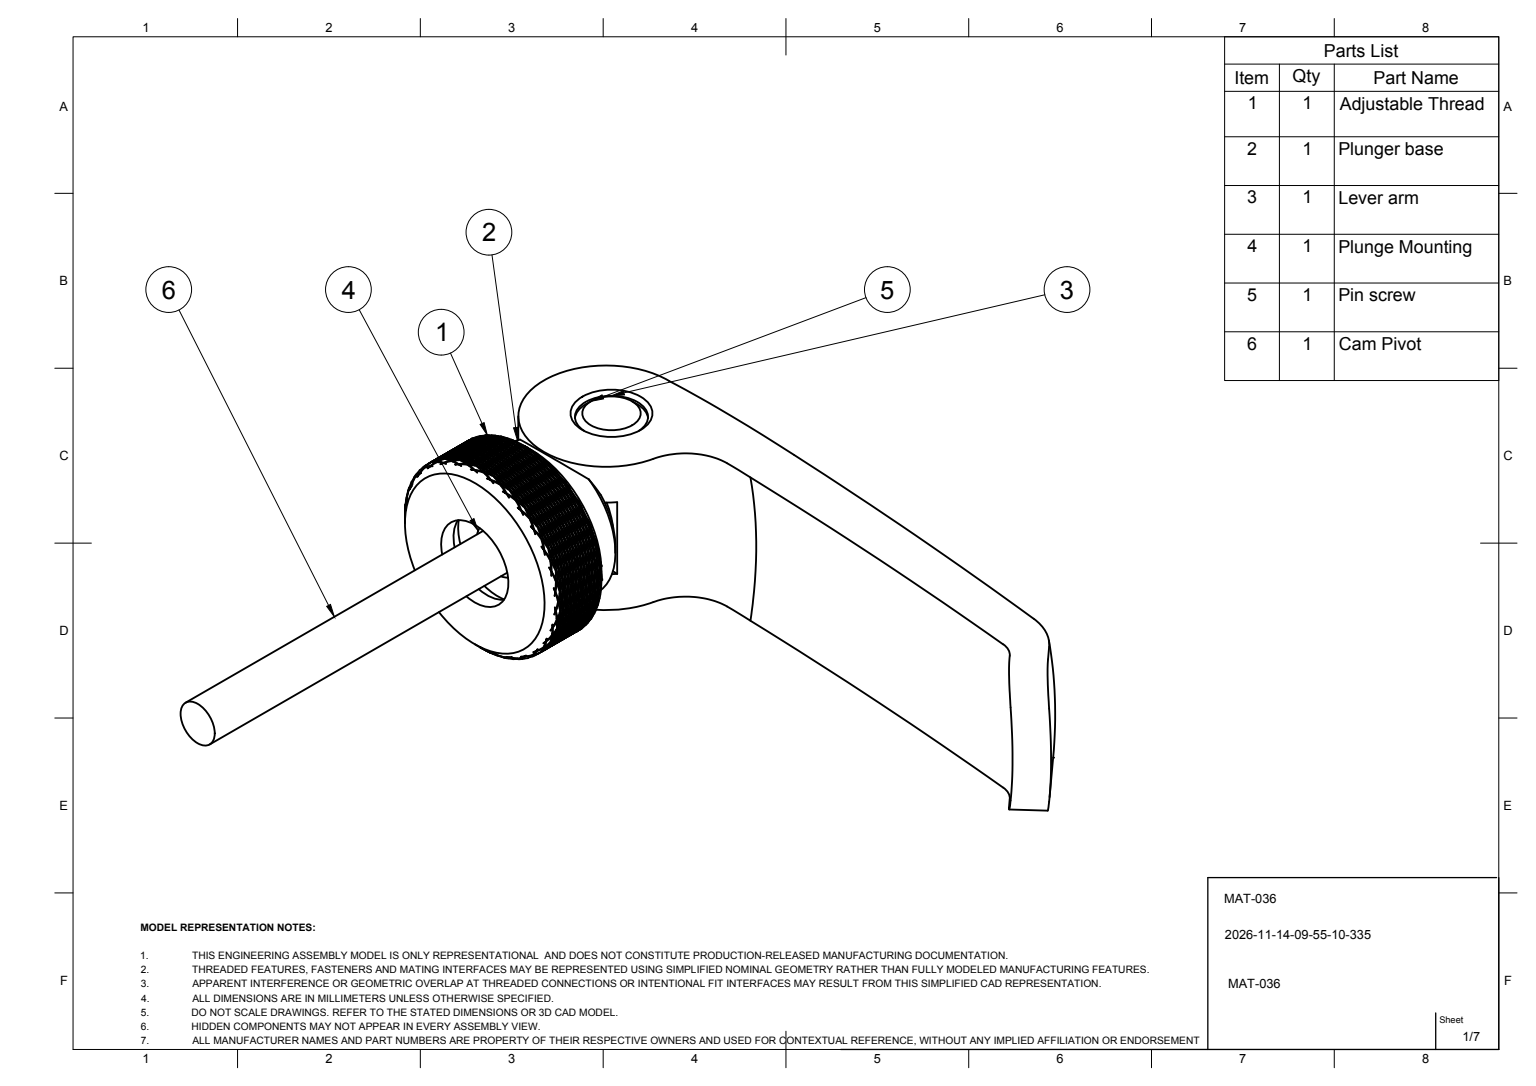
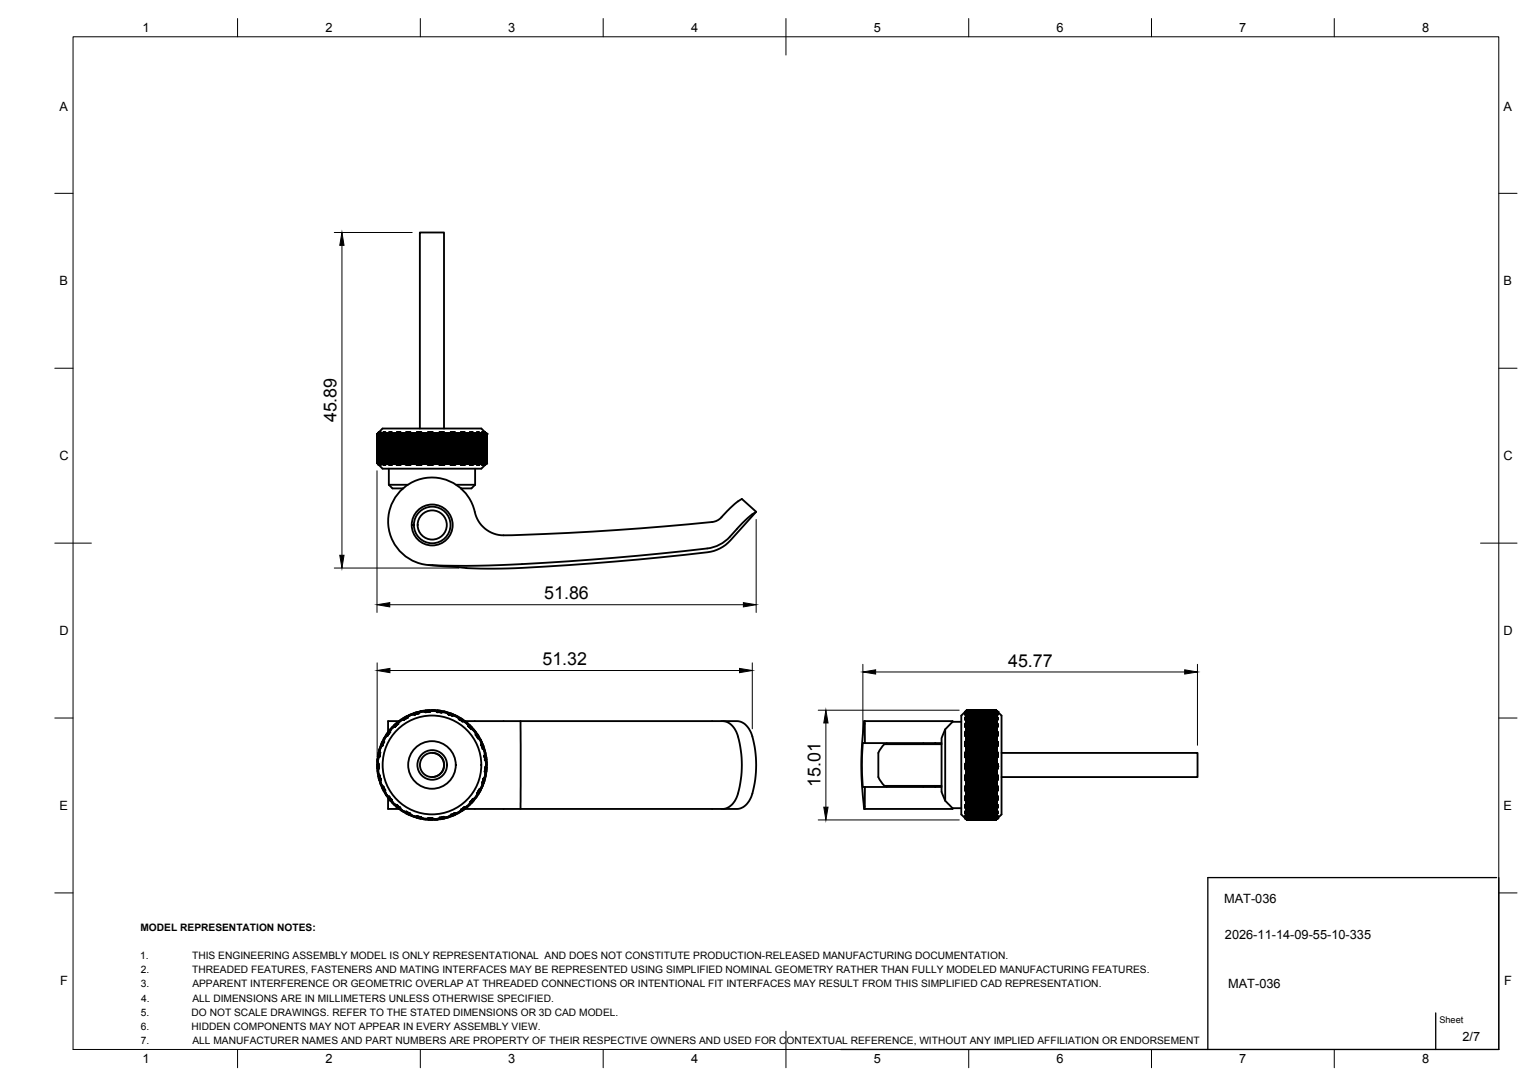
ISO-10303-21;
HEADER;
/* Generated by software containing ST-Developer
 * from STEP Tools, Inc. (www.steptools.com) 
 */

FILE_DESCRIPTION(
/* description */ (''),
/* implementation_level */ '2;1');

FILE_NAME(
/* name */ 'MAT-036.step',
/* time_stamp */ '2026-11-14T09:55:16-08:00',
/* author */ (''),
/* organization */ (''),
/* preprocessor_version */ 'ST-DEVELOPER v20.2',
/* originating_system */ 'Autodesk Translation Framework v15.17.0.0',
/* authorisation */ '');

FILE_SCHEMA (('AUTOMOTIVE_DESIGN { 1 0 10303 214 3 1 1 }'));
ENDSEC;

DATA;
#10=MECHANICAL_DESIGN_GEOMETRIC_PRESENTATION_REPRESENTATION('',(#56,#57,
#58,#59,#60,#61,#62,#63),#170250);
#11=ITEM_DEFINED_TRANSFORMATION($,$,#71472,#77757);
#12=ITEM_DEFINED_TRANSFORMATION($,$,#77641,#77758);
#13=ITEM_DEFINED_TRANSFORMATION($,$,#77681,#77759);
#14=ITEM_DEFINED_TRANSFORMATION($,$,#77711,#77760);
#15=ITEM_DEFINED_TRANSFORMATION($,$,#77739,#77761);
#16=ITEM_DEFINED_TRANSFORMATION($,$,#77751,#77762);
#17=(
REPRESENTATION_RELATIONSHIP($,$,#170276,#170275)
REPRESENTATION_RELATIONSHIP_WITH_TRANSFORMATION(#11)
SHAPE_REPRESENTATION_RELATIONSHIP()
);
#18=(
REPRESENTATION_RELATIONSHIP($,$,#170277,#170275)
REPRESENTATION_RELATIONSHIP_WITH_TRANSFORMATION(#12)
SHAPE_REPRESENTATION_RELATIONSHIP()
);
#19=(
REPRESENTATION_RELATIONSHIP($,$,#170278,#170275)
REPRESENTATION_RELATIONSHIP_WITH_TRANSFORMATION(#13)
SHAPE_REPRESENTATION_RELATIONSHIP()
);
#20=(
REPRESENTATION_RELATIONSHIP($,$,#170279,#170275)
REPRESENTATION_RELATIONSHIP_WITH_TRANSFORMATION(#14)
SHAPE_REPRESENTATION_RELATIONSHIP()
);
#21=(
REPRESENTATION_RELATIONSHIP($,$,#170280,#170275)
REPRESENTATION_RELATIONSHIP_WITH_TRANSFORMATION(#15)
SHAPE_REPRESENTATION_RELATIONSHIP()
);
#22=(
REPRESENTATION_RELATIONSHIP($,$,#170281,#170275)
REPRESENTATION_RELATIONSHIP_WITH_TRANSFORMATION(#16)
SHAPE_REPRESENTATION_RELATIONSHIP()
);
#23=CONTEXT_DEPENDENT_SHAPE_REPRESENTATION(#17,#170269);
#24=CONTEXT_DEPENDENT_SHAPE_REPRESENTATION(#18,#170270);
#25=CONTEXT_DEPENDENT_SHAPE_REPRESENTATION(#19,#170271);
#26=CONTEXT_DEPENDENT_SHAPE_REPRESENTATION(#20,#170272);
#27=CONTEXT_DEPENDENT_SHAPE_REPRESENTATION(#21,#170273);
#28=CONTEXT_DEPENDENT_SHAPE_REPRESENTATION(#22,#170274);
#29=NEXT_ASSEMBLY_USAGE_OCCURRENCE('Adjustable Thread:1',
'Adjustable Thread:1','Adjustable Thread:1',#170283,#170284,
'Adjustable Thread:1');
#30=NEXT_ASSEMBLY_USAGE_OCCURRENCE('Plunger base:1','Plunger base:1',
'Plunger base:1',#170283,#170285,'Plunger base:1');
#31=NEXT_ASSEMBLY_USAGE_OCCURRENCE('Lever arm:1','Lever arm:1',
'Lever arm:1',#170283,#170286,'Lever arm:1');
#32=NEXT_ASSEMBLY_USAGE_OCCURRENCE('Plunge Mounting:1',
'Plunge Mounting:1','Plunge Mounting:1',#170283,#170287,
'Plunge Mounting:1');
#33=NEXT_ASSEMBLY_USAGE_OCCURRENCE('Pin screw:1','Pin screw:1',
'Pin screw:1',#170283,#170288,'Pin screw:1');
#34=NEXT_ASSEMBLY_USAGE_OCCURRENCE('Cam Pivot:1','Cam Pivot:1',
'Cam Pivot:1',#170283,#170289,'Cam Pivot:1');
#35=SPHERICAL_SURFACE('',#77715,4.00000000000002);
#36=B_SPLINE_SURFACE_WITH_KNOTS('',3,3,((#168992,#168993,#168994,#168995),
(#168996,#168997,#168998,#168999),(#169000,#169001,#169002,#169003),(#169004,
#169005,#169006,#169007),(#169008,#169009,#169010,#169011),(#169012,#169013,
#169014,#169015),(#169016,#169017,#169018,#169019),(#169020,#169021,#169022,
#169023),(#169024,#169025,#169026,#169027),(#169028,#169029,#169030,#169031)),
 .UNSPECIFIED.,.F.,.F.,.F.,(4,1,1,1,3,4),(4,4),(0.135790601649557,0.226849968153009,
0.317909334656459,0.40896870115991,0.500028067663362,0.5036704423235),(0.807901539596212,
1.),.UNSPECIFIED.);
#37=B_SPLINE_SURFACE_WITH_KNOTS('',3,3,((#169171,#169172,#169173,#169174,
#169175,#169176,#169177),(#169178,#169179,#169180,#169181,#169182,#169183,
#169184),(#169185,#169186,#169187,#169188,#169189,#169190,#169191),(#169192,
#169193,#169194,#169195,#169196,#169197,#169198),(#169199,#169200,#169201,
#169202,#169203,#169204,#169205),(#169206,#169207,#169208,#169209,#169210,
#169211,#169212),(#169213,#169214,#169215,#169216,#169217,#169218,#169219),
(#169220,#169221,#169222,#169223,#169224,#169225,#169226),(#169227,#169228,
#169229,#169230,#169231,#169232,#169233),(#169234,#169235,#169236,#169237,
#169238,#169239,#169240),(#169241,#169242,#169243,#169244,#169245,#169246,
#169247),(#169248,#169249,#169250,#169251,#169252,#169253,#169254),(#169255,
#169256,#169257,#169258,#169259,#169260,#169261)),.UNSPECIFIED.,.F.,.F.,
 .F.,(4,3,1,1,1,3,4),(4,3,4),(0.114681185572966,0.118496689180301,0.213879533801066,
0.309262378421832,0.404645223042596,0.500028067663362,0.500047049913778),
(-2.58598232202791E-10,0.97179933976621,0.977592668595424),
 .UNSPECIFIED.);
#38=B_SPLINE_SURFACE_WITH_KNOTS('',3,3,((#169612,#169613,#169614,#169615,
#169616,#169617),(#169618,#169619,#169620,#169621,#169622,#169623),(#169624,
#169625,#169626,#169627,#169628,#169629),(#169630,#169631,#169632,#169633,
#169634,#169635),(#169636,#169637,#169638,#169639,#169640,#169641),(#169642,
#169643,#169644,#169645,#169646,#169647),(#169648,#169649,#169650,#169651,
#169652,#169653),(#169654,#169655,#169656,#169657,#169658,#169659),(#169660,
#169661,#169662,#169663,#169664,#169665),(#169666,#169667,#169668,#169669,
#169670,#169671),(#169672,#169673,#169674,#169675,#169676,#169677),(#169678,
#169679,#169680,#169681,#169682,#169683)),.UNSPECIFIED.,.F.,.F.,.F.,(4,
1,1,1,2,1,1,1,4),(4,2,4),(0.618524756843663,0.666209162238205,0.713893567632747,
0.761577973027289,0.809262378421831,0.856946783816374,0.904631189210916,
0.952315594605458,1.),(0.,0.931730586032522,0.937129966266598),
 .UNSPECIFIED.);
#39=B_SPLINE_SURFACE_WITH_KNOTS('',3,3,((#169891,#169892,#169893,#169894),
(#169895,#169896,#169897,#169898),(#169899,#169900,#169901,#169902),(#169903,
#169904,#169905,#169906),(#169907,#169908,#169909,#169910),(#169911,#169912,
#169913,#169914),(#169915,#169916,#169917,#169918),(#169919,#169920,#169921,
#169922),(#169923,#169924,#169925,#169926),(#169927,#169928,#169929,#169930),
(#169931,#169932,#169933,#169934),(#169935,#169936,#169937,#169938),(#169939,
#169940,#169941,#169942),(#169943,#169944,#169945,#169946),(#169947,#169948,
#169949,#169950)),.UNSPECIFIED.,.F.,.F.,.F.,(4,3,1,1,1,2,1,1,1,4),(4,4),
(0.632176856006048,0.635818669312919,0.681341335648804,0.726864001984689,
0.772386668320574,0.81790933465646,0.863432000992345,0.90895466732823,0.954477333664115,
1.),(0.0153819466590792,1.),.UNSPECIFIED.);
#40=OPEN_SHELL('',(#71352));
#41=OPEN_SHELL('',(#71353));
#42=SHELL_BASED_SURFACE_MODEL('Body2',(#40));
#43=SHELL_BASED_SURFACE_MODEL('Body3',(#41));
#44=SHAPE_REPRESENTATION_RELATIONSHIP('SRR','None',#170276,#50);
#45=SHAPE_REPRESENTATION_RELATIONSHIP('SRR','None',#170277,#51);
#46=SHAPE_REPRESENTATION_RELATIONSHIP('SRR','None',#170278,#52);
#47=SHAPE_REPRESENTATION_RELATIONSHIP('SRR','None',#170279,#53);
#48=SHAPE_REPRESENTATION_RELATIONSHIP('SRR','None',#170280,#54);
#49=SHAPE_REPRESENTATION_RELATIONSHIP('SRR','None',#170281,#55);
#50=ADVANCED_BREP_SHAPE_REPRESENTATION('',(#64),#170244);
#51=ADVANCED_BREP_SHAPE_REPRESENTATION('',(#65),#170245);
#52=ADVANCED_BREP_SHAPE_REPRESENTATION('',(#66),#170246);
#53=ADVANCED_BREP_SHAPE_REPRESENTATION('',(#67),#170247);
#54=ADVANCED_BREP_SHAPE_REPRESENTATION('',(#68),#170248);
#55=ADVANCED_BREP_SHAPE_REPRESENTATION('',(#69),#170249);
#56=STYLED_ITEM('',(#170315),#64);
#57=STYLED_ITEM('',(#170314),#65);
#58=STYLED_ITEM('',(#170314),#42);
#59=STYLED_ITEM('',(#170314),#43);
#60=STYLED_ITEM('',(#170316),#66);
#61=STYLED_ITEM('',(#170315),#67);
#62=STYLED_ITEM('',(#170317),#68);
#63=STYLED_ITEM('',(#170315),#69);
#64=MANIFOLD_SOLID_BREP('Body1',#71398);
#65=MANIFOLD_SOLID_BREP('Body1',#71399);
#66=MANIFOLD_SOLID_BREP('Body1',#71400);
#67=MANIFOLD_SOLID_BREP('Body1',#71401);
#68=MANIFOLD_SOLID_BREP('Body1',#71402);
#69=MANIFOLD_SOLID_BREP('Body1',#71403);
#70=FACE_BOUND('',#15472,.T.);
#71=FACE_BOUND('',#15675,.T.);
#72=FACE_BOUND('',#15851,.T.);
#73=FACE_BOUND('',#15853,.T.);
#74=FACE_BOUND('',#15862,.T.);
#75=FACE_BOUND('',#15864,.T.);
#76=FACE_BOUND('',#15893,.T.);
#77=FACE_BOUND('',#15895,.T.);
#78=FACE_BOUND('',#15897,.T.);
#79=FACE_BOUND('',#15901,.T.);
#80=FACE_BOUND('',#15903,.T.);
#81=FACE_BOUND('',#15905,.T.);
#82=FACE_BOUND('',#15911,.T.);
#83=FACE_BOUND('',#15916,.T.);
#84=FACE_BOUND('',#15918,.T.);
#85=FACE_BOUND('',#15920,.T.);
#86=PLANE('',#77414);
#87=PLANE('',#77609);
#88=PLANE('',#77639);
#89=PLANE('',#77640);
#90=PLANE('',#77665);
#91=PLANE('',#77666);
#92=PLANE('',#77667);
#93=PLANE('',#77670);
#94=PLANE('',#77672);
#95=PLANE('',#77673);
#96=PLANE('',#77674);
#97=PLANE('',#77675);
#98=PLANE('',#77702);
#99=PLANE('',#77704);
#100=PLANE('',#77706);
#101=PLANE('',#77707);
#102=PLANE('',#77710);
#103=PLANE('',#77733);
#104=PLANE('',#77734);
#105=PLANE('',#77735);
#106=PLANE('',#77737);
#107=PLANE('',#77738);
#108=PLANE('',#77748);
#109=PLANE('',#77749);
#110=PLANE('',#77755);
#111=PLANE('',#77756);
#112=ELLIPSE('',#76563,9.43047305119864,1.30240788908406);
#113=ELLIPSE('',#76566,9.43046793206525,1.30241506001113);
#114=ELLIPSE('',#76569,9.43050328768157,1.3024182004793);
#115=ELLIPSE('',#76572,9.43068708057878,1.30243363570333);
#116=ELLIPSE('',#76575,9.43006152330499,1.30236357371331);
#117=ELLIPSE('',#76578,9.4302777984402,1.30238875446472);
#118=ELLIPSE('',#76581,9.43072787174344,1.30243587534547);
#119=ELLIPSE('',#76584,9.43045773730215,1.30241075091437);
#120=ELLIPSE('',#76587,9.43030510916545,1.30239601642258);
#121=ELLIPSE('',#76590,9.43064494614307,1.30242369243536);
#122=ELLIPSE('',#76593,9.43056062900003,1.30242031583658);
#123=ELLIPSE('',#76596,9.43045585415815,1.30241175558088);
#124=ELLIPSE('',#76599,9.43046939213538,1.30240966255557);
#125=ELLIPSE('',#76602,9.43067088687587,1.30243579801834);
#126=ELLIPSE('',#76605,9.43040719667397,1.30240457641196);
#127=ELLIPSE('',#76608,9.42988108574405,1.30234497490862);
#128=ELLIPSE('',#76611,9.43068064311873,1.30243410507078);
#129=ELLIPSE('',#76614,9.43052303530734,1.30242084912571);
#130=ELLIPSE('',#76617,9.43038125328305,1.30240668645391);
#131=ELLIPSE('',#76620,9.43072128552616,1.30244009783621);
#132=ELLIPSE('',#76623,9.4305707477918,1.30242345770117);
#133=ELLIPSE('',#76626,9.43046465435441,1.30241113143356);
#134=ELLIPSE('',#76629,9.4308407271015,1.30245127577812);
#135=ELLIPSE('',#76632,9.43070104226015,1.30243878786344);
#136=ELLIPSE('',#76635,9.43055049151391,1.30242224667773);
#137=ELLIPSE('',#76638,9.43061695677763,1.30242474192035);
#138=ELLIPSE('',#76641,9.43035235935973,1.30239838521342);
#139=ELLIPSE('',#76644,9.4305559320503,1.30242196321693);
#140=ELLIPSE('',#76647,9.43068952357752,1.30243327777871);
#141=ELLIPSE('',#77415,9.431895379298,1.30254932670111);
#142=ELLIPSE('',#77418,15.3174410154795,1.90661239924035);
#143=ELLIPSE('',#77421,15.3157768747818,1.90647582479234);
#144=ELLIPSE('',#77424,15.3170696122663,1.90658252792732);
#145=ELLIPSE('',#77427,15.3167139940069,1.90655328959697);
#146=ELLIPSE('',#77430,15.3168209377553,1.90657168275161);
#147=ELLIPSE('',#77433,15.3160754936824,1.90650905813206);
#148=ELLIPSE('',#77436,15.3161208425833,1.90650426169268);
#149=ELLIPSE('',#77439,15.3159589603063,1.90649559716548);
#150=ELLIPSE('',#77442,15.3157944590339,1.9064768703695);
#151=ELLIPSE('',#77445,15.3172323469206,1.9066030234614);
#152=ELLIPSE('',#77448,15.3155039380165,1.9064570427492);
#153=ELLIPSE('',#77451,15.3159291529044,1.90649334528717);
#154=ELLIPSE('',#77454,15.3157700330761,1.90647081272421);
#155=ELLIPSE('',#77457,15.3160955154982,1.90650647722667);
#156=ELLIPSE('',#77460,15.3166693144536,1.90656216883429);
#157=ELLIPSE('',#77463,15.3166817133067,1.90655124693864);
#158=ELLIPSE('',#77466,15.31703730362,1.90657833462818);
#159=ELLIPSE('',#77469,15.3160164937855,1.90649874196003);
#160=ELLIPSE('',#77472,15.3158753484009,1.90648217113556);
#161=ELLIPSE('',#77475,15.3162380117898,1.90650822609983);
#162=ELLIPSE('',#77478,15.3156441463648,1.90646585124018);
#163=ELLIPSE('',#77481,15.317005919152,1.90658194664794);
#164=ELLIPSE('',#77484,15.3161739347467,1.90650429978856);
#165=ELLIPSE('',#77487,15.3153630258202,1.90644004375235);
#166=ELLIPSE('',#77490,15.3163094563979,1.90652013375223);
#167=ELLIPSE('',#77493,15.3167561122212,1.90656182181374);
#168=ELLIPSE('',#77496,15.3163730027201,1.90652953147296);
#169=ELLIPSE('',#77499,15.315903684448,1.90649008174056);
#170=ELLIPSE('',#77530,3.69853833711443,0.520053862149324);
#171=ELLIPSE('',#77535,3.6990050944682,0.520121997590068);
#172=ELLIPSE('',#77538,3.69740745136945,0.519884819312743);
#173=ELLIPSE('',#77541,3.6973850577443,0.519871926709589);
#174=ELLIPSE('',#77544,3.69880689749974,0.520100628836089);
#175=ELLIPSE('',#77547,3.69848799508326,0.520043846508826);
#176=ELLIPSE('',#77552,3.6988594244713,0.520105289468088);
#177=ELLIPSE('',#77555,3.6986202776342,0.520065731438254);
#178=ELLIPSE('',#77558,3.69735633553684,0.519872421748739);
#179=ELLIPSE('',#77561,3.69840385438922,0.520042143078421);
#180=ELLIPSE('',#77566,3.69753466975073,0.519893625210943);
#181=ELLIPSE('',#77569,3.69957450398795,0.520227606150056);
#182=ELLIPSE('',#77574,3.69928463265645,0.520166995452598);
#183=ELLIPSE('',#77579,3.69917885823403,0.520148170670083);
#184=ELLIPSE('',#77582,3.69767815300263,0.519919195910691);
#185=ELLIPSE('',#77589,3.69757944713663,0.519903285571644);
#186=ELLIPSE('',#77592,3.69653763812213,0.519733793607226);
#187=ELLIPSE('',#77595,3.69967418134432,0.520228182339355);
#188=ELLIPSE('',#77598,3.69741584633747,0.519874782638118);
#189=ELLIPSE('',#77601,3.69673411928317,0.519776228529677);
#190=ELLIPSE('',#77604,3.69979295210335,0.520255955848595);
#191=ELLIPSE('',#77607,3.69808486598988,0.51998245490985);
#192=ELLIPSE('',#77705,65.55169862647,42.389902647677);
#193=ELLIPSE('',#77708,65.5506952259048,42.388915448489);
#194=(
BOUNDED_SURFACE()
B_SPLINE_SURFACE(1,2,((#95581,#95582,#95583),(#95584,#95585,#95586)),
 .UNSPECIFIED.,.F.,.F.,.F.)
B_SPLINE_SURFACE_WITH_KNOTS((2,2),(3,3),(0.,0.289681084359929),(0.331965345783649,
0.349369696259361),.UNSPECIFIED.)
GEOMETRIC_REPRESENTATION_ITEM()
RATIONAL_B_SPLINE_SURFACE(((0.988555124858681,0.99035748704491,0.99513694090229),
(0.988555124858681,0.99035748704491,0.99513694090229)))
REPRESENTATION_ITEM('')
SURFACE()
);
#195=(
BOUNDED_SURFACE()
B_SPLINE_SURFACE(1,2,((#95600,#95601,#95602,#95603,#95604),(#95605,#95606,
#95607,#95608,#95609),(#95610,#95611,#95612,#95613,#95614)),
 .UNSPECIFIED.,.F.,.F.,.F.)
B_SPLINE_SURFACE_WITH_KNOTS((2,1,2),(3,2,3),(-0.00289807040992861,0.,0.29039955403664),
(0.383340713896693,0.383933227114987,0.401145492974693),.UNSPECIFIED.)
GEOMETRIC_REPRESENTATION_ITEM()
RATIONAL_B_SPLINE_SURFACE(((0.988246641953811,0.988246641953811,0.988246641953811,
0.986737013496293,0.988139125479962),(0.988246641953811,0.988246641953811,
0.988246641953811,0.986737013496293,0.988139125479962),(0.988246641953811,
0.988246641953811,0.988246641953811,0.986737013496293,0.988139125479961)))
REPRESENTATION_ITEM('')
SURFACE()
);
#196=(
BOUNDED_SURFACE()
B_SPLINE_SURFACE(1,2,((#95639,#95640,#95641),(#95642,#95643,#95644)),
 .UNSPECIFIED.,.F.,.F.,.F.)
B_SPLINE_SURFACE_WITH_KNOTS((2,2),(3,3),(0.,0.289681084359919),(0.331965345783649,
0.349369696259361),.UNSPECIFIED.)
GEOMETRIC_REPRESENTATION_ITEM()
RATIONAL_B_SPLINE_SURFACE(((0.988555124858681,0.99035748704491,0.99513694090229),
(0.988555124858682,0.99035748704491,0.99513694090229)))
REPRESENTATION_ITEM('')
SURFACE()
);
#197=(
BOUNDED_SURFACE()
B_SPLINE_SURFACE(1,2,((#95648,#95649,#95650,#95651,#95652),(#95653,#95654,
#95655,#95656,#95657),(#95658,#95659,#95660,#95661,#95662)),
 .UNSPECIFIED.,.F.,.F.,.F.)
B_SPLINE_SURFACE_WITH_KNOTS((2,1,2),(3,2,3),(-0.00289807040992683,0.,0.290399554012505),
(0.38334071392065,0.383933227114987,0.401145492974695),.UNSPECIFIED.)
GEOMETRIC_REPRESENTATION_ITEM()
RATIONAL_B_SPLINE_SURFACE(((0.988246641953811,0.988246641953811,0.988246641953811,
0.986737013496293,0.988139125479962),(0.988246641953811,0.988246641953811,
0.988246641953811,0.986737013496293,0.988139125479962),(0.988246641953811,
0.988246641953811,0.988246641953811,0.986737013496293,0.988139125479962)))
REPRESENTATION_ITEM('')
SURFACE()
);
#198=(
BOUNDED_SURFACE()
B_SPLINE_SURFACE(1,2,((#95687,#95688,#95689),(#95690,#95691,#95692)),
 .UNSPECIFIED.,.F.,.F.,.F.)
B_SPLINE_SURFACE_WITH_KNOTS((2,2),(3,3),(0.,0.289681084359922),(0.331965345783648,
0.349369696259454),.UNSPECIFIED.)
GEOMETRIC_REPRESENTATION_ITEM()
RATIONAL_B_SPLINE_SURFACE(((0.988555124858681,0.99035748704492,0.995136940902341),
(0.988555124858682,0.99035748704492,0.995136940902341)))
REPRESENTATION_ITEM('')
SURFACE()
);
#199=(
BOUNDED_SURFACE()
B_SPLINE_SURFACE(1,2,((#95696,#95697,#95698,#95699,#95700),(#95701,#95702,
#95703,#95704,#95705),(#95706,#95707,#95708,#95709,#95710)),
 .UNSPECIFIED.,.F.,.F.,.F.)
B_SPLINE_SURFACE_WITH_KNOTS((2,1,2),(3,2,3),(-0.00289807040992654,0.,0.290399554026877),
(0.383340713906249,0.383933227114987,0.401145492974697),.UNSPECIFIED.)
GEOMETRIC_REPRESENTATION_ITEM()
RATIONAL_B_SPLINE_SURFACE(((0.988246641953811,0.988246641953811,0.988246641953811,
0.986737013496293,0.988139125479962),(0.988246641953811,0.988246641953811,
0.988246641953811,0.986737013496293,0.988139125479962),(0.988246641953811,
0.988246641953811,0.988246641953811,0.986737013496293,0.988139125479962)))
REPRESENTATION_ITEM('')
SURFACE()
);
#200=(
BOUNDED_SURFACE()
B_SPLINE_SURFACE(1,2,((#95735,#95736,#95737),(#95738,#95739,#95740)),
 .UNSPECIFIED.,.F.,.F.,.F.)
B_SPLINE_SURFACE_WITH_KNOTS((2,2),(3,3),(0.,0.289681084359918),(0.331965345783649,
0.349369696259361),.UNSPECIFIED.)
GEOMETRIC_REPRESENTATION_ITEM()
RATIONAL_B_SPLINE_SURFACE(((0.988555124858682,0.99035748704491,0.99513694090229),
(0.988555124858682,0.99035748704491,0.99513694090229)))
REPRESENTATION_ITEM('')
SURFACE()
);
#201=(
BOUNDED_SURFACE()
B_SPLINE_SURFACE(1,2,((#95744,#95745,#95746,#95747,#95748),(#95749,#95750,
#95751,#95752,#95753),(#95754,#95755,#95756,#95757,#95758)),
 .UNSPECIFIED.,.F.,.F.,.F.)
B_SPLINE_SURFACE_WITH_KNOTS((2,1,2),(3,2,3),(-0.00289807040992802,0.,0.29039955403663),
(0.383340713896644,0.383933227114987,0.401145492974693),.UNSPECIFIED.)
GEOMETRIC_REPRESENTATION_ITEM()
RATIONAL_B_SPLINE_SURFACE(((0.988246641953811,0.988246641953811,0.988246641953811,
0.986737013496293,0.988139125479962),(0.988246641953811,0.988246641953811,
0.988246641953811,0.986737013496293,0.988139125479962),(0.988246641953811,
0.988246641953811,0.988246641953811,0.986737013496293,0.988139125479962)))
REPRESENTATION_ITEM('')
SURFACE()
);
#202=(
BOUNDED_SURFACE()
B_SPLINE_SURFACE(1,2,((#95783,#95784,#95785),(#95786,#95787,#95788)),
 .UNSPECIFIED.,.F.,.F.,.F.)
B_SPLINE_SURFACE_WITH_KNOTS((2,2),(3,3),(0.,0.289681084359923),(0.331965345783649,
0.349369696259361),.UNSPECIFIED.)
GEOMETRIC_REPRESENTATION_ITEM()
RATIONAL_B_SPLINE_SURFACE(((0.988555124858681,0.99035748704491,0.99513694090229),
(0.988555124858682,0.99035748704491,0.99513694090229)))
REPRESENTATION_ITEM('')
SURFACE()
);
#203=(
BOUNDED_SURFACE()
B_SPLINE_SURFACE(1,2,((#95792,#95793,#95794,#95795,#95796),(#95797,#95798,
#95799,#95800,#95801),(#95802,#95803,#95804,#95805,#95806)),
 .UNSPECIFIED.,.F.,.F.,.F.)
B_SPLINE_SURFACE_WITH_KNOTS((2,1,2),(3,2,3),(-0.00289807040992325,0.,0.290399554035561),
(0.383340713897236,0.383933227114987,0.401145492974693),.UNSPECIFIED.)
GEOMETRIC_REPRESENTATION_ITEM()
RATIONAL_B_SPLINE_SURFACE(((0.988246641953811,0.988246641953811,0.988246641953811,
0.986737013496293,0.988139125479962),(0.988246641953811,0.988246641953811,
0.988246641953811,0.986737013496293,0.988139125479962),(0.988246641953811,
0.988246641953811,0.988246641953811,0.986737013496293,0.988139125479961)))
REPRESENTATION_ITEM('')
SURFACE()
);
#204=(
BOUNDED_SURFACE()
B_SPLINE_SURFACE(1,2,((#95831,#95832,#95833),(#95834,#95835,#95836)),
 .UNSPECIFIED.,.F.,.F.,.F.)
B_SPLINE_SURFACE_WITH_KNOTS((2,2),(3,3),(0.,0.289681084359924),(0.331965345783649,
0.349369696259361),.UNSPECIFIED.)
GEOMETRIC_REPRESENTATION_ITEM()
RATIONAL_B_SPLINE_SURFACE(((0.988555124858681,0.99035748704491,0.99513694090229),
(0.988555124858682,0.99035748704491,0.99513694090229)))
REPRESENTATION_ITEM('')
SURFACE()
);
#205=(
BOUNDED_SURFACE()
B_SPLINE_SURFACE(1,2,((#95840,#95841,#95842,#95843,#95844),(#95845,#95846,
#95847,#95848,#95849),(#95850,#95851,#95852,#95853,#95854)),
 .UNSPECIFIED.,.F.,.F.,.F.)
B_SPLINE_SURFACE_WITH_KNOTS((2,1,2),(3,2,3),(-0.00289807040992448,0.,0.290399554023854),
(0.383340713909065,0.383933227114976,0.401145492974693),.UNSPECIFIED.)
GEOMETRIC_REPRESENTATION_ITEM()
RATIONAL_B_SPLINE_SURFACE(((0.988246641953813,0.988246641953813,0.988246641953813,
0.986737013496292,0.988139125479961),(0.988246641953813,0.988246641953813,
0.988246641953813,0.986737013496292,0.988139125479961),(0.988246641953813,
0.988246641953813,0.988246641953813,0.986737013496292,0.988139125479961)))
REPRESENTATION_ITEM('')
SURFACE()
);
#206=(
BOUNDED_SURFACE()
B_SPLINE_SURFACE(1,2,((#95879,#95880,#95881),(#95882,#95883,#95884)),
 .UNSPECIFIED.,.F.,.F.,.F.)
B_SPLINE_SURFACE_WITH_KNOTS((2,2),(3,3),(0.,0.289681084359932),(0.331965345783649,
0.349369696259361),.UNSPECIFIED.)
GEOMETRIC_REPRESENTATION_ITEM()
RATIONAL_B_SPLINE_SURFACE(((0.988555124858682,0.99035748704491,0.99513694090229),
(0.988555124858682,0.99035748704491,0.99513694090229)))
REPRESENTATION_ITEM('')
SURFACE()
);
#207=(
BOUNDED_SURFACE()
B_SPLINE_SURFACE(1,2,((#95888,#95889,#95890,#95891,#95892),(#95893,#95894,
#95895,#95896,#95897),(#95898,#95899,#95900,#95901,#95902)),
 .UNSPECIFIED.,.F.,.F.,.F.)
B_SPLINE_SURFACE_WITH_KNOTS((2,1,2),(3,2,3),(-0.00289807040992691,0.,0.290399554024332),
(0.383340713908832,0.383933227114987,0.401145492974693),.UNSPECIFIED.)
GEOMETRIC_REPRESENTATION_ITEM()
RATIONAL_B_SPLINE_SURFACE(((0.988246641953811,0.988246641953811,0.988246641953811,
0.986737013496293,0.988139125479962),(0.988246641953811,0.988246641953811,
0.988246641953811,0.986737013496293,0.988139125479962),(0.988246641953811,
0.988246641953811,0.988246641953811,0.986737013496293,0.988139125479962)))
REPRESENTATION_ITEM('')
SURFACE()
);
#208=(
BOUNDED_SURFACE()
B_SPLINE_SURFACE(1,2,((#95912,#95913,#95914),(#95915,#95916,#95917)),
 .UNSPECIFIED.,.F.,.F.,.F.)
B_SPLINE_SURFACE_WITH_KNOTS((2,2),(3,3),(0.,0.289681084359925),(0.331965345783649,
0.349369696259361),.UNSPECIFIED.)
GEOMETRIC_REPRESENTATION_ITEM()
RATIONAL_B_SPLINE_SURFACE(((0.988555124858682,0.99035748704491,0.99513694090229),
(0.988555124858682,0.99035748704491,0.99513694090229)))
REPRESENTATION_ITEM('')
SURFACE()
);
#209=(
BOUNDED_SURFACE()
B_SPLINE_SURFACE(1,2,((#95921,#95922,#95923,#95924,#95925),(#95926,#95927,
#95928,#95929,#95930),(#95931,#95932,#95933,#95934,#95935)),
 .UNSPECIFIED.,.F.,.F.,.F.)
B_SPLINE_SURFACE_WITH_KNOTS((2,1,2),(3,2,3),(-0.00289807040992912,0.,0.290399554034495),
(0.383340713898888,0.383933227114987,0.401145492974693),.UNSPECIFIED.)
GEOMETRIC_REPRESENTATION_ITEM()
RATIONAL_B_SPLINE_SURFACE(((0.988246641953811,0.988246641953811,0.988246641953811,
0.986737013496293,0.988139125479962),(0.988246641953811,0.988246641953811,
0.988246641953811,0.986737013496293,0.988139125479962),(0.988246641953811,
0.988246641953811,0.988246641953811,0.986737013496293,0.988139125479962)))
REPRESENTATION_ITEM('')
SURFACE()
);
#210=(
BOUNDED_SURFACE()
B_SPLINE_SURFACE(1,2,((#95960,#95961,#95962),(#95963,#95964,#95965)),
 .UNSPECIFIED.,.F.,.F.,.F.)
B_SPLINE_SURFACE_WITH_KNOTS((2,2),(3,3),(0.,0.28968108435992),(0.331965345783649,
0.349369696259364),.UNSPECIFIED.)
GEOMETRIC_REPRESENTATION_ITEM()
RATIONAL_B_SPLINE_SURFACE(((0.988555124858682,0.990357487044911,0.995136940902291),
(0.988555124858682,0.990357487044911,0.995136940902291)))
REPRESENTATION_ITEM('')
SURFACE()
);
#211=(
BOUNDED_SURFACE()
B_SPLINE_SURFACE(1,2,((#95969,#95970,#95971,#95972,#95973),(#95974,#95975,
#95976,#95977,#95978),(#95979,#95980,#95981,#95982,#95983)),
 .UNSPECIFIED.,.F.,.F.,.F.)
B_SPLINE_SURFACE_WITH_KNOTS((2,1,2),(3,2,3),(-0.0028980704099176,0.,0.290399554034344),
(0.383340713897888,0.383933227114987,0.401145492974693),.UNSPECIFIED.)
GEOMETRIC_REPRESENTATION_ITEM()
RATIONAL_B_SPLINE_SURFACE(((0.988246641953811,0.988246641953811,0.988246641953811,
0.986737013496293,0.988139125479962),(0.988246641953811,0.988246641953811,
0.988246641953811,0.986737013496293,0.988139125479962),(0.988246641953811,
0.988246641953811,0.988246641953811,0.986737013496293,0.988139125479961)))
REPRESENTATION_ITEM('')
SURFACE()
);
#212=(
BOUNDED_SURFACE()
B_SPLINE_SURFACE(1,2,((#96008,#96009,#96010),(#96011,#96012,#96013)),
 .UNSPECIFIED.,.F.,.F.,.F.)
B_SPLINE_SURFACE_WITH_KNOTS((2,2),(3,3),(0.,0.289681084359917),(0.331965345783649,
0.349369696259361),.UNSPECIFIED.)
GEOMETRIC_REPRESENTATION_ITEM()
RATIONAL_B_SPLINE_SURFACE(((0.988555124858681,0.99035748704491,0.99513694090229),
(0.988555124858681,0.99035748704491,0.99513694090229)))
REPRESENTATION_ITEM('')
SURFACE()
);
#213=(
BOUNDED_SURFACE()
B_SPLINE_SURFACE(1,2,((#96017,#96018,#96019,#96020,#96021),(#96022,#96023,
#96024,#96025,#96026),(#96027,#96028,#96029,#96030,#96031)),
 .UNSPECIFIED.,.F.,.F.,.F.)
B_SPLINE_SURFACE_WITH_KNOTS((2,1,2),(3,2,3),(-0.00289807040991716,0.,0.29039955402085),
(0.383340713911338,0.383933227114987,0.401145492974693),.UNSPECIFIED.)
GEOMETRIC_REPRESENTATION_ITEM()
RATIONAL_B_SPLINE_SURFACE(((0.988246641953811,0.988246641953811,0.988246641953811,
0.986737013496293,0.988139125479962),(0.988246641953811,0.988246641953811,
0.988246641953811,0.986737013496293,0.988139125479962),(0.988246641953811,
0.988246641953811,0.988246641953811,0.986737013496293,0.988139125479962)))
REPRESENTATION_ITEM('')
SURFACE()
);
#214=(
BOUNDED_SURFACE()
B_SPLINE_SURFACE(1,2,((#96056,#96057,#96058),(#96059,#96060,#96061)),
 .UNSPECIFIED.,.F.,.F.,.F.)
B_SPLINE_SURFACE_WITH_KNOTS((2,2),(3,3),(0.,0.289681084359927),(0.331965345783649,
0.349369696259361),.UNSPECIFIED.)
GEOMETRIC_REPRESENTATION_ITEM()
RATIONAL_B_SPLINE_SURFACE(((0.988555124858681,0.99035748704491,0.99513694090229),
(0.988555124858682,0.99035748704491,0.99513694090229)))
REPRESENTATION_ITEM('')
SURFACE()
);
#215=(
BOUNDED_SURFACE()
B_SPLINE_SURFACE(1,2,((#96065,#96066,#96067,#96068,#96069),(#96070,#96071,
#96072,#96073,#96074),(#96075,#96076,#96077,#96078,#96079)),
 .UNSPECIFIED.,.F.,.F.,.F.)
B_SPLINE_SURFACE_WITH_KNOTS((2,1,2),(3,2,3),(-0.00289807040991567,0.,0.290399554021739),
(0.3833407139103,0.383933227114987,0.401145492974693),.UNSPECIFIED.)
GEOMETRIC_REPRESENTATION_ITEM()
RATIONAL_B_SPLINE_SURFACE(((0.988246641953811,0.988246641953811,0.988246641953811,
0.986737013496293,0.988139125479962),(0.988246641953811,0.988246641953811,
0.988246641953811,0.986737013496293,0.988139125479962),(0.988246641953811,
0.988246641953811,0.988246641953811,0.986737013496293,0.988139125479962)))
REPRESENTATION_ITEM('')
SURFACE()
);
#216=(
BOUNDED_SURFACE()
B_SPLINE_SURFACE(1,2,((#96104,#96105,#96106),(#96107,#96108,#96109)),
 .UNSPECIFIED.,.F.,.F.,.F.)
B_SPLINE_SURFACE_WITH_KNOTS((2,2),(3,3),(0.,0.289681084359927),(0.331965345783649,
0.349369696259361),.UNSPECIFIED.)
GEOMETRIC_REPRESENTATION_ITEM()
RATIONAL_B_SPLINE_SURFACE(((0.988555124858681,0.99035748704491,0.99513694090229),
(0.988555124858682,0.99035748704491,0.99513694090229)))
REPRESENTATION_ITEM('')
SURFACE()
);
#217=(
BOUNDED_SURFACE()
B_SPLINE_SURFACE(1,2,((#96113,#96114,#96115,#96116,#96117),(#96118,#96119,
#96120,#96121,#96122),(#96123,#96124,#96125,#96126,#96127)),
 .UNSPECIFIED.,.F.,.F.,.F.)
B_SPLINE_SURFACE_WITH_KNOTS((2,1,2),(3,2,3),(-0.00289807040991562,0.,0.290399554030109),
(0.383340713901925,0.383933227114987,0.401145492974693),.UNSPECIFIED.)
GEOMETRIC_REPRESENTATION_ITEM()
RATIONAL_B_SPLINE_SURFACE(((0.988246641953811,0.988246641953811,0.988246641953811,
0.986737013496293,0.988139125479962),(0.988246641953811,0.988246641953811,
0.988246641953811,0.986737013496293,0.988139125479962),(0.988246641953811,
0.988246641953811,0.988246641953811,0.986737013496293,0.988139125479962)))
REPRESENTATION_ITEM('')
SURFACE()
);
#218=(
BOUNDED_SURFACE()
B_SPLINE_SURFACE(1,2,((#96152,#96153,#96154),(#96155,#96156,#96157)),
 .UNSPECIFIED.,.F.,.F.,.F.)
B_SPLINE_SURFACE_WITH_KNOTS((2,2),(3,3),(0.,0.289681084359926),(0.331965345783649,
0.349369696259361),.UNSPECIFIED.)
GEOMETRIC_REPRESENTATION_ITEM()
RATIONAL_B_SPLINE_SURFACE(((0.988555124858682,0.99035748704491,0.99513694090229),
(0.988555124858682,0.99035748704491,0.99513694090229)))
REPRESENTATION_ITEM('')
SURFACE()
);
#219=(
BOUNDED_SURFACE()
B_SPLINE_SURFACE(1,2,((#96161,#96162,#96163,#96164,#96165),(#96166,#96167,
#96168,#96169,#96170),(#96171,#96172,#96173,#96174,#96175)),
 .UNSPECIFIED.,.F.,.F.,.F.)
B_SPLINE_SURFACE_WITH_KNOTS((2,1,2),(3,2,3),(-0.00289807040991561,0.,0.290399554022484),
(0.383340713909549,0.383933227114987,0.401145492974693),.UNSPECIFIED.)
GEOMETRIC_REPRESENTATION_ITEM()
RATIONAL_B_SPLINE_SURFACE(((0.988246641953811,0.988246641953811,0.988246641953811,
0.986737013496293,0.988139125479962),(0.988246641953811,0.988246641953811,
0.988246641953811,0.986737013496293,0.988139125479962),(0.988246641953811,
0.988246641953811,0.988246641953811,0.986737013496293,0.988139125479962)))
REPRESENTATION_ITEM('')
SURFACE()
);
#220=(
BOUNDED_SURFACE()
B_SPLINE_SURFACE(1,2,((#96200,#96201,#96202),(#96203,#96204,#96205)),
 .UNSPECIFIED.,.F.,.F.,.F.)
B_SPLINE_SURFACE_WITH_KNOTS((2,2),(3,3),(0.,0.289681084359927),(0.331965345783649,
0.349369696259361),.UNSPECIFIED.)
GEOMETRIC_REPRESENTATION_ITEM()
RATIONAL_B_SPLINE_SURFACE(((0.988555124858682,0.99035748704491,0.99513694090229),
(0.988555124858682,0.99035748704491,0.99513694090229)))
REPRESENTATION_ITEM('')
SURFACE()
);
#221=(
BOUNDED_SURFACE()
B_SPLINE_SURFACE(1,2,((#96209,#96210,#96211,#96212,#96213),(#96214,#96215,
#96216,#96217,#96218),(#96219,#96220,#96221,#96222,#96223)),
 .UNSPECIFIED.,.F.,.F.,.F.)
B_SPLINE_SURFACE_WITH_KNOTS((2,1,2),(3,2,3),(-0.00289807040991793,0.,0.290399554012505),
(0.38334071391976,0.383933227114987,0.401145492974693),.UNSPECIFIED.)
GEOMETRIC_REPRESENTATION_ITEM()
RATIONAL_B_SPLINE_SURFACE(((0.988246641953811,0.988246641953811,0.988246641953811,
0.986737013496293,0.988139125479962),(0.988246641953811,0.988246641953811,
0.988246641953811,0.986737013496293,0.988139125479962),(0.988246641953811,
0.988246641953811,0.988246641953811,0.986737013496293,0.988139125479962)))
REPRESENTATION_ITEM('')
SURFACE()
);
#222=(
BOUNDED_SURFACE()
B_SPLINE_SURFACE(1,2,((#96248,#96249,#96250),(#96251,#96252,#96253)),
 .UNSPECIFIED.,.F.,.F.,.F.)
B_SPLINE_SURFACE_WITH_KNOTS((2,2),(3,3),(0.,0.289681084359918),(0.331965345783649,
0.349369696259361),.UNSPECIFIED.)
GEOMETRIC_REPRESENTATION_ITEM()
RATIONAL_B_SPLINE_SURFACE(((0.988555124858682,0.99035748704491,0.99513694090229),
(0.988555124858682,0.99035748704491,0.99513694090229)))
REPRESENTATION_ITEM('')
SURFACE()
);
#223=(
BOUNDED_SURFACE()
B_SPLINE_SURFACE(1,2,((#96257,#96258,#96259,#96260,#96261),(#96262,#96263,
#96264,#96265,#96266),(#96267,#96268,#96269,#96270,#96271)),
 .UNSPECIFIED.,.F.,.F.,.F.)
B_SPLINE_SURFACE_WITH_KNOTS((2,1,2),(3,2,3),(-0.00289807040991568,0.,0.290399554034899),
(0.38334071389714,0.383933227114987,0.401145492974693),.UNSPECIFIED.)
GEOMETRIC_REPRESENTATION_ITEM()
RATIONAL_B_SPLINE_SURFACE(((0.988246641953811,0.988246641953811,0.988246641953811,
0.986737013496293,0.988139125479962),(0.988246641953811,0.988246641953811,
0.988246641953811,0.986737013496293,0.988139125479962),(0.988246641953811,
0.988246641953811,0.988246641953811,0.986737013496293,0.988139125479962)))
REPRESENTATION_ITEM('')
SURFACE()
);
#224=(
BOUNDED_SURFACE()
B_SPLINE_SURFACE(1,2,((#96296,#96297,#96298),(#96299,#96300,#96301)),
 .UNSPECIFIED.,.F.,.F.,.F.)
B_SPLINE_SURFACE_WITH_KNOTS((2,2),(3,3),(0.,0.289681084359924),(0.331965345783649,
0.349369696259361),.UNSPECIFIED.)
GEOMETRIC_REPRESENTATION_ITEM()
RATIONAL_B_SPLINE_SURFACE(((0.988555124858681,0.99035748704491,0.99513694090229),
(0.988555124858682,0.99035748704491,0.99513694090229)))
REPRESENTATION_ITEM('')
SURFACE()
);
#225=(
BOUNDED_SURFACE()
B_SPLINE_SURFACE(1,2,((#96305,#96306,#96307,#96308,#96309),(#96310,#96311,
#96312,#96313,#96314),(#96315,#96316,#96317,#96318,#96319)),
 .UNSPECIFIED.,.F.,.F.,.F.)
B_SPLINE_SURFACE_WITH_KNOTS((2,1,2),(3,2,3),(-0.0028980704099169,0.,0.290399554016211),
(0.383340713915951,0.383933227114987,0.401145492974693),.UNSPECIFIED.)
GEOMETRIC_REPRESENTATION_ITEM()
RATIONAL_B_SPLINE_SURFACE(((0.988246641953811,0.988246641953811,0.988246641953811,
0.986737013496293,0.988139125479962),(0.988246641953811,0.988246641953811,
0.988246641953811,0.986737013496293,0.988139125479962),(0.988246641953811,
0.988246641953811,0.988246641953811,0.986737013496293,0.988139125479962)))
REPRESENTATION_ITEM('')
SURFACE()
);
#226=(
BOUNDED_SURFACE()
B_SPLINE_SURFACE(1,2,((#96344,#96345,#96346),(#96347,#96348,#96349)),
 .UNSPECIFIED.,.F.,.F.,.F.)
B_SPLINE_SURFACE_WITH_KNOTS((2,2),(3,3),(0.,0.289681084359922),(0.331965345783649,
0.349369696259361),.UNSPECIFIED.)
GEOMETRIC_REPRESENTATION_ITEM()
RATIONAL_B_SPLINE_SURFACE(((0.988555124858682,0.99035748704491,0.99513694090229),
(0.988555124858682,0.99035748704491,0.99513694090229)))
REPRESENTATION_ITEM('')
SURFACE()
);
#227=(
BOUNDED_SURFACE()
B_SPLINE_SURFACE(1,2,((#96353,#96354,#96355,#96356,#96357),(#96358,#96359,
#96360,#96361,#96362),(#96363,#96364,#96365,#96366,#96367)),
 .UNSPECIFIED.,.F.,.F.,.F.)
B_SPLINE_SURFACE_WITH_KNOTS((2,1,2),(3,2,3),(-0.00289807040992971,0.,0.290399554009193),
(0.38334071392425,0.383933227114987,0.401145492974693),.UNSPECIFIED.)
GEOMETRIC_REPRESENTATION_ITEM()
RATIONAL_B_SPLINE_SURFACE(((0.988246641953811,0.988246641953811,0.988246641953811,
0.986737013496293,0.988139125479962),(0.988246641953811,0.988246641953811,
0.988246641953811,0.986737013496293,0.988139125479962),(0.988246641953811,
0.988246641953811,0.988246641953811,0.986737013496293,0.988139125479962)))
REPRESENTATION_ITEM('')
SURFACE()
);
#228=(
BOUNDED_SURFACE()
B_SPLINE_SURFACE(1,2,((#96392,#96393,#96394),(#96395,#96396,#96397)),
 .UNSPECIFIED.,.F.,.F.,.F.)
B_SPLINE_SURFACE_WITH_KNOTS((2,2),(3,3),(0.,0.28968108435992),(0.331965345783649,
0.349369696259361),.UNSPECIFIED.)
GEOMETRIC_REPRESENTATION_ITEM()
RATIONAL_B_SPLINE_SURFACE(((0.988555124858682,0.99035748704491,0.99513694090229),
(0.988555124858682,0.99035748704491,0.99513694090229)))
REPRESENTATION_ITEM('')
SURFACE()
);
#229=(
BOUNDED_SURFACE()
B_SPLINE_SURFACE(1,2,((#96401,#96402,#96403,#96404,#96405),(#96406,#96407,
#96408,#96409,#96410),(#96411,#96412,#96413,#96414,#96415)),
 .UNSPECIFIED.,.F.,.F.,.F.)
B_SPLINE_SURFACE_WITH_KNOTS((2,1,2),(3,2,3),(-0.00289807040991918,0.,0.290399554039631),
(0.383340713892758,0.383933227114987,0.401145492974693),.UNSPECIFIED.)
GEOMETRIC_REPRESENTATION_ITEM()
RATIONAL_B_SPLINE_SURFACE(((0.988246641953811,0.988246641953811,0.988246641953811,
0.986737013496293,0.988139125479962),(0.988246641953811,0.988246641953811,
0.988246641953811,0.986737013496293,0.988139125479962),(0.988246641953811,
0.988246641953811,0.988246641953811,0.986737013496293,0.988139125479962)))
REPRESENTATION_ITEM('')
SURFACE()
);
#230=(
BOUNDED_SURFACE()
B_SPLINE_SURFACE(1,2,((#96440,#96441,#96442),(#96443,#96444,#96445)),
 .UNSPECIFIED.,.F.,.F.,.F.)
B_SPLINE_SURFACE_WITH_KNOTS((2,2),(3,3),(0.,0.289681084359919),(0.331965345783649,
0.349369696259361),.UNSPECIFIED.)
GEOMETRIC_REPRESENTATION_ITEM()
RATIONAL_B_SPLINE_SURFACE(((0.988555124858682,0.99035748704491,0.99513694090229),
(0.988555124858682,0.99035748704491,0.99513694090229)))
REPRESENTATION_ITEM('')
SURFACE()
);
#231=(
BOUNDED_SURFACE()
B_SPLINE_SURFACE(1,2,((#96449,#96450,#96451,#96452,#96453),(#96454,#96455,
#96456,#96457,#96458),(#96459,#96460,#96461,#96462,#96463)),
 .UNSPECIFIED.,.F.,.F.,.F.)
B_SPLINE_SURFACE_WITH_KNOTS((2,1,2),(3,2,3),(-0.0028980704099156,0.,0.290399554016024),
(0.383340713916008,0.383933227114987,0.401145492974693),.UNSPECIFIED.)
GEOMETRIC_REPRESENTATION_ITEM()
RATIONAL_B_SPLINE_SURFACE(((0.988246641953811,0.988246641953811,0.988246641953811,
0.986737013496293,0.988139125479962),(0.988246641953811,0.988246641953811,
0.988246641953811,0.986737013496293,0.988139125479962),(0.988246641953811,
0.988246641953811,0.988246641953811,0.986737013496293,0.988139125479962)))
REPRESENTATION_ITEM('')
SURFACE()
);
#232=(
BOUNDED_SURFACE()
B_SPLINE_SURFACE(1,2,((#96488,#96489,#96490),(#96491,#96492,#96493)),
 .UNSPECIFIED.,.F.,.F.,.F.)
B_SPLINE_SURFACE_WITH_KNOTS((2,2),(3,3),(0.,0.289681084359922),(0.331965345783649,
0.349369696259361),.UNSPECIFIED.)
GEOMETRIC_REPRESENTATION_ITEM()
RATIONAL_B_SPLINE_SURFACE(((0.988555124858681,0.99035748704491,0.99513694090229),
(0.988555124858682,0.99035748704491,0.99513694090229)))
REPRESENTATION_ITEM('')
SURFACE()
);
#233=(
BOUNDED_SURFACE()
B_SPLINE_SURFACE(1,2,((#96497,#96498,#96499,#96500,#96501),(#96502,#96503,
#96504,#96505,#96506),(#96507,#96508,#96509,#96510,#96511)),
 .UNSPECIFIED.,.F.,.F.,.F.)
B_SPLINE_SURFACE_WITH_KNOTS((2,1,2),(3,2,3),(-0.00289807040991647,0.,0.290399554018306),
(0.383340713913812,0.383933227114987,0.401145492974693),.UNSPECIFIED.)
GEOMETRIC_REPRESENTATION_ITEM()
RATIONAL_B_SPLINE_SURFACE(((0.988246641953811,0.988246641953811,0.988246641953811,
0.986737013496293,0.988139125479962),(0.988246641953811,0.988246641953811,
0.988246641953811,0.986737013496293,0.988139125479962),(0.988246641953811,
0.988246641953811,0.988246641953811,0.986737013496293,0.988139125479962)))
REPRESENTATION_ITEM('')
SURFACE()
);
#234=(
BOUNDED_SURFACE()
B_SPLINE_SURFACE(1,2,((#96536,#96537,#96538),(#96539,#96540,#96541)),
 .UNSPECIFIED.,.F.,.F.,.F.)
B_SPLINE_SURFACE_WITH_KNOTS((2,2),(3,3),(0.,0.289681084359919),(0.331965345783649,
0.349369696259361),.UNSPECIFIED.)
GEOMETRIC_REPRESENTATION_ITEM()
RATIONAL_B_SPLINE_SURFACE(((0.988555124858681,0.99035748704491,0.99513694090229),
(0.988555124858681,0.99035748704491,0.99513694090229)))
REPRESENTATION_ITEM('')
SURFACE()
);
#235=(
BOUNDED_SURFACE()
B_SPLINE_SURFACE(1,2,((#96545,#96546,#96547,#96548,#96549),(#96550,#96551,
#96552,#96553,#96554),(#96555,#96556,#96557,#96558,#96559)),
 .UNSPECIFIED.,.F.,.F.,.F.)
B_SPLINE_SURFACE_WITH_KNOTS((2,1,2),(3,2,3),(-0.00289807040991561,0.,0.29039955400762),
(0.383340713924413,0.383933227114987,0.401145492974693),.UNSPECIFIED.)
GEOMETRIC_REPRESENTATION_ITEM()
RATIONAL_B_SPLINE_SURFACE(((0.988246641953811,0.988246641953811,0.988246641953811,
0.986737013496293,0.988139125479961),(0.988246641953811,0.988246641953811,
0.988246641953811,0.986737013496293,0.988139125479961),(0.988246641953811,
0.988246641953811,0.988246641953811,0.986737013496293,0.988139125479961)))
REPRESENTATION_ITEM('')
SURFACE()
);
#236=(
BOUNDED_SURFACE()
B_SPLINE_SURFACE(1,2,((#96584,#96585,#96586),(#96587,#96588,#96589)),
 .UNSPECIFIED.,.F.,.F.,.F.)
B_SPLINE_SURFACE_WITH_KNOTS((2,2),(3,3),(0.,0.289681084359919),(0.331965345783649,
0.349369696259361),.UNSPECIFIED.)
GEOMETRIC_REPRESENTATION_ITEM()
RATIONAL_B_SPLINE_SURFACE(((0.988555124858682,0.99035748704491,0.99513694090229),
(0.988555124858682,0.99035748704491,0.99513694090229)))
REPRESENTATION_ITEM('')
SURFACE()
);
#237=(
BOUNDED_SURFACE()
B_SPLINE_SURFACE(1,2,((#96593,#96594,#96595,#96596,#96597),(#96598,#96599,
#96600,#96601,#96602),(#96603,#96604,#96605,#96606,#96607)),
 .UNSPECIFIED.,.F.,.F.,.F.)
B_SPLINE_SURFACE_WITH_KNOTS((2,1,2),(3,2,3),(-0.00289807040991639,0.,0.290399554026997),
(0.383340713905114,0.383933227114987,0.401145492974693),.UNSPECIFIED.)
GEOMETRIC_REPRESENTATION_ITEM()
RATIONAL_B_SPLINE_SURFACE(((0.988246641953811,0.988246641953811,0.988246641953811,
0.986737013496293,0.988139125479962),(0.988246641953811,0.988246641953811,
0.988246641953811,0.986737013496293,0.988139125479962),(0.988246641953811,
0.988246641953811,0.988246641953811,0.986737013496293,0.988139125479962)))
REPRESENTATION_ITEM('')
SURFACE()
);
#238=(
BOUNDED_SURFACE()
B_SPLINE_SURFACE(1,2,((#96632,#96633,#96634),(#96635,#96636,#96637)),
 .UNSPECIFIED.,.F.,.F.,.F.)
B_SPLINE_SURFACE_WITH_KNOTS((2,2),(3,3),(0.,0.28968108435992),(0.331965345783649,
0.349369696259361),.UNSPECIFIED.)
GEOMETRIC_REPRESENTATION_ITEM()
RATIONAL_B_SPLINE_SURFACE(((0.988555124858682,0.99035748704491,0.99513694090229),
(0.988555124858682,0.99035748704491,0.99513694090229)))
REPRESENTATION_ITEM('')
SURFACE()
);
#239=(
BOUNDED_SURFACE()
B_SPLINE_SURFACE(1,2,((#96641,#96642,#96643,#96644,#96645),(#96646,#96647,
#96648,#96649,#96650),(#96651,#96652,#96653,#96654,#96655)),
 .UNSPECIFIED.,.F.,.F.,.F.)
B_SPLINE_SURFACE_WITH_KNOTS((2,1,2),(3,2,3),(-0.00289807040991643,0.,0.290399554033924),
(0.383340713898191,0.383933227114987,0.401145492974693),.UNSPECIFIED.)
GEOMETRIC_REPRESENTATION_ITEM()
RATIONAL_B_SPLINE_SURFACE(((0.988246641953811,0.988246641953811,0.988246641953811,
0.986737013496293,0.988139125479961),(0.988246641953811,0.988246641953811,
0.988246641953811,0.986737013496293,0.988139125479961),(0.988246641953811,
0.988246641953811,0.988246641953811,0.986737013496293,0.988139125479961)))
REPRESENTATION_ITEM('')
SURFACE()
);
#240=(
BOUNDED_SURFACE()
B_SPLINE_SURFACE(1,2,((#96680,#96681,#96682),(#96683,#96684,#96685)),
 .UNSPECIFIED.,.F.,.F.,.F.)
B_SPLINE_SURFACE_WITH_KNOTS((2,2),(3,3),(0.,0.289681084359918),(0.331965345783649,
0.349369696259361),.UNSPECIFIED.)
GEOMETRIC_REPRESENTATION_ITEM()
RATIONAL_B_SPLINE_SURFACE(((0.988555124858681,0.99035748704491,0.99513694090229),
(0.988555124858681,0.99035748704491,0.99513694090229)))
REPRESENTATION_ITEM('')
SURFACE()
);
#241=(
BOUNDED_SURFACE()
B_SPLINE_SURFACE(1,2,((#96689,#96690,#96691,#96692,#96693),(#96694,#96695,
#96696,#96697,#96698),(#96699,#96700,#96701,#96702,#96703)),
 .UNSPECIFIED.,.F.,.F.,.F.)
B_SPLINE_SURFACE_WITH_KNOTS((2,1,2),(3,2,3),(-0.00289807040991642,0.,0.290399554026227),
(0.383340713905887,0.383933227114987,0.401145492974693),.UNSPECIFIED.)
GEOMETRIC_REPRESENTATION_ITEM()
RATIONAL_B_SPLINE_SURFACE(((0.988246641953811,0.988246641953811,0.988246641953811,
0.986737013496293,0.988139125479962),(0.988246641953811,0.988246641953811,
0.988246641953811,0.986737013496293,0.988139125479962),(0.988246641953811,
0.988246641953811,0.988246641953811,0.986737013496293,0.988139125479961)))
REPRESENTATION_ITEM('')
SURFACE()
);
#242=(
BOUNDED_SURFACE()
B_SPLINE_SURFACE(1,2,((#96728,#96729,#96730),(#96731,#96732,#96733)),
 .UNSPECIFIED.,.F.,.F.,.F.)
B_SPLINE_SURFACE_WITH_KNOTS((2,2),(3,3),(0.,0.289681084359924),(0.331965345783649,
0.349369696259361),.UNSPECIFIED.)
GEOMETRIC_REPRESENTATION_ITEM()
RATIONAL_B_SPLINE_SURFACE(((0.988555124858681,0.99035748704491,0.99513694090229),
(0.988555124858681,0.99035748704491,0.99513694090229)))
REPRESENTATION_ITEM('')
SURFACE()
);
#243=(
BOUNDED_SURFACE()
B_SPLINE_SURFACE(1,2,((#96737,#96738,#96739,#96740,#96741),(#96742,#96743,
#96744,#96745,#96746),(#96747,#96748,#96749,#96750,#96751)),
 .UNSPECIFIED.,.F.,.F.,.F.)
B_SPLINE_SURFACE_WITH_KNOTS((2,1,2),(3,2,3),(-0.00289807040991638,0.,0.290399554027218),
(0.383340713904892,0.383933227114987,0.401145492974692),.UNSPECIFIED.)
GEOMETRIC_REPRESENTATION_ITEM()
RATIONAL_B_SPLINE_SURFACE(((0.988246641953811,0.988246641953811,0.988246641953811,
0.986737013496293,0.988139125479961),(0.988246641953811,0.988246641953811,
0.988246641953811,0.986737013496293,0.988139125479961),(0.988246641953811,
0.988246641953811,0.988246641953811,0.986737013496293,0.988139125479961)))
REPRESENTATION_ITEM('')
SURFACE()
);
#244=(
BOUNDED_SURFACE()
B_SPLINE_SURFACE(1,2,((#96764,#96765,#96766),(#96767,#96768,#96769)),
 .UNSPECIFIED.,.F.,.F.,.F.)
B_SPLINE_SURFACE_WITH_KNOTS((2,2),(3,3),(0.,0.289681084359914),(0.33196534578365,
0.349369696259362),.UNSPECIFIED.)
GEOMETRIC_REPRESENTATION_ITEM()
RATIONAL_B_SPLINE_SURFACE(((0.988555124858682,0.990357487044911,0.99513694090229),
(0.988555124858682,0.990357487044911,0.99513694090229)))
REPRESENTATION_ITEM('')
SURFACE()
);
#245=(
BOUNDED_SURFACE()
B_SPLINE_SURFACE(1,2,((#96785,#96786,#96787,#96788,#96789),(#96790,#96791,
#96792,#96793,#96794),(#96795,#96796,#96797,#96798,#96799)),
 .UNSPECIFIED.,.F.,.F.,.F.)
B_SPLINE_SURFACE_WITH_KNOTS((2,1,2),(3,2,3),(-0.00289807040991564,0.,0.290399554037147),
(0.383340713894887,0.383933227114985,0.401145492974692),.UNSPECIFIED.)
GEOMETRIC_REPRESENTATION_ITEM()
RATIONAL_B_SPLINE_SURFACE(((0.988246641953811,0.988246641953811,0.988246641953811,
0.986737013496293,0.988139125479961),(0.988246641953811,0.988246641953811,
0.988246641953811,0.986737013496293,0.988139125479961),(0.988246641953811,
0.988246641953811,0.988246641953811,0.986737013496293,0.988139125479961)))
REPRESENTATION_ITEM('')
SURFACE()
);
#246=(
BOUNDED_SURFACE()
B_SPLINE_SURFACE(1,2,((#96824,#96825,#96826),(#96827,#96828,#96829)),
 .UNSPECIFIED.,.F.,.F.,.F.)
B_SPLINE_SURFACE_WITH_KNOTS((2,2),(3,3),(0.,0.289681084359935),(0.33196534578365,
0.349369696259361),.UNSPECIFIED.)
GEOMETRIC_REPRESENTATION_ITEM()
RATIONAL_B_SPLINE_SURFACE(((0.988555124858682,0.990357487044911,0.99513694090229),
(0.988555124858682,0.990357487044911,0.99513694090229)))
REPRESENTATION_ITEM('')
SURFACE()
);
#247=(
BOUNDED_SURFACE()
B_SPLINE_SURFACE(1,2,((#96833,#96834,#96835,#96836,#96837),(#96838,#96839,
#96840,#96841,#96842),(#96843,#96844,#96845,#96846,#96847)),
 .UNSPECIFIED.,.F.,.F.,.F.)
B_SPLINE_SURFACE_WITH_KNOTS((2,1,2),(3,2,3),(-0.00289807040991981,0.,0.29039955402774),
(0.383340713904713,0.383933227114987,0.401145492974693),.UNSPECIFIED.)
GEOMETRIC_REPRESENTATION_ITEM()
RATIONAL_B_SPLINE_SURFACE(((0.988246641953811,0.988246641953811,0.988246641953811,
0.986737013496293,0.988139125479962),(0.988246641953811,0.988246641953811,
0.988246641953811,0.986737013496293,0.988139125479962),(0.988246641953811,
0.988246641953811,0.988246641953811,0.986737013496293,0.988139125479962)))
REPRESENTATION_ITEM('')
SURFACE()
);
#248=(
BOUNDED_SURFACE()
B_SPLINE_SURFACE(1,2,((#96872,#96873,#96874),(#96875,#96876,#96877)),
 .UNSPECIFIED.,.F.,.F.,.F.)
B_SPLINE_SURFACE_WITH_KNOTS((2,2),(3,3),(0.,0.289681084359928),(0.331965345783649,
0.349369696259361),.UNSPECIFIED.)
GEOMETRIC_REPRESENTATION_ITEM()
RATIONAL_B_SPLINE_SURFACE(((0.988555124858681,0.99035748704491,0.99513694090229),
(0.988555124858681,0.99035748704491,0.99513694090229)))
REPRESENTATION_ITEM('')
SURFACE()
);
#249=(
BOUNDED_SURFACE()
B_SPLINE_SURFACE(1,2,((#96881,#96882,#96883,#96884,#96885),(#96886,#96887,
#96888,#96889,#96890),(#96891,#96892,#96893,#96894,#96895)),
 .UNSPECIFIED.,.F.,.F.,.F.)
B_SPLINE_SURFACE_WITH_KNOTS((2,1,2),(3,2,3),(-0.00289807040991899,0.,0.290399554020957),
(0.383340713911414,0.383933227114987,0.401145492974693),.UNSPECIFIED.)
GEOMETRIC_REPRESENTATION_ITEM()
RATIONAL_B_SPLINE_SURFACE(((0.988246641953811,0.988246641953811,0.988246641953811,
0.986737013496293,0.988139125479962),(0.988246641953811,0.988246641953811,
0.988246641953811,0.986737013496293,0.988139125479962),(0.988246641953811,
0.988246641953811,0.988246641953811,0.986737013496293,0.988139125479962)))
REPRESENTATION_ITEM('')
SURFACE()
);
#250=(
BOUNDED_SURFACE()
B_SPLINE_SURFACE(1,2,((#96920,#96921,#96922),(#96923,#96924,#96925)),
 .UNSPECIFIED.,.F.,.F.,.F.)
B_SPLINE_SURFACE_WITH_KNOTS((2,2),(3,3),(0.,0.289681084359927),(0.331965345783649,
0.349369696259361),.UNSPECIFIED.)
GEOMETRIC_REPRESENTATION_ITEM()
RATIONAL_B_SPLINE_SURFACE(((0.988555124858681,0.99035748704491,0.99513694090229),
(0.988555124858681,0.99035748704491,0.99513694090229)))
REPRESENTATION_ITEM('')
SURFACE()
);
#251=(
BOUNDED_SURFACE()
B_SPLINE_SURFACE(1,2,((#96941,#96942,#96943,#96944,#96945),(#96946,#96947,
#96948,#96949,#96950),(#96951,#96952,#96953,#96954,#96955)),
 .UNSPECIFIED.,.F.,.F.,.F.)
B_SPLINE_SURFACE_WITH_KNOTS((2,1,2),(3,2,3),(-0.0028980704099201,0.,0.290399554036522),
(0.383340713895899,0.383933227114987,0.401145492974693),.UNSPECIFIED.)
GEOMETRIC_REPRESENTATION_ITEM()
RATIONAL_B_SPLINE_SURFACE(((0.988246641953811,0.988246641953811,0.988246641953811,
0.986737013496293,0.988139125479962),(0.988246641953811,0.988246641953811,
0.988246641953811,0.986737013496293,0.988139125479962),(0.988246641953811,
0.988246641953811,0.988246641953811,0.986737013496293,0.988139125479962)))
REPRESENTATION_ITEM('')
SURFACE()
);
#252=(
BOUNDED_SURFACE()
B_SPLINE_SURFACE(1,2,((#96958,#96959,#96960,#96961,#96962),(#96963,#96964,
#96965,#96966,#96967)),.UNSPECIFIED.,.F.,.F.,.F.)
B_SPLINE_SURFACE_WITH_KNOTS((2,2),(3,2,3),(0.709593954894314,1.),(0.331470144829386,
0.332069149066804,0.349473499542517),.UNSPECIFIED.)
GEOMETRIC_REPRESENTATION_ITEM()
RATIONAL_B_SPLINE_SURFACE(((0.988576730109495,0.988576730109495,0.988576730109495,
0.990396848309667,0.99519405818099),(0.988576730109495,0.988576730109495,
0.988576730109495,0.990396848309667,0.99519405818099)))
REPRESENTATION_ITEM('')
SURFACE()
);
#253=(
BOUNDED_SURFACE()
B_SPLINE_SURFACE(1,2,((#96978,#96979,#96980),(#96981,#96982,#96983),(#96984,
#96985,#96986)),.UNSPECIFIED.,.F.,.F.,.F.)
B_SPLINE_SURFACE_WITH_KNOTS((2,1,2),(3,3),(0.707422104796139,0.710318915639742,
1.),(0.383830569465724,0.401042835325431),.UNSPECIFIED.)
GEOMETRIC_REPRESENTATION_ITEM()
RATIONAL_B_SPLINE_SURFACE(((0.988264753026337,0.986737758323643,0.988122504062136),
(0.988264753026337,0.986737758323643,0.988122504062136),(0.988264753026337,
0.986737758323643,0.988122504062136)))
REPRESENTATION_ITEM('')
SURFACE()
);
#254=(
BOUNDED_SURFACE()
B_SPLINE_SURFACE(1,2,((#96997,#96998,#96999,#97000,#97001),(#97002,#97003,
#97004,#97005,#97006)),.UNSPECIFIED.,.F.,.F.,.F.)
B_SPLINE_SURFACE_WITH_KNOTS((2,2),(3,2,3),(0.709593954927603,1.),(0.331470144862805,
0.332069149066804,0.349473499542517),.UNSPECIFIED.)
GEOMETRIC_REPRESENTATION_ITEM()
RATIONAL_B_SPLINE_SURFACE(((0.988576730109495,0.988576730109495,0.988576730109495,
0.990396848309667,0.99519405818099),(0.988576730109495,0.988576730109495,
0.988576730109495,0.990396848309667,0.99519405818099)))
REPRESENTATION_ITEM('')
SURFACE()
);
#255=(
BOUNDED_SURFACE()
B_SPLINE_SURFACE(1,2,((#97014,#97015,#97016),(#97017,#97018,#97019),(#97020,
#97021,#97022)),.UNSPECIFIED.,.F.,.F.,.F.)
B_SPLINE_SURFACE_WITH_KNOTS((2,1,2),(3,3),(0.707422104796059,0.710318915639662,
1.),(0.383830569465724,0.401042835325431),.UNSPECIFIED.)
GEOMETRIC_REPRESENTATION_ITEM()
RATIONAL_B_SPLINE_SURFACE(((0.988264753026337,0.986737758323643,0.988122504062136),
(0.988264753026337,0.986737758323643,0.988122504062136),(0.988264753026337,
0.986737758323643,0.988122504062136)))
REPRESENTATION_ITEM('')
SURFACE()
);
#256=(
BOUNDED_SURFACE()
B_SPLINE_SURFACE(1,2,((#97033,#97034,#97035,#97036,#97037),(#97038,#97039,
#97040,#97041,#97042)),.UNSPECIFIED.,.F.,.F.,.F.)
B_SPLINE_SURFACE_WITH_KNOTS((2,2),(3,2,3),(0.70959395491761,1.),(0.33147014485254,
0.332069149066805,0.349473499542517),.UNSPECIFIED.)
GEOMETRIC_REPRESENTATION_ITEM()
RATIONAL_B_SPLINE_SURFACE(((0.988576730109495,0.988576730109495,0.988576730109495,
0.990396848309667,0.99519405818099),(0.988576730109495,0.988576730109495,
0.988576730109495,0.990396848309667,0.99519405818099)))
REPRESENTATION_ITEM('')
SURFACE()
);
#257=(
BOUNDED_SURFACE()
B_SPLINE_SURFACE(1,2,((#97050,#97051,#97052),(#97053,#97054,#97055),(#97056,
#97057,#97058)),.UNSPECIFIED.,.F.,.F.,.F.)
B_SPLINE_SURFACE_WITH_KNOTS((2,1,2),(3,3),(0.707422104796478,0.710318915640077,
1.),(0.383830569465723,0.40104283532543),.UNSPECIFIED.)
GEOMETRIC_REPRESENTATION_ITEM()
RATIONAL_B_SPLINE_SURFACE(((0.988264753026337,0.986737758323643,0.988122504062136),
(0.988264753026337,0.986737758323643,0.988122504062136),(0.988264753026337,
0.986737758323643,0.988122504062136)))
REPRESENTATION_ITEM('')
SURFACE()
);
#258=(
BOUNDED_SURFACE()
B_SPLINE_SURFACE(1,2,((#97069,#97070,#97071,#97072,#97073),(#97074,#97075,
#97076,#97077,#97078)),.UNSPECIFIED.,.F.,.F.,.F.)
B_SPLINE_SURFACE_WITH_KNOTS((2,2),(3,2,3),(0.709593954926867,1.),(0.331470144853475,
0.332069149066805,0.349473499542518),.UNSPECIFIED.)
GEOMETRIC_REPRESENTATION_ITEM()
RATIONAL_B_SPLINE_SURFACE(((0.988576730109495,0.988576730109495,0.988576730109495,
0.990396848309667,0.995194058180991),(0.988576730109495,0.988576730109495,
0.988576730109495,0.990396848309667,0.995194058180991)))
REPRESENTATION_ITEM('')
SURFACE()
);
#259=(
BOUNDED_SURFACE()
B_SPLINE_SURFACE(1,2,((#97086,#97087,#97088),(#97089,#97090,#97091),(#97092,
#97093,#97094)),.UNSPECIFIED.,.F.,.F.,.F.)
B_SPLINE_SURFACE_WITH_KNOTS((2,1,2),(3,3),(0.707422104796401,0.710318915640001,
1.),(0.383830569465724,0.40104283532543),.UNSPECIFIED.)
GEOMETRIC_REPRESENTATION_ITEM()
RATIONAL_B_SPLINE_SURFACE(((0.988264753026337,0.986737758323643,0.988122504062135),
(0.988264753026337,0.986737758323643,0.988122504062135),(0.988264753026337,
0.986737758323643,0.988122504062135)))
REPRESENTATION_ITEM('')
SURFACE()
);
#260=(
BOUNDED_SURFACE()
B_SPLINE_SURFACE(1,2,((#97105,#97106,#97107,#97108,#97109),(#97110,#97111,
#97112,#97113,#97114)),.UNSPECIFIED.,.F.,.F.,.F.)
B_SPLINE_SURFACE_WITH_KNOTS((2,2),(3,2,3),(0.709593954920529,1.),(0.331470144847347,
0.332069149066804,0.349473499542517),.UNSPECIFIED.)
GEOMETRIC_REPRESENTATION_ITEM()
RATIONAL_B_SPLINE_SURFACE(((0.988576730109495,0.988576730109495,0.988576730109495,
0.990396848309667,0.99519405818099),(0.988576730109495,0.988576730109495,
0.988576730109495,0.990396848309667,0.99519405818099)))
REPRESENTATION_ITEM('')
SURFACE()
);
#261=(
BOUNDED_SURFACE()
B_SPLINE_SURFACE(1,2,((#97122,#97123,#97124),(#97125,#97126,#97127),(#97128,
#97129,#97130)),.UNSPECIFIED.,.F.,.F.,.F.)
B_SPLINE_SURFACE_WITH_KNOTS((2,1,2),(3,3),(0.707422104796399,0.710318915639999,
1.),(0.383830569465724,0.401042835325431),.UNSPECIFIED.)
GEOMETRIC_REPRESENTATION_ITEM()
RATIONAL_B_SPLINE_SURFACE(((0.988264753026337,0.986737758323643,0.988122504062135),
(0.988264753026337,0.986737758323643,0.988122504062135),(0.988264753026337,
0.986737758323643,0.988122504062135)))
REPRESENTATION_ITEM('')
SURFACE()
);
#262=(
BOUNDED_SURFACE()
B_SPLINE_SURFACE(1,2,((#97141,#97142,#97143,#97144,#97145),(#97146,#97147,
#97148,#97149,#97150)),.UNSPECIFIED.,.F.,.F.,.F.)
B_SPLINE_SURFACE_WITH_KNOTS((2,2),(3,2,3),(0.709593954913145,1.),(0.331470144839669,
0.332069149066804,0.349473499542517),.UNSPECIFIED.)
GEOMETRIC_REPRESENTATION_ITEM()
RATIONAL_B_SPLINE_SURFACE(((0.988576730109495,0.988576730109495,0.988576730109495,
0.990396848309667,0.99519405818099),(0.988576730109495,0.988576730109495,
0.988576730109495,0.990396848309667,0.99519405818099)))
REPRESENTATION_ITEM('')
SURFACE()
);
#263=(
BOUNDED_SURFACE()
B_SPLINE_SURFACE(1,2,((#97158,#97159,#97160),(#97161,#97162,#97163),(#97164,
#97165,#97166)),.UNSPECIFIED.,.F.,.F.,.F.)
B_SPLINE_SURFACE_WITH_KNOTS((2,1,2),(3,3),(0.707422104796394,0.710318915639994,
1.),(0.383830569465724,0.401042835325431),.UNSPECIFIED.)
GEOMETRIC_REPRESENTATION_ITEM()
RATIONAL_B_SPLINE_SURFACE(((0.988264753026337,0.986737758323643,0.988122504062135),
(0.988264753026337,0.986737758323643,0.988122504062135),(0.988264753026337,
0.986737758323643,0.988122504062135)))
REPRESENTATION_ITEM('')
SURFACE()
);
#264=(
BOUNDED_SURFACE()
B_SPLINE_SURFACE(1,2,((#97177,#97178,#97179,#97180,#97181),(#97182,#97183,
#97184,#97185,#97186)),.UNSPECIFIED.,.F.,.F.,.F.)
B_SPLINE_SURFACE_WITH_KNOTS((2,2),(3,2,3),(0.709593954887389,1.),(0.331470144814559,
0.332069149066804,0.349473499542517),.UNSPECIFIED.)
GEOMETRIC_REPRESENTATION_ITEM()
RATIONAL_B_SPLINE_SURFACE(((0.988576730109495,0.988576730109495,0.988576730109495,
0.990396848309667,0.99519405818099),(0.988576730109495,0.988576730109495,
0.988576730109495,0.990396848309667,0.99519405818099)))
REPRESENTATION_ITEM('')
SURFACE()
);
#265=(
BOUNDED_SURFACE()
B_SPLINE_SURFACE(1,2,((#97194,#97195,#97196),(#97197,#97198,#97199),(#97200,
#97201,#97202)),.UNSPECIFIED.,.F.,.F.,.F.)
B_SPLINE_SURFACE_WITH_KNOTS((2,1,2),(3,3),(0.7074221047964,0.71031891564,
1.),(0.383830569465724,0.401042835325431),.UNSPECIFIED.)
GEOMETRIC_REPRESENTATION_ITEM()
RATIONAL_B_SPLINE_SURFACE(((0.988264753026337,0.986737758323643,0.988122504062136),
(0.988264753026337,0.986737758323643,0.988122504062136),(0.988264753026337,
0.986737758323643,0.988122504062136)))
REPRESENTATION_ITEM('')
SURFACE()
);
#266=(
BOUNDED_SURFACE()
B_SPLINE_SURFACE(1,2,((#97213,#97214,#97215,#97216,#97217),(#97218,#97219,
#97220,#97221,#97222)),.UNSPECIFIED.,.F.,.F.,.F.)
B_SPLINE_SURFACE_WITH_KNOTS((2,2),(3,2,3),(0.709593954900147,1.),(0.331470144834562,
0.332069149066804,0.349473499542517),.UNSPECIFIED.)
GEOMETRIC_REPRESENTATION_ITEM()
RATIONAL_B_SPLINE_SURFACE(((0.988576730109495,0.988576730109495,0.988576730109495,
0.990396848309667,0.99519405818099),(0.988576730109495,0.988576730109495,
0.988576730109495,0.990396848309667,0.99519405818099)))
REPRESENTATION_ITEM('')
SURFACE()
);
#267=(
BOUNDED_SURFACE()
B_SPLINE_SURFACE(1,2,((#97230,#97231,#97232),(#97233,#97234,#97235),(#97236,
#97237,#97238)),.UNSPECIFIED.,.F.,.F.,.F.)
B_SPLINE_SURFACE_WITH_KNOTS((2,1,2),(3,3),(0.70742210479648,0.710318915640079,
1.),(0.383830569465724,0.401042835325431),.UNSPECIFIED.)
GEOMETRIC_REPRESENTATION_ITEM()
RATIONAL_B_SPLINE_SURFACE(((0.988264753026337,0.986737758323643,0.988122504062135),
(0.988264753026337,0.986737758323643,0.988122504062135),(0.988264753026337,
0.986737758323643,0.988122504062135)))
REPRESENTATION_ITEM('')
SURFACE()
);
#268=(
BOUNDED_SURFACE()
B_SPLINE_SURFACE(1,2,((#97249,#97250,#97251,#97252,#97253),(#97254,#97255,
#97256,#97257,#97258)),.UNSPECIFIED.,.F.,.F.,.F.)
B_SPLINE_SURFACE_WITH_KNOTS((2,2),(3,2,3),(0.709593954911915,1.),(0.331470144846543,
0.332069149066804,0.349473499542517),.UNSPECIFIED.)
GEOMETRIC_REPRESENTATION_ITEM()
RATIONAL_B_SPLINE_SURFACE(((0.988576730109495,0.988576730109495,0.988576730109495,
0.990396848309667,0.99519405818099),(0.988576730109495,0.988576730109495,
0.988576730109495,0.990396848309667,0.99519405818099)))
REPRESENTATION_ITEM('')
SURFACE()
);
#269=(
BOUNDED_SURFACE()
B_SPLINE_SURFACE(1,2,((#97266,#97267,#97268),(#97269,#97270,#97271),(#97272,
#97273,#97274)),.UNSPECIFIED.,.F.,.F.,.F.)
B_SPLINE_SURFACE_WITH_KNOTS((2,1,2),(3,3),(0.707422104796394,0.710318915639994,
1.),(0.383830569465724,0.401042835325431),.UNSPECIFIED.)
GEOMETRIC_REPRESENTATION_ITEM()
RATIONAL_B_SPLINE_SURFACE(((0.988264753026337,0.986737758323643,0.988122504062135),
(0.988264753026337,0.986737758323643,0.988122504062135),(0.988264753026337,
0.986737758323643,0.988122504062135)))
REPRESENTATION_ITEM('')
SURFACE()
);
#270=(
BOUNDED_SURFACE()
B_SPLINE_SURFACE(1,2,((#97285,#97286,#97287,#97288,#97289),(#97290,#97291,
#97292,#97293,#97294)),.UNSPECIFIED.,.F.,.F.,.F.)
B_SPLINE_SURFACE_WITH_KNOTS((2,2),(3,2,3),(0.709593954893798,1.),(0.331470144828196,
0.332069149066804,0.349473499542517),.UNSPECIFIED.)
GEOMETRIC_REPRESENTATION_ITEM()
RATIONAL_B_SPLINE_SURFACE(((0.988576730109495,0.988576730109495,0.988576730109495,
0.990396848309667,0.99519405818099),(0.988576730109495,0.988576730109495,
0.988576730109495,0.990396848309667,0.99519405818099)))
REPRESENTATION_ITEM('')
SURFACE()
);
#271=(
BOUNDED_SURFACE()
B_SPLINE_SURFACE(1,2,((#97302,#97303,#97304),(#97305,#97306,#97307),(#97308,
#97309,#97310)),.UNSPECIFIED.,.F.,.F.,.F.)
B_SPLINE_SURFACE_WITH_KNOTS((2,1,2),(3,3),(0.707422104796478,0.710318915640077,
1.),(0.383830569465724,0.401042835325431),.UNSPECIFIED.)
GEOMETRIC_REPRESENTATION_ITEM()
RATIONAL_B_SPLINE_SURFACE(((0.988264753026337,0.986737758323643,0.988122504062136),
(0.988264753026337,0.986737758323643,0.988122504062136),(0.988264753026337,
0.986737758323643,0.988122504062136)))
REPRESENTATION_ITEM('')
SURFACE()
);
#272=(
BOUNDED_SURFACE()
B_SPLINE_SURFACE(1,2,((#97321,#97322,#97323,#97324,#97325),(#97326,#97327,
#97328,#97329,#97330)),.UNSPECIFIED.,.F.,.F.,.F.)
B_SPLINE_SURFACE_WITH_KNOTS((2,2),(3,2,3),(0.709593954913158,1.),(0.331470144847742,
0.332069149066804,0.349473499542517),.UNSPECIFIED.)
GEOMETRIC_REPRESENTATION_ITEM()
RATIONAL_B_SPLINE_SURFACE(((0.988576730109495,0.988576730109495,0.988576730109495,
0.990396848309667,0.99519405818099),(0.988576730109495,0.988576730109495,
0.988576730109495,0.990396848309667,0.99519405818099)))
REPRESENTATION_ITEM('')
SURFACE()
);
#273=(
BOUNDED_SURFACE()
B_SPLINE_SURFACE(1,2,((#97338,#97339,#97340),(#97341,#97342,#97343),(#97344,
#97345,#97346)),.UNSPECIFIED.,.F.,.F.,.F.)
B_SPLINE_SURFACE_WITH_KNOTS((2,1,2),(3,3),(0.707422104796117,0.71031891563972,
1.),(0.383830569465724,0.401042835325431),.UNSPECIFIED.)
GEOMETRIC_REPRESENTATION_ITEM()
RATIONAL_B_SPLINE_SURFACE(((0.988264753026337,0.986737758323643,0.988122504062136),
(0.988264753026337,0.986737758323643,0.988122504062136),(0.988264753026337,
0.986737758323643,0.988122504062136)))
REPRESENTATION_ITEM('')
SURFACE()
);
#274=(
BOUNDED_SURFACE()
B_SPLINE_SURFACE(1,2,((#97357,#97358,#97359,#97360,#97361),(#97362,#97363,
#97364,#97365,#97366)),.UNSPECIFIED.,.F.,.F.,.F.)
B_SPLINE_SURFACE_WITH_KNOTS((2,2),(3,2,3),(0.709593954916007,1.),(0.331470144842851,
0.332069149066804,0.349473499542517),.UNSPECIFIED.)
GEOMETRIC_REPRESENTATION_ITEM()
RATIONAL_B_SPLINE_SURFACE(((0.988576730109495,0.988576730109495,0.988576730109495,
0.990396848309667,0.99519405818099),(0.988576730109495,0.988576730109495,
0.988576730109495,0.990396848309667,0.99519405818099)))
REPRESENTATION_ITEM('')
SURFACE()
);
#275=(
BOUNDED_SURFACE()
B_SPLINE_SURFACE(1,2,((#97374,#97375,#97376),(#97377,#97378,#97379),(#97380,
#97381,#97382)),.UNSPECIFIED.,.F.,.F.,.F.)
B_SPLINE_SURFACE_WITH_KNOTS((2,1,2),(3,3),(0.707422104795055,0.710318915638668,
1.),(0.383830569465724,0.401042835325431),.UNSPECIFIED.)
GEOMETRIC_REPRESENTATION_ITEM()
RATIONAL_B_SPLINE_SURFACE(((0.988264753026337,0.986737758323643,0.988122504062136),
(0.988264753026337,0.986737758323643,0.988122504062136),(0.988264753026337,
0.986737758323643,0.988122504062136)))
REPRESENTATION_ITEM('')
SURFACE()
);
#276=(
BOUNDED_SURFACE()
B_SPLINE_SURFACE(1,2,((#97393,#97394,#97395,#97396,#97397),(#97398,#97399,
#97400,#97401,#97402)),.UNSPECIFIED.,.F.,.F.,.F.)
B_SPLINE_SURFACE_WITH_KNOTS((2,2),(3,2,3),(0.709593954907459,1.),(0.331470144835858,
0.332069149066804,0.349473499542517),.UNSPECIFIED.)
GEOMETRIC_REPRESENTATION_ITEM()
RATIONAL_B_SPLINE_SURFACE(((0.988576730109495,0.988576730109495,0.988576730109495,
0.990396848309667,0.99519405818099),(0.988576730109495,0.988576730109495,
0.988576730109495,0.990396848309667,0.99519405818099)))
REPRESENTATION_ITEM('')
SURFACE()
);
#277=(
BOUNDED_SURFACE()
B_SPLINE_SURFACE(1,2,((#97410,#97411,#97412),(#97413,#97414,#97415),(#97416,
#97417,#97418)),.UNSPECIFIED.,.F.,.F.,.F.)
B_SPLINE_SURFACE_WITH_KNOTS((2,1,2),(3,3),(0.707422104796353,0.710318915639953,
1.),(0.383830569465724,0.401042835325431),.UNSPECIFIED.)
GEOMETRIC_REPRESENTATION_ITEM()
RATIONAL_B_SPLINE_SURFACE(((0.988264753026337,0.986737758323643,0.988122504062136),
(0.988264753026337,0.986737758323643,0.988122504062136),(0.988264753026337,
0.986737758323643,0.988122504062136)))
REPRESENTATION_ITEM('')
SURFACE()
);
#278=(
BOUNDED_SURFACE()
B_SPLINE_SURFACE(1,2,((#97429,#97430,#97431,#97432,#97433),(#97434,#97435,
#97436,#97437,#97438)),.UNSPECIFIED.,.F.,.F.,.F.)
B_SPLINE_SURFACE_WITH_KNOTS((2,2),(3,2,3),(0.709593954923838,1.),(0.331470144850567,
0.332069149066804,0.349473499542517),.UNSPECIFIED.)
GEOMETRIC_REPRESENTATION_ITEM()
RATIONAL_B_SPLINE_SURFACE(((0.988576730109495,0.988576730109495,0.988576730109495,
0.990396848309667,0.99519405818099),(0.988576730109495,0.988576730109495,
0.988576730109495,0.990396848309667,0.99519405818099)))
REPRESENTATION_ITEM('')
SURFACE()
);
#279=(
BOUNDED_SURFACE()
B_SPLINE_SURFACE(1,2,((#97446,#97447,#97448),(#97449,#97450,#97451),(#97452,
#97453,#97454)),.UNSPECIFIED.,.F.,.F.,.F.)
B_SPLINE_SURFACE_WITH_KNOTS((2,1,2),(3,3),(0.707422104796472,0.710318915640071,
1.),(0.383830569465724,0.401042835325431),.UNSPECIFIED.)
GEOMETRIC_REPRESENTATION_ITEM()
RATIONAL_B_SPLINE_SURFACE(((0.988264753026337,0.986737758323643,0.988122504062136),
(0.988264753026337,0.986737758323643,0.988122504062136),(0.988264753026337,
0.986737758323643,0.988122504062136)))
REPRESENTATION_ITEM('')
SURFACE()
);
#280=(
BOUNDED_SURFACE()
B_SPLINE_SURFACE(1,2,((#97462,#97463,#97464,#97465,#97466),(#97467,#97468,
#97469,#97470,#97471)),.UNSPECIFIED.,.F.,.F.,.F.)
B_SPLINE_SURFACE_WITH_KNOTS((2,2),(3,2,3),(0.709961110188848,1.),(0.331837300123762,
0.332069149066804,0.349473499542517),.UNSPECIFIED.)
GEOMETRIC_REPRESENTATION_ITEM()
RATIONAL_B_SPLINE_SURFACE(((0.988576730109495,0.988576730109495,0.988576730109495,
0.990396848309667,0.99519405818099),(0.988576730109495,0.988576730109495,
0.988576730109495,0.990396848309667,0.99519405818099)))
REPRESENTATION_ITEM('')
SURFACE()
);
#281=(
BOUNDED_SURFACE()
B_SPLINE_SURFACE(1,2,((#97473,#97474,#97475),(#97476,#97477,#97478),(#97479,
#97480,#97481)),.UNSPECIFIED.,.F.,.F.,.F.)
B_SPLINE_SURFACE_WITH_KNOTS((2,1,2),(3,3),(0.707422104796241,0.710318915639843,
1.),(0.383830569465724,0.401042835325431),.UNSPECIFIED.)
GEOMETRIC_REPRESENTATION_ITEM()
RATIONAL_B_SPLINE_SURFACE(((0.988264753026337,0.986737758323643,0.988122504062135),
(0.988264753026337,0.986737758323643,0.988122504062135),(0.988264753026337,
0.986737758323643,0.988122504062135)))
REPRESENTATION_ITEM('')
SURFACE()
);
#282=(
BOUNDED_SURFACE()
B_SPLINE_SURFACE(1,2,((#97492,#97493,#97494,#97495,#97496),(#97497,#97498,
#97499,#97500,#97501)),.UNSPECIFIED.,.F.,.F.,.F.)
B_SPLINE_SURFACE_WITH_KNOTS((2,2),(3,2,3),(0.70959395489228,1.),(0.331470144827466,
0.332069149066804,0.349473499542517),.UNSPECIFIED.)
GEOMETRIC_REPRESENTATION_ITEM()
RATIONAL_B_SPLINE_SURFACE(((0.988576730109495,0.988576730109495,0.988576730109495,
0.990396848309667,0.99519405818099),(0.988576730109495,0.988576730109495,
0.988576730109495,0.990396848309667,0.99519405818099)))
REPRESENTATION_ITEM('')
SURFACE()
);
#283=(
BOUNDED_SURFACE()
B_SPLINE_SURFACE(1,2,((#97509,#97510,#97511),(#97512,#97513,#97514),(#97515,
#97516,#97517)),.UNSPECIFIED.,.F.,.F.,.F.)
B_SPLINE_SURFACE_WITH_KNOTS((2,1,2),(3,3),(0.707422104796478,0.710318915640077,
1.),(0.383830569465724,0.401042835325431),.UNSPECIFIED.)
GEOMETRIC_REPRESENTATION_ITEM()
RATIONAL_B_SPLINE_SURFACE(((0.988264753026337,0.986737758323643,0.988122504062136),
(0.988264753026337,0.986737758323643,0.988122504062136),(0.988264753026337,
0.986737758323643,0.988122504062136)))
REPRESENTATION_ITEM('')
SURFACE()
);
#284=(
BOUNDED_SURFACE()
B_SPLINE_SURFACE(1,2,((#97528,#97529,#97530,#97531,#97532),(#97533,#97534,
#97535,#97536,#97537)),.UNSPECIFIED.,.F.,.F.,.F.)
B_SPLINE_SURFACE_WITH_KNOTS((2,2),(3,2,3),(0.709593954915317,1.),(0.33147014485014,
0.332069149066804,0.349473499542517),.UNSPECIFIED.)
GEOMETRIC_REPRESENTATION_ITEM()
RATIONAL_B_SPLINE_SURFACE(((0.988576730109495,0.988576730109495,0.988576730109495,
0.990396848309667,0.99519405818099),(0.988576730109495,0.988576730109495,
0.988576730109495,0.990396848309667,0.99519405818099)))
REPRESENTATION_ITEM('')
SURFACE()
);
#285=(
BOUNDED_SURFACE()
B_SPLINE_SURFACE(1,2,((#97545,#97546,#97547),(#97548,#97549,#97550),(#97551,
#97552,#97553)),.UNSPECIFIED.,.F.,.F.,.F.)
B_SPLINE_SURFACE_WITH_KNOTS((2,1,2),(3,3),(0.707422104796476,0.710318915640075,
1.),(0.383830569465724,0.401042835325431),.UNSPECIFIED.)
GEOMETRIC_REPRESENTATION_ITEM()
RATIONAL_B_SPLINE_SURFACE(((0.988264753026337,0.986737758323643,0.988122504062135),
(0.988264753026337,0.986737758323643,0.988122504062135),(0.988264753026337,
0.986737758323643,0.988122504062135)))
REPRESENTATION_ITEM('')
SURFACE()
);
#286=(
BOUNDED_SURFACE()
B_SPLINE_SURFACE(1,2,((#97564,#97565,#97566,#97567,#97568),(#97569,#97570,
#97571,#97572,#97573)),.UNSPECIFIED.,.F.,.F.,.F.)
B_SPLINE_SURFACE_WITH_KNOTS((2,2),(3,2,3),(0.70959395491621,1.),(0.331470144850383,
0.332069149066804,0.349473499542517),.UNSPECIFIED.)
GEOMETRIC_REPRESENTATION_ITEM()
RATIONAL_B_SPLINE_SURFACE(((0.988576730109495,0.988576730109495,0.988576730109495,
0.990396848309667,0.99519405818099),(0.988576730109495,0.988576730109495,
0.988576730109495,0.990396848309667,0.99519405818099)))
REPRESENTATION_ITEM('')
SURFACE()
);
#287=(
BOUNDED_SURFACE()
B_SPLINE_SURFACE(1,2,((#97581,#97582,#97583),(#97584,#97585,#97586),(#97587,
#97588,#97589)),.UNSPECIFIED.,.F.,.F.,.F.)
B_SPLINE_SURFACE_WITH_KNOTS((2,1,2),(3,3),(0.707422104796473,0.710318915640072,
1.),(0.383830569465724,0.401042835325431),.UNSPECIFIED.)
GEOMETRIC_REPRESENTATION_ITEM()
RATIONAL_B_SPLINE_SURFACE(((0.988264753026337,0.986737758323643,0.988122504062135),
(0.988264753026337,0.986737758323643,0.988122504062135),(0.988264753026337,
0.986737758323643,0.988122504062135)))
REPRESENTATION_ITEM('')
SURFACE()
);
#288=(
BOUNDED_SURFACE()
B_SPLINE_SURFACE(1,2,((#97600,#97601,#97602,#97603,#97604),(#97605,#97606,
#97607,#97608,#97609)),.UNSPECIFIED.,.F.,.F.,.F.)
B_SPLINE_SURFACE_WITH_KNOTS((2,2),(3,2,3),(0.709593954915993,1.),(0.331470144842909,
0.332069149066804,0.349473499542517),.UNSPECIFIED.)
GEOMETRIC_REPRESENTATION_ITEM()
RATIONAL_B_SPLINE_SURFACE(((0.988576730109495,0.988576730109495,0.988576730109495,
0.990396848309667,0.99519405818099),(0.988576730109495,0.988576730109495,
0.988576730109495,0.990396848309667,0.99519405818099)))
REPRESENTATION_ITEM('')
SURFACE()
);
#289=(
BOUNDED_SURFACE()
B_SPLINE_SURFACE(1,2,((#97617,#97618,#97619),(#97620,#97621,#97622),(#97623,
#97624,#97625)),.UNSPECIFIED.,.F.,.F.,.F.)
B_SPLINE_SURFACE_WITH_KNOTS((2,1,2),(3,3),(0.707422104796323,0.710318915639924,
1.),(0.383830569465724,0.401042835325431),.UNSPECIFIED.)
GEOMETRIC_REPRESENTATION_ITEM()
RATIONAL_B_SPLINE_SURFACE(((0.988264753026337,0.986737758323643,0.988122504062136),
(0.988264753026337,0.986737758323643,0.988122504062136),(0.988264753026337,
0.986737758323643,0.988122504062136)))
REPRESENTATION_ITEM('')
SURFACE()
);
#290=(
BOUNDED_SURFACE()
B_SPLINE_SURFACE(1,2,((#97636,#97637,#97638,#97639,#97640),(#97641,#97642,
#97643,#97644,#97645)),.UNSPECIFIED.,.F.,.F.,.F.)
B_SPLINE_SURFACE_WITH_KNOTS((2,2),(3,2,3),(0.7095939549075,1.),(0.331470144834758,
0.332069149066804,0.349473499542517),.UNSPECIFIED.)
GEOMETRIC_REPRESENTATION_ITEM()
RATIONAL_B_SPLINE_SURFACE(((0.988576730109495,0.988576730109495,0.988576730109495,
0.990396848309667,0.99519405818099),(0.988576730109495,0.988576730109495,
0.988576730109495,0.990396848309667,0.99519405818099)))
REPRESENTATION_ITEM('')
SURFACE()
);
#291=(
BOUNDED_SURFACE()
B_SPLINE_SURFACE(1,2,((#97653,#97654,#97655),(#97656,#97657,#97658),(#97659,
#97660,#97661)),.UNSPECIFIED.,.F.,.F.,.F.)
B_SPLINE_SURFACE_WITH_KNOTS((2,1,2),(3,3),(0.707422104796278,0.710318915639879,
1.),(0.383830569465724,0.401042835325431),.UNSPECIFIED.)
GEOMETRIC_REPRESENTATION_ITEM()
RATIONAL_B_SPLINE_SURFACE(((0.988264753026337,0.986737758323643,0.988122504062136),
(0.988264753026337,0.986737758323643,0.988122504062136),(0.988264753026337,
0.986737758323643,0.988122504062136)))
REPRESENTATION_ITEM('')
SURFACE()
);
#292=(
BOUNDED_SURFACE()
B_SPLINE_SURFACE(1,2,((#97672,#97673,#97674,#97675,#97676),(#97677,#97678,
#97679,#97680,#97681)),.UNSPECIFIED.,.F.,.F.,.F.)
B_SPLINE_SURFACE_WITH_KNOTS((2,2),(3,2,3),(0.709593954908083,1.),(0.331470144835444,
0.332069149066804,0.349473499542517),.UNSPECIFIED.)
GEOMETRIC_REPRESENTATION_ITEM()
RATIONAL_B_SPLINE_SURFACE(((0.988576730109495,0.988576730109495,0.988576730109495,
0.990396848309667,0.99519405818099),(0.988576730109495,0.988576730109495,
0.988576730109495,0.990396848309667,0.99519405818099)))
REPRESENTATION_ITEM('')
SURFACE()
);
#293=(
BOUNDED_SURFACE()
B_SPLINE_SURFACE(1,2,((#97689,#97690,#97691),(#97692,#97693,#97694),(#97695,
#97696,#97697)),.UNSPECIFIED.,.F.,.F.,.F.)
B_SPLINE_SURFACE_WITH_KNOTS((2,1,2),(3,3),(0.707422104795113,0.710318915638726,
1.),(0.383830569465724,0.401042835325439),.UNSPECIFIED.)
GEOMETRIC_REPRESENTATION_ITEM()
RATIONAL_B_SPLINE_SURFACE(((0.988264753026337,0.986737758323642,0.988122504062137),
(0.988264753026337,0.986737758323642,0.988122504062137),(0.988264753026337,
0.986737758323642,0.988122504062137)))
REPRESENTATION_ITEM('')
SURFACE()
);
#294=(
BOUNDED_SURFACE()
B_SPLINE_SURFACE(1,2,((#97708,#97709,#97710,#97711,#97712),(#97713,#97714,
#97715,#97716,#97717)),.UNSPECIFIED.,.F.,.F.,.F.)
B_SPLINE_SURFACE_WITH_KNOTS((2,2),(3,2,3),(0.709593954917731,1.),(0.331470144846068,
0.332069149066804,0.349473499542517),.UNSPECIFIED.)
GEOMETRIC_REPRESENTATION_ITEM()
RATIONAL_B_SPLINE_SURFACE(((0.988576730109495,0.988576730109495,0.988576730109495,
0.990396848309667,0.99519405818099),(0.988576730109495,0.988576730109495,
0.988576730109495,0.990396848309667,0.99519405818099)))
REPRESENTATION_ITEM('')
SURFACE()
);
#295=(
BOUNDED_SURFACE()
B_SPLINE_SURFACE(1,2,((#97725,#97726,#97727),(#97728,#97729,#97730),(#97731,
#97732,#97733)),.UNSPECIFIED.,.F.,.F.,.F.)
B_SPLINE_SURFACE_WITH_KNOTS((2,1,2),(3,3),(0.707422104795338,0.710318915638948,
1.),(0.383830569465724,0.401042835325431),.UNSPECIFIED.)
GEOMETRIC_REPRESENTATION_ITEM()
RATIONAL_B_SPLINE_SURFACE(((0.988264753026337,0.986737758323643,0.988122504062136),
(0.988264753026337,0.986737758323643,0.988122504062136),(0.988264753026337,
0.986737758323643,0.988122504062136)))
REPRESENTATION_ITEM('')
SURFACE()
);
#296=(
BOUNDED_SURFACE()
B_SPLINE_SURFACE(1,2,((#97744,#97745,#97746,#97747,#97748),(#97749,#97750,
#97751,#97752,#97753)),.UNSPECIFIED.,.F.,.F.,.F.)
B_SPLINE_SURFACE_WITH_KNOTS((2,2),(3,2,3),(0.709593954917719,1.),(0.331470144853412,
0.332069149066804,0.349473499542517),.UNSPECIFIED.)
GEOMETRIC_REPRESENTATION_ITEM()
RATIONAL_B_SPLINE_SURFACE(((0.988576730109495,0.988576730109495,0.988576730109495,
0.990396848309667,0.99519405818099),(0.988576730109495,0.988576730109495,
0.988576730109495,0.990396848309667,0.99519405818099)))
REPRESENTATION_ITEM('')
SURFACE()
);
#297=(
BOUNDED_SURFACE()
B_SPLINE_SURFACE(1,2,((#97761,#97762,#97763),(#97764,#97765,#97766),(#97767,
#97768,#97769)),.UNSPECIFIED.,.F.,.F.,.F.)
B_SPLINE_SURFACE_WITH_KNOTS((2,1,2),(3,3),(0.707422104795584,0.710318915639192,
1.),(0.383830569465714,0.401042835325431),.UNSPECIFIED.)
GEOMETRIC_REPRESENTATION_ITEM()
RATIONAL_B_SPLINE_SURFACE(((0.988264753026339,0.986737758323642,0.988122504062136),
(0.988264753026339,0.986737758323642,0.988122504062136),(0.988264753026339,
0.986737758323642,0.988122504062136)))
REPRESENTATION_ITEM('')
SURFACE()
);
#298=(
BOUNDED_SURFACE()
B_SPLINE_SURFACE(1,2,((#97780,#97781,#97782,#97783,#97784),(#97785,#97786,
#97787,#97788,#97789)),.UNSPECIFIED.,.F.,.F.,.F.)
B_SPLINE_SURFACE_WITH_KNOTS((2,2),(3,2,3),(0.709593954893256,1.),(0.331470144829105,
0.332069149066804,0.349473499542517),.UNSPECIFIED.)
GEOMETRIC_REPRESENTATION_ITEM()
RATIONAL_B_SPLINE_SURFACE(((0.988576730109495,0.988576730109495,0.988576730109495,
0.990396848309667,0.99519405818099),(0.988576730109495,0.988576730109495,
0.988576730109495,0.990396848309667,0.99519405818099)))
REPRESENTATION_ITEM('')
SURFACE()
);
#299=(
BOUNDED_SURFACE()
B_SPLINE_SURFACE(1,2,((#97797,#97798,#97799),(#97800,#97801,#97802),(#97803,
#97804,#97805)),.UNSPECIFIED.,.F.,.F.,.F.)
B_SPLINE_SURFACE_WITH_KNOTS((2,1,2),(3,3),(0.707422104795713,0.71031891563932,
1.),(0.383830569465724,0.401042835325432),.UNSPECIFIED.)
GEOMETRIC_REPRESENTATION_ITEM()
RATIONAL_B_SPLINE_SURFACE(((0.988264753026337,0.986737758323643,0.988122504062136),
(0.988264753026337,0.986737758323643,0.988122504062136),(0.988264753026337,
0.986737758323643,0.988122504062136)))
REPRESENTATION_ITEM('')
SURFACE()
);
#300=(
BOUNDED_SURFACE()
B_SPLINE_SURFACE(1,2,((#97816,#97817,#97818,#97819,#97820),(#97821,#97822,
#97823,#97824,#97825)),.UNSPECIFIED.,.F.,.F.,.F.)
B_SPLINE_SURFACE_WITH_KNOTS((2,2),(3,2,3),(0.709593954897723,1.),(0.331470144833009,
0.332069149066804,0.349473499542517),.UNSPECIFIED.)
GEOMETRIC_REPRESENTATION_ITEM()
RATIONAL_B_SPLINE_SURFACE(((0.988576730109495,0.988576730109495,0.988576730109495,
0.990396848309667,0.99519405818099),(0.988576730109495,0.988576730109495,
0.988576730109495,0.990396848309667,0.99519405818099)))
REPRESENTATION_ITEM('')
SURFACE()
);
#301=(
BOUNDED_SURFACE()
B_SPLINE_SURFACE(1,2,((#97833,#97834,#97835),(#97836,#97837,#97838),(#97839,
#97840,#97841)),.UNSPECIFIED.,.F.,.F.,.F.)
B_SPLINE_SURFACE_WITH_KNOTS((2,1,2),(3,3),(0.707422104795225,0.710318915638837,
1.),(0.383830569465724,0.401042835325431),.UNSPECIFIED.)
GEOMETRIC_REPRESENTATION_ITEM()
RATIONAL_B_SPLINE_SURFACE(((0.988264753026337,0.986737758323643,0.988122504062136),
(0.988264753026337,0.986737758323643,0.988122504062136),(0.988264753026337,
0.986737758323643,0.988122504062136)))
REPRESENTATION_ITEM('')
SURFACE()
);
#302=(
BOUNDED_SURFACE()
B_SPLINE_SURFACE(1,2,((#97852,#97853,#97854,#97855,#97856),(#97857,#97858,
#97859,#97860,#97861)),.UNSPECIFIED.,.F.,.F.,.F.)
B_SPLINE_SURFACE_WITH_KNOTS((2,2),(3,2,3),(0.709593954907626,1.),(0.331470144835888,
0.332069149066804,0.349473499542517),.UNSPECIFIED.)
GEOMETRIC_REPRESENTATION_ITEM()
RATIONAL_B_SPLINE_SURFACE(((0.988576730109495,0.988576730109495,0.988576730109495,
0.990396848309667,0.99519405818099),(0.988576730109495,0.988576730109495,
0.988576730109495,0.990396848309667,0.99519405818099)))
REPRESENTATION_ITEM('')
SURFACE()
);
#303=(
BOUNDED_SURFACE()
B_SPLINE_SURFACE(1,2,((#97869,#97870,#97871),(#97872,#97873,#97874),(#97875,
#97876,#97877)),.UNSPECIFIED.,.F.,.F.,.F.)
B_SPLINE_SURFACE_WITH_KNOTS((2,1,2),(3,3),(0.707422104795377,0.710318915638987,
1.),(0.383830569465724,0.401042835325434),.UNSPECIFIED.)
GEOMETRIC_REPRESENTATION_ITEM()
RATIONAL_B_SPLINE_SURFACE(((0.988264753026337,0.986737758323643,0.988122504062136),
(0.988264753026337,0.986737758323643,0.988122504062136),(0.988264753026337,
0.986737758323643,0.988122504062136)))
REPRESENTATION_ITEM('')
SURFACE()
);
#304=(
BOUNDED_SURFACE()
B_SPLINE_SURFACE(1,2,((#97888,#97889,#97890,#97891,#97892),(#97893,#97894,
#97895,#97896,#97897)),.UNSPECIFIED.,.F.,.F.,.F.)
B_SPLINE_SURFACE_WITH_KNOTS((2,2),(3,2,3),(0.709593954929305,1.),(0.331470144857018,
0.332069149066804,0.349473499542517),.UNSPECIFIED.)
GEOMETRIC_REPRESENTATION_ITEM()
RATIONAL_B_SPLINE_SURFACE(((0.988576730109495,0.988576730109495,0.988576730109495,
0.990396848309667,0.99519405818099),(0.988576730109495,0.988576730109495,
0.988576730109495,0.990396848309667,0.99519405818099)))
REPRESENTATION_ITEM('')
SURFACE()
);
#305=(
BOUNDED_SURFACE()
B_SPLINE_SURFACE(1,2,((#97905,#97906,#97907),(#97908,#97909,#97910),(#97911,
#97912,#97913)),.UNSPECIFIED.,.F.,.F.,.F.)
B_SPLINE_SURFACE_WITH_KNOTS((2,1,2),(3,3),(0.707422104795348,0.710318915638958,
1.),(0.383830569465724,0.401042835325432),.UNSPECIFIED.)
GEOMETRIC_REPRESENTATION_ITEM()
RATIONAL_B_SPLINE_SURFACE(((0.988264753026337,0.986737758323643,0.988122504062136),
(0.988264753026337,0.986737758323643,0.988122504062136),(0.988264753026337,
0.986737758323643,0.988122504062136)))
REPRESENTATION_ITEM('')
SURFACE()
);
#306=(
BOUNDED_SURFACE()
B_SPLINE_SURFACE(1,2,((#97924,#97925,#97926,#97927,#97928),(#97929,#97930,
#97931,#97932,#97933)),.UNSPECIFIED.,.F.,.F.,.F.)
B_SPLINE_SURFACE_WITH_KNOTS((2,2),(3,2,3),(0.709593954903671,1.),(0.331470144831592,
0.332069149066804,0.349473499542517),.UNSPECIFIED.)
GEOMETRIC_REPRESENTATION_ITEM()
RATIONAL_B_SPLINE_SURFACE(((0.988576730109495,0.988576730109495,0.988576730109495,
0.990396848309667,0.99519405818099),(0.988576730109495,0.988576730109495,
0.988576730109495,0.990396848309667,0.99519405818099)))
REPRESENTATION_ITEM('')
SURFACE()
);
#307=(
BOUNDED_SURFACE()
B_SPLINE_SURFACE(1,2,((#97941,#97942,#97943),(#97944,#97945,#97946),(#97947,
#97948,#97949)),.UNSPECIFIED.,.F.,.F.,.F.)
B_SPLINE_SURFACE_WITH_KNOTS((2,1,2),(3,3),(0.707422104795167,0.710318915638779,
1.),(0.383830569465724,0.401042835325431),.UNSPECIFIED.)
GEOMETRIC_REPRESENTATION_ITEM()
RATIONAL_B_SPLINE_SURFACE(((0.988264753026337,0.986737758323643,0.988122504062136),
(0.988264753026337,0.986737758323643,0.988122504062136),(0.988264753026337,
0.986737758323643,0.988122504062136)))
REPRESENTATION_ITEM('')
SURFACE()
);
#308=(
BOUNDED_SURFACE()
B_SPLINE_SURFACE(1,2,((#97960,#97961,#97962,#97963,#97964),(#97965,#97966,
#97967,#97968,#97969)),.UNSPECIFIED.,.F.,.F.,.F.)
B_SPLINE_SURFACE_WITH_KNOTS((2,2),(3,2,3),(0.709593954891873,1.),(0.33147014482002,
0.332069149066804,0.349473499542517),.UNSPECIFIED.)
GEOMETRIC_REPRESENTATION_ITEM()
RATIONAL_B_SPLINE_SURFACE(((0.988576730109495,0.988576730109495,0.988576730109495,
0.990396848309667,0.99519405818099),(0.988576730109495,0.988576730109495,
0.988576730109495,0.990396848309667,0.99519405818099)))
REPRESENTATION_ITEM('')
SURFACE()
);
#309=(
BOUNDED_SURFACE()
B_SPLINE_SURFACE(1,2,((#97983,#97984,#97985),(#97986,#97987,#97988),(#97989,
#97990,#97991)),.UNSPECIFIED.,.F.,.F.,.F.)
B_SPLINE_SURFACE_WITH_KNOTS((2,1,2),(3,3),(0.707422104796028,0.710318915639632,
1.),(0.383830569465724,0.401042835325431),.UNSPECIFIED.)
GEOMETRIC_REPRESENTATION_ITEM()
RATIONAL_B_SPLINE_SURFACE(((0.988264753026337,0.986737758323643,0.988122504062135),
(0.988264753026337,0.986737758323643,0.988122504062135),(0.988264753026337,
0.986737758323643,0.988122504062135)))
REPRESENTATION_ITEM('')
SURFACE()
);
#310=(
BOUNDED_SURFACE()
B_SPLINE_SURFACE(1,2,((#97993,#97994,#97995),(#97996,#97997,#97998)),
 .UNSPECIFIED.,.F.,.F.,.F.)
B_SPLINE_SURFACE_WITH_KNOTS((2,2),(3,3),(0.710318915639632,1.),(0.366717817351065,
0.383933227114987),.UNSPECIFIED.)
GEOMETRIC_REPRESENTATION_ITEM()
RATIONAL_B_SPLINE_SURFACE(((0.994179254576316,0.989756546152321,0.988246641953811),
(0.994179254576316,0.989756546152321,0.988246641953811)))
REPRESENTATION_ITEM('')
SURFACE()
);
#311=(
BOUNDED_SURFACE()
B_SPLINE_SURFACE(1,2,((#98007,#98008,#98009,#98010,#98011,#98012,#98013),
(#98014,#98015,#98016,#98017,#98018,#98019,#98020)),.UNSPECIFIED.,.F.,.F.,
 .F.)
B_SPLINE_SURFACE_WITH_KNOTS((2,2),(3,2,2,3),(0.710192959007138,1.),(0.349194141236593,
0.349369696259361,0.357142857142857,0.366925198536205),.UNSPECIFIED.)
GEOMETRIC_REPRESENTATION_ITEM()
RATIONAL_B_SPLINE_SURFACE(((0.99513694090229,0.99513694090229,0.99513694090229,
0.997271548787858,1.,0.99656630788526,0.994073123128689),(0.99513694090229,
0.99513694090229,0.99513694090229,0.997271548787858,1.,0.99656630788526,
0.994073123128689)))
REPRESENTATION_ITEM('')
SURFACE()
);
#312=(
BOUNDED_SURFACE()
B_SPLINE_SURFACE(1,2,((#98033,#98034,#98035),(#98036,#98037,#98038)),
 .UNSPECIFIED.,.F.,.F.,.F.)
B_SPLINE_SURFACE_WITH_KNOTS((2,2),(3,3),(0.710318915638778,1.),(0.366717817351071,
0.383933227114987),.UNSPECIFIED.)
GEOMETRIC_REPRESENTATION_ITEM()
RATIONAL_B_SPLINE_SURFACE(((0.994179254576313,0.989756546152321,0.988246641953811),
(0.994179254576313,0.989756546152321,0.988246641953811)))
REPRESENTATION_ITEM('')
SURFACE()
);
#313=(
BOUNDED_SURFACE()
B_SPLINE_SURFACE(1,2,((#98040,#98041,#98042,#98043,#98044,#98045,#98046),
(#98047,#98048,#98049,#98050,#98051,#98052,#98053)),.UNSPECIFIED.,.F.,.F.,
 .F.)
B_SPLINE_SURFACE_WITH_KNOTS((2,2),(3,2,2,3),(0.710192959007322,1.),(0.349194141236593,
0.349369696259361,0.357142857142857,0.366925198536205),.UNSPECIFIED.)
GEOMETRIC_REPRESENTATION_ITEM()
RATIONAL_B_SPLINE_SURFACE(((0.99513694090229,0.99513694090229,0.99513694090229,
0.997271548787858,1.,0.99656630788526,0.99407312312869),(0.99513694090229,
0.99513694090229,0.99513694090229,0.997271548787858,1.,0.99656630788526,
0.99407312312869)))
REPRESENTATION_ITEM('')
SURFACE()
);
#314=(
BOUNDED_SURFACE()
B_SPLINE_SURFACE(1,2,((#98066,#98067,#98068),(#98069,#98070,#98071)),
 .UNSPECIFIED.,.F.,.F.,.F.)
B_SPLINE_SURFACE_WITH_KNOTS((2,2),(3,3),(0.710318915638965,1.),(0.366717817351071,
0.383933227115084),.UNSPECIFIED.)
GEOMETRIC_REPRESENTATION_ITEM()
RATIONAL_B_SPLINE_SURFACE(((0.994179254576314,0.989756546152296,0.988246641953794),
(0.994179254576314,0.989756546152296,0.988246641953794)))
REPRESENTATION_ITEM('')
SURFACE()
);
#315=(
BOUNDED_SURFACE()
B_SPLINE_SURFACE(1,2,((#98073,#98074,#98075,#98076,#98077,#98078,#98079),
(#98080,#98081,#98082,#98083,#98084,#98085,#98086)),.UNSPECIFIED.,.F.,.F.,
 .F.)
B_SPLINE_SURFACE_WITH_KNOTS((2,2),(3,2,2,3),(0.710192959007349,1.),(0.349194141236593,
0.349369696259361,0.357142857142857,0.366925198536205),.UNSPECIFIED.)
GEOMETRIC_REPRESENTATION_ITEM()
RATIONAL_B_SPLINE_SURFACE(((0.99513694090229,0.99513694090229,0.99513694090229,
0.997271548787858,1.,0.99656630788526,0.994073123128689),(0.99513694090229,
0.99513694090229,0.99513694090229,0.997271548787858,1.,0.99656630788526,
0.994073123128689)))
REPRESENTATION_ITEM('')
SURFACE()
);
#316=(
BOUNDED_SURFACE()
B_SPLINE_SURFACE(1,2,((#98099,#98100,#98101),(#98102,#98103,#98104)),
 .UNSPECIFIED.,.F.,.F.,.F.)
B_SPLINE_SURFACE_WITH_KNOTS((2,2),(3,3),(0.710318915638993,1.),(0.366717817351071,
0.383933227114987),.UNSPECIFIED.)
GEOMETRIC_REPRESENTATION_ITEM()
RATIONAL_B_SPLINE_SURFACE(((0.994179254576313,0.989756546152321,0.988246641953811),
(0.994179254576313,0.989756546152321,0.988246641953811)))
REPRESENTATION_ITEM('')
SURFACE()
);
#317=(
BOUNDED_SURFACE()
B_SPLINE_SURFACE(1,2,((#98106,#98107,#98108,#98109,#98110,#98111,#98112),
(#98113,#98114,#98115,#98116,#98117,#98118,#98119)),.UNSPECIFIED.,.F.,.F.,
 .F.)
B_SPLINE_SURFACE_WITH_KNOTS((2,2),(3,2,2,3),(0.710192959007199,1.),(0.349194141236593,
0.349369696259361,0.357142857142857,0.366925198536205),.UNSPECIFIED.)
GEOMETRIC_REPRESENTATION_ITEM()
RATIONAL_B_SPLINE_SURFACE(((0.99513694090229,0.99513694090229,0.99513694090229,
0.997271548787858,1.,0.99656630788526,0.994073123128689),(0.99513694090229,
0.99513694090229,0.99513694090229,0.997271548787858,1.,0.99656630788526,
0.994073123128689)))
REPRESENTATION_ITEM('')
SURFACE()
);
#318=(
BOUNDED_SURFACE()
B_SPLINE_SURFACE(1,2,((#98132,#98133,#98134),(#98135,#98136,#98137)),
 .UNSPECIFIED.,.F.,.F.,.F.)
B_SPLINE_SURFACE_WITH_KNOTS((2,2),(3,3),(0.710318915638838,1.),(0.366717817351071,
0.383933227114987),.UNSPECIFIED.)
GEOMETRIC_REPRESENTATION_ITEM()
RATIONAL_B_SPLINE_SURFACE(((0.994179254576313,0.98975654615232,0.988246641953811),
(0.994179254576313,0.989756546152321,0.988246641953811)))
REPRESENTATION_ITEM('')
SURFACE()
);
#319=(
BOUNDED_SURFACE()
B_SPLINE_SURFACE(1,2,((#98139,#98140,#98141,#98142,#98143,#98144,#98145),
(#98146,#98147,#98148,#98149,#98150,#98151,#98152)),.UNSPECIFIED.,.F.,.F.,
 .F.)
B_SPLINE_SURFACE_WITH_KNOTS((2,2),(3,2,2,3),(0.710192959007675,1.),(0.349194141236593,
0.349369696259361,0.357142857142857,0.366925198536205),.UNSPECIFIED.)
GEOMETRIC_REPRESENTATION_ITEM()
RATIONAL_B_SPLINE_SURFACE(((0.99513694090229,0.99513694090229,0.99513694090229,
0.997271548787858,1.,0.99656630788526,0.99407312312869),(0.99513694090229,
0.99513694090229,0.99513694090229,0.997271548787858,1.,0.99656630788526,
0.99407312312869)))
REPRESENTATION_ITEM('')
SURFACE()
);
#320=(
BOUNDED_SURFACE()
B_SPLINE_SURFACE(1,2,((#98165,#98166,#98167),(#98168,#98169,#98170)),
 .UNSPECIFIED.,.F.,.F.,.F.)
B_SPLINE_SURFACE_WITH_KNOTS((2,2),(3,3),(0.710318915639317,1.),(0.366717817351071,
0.383933227114987),.UNSPECIFIED.)
GEOMETRIC_REPRESENTATION_ITEM()
RATIONAL_B_SPLINE_SURFACE(((0.994179254576314,0.989756546152321,0.988246641953811),
(0.994179254576314,0.989756546152321,0.988246641953811)))
REPRESENTATION_ITEM('')
SURFACE()
);
#321=(
BOUNDED_SURFACE()
B_SPLINE_SURFACE(1,2,((#98172,#98173,#98174,#98175,#98176,#98177,#98178),
(#98179,#98180,#98181,#98182,#98183,#98184,#98185)),.UNSPECIFIED.,.F.,.F.,
 .F.)
B_SPLINE_SURFACE_WITH_KNOTS((2,2),(3,2,2,3),(0.71019295900755,1.),(0.349194141236582,
0.349369696259351,0.357142857142857,0.366925198536205),.UNSPECIFIED.)
GEOMETRIC_REPRESENTATION_ITEM()
RATIONAL_B_SPLINE_SURFACE(((0.995136940902284,0.995136940902284,0.995136940902284,
0.997271548787855,1.,0.99656630788526,0.99407312312869),(0.995136940902284,
0.995136940902284,0.995136940902284,0.997271548787855,1.,0.99656630788526,
0.99407312312869)))
REPRESENTATION_ITEM('')
SURFACE()
);
#322=(
BOUNDED_SURFACE()
B_SPLINE_SURFACE(1,2,((#98198,#98199,#98200),(#98201,#98202,#98203)),
 .UNSPECIFIED.,.F.,.F.,.F.)
B_SPLINE_SURFACE_WITH_KNOTS((2,2),(3,3),(0.710318915639189,1.),(0.366717817351071,
0.383933227114987),.UNSPECIFIED.)
GEOMETRIC_REPRESENTATION_ITEM()
RATIONAL_B_SPLINE_SURFACE(((0.994179254576313,0.98975654615232,0.988246641953811),
(0.994179254576313,0.989756546152321,0.988246641953811)))
REPRESENTATION_ITEM('')
SURFACE()
);
#323=(
BOUNDED_SURFACE()
B_SPLINE_SURFACE(1,2,((#98205,#98206,#98207,#98208,#98209,#98210,#98211),
(#98212,#98213,#98214,#98215,#98216,#98217,#98218)),.UNSPECIFIED.,.F.,.F.,
 .F.)
B_SPLINE_SURFACE_WITH_KNOTS((2,2),(3,2,2,3),(0.71019295900731,1.),(0.349194141236593,
0.349369696259361,0.357142857142857,0.366925198536205),.UNSPECIFIED.)
GEOMETRIC_REPRESENTATION_ITEM()
RATIONAL_B_SPLINE_SURFACE(((0.99513694090229,0.99513694090229,0.99513694090229,
0.997271548787858,1.,0.99656630788526,0.99407312312869),(0.99513694090229,
0.99513694090229,0.99513694090229,0.997271548787858,1.,0.99656630788526,
0.99407312312869)))
REPRESENTATION_ITEM('')
SURFACE()
);
#324=(
BOUNDED_SURFACE()
B_SPLINE_SURFACE(1,2,((#98231,#98232,#98233),(#98234,#98235,#98236)),
 .UNSPECIFIED.,.F.,.F.,.F.)
B_SPLINE_SURFACE_WITH_KNOTS((2,2),(3,3),(0.71031891563895,1.),(0.366717817351071,
0.383933227114987),.UNSPECIFIED.)
GEOMETRIC_REPRESENTATION_ITEM()
RATIONAL_B_SPLINE_SURFACE(((0.994179254576313,0.98975654615232,0.988246641953811),
(0.994179254576313,0.989756546152321,0.988246641953811)))
REPRESENTATION_ITEM('')
SURFACE()
);
#325=(
BOUNDED_SURFACE()
B_SPLINE_SURFACE(1,2,((#98238,#98239,#98240,#98241,#98242,#98243,#98244),
(#98245,#98246,#98247,#98248,#98249,#98250,#98251)),.UNSPECIFIED.,.F.,.F.,
 .F.)
B_SPLINE_SURFACE_WITH_KNOTS((2,2),(3,2,2,3),(0.710192959007093,1.),(0.349194141236593,
0.349369696259361,0.357142857142857,0.366925198536205),.UNSPECIFIED.)
GEOMETRIC_REPRESENTATION_ITEM()
RATIONAL_B_SPLINE_SURFACE(((0.99513694090229,0.99513694090229,0.99513694090229,
0.997271548787859,1.,0.99656630788526,0.994073123128689),(0.99513694090229,
0.99513694090229,0.99513694090229,0.997271548787859,1.,0.99656630788526,
0.994073123128689)))
REPRESENTATION_ITEM('')
SURFACE()
);
#326=(
BOUNDED_SURFACE()
B_SPLINE_SURFACE(1,2,((#98266,#98267,#98268),(#98269,#98270,#98271)),
 .UNSPECIFIED.,.F.,.F.,.F.)
B_SPLINE_SURFACE_WITH_KNOTS((2,2),(3,3),(0.710318915638735,1.),(0.366717817351071,
0.38393322711499),.UNSPECIFIED.)
GEOMETRIC_REPRESENTATION_ITEM()
RATIONAL_B_SPLINE_SURFACE(((0.994179254576314,0.98975654615232,0.988246641953811),
(0.994179254576314,0.98975654615232,0.988246641953811)))
REPRESENTATION_ITEM('')
SURFACE()
);
#327=(
BOUNDED_SURFACE()
B_SPLINE_SURFACE(1,2,((#98273,#98274,#98275,#98276,#98277,#98278,#98279),
(#98280,#98281,#98282,#98283,#98284,#98285,#98286)),.UNSPECIFIED.,.F.,.F.,
 .F.)
B_SPLINE_SURFACE_WITH_KNOTS((2,2),(3,2,2,3),(0.710192959008241,1.),(0.349194141236593,
0.349369696259361,0.357142857142857,0.366925198536205),.UNSPECIFIED.)
GEOMETRIC_REPRESENTATION_ITEM()
RATIONAL_B_SPLINE_SURFACE(((0.99513694090229,0.99513694090229,0.99513694090229,
0.997271548787858,1.,0.99656630788526,0.99407312312869),(0.99513694090229,
0.99513694090229,0.99513694090229,0.997271548787858,1.,0.99656630788526,
0.99407312312869)))
REPRESENTATION_ITEM('')
SURFACE()
);
#328=(
BOUNDED_SURFACE()
B_SPLINE_SURFACE(1,2,((#98299,#98300,#98301),(#98302,#98303,#98304)),
 .UNSPECIFIED.,.F.,.F.,.F.)
B_SPLINE_SURFACE_WITH_KNOTS((2,2),(3,3),(0.710318915639881,1.),(0.366717817351071,
0.383933227114987),.UNSPECIFIED.)
GEOMETRIC_REPRESENTATION_ITEM()
RATIONAL_B_SPLINE_SURFACE(((0.994179254576313,0.989756546152321,0.988246641953811),
(0.994179254576313,0.989756546152321,0.988246641953811)))
REPRESENTATION_ITEM('')
SURFACE()
);
#329=(
BOUNDED_SURFACE()
B_SPLINE_SURFACE(1,2,((#98306,#98307,#98308,#98309,#98310,#98311,#98312),
(#98313,#98314,#98315,#98316,#98317,#98318,#98319)),.UNSPECIFIED.,.F.,.F.,
 .F.)
B_SPLINE_SURFACE_WITH_KNOTS((2,2),(3,2,2,3),(0.710192959008286,1.),(0.349194141236593,
0.349369696259361,0.357142857142857,0.366925198536205),.UNSPECIFIED.)
GEOMETRIC_REPRESENTATION_ITEM()
RATIONAL_B_SPLINE_SURFACE(((0.99513694090229,0.99513694090229,0.99513694090229,
0.997271548787858,1.,0.99656630788526,0.994073123128689),(0.99513694090229,
0.99513694090229,0.99513694090229,0.997271548787858,1.,0.99656630788526,
0.994073123128689)))
REPRESENTATION_ITEM('')
SURFACE()
);
#330=(
BOUNDED_SURFACE()
B_SPLINE_SURFACE(1,2,((#98332,#98333,#98334),(#98335,#98336,#98337)),
 .UNSPECIFIED.,.F.,.F.,.F.)
B_SPLINE_SURFACE_WITH_KNOTS((2,2),(3,3),(0.710318915639926,1.),(0.366717817351071,
0.383933227114987),.UNSPECIFIED.)
GEOMETRIC_REPRESENTATION_ITEM()
RATIONAL_B_SPLINE_SURFACE(((0.994179254576313,0.989756546152321,0.988246641953811),
(0.994179254576313,0.989756546152321,0.988246641953811)))
REPRESENTATION_ITEM('')
SURFACE()
);
#331=(
BOUNDED_SURFACE()
B_SPLINE_SURFACE(1,2,((#98339,#98340,#98341,#98342,#98343,#98344,#98345),
(#98346,#98347,#98348,#98349,#98350,#98351,#98352)),.UNSPECIFIED.,.F.,.F.,
 .F.)
B_SPLINE_SURFACE_WITH_KNOTS((2,2),(3,2,2,3),(0.710192959008439,1.),(0.349194141236593,
0.349369696259361,0.357142857142857,0.366925198536205),.UNSPECIFIED.)
GEOMETRIC_REPRESENTATION_ITEM()
RATIONAL_B_SPLINE_SURFACE(((0.99513694090229,0.99513694090229,0.99513694090229,
0.997271548787858,1.,0.99656630788526,0.994073123128689),(0.99513694090229,
0.99513694090229,0.99513694090229,0.997271548787858,1.,0.99656630788526,
0.994073123128689)))
REPRESENTATION_ITEM('')
SURFACE()
);
#332=(
BOUNDED_SURFACE()
B_SPLINE_SURFACE(1,2,((#98365,#98366,#98367),(#98368,#98369,#98370)),
 .UNSPECIFIED.,.F.,.F.,.F.)
B_SPLINE_SURFACE_WITH_KNOTS((2,2),(3,3),(0.710318915640072,1.),(0.366717817351071,
0.383933227114987),.UNSPECIFIED.)
GEOMETRIC_REPRESENTATION_ITEM()
RATIONAL_B_SPLINE_SURFACE(((0.994179254576314,0.989756546152321,0.988246641953811),
(0.994179254576314,0.989756546152321,0.988246641953811)))
REPRESENTATION_ITEM('')
SURFACE()
);
#333=(
BOUNDED_SURFACE()
B_SPLINE_SURFACE(1,2,((#98372,#98373,#98374,#98375,#98376,#98377,#98378),
(#98379,#98380,#98381,#98382,#98383,#98384,#98385)),.UNSPECIFIED.,.F.,.F.,
 .F.)
B_SPLINE_SURFACE_WITH_KNOTS((2,2),(3,2,2,3),(0.710192959008445,1.),(0.349194141236593,
0.349369696259361,0.357142857142857,0.366925198536205),.UNSPECIFIED.)
GEOMETRIC_REPRESENTATION_ITEM()
RATIONAL_B_SPLINE_SURFACE(((0.99513694090229,0.99513694090229,0.99513694090229,
0.997271548787858,1.,0.99656630788526,0.99407312312869),(0.99513694090229,
0.99513694090229,0.99513694090229,0.997271548787858,1.,0.99656630788526,
0.99407312312869)))
REPRESENTATION_ITEM('')
SURFACE()
);
#334=(
BOUNDED_SURFACE()
B_SPLINE_SURFACE(1,2,((#98398,#98399,#98400),(#98401,#98402,#98403)),
 .UNSPECIFIED.,.F.,.F.,.F.)
B_SPLINE_SURFACE_WITH_KNOTS((2,2),(3,3),(0.710318915640078,1.),(0.36671781735104,
0.383933227114987),.UNSPECIFIED.)
GEOMETRIC_REPRESENTATION_ITEM()
RATIONAL_B_SPLINE_SURFACE(((0.994179254576329,0.989756546152323,0.988246641953811),
(0.994179254576329,0.989756546152323,0.988246641953811)))
REPRESENTATION_ITEM('')
SURFACE()
);
#335=(
BOUNDED_SURFACE()
B_SPLINE_SURFACE(1,2,((#98405,#98406,#98407,#98408,#98409,#98410,#98411),
(#98412,#98413,#98414,#98415,#98416,#98417,#98418)),.UNSPECIFIED.,.F.,.F.,
 .F.)
B_SPLINE_SURFACE_WITH_KNOTS((2,2),(3,2,2,3),(0.710192959008438,1.),(0.349194141236593,
0.349369696259361,0.357142857142857,0.366925198536205),.UNSPECIFIED.)
GEOMETRIC_REPRESENTATION_ITEM()
RATIONAL_B_SPLINE_SURFACE(((0.99513694090229,0.99513694090229,0.99513694090229,
0.997271548787858,1.,0.99656630788526,0.99407312312869),(0.99513694090229,
0.99513694090229,0.99513694090229,0.997271548787858,1.,0.99656630788526,
0.99407312312869)))
REPRESENTATION_ITEM('')
SURFACE()
);
#336=(
BOUNDED_SURFACE()
B_SPLINE_SURFACE(1,2,((#98433,#98434,#98435),(#98436,#98437,#98438)),
 .UNSPECIFIED.,.F.,.F.,.F.)
B_SPLINE_SURFACE_WITH_KNOTS((2,2),(3,3),(0.710318915640075,1.),(0.366717817351071,
0.383933227114987),.UNSPECIFIED.)
GEOMETRIC_REPRESENTATION_ITEM()
RATIONAL_B_SPLINE_SURFACE(((0.994179254576313,0.989756546152321,0.988246641953811),
(0.994179254576313,0.989756546152321,0.988246641953811)))
REPRESENTATION_ITEM('')
SURFACE()
);
#337=(
BOUNDED_SURFACE()
B_SPLINE_SURFACE(1,2,((#98440,#98441,#98442,#98443,#98444,#98445,#98446),
(#98447,#98448,#98449,#98450,#98451,#98452,#98453)),.UNSPECIFIED.,.F.,.F.,
 .F.)
B_SPLINE_SURFACE_WITH_KNOTS((2,2),(3,2,2,3),(0.710192959008205,1.),(0.349194141236593,
0.349369696259361,0.357142857142857,0.366925198536205),.UNSPECIFIED.)
GEOMETRIC_REPRESENTATION_ITEM()
RATIONAL_B_SPLINE_SURFACE(((0.99513694090229,0.99513694090229,0.99513694090229,
0.997271548787858,1.,0.99656630788526,0.99407312312869),(0.99513694090229,
0.99513694090229,0.99513694090229,0.997271548787858,1.,0.99656630788526,
0.99407312312869)))
REPRESENTATION_ITEM('')
SURFACE()
);
#338=(
BOUNDED_SURFACE()
B_SPLINE_SURFACE(1,2,((#98468,#98469,#98470),(#98471,#98472,#98473)),
 .UNSPECIFIED.,.F.,.F.,.F.)
B_SPLINE_SURFACE_WITH_KNOTS((2,2),(3,3),(0.710318915639842,1.),(0.366717817351071,
0.383933227114987),.UNSPECIFIED.)
GEOMETRIC_REPRESENTATION_ITEM()
RATIONAL_B_SPLINE_SURFACE(((0.994179254576314,0.989756546152321,0.988246641953811),
(0.994179254576314,0.989756546152321,0.988246641953811)))
REPRESENTATION_ITEM('')
SURFACE()
);
#339=(
BOUNDED_SURFACE()
B_SPLINE_SURFACE(1,2,((#98475,#98476,#98477,#98478,#98479,#98480,#98481),
(#98482,#98483,#98484,#98485,#98486,#98487,#98488)),.UNSPECIFIED.,.F.,.F.,
 .F.)
B_SPLINE_SURFACE_WITH_KNOTS((2,2),(3,2,2,3),(0.710192959008435,1.),(0.349194141236593,
0.349369696259361,0.357142857142857,0.366925198536205),.UNSPECIFIED.)
GEOMETRIC_REPRESENTATION_ITEM()
RATIONAL_B_SPLINE_SURFACE(((0.99513694090229,0.99513694090229,0.99513694090229,
0.997271548787858,1.,0.99656630788526,0.994073123128689),(0.99513694090229,
0.99513694090229,0.99513694090229,0.997271548787858,1.,0.99656630788526,
0.994073123128689)))
REPRESENTATION_ITEM('')
SURFACE()
);
#340=(
BOUNDED_SURFACE()
B_SPLINE_SURFACE(1,2,((#98501,#98502,#98503),(#98504,#98505,#98506)),
 .UNSPECIFIED.,.F.,.F.,.F.)
B_SPLINE_SURFACE_WITH_KNOTS((2,2),(3,3),(0.710318915640073,1.),(0.366717817351071,
0.383933227114987),.UNSPECIFIED.)
GEOMETRIC_REPRESENTATION_ITEM()
RATIONAL_B_SPLINE_SURFACE(((0.994179254576314,0.989756546152321,0.988246641953811),
(0.994179254576314,0.989756546152321,0.988246641953811)))
REPRESENTATION_ITEM('')
SURFACE()
);
#341=(
BOUNDED_SURFACE()
B_SPLINE_SURFACE(1,2,((#98508,#98509,#98510,#98511,#98512,#98513,#98514),
(#98515,#98516,#98517,#98518,#98519,#98520,#98521)),.UNSPECIFIED.,.F.,.F.,
 .F.)
B_SPLINE_SURFACE_WITH_KNOTS((2,2),(3,2,2,3),(0.71019295900831,1.),(0.349194141236593,
0.349369696259361,0.357142857142857,0.366925198536205),.UNSPECIFIED.)
GEOMETRIC_REPRESENTATION_ITEM()
RATIONAL_B_SPLINE_SURFACE(((0.99513694090229,0.99513694090229,0.99513694090229,
0.997271548787858,1.,0.99656630788526,0.99407312312869),(0.99513694090229,
0.99513694090229,0.99513694090229,0.997271548787858,1.,0.99656630788526,
0.99407312312869)))
REPRESENTATION_ITEM('')
SURFACE()
);
#342=(
BOUNDED_SURFACE()
B_SPLINE_SURFACE(1,2,((#98534,#98535,#98536),(#98537,#98538,#98539)),
 .UNSPECIFIED.,.F.,.F.,.F.)
B_SPLINE_SURFACE_WITH_KNOTS((2,2),(3,3),(0.71031891563995,1.),(0.366717817351071,
0.383933227114987),.UNSPECIFIED.)
GEOMETRIC_REPRESENTATION_ITEM()
RATIONAL_B_SPLINE_SURFACE(((0.994179254576314,0.989756546152321,0.988246641953811),
(0.994179254576314,0.989756546152321,0.988246641953811)))
REPRESENTATION_ITEM('')
SURFACE()
);
#343=(
BOUNDED_SURFACE()
B_SPLINE_SURFACE(1,2,((#98541,#98542,#98543,#98544,#98545,#98546,#98547),
(#98548,#98549,#98550,#98551,#98552,#98553,#98554)),.UNSPECIFIED.,.F.,.F.,
 .F.)
B_SPLINE_SURFACE_WITH_KNOTS((2,2),(3,2,2,3),(0.710192959007032,1.),(0.349194141236593,
0.349369696259361,0.357142857142857,0.366925198536205),.UNSPECIFIED.)
GEOMETRIC_REPRESENTATION_ITEM()
RATIONAL_B_SPLINE_SURFACE(((0.99513694090229,0.99513694090229,0.99513694090229,
0.997271548787858,1.,0.99656630788526,0.994073123128689),(0.99513694090229,
0.99513694090229,0.99513694090229,0.997271548787858,1.,0.99656630788526,
0.994073123128689)))
REPRESENTATION_ITEM('')
SURFACE()
);
#344=(
BOUNDED_SURFACE()
B_SPLINE_SURFACE(1,2,((#98569,#98570,#98571),(#98572,#98573,#98574)),
 .UNSPECIFIED.,.F.,.F.,.F.)
B_SPLINE_SURFACE_WITH_KNOTS((2,2),(3,3),(0.710318915638672,1.),(0.366717817351071,
0.383933227114987),.UNSPECIFIED.)
GEOMETRIC_REPRESENTATION_ITEM()
RATIONAL_B_SPLINE_SURFACE(((0.994179254576314,0.989756546152321,0.988246641953811),
(0.994179254576314,0.989756546152321,0.988246641953811)))
REPRESENTATION_ITEM('')
SURFACE()
);
#345=(
BOUNDED_SURFACE()
B_SPLINE_SURFACE(1,2,((#98576,#98577,#98578,#98579,#98580,#98581,#98582),
(#98583,#98584,#98585,#98586,#98587,#98588,#98589)),.UNSPECIFIED.,.F.,.F.,
 .F.)
B_SPLINE_SURFACE_WITH_KNOTS((2,2),(3,2,2,3),(0.710192959008083,1.),(0.349194141236593,
0.349369696259361,0.357142857142857,0.366925198536205),.UNSPECIFIED.)
GEOMETRIC_REPRESENTATION_ITEM()
RATIONAL_B_SPLINE_SURFACE(((0.99513694090229,0.99513694090229,0.99513694090229,
0.997271548787858,1.,0.99656630788526,0.99407312312869),(0.99513694090229,
0.99513694090229,0.99513694090229,0.997271548787858,1.,0.996566307885261,
0.99407312312869)))
REPRESENTATION_ITEM('')
SURFACE()
);
#346=(
BOUNDED_SURFACE()
B_SPLINE_SURFACE(1,2,((#98602,#98603,#98604),(#98605,#98606,#98607)),
 .UNSPECIFIED.,.F.,.F.,.F.)
B_SPLINE_SURFACE_WITH_KNOTS((2,2),(3,3),(0.71031891563972,1.),(0.36671781735083,
0.383933227114987),.UNSPECIFIED.)
GEOMETRIC_REPRESENTATION_ITEM()
RATIONAL_B_SPLINE_SURFACE(((0.994179254576438,0.989756546152342,0.988246641953811),
(0.994179254576438,0.989756546152342,0.988246641953811)))
REPRESENTATION_ITEM('')
SURFACE()
);
#347=(
BOUNDED_SURFACE()
B_SPLINE_SURFACE(1,2,((#98609,#98610,#98611,#98612,#98613,#98614,#98615),
(#98616,#98617,#98618,#98619,#98620,#98621,#98622)),.UNSPECIFIED.,.F.,.F.,
 .F.)
B_SPLINE_SURFACE_WITH_KNOTS((2,2),(3,2,2,3),(0.710192959008441,1.),(0.349194141236593,
0.349369696259361,0.357142857142857,0.366925198536205),.UNSPECIFIED.)
GEOMETRIC_REPRESENTATION_ITEM()
RATIONAL_B_SPLINE_SURFACE(((0.99513694090229,0.99513694090229,0.99513694090229,
0.997271548787858,1.,0.99656630788526,0.99407312312869),(0.99513694090229,
0.99513694090229,0.99513694090229,0.997271548787858,1.,0.99656630788526,
0.99407312312869)))
REPRESENTATION_ITEM('')
SURFACE()
);
#348=(
BOUNDED_SURFACE()
B_SPLINE_SURFACE(1,2,((#98635,#98636,#98637),(#98638,#98639,#98640)),
 .UNSPECIFIED.,.F.,.F.,.F.)
B_SPLINE_SURFACE_WITH_KNOTS((2,2),(3,3),(0.710318915640079,1.),(0.366717817350746,
0.383933227114987),.UNSPECIFIED.)
GEOMETRIC_REPRESENTATION_ITEM()
RATIONAL_B_SPLINE_SURFACE(((0.99417925457648,0.989756546152349,0.988246641953811),
(0.99417925457648,0.989756546152349,0.988246641953811)))
REPRESENTATION_ITEM('')
SURFACE()
);
#349=(
BOUNDED_SURFACE()
B_SPLINE_SURFACE(1,2,((#98642,#98643,#98644,#98645,#98646,#98647,#98648),
(#98649,#98650,#98651,#98652,#98653,#98654,#98655)),.UNSPECIFIED.,.F.,.F.,
 .F.)
B_SPLINE_SURFACE_WITH_KNOTS((2,2),(3,2,2,3),(0.710192959008353,1.),(0.349194141236593,
0.349369696259361,0.357142857142857,0.366925198536205),.UNSPECIFIED.)
GEOMETRIC_REPRESENTATION_ITEM()
RATIONAL_B_SPLINE_SURFACE(((0.99513694090229,0.99513694090229,0.99513694090229,
0.997271548787858,1.,0.99656630788526,0.994073123128689),(0.99513694090229,
0.99513694090229,0.99513694090229,0.997271548787858,1.,0.99656630788526,
0.994073123128689)))
REPRESENTATION_ITEM('')
SURFACE()
);
#350=(
BOUNDED_SURFACE()
B_SPLINE_SURFACE(1,2,((#98668,#98669,#98670),(#98671,#98672,#98673)),
 .UNSPECIFIED.,.F.,.F.,.F.)
B_SPLINE_SURFACE_WITH_KNOTS((2,2),(3,3),(0.710318915639995,1.),(0.366717817351071,
0.383933227114987),.UNSPECIFIED.)
GEOMETRIC_REPRESENTATION_ITEM()
RATIONAL_B_SPLINE_SURFACE(((0.994179254576314,0.989756546152321,0.988246641953811),
(0.994179254576314,0.989756546152321,0.988246641953811)))
REPRESENTATION_ITEM('')
SURFACE()
);
#351=(
BOUNDED_SURFACE()
B_SPLINE_SURFACE(1,2,((#98675,#98676,#98677,#98678,#98679,#98680,#98681),
(#98682,#98683,#98684,#98685,#98686,#98687,#98688)),.UNSPECIFIED.,.F.,.F.,
 .F.)
B_SPLINE_SURFACE_WITH_KNOTS((2,2),(3,2,2,3),(0.710192959008441,1.),(0.349194141236593,
0.349369696259361,0.357142857142857,0.366925198536205),.UNSPECIFIED.)
GEOMETRIC_REPRESENTATION_ITEM()
RATIONAL_B_SPLINE_SURFACE(((0.99513694090229,0.99513694090229,0.99513694090229,
0.997271548787858,1.,0.99656630788526,0.99407312312869),(0.99513694090229,
0.99513694090229,0.99513694090229,0.997271548787858,1.,0.99656630788526,
0.99407312312869)))
REPRESENTATION_ITEM('')
SURFACE()
);
#352=(
BOUNDED_SURFACE()
B_SPLINE_SURFACE(1,2,((#98701,#98702,#98703),(#98704,#98705,#98706)),
 .UNSPECIFIED.,.F.,.F.,.F.)
B_SPLINE_SURFACE_WITH_KNOTS((2,2),(3,3),(0.71031891564008,1.),(0.366717817351071,
0.383933227114987),.UNSPECIFIED.)
GEOMETRIC_REPRESENTATION_ITEM()
RATIONAL_B_SPLINE_SURFACE(((0.994179254576313,0.989756546152321,0.988246641953811),
(0.994179254576313,0.989756546152321,0.988246641953811)))
REPRESENTATION_ITEM('')
SURFACE()
);
#353=(
BOUNDED_SURFACE()
B_SPLINE_SURFACE(1,2,((#98708,#98709,#98710,#98711,#98712,#98713,#98714),
(#98715,#98716,#98717,#98718,#98719,#98720,#98721)),.UNSPECIFIED.,.F.,.F.,
 .F.)
B_SPLINE_SURFACE_WITH_KNOTS((2,2),(3,2,2,3),(0.710192959008357,1.),(0.349194141236593,
0.349369696259361,0.357142857142857,0.366925198536205),.UNSPECIFIED.)
GEOMETRIC_REPRESENTATION_ITEM()
RATIONAL_B_SPLINE_SURFACE(((0.99513694090229,0.99513694090229,0.99513694090229,
0.997271548787858,1.,0.99656630788526,0.99407312312869),(0.99513694090229,
0.99513694090229,0.99513694090229,0.997271548787858,1.,0.99656630788526,
0.99407312312869)))
REPRESENTATION_ITEM('')
SURFACE()
);
#354=(
BOUNDED_SURFACE()
B_SPLINE_SURFACE(1,2,((#98734,#98735,#98736),(#98737,#98738,#98739)),
 .UNSPECIFIED.,.F.,.F.,.F.)
B_SPLINE_SURFACE_WITH_KNOTS((2,2),(3,3),(0.710318915639997,1.),(0.366717817350691,
0.383933227114987),.UNSPECIFIED.)
GEOMETRIC_REPRESENTATION_ITEM()
RATIONAL_B_SPLINE_SURFACE(((0.994179254576509,0.989756546152354,0.988246641953811),
(0.994179254576509,0.989756546152354,0.988246641953811)))
REPRESENTATION_ITEM('')
SURFACE()
);
#355=(
BOUNDED_SURFACE()
B_SPLINE_SURFACE(1,2,((#98741,#98742,#98743,#98744,#98745,#98746,#98747),
(#98748,#98749,#98750,#98751,#98752,#98753,#98754)),.UNSPECIFIED.,.F.,.F.,
 .F.)
B_SPLINE_SURFACE_WITH_KNOTS((2,2),(3,2,2,3),(0.710192959008355,1.),(0.349194141236593,
0.349369696259361,0.357142857142857,0.366925198536205),.UNSPECIFIED.)
GEOMETRIC_REPRESENTATION_ITEM()
RATIONAL_B_SPLINE_SURFACE(((0.99513694090229,0.99513694090229,0.99513694090229,
0.997271548787858,1.,0.99656630788526,0.994073123128689),(0.99513694090229,
0.99513694090229,0.99513694090229,0.997271548787858,1.,0.99656630788526,
0.994073123128689)))
REPRESENTATION_ITEM('')
SURFACE()
);
#356=(
BOUNDED_SURFACE()
B_SPLINE_SURFACE(1,2,((#98769,#98770,#98771),(#98772,#98773,#98774)),
 .UNSPECIFIED.,.F.,.F.,.F.)
B_SPLINE_SURFACE_WITH_KNOTS((2,2),(3,3),(0.710318915639994,1.),(0.366717817351071,
0.383933227114987),.UNSPECIFIED.)
GEOMETRIC_REPRESENTATION_ITEM()
RATIONAL_B_SPLINE_SURFACE(((0.994179254576314,0.989756546152321,0.988246641953811),
(0.994179254576314,0.989756546152321,0.988246641953811)))
REPRESENTATION_ITEM('')
SURFACE()
);
#357=(
BOUNDED_SURFACE()
B_SPLINE_SURFACE(1,2,((#98776,#98777,#98778,#98779,#98780,#98781,#98782),
(#98783,#98784,#98785,#98786,#98787,#98788,#98789)),.UNSPECIFIED.,.F.,.F.,
 .F.)
B_SPLINE_SURFACE_WITH_KNOTS((2,2),(3,2,2,3),(0.710192959008362,1.),(0.349194141236593,
0.349369696259361,0.357142857142857,0.366925198536205),.UNSPECIFIED.)
GEOMETRIC_REPRESENTATION_ITEM()
RATIONAL_B_SPLINE_SURFACE(((0.99513694090229,0.99513694090229,0.99513694090229,
0.997271548787859,1.,0.99656630788526,0.99407312312869),(0.99513694090229,
0.99513694090229,0.99513694090229,0.997271548787859,1.,0.99656630788526,
0.99407312312869)))
REPRESENTATION_ITEM('')
SURFACE()
);
#358=(
BOUNDED_SURFACE()
B_SPLINE_SURFACE(1,2,((#98804,#98805,#98806),(#98807,#98808,#98809)),
 .UNSPECIFIED.,.F.,.F.,.F.)
B_SPLINE_SURFACE_WITH_KNOTS((2,2),(3,3),(0.710318915640001,1.),(0.366717817351071,
0.383933227114987),.UNSPECIFIED.)
GEOMETRIC_REPRESENTATION_ITEM()
RATIONAL_B_SPLINE_SURFACE(((0.994179254576314,0.989756546152321,0.988246641953811),
(0.994179254576314,0.989756546152321,0.988246641953811)))
REPRESENTATION_ITEM('')
SURFACE()
);
#359=(
BOUNDED_SURFACE()
B_SPLINE_SURFACE(1,2,((#98811,#98812,#98813,#98814,#98815,#98816,#98817),
(#98818,#98819,#98820,#98821,#98822,#98823,#98824)),.UNSPECIFIED.,.F.,.F.,
 .F.)
B_SPLINE_SURFACE_WITH_KNOTS((2,2),(3,2,2,3),(0.710192959008356,1.),(0.349194141236593,
0.349369696259361,0.357142857142857,0.366925198536205),.UNSPECIFIED.)
GEOMETRIC_REPRESENTATION_ITEM()
RATIONAL_B_SPLINE_SURFACE(((0.99513694090229,0.99513694090229,0.99513694090229,
0.997271548787858,1.,0.99656630788526,0.99407312312869),(0.99513694090229,
0.99513694090229,0.99513694090229,0.997271548787858,1.,0.99656630788526,
0.99407312312869)))
REPRESENTATION_ITEM('')
SURFACE()
);
#360=(
BOUNDED_SURFACE()
B_SPLINE_SURFACE(1,2,((#98839,#98840,#98841),(#98842,#98843,#98844)),
 .UNSPECIFIED.,.F.,.F.,.F.)
B_SPLINE_SURFACE_WITH_KNOTS((2,2),(3,3),(0.710318915639994,1.),(0.366717817351071,
0.383933227114986),.UNSPECIFIED.)
GEOMETRIC_REPRESENTATION_ITEM()
RATIONAL_B_SPLINE_SURFACE(((0.994179254576314,0.989756546152321,0.988246641953811),
(0.994179254576314,0.989756546152321,0.988246641953811)))
REPRESENTATION_ITEM('')
SURFACE()
);
#361=(
BOUNDED_SURFACE()
B_SPLINE_SURFACE(1,2,((#98846,#98847,#98848,#98849,#98850,#98851,#98852),
(#98853,#98854,#98855,#98856,#98857,#98858,#98859)),.UNSPECIFIED.,.F.,.F.,
 .F.)
B_SPLINE_SURFACE_WITH_KNOTS((2,2),(3,2,2,3),(0.710192959007468,1.),(0.349194141236594,
0.349369696259362,0.357142857142857,0.366925198536205),.UNSPECIFIED.)
GEOMETRIC_REPRESENTATION_ITEM()
RATIONAL_B_SPLINE_SURFACE(((0.99513694090229,0.99513694090229,0.99513694090229,
0.997271548787859,1.,0.996566307885261,0.99407312312869),(0.99513694090229,
0.99513694090229,0.99513694090229,0.997271548787859,1.,0.996566307885261,
0.99407312312869)))
REPRESENTATION_ITEM('')
SURFACE()
);
#362=(
BOUNDED_SURFACE()
B_SPLINE_SURFACE(1,2,((#98872,#98873,#98874),(#98875,#98876,#98877)),
 .UNSPECIFIED.,.F.,.F.,.F.)
B_SPLINE_SURFACE_WITH_KNOTS((2,2),(3,3),(0.710318915639108,1.),(0.366717817351052,
0.383933227114987),.UNSPECIFIED.)
GEOMETRIC_REPRESENTATION_ITEM()
RATIONAL_B_SPLINE_SURFACE(((0.994179254576324,0.989756546152323,0.988246641953811),
(0.994179254576324,0.989756546152322,0.988246641953811)))
REPRESENTATION_ITEM('')
SURFACE()
);
#363=(
BOUNDED_SURFACE()
B_SPLINE_SURFACE(1,2,((#98879,#98880,#98881,#98882,#98883,#98884,#98885),
(#98886,#98887,#98888,#98889,#98890,#98891,#98892)),.UNSPECIFIED.,.F.,.F.,
 .F.)
B_SPLINE_SURFACE_WITH_KNOTS((2,2),(3,2,2,3),(0.710192959008014,1.),(0.349194141236593,
0.349369696259361,0.357142857142857,0.366925198536205),.UNSPECIFIED.)
GEOMETRIC_REPRESENTATION_ITEM()
RATIONAL_B_SPLINE_SURFACE(((0.99513694090229,0.99513694090229,0.99513694090229,
0.997271548787858,1.,0.99656630788526,0.994073123128689),(0.99513694090229,
0.99513694090229,0.99513694090229,0.997271548787858,1.,0.99656630788526,
0.994073123128689)))
REPRESENTATION_ITEM('')
SURFACE()
);
#364=(
BOUNDED_SURFACE()
B_SPLINE_SURFACE(1,2,((#98905,#98906,#98907),(#98908,#98909,#98910)),
 .UNSPECIFIED.,.F.,.F.,.F.)
B_SPLINE_SURFACE_WITH_KNOTS((2,2),(3,3),(0.710318915639655,1.),(0.366717817351039,
0.383933227114987),.UNSPECIFIED.)
GEOMETRIC_REPRESENTATION_ITEM()
RATIONAL_B_SPLINE_SURFACE(((0.99417925457633,0.989756546152323,0.988246641953811),
(0.99417925457633,0.989756546152323,0.988246641953811)))
REPRESENTATION_ITEM('')
SURFACE()
);
#365=(
BOUNDED_SURFACE()
B_SPLINE_SURFACE(1,2,((#98912,#98913,#98914,#98915,#98916,#98917,#98918),
(#98919,#98920,#98921,#98922,#98923,#98924,#98925)),.UNSPECIFIED.,.F.,.F.,
 .F.)
B_SPLINE_SURFACE_WITH_KNOTS((2,2),(3,2,2,3),(0.710192959008103,1.),(0.349194141236593,
0.349369696259361,0.357142857142857,0.366925198536205),.UNSPECIFIED.)
GEOMETRIC_REPRESENTATION_ITEM()
RATIONAL_B_SPLINE_SURFACE(((0.99513694090229,0.99513694090229,0.99513694090229,
0.997271548787858,1.,0.99656630788526,0.99407312312869),(0.99513694090229,
0.99513694090229,0.99513694090229,0.997271548787858,1.,0.99656630788526,
0.99407312312869)))
REPRESENTATION_ITEM('')
SURFACE()
);
#366=(
BOUNDED_SURFACE()
B_SPLINE_SURFACE(1,2,((#98938,#98939,#98940),(#98941,#98942,#98943)),
 .UNSPECIFIED.,.F.,.F.,.F.)
B_SPLINE_SURFACE_WITH_KNOTS((2,2),(3,3),(0.710318915639745,1.),(0.366717817351071,
0.383933227114987),.UNSPECIFIED.)
GEOMETRIC_REPRESENTATION_ITEM()
RATIONAL_B_SPLINE_SURFACE(((0.994179254576314,0.989756546152321,0.988246641953811),
(0.994179254576314,0.989756546152321,0.988246641953811)))
REPRESENTATION_ITEM('')
SURFACE()
);
#367=(
BOUNDED_SURFACE()
B_SPLINE_SURFACE(1,2,((#98945,#98946,#98947,#98948,#98949,#98950,#98951),
(#98952,#98953,#98954,#98955,#98956,#98957,#98958)),.UNSPECIFIED.,.F.,.F.,
 .F.)
B_SPLINE_SURFACE_WITH_KNOTS((2,2),(3,2,2,3),(0.710192959007991,1.),(0.349194141236593,
0.349369696259361,0.357142857142857,0.366925198536206),.UNSPECIFIED.)
GEOMETRIC_REPRESENTATION_ITEM()
RATIONAL_B_SPLINE_SURFACE(((0.99513694090229,0.99513694090229,0.99513694090229,
0.997271548787859,1.,0.99656630788526,0.994073123128689),(0.99513694090229,
0.99513694090229,0.99513694090229,0.997271548787859,1.,0.99656630788526,
0.994073123128689)))
REPRESENTATION_ITEM('')
SURFACE()
);
#368=(
BOUNDED_SURFACE()
B_SPLINE_SURFACE(1,2,((#98966,#98967,#98968,#98969,#98970),(#98971,#98972,
#98973,#98974,#98975)),.UNSPECIFIED.,.F.,.F.,.F.)
B_SPLINE_SURFACE_WITH_KNOTS((2,2),(3,2,3),(0.,0.29040523113993),(0.40044464504831,
0.401042835325431,0.418415696246123),.UNSPECIFIED.)
GEOMETRIC_REPRESENTATION_ITEM()
RATIONAL_B_SPLINE_SURFACE(((0.988122504062136,0.988122504062136,0.988122504062136,
0.989520169850094,0.993884164197532),(0.988122504062135,0.988122504062135,
0.988122504062135,0.989520169850094,0.993884164197532)))
REPRESENTATION_ITEM('')
SURFACE()
);
#369=(
BOUNDED_SURFACE()
B_SPLINE_SURFACE(1,2,((#98984,#98985,#98986),(#98987,#98988,#98989)),
 .UNSPECIFIED.,.F.,.F.,.F.)
B_SPLINE_SURFACE_WITH_KNOTS((2,2),(3,3),(0.,0.289681084359929),(0.314840108491246,
0.332069149066805),.UNSPECIFIED.)
GEOMETRIC_REPRESENTATION_ITEM()
RATIONAL_B_SPLINE_SURFACE(((0.98789057959819,0.986774945528862,0.988576730109495),
(0.98789057959819,0.986774945528862,0.988576730109495)))
REPRESENTATION_ITEM('')
SURFACE()
);
#370=(
BOUNDED_SURFACE()
B_SPLINE_SURFACE(1,2,((#98998,#98999,#99000,#99001,#99002),(#99003,#99004,
#99005,#99006,#99007)),.UNSPECIFIED.,.F.,.F.,.F.)
B_SPLINE_SURFACE_WITH_KNOTS((2,2),(3,2,3),(0.,0.290405231173627),(0.400444645014739,
0.401042835325431,0.418415696246122),.UNSPECIFIED.)
GEOMETRIC_REPRESENTATION_ITEM()
RATIONAL_B_SPLINE_SURFACE(((0.988122504062135,0.988122504062135,0.988122504062135,
0.989520169850094,0.993884164197532),(0.988122504062135,0.988122504062135,
0.988122504062135,0.989520169850094,0.993884164197532)))
REPRESENTATION_ITEM('')
SURFACE()
);
#371=(
BOUNDED_SURFACE()
B_SPLINE_SURFACE(1,2,((#99009,#99010,#99011),(#99012,#99013,#99014)),
 .UNSPECIFIED.,.F.,.F.,.F.)
B_SPLINE_SURFACE_WITH_KNOTS((2,2),(3,3),(0.,0.28968108435993),(0.314840108491247,
0.332069149066804),.UNSPECIFIED.)
GEOMETRIC_REPRESENTATION_ITEM()
RATIONAL_B_SPLINE_SURFACE(((0.98789057959819,0.986774945528862,0.988576730109495),
(0.98789057959819,0.986774945528862,0.988576730109495)))
REPRESENTATION_ITEM('')
SURFACE()
);
#372=(
BOUNDED_SURFACE()
B_SPLINE_SURFACE(1,2,((#99023,#99024,#99025,#99026,#99027),(#99028,#99029,
#99030,#99031,#99032)),.UNSPECIFIED.,.F.,.F.,.F.)
B_SPLINE_SURFACE_WITH_KNOTS((2,2),(3,2,3),(0.,0.290405231161606),(0.400444645026067,
0.40104283532543,0.418415696246121),.UNSPECIFIED.)
GEOMETRIC_REPRESENTATION_ITEM()
RATIONAL_B_SPLINE_SURFACE(((0.988122504062135,0.988122504062135,0.988122504062135,
0.989520169850093,0.993884164197532),(0.988122504062135,0.988122504062135,
0.988122504062135,0.989520169850093,0.993884164197532)))
REPRESENTATION_ITEM('')
SURFACE()
);
#373=(
BOUNDED_SURFACE()
B_SPLINE_SURFACE(1,2,((#99034,#99035,#99036),(#99037,#99038,#99039)),
 .UNSPECIFIED.,.F.,.F.,.F.)
B_SPLINE_SURFACE_WITH_KNOTS((2,2),(3,3),(0.,0.289681084359922),(0.314840108491247,
0.332069149066805),.UNSPECIFIED.)
GEOMETRIC_REPRESENTATION_ITEM()
RATIONAL_B_SPLINE_SURFACE(((0.98789057959819,0.986774945528862,0.988576730109495),
(0.98789057959819,0.986774945528862,0.988576730109495)))
REPRESENTATION_ITEM('')
SURFACE()
);
#374=(
BOUNDED_SURFACE()
B_SPLINE_SURFACE(1,2,((#99048,#99049,#99050,#99051,#99052),(#99053,#99054,
#99055,#99056,#99057)),.UNSPECIFIED.,.F.,.F.,.F.)
B_SPLINE_SURFACE_WITH_KNOTS((2,2),(3,2,3),(0.,0.290405231142216),(0.400444645037561,
0.40104283532543,0.418415696246121),.UNSPECIFIED.)
GEOMETRIC_REPRESENTATION_ITEM()
RATIONAL_B_SPLINE_SURFACE(((0.988122504062135,0.988122504062135,0.988122504062135,
0.989520169850093,0.993884164197532),(0.988122504062135,0.988122504062135,
0.988122504062135,0.989520169850093,0.993884164197532)))
REPRESENTATION_ITEM('')
SURFACE()
);
#375=(
BOUNDED_SURFACE()
B_SPLINE_SURFACE(1,2,((#99059,#99060,#99061),(#99062,#99063,#99064)),
 .UNSPECIFIED.,.F.,.F.,.F.)
B_SPLINE_SURFACE_WITH_KNOTS((2,2),(3,3),(0.,0.289681084359915),(0.314840108491247,
0.332069149066805),.UNSPECIFIED.)
GEOMETRIC_REPRESENTATION_ITEM()
RATIONAL_B_SPLINE_SURFACE(((0.98789057959819,0.986774945528862,0.988576730109495),
(0.98789057959819,0.986774945528862,0.988576730109495)))
REPRESENTATION_ITEM('')
SURFACE()
);
#376=(
BOUNDED_SURFACE()
B_SPLINE_SURFACE(1,2,((#99073,#99074,#99075,#99076,#99077),(#99078,#99079,
#99080,#99081,#99082)),.UNSPECIFIED.,.F.,.F.,.F.)
B_SPLINE_SURFACE_WITH_KNOTS((2,2),(3,2,3),(0.,0.290405231151886),(0.400444645028098,
0.401042835325431,0.418415696246121),.UNSPECIFIED.)
GEOMETRIC_REPRESENTATION_ITEM()
RATIONAL_B_SPLINE_SURFACE(((0.988122504062136,0.988122504062136,0.988122504062136,
0.989520169850094,0.993884164197532),(0.988122504062136,0.988122504062136,
0.988122504062136,0.989520169850094,0.993884164197532)))
REPRESENTATION_ITEM('')
SURFACE()
);
#377=(
BOUNDED_SURFACE()
B_SPLINE_SURFACE(1,2,((#99084,#99085,#99086),(#99087,#99088,#99089)),
 .UNSPECIFIED.,.F.,.F.,.F.)
B_SPLINE_SURFACE_WITH_KNOTS((2,2),(3,3),(0.,0.289681084359921),(0.314840108491246,
0.332069149066804),.UNSPECIFIED.)
GEOMETRIC_REPRESENTATION_ITEM()
RATIONAL_B_SPLINE_SURFACE(((0.98789057959819,0.986774945528862,0.988576730109495),
(0.98789057959819,0.986774945528862,0.988576730109495)))
REPRESENTATION_ITEM('')
SURFACE()
);
#378=(
BOUNDED_SURFACE()
B_SPLINE_SURFACE(1,2,((#99098,#99099,#99100,#99101,#99102),(#99103,#99104,
#99105,#99106,#99107)),.UNSPECIFIED.,.F.,.F.,.F.)
B_SPLINE_SURFACE_WITH_KNOTS((2,2),(3,2,3),(0.,0.290405231115877),(0.400444645063817,
0.401042835325431,0.418415696246122),.UNSPECIFIED.)
GEOMETRIC_REPRESENTATION_ITEM()
RATIONAL_B_SPLINE_SURFACE(((0.988122504062135,0.988122504062135,0.988122504062135,
0.989520169850094,0.993884164197532),(0.988122504062136,0.988122504062136,
0.988122504062136,0.989520169850094,0.993884164197532)))
REPRESENTATION_ITEM('')
SURFACE()
);
#379=(
BOUNDED_SURFACE()
B_SPLINE_SURFACE(1,2,((#99109,#99110,#99111),(#99112,#99113,#99114)),
 .UNSPECIFIED.,.F.,.F.,.F.)
B_SPLINE_SURFACE_WITH_KNOTS((2,2),(3,3),(0.,0.289681084359917),(0.314840108491246,
0.332069149066804),.UNSPECIFIED.)
GEOMETRIC_REPRESENTATION_ITEM()
RATIONAL_B_SPLINE_SURFACE(((0.98789057959819,0.986774945528862,0.988576730109495),
(0.98789057959819,0.986774945528862,0.988576730109495)))
REPRESENTATION_ITEM('')
SURFACE()
);
#380=(
BOUNDED_SURFACE()
B_SPLINE_SURFACE(1,2,((#99123,#99124,#99125,#99126,#99127),(#99128,#99129,
#99130,#99131,#99132)),.UNSPECIFIED.,.F.,.F.,.F.)
B_SPLINE_SURFACE_WITH_KNOTS((2,2),(3,2,3),(0.,0.290405231151133),(0.400444645029202,
0.401042835325431,0.418415696246122),.UNSPECIFIED.)
GEOMETRIC_REPRESENTATION_ITEM()
RATIONAL_B_SPLINE_SURFACE(((0.988122504062136,0.988122504062136,0.988122504062136,
0.989520169850094,0.993884164197532),(0.988122504062135,0.988122504062135,
0.988122504062135,0.989520169850094,0.993884164197532)))
REPRESENTATION_ITEM('')
SURFACE()
);
#381=(
BOUNDED_SURFACE()
B_SPLINE_SURFACE(1,2,((#99134,#99135,#99136),(#99137,#99138,#99139)),
 .UNSPECIFIED.,.F.,.F.,.F.)
B_SPLINE_SURFACE_WITH_KNOTS((2,2),(3,3),(0.,0.289681084359922),(0.314840108491246,
0.332069149066804),.UNSPECIFIED.)
GEOMETRIC_REPRESENTATION_ITEM()
RATIONAL_B_SPLINE_SURFACE(((0.98789057959819,0.986774945528862,0.988576730109495),
(0.98789057959819,0.986774945528862,0.988576730109495)))
REPRESENTATION_ITEM('')
SURFACE()
);
#382=(
BOUNDED_SURFACE()
B_SPLINE_SURFACE(1,2,((#99148,#99149,#99150,#99151,#99152),(#99153,#99154,
#99155,#99156,#99157)),.UNSPECIFIED.,.F.,.F.,.F.)
B_SPLINE_SURFACE_WITH_KNOTS((2,2),(3,2,3),(0.,0.290405231117896),(0.400444645069685,
0.401042835325431,0.418415696246122),.UNSPECIFIED.)
GEOMETRIC_REPRESENTATION_ITEM()
RATIONAL_B_SPLINE_SURFACE(((0.988122504062136,0.988122504062136,0.988122504062136,
0.989520169850094,0.993884164197532),(0.988122504062135,0.988122504062135,
0.988122504062135,0.989520169850094,0.993884164197532)))
REPRESENTATION_ITEM('')
SURFACE()
);
#383=(
BOUNDED_SURFACE()
B_SPLINE_SURFACE(1,2,((#99159,#99160,#99161),(#99162,#99163,#99164)),
 .UNSPECIFIED.,.F.,.F.,.F.)
B_SPLINE_SURFACE_WITH_KNOTS((2,2),(3,3),(0.,0.289681084359918),(0.314840108491246,
0.332069149066804),.UNSPECIFIED.)
GEOMETRIC_REPRESENTATION_ITEM()
RATIONAL_B_SPLINE_SURFACE(((0.98789057959819,0.986774945528862,0.988576730109495),
(0.98789057959819,0.986774945528862,0.988576730109495)))
REPRESENTATION_ITEM('')
SURFACE()
);
#384=(
BOUNDED_SURFACE()
B_SPLINE_SURFACE(1,2,((#99173,#99174,#99175,#99176,#99177),(#99178,#99179,
#99180,#99181,#99182)),.UNSPECIFIED.,.F.,.F.,.F.)
B_SPLINE_SURFACE_WITH_KNOTS((2,2),(3,2,3),(0.,0.290405231125489),(0.400444645062306,
0.401042835325431,0.418415696246122),.UNSPECIFIED.)
GEOMETRIC_REPRESENTATION_ITEM()
RATIONAL_B_SPLINE_SURFACE(((0.988122504062135,0.988122504062135,0.988122504062135,
0.989520169850094,0.993884164197532),(0.988122504062136,0.988122504062136,
0.988122504062136,0.989520169850094,0.993884164197532)))
REPRESENTATION_ITEM('')
SURFACE()
);
#385=(
BOUNDED_SURFACE()
B_SPLINE_SURFACE(1,2,((#99184,#99185,#99186),(#99187,#99188,#99189)),
 .UNSPECIFIED.,.F.,.F.,.F.)
B_SPLINE_SURFACE_WITH_KNOTS((2,2),(3,3),(0.,0.289681084359918),(0.314840108491246,
0.332069149066804),.UNSPECIFIED.)
GEOMETRIC_REPRESENTATION_ITEM()
RATIONAL_B_SPLINE_SURFACE(((0.98789057959819,0.986774945528862,0.988576730109495),
(0.98789057959819,0.986774945528862,0.988576730109495)))
REPRESENTATION_ITEM('')
SURFACE()
);
#386=(
BOUNDED_SURFACE()
B_SPLINE_SURFACE(1,2,((#99198,#99199,#99200,#99201,#99202),(#99203,#99204,
#99205,#99206,#99207)),.UNSPECIFIED.,.F.,.F.,.F.)
B_SPLINE_SURFACE_WITH_KNOTS((2,2),(3,2,3),(0.,0.290405231155539),(0.400444645032021,
0.401042835325431,0.418415696246122),.UNSPECIFIED.)
GEOMETRIC_REPRESENTATION_ITEM()
RATIONAL_B_SPLINE_SURFACE(((0.988122504062136,0.988122504062136,0.988122504062136,
0.989520169850094,0.993884164197532),(0.988122504062136,0.988122504062136,
0.988122504062136,0.989520169850094,0.993884164197532)))
REPRESENTATION_ITEM('')
SURFACE()
);
#387=(
BOUNDED_SURFACE()
B_SPLINE_SURFACE(1,2,((#99209,#99210,#99211),(#99212,#99213,#99214)),
 .UNSPECIFIED.,.F.,.F.,.F.)
B_SPLINE_SURFACE_WITH_KNOTS((2,2),(3,3),(0.,0.289681084359924),(0.314840108491246,
0.332069149066804),.UNSPECIFIED.)
GEOMETRIC_REPRESENTATION_ITEM()
RATIONAL_B_SPLINE_SURFACE(((0.98789057959819,0.986774945528862,0.988576730109495),
(0.98789057959819,0.986774945528862,0.988576730109495)))
REPRESENTATION_ITEM('')
SURFACE()
);
#388=(
BOUNDED_SURFACE()
B_SPLINE_SURFACE(1,2,((#99223,#99224,#99225,#99226,#99227),(#99228,#99229,
#99230,#99231,#99232)),.UNSPECIFIED.,.F.,.F.,.F.)
B_SPLINE_SURFACE_WITH_KNOTS((2,2),(3,2,3),(0.,0.290405231152987),(0.400444645034762,
0.401042835325431,0.418415696246122),.UNSPECIFIED.)
GEOMETRIC_REPRESENTATION_ITEM()
RATIONAL_B_SPLINE_SURFACE(((0.988122504062136,0.988122504062136,0.988122504062136,
0.989520169850094,0.993884164197532),(0.988122504062136,0.988122504062136,
0.988122504062136,0.989520169850094,0.993884164197532)))
REPRESENTATION_ITEM('')
SURFACE()
);
#389=(
BOUNDED_SURFACE()
B_SPLINE_SURFACE(1,2,((#99234,#99235,#99236),(#99237,#99238,#99239)),
 .UNSPECIFIED.,.F.,.F.,.F.)
B_SPLINE_SURFACE_WITH_KNOTS((2,2),(3,3),(0.,0.289681084359924),(0.314840108491246,
0.332069149066804),.UNSPECIFIED.)
GEOMETRIC_REPRESENTATION_ITEM()
RATIONAL_B_SPLINE_SURFACE(((0.98789057959819,0.986774945528862,0.988576730109495),
(0.98789057959819,0.986774945528862,0.988576730109495)))
REPRESENTATION_ITEM('')
SURFACE()
);
#390=(
BOUNDED_SURFACE()
B_SPLINE_SURFACE(1,2,((#99248,#99249,#99250,#99251,#99252),(#99253,#99254,
#99255,#99256,#99257)),.UNSPECIFIED.,.F.,.F.,.F.)
B_SPLINE_SURFACE_WITH_KNOTS((2,2),(3,2,3),(0.,0.290405231142137),(0.400444645037875,
0.401042835325431,0.418415696246122),.UNSPECIFIED.)
GEOMETRIC_REPRESENTATION_ITEM()
RATIONAL_B_SPLINE_SURFACE(((0.988122504062136,0.988122504062136,0.988122504062136,
0.989520169850094,0.993884164197532),(0.988122504062136,0.988122504062136,
0.988122504062136,0.989520169850094,0.993884164197532)))
REPRESENTATION_ITEM('')
SURFACE()
);
#391=(
BOUNDED_SURFACE()
B_SPLINE_SURFACE(1,2,((#99259,#99260,#99261),(#99262,#99263,#99264)),
 .UNSPECIFIED.,.F.,.F.,.F.)
B_SPLINE_SURFACE_WITH_KNOTS((2,2),(3,3),(0.,0.28968108435992),(0.314840108491246,
0.332069149066804),.UNSPECIFIED.)
GEOMETRIC_REPRESENTATION_ITEM()
RATIONAL_B_SPLINE_SURFACE(((0.98789057959819,0.986774945528862,0.988576730109495),
(0.98789057959819,0.986774945528862,0.988576730109495)))
REPRESENTATION_ITEM('')
SURFACE()
);
#392=(
BOUNDED_SURFACE()
B_SPLINE_SURFACE(1,2,((#99273,#99274,#99275,#99276,#99277),(#99278,#99279,
#99280,#99281,#99282)),.UNSPECIFIED.,.F.,.F.,.F.)
B_SPLINE_SURFACE_WITH_KNOTS((2,2),(3,2,3),(0.,0.290405231138609),(0.400444645042956,
0.401042835325431,0.418415696246122),.UNSPECIFIED.)
GEOMETRIC_REPRESENTATION_ITEM()
RATIONAL_B_SPLINE_SURFACE(((0.988122504062136,0.988122504062136,0.988122504062136,
0.989520169850094,0.993884164197532),(0.988122504062136,0.988122504062136,
0.988122504062136,0.989520169850094,0.993884164197532)))
REPRESENTATION_ITEM('')
SURFACE()
);
#393=(
BOUNDED_SURFACE()
B_SPLINE_SURFACE(1,2,((#99284,#99285,#99286),(#99287,#99288,#99289)),
 .UNSPECIFIED.,.F.,.F.,.F.)
B_SPLINE_SURFACE_WITH_KNOTS((2,2),(3,3),(0.,0.289681084359919),(0.314840108491246,
0.332069149066804),.UNSPECIFIED.)
GEOMETRIC_REPRESENTATION_ITEM()
RATIONAL_B_SPLINE_SURFACE(((0.98789057959819,0.986774945528862,0.988576730109495),
(0.98789057959819,0.986774945528862,0.988576730109495)))
REPRESENTATION_ITEM('')
SURFACE()
);
#394=(
BOUNDED_SURFACE()
B_SPLINE_SURFACE(1,2,((#99298,#99299,#99300,#99301,#99302),(#99303,#99304,
#99305,#99306,#99307)),.UNSPECIFIED.,.F.,.F.,.F.)
B_SPLINE_SURFACE_WITH_KNOTS((2,2),(3,2,3),(0.,0.290405231111565),(0.400444645068332,
0.401042835325431,0.418415696246122),.UNSPECIFIED.)
GEOMETRIC_REPRESENTATION_ITEM()
RATIONAL_B_SPLINE_SURFACE(((0.988122504062136,0.988122504062136,0.988122504062136,
0.989520169850094,0.993884164197532),(0.988122504062135,0.988122504062135,
0.988122504062135,0.989520169850094,0.993884164197532)))
REPRESENTATION_ITEM('')
SURFACE()
);
#395=(
BOUNDED_SURFACE()
B_SPLINE_SURFACE(1,2,((#99309,#99310,#99311),(#99312,#99313,#99314)),
 .UNSPECIFIED.,.F.,.F.,.F.)
B_SPLINE_SURFACE_WITH_KNOTS((2,2),(3,3),(0.,0.289681084359928),(0.314840108491246,
0.332069149066804),.UNSPECIFIED.)
GEOMETRIC_REPRESENTATION_ITEM()
RATIONAL_B_SPLINE_SURFACE(((0.98789057959819,0.986774945528862,0.988576730109495),
(0.98789057959819,0.986774945528862,0.988576730109495)))
REPRESENTATION_ITEM('')
SURFACE()
);
#396=(
BOUNDED_SURFACE()
B_SPLINE_SURFACE(1,2,((#99323,#99324,#99325,#99326,#99327),(#99328,#99329,
#99330,#99331,#99332)),.UNSPECIFIED.,.F.,.F.,.F.)
B_SPLINE_SURFACE_WITH_KNOTS((2,2),(3,2,3),(0.,0.290038987984222),(0.400810888203859,
0.401042835325431,0.418415696246122),.UNSPECIFIED.)
GEOMETRIC_REPRESENTATION_ITEM()
RATIONAL_B_SPLINE_SURFACE(((0.988122504062136,0.988122504062136,0.988122504062136,
0.989520169850094,0.993884164197532),(0.988122504062136,0.988122504062136,
0.988122504062136,0.989520169850094,0.993884164197532)))
REPRESENTATION_ITEM('')
SURFACE()
);
#397=(
BOUNDED_SURFACE()
B_SPLINE_SURFACE(1,2,((#99334,#99335,#99336),(#99337,#99338,#99339)),
 .UNSPECIFIED.,.F.,.F.,.F.)
B_SPLINE_SURFACE_WITH_KNOTS((2,2),(3,3),(0.,0.289681084359918),(0.314840108491245,
0.332069149066804),.UNSPECIFIED.)
GEOMETRIC_REPRESENTATION_ITEM()
RATIONAL_B_SPLINE_SURFACE(((0.98789057959819,0.986774945528862,0.988576730109495),
(0.98789057959819,0.986774945528862,0.988576730109495)))
REPRESENTATION_ITEM('')
SURFACE()
);
#398=(
BOUNDED_SURFACE()
B_SPLINE_SURFACE(1,2,((#99348,#99349,#99350,#99351,#99352),(#99353,#99354,
#99355,#99356,#99357)),.UNSPECIFIED.,.F.,.F.,.F.)
B_SPLINE_SURFACE_WITH_KNOTS((2,2),(3,2,3),(0.,0.290405231165758),(0.400444645022587,
0.401042835325431,0.418415696246122),.UNSPECIFIED.)
GEOMETRIC_REPRESENTATION_ITEM()
RATIONAL_B_SPLINE_SURFACE(((0.988122504062135,0.988122504062135,0.988122504062135,
0.989520169850094,0.993884164197532),(0.988122504062135,0.988122504062135,
0.988122504062135,0.989520169850094,0.993884164197532)))
REPRESENTATION_ITEM('')
SURFACE()
);
#399=(
BOUNDED_SURFACE()
B_SPLINE_SURFACE(1,2,((#99359,#99360,#99361),(#99362,#99363,#99364)),
 .UNSPECIFIED.,.F.,.F.,.F.)
B_SPLINE_SURFACE_WITH_KNOTS((2,2),(3,3),(0.,0.289681084359926),(0.314840108491246,
0.332069149066804),.UNSPECIFIED.)
GEOMETRIC_REPRESENTATION_ITEM()
RATIONAL_B_SPLINE_SURFACE(((0.98789057959819,0.986774945528862,0.988576730109495),
(0.98789057959819,0.986774945528862,0.988576730109495)))
REPRESENTATION_ITEM('')
SURFACE()
);
#400=(
BOUNDED_SURFACE()
B_SPLINE_SURFACE(1,2,((#99373,#99374,#99375,#99376,#99377),(#99378,#99379,
#99380,#99381,#99382)),.UNSPECIFIED.,.F.,.F.,.F.)
B_SPLINE_SURFACE_WITH_KNOTS((2,2),(3,2,3),(0.,0.290405231142974),(0.40044464504501,
0.401042835325431,0.418415696246122),.UNSPECIFIED.)
GEOMETRIC_REPRESENTATION_ITEM()
RATIONAL_B_SPLINE_SURFACE(((0.988122504062136,0.988122504062136,0.988122504062136,
0.989520169850094,0.993884164197532),(0.988122504062136,0.988122504062136,
0.988122504062136,0.989520169850094,0.993884164197532)))
REPRESENTATION_ITEM('')
SURFACE()
);
#401=(
BOUNDED_SURFACE()
B_SPLINE_SURFACE(1,2,((#99384,#99385,#99386),(#99387,#99388,#99389)),
 .UNSPECIFIED.,.F.,.F.,.F.)
B_SPLINE_SURFACE_WITH_KNOTS((2,2),(3,3),(0.,0.289681084359927),(0.314840108491246,
0.332069149066804),.UNSPECIFIED.)
GEOMETRIC_REPRESENTATION_ITEM()
RATIONAL_B_SPLINE_SURFACE(((0.98789057959819,0.986774945528862,0.988576730109495),
(0.98789057959819,0.986774945528862,0.988576730109495)))
REPRESENTATION_ITEM('')
SURFACE()
);
#402=(
BOUNDED_SURFACE()
B_SPLINE_SURFACE(1,2,((#99398,#99399,#99400,#99401,#99402),(#99403,#99404,
#99405,#99406,#99407)),.UNSPECIFIED.,.F.,.F.,.F.)
B_SPLINE_SURFACE_WITH_KNOTS((2,2),(3,2,3),(0.,0.290405231138202),(0.400444645049142,
0.401042835325431,0.418415696246122),.UNSPECIFIED.)
GEOMETRIC_REPRESENTATION_ITEM()
RATIONAL_B_SPLINE_SURFACE(((0.988122504062135,0.988122504062135,0.988122504062135,
0.989520169850094,0.993884164197532),(0.988122504062135,0.988122504062135,
0.988122504062135,0.989520169850094,0.993884164197532)))
REPRESENTATION_ITEM('')
SURFACE()
);
#403=(
BOUNDED_SURFACE()
B_SPLINE_SURFACE(1,2,((#99409,#99410,#99411),(#99412,#99413,#99414)),
 .UNSPECIFIED.,.F.,.F.,.F.)
B_SPLINE_SURFACE_WITH_KNOTS((2,2),(3,3),(0.,0.289681084359929),(0.314840108491246,
0.332069149066804),.UNSPECIFIED.)
GEOMETRIC_REPRESENTATION_ITEM()
RATIONAL_B_SPLINE_SURFACE(((0.98789057959819,0.986774945528862,0.988576730109495),
(0.98789057959819,0.986774945528862,0.988576730109495)))
REPRESENTATION_ITEM('')
SURFACE()
);
#404=(
BOUNDED_SURFACE()
B_SPLINE_SURFACE(1,2,((#99423,#99424,#99425,#99426,#99427),(#99428,#99429,
#99430,#99431,#99432)),.UNSPECIFIED.,.F.,.F.,.F.)
B_SPLINE_SURFACE_WITH_KNOTS((2,2),(3,2,3),(0.,0.290405231155372),(0.400444645024719,
0.401042835325431,0.418415696246122),.UNSPECIFIED.)
GEOMETRIC_REPRESENTATION_ITEM()
RATIONAL_B_SPLINE_SURFACE(((0.988122504062136,0.988122504062136,0.988122504062136,
0.989520169850094,0.993884164197532),(0.988122504062136,0.988122504062136,
0.988122504062136,0.989520169850094,0.993884164197532)))
REPRESENTATION_ITEM('')
SURFACE()
);
#405=(
BOUNDED_SURFACE()
B_SPLINE_SURFACE(1,2,((#99434,#99435,#99436),(#99437,#99438,#99439)),
 .UNSPECIFIED.,.F.,.F.,.F.)
B_SPLINE_SURFACE_WITH_KNOTS((2,2),(3,3),(0.,0.289681084359924),(0.314840108491246,
0.332069149066804),.UNSPECIFIED.)
GEOMETRIC_REPRESENTATION_ITEM()
RATIONAL_B_SPLINE_SURFACE(((0.98789057959819,0.986774945528862,0.988576730109495),
(0.98789057959819,0.986774945528862,0.988576730109495)))
REPRESENTATION_ITEM('')
SURFACE()
);
#406=(
BOUNDED_SURFACE()
B_SPLINE_SURFACE(1,2,((#99448,#99449,#99450,#99451,#99452),(#99453,#99454,
#99455,#99456,#99457)),.UNSPECIFIED.,.F.,.F.,.F.)
B_SPLINE_SURFACE_WITH_KNOTS((2,2),(3,2,3),(0.,0.290405231151189),(0.40044464502924,
0.401042835325431,0.418415696246122),.UNSPECIFIED.)
GEOMETRIC_REPRESENTATION_ITEM()
RATIONAL_B_SPLINE_SURFACE(((0.988122504062136,0.988122504062136,0.988122504062136,
0.989520169850094,0.993884164197532),(0.988122504062136,0.988122504062136,
0.988122504062136,0.989520169850094,0.993884164197532)))
REPRESENTATION_ITEM('')
SURFACE()
);
#407=(
BOUNDED_SURFACE()
B_SPLINE_SURFACE(1,2,((#99459,#99460,#99461),(#99462,#99463,#99464)),
 .UNSPECIFIED.,.F.,.F.,.F.)
B_SPLINE_SURFACE_WITH_KNOTS((2,2),(3,3),(0.,0.289681084359917),(0.314840108491246,
0.332069149066804),.UNSPECIFIED.)
GEOMETRIC_REPRESENTATION_ITEM()
RATIONAL_B_SPLINE_SURFACE(((0.98789057959819,0.986774945528862,0.988576730109495),
(0.98789057959819,0.986774945528862,0.988576730109495)))
REPRESENTATION_ITEM('')
SURFACE()
);
#408=(
BOUNDED_SURFACE()
B_SPLINE_SURFACE(1,2,((#99473,#99474,#99475,#99476,#99477),(#99478,#99479,
#99480,#99481,#99482)),.UNSPECIFIED.,.F.,.F.,.F.)
B_SPLINE_SURFACE_WITH_KNOTS((2,2),(3,2,3),(0.,0.290405231148719),(0.400444645031816,
0.401042835325431,0.418415696246123),.UNSPECIFIED.)
GEOMETRIC_REPRESENTATION_ITEM()
RATIONAL_B_SPLINE_SURFACE(((0.988122504062136,0.988122504062136,0.988122504062136,
0.989520169850094,0.993884164197532),(0.988122504062136,0.988122504062136,
0.988122504062136,0.989520169850094,0.993884164197532)))
REPRESENTATION_ITEM('')
SURFACE()
);
#409=(
BOUNDED_SURFACE()
B_SPLINE_SURFACE(1,2,((#99484,#99485,#99486),(#99487,#99488,#99489)),
 .UNSPECIFIED.,.F.,.F.,.F.)
B_SPLINE_SURFACE_WITH_KNOTS((2,2),(3,3),(0.,0.289681084359925),(0.314840108491246,
0.332069149066812),.UNSPECIFIED.)
GEOMETRIC_REPRESENTATION_ITEM()
RATIONAL_B_SPLINE_SURFACE(((0.98789057959819,0.986774945528861,0.988576730109497),
(0.98789057959819,0.986774945528861,0.988576730109497)))
REPRESENTATION_ITEM('')
SURFACE()
);
#410=(
BOUNDED_SURFACE()
B_SPLINE_SURFACE(1,2,((#99498,#99499,#99500,#99501,#99502),(#99503,#99504,
#99505,#99506,#99507)),.UNSPECIFIED.,.F.,.F.,.F.)
B_SPLINE_SURFACE_WITH_KNOTS((2,2),(3,2,3),(0.,0.290405231137082),(0.400444645044425,
0.401042835325431,0.418415696246122),.UNSPECIFIED.)
GEOMETRIC_REPRESENTATION_ITEM()
RATIONAL_B_SPLINE_SURFACE(((0.988122504062135,0.988122504062135,0.988122504062135,
0.989520169850094,0.993884164197532),(0.988122504062135,0.988122504062135,
0.988122504062135,0.989520169850094,0.993884164197532)))
REPRESENTATION_ITEM('')
SURFACE()
);
#411=(
BOUNDED_SURFACE()
B_SPLINE_SURFACE(1,2,((#99509,#99510,#99511),(#99512,#99513,#99514)),
 .UNSPECIFIED.,.F.,.F.,.F.)
B_SPLINE_SURFACE_WITH_KNOTS((2,2),(3,3),(0.,0.289681084359928),(0.314840108491246,
0.332069149066804),.UNSPECIFIED.)
GEOMETRIC_REPRESENTATION_ITEM()
RATIONAL_B_SPLINE_SURFACE(((0.98789057959819,0.986774945528862,0.988576730109495),
(0.98789057959819,0.986774945528862,0.988576730109495)))
REPRESENTATION_ITEM('')
SURFACE()
);
#412=(
BOUNDED_SURFACE()
B_SPLINE_SURFACE(1,2,((#99523,#99524,#99525,#99526,#99527),(#99528,#99529,
#99530,#99531,#99532)),.UNSPECIFIED.,.F.,.F.,.F.)
B_SPLINE_SURFACE_WITH_KNOTS((2,2),(3,2,3),(0.,0.290405231145953),(0.400444645042899,
0.401042835325431,0.418415696246122),.UNSPECIFIED.)
GEOMETRIC_REPRESENTATION_ITEM()
RATIONAL_B_SPLINE_SURFACE(((0.988122504062136,0.988122504062136,0.988122504062136,
0.989520169850094,0.993884164197532),(0.988122504062135,0.988122504062135,
0.988122504062135,0.989520169850094,0.993884164197532)))
REPRESENTATION_ITEM('')
SURFACE()
);
#413=(
BOUNDED_SURFACE()
B_SPLINE_SURFACE(1,2,((#99534,#99535,#99536),(#99537,#99538,#99539)),
 .UNSPECIFIED.,.F.,.F.,.F.)
B_SPLINE_SURFACE_WITH_KNOTS((2,2),(3,3),(0.,0.289681084359932),(0.314840108491246,
0.332069149066804),.UNSPECIFIED.)
GEOMETRIC_REPRESENTATION_ITEM()
RATIONAL_B_SPLINE_SURFACE(((0.98789057959819,0.986774945528862,0.988576730109495),
(0.98789057959819,0.986774945528862,0.988576730109495)))
REPRESENTATION_ITEM('')
SURFACE()
);
#414=(
BOUNDED_SURFACE()
B_SPLINE_SURFACE(1,2,((#99548,#99549,#99550,#99551,#99552),(#99553,#99554,
#99555,#99556,#99557)),.UNSPECIFIED.,.F.,.F.,.F.)
B_SPLINE_SURFACE_WITH_KNOTS((2,2),(3,2,3),(0.,0.290405231150516),(0.400444645038493,
0.401042835325431,0.418415696246122),.UNSPECIFIED.)
GEOMETRIC_REPRESENTATION_ITEM()
RATIONAL_B_SPLINE_SURFACE(((0.988122504062136,0.988122504062136,0.988122504062136,
0.989520169850094,0.993884164197532),(0.988122504062135,0.988122504062135,
0.988122504062135,0.989520169850094,0.993884164197532)))
REPRESENTATION_ITEM('')
SURFACE()
);
#415=(
BOUNDED_SURFACE()
B_SPLINE_SURFACE(1,2,((#99559,#99560,#99561),(#99562,#99563,#99564)),
 .UNSPECIFIED.,.F.,.F.,.F.)
B_SPLINE_SURFACE_WITH_KNOTS((2,2),(3,3),(0.,0.289681084359926),(0.314840108491246,
0.332069149066806),.UNSPECIFIED.)
GEOMETRIC_REPRESENTATION_ITEM()
RATIONAL_B_SPLINE_SURFACE(((0.98789057959819,0.986774945528862,0.988576730109495),
(0.98789057959819,0.986774945528862,0.988576730109495)))
REPRESENTATION_ITEM('')
SURFACE()
);
#416=(
BOUNDED_SURFACE()
B_SPLINE_SURFACE(1,2,((#99573,#99574,#99575,#99576,#99577),(#99578,#99579,
#99580,#99581,#99582)),.UNSPECIFIED.,.F.,.F.,.F.)
B_SPLINE_SURFACE_WITH_KNOTS((2,2),(3,2,3),(0.,0.290405231145865),(0.400444645042583,
0.401042835325431,0.418415696246123),.UNSPECIFIED.)
GEOMETRIC_REPRESENTATION_ITEM()
RATIONAL_B_SPLINE_SURFACE(((0.988122504062135,0.988122504062135,0.988122504062135,
0.989520169850094,0.993884164197532),(0.988122504062136,0.988122504062136,
0.988122504062136,0.989520169850094,0.993884164197532)))
REPRESENTATION_ITEM('')
SURFACE()
);
#417=(
BOUNDED_SURFACE()
B_SPLINE_SURFACE(1,2,((#99584,#99585,#99586),(#99587,#99588,#99589)),
 .UNSPECIFIED.,.F.,.F.,.F.)
B_SPLINE_SURFACE_WITH_KNOTS((2,2),(3,3),(0.,0.289681084359922),(0.314840108491246,
0.332069149066804),.UNSPECIFIED.)
GEOMETRIC_REPRESENTATION_ITEM()
RATIONAL_B_SPLINE_SURFACE(((0.98789057959819,0.986774945528862,0.988576730109495),
(0.98789057959819,0.986774945528862,0.988576730109495)))
REPRESENTATION_ITEM('')
SURFACE()
);
#418=(
BOUNDED_SURFACE()
B_SPLINE_SURFACE(1,2,((#99598,#99599,#99600,#99601,#99602),(#99603,#99604,
#99605,#99606,#99607)),.UNSPECIFIED.,.F.,.F.,.F.)
B_SPLINE_SURFACE_WITH_KNOTS((2,2),(3,2,3),(0.,0.290405231151855),(0.400444645029575,
0.401042835325431,0.418415696246125),.UNSPECIFIED.)
GEOMETRIC_REPRESENTATION_ITEM()
RATIONAL_B_SPLINE_SURFACE(((0.988122504062136,0.988122504062136,0.988122504062136,
0.989520169850094,0.993884164197534),(0.988122504062136,0.988122504062136,
0.988122504062136,0.989520169850094,0.993884164197534)))
REPRESENTATION_ITEM('')
SURFACE()
);
#419=(
BOUNDED_SURFACE()
B_SPLINE_SURFACE(1,2,((#99609,#99610,#99611),(#99612,#99613,#99614)),
 .UNSPECIFIED.,.F.,.F.,.F.)
B_SPLINE_SURFACE_WITH_KNOTS((2,2),(3,3),(0.,0.289681084359918),(0.314840108491246,
0.332069149066807),.UNSPECIFIED.)
GEOMETRIC_REPRESENTATION_ITEM()
RATIONAL_B_SPLINE_SURFACE(((0.98789057959819,0.986774945528862,0.988576730109496),
(0.98789057959819,0.986774945528862,0.988576730109496)))
REPRESENTATION_ITEM('')
SURFACE()
);
#420=(
BOUNDED_SURFACE()
B_SPLINE_SURFACE(1,2,((#99623,#99624,#99625,#99626,#99627),(#99628,#99629,
#99630,#99631,#99632)),.UNSPECIFIED.,.F.,.F.,.F.)
B_SPLINE_SURFACE_WITH_KNOTS((2,2),(3,2,3),(0.,0.290405231144711),(0.400444645036177,
0.401042835325431,0.418415696246122),.UNSPECIFIED.)
GEOMETRIC_REPRESENTATION_ITEM()
RATIONAL_B_SPLINE_SURFACE(((0.988122504062135,0.988122504062135,0.988122504062135,
0.989520169850094,0.993884164197532),(0.988122504062135,0.988122504062135,
0.988122504062135,0.989520169850094,0.993884164197532)))
REPRESENTATION_ITEM('')
SURFACE()
);
#421=(
BOUNDED_SURFACE()
B_SPLINE_SURFACE(1,2,((#99634,#99635,#99636),(#99637,#99638,#99639)),
 .UNSPECIFIED.,.F.,.F.,.F.)
B_SPLINE_SURFACE_WITH_KNOTS((2,2),(3,3),(0.,0.289681084359923),(0.314840108491246,
0.332069149066806),.UNSPECIFIED.)
GEOMETRIC_REPRESENTATION_ITEM()
RATIONAL_B_SPLINE_SURFACE(((0.98789057959819,0.986774945528862,0.988576730109495),
(0.98789057959819,0.986774945528862,0.988576730109495)))
REPRESENTATION_ITEM('')
SURFACE()
);
#422=(
BOUNDED_SURFACE()
B_SPLINE_SURFACE(1,2,((#99648,#99649,#99650,#99651,#99652),(#99653,#99654,
#99655,#99656,#99657)),.UNSPECIFIED.,.F.,.F.,.F.)
B_SPLINE_SURFACE_WITH_KNOTS((2,2),(3,2,3),(0.,0.29040523112861),(0.400444645052479,
0.401042835325431,0.418415696246122),.UNSPECIFIED.)
GEOMETRIC_REPRESENTATION_ITEM()
RATIONAL_B_SPLINE_SURFACE(((0.988122504062135,0.988122504062135,0.988122504062135,
0.989520169850094,0.993884164197532),(0.988122504062135,0.988122504062135,
0.988122504062135,0.989520169850094,0.993884164197532)))
REPRESENTATION_ITEM('')
SURFACE()
);
#423=(
BOUNDED_SURFACE()
B_SPLINE_SURFACE(1,2,((#99659,#99660,#99661),(#99662,#99663,#99664)),
 .UNSPECIFIED.,.F.,.F.,.F.)
B_SPLINE_SURFACE_WITH_KNOTS((2,2),(3,3),(0.,0.289681084359918),(0.314840108491246,
0.332069149066804),.UNSPECIFIED.)
GEOMETRIC_REPRESENTATION_ITEM()
RATIONAL_B_SPLINE_SURFACE(((0.98789057959819,0.986774945528862,0.988576730109495),
(0.98789057959819,0.986774945528862,0.988576730109495)))
REPRESENTATION_ITEM('')
SURFACE()
);
#424=(
BOUNDED_SURFACE()
B_SPLINE_SURFACE(1,2,((#99673,#99674,#99675,#99676,#99677),(#99678,#99679,
#99680,#99681,#99682)),.UNSPECIFIED.,.F.,.F.,.F.)
B_SPLINE_SURFACE_WITH_KNOTS((2,2),(3,2,3),(0.,0.290405231116345),(0.400444645064969,
0.401042835325431,0.418415696246122),.UNSPECIFIED.)
GEOMETRIC_REPRESENTATION_ITEM()
RATIONAL_B_SPLINE_SURFACE(((0.988122504062136,0.988122504062136,0.988122504062136,
0.989520169850094,0.993884164197532),(0.988122504062136,0.988122504062136,
0.988122504062136,0.989520169850094,0.993884164197532)))
REPRESENTATION_ITEM('')
SURFACE()
);
#425=(
BOUNDED_SURFACE()
B_SPLINE_SURFACE(1,2,((#99684,#99685,#99686),(#99687,#99688,#99689)),
 .UNSPECIFIED.,.F.,.F.,.F.)
B_SPLINE_SURFACE_WITH_KNOTS((2,2),(3,3),(0.,0.289681084359931),(0.314840108491246,
0.332069149066804),.UNSPECIFIED.)
GEOMETRIC_REPRESENTATION_ITEM()
RATIONAL_B_SPLINE_SURFACE(((0.98789057959819,0.986774945528862,0.988576730109495),
(0.98789057959819,0.986774945528862,0.988576730109495)))
REPRESENTATION_ITEM('')
SURFACE()
);
#426=(
BOUNDED_SURFACE()
B_SPLINE_SURFACE(1,2,((#99691,#99692,#99693),(#99694,#99695,#99696)),
 .UNSPECIFIED.,.F.,.F.,.F.)
B_SPLINE_SURFACE_WITH_KNOTS((2,2),(3,3),(0.,0.289807040992008),(0.366820493751253,
0.384035903515169),.UNSPECIFIED.)
GEOMETRIC_REPRESENTATION_ITEM()
RATIONAL_B_SPLINE_SURFACE(((0.994126602224873,0.989721266390694,0.988228734781998),
(0.994126602224873,0.989721266390694,0.988228734781998)))
REPRESENTATION_ITEM('')
SURFACE()
);
#427=(
BOUNDED_SURFACE()
B_SPLINE_SURFACE(1,2,((#99725,#99726,#99727,#99728,#99729,#99730,#99731),
(#99732,#99733,#99734,#99735,#99736,#99737,#99738)),.UNSPECIFIED.,.F.,.F.,
 .F.)
B_SPLINE_SURFACE_WITH_KNOTS((2,2),(3,2,2,3),(0.,0.289681084359932),(0.34926499147441,
0.357142857142857,0.366820493751254,0.366996048774023),.UNSPECIFIED.)
GEOMETRIC_REPRESENTATION_ITEM()
RATIONAL_B_SPLINE_SURFACE(((0.995079542144874,0.997234796441972,1.,0.996603060231146,
0.994126602224873,0.994126602224873,0.994126602224873),(0.995079542144874,
0.997234796441972,1.,0.996603060231146,0.994126602224873,0.994126602224873,
0.994126602224873)))
REPRESENTATION_ITEM('')
SURFACE()
);
#428=(
BOUNDED_SURFACE()
B_SPLINE_SURFACE(1,2,((#99740,#99741,#99742),(#99743,#99744,#99745)),
 .UNSPECIFIED.,.F.,.F.,.F.)
B_SPLINE_SURFACE_WITH_KNOTS((2,2),(3,3),(0.,0.289807040992861),(0.366820493751253,
0.384035903515169),.UNSPECIFIED.)
GEOMETRIC_REPRESENTATION_ITEM()
RATIONAL_B_SPLINE_SURFACE(((0.994126602224873,0.989721266390694,0.988228734781998),
(0.994126602224873,0.989721266390694,0.988228734781998)))
REPRESENTATION_ITEM('')
SURFACE()
);
#429=(
BOUNDED_SURFACE()
B_SPLINE_SURFACE(1,2,((#99774,#99775,#99776,#99777,#99778,#99779,#99780),
(#99781,#99782,#99783,#99784,#99785,#99786,#99787)),.UNSPECIFIED.,.F.,.F.,
 .F.)
B_SPLINE_SURFACE_WITH_KNOTS((2,2),(3,2,2,3),(0.,0.289681084360137),(0.34926499147441,
0.357142857142857,0.366820493751255,0.366996048774024),.UNSPECIFIED.)
GEOMETRIC_REPRESENTATION_ITEM()
RATIONAL_B_SPLINE_SURFACE(((0.995079542144874,0.997234796441972,1.,0.996603060231146,
0.994126602224872,0.994126602224872,0.994126602224872),(0.995079542144874,
0.997234796441972,1.,0.996603060231146,0.994126602224872,0.994126602224872,
0.994126602224872)))
REPRESENTATION_ITEM('')
SURFACE()
);
#430=(
BOUNDED_SURFACE()
B_SPLINE_SURFACE(1,2,((#99789,#99790,#99791),(#99792,#99793,#99794)),
 .UNSPECIFIED.,.F.,.F.,.F.)
B_SPLINE_SURFACE_WITH_KNOTS((2,2),(3,3),(0.,0.289807040992678),(0.366820493751253,
0.384035903515169),.UNSPECIFIED.)
GEOMETRIC_REPRESENTATION_ITEM()
RATIONAL_B_SPLINE_SURFACE(((0.994126602224873,0.989721266390694,0.988228734781998),
(0.994126602224873,0.989721266390694,0.988228734781998)))
REPRESENTATION_ITEM('')
SURFACE()
);
#431=(
BOUNDED_SURFACE()
B_SPLINE_SURFACE(1,2,((#99823,#99824,#99825,#99826,#99827,#99828,#99829),
(#99830,#99831,#99832,#99833,#99834,#99835,#99836)),.UNSPECIFIED.,.F.,.F.,
 .F.)
B_SPLINE_SURFACE_WITH_KNOTS((2,2),(3,2,2,3),(0.,0.289681084360355),(0.34926499147441,
0.357142857142857,0.366820493751254,0.366996048774023),.UNSPECIFIED.)
GEOMETRIC_REPRESENTATION_ITEM()
RATIONAL_B_SPLINE_SURFACE(((0.995079542144874,0.997234796441972,1.,0.996603060231146,
0.994126602224873,0.994126602224873,0.994126602224873),(0.995079542144874,
0.997234796441972,1.,0.996603060231146,0.994126602224873,0.994126602224873,
0.994126602224873)))
REPRESENTATION_ITEM('')
SURFACE()
);
#432=(
BOUNDED_SURFACE()
B_SPLINE_SURFACE(1,2,((#99838,#99839,#99840),(#99841,#99842,#99843)),
 .UNSPECIFIED.,.F.,.F.,.F.)
B_SPLINE_SURFACE_WITH_KNOTS((2,2),(3,3),(0.,0.289807040992652),(0.366820493751253,
0.384035903515169),.UNSPECIFIED.)
GEOMETRIC_REPRESENTATION_ITEM()
RATIONAL_B_SPLINE_SURFACE(((0.994126602224873,0.989721266390694,0.988228734781998),
(0.994126602224873,0.989721266390694,0.988228734781998)))
REPRESENTATION_ITEM('')
SURFACE()
);
#433=(
BOUNDED_SURFACE()
B_SPLINE_SURFACE(1,2,((#99872,#99873,#99874,#99875,#99876,#99877,#99878),
(#99879,#99880,#99881,#99882,#99883,#99884,#99885)),.UNSPECIFIED.,.F.,.F.,
 .F.)
B_SPLINE_SURFACE_WITH_KNOTS((2,2),(3,2,2,3),(0.,0.289681084359916),(0.34926499147441,
0.357142857142857,0.366820493751254,0.366996048774023),.UNSPECIFIED.)
GEOMETRIC_REPRESENTATION_ITEM()
RATIONAL_B_SPLINE_SURFACE(((0.995079542144874,0.997234796441972,1.,0.996603060231146,
0.994126602224873,0.994126602224873,0.994126602224873),(0.995079542144874,
0.997234796441972,1.,0.996603060231146,0.994126602224873,0.994126602224873,
0.994126602224873)))
REPRESENTATION_ITEM('')
SURFACE()
);
#434=(
BOUNDED_SURFACE()
B_SPLINE_SURFACE(1,2,((#99887,#99888,#99889),(#99890,#99891,#99892)),
 .UNSPECIFIED.,.F.,.F.,.F.)
B_SPLINE_SURFACE_WITH_KNOTS((2,2),(3,3),(0.,0.289807040992801),(0.366820493751253,
0.384035903515169),.UNSPECIFIED.)
GEOMETRIC_REPRESENTATION_ITEM()
RATIONAL_B_SPLINE_SURFACE(((0.994126602224873,0.989721266390694,0.988228734781998),
(0.994126602224873,0.989721266390694,0.988228734781998)))
REPRESENTATION_ITEM('')
SURFACE()
);
#435=(
BOUNDED_SURFACE()
B_SPLINE_SURFACE(1,2,((#99921,#99922,#99923,#99924,#99925,#99926,#99927),
(#99928,#99929,#99930,#99931,#99932,#99933,#99934)),.UNSPECIFIED.,.F.,.F.,
 .F.)
B_SPLINE_SURFACE_WITH_KNOTS((2,2),(3,2,2,3),(0.,0.289681084359922),(0.34926499147441,
0.357142857142857,0.366820493751254,0.366996048774023),.UNSPECIFIED.)
GEOMETRIC_REPRESENTATION_ITEM()
RATIONAL_B_SPLINE_SURFACE(((0.995079542144874,0.997234796441972,1.,0.996603060231146,
0.994126602224873,0.994126602224873,0.994126602224873),(0.995079542144874,
0.997234796441972,1.,0.996603060231146,0.994126602224873,0.994126602224873,
0.994126602224873)))
REPRESENTATION_ITEM('')
SURFACE()
);
#436=(
BOUNDED_SURFACE()
B_SPLINE_SURFACE(1,2,((#99936,#99937,#99938),(#99939,#99940,#99941)),
 .UNSPECIFIED.,.F.,.F.,.F.)
B_SPLINE_SURFACE_WITH_KNOTS((2,2),(3,3),(0.,0.289807040992325),(0.366820493751253,
0.384035903515169),.UNSPECIFIED.)
GEOMETRIC_REPRESENTATION_ITEM()
RATIONAL_B_SPLINE_SURFACE(((0.994126602224873,0.989721266390694,0.988228734781998),
(0.994126602224873,0.989721266390694,0.988228734781998)))
REPRESENTATION_ITEM('')
SURFACE()
);
#437=(
BOUNDED_SURFACE()
B_SPLINE_SURFACE(1,2,((#99970,#99971,#99972,#99973,#99974,#99975,#99976),
(#99977,#99978,#99979,#99980,#99981,#99982,#99983)),.UNSPECIFIED.,.F.,.F.,
 .F.)
B_SPLINE_SURFACE_WITH_KNOTS((2,2),(3,2,2,3),(0.,0.289681084360531),(0.3492649914744,
0.357142857142857,0.366820493751254,0.366996048774023),.UNSPECIFIED.)
GEOMETRIC_REPRESENTATION_ITEM()
RATIONAL_B_SPLINE_SURFACE(((0.995079542144869,0.997234796441969,1.,0.996603060231146,
0.994126602224873,0.994126602224873,0.994126602224873),(0.995079542144869,
0.997234796441969,1.,0.996603060231146,0.994126602224873,0.994126602224873,
0.994126602224873)))
REPRESENTATION_ITEM('')
SURFACE()
);
#438=(
BOUNDED_SURFACE()
B_SPLINE_SURFACE(1,2,((#99985,#99986,#99987),(#99988,#99989,#99990)),
 .UNSPECIFIED.,.F.,.F.,.F.)
B_SPLINE_SURFACE_WITH_KNOTS((2,2),(3,3),(0.,0.289807040992452),(0.366820493751253,
0.384035903515169),.UNSPECIFIED.)
GEOMETRIC_REPRESENTATION_ITEM()
RATIONAL_B_SPLINE_SURFACE(((0.994126602224873,0.989721266390694,0.988228734781998),
(0.994126602224873,0.989721266390694,0.988228734781998)))
REPRESENTATION_ITEM('')
SURFACE()
);
#439=(
BOUNDED_SURFACE()
B_SPLINE_SURFACE(1,2,((#100019,#100020,#100021,#100022,#100023,#100024,
#100025),(#100026,#100027,#100028,#100029,#100030,#100031,#100032)),
 .UNSPECIFIED.,.F.,.F.,.F.)
B_SPLINE_SURFACE_WITH_KNOTS((2,2),(3,2,2,3),(0.,0.289681084359929),(0.34926499147441,
0.357142857142857,0.366820493751254,0.366996048774023),.UNSPECIFIED.)
GEOMETRIC_REPRESENTATION_ITEM()
RATIONAL_B_SPLINE_SURFACE(((0.995079542144874,0.997234796441972,1.,0.996603060231146,
0.994126602224873,0.994126602224873,0.994126602224873),(0.995079542144874,
0.997234796441972,1.,0.996603060231146,0.994126602224873,0.994126602224873,
0.994126602224873)))
REPRESENTATION_ITEM('')
SURFACE()
);
#440=(
BOUNDED_SURFACE()
B_SPLINE_SURFACE(1,2,((#100034,#100035,#100036),(#100037,#100038,#100039)),
 .UNSPECIFIED.,.F.,.F.,.F.)
B_SPLINE_SURFACE_WITH_KNOTS((2,2),(3,3),(0.,0.289807040992693),(0.366820493751253,
0.384035903515169),.UNSPECIFIED.)
GEOMETRIC_REPRESENTATION_ITEM()
RATIONAL_B_SPLINE_SURFACE(((0.994126602224873,0.989721266390694,0.988228734781998),
(0.994126602224873,0.989721266390694,0.988228734781998)))
REPRESENTATION_ITEM('')
SURFACE()
);
#441=(
BOUNDED_SURFACE()
B_SPLINE_SURFACE(1,2,((#100068,#100069,#100070,#100071,#100072,#100073,
#100074),(#100075,#100076,#100077,#100078,#100079,#100080,#100081)),
 .UNSPECIFIED.,.F.,.F.,.F.)
B_SPLINE_SURFACE_WITH_KNOTS((2,2),(3,2,2,3),(-0.000247526158567017,0.289681084359924),
(0.349122170180809,0.357142857142857,0.366820493751254,0.367068020353655),
 .UNSPECIFIED.)
GEOMETRIC_REPRESENTATION_ITEM()
RATIONAL_B_SPLINE_SURFACE(((0.995001595513646,0.997184664849756,1.,0.996603060231146,
0.994126602224873,0.994126602224873,0.994126602224873),(0.995001595513646,
0.997184664849755,1.,0.996603060231146,0.994126602224873,0.994126602224873,
0.994126602224873)))
REPRESENTATION_ITEM('')
SURFACE()
);
#442=(
BOUNDED_SURFACE()
B_SPLINE_SURFACE(1,2,((#100083,#100084,#100085),(#100086,#100087,#100088)),
 .UNSPECIFIED.,.F.,.F.,.F.)
B_SPLINE_SURFACE_WITH_KNOTS((2,2),(3,3),(0.,0.289807040992909),(0.366820493751253,
0.384035903515169),.UNSPECIFIED.)
GEOMETRIC_REPRESENTATION_ITEM()
RATIONAL_B_SPLINE_SURFACE(((0.994126602224873,0.989721266390694,0.988228734781998),
(0.994126602224873,0.989721266390694,0.988228734781998)))
REPRESENTATION_ITEM('')
SURFACE()
);
#443=(
BOUNDED_SURFACE()
B_SPLINE_SURFACE(1,2,((#100117,#100118,#100119,#100120,#100121,#100122,
#100123),(#100124,#100125,#100126,#100127,#100128,#100129,#100130)),
 .UNSPECIFIED.,.F.,.F.,.F.)
B_SPLINE_SURFACE_WITH_KNOTS((2,2),(3,2,2,3),(0.,0.28968108435992),(0.34926499147441,
0.357142857142857,0.366820493751254,0.366996048774023),.UNSPECIFIED.)
GEOMETRIC_REPRESENTATION_ITEM()
RATIONAL_B_SPLINE_SURFACE(((0.995079542144874,0.997234796441972,1.,0.996603060231146,
0.994126602224873,0.994126602224873,0.994126602224873),(0.995079542144874,
0.997234796441972,1.,0.996603060231146,0.994126602224873,0.994126602224873,
0.994126602224873)))
REPRESENTATION_ITEM('')
SURFACE()
);
#444=(
BOUNDED_SURFACE()
B_SPLINE_SURFACE(1,2,((#100132,#100133,#100134),(#100135,#100136,#100137)),
 .UNSPECIFIED.,.F.,.F.,.F.)
B_SPLINE_SURFACE_WITH_KNOTS((2,2),(3,3),(0.,0.28980704099176),(0.366820493751253,
0.384035903515169),.UNSPECIFIED.)
GEOMETRIC_REPRESENTATION_ITEM()
RATIONAL_B_SPLINE_SURFACE(((0.994126602224873,0.989721266390694,0.988228734781998),
(0.994126602224873,0.989721266390694,0.988228734781998)))
REPRESENTATION_ITEM('')
SURFACE()
);
#445=(
BOUNDED_SURFACE()
B_SPLINE_SURFACE(1,2,((#100166,#100167,#100168,#100169,#100170,#100171,
#100172),(#100173,#100174,#100175,#100176,#100177,#100178,#100179)),
 .UNSPECIFIED.,.F.,.F.,.F.)
B_SPLINE_SURFACE_WITH_KNOTS((2,2),(3,2,2,3),(0.,0.289681084359916),(0.34926499147441,
0.357142857142857,0.366820493751263,0.366996048774032),.UNSPECIFIED.)
GEOMETRIC_REPRESENTATION_ITEM()
RATIONAL_B_SPLINE_SURFACE(((0.995079542144874,0.997234796441972,1.,0.996603060231143,
0.994126602224868,0.994126602224868,0.994126602224868),(0.995079542144874,
0.997234796441972,1.,0.996603060231143,0.994126602224868,0.994126602224868,
0.994126602224868)))
REPRESENTATION_ITEM('')
SURFACE()
);
#446=(
BOUNDED_SURFACE()
B_SPLINE_SURFACE(1,2,((#100181,#100182,#100183),(#100184,#100185,#100186)),
 .UNSPECIFIED.,.F.,.F.,.F.)
B_SPLINE_SURFACE_WITH_KNOTS((2,2),(3,3),(0.,0.289807040991715),(0.366820493751253,
0.384035903515169),.UNSPECIFIED.)
GEOMETRIC_REPRESENTATION_ITEM()
RATIONAL_B_SPLINE_SURFACE(((0.994126602224873,0.989721266390694,0.988228734781998),
(0.994126602224873,0.989721266390694,0.988228734781998)))
REPRESENTATION_ITEM('')
SURFACE()
);
#447=(
BOUNDED_SURFACE()
B_SPLINE_SURFACE(1,2,((#100215,#100216,#100217,#100218,#100219,#100220,
#100221),(#100222,#100223,#100224,#100225,#100226,#100227,#100228)),
 .UNSPECIFIED.,.F.,.F.,.F.)
B_SPLINE_SURFACE_WITH_KNOTS((2,2),(3,2,2,3),(0.,0.289681084359924),(0.34926499147441,
0.357142857142857,0.366820493751263,0.366996048774032),.UNSPECIFIED.)
GEOMETRIC_REPRESENTATION_ITEM()
RATIONAL_B_SPLINE_SURFACE(((0.995079542144874,0.997234796441972,1.,0.996603060231143,
0.994126602224868,0.994126602224868,0.994126602224868),(0.995079542144874,
0.997234796441972,1.,0.996603060231143,0.994126602224868,0.994126602224868,
0.994126602224868)))
REPRESENTATION_ITEM('')
SURFACE()
);
#448=(
BOUNDED_SURFACE()
B_SPLINE_SURFACE(1,2,((#100230,#100231,#100232),(#100233,#100234,#100235)),
 .UNSPECIFIED.,.F.,.F.,.F.)
B_SPLINE_SURFACE_WITH_KNOTS((2,2),(3,3),(0.,0.289807040991572),(0.366820493751253,
0.384035903515169),.UNSPECIFIED.)
GEOMETRIC_REPRESENTATION_ITEM()
RATIONAL_B_SPLINE_SURFACE(((0.994126602224873,0.989721266390694,0.988228734781998),
(0.994126602224873,0.989721266390694,0.988228734781998)))
REPRESENTATION_ITEM('')
SURFACE()
);
#449=(
BOUNDED_SURFACE()
B_SPLINE_SURFACE(1,2,((#100264,#100265,#100266,#100267,#100268,#100269,
#100270),(#100271,#100272,#100273,#100274,#100275,#100276,#100277)),
 .UNSPECIFIED.,.F.,.F.,.F.)
B_SPLINE_SURFACE_WITH_KNOTS((2,2),(3,2,2,3),(0.,0.289681084360495),(0.34926499147441,
0.357142857142857,0.366820493751263,0.366996048774032),.UNSPECIFIED.)
GEOMETRIC_REPRESENTATION_ITEM()
RATIONAL_B_SPLINE_SURFACE(((0.995079542144874,0.997234796441972,1.,0.996603060231143,
0.994126602224868,0.994126602224868,0.994126602224868),(0.995079542144874,
0.997234796441972,1.,0.996603060231143,0.994126602224868,0.994126602224868,
0.994126602224868)))
REPRESENTATION_ITEM('')
SURFACE()
);
#450=(
BOUNDED_SURFACE()
B_SPLINE_SURFACE(1,2,((#100279,#100280,#100281),(#100282,#100283,#100284)),
 .UNSPECIFIED.,.F.,.F.,.F.)
B_SPLINE_SURFACE_WITH_KNOTS((2,2),(3,3),(0.,0.289807040991562),(0.366820493751253,
0.384035903515169),.UNSPECIFIED.)
GEOMETRIC_REPRESENTATION_ITEM()
RATIONAL_B_SPLINE_SURFACE(((0.994126602224873,0.989721266390694,0.988228734781998),
(0.994126602224873,0.989721266390694,0.988228734781998)))
REPRESENTATION_ITEM('')
SURFACE()
);
#451=(
BOUNDED_SURFACE()
B_SPLINE_SURFACE(1,2,((#100313,#100314,#100315,#100316,#100317,#100318,
#100319),(#100320,#100321,#100322,#100323,#100324,#100325,#100326)),
 .UNSPECIFIED.,.F.,.F.,.F.)
B_SPLINE_SURFACE_WITH_KNOTS((2,2),(3,2,2,3),(-0.000247526265803812,0.289681084359927),
(0.349122170275924,0.357142857142857,0.366820493751263,0.367068020291019),
 .UNSPECIFIED.)
GEOMETRIC_REPRESENTATION_ITEM()
RATIONAL_B_SPLINE_SURFACE(((0.995001595565422,0.997184664883142,1.,0.996603060231143,
0.994126602224868,0.994126602224868,0.994126602224868),(0.995001595565422,
0.997184664883142,1.,0.996603060231143,0.994126602224868,0.994126602224868,
0.994126602224868)))
REPRESENTATION_ITEM('')
SURFACE()
);
#452=(
BOUNDED_SURFACE()
B_SPLINE_SURFACE(1,2,((#100328,#100329,#100330),(#100331,#100332,#100333)),
 .UNSPECIFIED.,.F.,.F.,.F.)
B_SPLINE_SURFACE_WITH_KNOTS((2,2),(3,3),(0.,0.289807040991566),(0.366820493751253,
0.384035903515169),.UNSPECIFIED.)
GEOMETRIC_REPRESENTATION_ITEM()
RATIONAL_B_SPLINE_SURFACE(((0.994126602224873,0.989721266390694,0.988228734781998),
(0.994126602224873,0.989721266390694,0.988228734781998)))
REPRESENTATION_ITEM('')
SURFACE()
);
#453=(
BOUNDED_SURFACE()
B_SPLINE_SURFACE(1,2,((#100362,#100363,#100364,#100365,#100366,#100367,
#100368),(#100369,#100370,#100371,#100372,#100373,#100374,#100375)),
 .UNSPECIFIED.,.F.,.F.,.F.)
B_SPLINE_SURFACE_WITH_KNOTS((2,2),(3,2,2,3),(-0.000247526295446904,0.289681084359932),
(0.349122170227907,0.357142857142857,0.366820493751263,0.367068020309611),
 .UNSPECIFIED.)
GEOMETRIC_REPRESENTATION_ITEM()
RATIONAL_B_SPLINE_SURFACE(((0.995001595539283,0.997184664866287,1.,0.996603060231143,
0.994126602224868,0.994126602224868,0.994126602224868),(0.995001595539283,
0.997184664866287,1.,0.996603060231143,0.994126602224868,0.994126602224868,
0.994126602224868)))
REPRESENTATION_ITEM('')
SURFACE()
);
#454=(
BOUNDED_SURFACE()
B_SPLINE_SURFACE(1,2,((#100377,#100378,#100379),(#100380,#100381,#100382)),
 .UNSPECIFIED.,.F.,.F.,.F.)
B_SPLINE_SURFACE_WITH_KNOTS((2,2),(3,3),(0.,0.289807040991565),(0.366820493751253,
0.384035903515169),.UNSPECIFIED.)
GEOMETRIC_REPRESENTATION_ITEM()
RATIONAL_B_SPLINE_SURFACE(((0.994126602224873,0.989721266390694,0.988228734781998),
(0.994126602224873,0.989721266390694,0.988228734781998)))
REPRESENTATION_ITEM('')
SURFACE()
);
#455=(
BOUNDED_SURFACE()
B_SPLINE_SURFACE(1,2,((#100390,#100391,#100392,#100393,#100394,#100395,
#100396),(#100397,#100398,#100399,#100400,#100401,#100402,#100403)),
 .UNSPECIFIED.,.F.,.F.,.F.)
B_SPLINE_SURFACE_WITH_KNOTS((2,2),(3,2,2,3),(0.,0.289681084359918),(0.34926499147441,
0.357142857142857,0.366820493751263,0.366996048774032),.UNSPECIFIED.)
GEOMETRIC_REPRESENTATION_ITEM()
RATIONAL_B_SPLINE_SURFACE(((0.995079542144874,0.997234796441972,1.,0.996603060231143,
0.994126602224868,0.994126602224868,0.994126602224868),(0.995079542144874,
0.997234796441972,1.,0.996603060231143,0.994126602224868,0.994126602224868,
0.994126602224868)))
REPRESENTATION_ITEM('')
SURFACE()
);
#456=(
BOUNDED_SURFACE()
B_SPLINE_SURFACE(1,2,((#100405,#100406,#100407),(#100408,#100409,#100410)),
 .UNSPECIFIED.,.F.,.F.,.F.)
B_SPLINE_SURFACE_WITH_KNOTS((2,2),(3,3),(0.,0.289807040991565),(0.366820493751253,
0.384035903515169),.UNSPECIFIED.)
GEOMETRIC_REPRESENTATION_ITEM()
RATIONAL_B_SPLINE_SURFACE(((0.994126602224873,0.989721266390694,0.988228734781998),
(0.994126602224873,0.989721266390694,0.988228734781998)))
REPRESENTATION_ITEM('')
SURFACE()
);
#457=(
BOUNDED_SURFACE()
B_SPLINE_SURFACE(1,2,((#100439,#100440,#100441,#100442,#100443,#100444,
#100445),(#100446,#100447,#100448,#100449,#100450,#100451,#100452)),
 .UNSPECIFIED.,.F.,.F.,.F.)
B_SPLINE_SURFACE_WITH_KNOTS((2,2),(3,2,2,3),(0.,0.289681084359923),(0.34926499147441,
0.357142857142857,0.366820493751263,0.366996048774032),.UNSPECIFIED.)
GEOMETRIC_REPRESENTATION_ITEM()
RATIONAL_B_SPLINE_SURFACE(((0.995079542144874,0.997234796441972,1.,0.996603060231143,
0.994126602224868,0.994126602224868,0.994126602224868),(0.995079542144874,
0.997234796441972,1.,0.996603060231143,0.994126602224868,0.994126602224868,
0.994126602224868)))
REPRESENTATION_ITEM('')
SURFACE()
);
#458=(
BOUNDED_SURFACE()
B_SPLINE_SURFACE(1,2,((#100454,#100455,#100456),(#100457,#100458,#100459)),
 .UNSPECIFIED.,.F.,.F.,.F.)
B_SPLINE_SURFACE_WITH_KNOTS((2,2),(3,3),(0.,0.289807040991669),(0.366820493751253,
0.384035903515169),.UNSPECIFIED.)
GEOMETRIC_REPRESENTATION_ITEM()
RATIONAL_B_SPLINE_SURFACE(((0.994126602224873,0.989721266390694,0.988228734781998),
(0.994126602224873,0.989721266390694,0.988228734781998)))
REPRESENTATION_ITEM('')
SURFACE()
);
#459=(
BOUNDED_SURFACE()
B_SPLINE_SURFACE(1,2,((#100488,#100489,#100490,#100491,#100492,#100493,
#100494),(#100495,#100496,#100497,#100498,#100499,#100500,#100501)),
 .UNSPECIFIED.,.F.,.F.,.F.)
B_SPLINE_SURFACE_WITH_KNOTS((2,2),(3,2,2,3),(-0.00024752625948705,0.289681084359921),
(0.349122170220907,0.357142857142857,0.366820493751263,0.367068020290794),
 .UNSPECIFIED.)
GEOMETRIC_REPRESENTATION_ITEM()
RATIONAL_B_SPLINE_SURFACE(((0.995001595535473,0.99718466486383,1.,0.996603060231143,
0.994126602224868,0.994126602224868,0.994126602224868),(0.995001595535473,
0.99718466486383,1.,0.996603060231143,0.994126602224868,0.994126602224868,
0.994126602224868)))
REPRESENTATION_ITEM('')
SURFACE()
);
#460=(
BOUNDED_SURFACE()
B_SPLINE_SURFACE(1,2,((#100503,#100504,#100505),(#100506,#100507,#100508)),
 .UNSPECIFIED.,.F.,.F.,.F.)
B_SPLINE_SURFACE_WITH_KNOTS((2,2),(3,3),(0.,0.289807040992969),(0.366820493751253,
0.384035903515169),.UNSPECIFIED.)
GEOMETRIC_REPRESENTATION_ITEM()
RATIONAL_B_SPLINE_SURFACE(((0.994126602224873,0.989721266390694,0.988228734781998),
(0.994126602224873,0.989721266390694,0.988228734781998)))
REPRESENTATION_ITEM('')
SURFACE()
);
#461=(
BOUNDED_SURFACE()
B_SPLINE_SURFACE(1,2,((#100537,#100538,#100539,#100540,#100541,#100542,
#100543),(#100544,#100545,#100546,#100547,#100548,#100549,#100550)),
 .UNSPECIFIED.,.F.,.F.,.F.)
B_SPLINE_SURFACE_WITH_KNOTS((2,2),(3,2,2,3),(0.,0.28968108435992),(0.34926499147441,
0.357142857142857,0.366820493751263,0.366996048774032),.UNSPECIFIED.)
GEOMETRIC_REPRESENTATION_ITEM()
RATIONAL_B_SPLINE_SURFACE(((0.995079542144874,0.997234796441972,1.,0.996603060231143,
0.994126602224868,0.994126602224868,0.994126602224868),(0.995079542144874,
0.997234796441972,1.,0.996603060231143,0.994126602224868,0.994126602224868,
0.994126602224868)))
REPRESENTATION_ITEM('')
SURFACE()
);
#462=(
BOUNDED_SURFACE()
B_SPLINE_SURFACE(1,2,((#100552,#100553,#100554),(#100555,#100556,#100557)),
 .UNSPECIFIED.,.F.,.F.,.F.)
B_SPLINE_SURFACE_WITH_KNOTS((2,2),(3,3),(0.,0.289807040991813),(0.366820493751013,
0.384035903515171),.UNSPECIFIED.)
GEOMETRIC_REPRESENTATION_ITEM()
RATIONAL_B_SPLINE_SURFACE(((0.994126602224996,0.989721266390715,0.988228734781998),
(0.994126602224996,0.989721266390715,0.988228734781998)))
REPRESENTATION_ITEM('')
SURFACE()
);
#463=(
BOUNDED_SURFACE()
B_SPLINE_SURFACE(1,2,((#100586,#100587,#100588,#100589,#100590,#100591,
#100592),(#100593,#100594,#100595,#100596,#100597,#100598,#100599)),
 .UNSPECIFIED.,.F.,.F.,.F.)
B_SPLINE_SURFACE_WITH_KNOTS((2,2),(3,2,2,3),(0.,0.289681084359919),(0.34926499147441,
0.357142857142857,0.366820493751263,0.366996048774032),.UNSPECIFIED.)
GEOMETRIC_REPRESENTATION_ITEM()
RATIONAL_B_SPLINE_SURFACE(((0.995079542144874,0.997234796441972,1.,0.996603060231143,
0.994126602224868,0.994126602224868,0.994126602224868),(0.995079542144874,
0.997234796441972,1.,0.996603060231143,0.994126602224868,0.994126602224868,
0.994126602224868)))
REPRESENTATION_ITEM('')
SURFACE()
);
#464=(
BOUNDED_SURFACE()
B_SPLINE_SURFACE(1,2,((#100601,#100602,#100603),(#100604,#100605,#100606)),
 .UNSPECIFIED.,.F.,.F.,.F.)
B_SPLINE_SURFACE_WITH_KNOTS((2,2),(3,3),(0.,0.289807040991562),(0.366820493751253,
0.384035903515169),.UNSPECIFIED.)
GEOMETRIC_REPRESENTATION_ITEM()
RATIONAL_B_SPLINE_SURFACE(((0.994126602224873,0.989721266390694,0.988228734781998),
(0.994126602224873,0.989721266390694,0.988228734781998)))
REPRESENTATION_ITEM('')
SURFACE()
);
#465=(
BOUNDED_SURFACE()
B_SPLINE_SURFACE(1,2,((#100635,#100636,#100637,#100638,#100639,#100640,
#100641),(#100642,#100643,#100644,#100645,#100646,#100647,#100648)),
 .UNSPECIFIED.,.F.,.F.,.F.)
B_SPLINE_SURFACE_WITH_KNOTS((2,2),(3,2,2,3),(0.,0.289681084359922),(0.34926499147441,
0.357142857142857,0.366820493751263,0.366996048774032),.UNSPECIFIED.)
GEOMETRIC_REPRESENTATION_ITEM()
RATIONAL_B_SPLINE_SURFACE(((0.995079542144874,0.997234796441972,1.,0.996603060231143,
0.994126602224868,0.994126602224868,0.994126602224868),(0.995079542144874,
0.997234796441972,1.,0.996603060231143,0.994126602224868,0.994126602224868,
0.994126602224868)))
REPRESENTATION_ITEM('')
SURFACE()
);
#466=(
BOUNDED_SURFACE()
B_SPLINE_SURFACE(1,2,((#100650,#100651,#100652),(#100653,#100654,#100655)),
 .UNSPECIFIED.,.F.,.F.,.F.)
B_SPLINE_SURFACE_WITH_KNOTS((2,2),(3,3),(0.,0.289807040991559),(0.366820493751253,
0.384035903515169),.UNSPECIFIED.)
GEOMETRIC_REPRESENTATION_ITEM()
RATIONAL_B_SPLINE_SURFACE(((0.994126602224873,0.989721266390694,0.988228734781998),
(0.994126602224873,0.989721266390694,0.988228734781998)))
REPRESENTATION_ITEM('')
SURFACE()
);
#467=(
BOUNDED_SURFACE()
B_SPLINE_SURFACE(1,2,((#100684,#100685,#100686,#100687,#100688,#100689,
#100690),(#100691,#100692,#100693,#100694,#100695,#100696,#100697)),
 .UNSPECIFIED.,.F.,.F.,.F.)
B_SPLINE_SURFACE_WITH_KNOTS((2,2),(3,2,2,3),(0.,0.289681084359918),(0.34926499147441,
0.357142857142857,0.366820493751263,0.366996048774032),.UNSPECIFIED.)
GEOMETRIC_REPRESENTATION_ITEM()
RATIONAL_B_SPLINE_SURFACE(((0.995079542144874,0.997234796441972,1.,0.996603060231143,
0.994126602224868,0.994126602224868,0.994126602224868),(0.995079542144874,
0.997234796441972,1.,0.996603060231143,0.994126602224868,0.994126602224868,
0.994126602224868)))
REPRESENTATION_ITEM('')
SURFACE()
);
#468=(
BOUNDED_SURFACE()
B_SPLINE_SURFACE(1,2,((#100699,#100700,#100701),(#100702,#100703,#100704)),
 .UNSPECIFIED.,.F.,.F.,.F.)
B_SPLINE_SURFACE_WITH_KNOTS((2,2),(3,3),(0.,0.289807040991558),(0.366820493751253,
0.384035903515169),.UNSPECIFIED.)
GEOMETRIC_REPRESENTATION_ITEM()
RATIONAL_B_SPLINE_SURFACE(((0.994126602224873,0.989721266390694,0.988228734781998),
(0.994126602224873,0.989721266390694,0.988228734781998)))
REPRESENTATION_ITEM('')
SURFACE()
);
#469=(
BOUNDED_SURFACE()
B_SPLINE_SURFACE(1,2,((#100733,#100734,#100735,#100736,#100737,#100738,
#100739),(#100740,#100741,#100742,#100743,#100744,#100745,#100746)),
 .UNSPECIFIED.,.F.,.F.,.F.)
B_SPLINE_SURFACE_WITH_KNOTS((2,2),(3,2,2,3),(0.,0.289681084359919),(0.34926499147441,
0.357142857142857,0.366820493751263,0.366996048774032),.UNSPECIFIED.)
GEOMETRIC_REPRESENTATION_ITEM()
RATIONAL_B_SPLINE_SURFACE(((0.995079542144874,0.997234796441972,1.,0.996603060231143,
0.994126602224868,0.994126602224868,0.994126602224868),(0.995079542144874,
0.997234796441972,1.,0.996603060231143,0.994126602224868,0.994126602224868,
0.994126602224868)))
REPRESENTATION_ITEM('')
SURFACE()
);
#470=(
BOUNDED_SURFACE()
B_SPLINE_SURFACE(1,2,((#100748,#100749,#100750),(#100751,#100752,#100753)),
 .UNSPECIFIED.,.F.,.F.,.F.)
B_SPLINE_SURFACE_WITH_KNOTS((2,2),(3,3),(0.,0.289807040991561),(0.366820493751253,
0.384035903515169),.UNSPECIFIED.)
GEOMETRIC_REPRESENTATION_ITEM()
RATIONAL_B_SPLINE_SURFACE(((0.994126602224873,0.989721266390694,0.988228734781998),
(0.994126602224873,0.989721266390694,0.988228734781998)))
REPRESENTATION_ITEM('')
SURFACE()
);
#471=(
BOUNDED_SURFACE()
B_SPLINE_SURFACE(1,2,((#100782,#100783,#100784,#100785,#100786,#100787,
#100788),(#100789,#100790,#100791,#100792,#100793,#100794,#100795)),
 .UNSPECIFIED.,.F.,.F.,.F.)
B_SPLINE_SURFACE_WITH_KNOTS((2,2),(3,2,2,3),(-0.00024752608979232,0.289681084359921),
(0.349122170468145,0.357142857142857,0.366820493751263,0.367068020114749),
 .UNSPECIFIED.)
GEOMETRIC_REPRESENTATION_ITEM()
RATIONAL_B_SPLINE_SURFACE(((0.99500159567006,0.997184664950614,1.,0.996603060231143,
0.994126602224868,0.994126602224868,0.994126602224868),(0.99500159567006,
0.997184664950614,1.,0.996603060231143,0.994126602224868,0.994126602224868,
0.994126602224868)))
REPRESENTATION_ITEM('')
SURFACE()
);
#472=(
BOUNDED_SURFACE()
B_SPLINE_SURFACE(1,2,((#100797,#100798,#100799),(#100800,#100801,#100802)),
 .UNSPECIFIED.,.F.,.F.,.F.)
B_SPLINE_SURFACE_WITH_KNOTS((2,2),(3,3),(0.,0.289807040991564),(0.366820493751253,
0.384035903515169),.UNSPECIFIED.)
GEOMETRIC_REPRESENTATION_ITEM()
RATIONAL_B_SPLINE_SURFACE(((0.994126602224873,0.989721266390694,0.988228734781998),
(0.994126602224873,0.989721266390694,0.988228734781998)))
REPRESENTATION_ITEM('')
SURFACE()
);
#473=(
BOUNDED_SURFACE()
B_SPLINE_SURFACE(1,2,((#100831,#100832,#100833,#100834,#100835,#100836,
#100837),(#100838,#100839,#100840,#100841,#100842,#100843,#100844)),
 .UNSPECIFIED.,.F.,.F.,.F.)
B_SPLINE_SURFACE_WITH_KNOTS((2,2),(3,2,2,3),(-0.000247526153271754,0.289681084359918),
(0.349122170380219,0.357142857142857,0.366820493751264,0.367068020171335),
 .UNSPECIFIED.)
GEOMETRIC_REPRESENTATION_ITEM()
RATIONAL_B_SPLINE_SURFACE(((0.995001595622196,0.99718466491975,1.,0.996603060231143,
0.994126602224868,0.994126602224868,0.994126602224868),(0.995001595622196,
0.99718466491975,1.,0.996603060231143,0.994126602224868,0.994126602224868,
0.994126602224868)))
REPRESENTATION_ITEM('')
SURFACE()
);
#474=(
BOUNDED_SURFACE()
B_SPLINE_SURFACE(1,2,((#100846,#100847,#100848),(#100849,#100850,#100851)),
 .UNSPECIFIED.,.F.,.F.,.F.)
B_SPLINE_SURFACE_WITH_KNOTS((2,2),(3,3),(0.,0.289807040991555),(0.366820493751253,
0.384035903515169),.UNSPECIFIED.)
GEOMETRIC_REPRESENTATION_ITEM()
RATIONAL_B_SPLINE_SURFACE(((0.994126602224873,0.989721266390694,0.988228734781998),
(0.994126602224873,0.989721266390694,0.988228734781998)))
REPRESENTATION_ITEM('')
SURFACE()
);
#475=(
BOUNDED_SURFACE()
B_SPLINE_SURFACE(1,2,((#100862,#100863,#100864,#100865,#100866,#100867,
#100868),(#100869,#100870,#100871,#100872,#100873,#100874,#100875)),
 .UNSPECIFIED.,.F.,.F.,.F.)
B_SPLINE_SURFACE_WITH_KNOTS((2,2),(3,2,2,3),(-0.000247526181841607,0.289681084359921),
(0.349122170318008,0.357142857142857,0.366820493751254,0.367068020198209),
 .UNSPECIFIED.)
GEOMETRIC_REPRESENTATION_ITEM()
RATIONAL_B_SPLINE_SURFACE(((0.995001595588331,0.997184664897914,1.,0.996603060231146,
0.994126602224873,0.994126602224873,0.994126602224873),(0.995001595588331,
0.997184664897914,1.,0.996603060231146,0.994126602224873,0.994126602224873,
0.994126602224873)))
REPRESENTATION_ITEM('')
SURFACE()
);
#476=(
BOUNDED_SURFACE()
B_SPLINE_SURFACE(1,2,((#100895,#100896,#100897),(#100898,#100899,#100900)),
 .UNSPECIFIED.,.F.,.F.,.F.)
B_SPLINE_SURFACE_WITH_KNOTS((2,2),(3,3),(0.,0.289807040991564),(0.366820493751253,
0.384035903515168),.UNSPECIFIED.)
GEOMETRIC_REPRESENTATION_ITEM()
RATIONAL_B_SPLINE_SURFACE(((0.994126602224873,0.989721266390694,0.988228734781998),
(0.994126602224873,0.989721266390694,0.988228734781998)))
REPRESENTATION_ITEM('')
SURFACE()
);
#477=(
BOUNDED_SURFACE()
B_SPLINE_SURFACE(1,2,((#100929,#100930,#100931,#100932,#100933,#100934,
#100935),(#100936,#100937,#100938,#100939,#100940,#100941,#100942)),
 .UNSPECIFIED.,.F.,.F.,.F.)
B_SPLINE_SURFACE_WITH_KNOTS((2,2),(3,2,2,3),(0.,0.289681084360377),(0.349264991474411,
0.357142857142857,0.366820493751254,0.366996048774023),.UNSPECIFIED.)
GEOMETRIC_REPRESENTATION_ITEM()
RATIONAL_B_SPLINE_SURFACE(((0.995079542144875,0.997234796441973,1.,0.996603060231146,
0.994126602224873,0.994126602224873,0.994126602224873),(0.995079542144875,
0.997234796441973,1.,0.996603060231146,0.994126602224873,0.994126602224873,
0.994126602224873)))
REPRESENTATION_ITEM('')
SURFACE()
);
#478=(
BOUNDED_SURFACE()
B_SPLINE_SURFACE(1,2,((#100944,#100945,#100946),(#100947,#100948,#100949)),
 .UNSPECIFIED.,.F.,.F.,.F.)
B_SPLINE_SURFACE_WITH_KNOTS((2,2),(3,3),(0.,0.289807040992019),(0.366820493751234,
0.384035903515169),.UNSPECIFIED.)
GEOMETRIC_REPRESENTATION_ITEM()
RATIONAL_B_SPLINE_SURFACE(((0.994126602224883,0.989721266390696,0.988228734781998),
(0.994126602224883,0.989721266390696,0.988228734781998)))
REPRESENTATION_ITEM('')
SURFACE()
);
#479=(
BOUNDED_SURFACE()
B_SPLINE_SURFACE(1,2,((#100978,#100979,#100980,#100981,#100982,#100983,
#100984),(#100985,#100986,#100987,#100988,#100989,#100990,#100991)),
 .UNSPECIFIED.,.F.,.F.,.F.)
B_SPLINE_SURFACE_WITH_KNOTS((2,2),(3,2,2,3),(0.,0.289681084359932),(0.34926499147441,
0.357142857142857,0.366820493751254,0.366996048774023),.UNSPECIFIED.)
GEOMETRIC_REPRESENTATION_ITEM()
RATIONAL_B_SPLINE_SURFACE(((0.995079542144874,0.997234796441972,1.,0.996603060231146,
0.994126602224873,0.994126602224873,0.994126602224873),(0.995079542144874,
0.997234796441972,1.,0.996603060231146,0.994126602224873,0.994126602224873,
0.994126602224873)))
REPRESENTATION_ITEM('')
SURFACE()
);
#480=(
BOUNDED_SURFACE()
B_SPLINE_SURFACE(1,2,((#100993,#100994,#100995),(#100996,#100997,#100998)),
 .UNSPECIFIED.,.F.,.F.,.F.)
B_SPLINE_SURFACE_WITH_KNOTS((2,2),(3,3),(0.,0.289807040991983),(0.366820493751253,
0.384035903515169),.UNSPECIFIED.)
GEOMETRIC_REPRESENTATION_ITEM()
RATIONAL_B_SPLINE_SURFACE(((0.994126602224873,0.989721266390694,0.988228734781998),
(0.994126602224873,0.989721266390694,0.988228734781998)))
REPRESENTATION_ITEM('')
SURFACE()
);
#481=(
BOUNDED_SURFACE()
B_SPLINE_SURFACE(1,2,((#101027,#101028,#101029,#101030,#101031,#101032,
#101033),(#101034,#101035,#101036,#101037,#101038,#101039,#101040)),
 .UNSPECIFIED.,.F.,.F.,.F.)
B_SPLINE_SURFACE_WITH_KNOTS((2,2),(3,2,2,3),(0.,0.289681084359986),(0.34926499147441,
0.357142857142857,0.366820493751254,0.366996048774023),.UNSPECIFIED.)
GEOMETRIC_REPRESENTATION_ITEM()
RATIONAL_B_SPLINE_SURFACE(((0.995079542144874,0.997234796441972,1.,0.996603060231146,
0.994126602224873,0.994126602224873,0.994126602224873),(0.995079542144874,
0.997234796441972,1.,0.996603060231146,0.994126602224873,0.994126602224873,
0.994126602224873)))
REPRESENTATION_ITEM('')
SURFACE()
);
#482=(
BOUNDED_SURFACE()
B_SPLINE_SURFACE(1,2,((#101042,#101043,#101044),(#101045,#101046,#101047)),
 .UNSPECIFIED.,.F.,.F.,.F.)
B_SPLINE_SURFACE_WITH_KNOTS((2,2),(3,3),(0.,0.289807040991897),(0.366820493751253,
0.38403590351517),.UNSPECIFIED.)
GEOMETRIC_REPRESENTATION_ITEM()
RATIONAL_B_SPLINE_SURFACE(((0.994126602224873,0.989721266390694,0.988228734781998),
(0.994126602224873,0.989721266390694,0.988228734781998)))
REPRESENTATION_ITEM('')
SURFACE()
);
#483=(
BOUNDED_SURFACE()
B_SPLINE_SURFACE(1,2,((#101076,#101077,#101078,#101079,#101080,#101081,
#101082),(#101083,#101084,#101085,#101086,#101087,#101088,#101089)),
 .UNSPECIFIED.,.F.,.F.,.F.)
B_SPLINE_SURFACE_WITH_KNOTS((2,2),(3,2,2,3),(-0.00024752631999515,0.289681084359929),
(0.349122170227001,0.357142857142857,0.366820493751255,0.367068020367516),
 .UNSPECIFIED.)
GEOMETRIC_REPRESENTATION_ITEM()
RATIONAL_B_SPLINE_SURFACE(((0.995001595538792,0.99718466486597,1.,0.996603060231146,
0.994126602224872,0.994126602224872,0.994126602224872),(0.995001595538792,
0.99718466486597,1.,0.996603060231146,0.994126602224872,0.994126602224872,
0.994126602224872)))
REPRESENTATION_ITEM('')
SURFACE()
);
#484=(
BOUNDED_SURFACE()
B_SPLINE_SURFACE(1,2,((#101091,#101092,#101093,#101094,#101095),(#101096,
#101097,#101098,#101099,#101100)),.UNSPECIFIED.,.F.,.F.,.F.)
B_SPLINE_SURFACE_WITH_KNOTS((2,2),(3,2,3),(0.710318915639635,1.),(0.400939219852743,
0.418312080773435,0.418485809382642),.UNSPECIFIED.)
GEOMETRIC_REPRESENTATION_ITEM()
RATIONAL_B_SPLINE_SURFACE(((0.988105937622242,0.989485911589766,0.99383221411677,
0.99383221411677,0.99383221411677),(0.988105937622242,0.989485911589766,
0.99383221411677,0.99383221411677,0.99383221411677)))
REPRESENTATION_ITEM('')
SURFACE()
);
#485=(
BOUNDED_SURFACE()
B_SPLINE_SURFACE(1,2,((#101111,#101112,#101113,#101114,#101115),(#101116,
#101117,#101118,#101119,#101120)),.UNSPECIFIED.,.F.,.F.,.F.)
B_SPLINE_SURFACE_WITH_KNOTS((2,2),(3,2,3),(0.710192959005959,1.),(0.314770575782735,
0.314942866188491,0.332171906764074),.UNSPECIFIED.)
GEOMETRIC_REPRESENTATION_ITEM()
RATIONAL_B_SPLINE_SURFACE(((0.987877375613935,0.987877375613935,0.987877375613935,
0.986779141655833,0.988598326347701),(0.987877375613935,0.987877375613935,
0.987877375613935,0.986779141655833,0.988598326347701)))
REPRESENTATION_ITEM('')
SURFACE()
);
#486=(
BOUNDED_SURFACE()
B_SPLINE_SURFACE(1,2,((#101132,#101133,#101134,#101135,#101136),(#101137,
#101138,#101139,#101140,#101141)),.UNSPECIFIED.,.F.,.F.,.F.)
B_SPLINE_SURFACE_WITH_KNOTS((2,2),(3,2,3),(0.710318915639749,1.),(0.400939219852741,
0.418312080773612,0.41848580938282),.UNSPECIFIED.)
GEOMETRIC_REPRESENTATION_ITEM()
RATIONAL_B_SPLINE_SURFACE(((0.988105937622242,0.98948591158978,0.993832214116859,
0.993832214116859,0.993832214116859),(0.988105937622242,0.98948591158978,
0.993832214116859,0.993832214116859,0.993832214116859)))
REPRESENTATION_ITEM('')
SURFACE()
);
#487=(
BOUNDED_SURFACE()
B_SPLINE_SURFACE(1,2,((#101152,#101153,#101154,#101155,#101156),(#101157,
#101158,#101159,#101160,#101161)),.UNSPECIFIED.,.F.,.F.,.F.)
B_SPLINE_SURFACE_WITH_KNOTS((2,2),(3,2,3),(0.710192959006404,1.),(0.314770575782736,
0.314942866188492,0.332171906764074),.UNSPECIFIED.)
GEOMETRIC_REPRESENTATION_ITEM()
RATIONAL_B_SPLINE_SURFACE(((0.987877375613934,0.987877375613934,0.987877375613934,
0.986779141655833,0.988598326347701),(0.987877375613934,0.987877375613934,
0.987877375613934,0.986779141655833,0.988598326347701)))
REPRESENTATION_ITEM('')
SURFACE()
);
#488=(
BOUNDED_SURFACE()
B_SPLINE_SURFACE(1,2,((#101173,#101174,#101175,#101176,#101177),(#101178,
#101179,#101180,#101181,#101182)),.UNSPECIFIED.,.F.,.F.,.F.)
B_SPLINE_SURFACE_WITH_KNOTS((2,2),(3,2,3),(0.710318915640079,1.),(0.400939219852742,
0.418312080773433,0.41848580938264),.UNSPECIFIED.)
GEOMETRIC_REPRESENTATION_ITEM()
RATIONAL_B_SPLINE_SURFACE(((0.988105937622242,0.989485911589765,0.99383221411677,
0.99383221411677,0.99383221411677),(0.988105937622242,0.989485911589765,
0.99383221411677,0.99383221411677,0.99383221411677)))
REPRESENTATION_ITEM('')
SURFACE()
);
#489=(
BOUNDED_SURFACE()
B_SPLINE_SURFACE(1,2,((#101193,#101194,#101195,#101196,#101197),(#101198,
#101199,#101200,#101201,#101202)),.UNSPECIFIED.,.F.,.F.,.F.)
B_SPLINE_SURFACE_WITH_KNOTS((2,2),(3,2,3),(0.710192959008441,1.),(0.314770575782762,
0.314942866188517,0.332171906764075),.UNSPECIFIED.)
GEOMETRIC_REPRESENTATION_ITEM()
RATIONAL_B_SPLINE_SURFACE(((0.987877375613931,0.987877375613931,0.987877375613931,
0.986779141655835,0.988598326347701),(0.987877375613931,0.987877375613931,
0.987877375613931,0.986779141655835,0.988598326347701)))
REPRESENTATION_ITEM('')
SURFACE()
);
#490=(
BOUNDED_SURFACE()
B_SPLINE_SURFACE(1,2,((#101214,#101215,#101216,#101217,#101218),(#101219,
#101220,#101221,#101222,#101223)),.UNSPECIFIED.,.F.,.F.,.F.)
B_SPLINE_SURFACE_WITH_KNOTS((2,2),(3,2,3),(0.71031891564008,1.),(0.400939219852742,
0.418312080773433,0.41848580938264),.UNSPECIFIED.)
GEOMETRIC_REPRESENTATION_ITEM()
RATIONAL_B_SPLINE_SURFACE(((0.988105937622242,0.989485911589765,0.99383221411677,
0.99383221411677,0.99383221411677),(0.988105937622242,0.989485911589765,
0.99383221411677,0.99383221411677,0.99383221411677)))
REPRESENTATION_ITEM('')
SURFACE()
);
#491=(
BOUNDED_SURFACE()
B_SPLINE_SURFACE(1,2,((#101234,#101235,#101236,#101237,#101238),(#101239,
#101240,#101241,#101242,#101243)),.UNSPECIFIED.,.F.,.F.,.F.)
B_SPLINE_SURFACE_WITH_KNOTS((2,2),(3,2,3),(0.710192959006408,1.),(0.314770575782736,
0.314942866188492,0.332171906764075),.UNSPECIFIED.)
GEOMETRIC_REPRESENTATION_ITEM()
RATIONAL_B_SPLINE_SURFACE(((0.987877375613934,0.987877375613934,0.987877375613934,
0.986779141655833,0.988598326347701),(0.987877375613934,0.987877375613934,
0.987877375613934,0.986779141655833,0.988598326347701)))
REPRESENTATION_ITEM('')
SURFACE()
);
#492=(
BOUNDED_SURFACE()
B_SPLINE_SURFACE(1,2,((#101255,#101256,#101257,#101258,#101259),(#101260,
#101261,#101262,#101263,#101264)),.UNSPECIFIED.,.F.,.F.,.F.)
B_SPLINE_SURFACE_WITH_KNOTS((2,2),(3,2,3),(0.710318915639995,1.),(0.400939219852743,
0.418312080773433,0.41848580938264),.UNSPECIFIED.)
GEOMETRIC_REPRESENTATION_ITEM()
RATIONAL_B_SPLINE_SURFACE(((0.988105937622242,0.989485911589766,0.99383221411677,
0.99383221411677,0.99383221411677),(0.988105937622242,0.989485911589766,
0.99383221411677,0.99383221411677,0.99383221411677)))
REPRESENTATION_ITEM('')
SURFACE()
);
#493=(
BOUNDED_SURFACE()
B_SPLINE_SURFACE(1,2,((#101275,#101276,#101277,#101278,#101279),(#101280,
#101281,#101282,#101283,#101284)),.UNSPECIFIED.,.F.,.F.,.F.)
B_SPLINE_SURFACE_WITH_KNOTS((2,2),(3,2,3),(0.710192959008355,1.),(0.314770575782761,
0.314942866188516,0.332171906764074),.UNSPECIFIED.)
GEOMETRIC_REPRESENTATION_ITEM()
RATIONAL_B_SPLINE_SURFACE(((0.987877375613931,0.987877375613931,0.987877375613931,
0.986779141655835,0.988598326347701),(0.987877375613931,0.987877375613931,
0.987877375613931,0.986779141655835,0.988598326347701)))
REPRESENTATION_ITEM('')
SURFACE()
);
#494=(
BOUNDED_SURFACE()
B_SPLINE_SURFACE(1,2,((#101296,#101297,#101298,#101299,#101300),(#101301,
#101302,#101303,#101304,#101305)),.UNSPECIFIED.,.F.,.F.,.F.)
B_SPLINE_SURFACE_WITH_KNOTS((2,2),(3,2,3),(0.710318915640001,1.),(0.400939219852743,
0.418312080773434,0.418485809382641),.UNSPECIFIED.)
GEOMETRIC_REPRESENTATION_ITEM()
RATIONAL_B_SPLINE_SURFACE(((0.988105937622242,0.989485911589766,0.99383221411677,
0.99383221411677,0.99383221411677),(0.988105937622242,0.989485911589766,
0.99383221411677,0.99383221411677,0.99383221411677)))
REPRESENTATION_ITEM('')
SURFACE()
);
#495=(
BOUNDED_SURFACE()
B_SPLINE_SURFACE(1,2,((#101316,#101317,#101318,#101319,#101320),(#101321,
#101322,#101323,#101324,#101325)),.UNSPECIFIED.,.F.,.F.,.F.)
B_SPLINE_SURFACE_WITH_KNOTS((2,2),(3,2,3),(0.710192959006325,1.),(0.314770575782735,
0.314942866188491,0.332171906764074),.UNSPECIFIED.)
GEOMETRIC_REPRESENTATION_ITEM()
RATIONAL_B_SPLINE_SURFACE(((0.987877375613935,0.987877375613935,0.987877375613935,
0.986779141655833,0.988598326347701),(0.987877375613935,0.987877375613935,
0.987877375613935,0.986779141655833,0.988598326347701)))
REPRESENTATION_ITEM('')
SURFACE()
);
#496=(
BOUNDED_SURFACE()
B_SPLINE_SURFACE(1,2,((#101337,#101338,#101339,#101340,#101341),(#101342,
#101343,#101344,#101345,#101346)),.UNSPECIFIED.,.F.,.F.,.F.)
B_SPLINE_SURFACE_WITH_KNOTS((2,2),(3,2,3),(0.710318915639997,1.),(0.400939219852743,
0.418312080773434,0.418485809382641),.UNSPECIFIED.)
GEOMETRIC_REPRESENTATION_ITEM()
RATIONAL_B_SPLINE_SURFACE(((0.988105937622242,0.989485911589766,0.99383221411677,
0.99383221411677,0.99383221411677),(0.988105937622242,0.989485911589766,
0.99383221411677,0.99383221411677,0.99383221411677)))
REPRESENTATION_ITEM('')
SURFACE()
);
#497=(
BOUNDED_SURFACE()
B_SPLINE_SURFACE(1,2,((#101357,#101358,#101359,#101360,#101361),(#101362,
#101363,#101364,#101365,#101366)),.UNSPECIFIED.,.F.,.F.,.F.)
B_SPLINE_SURFACE_WITH_KNOTS((2,2),(3,2,3),(0.710192959008357,1.),(0.314770575782761,
0.314942866188516,0.332171906764074),.UNSPECIFIED.)
GEOMETRIC_REPRESENTATION_ITEM()
RATIONAL_B_SPLINE_SURFACE(((0.987877375613931,0.987877375613931,0.987877375613931,
0.986779141655835,0.988598326347701),(0.987877375613931,0.987877375613931,
0.987877375613931,0.986779141655835,0.988598326347701)))
REPRESENTATION_ITEM('')
SURFACE()
);
#498=(
BOUNDED_SURFACE()
B_SPLINE_SURFACE(1,2,((#101378,#101379,#101380,#101381,#101382),(#101383,
#101384,#101385,#101386,#101387)),.UNSPECIFIED.,.F.,.F.,.F.)
B_SPLINE_SURFACE_WITH_KNOTS((2,2),(3,2,3),(0.710318915639995,1.),(0.400939219852743,
0.418312080773434,0.418485809382641),.UNSPECIFIED.)
GEOMETRIC_REPRESENTATION_ITEM()
RATIONAL_B_SPLINE_SURFACE(((0.988105937622242,0.989485911589766,0.99383221411677,
0.99383221411677,0.99383221411677),(0.988105937622242,0.989485911589766,
0.99383221411677,0.99383221411677,0.99383221411677)))
REPRESENTATION_ITEM('')
SURFACE()
);
#499=(
BOUNDED_SURFACE()
B_SPLINE_SURFACE(1,2,((#101398,#101399,#101400,#101401,#101402),(#101403,
#101404,#101405,#101406,#101407)),.UNSPECIFIED.,.F.,.F.,.F.)
B_SPLINE_SURFACE_WITH_KNOTS((2,2),(3,2,3),(0.710192959006321,1.),(0.314770575782735,
0.314942866188491,0.332171906764074),.UNSPECIFIED.)
GEOMETRIC_REPRESENTATION_ITEM()
RATIONAL_B_SPLINE_SURFACE(((0.987877375613935,0.987877375613935,0.987877375613935,
0.986779141655833,0.988598326347701),(0.987877375613935,0.987877375613935,
0.987877375613935,0.986779141655833,0.988598326347701)))
REPRESENTATION_ITEM('')
SURFACE()
);
#500=(
BOUNDED_SURFACE()
B_SPLINE_SURFACE(1,2,((#101419,#101420,#101421,#101422,#101423),(#101424,
#101425,#101426,#101427,#101428)),.UNSPECIFIED.,.F.,.F.,.F.)
B_SPLINE_SURFACE_WITH_KNOTS((2,2),(3,2,3),(0.710318915640079,1.),(0.400939219852743,
0.418312080773434,0.418485809382641),.UNSPECIFIED.)
GEOMETRIC_REPRESENTATION_ITEM()
RATIONAL_B_SPLINE_SURFACE(((0.988105937622242,0.989485911589766,0.99383221411677,
0.99383221411677,0.99383221411677),(0.988105937622242,0.989485911589766,
0.99383221411677,0.99383221411677,0.99383221411677)))
REPRESENTATION_ITEM('')
SURFACE()
);
#501=(
BOUNDED_SURFACE()
B_SPLINE_SURFACE(1,2,((#101439,#101440,#101441,#101442,#101443),(#101444,
#101445,#101446,#101447,#101448)),.UNSPECIFIED.,.F.,.F.,.F.)
B_SPLINE_SURFACE_WITH_KNOTS((2,2),(3,2,3),(0.71019295900844,1.),(0.314770575782761,
0.314942866188516,0.332171906764074),.UNSPECIFIED.)
GEOMETRIC_REPRESENTATION_ITEM()
RATIONAL_B_SPLINE_SURFACE(((0.987877375613931,0.987877375613931,0.987877375613931,
0.986779141655835,0.988598326347701),(0.987877375613931,0.987877375613931,
0.987877375613931,0.986779141655835,0.988598326347701)))
REPRESENTATION_ITEM('')
SURFACE()
);
#502=(
BOUNDED_SURFACE()
B_SPLINE_SURFACE(1,2,((#101460,#101461,#101462,#101463,#101464),(#101465,
#101466,#101467,#101468,#101469)),.UNSPECIFIED.,.F.,.F.,.F.)
B_SPLINE_SURFACE_WITH_KNOTS((2,2),(3,2,3),(0.710318915639987,1.),(0.400939219852743,
0.418312080773434,0.418485809382641),.UNSPECIFIED.)
GEOMETRIC_REPRESENTATION_ITEM()
RATIONAL_B_SPLINE_SURFACE(((0.988105937622242,0.989485911589766,0.99383221411677,
0.99383221411677,0.99383221411677),(0.988105937622242,0.989485911589766,
0.99383221411677,0.99383221411677,0.99383221411677)))
REPRESENTATION_ITEM('')
SURFACE()
);
#503=(
BOUNDED_SURFACE()
B_SPLINE_SURFACE(1,2,((#101480,#101481,#101482,#101483,#101484),(#101485,
#101486,#101487,#101488,#101489)),.UNSPECIFIED.,.F.,.F.,.F.)
B_SPLINE_SURFACE_WITH_KNOTS((2,2),(3,2,3),(0.710192959008348,1.),(0.314770575782761,
0.314942866188516,0.332171906764074),.UNSPECIFIED.)
GEOMETRIC_REPRESENTATION_ITEM()
RATIONAL_B_SPLINE_SURFACE(((0.987877375613931,0.987877375613931,0.987877375613931,
0.986779141655835,0.988598326347701),(0.987877375613931,0.987877375613931,
0.987877375613931,0.986779141655835,0.988598326347701)))
REPRESENTATION_ITEM('')
SURFACE()
);
#504=(
BOUNDED_SURFACE()
B_SPLINE_SURFACE(1,2,((#101501,#101502,#101503,#101504,#101505),(#101506,
#101507,#101508,#101509,#101510)),.UNSPECIFIED.,.F.,.F.,.F.)
B_SPLINE_SURFACE_WITH_KNOTS((2,2),(3,2,3),(0.71031891564008,1.),(0.400939219852743,
0.418312080773434,0.418485809382641),.UNSPECIFIED.)
GEOMETRIC_REPRESENTATION_ITEM()
RATIONAL_B_SPLINE_SURFACE(((0.988105937622242,0.989485911589766,0.99383221411677,
0.99383221411677,0.99383221411677),(0.988105937622242,0.989485911589766,
0.99383221411677,0.99383221411677,0.99383221411677)))
REPRESENTATION_ITEM('')
SURFACE()
);
#505=(
BOUNDED_SURFACE()
B_SPLINE_SURFACE(1,2,((#101521,#101522,#101523,#101524,#101525),(#101526,
#101527,#101528,#101529,#101530)),.UNSPECIFIED.,.F.,.F.,.F.)
B_SPLINE_SURFACE_WITH_KNOTS((2,2),(3,2,3),(0.710192959008438,1.),(0.314770575782761,
0.314942866188516,0.332171906764074),.UNSPECIFIED.)
GEOMETRIC_REPRESENTATION_ITEM()
RATIONAL_B_SPLINE_SURFACE(((0.987877375613931,0.987877375613931,0.987877375613931,
0.986779141655835,0.988598326347701),(0.987877375613931,0.987877375613931,
0.987877375613931,0.986779141655835,0.988598326347701)))
REPRESENTATION_ITEM('')
SURFACE()
);
#506=(
BOUNDED_SURFACE()
B_SPLINE_SURFACE(1,2,((#101542,#101543,#101544,#101545,#101546),(#101547,
#101548,#101549,#101550,#101551)),.UNSPECIFIED.,.F.,.F.,.F.)
B_SPLINE_SURFACE_WITH_KNOTS((2,2),(3,2,3),(0.710318915639721,1.),(0.400939219852743,
0.418312080773435,0.418485809382642),.UNSPECIFIED.)
GEOMETRIC_REPRESENTATION_ITEM()
RATIONAL_B_SPLINE_SURFACE(((0.988105937622242,0.989485911589766,0.99383221411677,
0.99383221411677,0.99383221411677),(0.988105937622242,0.989485911589766,
0.99383221411677,0.99383221411677,0.99383221411677)))
REPRESENTATION_ITEM('')
SURFACE()
);
#507=(
BOUNDED_SURFACE()
B_SPLINE_SURFACE(1,2,((#101562,#101563,#101564,#101565,#101566),(#101567,
#101568,#101569,#101570,#101571)),.UNSPECIFIED.,.F.,.F.,.F.)
B_SPLINE_SURFACE_WITH_KNOTS((2,2),(3,2,3),(0.710192959006046,1.),(0.314770575782735,
0.314942866188491,0.332171906764074),.UNSPECIFIED.)
GEOMETRIC_REPRESENTATION_ITEM()
RATIONAL_B_SPLINE_SURFACE(((0.987877375613935,0.987877375613935,0.987877375613935,
0.986779141655833,0.988598326347701),(0.987877375613935,0.987877375613935,
0.987877375613935,0.986779141655833,0.988598326347701)))
REPRESENTATION_ITEM('')
SURFACE()
);
#508=(
BOUNDED_SURFACE()
B_SPLINE_SURFACE(1,2,((#101583,#101584,#101585,#101586,#101587),(#101588,
#101589,#101590,#101591,#101592)),.UNSPECIFIED.,.F.,.F.,.F.)
B_SPLINE_SURFACE_WITH_KNOTS((2,2),(3,2,3),(0.710318915638673,1.),(0.400939219852743,
0.418312080773434,0.418485809382641),.UNSPECIFIED.)
GEOMETRIC_REPRESENTATION_ITEM()
RATIONAL_B_SPLINE_SURFACE(((0.988105937622242,0.989485911589766,0.99383221411677,
0.99383221411677,0.99383221411677),(0.988105937622242,0.989485911589766,
0.99383221411677,0.99383221411677,0.99383221411677)))
REPRESENTATION_ITEM('')
SURFACE()
);
#509=(
BOUNDED_SURFACE()
B_SPLINE_SURFACE(1,2,((#101603,#101604,#101605,#101606,#101607),(#101608,
#101609,#101610,#101611,#101612)),.UNSPECIFIED.,.F.,.F.,.F.)
B_SPLINE_SURFACE_WITH_KNOTS((2,2),(3,2,3),(0.710192959007032,1.),(0.314770575782761,
0.314942866188516,0.332171906764074),.UNSPECIFIED.)
GEOMETRIC_REPRESENTATION_ITEM()
RATIONAL_B_SPLINE_SURFACE(((0.987877375613931,0.987877375613931,0.987877375613931,
0.986779141655835,0.988598326347701),(0.987877375613931,0.987877375613931,
0.987877375613931,0.986779141655835,0.988598326347701)))
REPRESENTATION_ITEM('')
SURFACE()
);
#510=(
BOUNDED_SURFACE()
B_SPLINE_SURFACE(1,2,((#101624,#101625,#101626,#101627,#101628),(#101629,
#101630,#101631,#101632,#101633)),.UNSPECIFIED.,.F.,.F.,.F.)
B_SPLINE_SURFACE_WITH_KNOTS((2,2),(3,2,3),(0.710318915639952,1.),(0.400939219852743,
0.418312080773434,0.418485809382641),.UNSPECIFIED.)
GEOMETRIC_REPRESENTATION_ITEM()
RATIONAL_B_SPLINE_SURFACE(((0.988105937622242,0.989485911589766,0.99383221411677,
0.99383221411677,0.99383221411677),(0.988105937622242,0.989485911589766,
0.99383221411677,0.99383221411677,0.99383221411677)))
REPRESENTATION_ITEM('')
SURFACE()
);
#511=(
BOUNDED_SURFACE()
B_SPLINE_SURFACE(1,2,((#101644,#101645,#101646,#101647,#101648),(#101649,
#101650,#101651,#101652,#101653)),.UNSPECIFIED.,.F.,.F.,.F.)
B_SPLINE_SURFACE_WITH_KNOTS((2,2),(3,2,3),(0.710192959006276,1.),(0.314770575782735,
0.314942866188491,0.332171906764074),.UNSPECIFIED.)
GEOMETRIC_REPRESENTATION_ITEM()
RATIONAL_B_SPLINE_SURFACE(((0.987877375613934,0.987877375613934,0.987877375613934,
0.986779141655832,0.988598326347701),(0.987877375613935,0.987877375613935,
0.987877375613935,0.986779141655832,0.988598326347701)))
REPRESENTATION_ITEM('')
SURFACE()
);
#512=(
BOUNDED_SURFACE()
B_SPLINE_SURFACE(1,2,((#101665,#101666,#101667,#101668,#101669),(#101670,
#101671,#101672,#101673,#101674)),.UNSPECIFIED.,.F.,.F.,.F.)
B_SPLINE_SURFACE_WITH_KNOTS((2,2),(3,2,3),(0.710318915640067,1.),(0.400939219852743,
0.418312080773434,0.418485809382641),.UNSPECIFIED.)
GEOMETRIC_REPRESENTATION_ITEM()
RATIONAL_B_SPLINE_SURFACE(((0.988105937622242,0.989485911589766,0.99383221411677,
0.99383221411677,0.99383221411677),(0.988105937622242,0.989485911589766,
0.99383221411677,0.99383221411677,0.99383221411677)))
REPRESENTATION_ITEM('')
SURFACE()
);
#513=(
BOUNDED_SURFACE()
B_SPLINE_SURFACE(1,2,((#101685,#101686,#101687,#101688,#101689),(#101690,
#101691,#101692,#101693,#101694)),.UNSPECIFIED.,.F.,.F.,.F.)
B_SPLINE_SURFACE_WITH_KNOTS((2,2),(3,2,3),(0.710192959008432,1.),(0.31477057578276,
0.314942866188515,0.332171906764074),.UNSPECIFIED.)
GEOMETRIC_REPRESENTATION_ITEM()
RATIONAL_B_SPLINE_SURFACE(((0.987877375613931,0.987877375613931,0.987877375613931,
0.986779141655835,0.988598326347701),(0.987877375613931,0.987877375613931,
0.987877375613931,0.986779141655835,0.988598326347701)))
REPRESENTATION_ITEM('')
SURFACE()
);
#514=(
BOUNDED_SURFACE()
B_SPLINE_SURFACE(1,2,((#101706,#101707,#101708,#101709,#101710),(#101711,
#101712,#101713,#101714,#101715)),.UNSPECIFIED.,.F.,.F.,.F.)
B_SPLINE_SURFACE_WITH_KNOTS((2,2),(3,2,3),(0.710318915639847,1.),(0.400939219852743,
0.418312080773434,0.418485809382641),.UNSPECIFIED.)
GEOMETRIC_REPRESENTATION_ITEM()
RATIONAL_B_SPLINE_SURFACE(((0.988105937622242,0.989485911589766,0.99383221411677,
0.99383221411677,0.99383221411677),(0.988105937622242,0.989485911589766,
0.99383221411677,0.99383221411677,0.99383221411677)))
REPRESENTATION_ITEM('')
SURFACE()
);
#515=(
BOUNDED_SURFACE()
B_SPLINE_SURFACE(1,2,((#101726,#101727,#101728,#101729,#101730),(#101731,
#101732,#101733,#101734,#101735)),.UNSPECIFIED.,.F.,.F.,.F.)
B_SPLINE_SURFACE_WITH_KNOTS((2,2),(3,2,3),(0.710192959006166,1.),(0.314770575782735,
0.314942866188491,0.332171906764074),.UNSPECIFIED.)
GEOMETRIC_REPRESENTATION_ITEM()
RATIONAL_B_SPLINE_SURFACE(((0.987877375613935,0.987877375613935,0.987877375613935,
0.986779141655833,0.988598326347701),(0.987877375613935,0.987877375613935,
0.987877375613935,0.986779141655833,0.988598326347701)))
REPRESENTATION_ITEM('')
SURFACE()
);
#516=(
BOUNDED_SURFACE()
B_SPLINE_SURFACE(1,2,((#101747,#101748,#101749,#101750,#101751),(#101752,
#101753,#101754,#101755,#101756)),.UNSPECIFIED.,.F.,.F.,.F.)
B_SPLINE_SURFACE_WITH_KNOTS((2,2),(3,2,3),(0.710318915640079,1.),(0.400939219852743,
0.418312080773434,0.418485809382641),.UNSPECIFIED.)
GEOMETRIC_REPRESENTATION_ITEM()
RATIONAL_B_SPLINE_SURFACE(((0.988105937622242,0.989485911589766,0.99383221411677,
0.99383221411677,0.99383221411677),(0.988105937622242,0.989485911589766,
0.99383221411677,0.99383221411677,0.99383221411677)))
REPRESENTATION_ITEM('')
SURFACE()
);
#517=(
BOUNDED_SURFACE()
B_SPLINE_SURFACE(1,2,((#101767,#101768,#101769,#101770,#101771),(#101772,
#101773,#101774,#101775,#101776)),.UNSPECIFIED.,.F.,.F.,.F.)
B_SPLINE_SURFACE_WITH_KNOTS((2,2),(3,2,3),(0.710192959008438,1.),(0.314770575782761,
0.314942866188516,0.332171906764074),.UNSPECIFIED.)
GEOMETRIC_REPRESENTATION_ITEM()
RATIONAL_B_SPLINE_SURFACE(((0.987877375613931,0.987877375613931,0.987877375613931,
0.986779141655835,0.988598326347701),(0.987877375613931,0.987877375613931,
0.987877375613931,0.986779141655835,0.988598326347701)))
REPRESENTATION_ITEM('')
SURFACE()
);
#518=(
BOUNDED_SURFACE()
B_SPLINE_SURFACE(1,2,((#101788,#101789,#101790,#101791,#101792),(#101793,
#101794,#101795,#101796,#101797)),.UNSPECIFIED.,.F.,.F.,.F.)
B_SPLINE_SURFACE_WITH_KNOTS((2,2),(3,2,3),(0.710318915638946,1.),(0.400939219852743,
0.418312080773434,0.418485809382641),.UNSPECIFIED.)
GEOMETRIC_REPRESENTATION_ITEM()
RATIONAL_B_SPLINE_SURFACE(((0.988105937622242,0.989485911589766,0.99383221411677,
0.99383221411677,0.99383221411677),(0.988105937622242,0.989485911589766,
0.99383221411677,0.99383221411677,0.99383221411677)))
REPRESENTATION_ITEM('')
SURFACE()
);
#519=(
BOUNDED_SURFACE()
B_SPLINE_SURFACE(1,2,((#101808,#101809,#101810,#101811,#101812),(#101813,
#101814,#101815,#101816,#101817)),.UNSPECIFIED.,.F.,.F.,.F.)
B_SPLINE_SURFACE_WITH_KNOTS((2,2),(3,2,3),(0.710192959005266,1.),(0.314770575782735,
0.314942866188491,0.332171906764074),.UNSPECIFIED.)
GEOMETRIC_REPRESENTATION_ITEM()
RATIONAL_B_SPLINE_SURFACE(((0.987877375613935,0.987877375613935,0.987877375613935,
0.986779141655833,0.988598326347701),(0.987877375613935,0.987877375613935,
0.987877375613935,0.986779141655833,0.988598326347701)))
REPRESENTATION_ITEM('')
SURFACE()
);
#520=(
BOUNDED_SURFACE()
B_SPLINE_SURFACE(1,2,((#101829,#101830,#101831,#101832,#101833),(#101834,
#101835,#101836,#101837,#101838)),.UNSPECIFIED.,.F.,.F.,.F.)
B_SPLINE_SURFACE_WITH_KNOTS((2,2),(3,2,3),(0.710318915639109,1.),(0.400939219852743,
0.418312080773434,0.418485809382641),.UNSPECIFIED.)
GEOMETRIC_REPRESENTATION_ITEM()
RATIONAL_B_SPLINE_SURFACE(((0.988105937622242,0.989485911589766,0.99383221411677,
0.99383221411677,0.99383221411677),(0.988105937622242,0.989485911589766,
0.99383221411677,0.99383221411677,0.99383221411677)))
REPRESENTATION_ITEM('')
SURFACE()
);
#521=(
BOUNDED_SURFACE()
B_SPLINE_SURFACE(1,2,((#101849,#101850,#101851,#101852,#101853),(#101854,
#101855,#101856,#101857,#101858)),.UNSPECIFIED.,.F.,.F.,.F.)
B_SPLINE_SURFACE_WITH_KNOTS((2,2),(3,2,3),(0.710192959007463,1.),(0.314770575782761,
0.314942866188516,0.332171906764074),.UNSPECIFIED.)
GEOMETRIC_REPRESENTATION_ITEM()
RATIONAL_B_SPLINE_SURFACE(((0.987877375613931,0.987877375613931,0.987877375613931,
0.986779141655835,0.988598326347701),(0.987877375613931,0.987877375613931,
0.987877375613931,0.986779141655835,0.988598326347701)))
REPRESENTATION_ITEM('')
SURFACE()
);
#522=(
BOUNDED_SURFACE()
B_SPLINE_SURFACE(1,2,((#101870,#101871,#101872,#101873,#101874),(#101875,
#101876,#101877,#101878,#101879)),.UNSPECIFIED.,.F.,.F.,.F.)
B_SPLINE_SURFACE_WITH_KNOTS((2,2),(3,2,3),(0.710318915638975,1.),(0.400939219852743,
0.418312080773434,0.418485809382641),.UNSPECIFIED.)
GEOMETRIC_REPRESENTATION_ITEM()
RATIONAL_B_SPLINE_SURFACE(((0.988105937622242,0.989485911589766,0.99383221411677,
0.99383221411677,0.99383221411677),(0.988105937622242,0.989485911589766,
0.99383221411677,0.99383221411677,0.99383221411677)))
REPRESENTATION_ITEM('')
SURFACE()
);
#523=(
BOUNDED_SURFACE()
B_SPLINE_SURFACE(1,2,((#101890,#101891,#101892,#101893,#101894),(#101895,
#101896,#101897,#101898,#101899)),.UNSPECIFIED.,.F.,.F.,.F.)
B_SPLINE_SURFACE_WITH_KNOTS((2,2),(3,2,3),(0.710192959005298,1.),(0.314770575782735,
0.314942866188491,0.332171906764074),.UNSPECIFIED.)
GEOMETRIC_REPRESENTATION_ITEM()
RATIONAL_B_SPLINE_SURFACE(((0.987877375613935,0.987877375613935,0.987877375613935,
0.986779141655833,0.988598326347701),(0.987877375613935,0.987877375613935,
0.987877375613935,0.986779141655833,0.988598326347701)))
REPRESENTATION_ITEM('')
SURFACE()
);
#524=(
BOUNDED_SURFACE()
B_SPLINE_SURFACE(1,2,((#101911,#101912,#101913,#101914,#101915),(#101916,
#101917,#101918,#101919,#101920)),.UNSPECIFIED.,.F.,.F.,.F.)
B_SPLINE_SURFACE_WITH_KNOTS((2,2),(3,2,3),(0.710318915639871,1.),(0.400939219852743,
0.418312080773435,0.418485809382642),.UNSPECIFIED.)
GEOMETRIC_REPRESENTATION_ITEM()
RATIONAL_B_SPLINE_SURFACE(((0.988105937622242,0.989485911589766,0.99383221411677,
0.99383221411677,0.99383221411677),(0.988105937622242,0.989485911589766,
0.99383221411677,0.99383221411677,0.99383221411677)))
REPRESENTATION_ITEM('')
SURFACE()
);
#525=(
BOUNDED_SURFACE()
B_SPLINE_SURFACE(1,2,((#101931,#101932,#101933,#101934,#101935),(#101936,
#101937,#101938,#101939,#101940)),.UNSPECIFIED.,.F.,.F.,.F.)
B_SPLINE_SURFACE_WITH_KNOTS((2,2),(3,2,3),(0.710192959008236,1.),(0.314770575782761,
0.314942866188516,0.332171906764074),.UNSPECIFIED.)
GEOMETRIC_REPRESENTATION_ITEM()
RATIONAL_B_SPLINE_SURFACE(((0.987877375613931,0.987877375613931,0.987877375613931,
0.986779141655835,0.988598326347701),(0.987877375613931,0.987877375613931,
0.987877375613931,0.986779141655835,0.988598326347701)))
REPRESENTATION_ITEM('')
SURFACE()
);
#526=(
BOUNDED_SURFACE()
B_SPLINE_SURFACE(1,2,((#101952,#101953,#101954,#101955,#101956),(#101957,
#101958,#101959,#101960,#101961)),.UNSPECIFIED.,.F.,.F.,.F.)
B_SPLINE_SURFACE_WITH_KNOTS((2,2),(3,2,3),(0.710318915638728,1.),(0.400939219852742,
0.418312080773556,0.418485809382764),.UNSPECIFIED.)
GEOMETRIC_REPRESENTATION_ITEM()
RATIONAL_B_SPLINE_SURFACE(((0.988105937622242,0.989485911589775,0.993832214116831,
0.993832214116831,0.993832214116831),(0.988105937622242,0.989485911589775,
0.993832214116831,0.993832214116831,0.993832214116831)))
REPRESENTATION_ITEM('')
SURFACE()
);
#527=(
BOUNDED_SURFACE()
B_SPLINE_SURFACE(1,2,((#101969,#101970,#101971,#101972,#101973),(#101974,
#101975,#101976,#101977,#101978)),.UNSPECIFIED.,.F.,.F.,.F.)
B_SPLINE_SURFACE_WITH_KNOTS((2,2),(3,2,3),(0.710192959005056,1.),(0.314770575782735,
0.314942866188491,0.332171906764074),.UNSPECIFIED.)
GEOMETRIC_REPRESENTATION_ITEM()
RATIONAL_B_SPLINE_SURFACE(((0.987877375613935,0.987877375613935,0.987877375613935,
0.986779141655833,0.988598326347701),(0.987877375613935,0.987877375613935,
0.987877375613935,0.986779141655833,0.988598326347701)))
REPRESENTATION_ITEM('')
SURFACE()
);
#528=(
BOUNDED_SURFACE()
B_SPLINE_SURFACE(1,2,((#101980,#101981,#101982,#101983,#101984),(#101985,
#101986,#101987,#101988,#101989)),.UNSPECIFIED.,.F.,.F.,.F.)
B_SPLINE_SURFACE_WITH_KNOTS((2,2),(3,2,3),(0.710318915638947,1.),(0.400939219852743,
0.418312080773435,0.418485809382642),.UNSPECIFIED.)
GEOMETRIC_REPRESENTATION_ITEM()
RATIONAL_B_SPLINE_SURFACE(((0.988105937622242,0.989485911589766,0.99383221411677,
0.99383221411677,0.99383221411677),(0.988105937622242,0.989485911589766,
0.99383221411677,0.99383221411677,0.99383221411677)))
REPRESENTATION_ITEM('')
SURFACE()
);
#529=(
BOUNDED_SURFACE()
B_SPLINE_SURFACE(1,2,((#102000,#102001,#102002,#102003,#102004),(#102005,
#102006,#102007,#102008,#102009)),.UNSPECIFIED.,.F.,.F.,.F.)
B_SPLINE_SURFACE_WITH_KNOTS((2,2),(3,2,3),(0.710192959007303,1.),(0.314770575782761,
0.314942866188516,0.332171906764074),.UNSPECIFIED.)
GEOMETRIC_REPRESENTATION_ITEM()
RATIONAL_B_SPLINE_SURFACE(((0.987877375613931,0.987877375613931,0.987877375613931,
0.986779141655835,0.988598326347701),(0.987877375613931,0.987877375613931,
0.987877375613931,0.986779141655835,0.988598326347701)))
REPRESENTATION_ITEM('')
SURFACE()
);
#530=(
BOUNDED_SURFACE()
B_SPLINE_SURFACE(1,2,((#102021,#102022,#102023,#102024,#102025),(#102026,
#102027,#102028,#102029,#102030)),.UNSPECIFIED.,.F.,.F.,.F.)
B_SPLINE_SURFACE_WITH_KNOTS((2,2),(3,2,3),(0.710318915639195,1.),(0.400939219852743,
0.418312080773434,0.418485809382641),.UNSPECIFIED.)
GEOMETRIC_REPRESENTATION_ITEM()
RATIONAL_B_SPLINE_SURFACE(((0.988105937622242,0.989485911589766,0.99383221411677,
0.99383221411677,0.99383221411677),(0.988105937622242,0.989485911589766,
0.99383221411677,0.99383221411677,0.99383221411677)))
REPRESENTATION_ITEM('')
SURFACE()
);
#531=(
BOUNDED_SURFACE()
B_SPLINE_SURFACE(1,2,((#102041,#102042,#102043,#102044,#102045),(#102046,
#102047,#102048,#102049,#102050)),.UNSPECIFIED.,.F.,.F.,.F.)
B_SPLINE_SURFACE_WITH_KNOTS((2,2),(3,2,3),(0.710192959005512,1.),(0.314770575782735,
0.314942866188491,0.332171906764074),.UNSPECIFIED.)
GEOMETRIC_REPRESENTATION_ITEM()
RATIONAL_B_SPLINE_SURFACE(((0.987877375613935,0.987877375613935,0.987877375613935,
0.986779141655833,0.988598326347701),(0.987877375613935,0.987877375613935,
0.987877375613935,0.986779141655833,0.988598326347701)))
REPRESENTATION_ITEM('')
SURFACE()
);
#532=(
BOUNDED_SURFACE()
B_SPLINE_SURFACE(1,2,((#102062,#102063,#102064,#102065,#102066),(#102067,
#102068,#102069,#102070,#102071)),.UNSPECIFIED.,.F.,.F.,.F.)
B_SPLINE_SURFACE_WITH_KNOTS((2,2),(3,2,3),(0.71031891563932,1.),(0.400939219852743,
0.418312080773435,0.418485809382642),.UNSPECIFIED.)
GEOMETRIC_REPRESENTATION_ITEM()
RATIONAL_B_SPLINE_SURFACE(((0.988105937622242,0.989485911589766,0.99383221411677,
0.99383221411677,0.99383221411677),(0.988105937622242,0.989485911589766,
0.99383221411677,0.99383221411677,0.99383221411677)))
REPRESENTATION_ITEM('')
SURFACE()
);
#533=(
BOUNDED_SURFACE()
B_SPLINE_SURFACE(1,2,((#102082,#102083,#102084,#102085,#102086),(#102087,
#102088,#102089,#102090,#102091)),.UNSPECIFIED.,.F.,.F.,.F.)
B_SPLINE_SURFACE_WITH_KNOTS((2,2),(3,2,3),(0.710192959007678,1.),(0.314770575782761,
0.314942866188516,0.332171906764074),.UNSPECIFIED.)
GEOMETRIC_REPRESENTATION_ITEM()
RATIONAL_B_SPLINE_SURFACE(((0.987877375613931,0.987877375613931,0.987877375613931,
0.986779141655835,0.988598326347701),(0.987877375613931,0.987877375613931,
0.987877375613931,0.986779141655835,0.988598326347701)))
REPRESENTATION_ITEM('')
SURFACE()
);
#534=(
BOUNDED_SURFACE()
B_SPLINE_SURFACE(1,2,((#102103,#102104,#102105,#102106,#102107),(#102108,
#102109,#102110,#102111,#102112)),.UNSPECIFIED.,.F.,.F.,.F.)
B_SPLINE_SURFACE_WITH_KNOTS((2,2),(3,2,3),(0.710318915638836,1.),(0.400939219852743,
0.418312080773437,0.418485809382644),.UNSPECIFIED.)
GEOMETRIC_REPRESENTATION_ITEM()
RATIONAL_B_SPLINE_SURFACE(((0.988105937622242,0.989485911589766,0.993832214116771,
0.993832214116771,0.993832214116771),(0.988105937622242,0.989485911589766,
0.993832214116771,0.993832214116771,0.993832214116771)))
REPRESENTATION_ITEM('')
SURFACE()
);
#535=(
BOUNDED_SURFACE()
B_SPLINE_SURFACE(1,2,((#102123,#102124,#102125,#102126,#102127),(#102128,
#102129,#102130,#102131,#102132)),.UNSPECIFIED.,.F.,.F.,.F.)
B_SPLINE_SURFACE_WITH_KNOTS((2,2),(3,2,3),(0.710192959005161,1.),(0.314770575782735,
0.314942866188491,0.332171906764077),.UNSPECIFIED.)
GEOMETRIC_REPRESENTATION_ITEM()
RATIONAL_B_SPLINE_SURFACE(((0.987877375613935,0.987877375613935,0.987877375613935,
0.986779141655832,0.988598326347702),(0.987877375613935,0.987877375613935,
0.987877375613935,0.986779141655832,0.988598326347702)))
REPRESENTATION_ITEM('')
SURFACE()
);
#536=(
BOUNDED_SURFACE()
B_SPLINE_SURFACE(1,2,((#102144,#102145,#102146,#102147,#102148),(#102149,
#102150,#102151,#102152,#102153)),.UNSPECIFIED.,.F.,.F.,.F.)
B_SPLINE_SURFACE_WITH_KNOTS((2,2),(3,2,3),(0.710318915638982,1.),(0.400939219852743,
0.418312080773434,0.418485809382641),.UNSPECIFIED.)
GEOMETRIC_REPRESENTATION_ITEM()
RATIONAL_B_SPLINE_SURFACE(((0.988105937622242,0.989485911589766,0.99383221411677,
0.99383221411677,0.99383221411677),(0.988105937622242,0.989485911589766,
0.99383221411677,0.99383221411677,0.99383221411677)))
REPRESENTATION_ITEM('')
SURFACE()
);
#537=(
BOUNDED_SURFACE()
B_SPLINE_SURFACE(1,2,((#102164,#102165,#102166,#102167,#102168),(#102169,
#102170,#102171,#102172,#102173)),.UNSPECIFIED.,.F.,.F.,.F.)
B_SPLINE_SURFACE_WITH_KNOTS((2,2),(3,2,3),(0.710192959007347,1.),(0.314770575782761,
0.314942866188516,0.332171906764075),.UNSPECIFIED.)
GEOMETRIC_REPRESENTATION_ITEM()
RATIONAL_B_SPLINE_SURFACE(((0.987877375613931,0.987877375613931,0.987877375613931,
0.986779141655835,0.988598326347701),(0.987877375613931,0.987877375613931,
0.987877375613931,0.986779141655835,0.988598326347701)))
REPRESENTATION_ITEM('')
SURFACE()
);
#538=(
BOUNDED_SURFACE()
B_SPLINE_SURFACE(1,2,((#102185,#102186,#102187,#102188,#102189),(#102190,
#102191,#102192,#102193,#102194)),.UNSPECIFIED.,.F.,.F.,.F.)
B_SPLINE_SURFACE_WITH_KNOTS((2,2),(3,2,3),(0.71031891563896,1.),(0.400939219852743,
0.418312080773435,0.418485809382642),.UNSPECIFIED.)
GEOMETRIC_REPRESENTATION_ITEM()
RATIONAL_B_SPLINE_SURFACE(((0.988105937622242,0.989485911589766,0.99383221411677,
0.99383221411677,0.99383221411677),(0.988105937622242,0.989485911589766,
0.99383221411677,0.99383221411677,0.99383221411677)))
REPRESENTATION_ITEM('')
SURFACE()
);
#539=(
BOUNDED_SURFACE()
B_SPLINE_SURFACE(1,2,((#102205,#102206,#102207,#102208,#102209),(#102210,
#102211,#102212,#102213,#102214)),.UNSPECIFIED.,.F.,.F.,.F.)
B_SPLINE_SURFACE_WITH_KNOTS((2,2),(3,2,3),(0.71019295900529,1.),(0.314770575782735,
0.314942866188491,0.332171906764074),.UNSPECIFIED.)
GEOMETRIC_REPRESENTATION_ITEM()
RATIONAL_B_SPLINE_SURFACE(((0.987877375613935,0.987877375613935,0.987877375613935,
0.986779141655833,0.988598326347701),(0.987877375613935,0.987877375613935,
0.987877375613935,0.986779141655833,0.988598326347701)))
REPRESENTATION_ITEM('')
SURFACE()
);
#540=(
BOUNDED_SURFACE()
B_SPLINE_SURFACE(1,2,((#102226,#102227,#102228,#102229,#102230),(#102231,
#102232,#102233,#102234,#102235)),.UNSPECIFIED.,.F.,.F.,.F.)
B_SPLINE_SURFACE_WITH_KNOTS((2,2),(3,2,3),(0.71031891563878,1.),(0.400939219852743,
0.418312080773434,0.418485809382641),.UNSPECIFIED.)
GEOMETRIC_REPRESENTATION_ITEM()
RATIONAL_B_SPLINE_SURFACE(((0.988105937622242,0.989485911589766,0.99383221411677,
0.99383221411677,0.99383221411677),(0.988105937622242,0.989485911589766,
0.99383221411677,0.99383221411677,0.99383221411677)))
REPRESENTATION_ITEM('')
SURFACE()
);
#541=(
BOUNDED_SURFACE()
B_SPLINE_SURFACE(1,2,((#102246,#102247,#102248,#102249,#102250),(#102251,
#102252,#102253,#102254,#102255)),.UNSPECIFIED.,.F.,.F.,.F.)
B_SPLINE_SURFACE_WITH_KNOTS((2,2),(3,2,3),(0.71019295900714,1.),(0.314770575782761,
0.314942866188516,0.332171906764074),.UNSPECIFIED.)
GEOMETRIC_REPRESENTATION_ITEM()
RATIONAL_B_SPLINE_SURFACE(((0.987877375613931,0.987877375613931,0.987877375613931,
0.986779141655835,0.988598326347701),(0.987877375613931,0.987877375613931,
0.987877375613931,0.986779141655835,0.988598326347701)))
REPRESENTATION_ITEM('')
SURFACE()
);
#542=(
BOUNDED_SURFACE()
B_SPLINE_SURFACE(1,2,((#102267,#102268,#102269),(#102270,#102271,#102272)),
 .UNSPECIFIED.,.F.,.F.,.F.)
B_SPLINE_SURFACE_WITH_KNOTS((2,2),(3,3),(0.710192959007992,1.),(0.366820493751253,
0.384035903515169),.UNSPECIFIED.)
GEOMETRIC_REPRESENTATION_ITEM()
RATIONAL_B_SPLINE_SURFACE(((0.994126602224873,0.989721266390694,0.988228734781998),
(0.994126602224873,0.989721266390694,0.988228734781998)))
REPRESENTATION_ITEM('')
SURFACE()
);
#543=(
BOUNDED_SURFACE()
B_SPLINE_SURFACE(1,2,((#102281,#102282,#102283,#102284,#102285,#102286,
#102287),(#102288,#102289,#102290,#102291,#102292,#102293,#102294)),
 .UNSPECIFIED.,.F.,.F.,.F.)
B_SPLINE_SURFACE_WITH_KNOTS((2,2),(3,2,2,3),(0.71031891563963,1.),(0.349264991474409,
0.357142857142857,0.366820493751254,0.366996048774023),.UNSPECIFIED.)
GEOMETRIC_REPRESENTATION_ITEM()
RATIONAL_B_SPLINE_SURFACE(((0.995079542144874,0.997234796441972,1.,0.996603060231146,
0.994126602224873,0.994126602224873,0.994126602224873),(0.995079542144874,
0.997234796441972,1.,0.996603060231146,0.994126602224873,0.994126602224873,
0.994126602224873)))
REPRESENTATION_ITEM('')
SURFACE()
);
#544=(
BOUNDED_SURFACE()
B_SPLINE_SURFACE(1,2,((#102302,#102303,#102304),(#102305,#102306,#102307)),
 .UNSPECIFIED.,.F.,.F.,.F.)
B_SPLINE_SURFACE_WITH_KNOTS((2,2),(3,3),(0.710192959007136,1.),(0.366820493751253,
0.384035903515172),.UNSPECIFIED.)
GEOMETRIC_REPRESENTATION_ITEM()
RATIONAL_B_SPLINE_SURFACE(((0.994126602224873,0.989721266390694,0.988228734781998),
(0.994126602224873,0.989721266390694,0.988228734781998)))
REPRESENTATION_ITEM('')
SURFACE()
);
#545=(
BOUNDED_SURFACE()
B_SPLINE_SURFACE(1,2,((#102316,#102317,#102318,#102319,#102320,#102321,
#102322),(#102323,#102324,#102325,#102326,#102327,#102328,#102329)),
 .UNSPECIFIED.,.F.,.F.,.F.)
B_SPLINE_SURFACE_WITH_KNOTS((2,2),(3,2,2,3),(0.710318915638783,1.),(0.349264991474413,
0.357142857142857,0.366820493751255,0.366996048774024),.UNSPECIFIED.)
GEOMETRIC_REPRESENTATION_ITEM()
RATIONAL_B_SPLINE_SURFACE(((0.995079542144876,0.997234796441973,1.,0.996603060231146,
0.994126602224872,0.994126602224872,0.994126602224872),(0.995079542144876,
0.997234796441973,1.,0.996603060231146,0.994126602224872,0.994126602224872,
0.994126602224872)))
REPRESENTATION_ITEM('')
SURFACE()
);
#546=(
BOUNDED_SURFACE()
B_SPLINE_SURFACE(1,2,((#102337,#102338,#102339),(#102340,#102341,#102342)),
 .UNSPECIFIED.,.F.,.F.,.F.)
B_SPLINE_SURFACE_WITH_KNOTS((2,2),(3,3),(0.710192959007322,1.),(0.366820493751253,
0.384035903515175),.UNSPECIFIED.)
GEOMETRIC_REPRESENTATION_ITEM()
RATIONAL_B_SPLINE_SURFACE(((0.994126602224873,0.989721266390693,0.988228734781997),
(0.994126602224873,0.989721266390693,0.988228734781997)))
REPRESENTATION_ITEM('')
SURFACE()
);
#547=(
BOUNDED_SURFACE()
B_SPLINE_SURFACE(1,2,((#102351,#102352,#102353,#102354,#102355,#102356,
#102357),(#102358,#102359,#102360,#102361,#102362,#102363,#102364)),
 .UNSPECIFIED.,.F.,.F.,.F.)
B_SPLINE_SURFACE_WITH_KNOTS((2,2),(3,2,2,3),(0.710318915638966,1.),(0.349264991474414,
0.357142857142857,0.366820493751254,0.366996048774023),.UNSPECIFIED.)
GEOMETRIC_REPRESENTATION_ITEM()
RATIONAL_B_SPLINE_SURFACE(((0.995079542144877,0.997234796441974,1.,0.996603060231146,
0.994126602224873,0.994126602224873,0.994126602224873),(0.995079542144877,
0.997234796441974,1.,0.996603060231146,0.994126602224873,0.994126602224873,
0.994126602224873)))
REPRESENTATION_ITEM('')
SURFACE()
);
#548=(
BOUNDED_SURFACE()
B_SPLINE_SURFACE(1,2,((#102372,#102373,#102374),(#102375,#102376,#102377)),
 .UNSPECIFIED.,.F.,.F.,.F.)
B_SPLINE_SURFACE_WITH_KNOTS((2,2),(3,3),(0.710192959007347,1.),(0.366820493751253,
0.384035903515169),.UNSPECIFIED.)
GEOMETRIC_REPRESENTATION_ITEM()
RATIONAL_B_SPLINE_SURFACE(((0.994126602224873,0.989721266390694,0.988228734781998),
(0.994126602224873,0.989721266390694,0.988228734781998)))
REPRESENTATION_ITEM('')
SURFACE()
);
#549=(
BOUNDED_SURFACE()
B_SPLINE_SURFACE(1,2,((#102386,#102387,#102388,#102389,#102390,#102391,
#102392),(#102393,#102394,#102395,#102396,#102397,#102398,#102399)),
 .UNSPECIFIED.,.F.,.F.,.F.)
B_SPLINE_SURFACE_WITH_KNOTS((2,2),(3,2,2,3),(0.710318915638992,1.),(0.349264991474409,
0.357142857142857,0.366820493751254,0.366996048774023),.UNSPECIFIED.)
GEOMETRIC_REPRESENTATION_ITEM()
RATIONAL_B_SPLINE_SURFACE(((0.995079542144874,0.997234796441972,1.,0.996603060231146,
0.994126602224873,0.994126602224873,0.994126602224873),(0.995079542144874,
0.997234796441972,1.,0.996603060231146,0.994126602224873,0.994126602224873,
0.994126602224873)))
REPRESENTATION_ITEM('')
SURFACE()
);
#550=(
BOUNDED_SURFACE()
B_SPLINE_SURFACE(1,2,((#102407,#102408,#102409),(#102410,#102411,#102412)),
 .UNSPECIFIED.,.F.,.F.,.F.)
B_SPLINE_SURFACE_WITH_KNOTS((2,2),(3,3),(0.710192959007198,1.),(0.366820493751253,
0.384035903515169),.UNSPECIFIED.)
GEOMETRIC_REPRESENTATION_ITEM()
RATIONAL_B_SPLINE_SURFACE(((0.994126602224873,0.989721266390694,0.988228734781998),
(0.994126602224873,0.989721266390694,0.988228734781998)))
REPRESENTATION_ITEM('')
SURFACE()
);
#551=(
BOUNDED_SURFACE()
B_SPLINE_SURFACE(1,2,((#102421,#102422,#102423,#102424,#102425,#102426,
#102427),(#102428,#102429,#102430,#102431,#102432,#102433,#102434)),
 .UNSPECIFIED.,.F.,.F.,.F.)
B_SPLINE_SURFACE_WITH_KNOTS((2,2),(3,2,2,3),(0.710318915638841,1.),(0.34926499147441,
0.357142857142857,0.366820493751254,0.366996048774023),.UNSPECIFIED.)
GEOMETRIC_REPRESENTATION_ITEM()
RATIONAL_B_SPLINE_SURFACE(((0.995079542144874,0.997234796441972,1.,0.996603060231146,
0.994126602224873,0.994126602224873,0.994126602224873),(0.995079542144874,
0.997234796441972,1.,0.996603060231146,0.994126602224873,0.994126602224873,
0.994126602224873)))
REPRESENTATION_ITEM('')
SURFACE()
);
#552=(
BOUNDED_SURFACE()
B_SPLINE_SURFACE(1,2,((#102442,#102443,#102444),(#102445,#102446,#102447)),
 .UNSPECIFIED.,.F.,.F.,.F.)
B_SPLINE_SURFACE_WITH_KNOTS((2,2),(3,3),(0.710192959007674,1.),(0.366820493751253,
0.384035903515168),.UNSPECIFIED.)
GEOMETRIC_REPRESENTATION_ITEM()
RATIONAL_B_SPLINE_SURFACE(((0.994126602224873,0.989721266390695,0.988228734781999),
(0.994126602224873,0.989721266390695,0.988228734781999)))
REPRESENTATION_ITEM('')
SURFACE()
);
#553=(
BOUNDED_SURFACE()
B_SPLINE_SURFACE(1,2,((#102456,#102457,#102458,#102459,#102460,#102461,
#102462),(#102463,#102464,#102465,#102466,#102467,#102468,#102469)),
 .UNSPECIFIED.,.F.,.F.,.F.)
B_SPLINE_SURFACE_WITH_KNOTS((2,2),(3,2,2,3),(0.71031891563931,1.),(0.349264991474391,
0.357142857142857,0.366820493751254,0.366996048774023),.UNSPECIFIED.)
GEOMETRIC_REPRESENTATION_ITEM()
RATIONAL_B_SPLINE_SURFACE(((0.995079542144864,0.997234796441966,1.,0.996603060231146,
0.994126602224873,0.994126602224873,0.994126602224873),(0.995079542144864,
0.997234796441966,1.,0.996603060231146,0.994126602224873,0.994126602224873,
0.994126602224873)))
REPRESENTATION_ITEM('')
SURFACE()
);
#554=(
BOUNDED_SURFACE()
B_SPLINE_SURFACE(1,2,((#102477,#102478,#102479),(#102480,#102481,#102482)),
 .UNSPECIFIED.,.F.,.F.,.F.)
B_SPLINE_SURFACE_WITH_KNOTS((2,2),(3,3),(0.710192959007547,1.),(0.366820493751253,
0.384035903515167),.UNSPECIFIED.)
GEOMETRIC_REPRESENTATION_ITEM()
RATIONAL_B_SPLINE_SURFACE(((0.994126602224873,0.989721266390695,0.988228734781999),
(0.994126602224873,0.989721266390695,0.988228734781999)))
REPRESENTATION_ITEM('')
SURFACE()
);
#555=(
BOUNDED_SURFACE()
B_SPLINE_SURFACE(1,2,((#102491,#102492,#102493,#102494,#102495,#102496,
#102497),(#102498,#102499,#102500,#102501,#102502,#102503,#102504)),
 .UNSPECIFIED.,.F.,.F.,.F.)
B_SPLINE_SURFACE_WITH_KNOTS((2,2),(3,2,2,3),(0.71031891563919,1.),(0.349264991474391,
0.357142857142857,0.366820493751254,0.366996048774023),.UNSPECIFIED.)
GEOMETRIC_REPRESENTATION_ITEM()
RATIONAL_B_SPLINE_SURFACE(((0.995079542144864,0.997234796441966,1.,0.996603060231146,
0.994126602224873,0.994126602224873,0.994126602224873),(0.995079542144864,
0.997234796441966,1.,0.996603060231146,0.994126602224873,0.994126602224873,
0.994126602224873)))
REPRESENTATION_ITEM('')
SURFACE()
);
#556=(
BOUNDED_SURFACE()
B_SPLINE_SURFACE(1,2,((#102512,#102513,#102514),(#102515,#102516,#102517)),
 .UNSPECIFIED.,.F.,.F.,.F.)
B_SPLINE_SURFACE_WITH_KNOTS((2,2),(3,3),(0.710192959007307,1.),(0.366820493751253,
0.384035903515168),.UNSPECIFIED.)
GEOMETRIC_REPRESENTATION_ITEM()
RATIONAL_B_SPLINE_SURFACE(((0.994126602224873,0.989721266390695,0.988228734781999),
(0.994126602224873,0.989721266390695,0.988228734781999)))
REPRESENTATION_ITEM('')
SURFACE()
);
#557=(
BOUNDED_SURFACE()
B_SPLINE_SURFACE(1,2,((#102526,#102527,#102528,#102529,#102530,#102531,
#102532),(#102533,#102534,#102535,#102536,#102537,#102538,#102539)),
 .UNSPECIFIED.,.F.,.F.,.F.)
B_SPLINE_SURFACE_WITH_KNOTS((2,2),(3,2,2,3),(0.710318915638953,1.),(0.349264991474392,
0.357142857142857,0.366820493751254,0.366996048774023),.UNSPECIFIED.)
GEOMETRIC_REPRESENTATION_ITEM()
RATIONAL_B_SPLINE_SURFACE(((0.995079542144865,0.997234796441966,1.,0.996603060231146,
0.994126602224873,0.994126602224873,0.994126602224873),(0.995079542144865,
0.997234796441966,1.,0.996603060231146,0.994126602224873,0.994126602224873,
0.994126602224873)))
REPRESENTATION_ITEM('')
SURFACE()
);
#558=(
BOUNDED_SURFACE()
B_SPLINE_SURFACE(1,2,((#102547,#102548,#102549),(#102550,#102551,#102552)),
 .UNSPECIFIED.,.F.,.F.,.F.)
B_SPLINE_SURFACE_WITH_KNOTS((2,2),(3,3),(0.710192959007092,1.),(0.366820493751253,
0.384035903515168),.UNSPECIFIED.)
GEOMETRIC_REPRESENTATION_ITEM()
RATIONAL_B_SPLINE_SURFACE(((0.994126602224873,0.989721266390695,0.988228734781998),
(0.994126602224873,0.989721266390695,0.988228734781998)))
REPRESENTATION_ITEM('')
SURFACE()
);
#559=(
BOUNDED_SURFACE()
B_SPLINE_SURFACE(1,2,((#102561,#102562,#102563,#102564,#102565,#102566,
#102567),(#102568,#102569,#102570,#102571,#102572,#102573,#102574)),
 .UNSPECIFIED.,.F.,.F.,.F.)
B_SPLINE_SURFACE_WITH_KNOTS((2,2),(3,2,2,3),(0.710318915638733,1.),(0.349264991474392,
0.357142857142857,0.366820493751254,0.366996048774023),.UNSPECIFIED.)
GEOMETRIC_REPRESENTATION_ITEM()
RATIONAL_B_SPLINE_SURFACE(((0.995079542144865,0.997234796441966,1.,0.996603060231146,
0.994126602224873,0.994126602224873,0.994126602224873),(0.995079542144865,
0.997234796441966,1.,0.996603060231146,0.994126602224873,0.994126602224873,
0.994126602224873)))
REPRESENTATION_ITEM('')
SURFACE()
);
#560=(
BOUNDED_SURFACE()
B_SPLINE_SURFACE(1,2,((#102582,#102583,#102584),(#102585,#102586,#102587)),
 .UNSPECIFIED.,.F.,.F.,.F.)
B_SPLINE_SURFACE_WITH_KNOTS((2,2),(3,3),(0.71019295900824,1.),(0.366820493751253,
0.384035903515169),.UNSPECIFIED.)
GEOMETRIC_REPRESENTATION_ITEM()
RATIONAL_B_SPLINE_SURFACE(((0.994126602224873,0.989721266390694,0.988228734781998),
(0.994126602224873,0.989721266390694,0.988228734781998)))
REPRESENTATION_ITEM('')
SURFACE()
);
#561=(
BOUNDED_SURFACE()
B_SPLINE_SURFACE(1,2,((#102596,#102597,#102598,#102599,#102600,#102601,
#102602),(#102603,#102604,#102605,#102606,#102607,#102608,#102609)),
 .UNSPECIFIED.,.F.,.F.,.F.)
B_SPLINE_SURFACE_WITH_KNOTS((2,2),(3,2,2,3),(0.710318915639881,1.),(0.349264991474409,
0.357142857142857,0.366820493751264,0.366996048774033),.UNSPECIFIED.)
GEOMETRIC_REPRESENTATION_ITEM()
RATIONAL_B_SPLINE_SURFACE(((0.995079542144874,0.997234796441972,1.,0.996603060231143,
0.994126602224868,0.994126602224868,0.994126602224868),(0.995079542144874,
0.997234796441972,1.,0.996603060231143,0.994126602224868,0.994126602224868,
0.994126602224868)))
REPRESENTATION_ITEM('')
SURFACE()
);
#562=(
BOUNDED_SURFACE()
B_SPLINE_SURFACE(1,2,((#102617,#102618,#102619),(#102620,#102621,#102622)),
 .UNSPECIFIED.,.F.,.F.,.F.)
B_SPLINE_SURFACE_WITH_KNOTS((2,2),(3,3),(0.710192959008287,1.),(0.366820493751253,
0.384035903515169),.UNSPECIFIED.)
GEOMETRIC_REPRESENTATION_ITEM()
RATIONAL_B_SPLINE_SURFACE(((0.994126602224873,0.989721266390694,0.988228734781998),
(0.994126602224873,0.989721266390694,0.988228734781998)))
REPRESENTATION_ITEM('')
SURFACE()
);
#563=(
BOUNDED_SURFACE()
B_SPLINE_SURFACE(1,2,((#102631,#102632,#102633,#102634,#102635,#102636,
#102637),(#102638,#102639,#102640,#102641,#102642,#102643,#102644)),
 .UNSPECIFIED.,.F.,.F.,.F.)
B_SPLINE_SURFACE_WITH_KNOTS((2,2),(3,2,2,3),(0.710318915639928,1.),(0.349264991474409,
0.357142857142857,0.366820493751264,0.366996048774033),.UNSPECIFIED.)
GEOMETRIC_REPRESENTATION_ITEM()
RATIONAL_B_SPLINE_SURFACE(((0.995079542144874,0.997234796441972,1.,0.996603060231143,
0.994126602224868,0.994126602224868,0.994126602224868),(0.995079542144874,
0.997234796441972,1.,0.996603060231143,0.994126602224868,0.994126602224868,
0.994126602224868)))
REPRESENTATION_ITEM('')
SURFACE()
);
#564=(
BOUNDED_SURFACE()
B_SPLINE_SURFACE(1,2,((#102652,#102653,#102654),(#102655,#102656,#102657)),
 .UNSPECIFIED.,.F.,.F.,.F.)
B_SPLINE_SURFACE_WITH_KNOTS((2,2),(3,3),(0.710192959008438,1.),(0.366820493751253,
0.384035903515169),.UNSPECIFIED.)
GEOMETRIC_REPRESENTATION_ITEM()
RATIONAL_B_SPLINE_SURFACE(((0.994126602224873,0.989721266390694,0.988228734781998),
(0.994126602224873,0.989721266390694,0.988228734781998)))
REPRESENTATION_ITEM('')
SURFACE()
);
#565=(
BOUNDED_SURFACE()
B_SPLINE_SURFACE(1,2,((#102666,#102667,#102668,#102669,#102670,#102671,
#102672),(#102673,#102674,#102675,#102676,#102677,#102678,#102679)),
 .UNSPECIFIED.,.F.,.F.,.F.)
B_SPLINE_SURFACE_WITH_KNOTS((2,2),(3,2,2,3),(0.710318915639478,1.),(0.349264991474409,
0.357142857142857,0.366820493751264,0.366996048774033),.UNSPECIFIED.)
GEOMETRIC_REPRESENTATION_ITEM()
RATIONAL_B_SPLINE_SURFACE(((0.995079542144874,0.997234796441972,1.,0.996603060231143,
0.994126602224868,0.994126602224868,0.994126602224868),(0.995079542144874,
0.997234796441972,1.,0.996603060231143,0.994126602224868,0.994126602224868,
0.994126602224868)))
REPRESENTATION_ITEM('')
SURFACE()
);
#566=(
BOUNDED_SURFACE()
B_SPLINE_SURFACE(1,2,((#102687,#102688,#102689),(#102690,#102691,#102692)),
 .UNSPECIFIED.,.F.,.F.,.F.)
B_SPLINE_SURFACE_WITH_KNOTS((2,2),(3,3),(0.710192959008445,1.),(0.366820493751253,
0.384035903515169),.UNSPECIFIED.)
GEOMETRIC_REPRESENTATION_ITEM()
RATIONAL_B_SPLINE_SURFACE(((0.994126602224873,0.989721266390694,0.988228734781998),
(0.994126602224873,0.989721266390694,0.988228734781998)))
REPRESENTATION_ITEM('')
SURFACE()
);
#567=(
BOUNDED_SURFACE()
B_SPLINE_SURFACE(1,2,((#102701,#102702,#102703,#102704,#102705,#102706,
#102707),(#102708,#102709,#102710,#102711,#102712,#102713,#102714)),
 .UNSPECIFIED.,.F.,.F.,.F.)
B_SPLINE_SURFACE_WITH_KNOTS((2,2),(3,2,2,3),(0.710318915640074,1.),(0.34926499147441,
0.357142857142857,0.366820493751264,0.366996048774033),.UNSPECIFIED.)
GEOMETRIC_REPRESENTATION_ITEM()
RATIONAL_B_SPLINE_SURFACE(((0.995079542144874,0.997234796441972,1.,0.996603060231143,
0.994126602224868,0.994126602224868,0.994126602224868),(0.995079542144874,
0.997234796441972,1.,0.996603060231143,0.994126602224868,0.994126602224868,
0.994126602224868)))
REPRESENTATION_ITEM('')
SURFACE()
);
#568=(
BOUNDED_SURFACE()
B_SPLINE_SURFACE(1,2,((#102722,#102723,#102724),(#102725,#102726,#102727)),
 .UNSPECIFIED.,.F.,.F.,.F.)
B_SPLINE_SURFACE_WITH_KNOTS((2,2),(3,3),(0.710192959008436,1.),(0.366820493751253,
0.384035903515169),.UNSPECIFIED.)
GEOMETRIC_REPRESENTATION_ITEM()
RATIONAL_B_SPLINE_SURFACE(((0.994126602224873,0.989721266390694,0.988228734781998),
(0.994126602224873,0.989721266390694,0.988228734781998)))
REPRESENTATION_ITEM('')
SURFACE()
);
#569=(
BOUNDED_SURFACE()
B_SPLINE_SURFACE(1,2,((#102736,#102737,#102738,#102739,#102740,#102741,
#102742),(#102743,#102744,#102745,#102746,#102747,#102748,#102749)),
 .UNSPECIFIED.,.F.,.F.,.F.)
B_SPLINE_SURFACE_WITH_KNOTS((2,2),(3,2,2,3),(0.710318915640068,1.),(0.349264991474409,
0.357142857142857,0.366820493751264,0.366996048774033),.UNSPECIFIED.)
GEOMETRIC_REPRESENTATION_ITEM()
RATIONAL_B_SPLINE_SURFACE(((0.995079542144874,0.997234796441972,1.,0.996603060231143,
0.994126602224868,0.994126602224868,0.994126602224868),(0.995079542144874,
0.997234796441972,1.,0.996603060231143,0.994126602224868,0.994126602224868,
0.994126602224868)))
REPRESENTATION_ITEM('')
SURFACE()
);
#570=(
BOUNDED_SURFACE()
B_SPLINE_SURFACE(1,2,((#102757,#102758,#102759),(#102760,#102761,#102762)),
 .UNSPECIFIED.,.F.,.F.,.F.)
B_SPLINE_SURFACE_WITH_KNOTS((2,2),(3,3),(0.710192959008435,1.),(0.366820493751253,
0.384035903515169),.UNSPECIFIED.)
GEOMETRIC_REPRESENTATION_ITEM()
RATIONAL_B_SPLINE_SURFACE(((0.994126602224873,0.989721266390694,0.988228734781998),
(0.994126602224873,0.989721266390694,0.988228734781998)))
REPRESENTATION_ITEM('')
SURFACE()
);
#571=(
BOUNDED_SURFACE()
B_SPLINE_SURFACE(1,2,((#102771,#102772,#102773,#102774,#102775,#102776,
#102777),(#102778,#102779,#102780,#102781,#102782,#102783,#102784)),
 .UNSPECIFIED.,.F.,.F.,.F.)
B_SPLINE_SURFACE_WITH_KNOTS((2,2),(3,2,2,3),(0.710318915640079,1.),(0.34926499147441,
0.357142857142857,0.366820493751264,0.366996048774033),.UNSPECIFIED.)
GEOMETRIC_REPRESENTATION_ITEM()
RATIONAL_B_SPLINE_SURFACE(((0.995079542144874,0.997234796441972,1.,0.996603060231143,
0.994126602224868,0.994126602224868,0.994126602224868),(0.995079542144874,
0.997234796441972,1.,0.996603060231143,0.994126602224868,0.994126602224868,
0.994126602224868)))
REPRESENTATION_ITEM('')
SURFACE()
);
#572=(
BOUNDED_SURFACE()
B_SPLINE_SURFACE(1,2,((#102792,#102793,#102794),(#102795,#102796,#102797)),
 .UNSPECIFIED.,.F.,.F.,.F.)
B_SPLINE_SURFACE_WITH_KNOTS((2,2),(3,3),(0.710192959008434,1.),(0.366820493751253,
0.384035903515169),.UNSPECIFIED.)
GEOMETRIC_REPRESENTATION_ITEM()
RATIONAL_B_SPLINE_SURFACE(((0.994126602224873,0.989721266390694,0.988228734781998),
(0.994126602224873,0.989721266390694,0.988228734781998)))
REPRESENTATION_ITEM('')
SURFACE()
);
#573=(
BOUNDED_SURFACE()
B_SPLINE_SURFACE(1,2,((#102806,#102807,#102808,#102809,#102810,#102811,
#102812),(#102813,#102814,#102815,#102816,#102817,#102818,#102819)),
 .UNSPECIFIED.,.F.,.F.,.F.)
B_SPLINE_SURFACE_WITH_KNOTS((2,2),(3,2,2,3),(0.710318915640073,1.),(0.349264991474409,
0.357142857142857,0.366820493751264,0.366996048774033),.UNSPECIFIED.)
GEOMETRIC_REPRESENTATION_ITEM()
RATIONAL_B_SPLINE_SURFACE(((0.995079542144874,0.997234796441972,1.,0.996603060231143,
0.994126602224868,0.994126602224868,0.994126602224868),(0.995079542144874,
0.997234796441972,1.,0.996603060231143,0.994126602224868,0.994126602224868,
0.994126602224868)))
REPRESENTATION_ITEM('')
SURFACE()
);
#574=(
BOUNDED_SURFACE()
B_SPLINE_SURFACE(1,2,((#102827,#102828,#102829),(#102830,#102831,#102832)),
 .UNSPECIFIED.,.F.,.F.,.F.)
B_SPLINE_SURFACE_WITH_KNOTS((2,2),(3,3),(0.71019295900833,1.),(0.366820493751253,
0.384035903515169),.UNSPECIFIED.)
GEOMETRIC_REPRESENTATION_ITEM()
RATIONAL_B_SPLINE_SURFACE(((0.994126602224873,0.989721266390694,0.988228734781998),
(0.994126602224873,0.989721266390694,0.988228734781998)))
REPRESENTATION_ITEM('')
SURFACE()
);
#575=(
BOUNDED_SURFACE()
B_SPLINE_SURFACE(1,2,((#102841,#102842,#102843,#102844,#102845,#102846,
#102847),(#102848,#102849,#102850,#102851,#102852,#102853,#102854)),
 .UNSPECIFIED.,.F.,.F.,.F.)
B_SPLINE_SURFACE_WITH_KNOTS((2,2),(3,2,2,3),(0.710318915639974,1.),(0.349264991474409,
0.357142857142857,0.366820493751264,0.366996048774033),.UNSPECIFIED.)
GEOMETRIC_REPRESENTATION_ITEM()
RATIONAL_B_SPLINE_SURFACE(((0.995079542144874,0.997234796441972,1.,0.996603060231143,
0.994126602224868,0.994126602224868,0.994126602224868),(0.995079542144874,
0.997234796441972,1.,0.996603060231143,0.994126602224868,0.994126602224868,
0.994126602224868)))
REPRESENTATION_ITEM('')
SURFACE()
);
#576=(
BOUNDED_SURFACE()
B_SPLINE_SURFACE(1,2,((#102862,#102863,#102864),(#102865,#102866,#102867)),
 .UNSPECIFIED.,.F.,.F.,.F.)
B_SPLINE_SURFACE_WITH_KNOTS((2,2),(3,3),(0.710192959007029,1.),(0.366820493751253,
0.384035903515169),.UNSPECIFIED.)
GEOMETRIC_REPRESENTATION_ITEM()
RATIONAL_B_SPLINE_SURFACE(((0.994126602224873,0.989721266390694,0.988228734781998),
(0.994126602224873,0.989721266390694,0.988228734781998)))
REPRESENTATION_ITEM('')
SURFACE()
);
#577=(
BOUNDED_SURFACE()
B_SPLINE_SURFACE(1,2,((#102876,#102877,#102878,#102879,#102880,#102881,
#102882),(#102883,#102884,#102885,#102886,#102887,#102888,#102889)),
 .UNSPECIFIED.,.F.,.F.,.F.)
B_SPLINE_SURFACE_WITH_KNOTS((2,2),(3,2,2,3),(0.71031891563867,1.),(0.34926499147441,
0.357142857142857,0.366820493751264,0.366996048774033),.UNSPECIFIED.)
GEOMETRIC_REPRESENTATION_ITEM()
RATIONAL_B_SPLINE_SURFACE(((0.995079542144874,0.997234796441972,1.,0.996603060231143,
0.994126602224868,0.994126602224868,0.994126602224868),(0.995079542144874,
0.997234796441972,1.,0.996603060231143,0.994126602224868,0.994126602224868,
0.994126602224868)))
REPRESENTATION_ITEM('')
SURFACE()
);
#578=(
BOUNDED_SURFACE()
B_SPLINE_SURFACE(1,2,((#102897,#102898,#102899),(#102900,#102901,#102902)),
 .UNSPECIFIED.,.F.,.F.,.F.)
B_SPLINE_SURFACE_WITH_KNOTS((2,2),(3,3),(0.710192959008187,1.),(0.366820493751026,
0.38403590351517),.UNSPECIFIED.)
GEOMETRIC_REPRESENTATION_ITEM()
RATIONAL_B_SPLINE_SURFACE(((0.994126602224989,0.989721266390714,0.988228734781998),
(0.994126602224989,0.989721266390714,0.988228734781998)))
REPRESENTATION_ITEM('')
SURFACE()
);
#579=(
BOUNDED_SURFACE()
B_SPLINE_SURFACE(1,2,((#102911,#102912,#102913,#102914,#102915,#102916,
#102917),(#102918,#102919,#102920,#102921,#102922,#102923,#102924)),
 .UNSPECIFIED.,.F.,.F.,.F.)
B_SPLINE_SURFACE_WITH_KNOTS((2,2),(3,2,2,3),(0.710318915639827,1.),(0.349264991474409,
0.357142857142857,0.366820493751264,0.366996048774033),.UNSPECIFIED.)
GEOMETRIC_REPRESENTATION_ITEM()
RATIONAL_B_SPLINE_SURFACE(((0.995079542144874,0.997234796441972,1.,0.996603060231143,
0.994126602224868,0.994126602224868,0.994126602224868),(0.995079542144874,
0.997234796441972,1.,0.996603060231143,0.994126602224868,0.994126602224868,
0.994126602224868)))
REPRESENTATION_ITEM('')
SURFACE()
);
#580=(
BOUNDED_SURFACE()
B_SPLINE_SURFACE(1,2,((#102932,#102933,#102934),(#102935,#102936,#102937)),
 .UNSPECIFIED.,.F.,.F.,.F.)
B_SPLINE_SURFACE_WITH_KNOTS((2,2),(3,3),(0.710192959008439,1.),(0.366820493751253,
0.384035903515169),.UNSPECIFIED.)
GEOMETRIC_REPRESENTATION_ITEM()
RATIONAL_B_SPLINE_SURFACE(((0.994126602224873,0.989721266390694,0.988228734781998),
(0.994126602224873,0.989721266390694,0.988228734781998)))
REPRESENTATION_ITEM('')
SURFACE()
);
#581=(
BOUNDED_SURFACE()
B_SPLINE_SURFACE(1,2,((#102946,#102947,#102948,#102949,#102950,#102951,
#102952),(#102953,#102954,#102955,#102956,#102957,#102958,#102959)),
 .UNSPECIFIED.,.F.,.F.,.F.)
B_SPLINE_SURFACE_WITH_KNOTS((2,2),(3,2,2,3),(0.710318915640079,1.),(0.349264991474409,
0.357142857142857,0.366820493751264,0.366996048774033),.UNSPECIFIED.)
GEOMETRIC_REPRESENTATION_ITEM()
RATIONAL_B_SPLINE_SURFACE(((0.995079542144874,0.997234796441972,1.,0.996603060231143,
0.994126602224868,0.994126602224868,0.994126602224868),(0.995079542144874,
0.997234796441972,1.,0.996603060231143,0.994126602224868,0.994126602224868,
0.994126602224868)))
REPRESENTATION_ITEM('')
SURFACE()
);
#582=(
BOUNDED_SURFACE()
B_SPLINE_SURFACE(1,2,((#102967,#102968,#102969),(#102970,#102971,#102972)),
 .UNSPECIFIED.,.F.,.F.,.F.)
B_SPLINE_SURFACE_WITH_KNOTS((2,2),(3,3),(0.710192959008441,1.),(0.366820493751253,
0.384035903515169),.UNSPECIFIED.)
GEOMETRIC_REPRESENTATION_ITEM()
RATIONAL_B_SPLINE_SURFACE(((0.994126602224873,0.989721266390694,0.988228734781998),
(0.994126602224873,0.989721266390694,0.988228734781998)))
REPRESENTATION_ITEM('')
SURFACE()
);
#583=(
BOUNDED_SURFACE()
B_SPLINE_SURFACE(1,2,((#102981,#102982,#102983,#102984,#102985,#102986,
#102987),(#102988,#102989,#102990,#102991,#102992,#102993,#102994)),
 .UNSPECIFIED.,.F.,.F.,.F.)
B_SPLINE_SURFACE_WITH_KNOTS((2,2),(3,2,2,3),(0.710318915640082,1.),(0.349264991474409,
0.357142857142857,0.366820493751264,0.366996048774033),.UNSPECIFIED.)
GEOMETRIC_REPRESENTATION_ITEM()
RATIONAL_B_SPLINE_SURFACE(((0.995079542144874,0.997234796441972,1.,0.996603060231143,
0.994126602224868,0.994126602224868,0.994126602224868),(0.995079542144874,
0.997234796441972,1.,0.996603060231143,0.994126602224868,0.994126602224868,
0.994126602224868)))
REPRESENTATION_ITEM('')
SURFACE()
);
#584=(
BOUNDED_SURFACE()
B_SPLINE_SURFACE(1,2,((#103002,#103003,#103004),(#103005,#103006,#103007)),
 .UNSPECIFIED.,.F.,.F.,.F.)
B_SPLINE_SURFACE_WITH_KNOTS((2,2),(3,3),(0.710192959008439,1.),(0.366820493751253,
0.384035903515169),.UNSPECIFIED.)
GEOMETRIC_REPRESENTATION_ITEM()
RATIONAL_B_SPLINE_SURFACE(((0.994126602224873,0.989721266390694,0.988228734781998),
(0.994126602224873,0.989721266390694,0.988228734781998)))
REPRESENTATION_ITEM('')
SURFACE()
);
#585=(
BOUNDED_SURFACE()
B_SPLINE_SURFACE(1,2,((#103016,#103017,#103018,#103019,#103020,#103021,
#103022),(#103023,#103024,#103025,#103026,#103027,#103028,#103029)),
 .UNSPECIFIED.,.F.,.F.,.F.)
B_SPLINE_SURFACE_WITH_KNOTS((2,2),(3,2,2,3),(0.710318915640079,1.),(0.349264991474409,
0.357142857142857,0.366820493751264,0.366996048774033),.UNSPECIFIED.)
GEOMETRIC_REPRESENTATION_ITEM()
RATIONAL_B_SPLINE_SURFACE(((0.995079542144874,0.997234796441972,1.,0.996603060231143,
0.994126602224868,0.994126602224868,0.994126602224868),(0.995079542144874,
0.997234796441972,1.,0.996603060231143,0.994126602224868,0.994126602224868,
0.994126602224868)))
REPRESENTATION_ITEM('')
SURFACE()
);
#586=(
BOUNDED_SURFACE()
B_SPLINE_SURFACE(1,2,((#103037,#103038,#103039),(#103040,#103041,#103042)),
 .UNSPECIFIED.,.F.,.F.,.F.)
B_SPLINE_SURFACE_WITH_KNOTS((2,2),(3,3),(0.710192959008439,1.),(0.366820493751253,
0.384035903515169),.UNSPECIFIED.)
GEOMETRIC_REPRESENTATION_ITEM()
RATIONAL_B_SPLINE_SURFACE(((0.994126602224873,0.989721266390694,0.988228734781998),
(0.994126602224873,0.989721266390694,0.988228734781998)))
REPRESENTATION_ITEM('')
SURFACE()
);
#587=(
BOUNDED_SURFACE()
B_SPLINE_SURFACE(1,2,((#103051,#103052,#103053,#103054,#103055,#103056,
#103057),(#103058,#103059,#103060,#103061,#103062,#103063,#103064)),
 .UNSPECIFIED.,.F.,.F.,.F.)
B_SPLINE_SURFACE_WITH_KNOTS((2,2),(3,2,2,3),(0.710318915640081,1.),(0.34926499147441,
0.357142857142857,0.366820493751264,0.366996048774033),.UNSPECIFIED.)
GEOMETRIC_REPRESENTATION_ITEM()
RATIONAL_B_SPLINE_SURFACE(((0.995079542144874,0.997234796441972,1.,0.996603060231143,
0.994126602224868,0.994126602224868,0.994126602224868),(0.995079542144874,
0.997234796441972,1.,0.996603060231143,0.994126602224868,0.994126602224868,
0.994126602224868)))
REPRESENTATION_ITEM('')
SURFACE()
);
#588=(
BOUNDED_SURFACE()
B_SPLINE_SURFACE(1,2,((#103072,#103073,#103074),(#103075,#103076,#103077)),
 .UNSPECIFIED.,.F.,.F.,.F.)
B_SPLINE_SURFACE_WITH_KNOTS((2,2),(3,3),(0.710192959008437,1.),(0.366820493751253,
0.384035903515169),.UNSPECIFIED.)
GEOMETRIC_REPRESENTATION_ITEM()
RATIONAL_B_SPLINE_SURFACE(((0.994126602224873,0.989721266390694,0.988228734781998),
(0.994126602224873,0.989721266390694,0.988228734781998)))
REPRESENTATION_ITEM('')
SURFACE()
);
#589=(
BOUNDED_SURFACE()
B_SPLINE_SURFACE(1,2,((#103086,#103087,#103088,#103089,#103090,#103091,
#103092),(#103093,#103094,#103095,#103096,#103097,#103098,#103099)),
 .UNSPECIFIED.,.F.,.F.,.F.)
B_SPLINE_SURFACE_WITH_KNOTS((2,2),(3,2,2,3),(0.710318915640083,1.),(0.349264991474409,
0.357142857142857,0.366820493751264,0.366996048774033),.UNSPECIFIED.)
GEOMETRIC_REPRESENTATION_ITEM()
RATIONAL_B_SPLINE_SURFACE(((0.995079542144874,0.997234796441972,1.,0.996603060231143,
0.994126602224867,0.994126602224867,0.994126602224867),(0.995079542144874,
0.997234796441972,1.,0.996603060231143,0.994126602224867,0.994126602224867,
0.994126602224867)))
REPRESENTATION_ITEM('')
SURFACE()
);
#590=(
BOUNDED_SURFACE()
B_SPLINE_SURFACE(1,2,((#103107,#103108,#103109),(#103110,#103111,#103112)),
 .UNSPECIFIED.,.F.,.F.,.F.)
B_SPLINE_SURFACE_WITH_KNOTS((2,2),(3,3),(0.710192959008444,1.),(0.366820493751253,
0.384035903515168),.UNSPECIFIED.)
GEOMETRIC_REPRESENTATION_ITEM()
RATIONAL_B_SPLINE_SURFACE(((0.994126602224873,0.989721266390695,0.988228734781999),
(0.994126602224873,0.989721266390695,0.988228734781999)))
REPRESENTATION_ITEM('')
SURFACE()
);
#591=(
BOUNDED_SURFACE()
B_SPLINE_SURFACE(1,2,((#103121,#103122,#103123,#103124,#103125,#103126,
#103127),(#103128,#103129,#103130,#103131,#103132,#103133,#103134)),
 .UNSPECIFIED.,.F.,.F.,.F.)
B_SPLINE_SURFACE_WITH_KNOTS((2,2),(3,2,2,3),(0.710318915640079,1.),(0.349264991474406,
0.357142857142857,0.366820493751254,0.366996048774023),.UNSPECIFIED.)
GEOMETRIC_REPRESENTATION_ITEM()
RATIONAL_B_SPLINE_SURFACE(((0.995079542144872,0.997234796441971,1.,0.996603060231146,
0.994126602224873,0.994126602224873,0.994126602224873),(0.995079542144872,
0.997234796441971,1.,0.996603060231146,0.994126602224873,0.994126602224873,
0.994126602224873)))
REPRESENTATION_ITEM('')
SURFACE()
);
#592=(
BOUNDED_SURFACE()
B_SPLINE_SURFACE(1,2,((#103142,#103143,#103144),(#103145,#103146,#103147)),
 .UNSPECIFIED.,.F.,.F.,.F.)
B_SPLINE_SURFACE_WITH_KNOTS((2,2),(3,3),(0.71019295900816,1.),(0.366820493751253,
0.384035903515168),.UNSPECIFIED.)
GEOMETRIC_REPRESENTATION_ITEM()
RATIONAL_B_SPLINE_SURFACE(((0.994126602224873,0.989721266390694,0.988228734781998),
(0.994126602224873,0.989721266390694,0.988228734781998)))
REPRESENTATION_ITEM('')
SURFACE()
);
#593=(
BOUNDED_SURFACE()
B_SPLINE_SURFACE(1,2,((#103156,#103157,#103158,#103159,#103160,#103161,
#103162),(#103163,#103164,#103165,#103166,#103167,#103168,#103169)),
 .UNSPECIFIED.,.F.,.F.,.F.)
B_SPLINE_SURFACE_WITH_KNOTS((2,2),(3,2,2,3),(0.710318915639601,1.),(0.349264991474411,
0.357142857142857,0.366820493751254,0.366996048774023),.UNSPECIFIED.)
GEOMETRIC_REPRESENTATION_ITEM()
RATIONAL_B_SPLINE_SURFACE(((0.995079542144875,0.997234796441973,1.,0.996603060231146,
0.994126602224873,0.994126602224873,0.994126602224873),(0.995079542144875,
0.997234796441973,1.,0.996603060231146,0.994126602224873,0.994126602224873,
0.994126602224873)))
REPRESENTATION_ITEM('')
SURFACE()
);
#594=(
BOUNDED_SURFACE()
B_SPLINE_SURFACE(1,2,((#103177,#103178,#103179),(#103180,#103181,#103182)),
 .UNSPECIFIED.,.F.,.F.,.F.)
B_SPLINE_SURFACE_WITH_KNOTS((2,2),(3,3),(0.710192959007978,1.),(0.366820493751235,
0.384035903515169),.UNSPECIFIED.)
GEOMETRIC_REPRESENTATION_ITEM()
RATIONAL_B_SPLINE_SURFACE(((0.994126602224882,0.989721266390696,0.988228734781998),
(0.994126602224882,0.989721266390696,0.988228734781998)))
REPRESENTATION_ITEM('')
SURFACE()
);
#595=(
BOUNDED_SURFACE()
B_SPLINE_SURFACE(1,2,((#103191,#103192,#103193,#103194,#103195,#103196,
#103197),(#103198,#103199,#103200,#103201,#103202,#103203,#103204)),
 .UNSPECIFIED.,.F.,.F.,.F.)
B_SPLINE_SURFACE_WITH_KNOTS((2,2),(3,2,2,3),(0.710318915639618,1.),(0.34926499147441,
0.357142857142857,0.366820493751254,0.366996048774023),.UNSPECIFIED.)
GEOMETRIC_REPRESENTATION_ITEM()
RATIONAL_B_SPLINE_SURFACE(((0.995079542144874,0.997234796441972,1.,0.996603060231146,
0.994126602224873,0.994126602224873,0.994126602224873),(0.995079542144874,
0.997234796441972,1.,0.996603060231146,0.994126602224873,0.994126602224873,
0.994126602224873)))
REPRESENTATION_ITEM('')
SURFACE()
);
#596=(
BOUNDED_SURFACE()
B_SPLINE_SURFACE(1,2,((#103212,#103213,#103214),(#103215,#103216,#103217)),
 .UNSPECIFIED.,.F.,.F.,.F.)
B_SPLINE_SURFACE_WITH_KNOTS((2,2),(3,3),(0.710192959008014,1.),(0.366820493751253,
0.384035903515169),.UNSPECIFIED.)
GEOMETRIC_REPRESENTATION_ITEM()
RATIONAL_B_SPLINE_SURFACE(((0.994126602224873,0.989721266390694,0.988228734781998),
(0.994126602224873,0.989721266390694,0.988228734781998)))
REPRESENTATION_ITEM('')
SURFACE()
);
#597=(
BOUNDED_SURFACE()
B_SPLINE_SURFACE(1,2,((#103226,#103227,#103228,#103229,#103230,#103231,
#103232),(#103233,#103234,#103235,#103236,#103237,#103238,#103239)),
 .UNSPECIFIED.,.F.,.F.,.F.)
B_SPLINE_SURFACE_WITH_KNOTS((2,2),(3,2,2,3),(0.710318915639658,1.),(0.34926499147441,
0.357142857142857,0.366820493751254,0.366996048774023),.UNSPECIFIED.)
GEOMETRIC_REPRESENTATION_ITEM()
RATIONAL_B_SPLINE_SURFACE(((0.995079542144874,0.997234796441972,1.,0.996603060231146,
0.994126602224873,0.994126602224873,0.994126602224873),(0.995079542144874,
0.997234796441972,1.,0.996603060231146,0.994126602224873,0.994126602224873,
0.994126602224873)))
REPRESENTATION_ITEM('')
SURFACE()
);
#598=(
BOUNDED_SURFACE()
B_SPLINE_SURFACE(1,2,((#103247,#103248,#103249),(#103250,#103251,#103252)),
 .UNSPECIFIED.,.F.,.F.,.F.)
B_SPLINE_SURFACE_WITH_KNOTS((2,2),(3,3),(0.710192959008105,1.),(0.366820493751253,
0.384035903515169),.UNSPECIFIED.)
GEOMETRIC_REPRESENTATION_ITEM()
RATIONAL_B_SPLINE_SURFACE(((0.994126602224873,0.989721266390694,0.988228734781998),
(0.994126602224873,0.989721266390694,0.988228734781998)))
REPRESENTATION_ITEM('')
SURFACE()
);
#599=(
BOUNDED_SURFACE()
B_SPLINE_SURFACE(1,2,((#103261,#103262,#103263,#103264,#103265,#103266,
#103267),(#103268,#103269,#103270,#103271,#103272,#103273,#103274)),
 .UNSPECIFIED.,.F.,.F.,.F.)
B_SPLINE_SURFACE_WITH_KNOTS((2,2),(3,2,2,3),(0.710318915639747,1.),(0.34926499147441,
0.357142857142857,0.366820493751255,0.366996048774024),.UNSPECIFIED.)
GEOMETRIC_REPRESENTATION_ITEM()
RATIONAL_B_SPLINE_SURFACE(((0.995079542144874,0.997234796441972,1.,0.996603060231146,
0.994126602224872,0.994126602224872,0.994126602224872),(0.995079542144874,
0.997234796441972,1.,0.996603060231146,0.994126602224872,0.994126602224872,
0.994126602224872)))
REPRESENTATION_ITEM('')
SURFACE()
);
#600=(
BOUNDED_SURFACE()
B_SPLINE_SURFACE(1,2,((#103282,#103283,#103284),(#103285,#103286,#103287)),
 .UNSPECIFIED.,.F.,.F.,.F.)
B_SPLINE_SURFACE_WITH_KNOTS((2,2),(3,3),(0.,0.289681084359928),(0.297753987024565,
0.314942866188516),.UNSPECIFIED.)
GEOMETRIC_REPRESENTATION_ITEM()
RATIONAL_B_SPLINE_SURFACE(((0.99297255681853,0.98897304955565,0.987877375613931),
(0.99297255681853,0.98897304955565,0.987877375613931)))
REPRESENTATION_ITEM('')
SURFACE()
);
#601=(
BOUNDED_SURFACE()
B_SPLINE_SURFACE(1,2,((#103296,#103297,#103298,#103299,#103300),(#103301,
#103302,#103303,#103304,#103305)),.UNSPECIFIED.,.F.,.F.,.F.)
B_SPLINE_SURFACE_WITH_KNOTS((2,2),(3,2,3),(0.,0.289807040992001),(0.418312080773434,
0.428571428571429,0.435879799328077),.UNSPECIFIED.)
GEOMETRIC_REPRESENTATION_ITEM()
RATIONAL_B_SPLINE_SURFACE(((0.99383221411677,0.99639887423472,1.,0.997434694412141,
0.995394338545807),(0.99383221411677,0.99639887423472,1.,0.997434694412141,
0.995394338545807)))
REPRESENTATION_ITEM('')
SURFACE()
);
#602=(
BOUNDED_SURFACE()
B_SPLINE_SURFACE(1,2,((#103313,#103314,#103315),(#103316,#103317,#103318)),
 .UNSPECIFIED.,.F.,.F.,.F.)
B_SPLINE_SURFACE_WITH_KNOTS((2,2),(3,3),(0.,0.289681084359927),(0.297753987024626,
0.314942866188684),.UNSPECIFIED.)
GEOMETRIC_REPRESENTATION_ITEM()
RATIONAL_B_SPLINE_SURFACE(((0.992972556818501,0.988973049555607,0.98787737561391),
(0.992972556818501,0.988973049555607,0.98787737561391)))
REPRESENTATION_ITEM('')
SURFACE()
);
#603=(
BOUNDED_SURFACE()
B_SPLINE_SURFACE(1,2,((#103327,#103328,#103329,#103330,#103331),(#103332,
#103333,#103334,#103335,#103336)),.UNSPECIFIED.,.F.,.F.,.F.)
B_SPLINE_SURFACE_WITH_KNOTS((2,2),(3,2,3),(0.,0.289807040991563),(0.418312080773433,
0.428571428571429,0.435879799328076),.UNSPECIFIED.)
GEOMETRIC_REPRESENTATION_ITEM()
RATIONAL_B_SPLINE_SURFACE(((0.993832214116769,0.99639887423472,1.,0.997434694412141,
0.995394338545808),(0.993832214116769,0.99639887423472,1.,0.997434694412141,
0.995394338545808)))
REPRESENTATION_ITEM('')
SURFACE()
);
#604=(
BOUNDED_SURFACE()
B_SPLINE_SURFACE(1,2,((#103344,#103345,#103346),(#103347,#103348,#103349)),
 .UNSPECIFIED.,.F.,.F.,.F.)
B_SPLINE_SURFACE_WITH_KNOTS((2,2),(3,3),(0.,0.289681084359919),(0.297753987024627,
0.314942866188517),.UNSPECIFIED.)
GEOMETRIC_REPRESENTATION_ITEM()
RATIONAL_B_SPLINE_SURFACE(((0.992972556818501,0.988973049555646,0.987877375613931),
(0.992972556818501,0.988973049555646,0.987877375613931)))
REPRESENTATION_ITEM('')
SURFACE()
);
#605=(
BOUNDED_SURFACE()
B_SPLINE_SURFACE(1,2,((#103358,#103359,#103360,#103361,#103362),(#103363,
#103364,#103365,#103366,#103367)),.UNSPECIFIED.,.F.,.F.,.F.)
B_SPLINE_SURFACE_WITH_KNOTS((2,2),(3,2,3),(0.,0.289807040991555),(0.418312080773433,
0.428571428571429,0.435879799328076),.UNSPECIFIED.)
GEOMETRIC_REPRESENTATION_ITEM()
RATIONAL_B_SPLINE_SURFACE(((0.993832214116769,0.99639887423472,1.,0.997434694412141,
0.995394338545808),(0.993832214116769,0.99639887423472,1.,0.997434694412141,
0.995394338545808)))
REPRESENTATION_ITEM('')
SURFACE()
);
#606=(
BOUNDED_SURFACE()
B_SPLINE_SURFACE(1,2,((#103375,#103376,#103377),(#103378,#103379,#103380)),
 .UNSPECIFIED.,.F.,.F.,.F.)
B_SPLINE_SURFACE_WITH_KNOTS((2,2),(3,3),(0.,0.289681084359924),(0.297753987024233,
0.314942866188517),.UNSPECIFIED.)
GEOMETRIC_REPRESENTATION_ITEM()
RATIONAL_B_SPLINE_SURFACE(((0.992972556818685,0.988973049555671,0.987877375613931),
(0.992972556818685,0.988973049555671,0.987877375613931)))
REPRESENTATION_ITEM('')
SURFACE()
);
#607=(
BOUNDED_SURFACE()
B_SPLINE_SURFACE(1,2,((#103389,#103390,#103391,#103392,#103393),(#103394,
#103395,#103396,#103397,#103398)),.UNSPECIFIED.,.F.,.F.,.F.)
B_SPLINE_SURFACE_WITH_KNOTS((2,2),(3,2,3),(0.,0.289807040991561),(0.418312080773433,
0.428571428571429,0.435879799328076),.UNSPECIFIED.)
GEOMETRIC_REPRESENTATION_ITEM()
RATIONAL_B_SPLINE_SURFACE(((0.993832214116769,0.99639887423472,1.,0.997434694412141,
0.995394338545808),(0.993832214116769,0.99639887423472,1.,0.997434694412141,
0.995394338545808)))
REPRESENTATION_ITEM('')
SURFACE()
);
#608=(
BOUNDED_SURFACE()
B_SPLINE_SURFACE(1,2,((#103406,#103407,#103408),(#103409,#103410,#103411)),
 .UNSPECIFIED.,.F.,.F.,.F.)
B_SPLINE_SURFACE_WITH_KNOTS((2,2),(3,3),(0.,0.28968108435992),(0.297753987024627,
0.314942866188517),.UNSPECIFIED.)
GEOMETRIC_REPRESENTATION_ITEM()
RATIONAL_B_SPLINE_SURFACE(((0.992972556818501,0.988973049555646,0.987877375613931),
(0.992972556818501,0.988973049555646,0.987877375613931)))
REPRESENTATION_ITEM('')
SURFACE()
);
#609=(
BOUNDED_SURFACE()
B_SPLINE_SURFACE(1,2,((#103420,#103421,#103422,#103423,#103424),(#103425,
#103426,#103427,#103428,#103429)),.UNSPECIFIED.,.F.,.F.,.F.)
B_SPLINE_SURFACE_WITH_KNOTS((2,2),(3,2,3),(0.,0.289807040991644),(0.418312080773434,
0.428571428571429,0.435879799328076),.UNSPECIFIED.)
GEOMETRIC_REPRESENTATION_ITEM()
RATIONAL_B_SPLINE_SURFACE(((0.99383221411677,0.99639887423472,1.,0.997434694412141,
0.995394338545808),(0.99383221411677,0.99639887423472,1.,0.997434694412141,
0.995394338545808)))
REPRESENTATION_ITEM('')
SURFACE()
);
#610=(
BOUNDED_SURFACE()
B_SPLINE_SURFACE(1,2,((#103437,#103438,#103439),(#103440,#103441,#103442)),
 .UNSPECIFIED.,.F.,.F.,.F.)
B_SPLINE_SURFACE_WITH_KNOTS((2,2),(3,3),(0.,0.289681084359923),(0.297753987024626,
0.314942866188516),.UNSPECIFIED.)
GEOMETRIC_REPRESENTATION_ITEM()
RATIONAL_B_SPLINE_SURFACE(((0.992972556818502,0.988973049555646,0.987877375613931),
(0.992972556818502,0.988973049555646,0.987877375613931)))
REPRESENTATION_ITEM('')
SURFACE()
);
#611=(
BOUNDED_SURFACE()
B_SPLINE_SURFACE(1,2,((#103451,#103452,#103453,#103454,#103455),(#103456,
#103457,#103458,#103459,#103460)),.UNSPECIFIED.,.F.,.F.,.F.)
B_SPLINE_SURFACE_WITH_KNOTS((2,2),(3,2,3),(0.,0.289807040991639),(0.418312080773434,
0.428571428571429,0.435879799328077),.UNSPECIFIED.)
GEOMETRIC_REPRESENTATION_ITEM()
RATIONAL_B_SPLINE_SURFACE(((0.99383221411677,0.996398874234721,1.,0.997434694412141,
0.995394338545807),(0.99383221411677,0.996398874234721,1.,0.997434694412141,
0.995394338545807)))
REPRESENTATION_ITEM('')
SURFACE()
);
#612=(
BOUNDED_SURFACE()
B_SPLINE_SURFACE(1,2,((#103468,#103469,#103470),(#103471,#103472,#103473)),
 .UNSPECIFIED.,.F.,.F.,.F.)
B_SPLINE_SURFACE_WITH_KNOTS((2,2),(3,3),(0.,0.289681084359918),(0.297753987024234,
0.314942866188516),.UNSPECIFIED.)
GEOMETRIC_REPRESENTATION_ITEM()
RATIONAL_B_SPLINE_SURFACE(((0.992972556818684,0.988973049555671,0.987877375613931),
(0.992972556818684,0.988973049555671,0.987877375613931)))
REPRESENTATION_ITEM('')
SURFACE()
);
#613=(
BOUNDED_SURFACE()
B_SPLINE_SURFACE(1,2,((#103482,#103483,#103484,#103485,#103486),(#103487,
#103488,#103489,#103490,#103491)),.UNSPECIFIED.,.F.,.F.,.F.)
B_SPLINE_SURFACE_WITH_KNOTS((2,2),(3,2,3),(0.,0.289807040991643),(0.418312080773434,
0.428571428571429,0.435879799328077),.UNSPECIFIED.)
GEOMETRIC_REPRESENTATION_ITEM()
RATIONAL_B_SPLINE_SURFACE(((0.99383221411677,0.99639887423472,1.,0.997434694412141,
0.995394338545807),(0.99383221411677,0.99639887423472,1.,0.997434694412141,
0.995394338545807)))
REPRESENTATION_ITEM('')
SURFACE()
);
#614=(
BOUNDED_SURFACE()
B_SPLINE_SURFACE(1,2,((#103499,#103500,#103501),(#103502,#103503,#103504)),
 .UNSPECIFIED.,.F.,.F.,.F.)
B_SPLINE_SURFACE_WITH_KNOTS((2,2),(3,3),(0.,0.289681084359921),(0.297753987024234,
0.314942866188516),.UNSPECIFIED.)
GEOMETRIC_REPRESENTATION_ITEM()
RATIONAL_B_SPLINE_SURFACE(((0.992972556818684,0.988973049555671,0.987877375613931),
(0.992972556818684,0.988973049555671,0.987877375613931)))
REPRESENTATION_ITEM('')
SURFACE()
);
#615=(
BOUNDED_SURFACE()
B_SPLINE_SURFACE(1,2,((#103513,#103514,#103515,#103516,#103517),(#103518,
#103519,#103520,#103521,#103522)),.UNSPECIFIED.,.F.,.F.,.F.)
B_SPLINE_SURFACE_WITH_KNOTS((2,2),(3,2,3),(0.,0.289807040991642),(0.418312080773434,
0.428571428571429,0.435879799328077),.UNSPECIFIED.)
GEOMETRIC_REPRESENTATION_ITEM()
RATIONAL_B_SPLINE_SURFACE(((0.99383221411677,0.996398874234721,1.,0.997434694412141,
0.995394338545807),(0.99383221411677,0.996398874234721,1.,0.997434694412141,
0.995394338545807)))
REPRESENTATION_ITEM('')
SURFACE()
);
#616=(
BOUNDED_SURFACE()
B_SPLINE_SURFACE(1,2,((#103530,#103531,#103532),(#103533,#103534,#103535)),
 .UNSPECIFIED.,.F.,.F.,.F.)
B_SPLINE_SURFACE_WITH_KNOTS((2,2),(3,3),(0.,0.289681084359921),(0.297753987024245,
0.314942866188516),.UNSPECIFIED.)
GEOMETRIC_REPRESENTATION_ITEM()
RATIONAL_B_SPLINE_SURFACE(((0.992972556818679,0.988973049555671,0.987877375613931),
(0.992972556818679,0.988973049555671,0.987877375613931)))
REPRESENTATION_ITEM('')
SURFACE()
);
#617=(
BOUNDED_SURFACE()
B_SPLINE_SURFACE(1,2,((#103544,#103545,#103546,#103547,#103548),(#103549,
#103550,#103551,#103552,#103553)),.UNSPECIFIED.,.F.,.F.,.F.)
B_SPLINE_SURFACE_WITH_KNOTS((2,2),(3,2,3),(0.,0.28980704099156),(0.418312080773434,
0.428571428571429,0.435879799328077),.UNSPECIFIED.)
GEOMETRIC_REPRESENTATION_ITEM()
RATIONAL_B_SPLINE_SURFACE(((0.99383221411677,0.996398874234721,1.,0.997434694412141,
0.995394338545807),(0.99383221411677,0.996398874234721,1.,0.997434694412141,
0.995394338545807)))
REPRESENTATION_ITEM('')
SURFACE()
);
#618=(
BOUNDED_SURFACE()
B_SPLINE_SURFACE(1,2,((#103561,#103562,#103563),(#103564,#103565,#103566)),
 .UNSPECIFIED.,.F.,.F.,.F.)
B_SPLINE_SURFACE_WITH_KNOTS((2,2),(3,3),(0.,0.289681084359924),(0.297753987024626,
0.314942866188516),.UNSPECIFIED.)
GEOMETRIC_REPRESENTATION_ITEM()
RATIONAL_B_SPLINE_SURFACE(((0.992972556818502,0.988973049555647,0.987877375613931),
(0.992972556818502,0.988973049555647,0.987877375613931)))
REPRESENTATION_ITEM('')
SURFACE()
);
#619=(
BOUNDED_SURFACE()
B_SPLINE_SURFACE(1,2,((#103575,#103576,#103577,#103578,#103579),(#103580,
#103581,#103582,#103583,#103584)),.UNSPECIFIED.,.F.,.F.,.F.)
B_SPLINE_SURFACE_WITH_KNOTS((2,2),(3,2,3),(0.,0.289807040991648),(0.418312080773434,
0.428571428571429,0.435879799328077),.UNSPECIFIED.)
GEOMETRIC_REPRESENTATION_ITEM()
RATIONAL_B_SPLINE_SURFACE(((0.99383221411677,0.996398874234721,1.,0.997434694412141,
0.995394338545807),(0.99383221411677,0.996398874234721,1.,0.997434694412141,
0.995394338545807)))
REPRESENTATION_ITEM('')
SURFACE()
);
#620=(
BOUNDED_SURFACE()
B_SPLINE_SURFACE(1,2,((#103592,#103593,#103594),(#103595,#103596,#103597)),
 .UNSPECIFIED.,.F.,.F.,.F.)
B_SPLINE_SURFACE_WITH_KNOTS((2,2),(3,3),(0.,0.289681084359922),(0.297753987024626,
0.314942866188516),.UNSPECIFIED.)
GEOMETRIC_REPRESENTATION_ITEM()
RATIONAL_B_SPLINE_SURFACE(((0.992972556818502,0.988973049555646,0.987877375613931),
(0.992972556818502,0.988973049555646,0.987877375613931)))
REPRESENTATION_ITEM('')
SURFACE()
);
#621=(
BOUNDED_SURFACE()
B_SPLINE_SURFACE(1,2,((#103606,#103607,#103608,#103609,#103610),(#103611,
#103612,#103613,#103614,#103615)),.UNSPECIFIED.,.F.,.F.,.F.)
B_SPLINE_SURFACE_WITH_KNOTS((2,2),(3,2,3),(0.,0.289807040991562),(0.418312080773434,
0.428571428571429,0.435879799328077),.UNSPECIFIED.)
GEOMETRIC_REPRESENTATION_ITEM()
RATIONAL_B_SPLINE_SURFACE(((0.99383221411677,0.99639887423472,1.,0.997434694412141,
0.995394338545807),(0.99383221411677,0.99639887423472,1.,0.997434694412141,
0.995394338545807)))
REPRESENTATION_ITEM('')
SURFACE()
);
#622=(
BOUNDED_SURFACE()
B_SPLINE_SURFACE(1,2,((#103623,#103624,#103625),(#103626,#103627,#103628)),
 .UNSPECIFIED.,.F.,.F.,.F.)
B_SPLINE_SURFACE_WITH_KNOTS((2,2),(3,3),(0.,0.289681084359921),(0.297753987024245,
0.314942866188516),.UNSPECIFIED.)
GEOMETRIC_REPRESENTATION_ITEM()
RATIONAL_B_SPLINE_SURFACE(((0.992972556818679,0.988973049555671,0.987877375613931),
(0.992972556818679,0.988973049555671,0.987877375613931)))
REPRESENTATION_ITEM('')
SURFACE()
);
#623=(
BOUNDED_SURFACE()
B_SPLINE_SURFACE(1,2,((#103637,#103638,#103639,#103640,#103641),(#103642,
#103643,#103644,#103645,#103646)),.UNSPECIFIED.,.F.,.F.,.F.)
B_SPLINE_SURFACE_WITH_KNOTS((2,2),(3,2,3),(0.,0.289807040991916),(0.418312080773434,
0.428571428571429,0.435879799328077),.UNSPECIFIED.)
GEOMETRIC_REPRESENTATION_ITEM()
RATIONAL_B_SPLINE_SURFACE(((0.99383221411677,0.996398874234721,1.,0.997434694412141,
0.995394338545807),(0.99383221411677,0.996398874234721,1.,0.997434694412141,
0.995394338545807)))
REPRESENTATION_ITEM('')
SURFACE()
);
#624=(
BOUNDED_SURFACE()
B_SPLINE_SURFACE(1,2,((#103654,#103655,#103656),(#103657,#103658,#103659)),
 .UNSPECIFIED.,.F.,.F.,.F.)
B_SPLINE_SURFACE_WITH_KNOTS((2,2),(3,3),(0.,0.28968108435992),(0.297753987024247,
0.314942866188516),.UNSPECIFIED.)
GEOMETRIC_REPRESENTATION_ITEM()
RATIONAL_B_SPLINE_SURFACE(((0.992972556818678,0.988973049555671,0.987877375613931),
(0.992972556818678,0.98897304955567,0.987877375613931)))
REPRESENTATION_ITEM('')
SURFACE()
);
#625=(
BOUNDED_SURFACE()
B_SPLINE_SURFACE(1,2,((#103668,#103669,#103670,#103671,#103672),(#103673,
#103674,#103675,#103676,#103677)),.UNSPECIFIED.,.F.,.F.,.F.)
B_SPLINE_SURFACE_WITH_KNOTS((2,2),(3,2,3),(0.,0.28980704099297),(0.418312080773434,
0.428571428571429,0.435879799328077),.UNSPECIFIED.)
GEOMETRIC_REPRESENTATION_ITEM()
RATIONAL_B_SPLINE_SURFACE(((0.99383221411677,0.996398874234721,1.,0.997434694412141,
0.995394338545807),(0.99383221411677,0.996398874234721,1.,0.997434694412141,
0.995394338545807)))
REPRESENTATION_ITEM('')
SURFACE()
);
#626=(
BOUNDED_SURFACE()
B_SPLINE_SURFACE(1,2,((#103685,#103686,#103687),(#103688,#103689,#103690)),
 .UNSPECIFIED.,.F.,.F.,.F.)
B_SPLINE_SURFACE_WITH_KNOTS((2,2),(3,3),(0.,0.28968108435992),(0.297753987024626,
0.314942866188516),.UNSPECIFIED.)
GEOMETRIC_REPRESENTATION_ITEM()
RATIONAL_B_SPLINE_SURFACE(((0.992972556818502,0.988973049555647,0.987877375613931),
(0.992972556818502,0.988973049555647,0.987877375613931)))
REPRESENTATION_ITEM('')
SURFACE()
);
#627=(
BOUNDED_SURFACE()
B_SPLINE_SURFACE(1,2,((#103699,#103700,#103701,#103702,#103703),(#103704,
#103705,#103706,#103707,#103708)),.UNSPECIFIED.,.F.,.F.,.F.)
B_SPLINE_SURFACE_WITH_KNOTS((2,2),(3,2,3),(0.,0.289807040991686),(0.418312080773434,
0.428571428571429,0.435879799328077),.UNSPECIFIED.)
GEOMETRIC_REPRESENTATION_ITEM()
RATIONAL_B_SPLINE_SURFACE(((0.99383221411677,0.99639887423472,1.,0.997434694412141,
0.995394338545807),(0.99383221411677,0.99639887423472,1.,0.997434694412141,
0.995394338545807)))
REPRESENTATION_ITEM('')
SURFACE()
);
#628=(
BOUNDED_SURFACE()
B_SPLINE_SURFACE(1,2,((#103716,#103717,#103718),(#103719,#103720,#103721)),
 .UNSPECIFIED.,.F.,.F.,.F.)
B_SPLINE_SURFACE_WITH_KNOTS((2,2),(3,3),(0.,0.289681084359925),(0.297753987024473,
0.314942866188516),.UNSPECIFIED.)
GEOMETRIC_REPRESENTATION_ITEM()
RATIONAL_B_SPLINE_SURFACE(((0.992972556818573,0.988973049555656,0.987877375613931),
(0.992972556818573,0.988973049555656,0.987877375613931)))
REPRESENTATION_ITEM('')
SURFACE()
);
#629=(
BOUNDED_SURFACE()
B_SPLINE_SURFACE(1,2,((#103730,#103731,#103732,#103733,#103734),(#103735,
#103736,#103737,#103738,#103739)),.UNSPECIFIED.,.F.,.F.,.F.)
B_SPLINE_SURFACE_WITH_KNOTS((2,2),(3,2,3),(0.,0.289807040991566),(0.418312080773433,
0.428571428571429,0.435879799328077),.UNSPECIFIED.)
GEOMETRIC_REPRESENTATION_ITEM()
RATIONAL_B_SPLINE_SURFACE(((0.99383221411677,0.99639887423472,1.,0.997434694412141,
0.995394338545807),(0.99383221411677,0.99639887423472,1.,0.997434694412141,
0.995394338545807)))
REPRESENTATION_ITEM('')
SURFACE()
);
#630=(
BOUNDED_SURFACE()
B_SPLINE_SURFACE(1,2,((#103747,#103748,#103749),(#103750,#103751,#103752)),
 .UNSPECIFIED.,.F.,.F.,.F.)
B_SPLINE_SURFACE_WITH_KNOTS((2,2),(3,3),(0.,0.289681084359922),(0.297753987024626,
0.314942866188516),.UNSPECIFIED.)
GEOMETRIC_REPRESENTATION_ITEM()
RATIONAL_B_SPLINE_SURFACE(((0.992972556818502,0.988973049555646,0.987877375613931),
(0.992972556818502,0.988973049555646,0.987877375613931)))
REPRESENTATION_ITEM('')
SURFACE()
);
#631=(
BOUNDED_SURFACE()
B_SPLINE_SURFACE(1,2,((#103761,#103762,#103763,#103764,#103765),(#103766,
#103767,#103768,#103769,#103770)),.UNSPECIFIED.,.F.,.F.,.F.)
B_SPLINE_SURFACE_WITH_KNOTS((2,2),(3,2,3),(0.,0.289807040991795),(0.418312080773434,
0.428571428571429,0.435879799328077),.UNSPECIFIED.)
GEOMETRIC_REPRESENTATION_ITEM()
RATIONAL_B_SPLINE_SURFACE(((0.99383221411677,0.996398874234721,1.,0.997434694412141,
0.995394338545807),(0.99383221411677,0.996398874234721,1.,0.997434694412141,
0.995394338545807)))
REPRESENTATION_ITEM('')
SURFACE()
);
#632=(
BOUNDED_SURFACE()
B_SPLINE_SURFACE(1,2,((#103778,#103779,#103780),(#103781,#103782,#103783)),
 .UNSPECIFIED.,.F.,.F.,.F.)
B_SPLINE_SURFACE_WITH_KNOTS((2,2),(3,3),(0.,0.289681084359927),(0.297753987024626,
0.314942866188516),.UNSPECIFIED.)
GEOMETRIC_REPRESENTATION_ITEM()
RATIONAL_B_SPLINE_SURFACE(((0.992972556818501,0.988973049555646,0.987877375613931),
(0.992972556818501,0.988973049555646,0.987877375613931)))
REPRESENTATION_ITEM('')
SURFACE()
);
#633=(
BOUNDED_SURFACE()
B_SPLINE_SURFACE(1,2,((#103792,#103793,#103794,#103795,#103796),(#103797,
#103798,#103799,#103800,#103801)),.UNSPECIFIED.,.F.,.F.,.F.)
B_SPLINE_SURFACE_WITH_KNOTS((2,2),(3,2,3),(0.,0.28980704099156),(0.418312080773434,
0.428571428571429,0.435879799328077),.UNSPECIFIED.)
GEOMETRIC_REPRESENTATION_ITEM()
RATIONAL_B_SPLINE_SURFACE(((0.99383221411677,0.996398874234721,1.,0.997434694412141,
0.995394338545807),(0.99383221411677,0.996398874234721,1.,0.997434694412141,
0.995394338545807)))
REPRESENTATION_ITEM('')
SURFACE()
);
#634=(
BOUNDED_SURFACE()
B_SPLINE_SURFACE(1,2,((#103809,#103810,#103811),(#103812,#103813,#103814)),
 .UNSPECIFIED.,.F.,.F.,.F.)
B_SPLINE_SURFACE_WITH_KNOTS((2,2),(3,3),(0.,0.289681084359927),(0.297753987024626,
0.314942866188516),.UNSPECIFIED.)
GEOMETRIC_REPRESENTATION_ITEM()
RATIONAL_B_SPLINE_SURFACE(((0.992972556818502,0.988973049555646,0.987877375613931),
(0.992972556818502,0.988973049555646,0.987877375613931)))
REPRESENTATION_ITEM('')
SURFACE()
);
#635=(
BOUNDED_SURFACE()
B_SPLINE_SURFACE(1,2,((#103823,#103824,#103825,#103826,#103827),(#103828,
#103829,#103830,#103831,#103832)),.UNSPECIFIED.,.F.,.F.,.F.)
B_SPLINE_SURFACE_WITH_KNOTS((2,2),(3,2,3),(0.,0.289807040992696),(0.418312080773434,
0.428571428571429,0.435879799328077),.UNSPECIFIED.)
GEOMETRIC_REPRESENTATION_ITEM()
RATIONAL_B_SPLINE_SURFACE(((0.99383221411677,0.996398874234721,1.,0.997434694412141,
0.995394338545807),(0.99383221411677,0.996398874234721,1.,0.997434694412141,
0.995394338545807)))
REPRESENTATION_ITEM('')
SURFACE()
);
#636=(
BOUNDED_SURFACE()
B_SPLINE_SURFACE(1,2,((#103840,#103841,#103842),(#103843,#103844,#103845)),
 .UNSPECIFIED.,.F.,.F.,.F.)
B_SPLINE_SURFACE_WITH_KNOTS((2,2),(3,3),(0.,0.289681084359927),(0.297753987024626,
0.314942866188516),.UNSPECIFIED.)
GEOMETRIC_REPRESENTATION_ITEM()
RATIONAL_B_SPLINE_SURFACE(((0.992972556818502,0.988973049555646,0.987877375613931),
(0.992972556818502,0.988973049555646,0.987877375613931)))
REPRESENTATION_ITEM('')
SURFACE()
);
#637=(
BOUNDED_SURFACE()
B_SPLINE_SURFACE(1,2,((#103854,#103855,#103856,#103857,#103858),(#103859,
#103860,#103861,#103862,#103863)),.UNSPECIFIED.,.F.,.F.,.F.)
B_SPLINE_SURFACE_WITH_KNOTS((2,2),(3,2,3),(0.,0.289807040992534),(0.418312080773434,
0.428571428571429,0.435879799328077),.UNSPECIFIED.)
GEOMETRIC_REPRESENTATION_ITEM()
RATIONAL_B_SPLINE_SURFACE(((0.99383221411677,0.996398874234721,1.,0.997434694412141,
0.995394338545807),(0.99383221411677,0.996398874234721,1.,0.997434694412141,
0.995394338545807)))
REPRESENTATION_ITEM('')
SURFACE()
);
#638=(
BOUNDED_SURFACE()
B_SPLINE_SURFACE(1,2,((#103871,#103872,#103873),(#103874,#103875,#103876)),
 .UNSPECIFIED.,.F.,.F.,.F.)
B_SPLINE_SURFACE_WITH_KNOTS((2,2),(3,3),(0.,0.289681084359924),(0.297753987024145,
0.314942866188516),.UNSPECIFIED.)
GEOMETRIC_REPRESENTATION_ITEM()
RATIONAL_B_SPLINE_SURFACE(((0.992972556818725,0.988973049555677,0.987877375613931),
(0.992972556818725,0.988973049555677,0.987877375613931)))
REPRESENTATION_ITEM('')
SURFACE()
);
#639=(
BOUNDED_SURFACE()
B_SPLINE_SURFACE(1,2,((#103885,#103886,#103887,#103888,#103889),(#103890,
#103891,#103892,#103893,#103894)),.UNSPECIFIED.,.F.,.F.,.F.)
B_SPLINE_SURFACE_WITH_KNOTS((2,2),(3,2,3),(0.,0.289807040992668),(0.418312080773434,
0.428571428571429,0.435879799328077),.UNSPECIFIED.)
GEOMETRIC_REPRESENTATION_ITEM()
RATIONAL_B_SPLINE_SURFACE(((0.99383221411677,0.996398874234721,1.,0.997434694412141,
0.995394338545807),(0.99383221411677,0.996398874234721,1.,0.997434694412141,
0.995394338545807)))
REPRESENTATION_ITEM('')
SURFACE()
);
#640=(
BOUNDED_SURFACE()
B_SPLINE_SURFACE(1,2,((#103902,#103903,#103904),(#103905,#103906,#103907)),
 .UNSPECIFIED.,.F.,.F.,.F.)
B_SPLINE_SURFACE_WITH_KNOTS((2,2),(3,3),(0.,0.28968108435992),(0.297753987024274,
0.314942866188516),.UNSPECIFIED.)
GEOMETRIC_REPRESENTATION_ITEM()
RATIONAL_B_SPLINE_SURFACE(((0.992972556818666,0.988973049555669,0.987877375613931),
(0.992972556818666,0.988973049555669,0.987877375613932)))
REPRESENTATION_ITEM('')
SURFACE()
);
#641=(
BOUNDED_SURFACE()
B_SPLINE_SURFACE(1,2,((#103916,#103917,#103918,#103919,#103920),(#103921,
#103922,#103923,#103924,#103925)),.UNSPECIFIED.,.F.,.F.,.F.)
B_SPLINE_SURFACE_WITH_KNOTS((2,2),(3,2,3),(0.,0.289807040991766),(0.418312080773434,
0.428571428571429,0.435879799328077),.UNSPECIFIED.)
GEOMETRIC_REPRESENTATION_ITEM()
RATIONAL_B_SPLINE_SURFACE(((0.99383221411677,0.996398874234721,1.,0.997434694412141,
0.995394338545807),(0.99383221411677,0.996398874234721,1.,0.997434694412141,
0.995394338545807)))
REPRESENTATION_ITEM('')
SURFACE()
);
#642=(
BOUNDED_SURFACE()
B_SPLINE_SURFACE(1,2,((#103933,#103934,#103935),(#103936,#103937,#103938)),
 .UNSPECIFIED.,.F.,.F.,.F.)
B_SPLINE_SURFACE_WITH_KNOTS((2,2),(3,3),(0.,0.289681084359923),(0.297753987024625,
0.314942866188631),.UNSPECIFIED.)
GEOMETRIC_REPRESENTATION_ITEM()
RATIONAL_B_SPLINE_SURFACE(((0.992972556818502,0.98897304955562,0.987877375613917),
(0.992972556818502,0.98897304955562,0.987877375613917)))
REPRESENTATION_ITEM('')
SURFACE()
);
#643=(
BOUNDED_SURFACE()
B_SPLINE_SURFACE(1,2,((#103947,#103948,#103949,#103950,#103951),(#103952,
#103953,#103954,#103955,#103956)),.UNSPECIFIED.,.F.,.F.,.F.)
B_SPLINE_SURFACE_WITH_KNOTS((2,2),(3,2,3),(0.,0.289807040992909),(0.418312080773434,
0.428571428571429,0.435879799328077),.UNSPECIFIED.)
GEOMETRIC_REPRESENTATION_ITEM()
RATIONAL_B_SPLINE_SURFACE(((0.99383221411677,0.996398874234721,1.,0.997434694412141,
0.995394338545807),(0.99383221411677,0.996398874234721,1.,0.997434694412141,
0.995394338545807)))
REPRESENTATION_ITEM('')
SURFACE()
);
#644=(
BOUNDED_SURFACE()
B_SPLINE_SURFACE(1,2,((#103964,#103965,#103966),(#103967,#103968,#103969)),
 .UNSPECIFIED.,.F.,.F.,.F.)
B_SPLINE_SURFACE_WITH_KNOTS((2,2),(3,3),(0.,0.289681084359929),(0.297753987024626,
0.314942866188516),.UNSPECIFIED.)
GEOMETRIC_REPRESENTATION_ITEM()
RATIONAL_B_SPLINE_SURFACE(((0.992972556818501,0.988973049555646,0.987877375613931),
(0.992972556818501,0.988973049555646,0.987877375613931)))
REPRESENTATION_ITEM('')
SURFACE()
);
#645=(
BOUNDED_SURFACE()
B_SPLINE_SURFACE(1,2,((#103978,#103979,#103980,#103981,#103982),(#103983,
#103984,#103985,#103986,#103987)),.UNSPECIFIED.,.F.,.F.,.F.)
B_SPLINE_SURFACE_WITH_KNOTS((2,2),(3,2,3),(0.,0.28980704099269),(0.418312080773434,
0.428571428571429,0.435879799328077),.UNSPECIFIED.)
GEOMETRIC_REPRESENTATION_ITEM()
RATIONAL_B_SPLINE_SURFACE(((0.99383221411677,0.99639887423472,1.,0.997434694412141,
0.995394338545807),(0.99383221411677,0.99639887423472,1.,0.997434694412141,
0.995394338545807)))
REPRESENTATION_ITEM('')
SURFACE()
);
#646=(
BOUNDED_SURFACE()
B_SPLINE_SURFACE(1,2,((#103995,#103996,#103997),(#103998,#103999,#104000)),
 .UNSPECIFIED.,.F.,.F.,.F.)
B_SPLINE_SURFACE_WITH_KNOTS((2,2),(3,3),(0.,0.289681084359937),(0.297753987024626,
0.314942866188516),.UNSPECIFIED.)
GEOMETRIC_REPRESENTATION_ITEM()
RATIONAL_B_SPLINE_SURFACE(((0.992972556818501,0.988973049555646,0.987877375613931),
(0.992972556818501,0.988973049555646,0.987877375613931)))
REPRESENTATION_ITEM('')
SURFACE()
);
#647=(
BOUNDED_SURFACE()
B_SPLINE_SURFACE(1,2,((#104009,#104010,#104011,#104012,#104013),(#104014,
#104015,#104016,#104017,#104018)),.UNSPECIFIED.,.F.,.F.,.F.)
B_SPLINE_SURFACE_WITH_KNOTS((2,2),(3,2,3),(0.,0.289807040992446),(0.418312080773434,
0.428571428571429,0.435879799328077),.UNSPECIFIED.)
GEOMETRIC_REPRESENTATION_ITEM()
RATIONAL_B_SPLINE_SURFACE(((0.99383221411677,0.996398874234721,1.,0.997434694412141,
0.995394338545807),(0.99383221411677,0.996398874234721,1.,0.997434694412141,
0.995394338545807)))
REPRESENTATION_ITEM('')
SURFACE()
);
#648=(
BOUNDED_SURFACE()
B_SPLINE_SURFACE(1,2,((#104026,#104027,#104028),(#104029,#104030,#104031)),
 .UNSPECIFIED.,.F.,.F.,.F.)
B_SPLINE_SURFACE_WITH_KNOTS((2,2),(3,3),(0.,0.289681084359928),(0.297753987024165,
0.314942866188516),.UNSPECIFIED.)
GEOMETRIC_REPRESENTATION_ITEM()
RATIONAL_B_SPLINE_SURFACE(((0.992972556818716,0.988973049555676,0.987877375613931),
(0.992972556818716,0.988973049555676,0.987877375613931)))
REPRESENTATION_ITEM('')
SURFACE()
);
#649=(
BOUNDED_SURFACE()
B_SPLINE_SURFACE(1,2,((#104040,#104041,#104042,#104043,#104044),(#104045,
#104046,#104047,#104048,#104049)),.UNSPECIFIED.,.F.,.F.,.F.)
B_SPLINE_SURFACE_WITH_KNOTS((2,2),(3,2,3),(0.,0.289807040992323),(0.418312080773434,
0.428571428571429,0.43587979932776),.UNSPECIFIED.)
GEOMETRIC_REPRESENTATION_ITEM()
RATIONAL_B_SPLINE_SURFACE(((0.99383221411677,0.996398874234721,1.,0.997434694412253,
0.995394338545984),(0.99383221411677,0.996398874234721,1.,0.997434694412253,
0.995394338545984)))
REPRESENTATION_ITEM('')
SURFACE()
);
#650=(
BOUNDED_SURFACE()
B_SPLINE_SURFACE(1,2,((#104057,#104058,#104059),(#104060,#104061,#104062)),
 .UNSPECIFIED.,.F.,.F.,.F.)
B_SPLINE_SURFACE_WITH_KNOTS((2,2),(3,3),(0.,0.289681084359923),(0.297753987024626,
0.314942866188518),.UNSPECIFIED.)
GEOMETRIC_REPRESENTATION_ITEM()
RATIONAL_B_SPLINE_SURFACE(((0.992972556818501,0.988973049555646,0.987877375613931),
(0.992972556818501,0.988973049555646,0.987877375613931)))
REPRESENTATION_ITEM('')
SURFACE()
);
#651=(
BOUNDED_SURFACE()
B_SPLINE_SURFACE(1,2,((#104071,#104072,#104073,#104074,#104075),(#104076,
#104077,#104078,#104079,#104080)),.UNSPECIFIED.,.F.,.F.,.F.)
B_SPLINE_SURFACE_WITH_KNOTS((2,2),(3,2,3),(0.,0.289807040992806),(0.418312080773434,
0.428571428571429,0.435879799328077),.UNSPECIFIED.)
GEOMETRIC_REPRESENTATION_ITEM()
RATIONAL_B_SPLINE_SURFACE(((0.99383221411677,0.99639887423472,1.,0.997434694412141,
0.995394338545807),(0.99383221411677,0.99639887423472,1.,0.997434694412141,
0.995394338545807)))
REPRESENTATION_ITEM('')
SURFACE()
);
#652=(
BOUNDED_SURFACE()
B_SPLINE_SURFACE(1,2,((#104088,#104089,#104090),(#104091,#104092,#104093)),
 .UNSPECIFIED.,.F.,.F.,.F.)
B_SPLINE_SURFACE_WITH_KNOTS((2,2),(3,3),(0.,0.289681084359917),(0.297753987024276,
0.314942866188516),.UNSPECIFIED.)
GEOMETRIC_REPRESENTATION_ITEM()
RATIONAL_B_SPLINE_SURFACE(((0.992972556818665,0.988973049555669,0.987877375613931),
(0.992972556818665,0.988973049555669,0.987877375613931)))
REPRESENTATION_ITEM('')
SURFACE()
);
#653=(
BOUNDED_SURFACE()
B_SPLINE_SURFACE(1,2,((#104102,#104103,#104104,#104105,#104106),(#104107,
#104108,#104109,#104110,#104111)),.UNSPECIFIED.,.F.,.F.,.F.)
B_SPLINE_SURFACE_WITH_KNOTS((2,2),(3,2,3),(0.,0.289807040992654),(0.418312080773434,
0.428571428571429,0.435879799328077),.UNSPECIFIED.)
GEOMETRIC_REPRESENTATION_ITEM()
RATIONAL_B_SPLINE_SURFACE(((0.99383221411677,0.996398874234721,1.,0.997434694412141,
0.995394338545807),(0.99383221411677,0.996398874234721,1.,0.997434694412141,
0.995394338545807)))
REPRESENTATION_ITEM('')
SURFACE()
);
#654=(
BOUNDED_SURFACE()
B_SPLINE_SURFACE(1,2,((#104119,#104120,#104121),(#104122,#104123,#104124)),
 .UNSPECIFIED.,.F.,.F.,.F.)
B_SPLINE_SURFACE_WITH_KNOTS((2,2),(3,3),(0.,0.289681084359925),(0.29775398702428,
0.314942866188516),.UNSPECIFIED.)
GEOMETRIC_REPRESENTATION_ITEM()
RATIONAL_B_SPLINE_SURFACE(((0.992972556818663,0.988973049555669,0.987877375613931),
(0.992972556818663,0.988973049555669,0.987877375613931)))
REPRESENTATION_ITEM('')
SURFACE()
);
#655=(
BOUNDED_SURFACE()
B_SPLINE_SURFACE(1,2,((#104133,#104134,#104135,#104136,#104137),(#104138,
#104139,#104140,#104141,#104142)),.UNSPECIFIED.,.F.,.F.,.F.)
B_SPLINE_SURFACE_WITH_KNOTS((2,2),(3,2,3),(0.,0.289807040992678),(0.418312080773434,
0.428571428571429,0.435879799327938),.UNSPECIFIED.)
GEOMETRIC_REPRESENTATION_ITEM()
RATIONAL_B_SPLINE_SURFACE(((0.99383221411677,0.99639887423472,1.,0.99743469441219,
0.995394338545885),(0.99383221411677,0.99639887423472,1.,0.99743469441219,
0.995394338545885)))
REPRESENTATION_ITEM('')
SURFACE()
);
#656=(
BOUNDED_SURFACE()
B_SPLINE_SURFACE(1,2,((#104150,#104151,#104152),(#104153,#104154,#104155)),
 .UNSPECIFIED.,.F.,.F.,.F.)
B_SPLINE_SURFACE_WITH_KNOTS((2,2),(3,3),(0.,0.289681084359921),(0.297753987024197,
0.314942866188516),.UNSPECIFIED.)
GEOMETRIC_REPRESENTATION_ITEM()
RATIONAL_B_SPLINE_SURFACE(((0.992972556818701,0.988973049555674,0.987877375613931),
(0.992972556818701,0.988973049555674,0.987877375613931)))
REPRESENTATION_ITEM('')
SURFACE()
);
#657=(
BOUNDED_SURFACE()
B_SPLINE_SURFACE(1,2,((#104164,#104165,#104166,#104167,#104168),(#104169,
#104170,#104171,#104172,#104173)),.UNSPECIFIED.,.F.,.F.,.F.)
B_SPLINE_SURFACE_WITH_KNOTS((2,2),(3,2,3),(0.,0.28980704099286),(0.418312080773434,
0.428571428571429,0.435879799328077),.UNSPECIFIED.)
GEOMETRIC_REPRESENTATION_ITEM()
RATIONAL_B_SPLINE_SURFACE(((0.99383221411677,0.996398874234721,1.,0.997434694412141,
0.995394338545807),(0.99383221411677,0.99639887423472,1.,0.997434694412141,
0.995394338545807)))
REPRESENTATION_ITEM('')
SURFACE()
);
#658=(
BOUNDED_SURFACE()
B_SPLINE_SURFACE(1,2,((#104181,#104182,#104183),(#104184,#104185,#104186)),
 .UNSPECIFIED.,.F.,.F.,.F.)
B_SPLINE_SURFACE_WITH_KNOTS((2,2),(3,3),(0.,0.289681084359929),(0.366717817351071,
0.383933227114987),.UNSPECIFIED.)
GEOMETRIC_REPRESENTATION_ITEM()
RATIONAL_B_SPLINE_SURFACE(((0.994179254576314,0.989756546152321,0.988246641953811),
(0.994179254576314,0.989756546152321,0.988246641953811)))
REPRESENTATION_ITEM('')
SURFACE()
);
#659=(
BOUNDED_SURFACE()
B_SPLINE_SURFACE(1,2,((#104197,#104198,#104199,#104200,#104201,#104202,
#104203),(#104204,#104205,#104206,#104207,#104208,#104209,#104210)),
 .UNSPECIFIED.,.F.,.F.,.F.)
B_SPLINE_SURFACE_WITH_KNOTS((2,2),(3,2,2,3),(-0.000384471073508479,0.289807040992007),
(0.348985225175754,0.349369696259361,0.357142857142857,0.367204964717613),
 .UNSPECIFIED.)
GEOMETRIC_REPRESENTATION_ITEM()
RATIONAL_B_SPLINE_SURFACE(((0.995136940902289,0.99513694090229,0.99513694090229,
0.997271548787858,1.,0.996468107373496,0.993931286686403),(0.99513694090229,
0.99513694090229,0.99513694090229,0.997271548787858,1.,0.996468107373496,
0.993931286686403)))
REPRESENTATION_ITEM('')
SURFACE()
);
#660=(
BOUNDED_SURFACE()
B_SPLINE_SURFACE(1,2,((#104233,#104234,#104235),(#104236,#104237,#104238)),
 .UNSPECIFIED.,.F.,.F.,.F.)
B_SPLINE_SURFACE_WITH_KNOTS((2,2),(3,3),(0.,0.289681084359933),(0.366717817351071,
0.383933227114989),.UNSPECIFIED.)
GEOMETRIC_REPRESENTATION_ITEM()
RATIONAL_B_SPLINE_SURFACE(((0.994179254576313,0.98975654615232,0.98824664195381),
(0.994179254576313,0.98975654615232,0.98824664195381)))
REPRESENTATION_ITEM('')
SURFACE()
);
#661=(
BOUNDED_SURFACE()
B_SPLINE_SURFACE(1,2,((#104240,#104241,#104242,#104243,#104244,#104245,
#104246),(#104247,#104248,#104249,#104250,#104251,#104252,#104253)),
 .UNSPECIFIED.,.F.,.F.,.F.)
B_SPLINE_SURFACE_WITH_KNOTS((2,2),(3,2,2,3),(-0.000384470876990202,0.289807040992908),
(0.348985225379442,0.349369696259359,0.357142857142857,0.3672049644935),
 .UNSPECIFIED.)
GEOMETRIC_REPRESENTATION_ITEM()
RATIONAL_B_SPLINE_SURFACE(((0.995136940902289,0.995136940902289,0.995136940902289,
0.997271548787858,1.,0.996468107452162,0.993931286799409),(0.995136940902289,
0.995136940902289,0.995136940902289,0.997271548787858,1.,0.996468107452162,
0.993931286799409)))
REPRESENTATION_ITEM('')
SURFACE()
);
#662=(
BOUNDED_SURFACE()
B_SPLINE_SURFACE(1,2,((#104276,#104277,#104278),(#104279,#104280,#104281)),
 .UNSPECIFIED.,.F.,.F.,.F.)
B_SPLINE_SURFACE_WITH_KNOTS((2,2),(3,3),(0.,0.289681084359918),(0.366717817351071,
0.383933227114993),.UNSPECIFIED.)
GEOMETRIC_REPRESENTATION_ITEM()
RATIONAL_B_SPLINE_SURFACE(((0.994179254576314,0.989756546152319,0.98824664195381),
(0.994179254576314,0.989756546152319,0.98824664195381)))
REPRESENTATION_ITEM('')
SURFACE()
);
#663=(
BOUNDED_SURFACE()
B_SPLINE_SURFACE(1,2,((#104283,#104284,#104285,#104286,#104287,#104288,
#104289),(#104290,#104291,#104292,#104293,#104294,#104295,#104296)),
 .UNSPECIFIED.,.F.,.F.,.F.)
B_SPLINE_SURFACE_WITH_KNOTS((2,2),(3,2,2,3),(-0.000384470989622132,0.289807040992866),
(0.348985225264237,0.349369696259357,0.357142857142857,0.367204964620462),
 .UNSPECIFIED.)
GEOMETRIC_REPRESENTATION_ITEM()
RATIONAL_B_SPLINE_SURFACE(((0.995136940902288,0.995136940902288,0.995136940902288,
0.997271548787857,1.,0.996468107407598,0.993931286735391),(0.995136940902287,
0.995136940902288,0.995136940902288,0.997271548787857,1.,0.996468107407597,
0.993931286735391)))
REPRESENTATION_ITEM('')
SURFACE()
);
#664=(
BOUNDED_SURFACE()
B_SPLINE_SURFACE(1,2,((#104319,#104320,#104321),(#104322,#104323,#104324)),
 .UNSPECIFIED.,.F.,.F.,.F.)
B_SPLINE_SURFACE_WITH_KNOTS((2,2),(3,3),(0.,0.289681084359924),(0.366717817351071,
0.383933227114987),.UNSPECIFIED.)
GEOMETRIC_REPRESENTATION_ITEM()
RATIONAL_B_SPLINE_SURFACE(((0.994179254576313,0.989756546152321,0.988246641953811),
(0.994179254576313,0.989756546152321,0.988246641953811)))
REPRESENTATION_ITEM('')
SURFACE()
);
#665=(
BOUNDED_SURFACE()
B_SPLINE_SURFACE(1,2,((#104326,#104327,#104328,#104329,#104330,#104331,
#104332),(#104333,#104334,#104335,#104336,#104337,#104338,#104339)),
 .UNSPECIFIED.,.F.,.F.,.F.)
B_SPLINE_SURFACE_WITH_KNOTS((2,2),(3,2,2,3),(-0.000384470951243084,0.289807040992824),
(0.348985225310178,0.349369696259357,0.357142857142857,0.367204964579277),
 .UNSPECIFIED.)
GEOMETRIC_REPRESENTATION_ITEM()
RATIONAL_B_SPLINE_SURFACE(((0.995136940902288,0.995136940902288,0.995136940902288,
0.997271548787857,1.,0.996468107422053,0.993931286756156),(0.995136940902288,
0.995136940902288,0.995136940902288,0.997271548787857,1.,0.996468107422054,
0.993931286756156)))
REPRESENTATION_ITEM('')
SURFACE()
);
#666=(
BOUNDED_SURFACE()
B_SPLINE_SURFACE(1,2,((#104362,#104363,#104364),(#104365,#104366,#104367)),
 .UNSPECIFIED.,.F.,.F.,.F.)
B_SPLINE_SURFACE_WITH_KNOTS((2,2),(3,3),(0.,0.289681084359916),(0.366717817351071,
0.383933227114987),.UNSPECIFIED.)
GEOMETRIC_REPRESENTATION_ITEM()
RATIONAL_B_SPLINE_SURFACE(((0.994179254576314,0.989756546152321,0.988246641953811),
(0.994179254576314,0.989756546152321,0.988246641953811)))
REPRESENTATION_ITEM('')
SURFACE()
);
#667=(
BOUNDED_SURFACE()
B_SPLINE_SURFACE(1,2,((#104369,#104370,#104371,#104372,#104373,#104374,
#104375),(#104376,#104377,#104378,#104379,#104380,#104381,#104382)),
 .UNSPECIFIED.,.F.,.F.,.F.)
B_SPLINE_SURFACE_WITH_KNOTS((2,2),(3,2,2,3),(-0.000384470777086583,0.289807040992855),
(0.348985225477453,0.349369696259359,0.357142857142857,0.367204964427647),
 .UNSPECIFIED.)
GEOMETRIC_REPRESENTATION_ITEM()
RATIONAL_B_SPLINE_SURFACE(((0.995136940902289,0.995136940902289,0.995136940902289,
0.997271548787858,1.,0.996468107475277,0.993931286832614),(0.995136940902289,
0.995136940902289,0.995136940902289,0.997271548787858,1.,0.996468107475277,
0.993931286832614)))
REPRESENTATION_ITEM('')
SURFACE()
);
#668=(
BOUNDED_SURFACE()
B_SPLINE_SURFACE(1,2,((#104405,#104406,#104407),(#104408,#104409,#104410)),
 .UNSPECIFIED.,.F.,.F.,.F.)
B_SPLINE_SURFACE_WITH_KNOTS((2,2),(3,3),(0.,0.289681084359922),(0.366717817351071,
0.383933227114987),.UNSPECIFIED.)
GEOMETRIC_REPRESENTATION_ITEM()
RATIONAL_B_SPLINE_SURFACE(((0.994179254576313,0.989756546152321,0.988246641953811),
(0.994179254576313,0.989756546152321,0.988246641953811)))
REPRESENTATION_ITEM('')
SURFACE()
);
#669=(
BOUNDED_SURFACE()
B_SPLINE_SURFACE(1,2,((#104412,#104413,#104414,#104415,#104416,#104417,
#104418),(#104419,#104420,#104421,#104422,#104423,#104424,#104425)),
 .UNSPECIFIED.,.F.,.F.,.F.)
B_SPLINE_SURFACE_WITH_KNOTS((2,2),(3,2,2,3),(-0.00038447093632129,0.289807040992328),
(0.348985225303722,0.349369696259343,0.357142857142857,0.367204964575977),
 .UNSPECIFIED.)
GEOMETRIC_REPRESENTATION_ITEM()
RATIONAL_B_SPLINE_SURFACE(((0.99513694090228,0.99513694090228,0.99513694090228,
0.997271548787852,1.,0.996468107423212,0.993931286757821),(0.99513694090228,
0.99513694090228,0.99513694090228,0.997271548787852,1.,0.996468107423212,
0.993931286757821)))
REPRESENTATION_ITEM('')
SURFACE()
);
#670=(
BOUNDED_SURFACE()
B_SPLINE_SURFACE(1,2,((#104448,#104449,#104450),(#104451,#104452,#104453)),
 .UNSPECIFIED.,.F.,.F.,.F.)
B_SPLINE_SURFACE_WITH_KNOTS((2,2),(3,3),(0.,0.28968108435993),(0.366717817351071,
0.383933227114987),.UNSPECIFIED.)
GEOMETRIC_REPRESENTATION_ITEM()
RATIONAL_B_SPLINE_SURFACE(((0.994179254576314,0.989756546152321,0.988246641953811),
(0.994179254576314,0.989756546152321,0.988246641953811)))
REPRESENTATION_ITEM('')
SURFACE()
);
#671=(
BOUNDED_SURFACE()
B_SPLINE_SURFACE(1,2,((#104455,#104456,#104457,#104458,#104459,#104460,
#104461),(#104462,#104463,#104464,#104465,#104466,#104467,#104468)),
 .UNSPECIFIED.,.F.,.F.,.F.)
B_SPLINE_SURFACE_WITH_KNOTS((2,2),(3,2,2,3),(-0.000384470852077006,0.289807040992451),
(0.348985225406444,0.349369696259343,0.357142857142857,0.367204964477797),
 .UNSPECIFIED.)
GEOMETRIC_REPRESENTATION_ITEM()
RATIONAL_B_SPLINE_SURFACE(((0.99513694090228,0.99513694090228,0.99513694090228,
0.997271548787852,1.,0.996468107457674,0.993931286807326),(0.99513694090228,
0.99513694090228,0.99513694090228,0.997271548787852,1.,0.996468107457674,
0.993931286807326)))
REPRESENTATION_ITEM('')
SURFACE()
);
#672=(
BOUNDED_SURFACE()
B_SPLINE_SURFACE(1,2,((#104476,#104477,#104478),(#104479,#104480,#104481)),
 .UNSPECIFIED.,.F.,.F.,.F.)
B_SPLINE_SURFACE_WITH_KNOTS((2,2),(3,3),(0.,0.289681084359928),(0.366717817351071,
0.383933227114987),.UNSPECIFIED.)
GEOMETRIC_REPRESENTATION_ITEM()
RATIONAL_B_SPLINE_SURFACE(((0.994179254576314,0.989756546152321,0.988246641953811),
(0.994179254576314,0.989756546152321,0.988246641953811)))
REPRESENTATION_ITEM('')
SURFACE()
);
#673=(
BOUNDED_SURFACE()
B_SPLINE_SURFACE(1,2,((#104483,#104484,#104485,#104486,#104487,#104488,
#104489),(#104490,#104491,#104492,#104493,#104494,#104495,#104496)),
 .UNSPECIFIED.,.F.,.F.,.F.)
B_SPLINE_SURFACE_WITH_KNOTS((2,2),(3,2,2,3),(-0.000384470769131978,0.289807040992686),
(0.348985225423804,0.349369696259343,0.357142857142857,0.367204964462875),
 .UNSPECIFIED.)
GEOMETRIC_REPRESENTATION_ITEM()
RATIONAL_B_SPLINE_SURFACE(((0.99513694090228,0.99513694090228,0.99513694090228,
0.997271548787852,1.,0.996468107462912,0.993931286814852),(0.99513694090228,
0.99513694090228,0.99513694090228,0.997271548787852,1.,0.996468107462912,
0.993931286814851)))
REPRESENTATION_ITEM('')
SURFACE()
);
#674=(
BOUNDED_SURFACE()
B_SPLINE_SURFACE(1,2,((#104519,#104520,#104521),(#104522,#104523,#104524)),
 .UNSPECIFIED.,.F.,.F.,.F.)
B_SPLINE_SURFACE_WITH_KNOTS((2,2),(3,3),(0.,0.289681084359927),(0.366717817351071,
0.383933227114987),.UNSPECIFIED.)
GEOMETRIC_REPRESENTATION_ITEM()
RATIONAL_B_SPLINE_SURFACE(((0.994179254576313,0.989756546152321,0.988246641953811),
(0.994179254576313,0.989756546152321,0.988246641953811)))
REPRESENTATION_ITEM('')
SURFACE()
);
#675=(
BOUNDED_SURFACE()
B_SPLINE_SURFACE(1,2,((#104526,#104527,#104528,#104529,#104530,#104531,
#104532),(#104533,#104534,#104535,#104536,#104537,#104538,#104539)),
 .UNSPECIFIED.,.F.,.F.,.F.)
B_SPLINE_SURFACE_WITH_KNOTS((2,2),(3,2,2,3),(-0.000384470922438091,0.289807040992906),
(0.348985225331245,0.349369696259343,0.357142857142857,0.367204964547758),
 .UNSPECIFIED.)
GEOMETRIC_REPRESENTATION_ITEM()
RATIONAL_B_SPLINE_SURFACE(((0.995136940902279,0.99513694090228,0.99513694090228,
0.997271548787852,1.,0.996468107433117,0.993931286772051),(0.99513694090228,
0.99513694090228,0.99513694090228,0.997271548787852,1.,0.996468107433117,
0.993931286772051)))
REPRESENTATION_ITEM('')
SURFACE()
);
#676=(
BOUNDED_SURFACE()
B_SPLINE_SURFACE(1,2,((#104562,#104563,#104564),(#104565,#104566,#104567)),
 .UNSPECIFIED.,.F.,.F.,.F.)
B_SPLINE_SURFACE_WITH_KNOTS((2,2),(3,3),(0.,0.28968108435992),(0.366717817350772,
0.383933227114987),.UNSPECIFIED.)
GEOMETRIC_REPRESENTATION_ITEM()
RATIONAL_B_SPLINE_SURFACE(((0.994179254576467,0.989756546152347,0.988246641953811),
(0.994179254576467,0.989756546152347,0.988246641953811)))
REPRESENTATION_ITEM('')
SURFACE()
);
#677=(
BOUNDED_SURFACE()
B_SPLINE_SURFACE(1,2,((#104569,#104570,#104571,#104572,#104573,#104574,
#104575),(#104576,#104577,#104578,#104579,#104580,#104581,#104582)),
 .UNSPECIFIED.,.F.,.F.,.F.)
B_SPLINE_SURFACE_WITH_KNOTS((2,2),(3,2,2,3),(-0.000384470727756695,0.289807040991758),
(0.348985225510703,0.349369696259361,0.357142857142857,0.367204964365651),
 .UNSPECIFIED.)
GEOMETRIC_REPRESENTATION_ITEM()
RATIONAL_B_SPLINE_SURFACE(((0.99513694090229,0.99513694090229,0.99513694090229,
0.997271548787858,1.,0.996468107497038,0.993931286863875),(0.99513694090229,
0.99513694090229,0.99513694090229,0.997271548787858,1.,0.996468107497038,
0.993931286863875)))
REPRESENTATION_ITEM('')
SURFACE()
);
#678=(
BOUNDED_SURFACE()
B_SPLINE_SURFACE(1,2,((#104605,#104606,#104607),(#104608,#104609,#104610)),
 .UNSPECIFIED.,.F.,.F.,.F.)
B_SPLINE_SURFACE_WITH_KNOTS((2,2),(3,3),(0.,0.28968108435992),(0.366717817350851,
0.383933227114987),.UNSPECIFIED.)
GEOMETRIC_REPRESENTATION_ITEM()
RATIONAL_B_SPLINE_SURFACE(((0.994179254576426,0.98975654615234,0.988246641953811),
(0.994179254576426,0.98975654615234,0.988246641953811)))
REPRESENTATION_ITEM('')
SURFACE()
);
#679=(
BOUNDED_SURFACE()
B_SPLINE_SURFACE(1,2,((#104612,#104613,#104614,#104615,#104616,#104617,
#104618),(#104619,#104620,#104621,#104622,#104623,#104624,#104625)),
 .UNSPECIFIED.,.F.,.F.,.F.)
B_SPLINE_SURFACE_WITH_KNOTS((2,2),(3,2,2,3),(-0.000384470761284522,0.289807040991714),
(0.348985225499164,0.349369696259361,0.357142857142857,0.36720496441584),
 .UNSPECIFIED.)
GEOMETRIC_REPRESENTATION_ITEM()
RATIONAL_B_SPLINE_SURFACE(((0.99513694090229,0.99513694090229,0.99513694090229,
0.997271548787858,1.,0.996468107479421,0.993931286838568),(0.99513694090229,
0.99513694090229,0.99513694090229,0.997271548787858,1.,0.996468107479422,
0.993931286838568)))
REPRESENTATION_ITEM('')
SURFACE()
);
#680=(
BOUNDED_SURFACE()
B_SPLINE_SURFACE(1,2,((#104648,#104649,#104650),(#104651,#104652,#104653)),
 .UNSPECIFIED.,.F.,.F.,.F.)
B_SPLINE_SURFACE_WITH_KNOTS((2,2),(3,3),(0.,0.289681084359927),(0.366717817351071,
0.383933227114987),.UNSPECIFIED.)
GEOMETRIC_REPRESENTATION_ITEM()
RATIONAL_B_SPLINE_SURFACE(((0.994179254576314,0.989756546152321,0.988246641953811),
(0.994179254576314,0.989756546152321,0.988246641953811)))
REPRESENTATION_ITEM('')
SURFACE()
);
#681=(
BOUNDED_SURFACE()
B_SPLINE_SURFACE(1,2,((#104655,#104656,#104657,#104658,#104659,#104660,
#104661),(#104662,#104663,#104664,#104665,#104666,#104667,#104668)),
 .UNSPECIFIED.,.F.,.F.,.F.)
B_SPLINE_SURFACE_WITH_KNOTS((2,2),(3,2,2,3),(-0.000384471191006712,0.289807040991564),
(0.348985225048002,0.349369696259361,0.357142857142857,0.367204964836913),
 .UNSPECIFIED.)
GEOMETRIC_REPRESENTATION_ITEM()
RATIONAL_B_SPLINE_SURFACE(((0.99513694090229,0.99513694090229,0.99513694090229,
0.997271548787858,1.,0.996468107331621,0.99393128662625),(0.99513694090229,
0.99513694090229,0.99513694090229,0.997271548787858,1.,0.996468107331621,
0.99393128662625)))
REPRESENTATION_ITEM('')
SURFACE()
);
#682=(
BOUNDED_SURFACE()
B_SPLINE_SURFACE(1,2,((#104691,#104692,#104693),(#104694,#104695,#104696)),
 .UNSPECIFIED.,.F.,.F.,.F.)
B_SPLINE_SURFACE_WITH_KNOTS((2,2),(3,3),(0.,0.289681084359927),(0.366717817351071,
0.383933227114987),.UNSPECIFIED.)
GEOMETRIC_REPRESENTATION_ITEM()
RATIONAL_B_SPLINE_SURFACE(((0.994179254576313,0.989756546152321,0.988246641953811),
(0.994179254576314,0.989756546152321,0.988246641953811)))
REPRESENTATION_ITEM('')
SURFACE()
);
#683=(
BOUNDED_SURFACE()
B_SPLINE_SURFACE(1,2,((#104698,#104699,#104700,#104701,#104702,#104703,
#104704),(#104705,#104706,#104707,#104708,#104709,#104710,#104711)),
 .UNSPECIFIED.,.F.,.F.,.F.)
B_SPLINE_SURFACE_WITH_KNOTS((2,2),(3,2,2,3),(-0.000384470750397015,0.289807040991566),
(0.348985225457864,0.349369696259361,0.357142857142857,0.367204964420445),
 .UNSPECIFIED.)
GEOMETRIC_REPRESENTATION_ITEM()
RATIONAL_B_SPLINE_SURFACE(((0.995136940902291,0.99513694090229,0.99513694090229,
0.997271548787858,1.,0.996468107477805,0.993931286836245),(0.995136940902291,
0.99513694090229,0.99513694090229,0.997271548787858,1.,0.996468107477805,
0.993931286836245)))
REPRESENTATION_ITEM('')
SURFACE()
);
#684=(
BOUNDED_SURFACE()
B_SPLINE_SURFACE(1,2,((#104734,#104735,#104736),(#104737,#104738,#104739)),
 .UNSPECIFIED.,.F.,.F.,.F.)
B_SPLINE_SURFACE_WITH_KNOTS((2,2),(3,3),(0.,0.289681084359929),(0.366717817350786,
0.383933227114987),.UNSPECIFIED.)
GEOMETRIC_REPRESENTATION_ITEM()
RATIONAL_B_SPLINE_SURFACE(((0.99417925457646,0.989756546152346,0.988246641953811),
(0.99417925457646,0.989756546152346,0.988246641953811)))
REPRESENTATION_ITEM('')
SURFACE()
);
#685=(
BOUNDED_SURFACE()
B_SPLINE_SURFACE(1,2,((#104741,#104742,#104743,#104744,#104745,#104746,
#104747),(#104748,#104749,#104750,#104751,#104752,#104753,#104754)),
 .UNSPECIFIED.,.F.,.F.,.F.)
B_SPLINE_SURFACE_WITH_KNOTS((2,2),(3,2,2,3),(-0.000384470913180565,0.289807040991567),
(0.3489852253338,0.349369696259361,0.357142857142857,0.367204964552289),
 .UNSPECIFIED.)
GEOMETRIC_REPRESENTATION_ITEM()
RATIONAL_B_SPLINE_SURFACE(((0.99513694090229,0.99513694090229,0.99513694090229,
0.997271548787858,1.,0.996468107431527,0.993931286769765),(0.99513694090229,
0.99513694090229,0.99513694090229,0.997271548787858,1.,0.996468107431527,
0.993931286769765)))
REPRESENTATION_ITEM('')
SURFACE()
);
#686=(
BOUNDED_SURFACE()
B_SPLINE_SURFACE(1,2,((#104777,#104778,#104779),(#104780,#104781,#104782)),
 .UNSPECIFIED.,.F.,.F.,.F.)
B_SPLINE_SURFACE_WITH_KNOTS((2,2),(3,3),(0.,0.289681084359931),(0.366717817351071,
0.383933227114987),.UNSPECIFIED.)
GEOMETRIC_REPRESENTATION_ITEM()
RATIONAL_B_SPLINE_SURFACE(((0.994179254576313,0.989756546152321,0.988246641953811),
(0.994179254576313,0.989756546152321,0.988246641953811)))
REPRESENTATION_ITEM('')
SURFACE()
);
#687=(
BOUNDED_SURFACE()
B_SPLINE_SURFACE(1,2,((#104784,#104785,#104786,#104787,#104788,#104789,
#104790),(#104791,#104792,#104793,#104794,#104795,#104796,#104797)),
 .UNSPECIFIED.,.F.,.F.,.F.)
B_SPLINE_SURFACE_WITH_KNOTS((2,2),(3,2,2,3),(-0.000384470870558051,0.289807040991559),
(0.348985225349386,0.349369696259361,0.357142857142857,0.367204964535364),
 .UNSPECIFIED.)
GEOMETRIC_REPRESENTATION_ITEM()
RATIONAL_B_SPLINE_SURFACE(((0.99513694090229,0.99513694090229,0.99513694090229,
0.997271548787858,1.,0.996468107437468,0.993931286778301),(0.99513694090229,
0.99513694090229,0.99513694090229,0.997271548787858,1.,0.996468107437468,
0.9939312867783)))
REPRESENTATION_ITEM('')
SURFACE()
);
#688=(
BOUNDED_SURFACE()
B_SPLINE_SURFACE(1,2,((#104820,#104821,#104822),(#104823,#104824,#104825)),
 .UNSPECIFIED.,.F.,.F.,.F.)
B_SPLINE_SURFACE_WITH_KNOTS((2,2),(3,3),(0.,0.28968108435992),(0.366717817351071,
0.383933227114987),.UNSPECIFIED.)
GEOMETRIC_REPRESENTATION_ITEM()
RATIONAL_B_SPLINE_SURFACE(((0.994179254576314,0.989756546152321,0.988246641953811),
(0.994179254576314,0.989756546152321,0.988246641953811)))
REPRESENTATION_ITEM('')
SURFACE()
);
#689=(
BOUNDED_SURFACE()
B_SPLINE_SURFACE(1,2,((#104827,#104828,#104829,#104830,#104831,#104832,
#104833),(#104834,#104835,#104836,#104837,#104838,#104839,#104840)),
 .UNSPECIFIED.,.F.,.F.,.F.)
B_SPLINE_SURFACE_WITH_KNOTS((2,2),(3,2,2,3),(-0.000384470880878568,0.289807040991565),
(0.348985225371886,0.349369696259361,0.357142857142857,0.367204964508579),
 .UNSPECIFIED.)
GEOMETRIC_REPRESENTATION_ITEM()
RATIONAL_B_SPLINE_SURFACE(((0.995136940902291,0.99513694090229,0.99513694090229,
0.997271548787858,1.,0.996468107446869,0.993931286791805),(0.995136940902291,
0.99513694090229,0.99513694090229,0.997271548787858,1.,0.996468107446869,
0.993931286791805)))
REPRESENTATION_ITEM('')
SURFACE()
);
#690=(
BOUNDED_SURFACE()
B_SPLINE_SURFACE(1,2,((#104863,#104864,#104865),(#104866,#104867,#104868)),
 .UNSPECIFIED.,.F.,.F.,.F.)
B_SPLINE_SURFACE_WITH_KNOTS((2,2),(3,3),(0.,0.289681084359924),(0.366717817351071,
0.383933227114987),.UNSPECIFIED.)
GEOMETRIC_REPRESENTATION_ITEM()
RATIONAL_B_SPLINE_SURFACE(((0.994179254576313,0.989756546152321,0.988246641953811),
(0.994179254576313,0.989756546152321,0.988246641953811)))
REPRESENTATION_ITEM('')
SURFACE()
);
#691=(
BOUNDED_SURFACE()
B_SPLINE_SURFACE(1,2,((#104870,#104871,#104872,#104873,#104874,#104875,
#104876),(#104877,#104878,#104879,#104880,#104881,#104882,#104883)),
 .UNSPECIFIED.,.F.,.F.,.F.)
B_SPLINE_SURFACE_WITH_KNOTS((2,2),(3,2,2,3),(-0.000384470963773044,0.289807040991667),
(0.348985225287661,0.349369696259361,0.357142857142857,0.367204964598757),
 .UNSPECIFIED.)
GEOMETRIC_REPRESENTATION_ITEM()
RATIONAL_B_SPLINE_SURFACE(((0.99513694090229,0.99513694090229,0.99513694090229,
0.997271548787858,1.,0.996468107415216,0.993931286746336),(0.99513694090229,
0.99513694090229,0.99513694090229,0.997271548787858,1.,0.996468107415216,
0.993931286746336)))
REPRESENTATION_ITEM('')
SURFACE()
);
#692=(
BOUNDED_SURFACE()
B_SPLINE_SURFACE(1,2,((#104906,#104907,#104908),(#104909,#104910,#104911)),
 .UNSPECIFIED.,.F.,.F.,.F.)
B_SPLINE_SURFACE_WITH_KNOTS((2,2),(3,3),(0.,0.289681084359924),(0.366717817351071,
0.383933227114987),.UNSPECIFIED.)
GEOMETRIC_REPRESENTATION_ITEM()
RATIONAL_B_SPLINE_SURFACE(((0.994179254576313,0.989756546152321,0.988246641953811),
(0.994179254576313,0.989756546152321,0.988246641953811)))
REPRESENTATION_ITEM('')
SURFACE()
);
#693=(
BOUNDED_SURFACE()
B_SPLINE_SURFACE(1,2,((#104913,#104914,#104915,#104916,#104917,#104918,
#104919),(#104920,#104921,#104922,#104923,#104924,#104925,#104926)),
 .UNSPECIFIED.,.F.,.F.,.F.)
B_SPLINE_SURFACE_WITH_KNOTS((2,2),(3,2,2,3),(-0.000384470506086084,0.289807040992968),
(0.348985225660948,0.349369696259361,0.357142857142857,0.367204964215901),
 .UNSPECIFIED.)
GEOMETRIC_REPRESENTATION_ITEM()
RATIONAL_B_SPLINE_SURFACE(((0.995136940902291,0.99513694090229,0.99513694090229,
0.997271548787858,1.,0.996468107549602,0.993931286939384),(0.995136940902291,
0.99513694090229,0.99513694090229,0.997271548787858,1.,0.996468107549602,
0.993931286939384)))
REPRESENTATION_ITEM('')
SURFACE()
);
#694=(
BOUNDED_SURFACE()
B_SPLINE_SURFACE(1,2,((#104949,#104950,#104951),(#104952,#104953,#104954)),
 .UNSPECIFIED.,.F.,.F.,.F.)
B_SPLINE_SURFACE_WITH_KNOTS((2,2),(3,3),(0.,0.289681084359921),(0.366717817350842,
0.383933227114987),.UNSPECIFIED.)
GEOMETRIC_REPRESENTATION_ITEM()
RATIONAL_B_SPLINE_SURFACE(((0.994179254576431,0.989756546152341,0.988246641953811),
(0.994179254576431,0.989756546152341,0.988246641953811)))
REPRESENTATION_ITEM('')
SURFACE()
);
#695=(
BOUNDED_SURFACE()
B_SPLINE_SURFACE(1,2,((#104956,#104957,#104958,#104959,#104960,#104961,
#104962),(#104963,#104964,#104965,#104966,#104967,#104968,#104969)),
 .UNSPECIFIED.,.F.,.F.,.F.)
B_SPLINE_SURFACE_WITH_KNOTS((2,2),(3,2,2,3),(-0.000384470883047098,0.289807040991813),
(0.34898522534491,0.349369696259361,0.357142857142857,0.367204964524695),
 .UNSPECIFIED.)
GEOMETRIC_REPRESENTATION_ITEM()
RATIONAL_B_SPLINE_SURFACE(((0.99513694090229,0.99513694090229,0.99513694090229,
0.997271548787858,1.,0.996468107441213,0.99393128678368),(0.99513694090229,
0.99513694090229,0.99513694090229,0.997271548787858,1.,0.996468107441213,
0.99393128678368)))
REPRESENTATION_ITEM('')
SURFACE()
);
#696=(
BOUNDED_SURFACE()
B_SPLINE_SURFACE(1,2,((#104992,#104993,#104994),(#104995,#104996,#104997)),
 .UNSPECIFIED.,.F.,.F.,.F.)
B_SPLINE_SURFACE_WITH_KNOTS((2,2),(3,3),(0.,0.289681084359923),(0.366717817351071,
0.383933227114987),.UNSPECIFIED.)
GEOMETRIC_REPRESENTATION_ITEM()
RATIONAL_B_SPLINE_SURFACE(((0.994179254576314,0.989756546152321,0.988246641953811),
(0.994179254576314,0.989756546152321,0.988246641953811)))
REPRESENTATION_ITEM('')
SURFACE()
);
#697=(
BOUNDED_SURFACE()
B_SPLINE_SURFACE(1,2,((#104999,#105000,#105001,#105002,#105003,#105004,
#105005),(#105006,#105007,#105008,#105009,#105010,#105011,#105012)),
 .UNSPECIFIED.,.F.,.F.,.F.)
B_SPLINE_SURFACE_WITH_KNOTS((2,2),(3,2,2,3),(-0.000384470884855509,0.289807040991563),
(0.348985225362649,0.349369696259361,0.357142857142857,0.367204964528156),
 .UNSPECIFIED.)
GEOMETRIC_REPRESENTATION_ITEM()
RATIONAL_B_SPLINE_SURFACE(((0.995136940902291,0.995136940902291,0.99513694090229,
0.997271548787858,1.,0.996468107439998,0.993931286781934),(0.995136940902291,
0.99513694090229,0.99513694090229,0.997271548787858,1.,0.996468107439998,
0.993931286781934)))
REPRESENTATION_ITEM('')
SURFACE()
);
#698=(
BOUNDED_SURFACE()
B_SPLINE_SURFACE(1,2,((#105035,#105036,#105037),(#105038,#105039,#105040)),
 .UNSPECIFIED.,.F.,.F.,.F.)
B_SPLINE_SURFACE_WITH_KNOTS((2,2),(3,3),(0.,0.289681084359921),(0.366717817351071,
0.383933227114987),.UNSPECIFIED.)
GEOMETRIC_REPRESENTATION_ITEM()
RATIONAL_B_SPLINE_SURFACE(((0.994179254576313,0.989756546152321,0.988246641953811),
(0.994179254576313,0.989756546152321,0.988246641953811)))
REPRESENTATION_ITEM('')
SURFACE()
);
#699=(
BOUNDED_SURFACE()
B_SPLINE_SURFACE(1,2,((#105042,#105043,#105044,#105045,#105046,#105047,
#105048),(#105049,#105050,#105051,#105052,#105053,#105054,#105055)),
 .UNSPECIFIED.,.F.,.F.,.F.)
B_SPLINE_SURFACE_WITH_KNOTS((2,2),(3,2,2,3),(-0.000384470797821128,0.289807040991558),
(0.348985225443547,0.349369696259361,0.357142857142857,0.367204964439945),
 .UNSPECIFIED.)
GEOMETRIC_REPRESENTATION_ITEM()
RATIONAL_B_SPLINE_SURFACE(((0.995136940902289,0.99513694090229,0.99513694090229,
0.997271548787858,1.,0.996468107470961,0.993931286826414),(0.99513694090229,
0.99513694090229,0.99513694090229,0.997271548787858,1.,0.996468107470961,
0.993931286826414)))
REPRESENTATION_ITEM('')
SURFACE()
);
#700=(
BOUNDED_SURFACE()
B_SPLINE_SURFACE(1,2,((#105078,#105079,#105080),(#105081,#105082,#105083)),
 .UNSPECIFIED.,.F.,.F.,.F.)
B_SPLINE_SURFACE_WITH_KNOTS((2,2),(3,3),(0.,0.289681084359919),(0.366717817351071,
0.383933227114987),.UNSPECIFIED.)
GEOMETRIC_REPRESENTATION_ITEM()
RATIONAL_B_SPLINE_SURFACE(((0.994179254576314,0.989756546152321,0.988246641953811),
(0.994179254576314,0.989756546152321,0.988246641953811)))
REPRESENTATION_ITEM('')
SURFACE()
);
#701=(
BOUNDED_SURFACE()
B_SPLINE_SURFACE(1,2,((#105085,#105086,#105087,#105088,#105089,#105090,
#105091),(#105092,#105093,#105094,#105095,#105096,#105097,#105098)),
 .UNSPECIFIED.,.F.,.F.,.F.)
B_SPLINE_SURFACE_WITH_KNOTS((2,2),(3,2,2,3),(-0.000384470745199549,0.28980704099156),
(0.348985225479933,0.349369696259361,0.357142857142857,0.367204964406885),
 .UNSPECIFIED.)
GEOMETRIC_REPRESENTATION_ITEM()
RATIONAL_B_SPLINE_SURFACE(((0.995136940902291,0.99513694090229,0.99513694090229,
0.997271548787858,1.,0.996468107482565,0.993931286843084),(0.995136940902291,
0.99513694090229,0.99513694090229,0.997271548787858,1.,0.996468107482565,
0.993931286843084)))
REPRESENTATION_ITEM('')
SURFACE()
);
#702=(
BOUNDED_SURFACE()
B_SPLINE_SURFACE(1,2,((#105121,#105122,#105123),(#105124,#105125,#105126)),
 .UNSPECIFIED.,.F.,.F.,.F.)
B_SPLINE_SURFACE_WITH_KNOTS((2,2),(3,3),(0.,0.289681084359919),(0.366717817351071,
0.383933227114987),.UNSPECIFIED.)
GEOMETRIC_REPRESENTATION_ITEM()
RATIONAL_B_SPLINE_SURFACE(((0.994179254576313,0.989756546152321,0.988246641953811),
(0.994179254576313,0.989756546152321,0.988246641953811)))
REPRESENTATION_ITEM('')
SURFACE()
);
#703=(
BOUNDED_SURFACE()
B_SPLINE_SURFACE(1,2,((#105128,#105129,#105130,#105131,#105132,#105133,
#105134),(#105135,#105136,#105137,#105138,#105139,#105140,#105141)),
 .UNSPECIFIED.,.F.,.F.,.F.)
B_SPLINE_SURFACE_WITH_KNOTS((2,2),(3,2,2,3),(-0.000384470876979244,0.289807040991562),
(0.348985225392862,0.349369696259361,0.357142857142857,0.36720496451606),
 .UNSPECIFIED.)
GEOMETRIC_REPRESENTATION_ITEM()
RATIONAL_B_SPLINE_SURFACE(((0.99513694090229,0.99513694090229,0.99513694090229,
0.997271548787858,1.,0.996468107444244,0.993931286788034),(0.99513694090229,
0.99513694090229,0.99513694090229,0.997271548787858,1.,0.996468107444244,
0.993931286788034)))
REPRESENTATION_ITEM('')
SURFACE()
);
#704=(
BOUNDED_SURFACE()
B_SPLINE_SURFACE(1,2,((#105164,#105165,#105166),(#105167,#105168,#105169)),
 .UNSPECIFIED.,.F.,.F.,.F.)
B_SPLINE_SURFACE_WITH_KNOTS((2,2),(3,3),(0.,0.289681084359922),(0.366717817351071,
0.383933227114987),.UNSPECIFIED.)
GEOMETRIC_REPRESENTATION_ITEM()
RATIONAL_B_SPLINE_SURFACE(((0.994179254576314,0.989756546152321,0.988246641953811),
(0.994179254576314,0.989756546152321,0.988246641953811)))
REPRESENTATION_ITEM('')
SURFACE()
);
#705=(
BOUNDED_SURFACE()
B_SPLINE_SURFACE(1,2,((#105171,#105172,#105173,#105174,#105175,#105176,
#105177),(#105178,#105179,#105180,#105181,#105182,#105183,#105184)),
 .UNSPECIFIED.,.F.,.F.,.F.)
B_SPLINE_SURFACE_WITH_KNOTS((2,2),(3,2,2,3),(-0.000384470896032662,0.289807040991558),
(0.348985225362887,0.349369696259361,0.357142857142857,0.367204964522724),
 .UNSPECIFIED.)
GEOMETRIC_REPRESENTATION_ITEM()
RATIONAL_B_SPLINE_SURFACE(((0.99513694090229,0.99513694090229,0.99513694090229,
0.997271548787858,1.,0.996468107441904,0.993931286784672),(0.99513694090229,
0.99513694090229,0.99513694090229,0.997271548787858,1.,0.996468107441904,
0.993931286784672)))
REPRESENTATION_ITEM('')
SURFACE()
);
#706=(
BOUNDED_SURFACE()
B_SPLINE_SURFACE(1,2,((#105201,#105202,#105203),(#105204,#105205,#105206)),
 .UNSPECIFIED.,.F.,.F.,.F.)
B_SPLINE_SURFACE_WITH_KNOTS((2,2),(3,3),(0.,0.289681084359918),(0.366717817351071,
0.383933227114987),.UNSPECIFIED.)
GEOMETRIC_REPRESENTATION_ITEM()
RATIONAL_B_SPLINE_SURFACE(((0.994179254576314,0.989756546152321,0.988246641953811),
(0.994179254576314,0.989756546152321,0.988246641953811)))
REPRESENTATION_ITEM('')
SURFACE()
);
#707=(
BOUNDED_SURFACE()
B_SPLINE_SURFACE(1,2,((#105214,#105215,#105216,#105217,#105218,#105219,
#105220),(#105221,#105222,#105223,#105224,#105225,#105226,#105227)),
 .UNSPECIFIED.,.F.,.F.,.F.)
B_SPLINE_SURFACE_WITH_KNOTS((2,2),(3,2,2,3),(-0.000384470919179307,0.28980704099156),
(0.348985225341793,0.349369696259357,0.357142857142857,0.367204964567339),
 .UNSPECIFIED.)
GEOMETRIC_REPRESENTATION_ITEM()
RATIONAL_B_SPLINE_SURFACE(((0.995136940902287,0.995136940902287,0.995136940902287,
0.997271548787857,1.,0.996468107426244,0.993931286762177),(0.995136940902288,
0.995136940902288,0.995136940902288,0.997271548787857,1.,0.996468107426244,
0.993931286762177)))
REPRESENTATION_ITEM('')
SURFACE()
);
#708=(
BOUNDED_SURFACE()
B_SPLINE_SURFACE(1,2,((#105250,#105251,#105252),(#105253,#105254,#105255)),
 .UNSPECIFIED.,.F.,.F.,.F.)
B_SPLINE_SURFACE_WITH_KNOTS((2,2),(3,3),(0.,0.289681084359925),(0.366717817350596,
0.383933227114986),.UNSPECIFIED.)
GEOMETRIC_REPRESENTATION_ITEM()
RATIONAL_B_SPLINE_SURFACE(((0.994179254576558,0.989756546152363,0.988246641953811),
(0.994179254576558,0.989756546152363,0.988246641953811)))
REPRESENTATION_ITEM('')
SURFACE()
);
#709=(
BOUNDED_SURFACE()
B_SPLINE_SURFACE(1,2,((#105257,#105258,#105259,#105260,#105261,#105262,
#105263),(#105264,#105265,#105266,#105267,#105268,#105269,#105270)),
 .UNSPECIFIED.,.F.,.F.,.F.)
B_SPLINE_SURFACE_WITH_KNOTS((2,2),(3,2,2,3),(-0.000384470951268838,0.289807040991836),
(0.348985225303333,0.349369696259362,0.357142857142857,0.367204964581818),
 .UNSPECIFIED.)
GEOMETRIC_REPRESENTATION_ITEM()
RATIONAL_B_SPLINE_SURFACE(((0.995136940902291,0.99513694090229,0.99513694090229,
0.997271548787859,1.,0.996468107421162,0.993931286754876),(0.995136940902291,
0.99513694090229,0.99513694090229,0.997271548787859,1.,0.996468107421162,
0.993931286754876)))
REPRESENTATION_ITEM('')
SURFACE()
);
#710=(
BOUNDED_SURFACE()
B_SPLINE_SURFACE(1,2,((#105293,#105294,#105295),(#105296,#105297,#105298)),
 .UNSPECIFIED.,.F.,.F.,.F.)
B_SPLINE_SURFACE_WITH_KNOTS((2,2),(3,3),(0.,0.289681084359919),(0.366717817351007,
0.383933227114987),.UNSPECIFIED.)
GEOMETRIC_REPRESENTATION_ITEM()
RATIONAL_B_SPLINE_SURFACE(((0.994179254576346,0.989756546152326,0.988246641953811),
(0.994179254576346,0.989756546152326,0.988246641953811)))
REPRESENTATION_ITEM('')
SURFACE()
);
#711=(
BOUNDED_SURFACE()
B_SPLINE_SURFACE(1,2,((#105300,#105301,#105302,#105303,#105304,#105305,
#105306),(#105307,#105308,#105309,#105310,#105311,#105312,#105313)),
 .UNSPECIFIED.,.F.,.F.,.F.)
B_SPLINE_SURFACE_WITH_KNOTS((2,2),(3,2,2,3),(-0.000384470793921457,0.289807040992022),
(0.348985225456814,0.349369696259361,0.357142857142857,0.367204964438393),
 .UNSPECIFIED.)
GEOMETRIC_REPRESENTATION_ITEM()
RATIONAL_B_SPLINE_SURFACE(((0.99513694090229,0.99513694090229,0.99513694090229,
0.997271548787858,1.,0.996468107471505,0.993931286827196),(0.99513694090229,
0.99513694090229,0.99513694090229,0.997271548787858,1.,0.996468107471505,
0.993931286827196)))
REPRESENTATION_ITEM('')
SURFACE()
);
#712=(
BOUNDED_SURFACE()
B_SPLINE_SURFACE(1,2,((#105336,#105337,#105338),(#105339,#105340,#105341)),
 .UNSPECIFIED.,.F.,.F.,.F.)
B_SPLINE_SURFACE_WITH_KNOTS((2,2),(3,3),(0.,0.289681084359933),(0.366717817351071,
0.383933227114987),.UNSPECIFIED.)
GEOMETRIC_REPRESENTATION_ITEM()
RATIONAL_B_SPLINE_SURFACE(((0.994179254576314,0.989756546152321,0.988246641953811),
(0.994179254576314,0.989756546152321,0.988246641953811)))
REPRESENTATION_ITEM('')
SURFACE()
);
#713=(
BOUNDED_SURFACE()
B_SPLINE_SURFACE(1,2,((#105343,#105344,#105345,#105346,#105347,#105348,
#105349),(#105350,#105351,#105352,#105353,#105354,#105355,#105356)),
 .UNSPECIFIED.,.F.,.F.,.F.)
B_SPLINE_SURFACE_WITH_KNOTS((2,2),(3,2,2,3),(-0.000384470853099693,0.289807040991983),
(0.34898522538828,0.349369696259361,0.357142857142857,0.367204964474479),
 .UNSPECIFIED.)
GEOMETRIC_REPRESENTATION_ITEM()
RATIONAL_B_SPLINE_SURFACE(((0.995136940902289,0.99513694090229,0.99513694090229,
0.997271548787858,1.,0.996468107458839,0.993931286808999),(0.995136940902289,
0.99513694090229,0.99513694090229,0.997271548787858,1.,0.996468107458839,
0.993931286808999)))
REPRESENTATION_ITEM('')
SURFACE()
);
#714=(
BOUNDED_SURFACE()
B_SPLINE_SURFACE(1,2,((#105379,#105380,#105381),(#105382,#105383,#105384)),
 .UNSPECIFIED.,.F.,.F.,.F.)
B_SPLINE_SURFACE_WITH_KNOTS((2,2),(3,3),(0.,0.289681084359926),(0.366717817351071,
0.383933227114987),.UNSPECIFIED.)
GEOMETRIC_REPRESENTATION_ITEM()
RATIONAL_B_SPLINE_SURFACE(((0.994179254576314,0.989756546152321,0.988246641953811),
(0.994179254576314,0.989756546152321,0.988246641953811)))
REPRESENTATION_ITEM('')
SURFACE()
);
#715=(
BOUNDED_SURFACE()
B_SPLINE_SURFACE(1,2,((#105398,#105399,#105400,#105401,#105402,#105403,
#105404),(#105405,#105406,#105407,#105408,#105409,#105410,#105411)),
 .UNSPECIFIED.,.F.,.F.,.F.)
B_SPLINE_SURFACE_WITH_KNOTS((2,2),(3,2,2,3),(-0.000384472577672092,0.289807040991895),
(0.348985223670602,0.349369696259361,0.357142857142857,0.367204966456659),
 .UNSPECIFIED.)
GEOMETRIC_REPRESENTATION_ITEM()
RATIONAL_B_SPLINE_SURFACE(((0.995136940902289,0.99513694090229,0.99513694090229,
0.997271548787858,1.,0.996468106763076,0.99393128580952),(0.99513694090229,
0.99513694090229,0.99513694090229,0.997271548787858,1.,0.996468106763076,
0.993931285809521)))
REPRESENTATION_ITEM('')
SURFACE()
);
#716=(
BOUNDED_SURFACE()
B_SPLINE_SURFACE(1,2,((#105413,#105414,#105415,#105416,#105417),(#105418,
#105419,#105420,#105421,#105422)),.UNSPECIFIED.,.F.,.F.,.F.)
B_SPLINE_SURFACE_WITH_KNOTS((2,2),(3,2,3),(0.710192959007142,1.),(0.297684616398914,
0.297856505190553,0.315045384354504),.UNSPECIFIED.)
GEOMETRIC_REPRESENTATION_ITEM()
RATIONAL_B_SPLINE_SURFACE(((0.99292495227316,0.99292495227316,0.99292495227316,
0.988942764095695,0.98786440923939),(0.99292495227316,0.99292495227316,
0.99292495227316,0.988942764095695,0.98786440923939)))
REPRESENTATION_ITEM('')
SURFACE()
);
#717=(
BOUNDED_SURFACE()
B_SPLINE_SURFACE(1,2,((#105433,#105434,#105435,#105436,#105437,#105438,
#105439),(#105440,#105441,#105442,#105443,#105444,#105445,#105446)),
 .UNSPECIFIED.,.F.,.F.,.F.)
B_SPLINE_SURFACE_WITH_KNOTS((2,2),(3,2,2,3),(0.710318915639639,1.),(0.418207303127979,
0.428571428571429,0.435775021682622,0.435950698868169),.UNSPECIFIED.)
GEOMETRIC_REPRESENTATION_ITEM()
RATIONAL_B_SPLINE_SURFACE(((0.993779895952495,0.996362096314125,1.,0.997471472332736,
0.995452950231063,0.995452950231063,0.995452950231063),(0.993779895952495,
0.996362096314125,1.,0.997471472332736,0.995452950231063,0.995452950231063,
0.995452950231063)))
REPRESENTATION_ITEM('')
SURFACE()
);
#718=(
BOUNDED_SURFACE()
B_SPLINE_SURFACE(1,2,((#105463,#105464,#105465,#105466,#105467),(#105468,
#105469,#105470,#105471,#105472)),.UNSPECIFIED.,.F.,.F.,.F.)
B_SPLINE_SURFACE_WITH_KNOTS((2,2),(3,2,3),(0.710192959007996,1.),(0.297684616398975,
0.297856505190614,0.315045384354503),.UNSPECIFIED.)
GEOMETRIC_REPRESENTATION_ITEM()
RATIONAL_B_SPLINE_SURFACE(((0.992924952273131,0.992924952273131,0.992924952273131,
0.988942764095691,0.98786440923939),(0.992924952273131,0.992924952273131,
0.992924952273131,0.988942764095691,0.98786440923939)))
REPRESENTATION_ITEM('')
SURFACE()
);
#719=(
BOUNDED_SURFACE()
B_SPLINE_SURFACE(1,2,((#105480,#105481,#105482,#105483,#105484,#105485,
#105486),(#105487,#105488,#105489,#105490,#105491,#105492,#105493)),
 .UNSPECIFIED.,.F.,.F.,.F.)
B_SPLINE_SURFACE_WITH_KNOTS((2,2),(3,2,2,3),(0.710318915640079,1.),(0.418207303127978,
0.428571428571429,0.435775021682621,0.435950698868168),.UNSPECIFIED.)
GEOMETRIC_REPRESENTATION_ITEM()
RATIONAL_B_SPLINE_SURFACE(((0.993779895952494,0.996362096314125,1.,0.997471472332737,
0.995452950231064,0.995452950231064,0.995452950231064),(0.993779895952495,
0.996362096314125,1.,0.997471472332737,0.995452950231064,0.995452950231064,
0.995452950231064)))
REPRESENTATION_ITEM('')
SURFACE()
);
#720=(
BOUNDED_SURFACE()
B_SPLINE_SURFACE(1,2,((#105510,#105511,#105512,#105513,#105514),(#105515,
#105516,#105517,#105518,#105519)),.UNSPECIFIED.,.F.,.F.,.F.)
B_SPLINE_SURFACE_WITH_KNOTS((2,2),(3,2,3),(0.710192959008438,1.),(0.297684616398975,
0.297856505190614,0.315045384354504),.UNSPECIFIED.)
GEOMETRIC_REPRESENTATION_ITEM()
RATIONAL_B_SPLINE_SURFACE(((0.992924952273132,0.992924952273132,0.992924952273132,
0.988942764095691,0.98786440923939),(0.992924952273132,0.992924952273132,
0.992924952273132,0.988942764095691,0.98786440923939)))
REPRESENTATION_ITEM('')
SURFACE()
);
#721=(
BOUNDED_SURFACE()
B_SPLINE_SURFACE(1,2,((#105527,#105528,#105529,#105530,#105531,#105532,
#105533),(#105534,#105535,#105536,#105537,#105538,#105539,#105540)),
 .UNSPECIFIED.,.F.,.F.,.F.)
B_SPLINE_SURFACE_WITH_KNOTS((2,2),(3,2,2,3),(0.710318915639646,1.),(0.418207303127977,
0.428571428571429,0.435775021682621,0.435950698868168),.UNSPECIFIED.)
GEOMETRIC_REPRESENTATION_ITEM()
RATIONAL_B_SPLINE_SURFACE(((0.993779895952494,0.996362096314125,1.,0.997471472332737,
0.995452950231064,0.995452950231064,0.995452950231064),(0.993779895952494,
0.996362096314125,1.,0.997471472332737,0.995452950231064,0.995452950231064,
0.995452950231064)))
REPRESENTATION_ITEM('')
SURFACE()
);
#722=(
BOUNDED_SURFACE()
B_SPLINE_SURFACE(1,2,((#105557,#105558,#105559,#105560,#105561),(#105562,
#105563,#105564,#105565,#105566)),.UNSPECIFIED.,.F.,.F.,.F.)
B_SPLINE_SURFACE_WITH_KNOTS((2,2),(3,2,3),(0.71019295900844,1.),(0.297684616398975,
0.297856505190614,0.315045384354504),.UNSPECIFIED.)
GEOMETRIC_REPRESENTATION_ITEM()
RATIONAL_B_SPLINE_SURFACE(((0.992924952273132,0.992924952273132,0.992924952273132,
0.988942764095691,0.98786440923939),(0.992924952273131,0.992924952273131,
0.992924952273131,0.988942764095691,0.98786440923939)))
REPRESENTATION_ITEM('')
SURFACE()
);
#723=(
BOUNDED_SURFACE()
B_SPLINE_SURFACE(1,2,((#105574,#105575,#105576,#105577,#105578,#105579,
#105580),(#105581,#105582,#105583,#105584,#105585,#105586,#105587)),
 .UNSPECIFIED.,.F.,.F.,.F.)
B_SPLINE_SURFACE_WITH_KNOTS((2,2),(3,2,2,3),(0.710318915640077,1.),(0.418207303127978,
0.428571428571429,0.435775021682621,0.435950698868168),.UNSPECIFIED.)
GEOMETRIC_REPRESENTATION_ITEM()
RATIONAL_B_SPLINE_SURFACE(((0.993779895952495,0.996362096314125,1.,0.997471472332737,
0.995452950231063,0.995452950231063,0.995452950231063),(0.993779895952495,
0.996362096314125,1.,0.997471472332737,0.995452950231063,0.995452950231063,
0.995452950231063)))
REPRESENTATION_ITEM('')
SURFACE()
);
#724=(
BOUNDED_SURFACE()
B_SPLINE_SURFACE(1,2,((#105604,#105605,#105606,#105607,#105608),(#105609,
#105610,#105611,#105612,#105613)),.UNSPECIFIED.,.F.,.F.,.F.)
B_SPLINE_SURFACE_WITH_KNOTS((2,2),(3,2,3),(0.710192959008444,1.),(0.297684616398975,
0.297856505190614,0.315045384354504),.UNSPECIFIED.)
GEOMETRIC_REPRESENTATION_ITEM()
RATIONAL_B_SPLINE_SURFACE(((0.992924952273132,0.992924952273132,0.992924952273132,
0.988942764095691,0.98786440923939),(0.992924952273131,0.992924952273131,
0.992924952273131,0.988942764095691,0.98786440923939)))
REPRESENTATION_ITEM('')
SURFACE()
);
#725=(
BOUNDED_SURFACE()
B_SPLINE_SURFACE(1,2,((#105621,#105622,#105623,#105624,#105625,#105626,
#105627),(#105628,#105629,#105630,#105631,#105632,#105633,#105634)),
 .UNSPECIFIED.,.F.,.F.,.F.)
B_SPLINE_SURFACE_WITH_KNOTS((2,2),(3,2,2,3),(0.710318915639999,1.),(0.418207303127979,
0.428571428571429,0.435775021682621,0.435950698868168),.UNSPECIFIED.)
GEOMETRIC_REPRESENTATION_ITEM()
RATIONAL_B_SPLINE_SURFACE(((0.993779895952495,0.996362096314125,1.,0.997471472332737,
0.995452950231064,0.995452950231064,0.995452950231064),(0.993779895952495,
0.996362096314125,1.,0.997471472332737,0.995452950231064,0.995452950231064,
0.995452950231064)))
REPRESENTATION_ITEM('')
SURFACE()
);
#726=(
BOUNDED_SURFACE()
B_SPLINE_SURFACE(1,2,((#105651,#105652,#105653,#105654,#105655),(#105656,
#105657,#105658,#105659,#105660)),.UNSPECIFIED.,.F.,.F.,.F.)
B_SPLINE_SURFACE_WITH_KNOTS((2,2),(3,2,3),(0.710192959008359,1.),(0.297684616398974,
0.297856505190613,0.315045384354503),.UNSPECIFIED.)
GEOMETRIC_REPRESENTATION_ITEM()
RATIONAL_B_SPLINE_SURFACE(((0.992924952273132,0.992924952273132,0.992924952273132,
0.988942764095691,0.98786440923939),(0.992924952273132,0.992924952273132,
0.992924952273132,0.988942764095691,0.98786440923939)))
REPRESENTATION_ITEM('')
SURFACE()
);
#727=(
BOUNDED_SURFACE()
B_SPLINE_SURFACE(1,2,((#105668,#105669,#105670,#105671,#105672,#105673,
#105674),(#105675,#105676,#105677,#105678,#105679,#105680,#105681)),
 .UNSPECIFIED.,.F.,.F.,.F.)
B_SPLINE_SURFACE_WITH_KNOTS((2,2),(3,2,2,3),(0.710318915639655,1.),(0.418207303127979,
0.428571428571429,0.435775021682622,0.435950698868169),.UNSPECIFIED.)
GEOMETRIC_REPRESENTATION_ITEM()
RATIONAL_B_SPLINE_SURFACE(((0.993779895952495,0.996362096314125,1.,0.997471472332736,
0.995452950231063,0.995452950231063,0.995452950231063),(0.993779895952495,
0.996362096314125,1.,0.997471472332736,0.995452950231063,0.995452950231063,
0.995452950231063)))
REPRESENTATION_ITEM('')
SURFACE()
);
#728=(
BOUNDED_SURFACE()
B_SPLINE_SURFACE(1,2,((#105698,#105699,#105700,#105701,#105702),(#105703,
#105704,#105705,#105706,#105707)),.UNSPECIFIED.,.F.,.F.,.F.)
B_SPLINE_SURFACE_WITH_KNOTS((2,2),(3,2,3),(0.710192959008363,1.),(0.297684616398974,
0.297856505190613,0.315045384354503),.UNSPECIFIED.)
GEOMETRIC_REPRESENTATION_ITEM()
RATIONAL_B_SPLINE_SURFACE(((0.992924952273132,0.992924952273132,0.992924952273132,
0.988942764095691,0.98786440923939),(0.992924952273132,0.992924952273132,
0.992924952273132,0.988942764095691,0.98786440923939)))
REPRESENTATION_ITEM('')
SURFACE()
);
#729=(
BOUNDED_SURFACE()
B_SPLINE_SURFACE(1,2,((#105715,#105716,#105717,#105718,#105719,#105720,
#105721),(#105722,#105723,#105724,#105725,#105726,#105727,#105728)),
 .UNSPECIFIED.,.F.,.F.,.F.)
B_SPLINE_SURFACE_WITH_KNOTS((2,2),(3,2,2,3),(0.71031891564,1.),(0.418207303127979,
0.428571428571429,0.435775021682622,0.435950698868169),.UNSPECIFIED.)
GEOMETRIC_REPRESENTATION_ITEM()
RATIONAL_B_SPLINE_SURFACE(((0.993779895952495,0.996362096314125,1.,0.997471472332736,
0.995452950231063,0.995452950231063,0.995452950231063),(0.993779895952495,
0.996362096314125,1.,0.997471472332736,0.995452950231063,0.995452950231063,
0.995452950231063)))
REPRESENTATION_ITEM('')
SURFACE()
);
#730=(
BOUNDED_SURFACE()
B_SPLINE_SURFACE(1,2,((#105745,#105746,#105747,#105748,#105749),(#105750,
#105751,#105752,#105753,#105754)),.UNSPECIFIED.,.F.,.F.,.F.)
B_SPLINE_SURFACE_WITH_KNOTS((2,2),(3,2,3),(0.710192959008359,1.),(0.297684616398974,
0.297856505190613,0.315045384354503),.UNSPECIFIED.)
GEOMETRIC_REPRESENTATION_ITEM()
RATIONAL_B_SPLINE_SURFACE(((0.992924952273132,0.992924952273132,0.992924952273132,
0.988942764095691,0.98786440923939),(0.992924952273132,0.992924952273132,
0.992924952273132,0.988942764095691,0.98786440923939)))
REPRESENTATION_ITEM('')
SURFACE()
);
#731=(
BOUNDED_SURFACE()
B_SPLINE_SURFACE(1,2,((#105762,#105763,#105764,#105765,#105766,#105767,
#105768),(#105769,#105770,#105771,#105772,#105773,#105774,#105775)),
 .UNSPECIFIED.,.F.,.F.,.F.)
B_SPLINE_SURFACE_WITH_KNOTS((2,2),(3,2,2,3),(0.710318915639998,1.),(0.418207303127979,
0.428571428571429,0.435775021682622,0.435950698868169),.UNSPECIFIED.)
GEOMETRIC_REPRESENTATION_ITEM()
RATIONAL_B_SPLINE_SURFACE(((0.993779895952495,0.996362096314125,1.,0.997471472332736,
0.995452950231063,0.995452950231063,0.995452950231063),(0.993779895952495,
0.996362096314125,1.,0.997471472332736,0.995452950231063,0.995452950231063,
0.995452950231063)))
REPRESENTATION_ITEM('')
SURFACE()
);
#732=(
BOUNDED_SURFACE()
B_SPLINE_SURFACE(1,2,((#105792,#105793,#105794,#105795,#105796),(#105797,
#105798,#105799,#105800,#105801)),.UNSPECIFIED.,.F.,.F.,.F.)
B_SPLINE_SURFACE_WITH_KNOTS((2,2),(3,2,3),(0.710192959008358,1.),(0.297684616398974,
0.297856505190613,0.315045384354503),.UNSPECIFIED.)
GEOMETRIC_REPRESENTATION_ITEM()
RATIONAL_B_SPLINE_SURFACE(((0.992924952273132,0.992924952273132,0.992924952273132,
0.988942764095691,0.98786440923939),(0.992924952273132,0.992924952273132,
0.992924952273132,0.988942764095691,0.98786440923939)))
REPRESENTATION_ITEM('')
SURFACE()
);
#733=(
BOUNDED_SURFACE()
B_SPLINE_SURFACE(1,2,((#105809,#105810,#105811,#105812,#105813,#105814,
#105815),(#105816,#105817,#105818,#105819,#105820,#105821,#105822)),
 .UNSPECIFIED.,.F.,.F.,.F.)
B_SPLINE_SURFACE_WITH_KNOTS((2,2),(3,2,2,3),(0.71031891563967,1.),(0.418207303127979,
0.428571428571429,0.435775021682622,0.435950698868169),.UNSPECIFIED.)
GEOMETRIC_REPRESENTATION_ITEM()
RATIONAL_B_SPLINE_SURFACE(((0.993779895952495,0.996362096314125,1.,0.997471472332736,
0.995452950231063,0.995452950231063,0.995452950231063),(0.993779895952495,
0.996362096314125,1.,0.997471472332736,0.995452950231063,0.995452950231063,
0.995452950231063)))
REPRESENTATION_ITEM('')
SURFACE()
);
#734=(
BOUNDED_SURFACE()
B_SPLINE_SURFACE(1,2,((#105839,#105840,#105841,#105842,#105843),(#105844,
#105845,#105846,#105847,#105848)),.UNSPECIFIED.,.F.,.F.,.F.)
B_SPLINE_SURFACE_WITH_KNOTS((2,2),(3,2,3),(0.71019295900844,1.),(0.297684616398974,
0.297856505190613,0.315045384354503),.UNSPECIFIED.)
GEOMETRIC_REPRESENTATION_ITEM()
RATIONAL_B_SPLINE_SURFACE(((0.992924952273132,0.992924952273132,0.992924952273132,
0.988942764095691,0.98786440923939),(0.992924952273132,0.992924952273132,
0.992924952273132,0.988942764095691,0.98786440923939)))
REPRESENTATION_ITEM('')
SURFACE()
);
#735=(
BOUNDED_SURFACE()
B_SPLINE_SURFACE(1,2,((#105856,#105857,#105858,#105859,#105860,#105861,
#105862),(#105863,#105864,#105865,#105866,#105867,#105868,#105869)),
 .UNSPECIFIED.,.F.,.F.,.F.)
B_SPLINE_SURFACE_WITH_KNOTS((2,2),(3,2,2,3),(0.710318915639991,1.),(0.418207303127979,
0.428571428571429,0.435775021682622,0.435950698868169),.UNSPECIFIED.)
GEOMETRIC_REPRESENTATION_ITEM()
RATIONAL_B_SPLINE_SURFACE(((0.993779895952495,0.996362096314125,1.,0.997471472332736,
0.995452950231063,0.995452950231063,0.995452950231063),(0.993779895952495,
0.996362096314125,1.,0.997471472332736,0.995452950231063,0.995452950231063,
0.995452950231063)))
REPRESENTATION_ITEM('')
SURFACE()
);
#736=(
BOUNDED_SURFACE()
B_SPLINE_SURFACE(1,2,((#105886,#105887,#105888,#105889,#105890),(#105891,
#105892,#105893,#105894,#105895)),.UNSPECIFIED.,.F.,.F.,.F.)
B_SPLINE_SURFACE_WITH_KNOTS((2,2),(3,2,3),(0.710192959008349,1.),(0.297684616398974,
0.297856505190613,0.315045384354503),.UNSPECIFIED.)
GEOMETRIC_REPRESENTATION_ITEM()
RATIONAL_B_SPLINE_SURFACE(((0.992924952273132,0.992924952273132,0.992924952273132,
0.988942764095691,0.98786440923939),(0.992924952273132,0.992924952273132,
0.992924952273132,0.988942764095691,0.98786440923939)))
REPRESENTATION_ITEM('')
SURFACE()
);
#737=(
BOUNDED_SURFACE()
B_SPLINE_SURFACE(1,2,((#105903,#105904,#105905,#105906,#105907,#105908,
#105909),(#105910,#105911,#105912,#105913,#105914,#105915,#105916)),
 .UNSPECIFIED.,.F.,.F.,.F.)
B_SPLINE_SURFACE_WITH_KNOTS((2,2),(3,2,2,3),(0.710318915640076,1.),(0.418207303127979,
0.428571428571429,0.435775021682622,0.435950698868169),.UNSPECIFIED.)
GEOMETRIC_REPRESENTATION_ITEM()
RATIONAL_B_SPLINE_SURFACE(((0.993779895952495,0.996362096314125,1.,0.997471472332736,
0.995452950231063,0.995452950231063,0.995452950231063),(0.993779895952495,
0.996362096314125,1.,0.997471472332736,0.995452950231063,0.995452950231063,
0.995452950231063)))
REPRESENTATION_ITEM('')
SURFACE()
);
#738=(
BOUNDED_SURFACE()
B_SPLINE_SURFACE(1,2,((#105933,#105934,#105935,#105936,#105937),(#105938,
#105939,#105940,#105941,#105942)),.UNSPECIFIED.,.F.,.F.,.F.)
B_SPLINE_SURFACE_WITH_KNOTS((2,2),(3,2,3),(0.710192959008437,1.),(0.297684616398974,
0.297856505190613,0.315045384354503),.UNSPECIFIED.)
GEOMETRIC_REPRESENTATION_ITEM()
RATIONAL_B_SPLINE_SURFACE(((0.992924952273132,0.992924952273132,0.992924952273132,
0.988942764095691,0.98786440923939),(0.992924952273132,0.992924952273132,
0.992924952273132,0.988942764095691,0.98786440923939)))
REPRESENTATION_ITEM('')
SURFACE()
);
#739=(
BOUNDED_SURFACE()
B_SPLINE_SURFACE(1,2,((#105950,#105951,#105952,#105953,#105954,#105955,
#105956),(#105957,#105958,#105959,#105960,#105961,#105962,#105963)),
 .UNSPECIFIED.,.F.,.F.,.F.)
B_SPLINE_SURFACE_WITH_KNOTS((2,2),(3,2,2,3),(0.710318915639662,1.),(0.418207303127979,
0.428571428571429,0.435775021682622,0.435950698868169),.UNSPECIFIED.)
GEOMETRIC_REPRESENTATION_ITEM()
RATIONAL_B_SPLINE_SURFACE(((0.993779895952495,0.996362096314125,1.,0.997471472332736,
0.995452950231063,0.995452950231063,0.995452950231063),(0.993779895952495,
0.996362096314125,1.,0.997471472332736,0.995452950231063,0.995452950231063,
0.995452950231063)))
REPRESENTATION_ITEM('')
SURFACE()
);
#740=(
BOUNDED_SURFACE()
B_SPLINE_SURFACE(1,2,((#105980,#105981,#105982,#105983,#105984),(#105985,
#105986,#105987,#105988,#105989)),.UNSPECIFIED.,.F.,.F.,.F.)
B_SPLINE_SURFACE_WITH_KNOTS((2,2),(3,2,3),(0.71019295900808,1.),(0.297684616398974,
0.297856505190613,0.315045384354503),.UNSPECIFIED.)
GEOMETRIC_REPRESENTATION_ITEM()
RATIONAL_B_SPLINE_SURFACE(((0.992924952273132,0.992924952273132,0.992924952273132,
0.988942764095691,0.98786440923939),(0.992924952273132,0.992924952273132,
0.992924952273132,0.988942764095691,0.98786440923939)))
REPRESENTATION_ITEM('')
SURFACE()
);
#741=(
BOUNDED_SURFACE()
B_SPLINE_SURFACE(1,2,((#105997,#105998,#105999,#106000,#106001,#106002,
#106003),(#106004,#106005,#106006,#106007,#106008,#106009,#106010)),
 .UNSPECIFIED.,.F.,.F.,.F.)
B_SPLINE_SURFACE_WITH_KNOTS((2,2),(3,2,2,3),(0.71031891563867,1.),(0.418207303127979,
0.428571428571429,0.435775021682622,0.435950698868169),.UNSPECIFIED.)
GEOMETRIC_REPRESENTATION_ITEM()
RATIONAL_B_SPLINE_SURFACE(((0.993779895952495,0.996362096314125,1.,0.997471472332736,
0.995452950231063,0.995452950231063,0.995452950231063),(0.993779895952495,
0.996362096314125,1.,0.997471472332736,0.995452950231063,0.995452950231063,
0.995452950231063)))
REPRESENTATION_ITEM('')
SURFACE()
);
#742=(
BOUNDED_SURFACE()
B_SPLINE_SURFACE(1,2,((#106027,#106028,#106029,#106030,#106031),(#106032,
#106033,#106034,#106035,#106036)),.UNSPECIFIED.,.F.,.F.,.F.)
B_SPLINE_SURFACE_WITH_KNOTS((2,2),(3,2,3),(0.710192959007034,1.),(0.297684616398974,
0.297856505190613,0.315045384354503),.UNSPECIFIED.)
GEOMETRIC_REPRESENTATION_ITEM()
RATIONAL_B_SPLINE_SURFACE(((0.992924952273132,0.992924952273132,0.992924952273132,
0.988942764095691,0.98786440923939),(0.992924952273132,0.992924952273132,
0.992924952273132,0.988942764095691,0.98786440923939)))
REPRESENTATION_ITEM('')
SURFACE()
);
#743=(
BOUNDED_SURFACE()
B_SPLINE_SURFACE(1,2,((#106044,#106045,#106046,#106047,#106048,#106049,
#106050),(#106051,#106052,#106053,#106054,#106055,#106056,#106057)),
 .UNSPECIFIED.,.F.,.F.,.F.)
B_SPLINE_SURFACE_WITH_KNOTS((2,2),(3,2,2,3),(0.710318915639954,1.),(0.418207303127979,
0.428571428571429,0.435775021682622,0.435950698868169),.UNSPECIFIED.)
GEOMETRIC_REPRESENTATION_ITEM()
RATIONAL_B_SPLINE_SURFACE(((0.993779895952495,0.996362096314125,1.,0.997471472332736,
0.995452950231063,0.995452950231063,0.995452950231063),(0.993779895952495,
0.996362096314125,1.,0.997471472332736,0.995452950231063,0.995452950231063,
0.995452950231063)))
REPRESENTATION_ITEM('')
SURFACE()
);
#744=(
BOUNDED_SURFACE()
B_SPLINE_SURFACE(1,2,((#106065,#106066,#106067,#106068,#106069),(#106070,
#106071,#106072,#106073,#106074)),.UNSPECIFIED.,.F.,.F.,.F.)
B_SPLINE_SURFACE_WITH_KNOTS((2,2),(3,2,3),(0.71019295900831,1.),(0.29768461639882,
0.297856505190461,0.315045384354504),.UNSPECIFIED.)
GEOMETRIC_REPRESENTATION_ITEM()
RATIONAL_B_SPLINE_SURFACE(((0.992924952273203,0.992924952273203,0.992924952273203,
0.988942764095701,0.98786440923939),(0.992924952273203,0.992924952273203,
0.992924952273203,0.988942764095701,0.98786440923939)))
REPRESENTATION_ITEM('')
SURFACE()
);
#745=(
BOUNDED_SURFACE()
B_SPLINE_SURFACE(1,2,((#106076,#106077,#106078,#106079,#106080,#106081,
#106082),(#106083,#106084,#106085,#106086,#106087,#106088,#106089)),
 .UNSPECIFIED.,.F.,.F.,.F.)
B_SPLINE_SURFACE_WITH_KNOTS((2,2),(3,2,2,3),(0.710318915640076,1.),(0.418207303127978,
0.428571428571429,0.435775021682622,0.435950698868169),.UNSPECIFIED.)
GEOMETRIC_REPRESENTATION_ITEM()
RATIONAL_B_SPLINE_SURFACE(((0.993779895952495,0.996362096314125,1.,0.997471472332736,
0.995452950231063,0.995452950231063,0.995452950231063),(0.993779895952495,
0.996362096314125,1.,0.997471472332736,0.995452950231063,0.995452950231063,
0.995452950231063)))
REPRESENTATION_ITEM('')
SURFACE()
);
#746=(
BOUNDED_SURFACE()
B_SPLINE_SURFACE(1,2,((#106106,#106107,#106108,#106109,#106110),(#106111,
#106112,#106113,#106114,#106115)),.UNSPECIFIED.,.F.,.F.,.F.)
B_SPLINE_SURFACE_WITH_KNOTS((2,2),(3,2,3),(0.710192959008433,1.),(0.297684616398974,
0.297856505190613,0.315045384354503),.UNSPECIFIED.)
GEOMETRIC_REPRESENTATION_ITEM()
RATIONAL_B_SPLINE_SURFACE(((0.992924952273132,0.992924952273132,0.992924952273132,
0.988942764095691,0.98786440923939),(0.992924952273132,0.992924952273132,
0.992924952273132,0.988942764095691,0.98786440923939)))
REPRESENTATION_ITEM('')
SURFACE()
);
#747=(
BOUNDED_SURFACE()
B_SPLINE_SURFACE(1,2,((#106123,#106124,#106125,#106126,#106127,#106128,
#106129),(#106130,#106131,#106132,#106133,#106134,#106135,#106136)),
 .UNSPECIFIED.,.F.,.F.,.F.)
B_SPLINE_SURFACE_WITH_KNOTS((2,2),(3,2,2,3),(0.71031891563985,1.),(0.418207303127979,
0.428571428571429,0.435775021682622,0.435950698868169),.UNSPECIFIED.)
GEOMETRIC_REPRESENTATION_ITEM()
RATIONAL_B_SPLINE_SURFACE(((0.993779895952495,0.996362096314125,1.,0.997471472332736,
0.995452950231063,0.995452950231063,0.995452950231063),(0.993779895952495,
0.996362096314125,1.,0.997471472332736,0.995452950231063,0.995452950231063,
0.995452950231063)))
REPRESENTATION_ITEM('')
SURFACE()
);
#748=(
BOUNDED_SURFACE()
B_SPLINE_SURFACE(1,2,((#106153,#106154,#106155,#106156,#106157),(#106158,
#106159,#106160,#106161,#106162)),.UNSPECIFIED.,.F.,.F.,.F.)
B_SPLINE_SURFACE_WITH_KNOTS((2,2),(3,2,3),(0.710192959008205,1.),(0.297684616398974,
0.297856505190613,0.315045384354503),.UNSPECIFIED.)
GEOMETRIC_REPRESENTATION_ITEM()
RATIONAL_B_SPLINE_SURFACE(((0.992924952273132,0.992924952273132,0.992924952273132,
0.988942764095691,0.987864409239391),(0.992924952273132,0.992924952273132,
0.992924952273132,0.988942764095691,0.98786440923939)))
REPRESENTATION_ITEM('')
SURFACE()
);
#749=(
BOUNDED_SURFACE()
B_SPLINE_SURFACE(1,2,((#106170,#106171,#106172,#106173,#106174,#106175,
#106176),(#106177,#106178,#106179,#106180,#106181,#106182,#106183)),
 .UNSPECIFIED.,.F.,.F.,.F.)
B_SPLINE_SURFACE_WITH_KNOTS((2,2),(3,2,2,3),(0.71031891564008,1.),(0.418207303127979,
0.428571428571429,0.435775021682622,0.435950698868169),.UNSPECIFIED.)
GEOMETRIC_REPRESENTATION_ITEM()
RATIONAL_B_SPLINE_SURFACE(((0.993779895952495,0.996362096314125,1.,0.997471472332736,
0.995452950231063,0.995452950231063,0.995452950231063),(0.993779895952495,
0.996362096314125,1.,0.997471472332736,0.995452950231063,0.995452950231063,
0.995452950231063)))
REPRESENTATION_ITEM('')
SURFACE()
);
#750=(
BOUNDED_SURFACE()
B_SPLINE_SURFACE(1,2,((#106200,#106201,#106202,#106203,#106204),(#106205,
#106206,#106207,#106208,#106209)),.UNSPECIFIED.,.F.,.F.,.F.)
B_SPLINE_SURFACE_WITH_KNOTS((2,2),(3,2,3),(0.71019295900844,1.),(0.297684616398974,
0.297856505190613,0.315045384354503),.UNSPECIFIED.)
GEOMETRIC_REPRESENTATION_ITEM()
RATIONAL_B_SPLINE_SURFACE(((0.992924952273132,0.992924952273132,0.992924952273132,
0.988942764095691,0.98786440923939),(0.992924952273132,0.992924952273132,
0.992924952273132,0.988942764095691,0.98786440923939)))
REPRESENTATION_ITEM('')
SURFACE()
);
#751=(
BOUNDED_SURFACE()
B_SPLINE_SURFACE(1,2,((#106217,#106218,#106219,#106220,#106221,#106222,
#106223),(#106224,#106225,#106226,#106227,#106228,#106229,#106230)),
 .UNSPECIFIED.,.F.,.F.,.F.)
B_SPLINE_SURFACE_WITH_KNOTS((2,2),(3,2,2,3),(0.710318915638946,1.),(0.418207303127979,
0.428571428571429,0.435775021682622,0.435950698868169),.UNSPECIFIED.)
GEOMETRIC_REPRESENTATION_ITEM()
RATIONAL_B_SPLINE_SURFACE(((0.993779895952495,0.996362096314125,1.,0.997471472332736,
0.995452950231063,0.995452950231063,0.995452950231063),(0.993779895952495,
0.996362096314125,1.,0.997471472332736,0.995452950231063,0.995452950231063,
0.995452950231063)))
REPRESENTATION_ITEM('')
SURFACE()
);
#752=(
BOUNDED_SURFACE()
B_SPLINE_SURFACE(1,2,((#106247,#106248,#106249,#106250,#106251),(#106252,
#106253,#106254,#106255,#106256)),.UNSPECIFIED.,.F.,.F.,.F.)
B_SPLINE_SURFACE_WITH_KNOTS((2,2),(3,2,3),(0.710192959007305,1.),(0.297684616398974,
0.297856505190613,0.315045384354503),.UNSPECIFIED.)
GEOMETRIC_REPRESENTATION_ITEM()
RATIONAL_B_SPLINE_SURFACE(((0.992924952273132,0.992924952273132,0.992924952273132,
0.988942764095691,0.98786440923939),(0.992924952273132,0.992924952273132,
0.992924952273132,0.988942764095691,0.98786440923939)))
REPRESENTATION_ITEM('')
SURFACE()
);
#753=(
BOUNDED_SURFACE()
B_SPLINE_SURFACE(1,2,((#106264,#106265,#106266,#106267,#106268,#106269,
#106270),(#106271,#106272,#106273,#106274,#106275,#106276,#106277)),
 .UNSPECIFIED.,.F.,.F.,.F.)
B_SPLINE_SURFACE_WITH_KNOTS((2,2),(3,2,2,3),(0.710318915639109,1.),(0.418207303127979,
0.428571428571429,0.435775021682622,0.435950698868169),.UNSPECIFIED.)
GEOMETRIC_REPRESENTATION_ITEM()
RATIONAL_B_SPLINE_SURFACE(((0.993779895952495,0.996362096314125,1.,0.997471472332736,
0.995452950231063,0.995452950231063,0.995452950231063),(0.993779895952495,
0.996362096314125,1.,0.997471472332736,0.995452950231063,0.995452950231063,
0.995452950231063)))
REPRESENTATION_ITEM('')
SURFACE()
);
#754=(
BOUNDED_SURFACE()
B_SPLINE_SURFACE(1,2,((#106294,#106295,#106296,#106297,#106298),(#106299,
#106300,#106301,#106302,#106303)),.UNSPECIFIED.,.F.,.F.,.F.)
B_SPLINE_SURFACE_WITH_KNOTS((2,2),(3,2,3),(0.710192959007464,1.),(0.297684616398492,
0.297856505190135,0.315045384354506),.UNSPECIFIED.)
GEOMETRIC_REPRESENTATION_ITEM()
RATIONAL_B_SPLINE_SURFACE(((0.992924952273353,0.992924952273353,0.992924952273353,
0.98894276409572,0.98786440923939),(0.992924952273353,0.992924952273353,
0.992924952273353,0.98894276409572,0.98786440923939)))
REPRESENTATION_ITEM('')
SURFACE()
);
#755=(
BOUNDED_SURFACE()
B_SPLINE_SURFACE(1,2,((#106311,#106312,#106313,#106314,#106315,#106316,
#106317),(#106318,#106319,#106320,#106321,#106322,#106323,#106324)),
 .UNSPECIFIED.,.F.,.F.,.F.)
B_SPLINE_SURFACE_WITH_KNOTS((2,2),(3,2,2,3),(0.710318915638971,1.),(0.418207303127979,
0.428571428571429,0.435775021682622,0.435950698868169),.UNSPECIFIED.)
GEOMETRIC_REPRESENTATION_ITEM()
RATIONAL_B_SPLINE_SURFACE(((0.993779895952495,0.996362096314125,1.,0.997471472332736,
0.995452950231063,0.995452950231063,0.995452950231063),(0.993779895952495,
0.996362096314125,1.,0.997471472332736,0.995452950231063,0.995452950231063,
0.995452950231063)))
REPRESENTATION_ITEM('')
SURFACE()
);
#756=(
BOUNDED_SURFACE()
B_SPLINE_SURFACE(1,2,((#106341,#106342,#106343,#106344,#106345),(#106346,
#106347,#106348,#106349,#106350)),.UNSPECIFIED.,.F.,.F.,.F.)
B_SPLINE_SURFACE_WITH_KNOTS((2,2),(3,2,3),(0.710192959007334,1.),(0.297684616398621,
0.297856505190263,0.315045384354506),.UNSPECIFIED.)
GEOMETRIC_REPRESENTATION_ITEM()
RATIONAL_B_SPLINE_SURFACE(((0.992924952273294,0.992924952273294,0.992924952273294,
0.988942764095713,0.98786440923939),(0.992924952273294,0.992924952273294,
0.992924952273294,0.988942764095713,0.98786440923939)))
REPRESENTATION_ITEM('')
SURFACE()
);
#757=(
BOUNDED_SURFACE()
B_SPLINE_SURFACE(1,2,((#106358,#106359,#106360,#106361,#106362,#106363,
#106364),(#106365,#106366,#106367,#106368,#106369,#106370,#106371)),
 .UNSPECIFIED.,.F.,.F.,.F.)
B_SPLINE_SURFACE_WITH_KNOTS((2,2),(3,2,2,3),(0.710318915639849,1.),(0.418207303127979,
0.428571428571429,0.435775021682622,0.435950698868169),.UNSPECIFIED.)
GEOMETRIC_REPRESENTATION_ITEM()
RATIONAL_B_SPLINE_SURFACE(((0.993779895952495,0.996362096314125,1.,0.997471472332736,
0.995452950231063,0.995452950231063,0.995452950231063),(0.993779895952495,
0.996362096314125,1.,0.997471472332736,0.995452950231063,0.995452950231063,
0.995452950231063)))
REPRESENTATION_ITEM('')
SURFACE()
);
#758=(
BOUNDED_SURFACE()
B_SPLINE_SURFACE(1,2,((#106388,#106389,#106390,#106391,#106392),(#106393,
#106394,#106395,#106396,#106397)),.UNSPECIFIED.,.F.,.F.,.F.)
B_SPLINE_SURFACE_WITH_KNOTS((2,2),(3,2,3),(0.710192959008238,1.),(0.297684616398974,
0.297856505190613,0.315045384354504),.UNSPECIFIED.)
GEOMETRIC_REPRESENTATION_ITEM()
RATIONAL_B_SPLINE_SURFACE(((0.992924952273132,0.992924952273132,0.992924952273132,
0.988942764095691,0.98786440923939),(0.992924952273132,0.992924952273132,
0.992924952273132,0.988942764095691,0.98786440923939)))
REPRESENTATION_ITEM('')
SURFACE()
);
#759=(
BOUNDED_SURFACE()
B_SPLINE_SURFACE(1,2,((#106405,#106406,#106407,#106408,#106409,#106410,
#106411),(#106412,#106413,#106414,#106415,#106416,#106417,#106418)),
 .UNSPECIFIED.,.F.,.F.,.F.)
B_SPLINE_SURFACE_WITH_KNOTS((2,2),(3,2,2,3),(0.710318915638589,1.),(0.418207303127979,
0.428571428571429,0.435775021682622,0.435950698868169),.UNSPECIFIED.)
GEOMETRIC_REPRESENTATION_ITEM()
RATIONAL_B_SPLINE_SURFACE(((0.993779895952495,0.996362096314125,1.,0.997471472332736,
0.995452950231063,0.995452950231063,0.995452950231063),(0.993779895952495,
0.996362096314125,1.,0.997471472332736,0.995452950231063,0.995452950231063,
0.995452950231063)))
REPRESENTATION_ITEM('')
SURFACE()
);
#760=(
BOUNDED_SURFACE()
B_SPLINE_SURFACE(1,2,((#106435,#106436,#106437,#106438,#106439),(#106440,
#106441,#106442,#106443,#106444)),.UNSPECIFIED.,.F.,.F.,.F.)
B_SPLINE_SURFACE_WITH_KNOTS((2,2),(3,2,3),(0.710192959006948,1.),(0.297684616398974,
0.297856505190613,0.315045384354503),.UNSPECIFIED.)
GEOMETRIC_REPRESENTATION_ITEM()
RATIONAL_B_SPLINE_SURFACE(((0.992924952273132,0.992924952273132,0.992924952273132,
0.988942764095691,0.98786440923939),(0.992924952273132,0.992924952273132,
0.992924952273132,0.988942764095691,0.98786440923939)))
REPRESENTATION_ITEM('')
SURFACE()
);
#761=(
BOUNDED_SURFACE()
B_SPLINE_SURFACE(1,2,((#106452,#106453,#106454,#106455,#106456,#106457,
#106458),(#106459,#106460,#106461,#106462,#106463,#106464,#106465)),
 .UNSPECIFIED.,.F.,.F.,.F.)
B_SPLINE_SURFACE_WITH_KNOTS((2,2),(3,2,2,3),(0.710318915638846,1.),(0.418207303127979,
0.428571428571429,0.435775021682622,0.435950698868169),.UNSPECIFIED.)
GEOMETRIC_REPRESENTATION_ITEM()
RATIONAL_B_SPLINE_SURFACE(((0.993779895952495,0.996362096314125,1.,0.997471472332736,
0.995452950231063,0.995452950231063,0.995452950231063),(0.993779895952495,
0.996362096314125,1.,0.997471472332736,0.995452950231063,0.995452950231063,
0.995452950231063)))
REPRESENTATION_ITEM('')
SURFACE()
);
#762=(
BOUNDED_SURFACE()
B_SPLINE_SURFACE(1,2,((#106482,#106483,#106484,#106485,#106486),(#106487,
#106488,#106489,#106490,#106491)),.UNSPECIFIED.,.F.,.F.,.F.)
B_SPLINE_SURFACE_WITH_KNOTS((2,2),(3,2,3),(0.710192959007198,1.),(0.297684616398974,
0.297856505190613,0.315045384354504),.UNSPECIFIED.)
GEOMETRIC_REPRESENTATION_ITEM()
RATIONAL_B_SPLINE_SURFACE(((0.992924952273132,0.992924952273132,0.992924952273132,
0.988942764095691,0.98786440923939),(0.992924952273132,0.992924952273132,
0.992924952273132,0.988942764095691,0.98786440923939)))
REPRESENTATION_ITEM('')
SURFACE()
);
#763=(
BOUNDED_SURFACE()
B_SPLINE_SURFACE(1,2,((#106499,#106500,#106501,#106502,#106503,#106504,
#106505),(#106506,#106507,#106508,#106509,#106510,#106511,#106512)),
 .UNSPECIFIED.,.F.,.F.,.F.)
B_SPLINE_SURFACE_WITH_KNOTS((2,2),(3,2,2,3),(0.710318915639085,1.),(0.418207303127979,
0.428571428571429,0.435775021682622,0.435950698868169),.UNSPECIFIED.)
GEOMETRIC_REPRESENTATION_ITEM()
RATIONAL_B_SPLINE_SURFACE(((0.993779895952495,0.996362096314125,1.,0.997471472332736,
0.995452950231063,0.995452950231063,0.995452950231063),(0.993779895952495,
0.996362096314125,1.,0.997471472332736,0.995452950231063,0.995452950231063,
0.995452950231063)))
REPRESENTATION_ITEM('')
SURFACE()
);
#764=(
BOUNDED_SURFACE()
B_SPLINE_SURFACE(1,2,((#106529,#106530,#106531,#106532,#106533),(#106534,
#106535,#106536,#106537,#106538)),.UNSPECIFIED.,.F.,.F.,.F.)
B_SPLINE_SURFACE_WITH_KNOTS((2,2),(3,2,3),(0.710192959007439,1.),(0.297684616398674,
0.297856505190316,0.315045384354505),.UNSPECIFIED.)
GEOMETRIC_REPRESENTATION_ITEM()
RATIONAL_B_SPLINE_SURFACE(((0.99292495227327,0.99292495227327,0.99292495227327,
0.98894276409571,0.98786440923939),(0.99292495227327,0.99292495227327,0.99292495227327,
0.988942764095709,0.98786440923939)))
REPRESENTATION_ITEM('')
SURFACE()
);
#765=(
BOUNDED_SURFACE()
B_SPLINE_SURFACE(1,2,((#106546,#106547,#106548,#106549,#106550,#106551,
#106552),(#106553,#106554,#106555,#106556,#106557,#106558,#106559)),
 .UNSPECIFIED.,.F.,.F.,.F.)
B_SPLINE_SURFACE_WITH_KNOTS((2,2),(3,2,2,3),(0.710318915639157,1.),(0.418207303127979,
0.428571428571429,0.435775021682622,0.435950698868169),.UNSPECIFIED.)
GEOMETRIC_REPRESENTATION_ITEM()
RATIONAL_B_SPLINE_SURFACE(((0.993779895952495,0.996362096314125,1.,0.997471472332736,
0.995452950231063,0.995452950231063,0.995452950231063),(0.993779895952495,
0.996362096314125,1.,0.997471472332736,0.995452950231063,0.995452950231063,
0.995452950231063)))
REPRESENTATION_ITEM('')
SURFACE()
);
#766=(
BOUNDED_SURFACE()
B_SPLINE_SURFACE(1,2,((#106576,#106577,#106578,#106579,#106580),(#106581,
#106582,#106583,#106584,#106585)),.UNSPECIFIED.,.F.,.F.,.F.)
B_SPLINE_SURFACE_WITH_KNOTS((2,2),(3,2,3),(0.710192959007517,1.),(0.297684616398974,
0.297856505190613,0.315045384354506),.UNSPECIFIED.)
GEOMETRIC_REPRESENTATION_ITEM()
RATIONAL_B_SPLINE_SURFACE(((0.992924952273132,0.992924952273132,0.992924952273132,
0.98894276409569,0.98786440923939),(0.992924952273132,0.992924952273132,
0.992924952273132,0.98894276409569,0.98786440923939)))
REPRESENTATION_ITEM('')
SURFACE()
);
#767=(
BOUNDED_SURFACE()
B_SPLINE_SURFACE(1,2,((#106593,#106594,#106595,#106596,#106597,#106598,
#106599),(#106600,#106601,#106602,#106603,#106604,#106605,#106606)),
 .UNSPECIFIED.,.F.,.F.,.F.)
B_SPLINE_SURFACE_WITH_KNOTS((2,2),(3,2,2,3),(0.710318915638831,1.),(0.418207303127979,
0.428571428571429,0.435775021682622,0.435950698868169),.UNSPECIFIED.)
GEOMETRIC_REPRESENTATION_ITEM()
RATIONAL_B_SPLINE_SURFACE(((0.993779895952495,0.996362096314125,1.,0.997471472332736,
0.995452950231063,0.995452950231063,0.995452950231063),(0.993779895952495,
0.996362096314125,1.,0.997471472332736,0.995452950231063,0.995452950231063,
0.995452950231063)))
REPRESENTATION_ITEM('')
SURFACE()
);
#768=(
BOUNDED_SURFACE()
B_SPLINE_SURFACE(1,2,((#106623,#106624,#106625,#106626,#106627),(#106628,
#106629,#106630,#106631,#106632)),.UNSPECIFIED.,.F.,.F.,.F.)
B_SPLINE_SURFACE_WITH_KNOTS((2,2),(3,2,3),(0.710192959007199,1.),(0.297684616398623,
0.297856505190265,0.315045384354506),.UNSPECIFIED.)
GEOMETRIC_REPRESENTATION_ITEM()
RATIONAL_B_SPLINE_SURFACE(((0.992924952273293,0.992924952273293,0.992924952273293,
0.988942764095713,0.98786440923939),(0.992924952273293,0.992924952273293,
0.992924952273293,0.988942764095713,0.98786440923939)))
REPRESENTATION_ITEM('')
SURFACE()
);
#769=(
BOUNDED_SURFACE()
B_SPLINE_SURFACE(1,2,((#106640,#106641,#106642,#106643,#106644,#106645,
#106646),(#106647,#106648,#106649,#106650,#106651,#106652,#106653)),
 .UNSPECIFIED.,.F.,.F.,.F.)
B_SPLINE_SURFACE_WITH_KNOTS((2,2),(3,2,2,3),(0.710318915638982,1.),(0.418207303127979,
0.428571428571429,0.435775021682622,0.435950698868169),.UNSPECIFIED.)
GEOMETRIC_REPRESENTATION_ITEM()
RATIONAL_B_SPLINE_SURFACE(((0.993779895952495,0.996362096314125,1.,0.997471472332736,
0.995452950231063,0.995452950231063,0.995452950231063),(0.993779895952495,
0.996362096314125,1.,0.997471472332736,0.995452950231063,0.995452950231063,
0.995452950231063)))
REPRESENTATION_ITEM('')
SURFACE()
);
#770=(
BOUNDED_SURFACE()
B_SPLINE_SURFACE(1,2,((#106670,#106671,#106672,#106673,#106674),(#106675,
#106676,#106677,#106678,#106679)),.UNSPECIFIED.,.F.,.F.,.F.)
B_SPLINE_SURFACE_WITH_KNOTS((2,2),(3,2,3),(0.710192959007344,1.),(0.297684616398843,
0.297856505190483,0.315045384354504),.UNSPECIFIED.)
GEOMETRIC_REPRESENTATION_ITEM()
RATIONAL_B_SPLINE_SURFACE(((0.992924952273192,0.992924952273192,0.992924952273192,
0.988942764095699,0.98786440923939),(0.992924952273192,0.992924952273192,
0.992924952273192,0.988942764095699,0.98786440923939)))
REPRESENTATION_ITEM('')
SURFACE()
);
#771=(
BOUNDED_SURFACE()
B_SPLINE_SURFACE(1,2,((#106687,#106688,#106689,#106690,#106691,#106692,
#106693),(#106694,#106695,#106696,#106697,#106698,#106699,#106700)),
 .UNSPECIFIED.,.F.,.F.,.F.)
B_SPLINE_SURFACE_WITH_KNOTS((2,2),(3,2,2,3),(0.710318915638968,1.),(0.418207303127979,
0.428571428571429,0.435775021682622,0.435950698868169),.UNSPECIFIED.)
GEOMETRIC_REPRESENTATION_ITEM()
RATIONAL_B_SPLINE_SURFACE(((0.993779895952495,0.996362096314125,1.,0.997471472332736,
0.995452950231063,0.995452950231063,0.995452950231063),(0.993779895952495,
0.996362096314125,1.,0.997471472332736,0.995452950231063,0.995452950231063,
0.995452950231063)))
REPRESENTATION_ITEM('')
SURFACE()
);
#772=(
BOUNDED_SURFACE()
B_SPLINE_SURFACE(1,2,((#106717,#106718,#106719,#106720,#106721),(#106722,
#106723,#106724,#106725,#106726)),.UNSPECIFIED.,.F.,.F.,.F.)
B_SPLINE_SURFACE_WITH_KNOTS((2,2),(3,2,3),(0.710192959007328,1.),(0.297684616398544,
0.297856505190187,0.315045384354506),.UNSPECIFIED.)
GEOMETRIC_REPRESENTATION_ITEM()
RATIONAL_B_SPLINE_SURFACE(((0.99292495227333,0.99292495227333,0.99292495227333,
0.988942764095718,0.98786440923939),(0.99292495227333,0.99292495227333,
0.99292495227333,0.988942764095718,0.98786440923939)))
REPRESENTATION_ITEM('')
SURFACE()
);
#773=(
BOUNDED_SURFACE()
B_SPLINE_SURFACE(1,2,((#106746,#106747,#106748,#106749,#106750,#106751,
#106752),(#106753,#106754,#106755,#106756,#106757,#106758,#106759)),
 .UNSPECIFIED.,.F.,.F.,.F.)
B_SPLINE_SURFACE_WITH_KNOTS((2,2),(3,2,2,3),(0.710318915638782,1.),(0.418207303127979,
0.428571428571429,0.435775021682622,0.435950698868169),.UNSPECIFIED.)
GEOMETRIC_REPRESENTATION_ITEM()
RATIONAL_B_SPLINE_SURFACE(((0.993779895952495,0.996362096314125,1.,0.997471472332736,
0.995452950231063,0.995452950231063,0.995452950231063),(0.993779895952495,
0.996362096314125,1.,0.997471472332736,0.995452950231063,0.995452950231063,
0.995452950231063)))
REPRESENTATION_ITEM('')
SURFACE()
);
#774=(
BOUNDED_SURFACE()
B_SPLINE_SURFACE(1,2,((#106761,#106762,#106763),(#106764,#106765,#106766)),
 .UNSPECIFIED.,.F.,.F.,.F.)
B_SPLINE_SURFACE_WITH_KNOTS((2,2),(3,3),(0.710318915639741,1.),(0.331965345783649,
0.349369696259361),.UNSPECIFIED.)
GEOMETRIC_REPRESENTATION_ITEM()
RATIONAL_B_SPLINE_SURFACE(((0.988555124858682,0.99035748704491,0.99513694090229),
(0.988555124858682,0.99035748704491,0.99513694090229)))
REPRESENTATION_ITEM('')
SURFACE()
);
#775=(
BOUNDED_SURFACE()
B_SPLINE_SURFACE(1,2,((#106775,#106776,#106777,#106778,#106779),(#106780,
#106781,#106782,#106783,#106784),(#106785,#106786,#106787,#106788,#106789)),
 .UNSPECIFIED.,.F.,.F.,.F.)
B_SPLINE_SURFACE_WITH_KNOTS((2,1,2),(3,2,3),(0.709600445964224,1.,1.00289807040992),
(0.383340713896642,0.383933227114987,0.401145492974693),.UNSPECIFIED.)
GEOMETRIC_REPRESENTATION_ITEM()
RATIONAL_B_SPLINE_SURFACE(((0.988246641953811,0.988246641953811,0.988246641953811,
0.986737013496293,0.988139125479961),(0.988246641953811,0.988246641953811,
0.988246641953811,0.986737013496293,0.988139125479961),(0.988246641953811,
0.988246641953811,0.988246641953811,0.986737013496293,0.988139125479961)))
REPRESENTATION_ITEM('')
SURFACE()
);
#776=(
BOUNDED_SURFACE()
B_SPLINE_SURFACE(1,2,((#106798,#106799,#106800),(#106801,#106802,#106803)),
 .UNSPECIFIED.,.F.,.F.,.F.)
B_SPLINE_SURFACE_WITH_KNOTS((2,2),(3,3),(0.710318915639637,1.),(0.331965345783649,
0.349369696259364),.UNSPECIFIED.)
GEOMETRIC_REPRESENTATION_ITEM()
RATIONAL_B_SPLINE_SURFACE(((0.988555124858682,0.990357487044911,0.995136940902291),
(0.988555124858682,0.990357487044911,0.995136940902291)))
REPRESENTATION_ITEM('')
SURFACE()
);
#777=(
BOUNDED_SURFACE()
B_SPLINE_SURFACE(1,2,((#106805,#106806,#106807,#106808,#106809),(#106810,
#106811,#106812,#106813,#106814),(#106815,#106816,#106817,#106818,#106819)),
 .UNSPECIFIED.,.F.,.F.,.F.)
B_SPLINE_SURFACE_WITH_KNOTS((2,1,2),(3,2,3),(0.709600445987324,1.,1.00289807040993),
(0.383340713920641,0.383933227114984,0.401145492974693),.UNSPECIFIED.)
GEOMETRIC_REPRESENTATION_ITEM()
RATIONAL_B_SPLINE_SURFACE(((0.988246641953811,0.988246641953811,0.988246641953811,
0.986737013496293,0.988139125479962),(0.988246641953811,0.988246641953811,
0.988246641953811,0.986737013496293,0.988139125479962),(0.988246641953811,
0.988246641953811,0.988246641953811,0.986737013496293,0.988139125479962)))
REPRESENTATION_ITEM('')
SURFACE()
);
#778=(
BOUNDED_SURFACE()
B_SPLINE_SURFACE(1,2,((#106828,#106829,#106830),(#106831,#106832,#106833)),
 .UNSPECIFIED.,.F.,.F.,.F.)
B_SPLINE_SURFACE_WITH_KNOTS((2,2),(3,3),(0.710318915638942,1.),(0.331965345783649,
0.349369696259367),.UNSPECIFIED.)
GEOMETRIC_REPRESENTATION_ITEM()
RATIONAL_B_SPLINE_SURFACE(((0.988555124858681,0.990357487044911,0.995136940902293),
(0.988555124858681,0.990357487044911,0.995136940902293)))
REPRESENTATION_ITEM('')
SURFACE()
);
#779=(
BOUNDED_SURFACE()
B_SPLINE_SURFACE(1,2,((#106835,#106836,#106837,#106838,#106839),(#106840,
#106841,#106842,#106843,#106844),(#106845,#106846,#106847,#106848,#106849)),
 .UNSPECIFIED.,.F.,.F.,.F.)
B_SPLINE_SURFACE_WITH_KNOTS((2,1,2),(3,2,3),(0.709600445972972,1.,1.00289807040993),
(0.383340713906237,0.383933227114983,0.401145492974693),.UNSPECIFIED.)
GEOMETRIC_REPRESENTATION_ITEM()
RATIONAL_B_SPLINE_SURFACE(((0.988246641953811,0.988246641953811,0.988246641953811,
0.986737013496293,0.988139125479961),(0.988246641953811,0.988246641953811,
0.988246641953811,0.986737013496293,0.988139125479961),(0.988246641953811,
0.988246641953811,0.988246641953811,0.986737013496293,0.988139125479961)))
REPRESENTATION_ITEM('')
SURFACE()
);
#780=(
BOUNDED_SURFACE()
B_SPLINE_SURFACE(1,2,((#106858,#106859,#106860),(#106861,#106862,#106863)),
 .UNSPECIFIED.,.F.,.F.,.F.)
B_SPLINE_SURFACE_WITH_KNOTS((2,2),(3,3),(0.710318915639095,1.),(0.331965345783647,
0.349369696259361),.UNSPECIFIED.)
GEOMETRIC_REPRESENTATION_ITEM()
RATIONAL_B_SPLINE_SURFACE(((0.988555124858681,0.99035748704491,0.99513694090229),
(0.988555124858681,0.99035748704491,0.99513694090229)))
REPRESENTATION_ITEM('')
SURFACE()
);
#781=(
BOUNDED_SURFACE()
B_SPLINE_SURFACE(1,2,((#106865,#106866,#106867,#106868,#106869),(#106870,
#106871,#106872,#106873,#106874),(#106875,#106876,#106877,#106878,#106879)),
 .UNSPECIFIED.,.F.,.F.,.F.)
B_SPLINE_SURFACE_WITH_KNOTS((2,1,2),(3,2,3),(0.7096004459634,1.,1.00289807040993),
(0.383340713896623,0.383933227114983,0.401145492974693),.UNSPECIFIED.)
GEOMETRIC_REPRESENTATION_ITEM()
RATIONAL_B_SPLINE_SURFACE(((0.988246641953811,0.988246641953811,0.988246641953811,
0.986737013496292,0.988139125479961),(0.988246641953811,0.988246641953811,
0.988246641953811,0.986737013496293,0.988139125479961),(0.988246641953811,
0.988246641953811,0.988246641953811,0.986737013496293,0.988139125479961)))
REPRESENTATION_ITEM('')
SURFACE()
);
#782=(
BOUNDED_SURFACE()
B_SPLINE_SURFACE(1,2,((#106888,#106889,#106890),(#106891,#106892,#106893)),
 .UNSPECIFIED.,.F.,.F.,.F.)
B_SPLINE_SURFACE_WITH_KNOTS((2,2),(3,3),(0.710318915639123,1.),(0.331965345783649,
0.349369696259361),.UNSPECIFIED.)
GEOMETRIC_REPRESENTATION_ITEM()
RATIONAL_B_SPLINE_SURFACE(((0.988555124858681,0.99035748704491,0.99513694090229),
(0.988555124858681,0.99035748704491,0.99513694090229)))
REPRESENTATION_ITEM('')
SURFACE()
);
#783=(
BOUNDED_SURFACE()
B_SPLINE_SURFACE(1,2,((#106895,#106896,#106897,#106898,#106899),(#106900,
#106901,#106902,#106903,#106904),(#106905,#106906,#106907,#106908,#106909)),
 .UNSPECIFIED.,.F.,.F.,.F.)
B_SPLINE_SURFACE_WITH_KNOTS((2,1,2),(3,2,3),(0.709600445963976,1.,1.00289807040993),
(0.383340713897237,0.383933227114985,0.401145492974693),.UNSPECIFIED.)
GEOMETRIC_REPRESENTATION_ITEM()
RATIONAL_B_SPLINE_SURFACE(((0.988246641953811,0.988246641953811,0.988246641953811,
0.986737013496293,0.988139125479962),(0.988246641953811,0.988246641953811,
0.988246641953811,0.986737013496293,0.988139125479962),(0.988246641953811,
0.988246641953811,0.988246641953811,0.986737013496293,0.988139125479962)))
REPRESENTATION_ITEM('')
SURFACE()
);
#784=(
BOUNDED_SURFACE()
B_SPLINE_SURFACE(1,2,((#106918,#106919,#106920),(#106921,#106922,#106923)),
 .UNSPECIFIED.,.F.,.F.,.F.)
B_SPLINE_SURFACE_WITH_KNOTS((2,2),(3,3),(0.710318915638953,1.),(0.331965345783649,
0.349369696259361),.UNSPECIFIED.)
GEOMETRIC_REPRESENTATION_ITEM()
RATIONAL_B_SPLINE_SURFACE(((0.988555124858682,0.99035748704491,0.99513694090229),
(0.988555124858681,0.99035748704491,0.99513694090229)))
REPRESENTATION_ITEM('')
SURFACE()
);
#785=(
BOUNDED_SURFACE()
B_SPLINE_SURFACE(1,2,((#106925,#106926,#106927,#106928,#106929),(#106930,
#106931,#106932,#106933,#106934),(#106935,#106936,#106937,#106938,#106939)),
 .UNSPECIFIED.,.F.,.F.,.F.)
B_SPLINE_SURFACE_WITH_KNOTS((2,1,2),(3,2,3),(0.709600445977375,1.,1.00289807040992),
(0.383340713910112,0.38393322711497,0.401145492974693),.UNSPECIFIED.)
GEOMETRIC_REPRESENTATION_ITEM()
RATIONAL_B_SPLINE_SURFACE(((0.988246641953814,0.988246641953814,0.988246641953814,
0.986737013496291,0.988139125479961),(0.988246641953814,0.988246641953814,
0.988246641953814,0.986737013496291,0.988139125479961),(0.988246641953814,
0.988246641953814,0.988246641953814,0.986737013496291,0.988139125479961)))
REPRESENTATION_ITEM('')
SURFACE()
);
#786=(
BOUNDED_SURFACE()
B_SPLINE_SURFACE(1,2,((#106948,#106949,#106950),(#106951,#106952,#106953)),
 .UNSPECIFIED.,.F.,.F.,.F.)
B_SPLINE_SURFACE_WITH_KNOTS((2,2),(3,3),(0.710318915639313,1.),(0.331965345783649,
0.349369696259361),.UNSPECIFIED.)
GEOMETRIC_REPRESENTATION_ITEM()
RATIONAL_B_SPLINE_SURFACE(((0.988555124858681,0.99035748704491,0.99513694090229),
(0.988555124858681,0.99035748704491,0.99513694090229)))
REPRESENTATION_ITEM('')
SURFACE()
);
#787=(
BOUNDED_SURFACE()
B_SPLINE_SURFACE(1,2,((#106955,#106956,#106957,#106958,#106959),(#106960,
#106961,#106962,#106963,#106964),(#106965,#106966,#106967,#106968,#106969)),
 .UNSPECIFIED.,.F.,.F.,.F.)
B_SPLINE_SURFACE_WITH_KNOTS((2,1,2),(3,2,3),(0.709600445975744,1.,1.00289807040992),
(0.383340713908609,0.383933227114969,0.401145492974693),.UNSPECIFIED.)
GEOMETRIC_REPRESENTATION_ITEM()
RATIONAL_B_SPLINE_SURFACE(((0.988246641953814,0.988246641953814,0.988246641953814,
0.986737013496292,0.988139125479962),(0.988246641953814,0.988246641953814,
0.988246641953814,0.986737013496292,0.988139125479962),(0.988246641953814,
0.988246641953814,0.988246641953814,0.986737013496292,0.988139125479962)))
REPRESENTATION_ITEM('')
SURFACE()
);
#788=(
BOUNDED_SURFACE()
B_SPLINE_SURFACE(1,2,((#106978,#106979,#106980),(#106981,#106982,#106983)),
 .UNSPECIFIED.,.F.,.F.,.F.)
B_SPLINE_SURFACE_WITH_KNOTS((2,2),(3,3),(0.710318915639192,1.),(0.331965345783646,
0.349369696259361),.UNSPECIFIED.)
GEOMETRIC_REPRESENTATION_ITEM()
RATIONAL_B_SPLINE_SURFACE(((0.988555124858681,0.99035748704491,0.99513694090229),
(0.988555124858681,0.99035748704491,0.99513694090229)))
REPRESENTATION_ITEM('')
SURFACE()
);
#789=(
BOUNDED_SURFACE()
B_SPLINE_SURFACE(1,2,((#106985,#106986,#106987,#106988,#106989),(#106990,
#106991,#106992,#106993,#106994),(#106995,#106996,#106997,#106998,#106999)),
 .UNSPECIFIED.,.F.,.F.,.F.)
B_SPLINE_SURFACE_WITH_KNOTS((2,1,2),(3,2,3),(0.709600445963145,1.,1.00289807040993),
(0.383340713896254,0.38393322711497,0.401145492974693),.UNSPECIFIED.)
GEOMETRIC_REPRESENTATION_ITEM()
RATIONAL_B_SPLINE_SURFACE(((0.988246641953814,0.988246641953814,0.988246641953814,
0.986737013496292,0.988139125479962),(0.988246641953814,0.988246641953814,
0.988246641953814,0.986737013496292,0.988139125479962),(0.988246641953814,
0.988246641953814,0.988246641953814,0.986737013496292,0.988139125479962)))
REPRESENTATION_ITEM('')
SURFACE()
);
#790=(
BOUNDED_SURFACE()
B_SPLINE_SURFACE(1,2,((#107008,#107009,#107010),(#107011,#107012,#107013)),
 .UNSPECIFIED.,.F.,.F.,.F.)
B_SPLINE_SURFACE_WITH_KNOTS((2,2),(3,3),(0.710318915638951,1.),(0.331965345783647,
0.349369696259361),.UNSPECIFIED.)
GEOMETRIC_REPRESENTATION_ITEM()
RATIONAL_B_SPLINE_SURFACE(((0.988555124858681,0.99035748704491,0.99513694090229),
(0.988555124858681,0.99035748704491,0.99513694090229)))
REPRESENTATION_ITEM('')
SURFACE()
);
#791=(
BOUNDED_SURFACE()
B_SPLINE_SURFACE(1,2,((#107015,#107016,#107017,#107018,#107019),(#107020,
#107021,#107022,#107023,#107024),(#107025,#107026,#107027,#107028,#107029)),
 .UNSPECIFIED.,.F.,.F.,.F.)
B_SPLINE_SURFACE_WITH_KNOTS((2,1,2),(3,2,3),(0.709600445963726,1.,1.00289807040993),
(0.383340713897051,0.38393322711497,0.401145492974693),.UNSPECIFIED.)
GEOMETRIC_REPRESENTATION_ITEM()
RATIONAL_B_SPLINE_SURFACE(((0.988246641953814,0.988246641953814,0.988246641953814,
0.986737013496292,0.988139125479961),(0.988246641953814,0.988246641953814,
0.988246641953814,0.986737013496292,0.988139125479961),(0.988246641953814,
0.988246641953814,0.988246641953814,0.986737013496292,0.988139125479961)))
REPRESENTATION_ITEM('')
SURFACE()
);
#792=(
BOUNDED_SURFACE()
B_SPLINE_SURFACE(1,2,((#107038,#107039,#107040),(#107041,#107042,#107043)),
 .UNSPECIFIED.,.F.,.F.,.F.)
B_SPLINE_SURFACE_WITH_KNOTS((2,2),(3,3),(0.710318915638733,1.),(0.331965345783646,
0.349369696259361),.UNSPECIFIED.)
GEOMETRIC_REPRESENTATION_ITEM()
RATIONAL_B_SPLINE_SURFACE(((0.988555124858681,0.99035748704491,0.99513694090229),
(0.988555124858681,0.99035748704491,0.99513694090229)))
REPRESENTATION_ITEM('')
SURFACE()
);
#793=(
BOUNDED_SURFACE()
B_SPLINE_SURFACE(1,2,((#107045,#107046,#107047,#107048,#107049),(#107050,
#107051,#107052,#107053,#107054),(#107055,#107056,#107057,#107058,#107059)),
 .UNSPECIFIED.,.F.,.F.,.F.)
B_SPLINE_SURFACE_WITH_KNOTS((2,1,2),(3,2,3),(0.709600445979167,1.,1.00289807040992),
(0.383340713911332,0.383933227114987,0.401145492974693),.UNSPECIFIED.)
GEOMETRIC_REPRESENTATION_ITEM()
RATIONAL_B_SPLINE_SURFACE(((0.988246641953811,0.988246641953811,0.988246641953811,
0.986737013496293,0.988139125479962),(0.988246641953811,0.988246641953811,
0.988246641953811,0.986737013496293,0.988139125479962),(0.988246641953811,
0.988246641953811,0.988246641953811,0.986737013496293,0.988139125479962)))
REPRESENTATION_ITEM('')
SURFACE()
);
#794=(
BOUNDED_SURFACE()
B_SPLINE_SURFACE(1,2,((#107068,#107069,#107070),(#107071,#107072,#107073)),
 .UNSPECIFIED.,.F.,.F.,.F.)
B_SPLINE_SURFACE_WITH_KNOTS((2,2),(3,3),(0.710318915639885,1.),(0.331965345783647,
0.349369696259361),.UNSPECIFIED.)
GEOMETRIC_REPRESENTATION_ITEM()
RATIONAL_B_SPLINE_SURFACE(((0.988555124858681,0.99035748704491,0.99513694090229),
(0.988555124858681,0.99035748704491,0.99513694090229)))
REPRESENTATION_ITEM('')
SURFACE()
);
#795=(
BOUNDED_SURFACE()
B_SPLINE_SURFACE(1,2,((#107075,#107076,#107077,#107078,#107079),(#107080,
#107081,#107082,#107083,#107084),(#107085,#107086,#107087,#107088,#107089)),
 .UNSPECIFIED.,.F.,.F.,.F.)
B_SPLINE_SURFACE_WITH_KNOTS((2,1,2),(3,2,3),(0.709600445978175,1.,1.00289807040992),
(0.383340713910296,0.383933227114987,0.401145492974693),.UNSPECIFIED.)
GEOMETRIC_REPRESENTATION_ITEM()
RATIONAL_B_SPLINE_SURFACE(((0.988246641953811,0.988246641953811,0.988246641953811,
0.986737013496293,0.988139125479961),(0.988246641953811,0.988246641953811,
0.988246641953811,0.986737013496293,0.988139125479961),(0.988246641953811,
0.988246641953811,0.988246641953811,0.986737013496293,0.988139125479961)))
REPRESENTATION_ITEM('')
SURFACE()
);
#796=(
BOUNDED_SURFACE()
B_SPLINE_SURFACE(1,2,((#107098,#107099,#107100),(#107101,#107102,#107103)),
 .UNSPECIFIED.,.F.,.F.,.F.)
B_SPLINE_SURFACE_WITH_KNOTS((2,2),(3,3),(0.71031891563993,1.),(0.331965345783646,
0.349369696259361),.UNSPECIFIED.)
GEOMETRIC_REPRESENTATION_ITEM()
RATIONAL_B_SPLINE_SURFACE(((0.988555124858681,0.99035748704491,0.99513694090229),
(0.988555124858681,0.99035748704491,0.99513694090229)))
REPRESENTATION_ITEM('')
SURFACE()
);
#797=(
BOUNDED_SURFACE()
B_SPLINE_SURFACE(1,2,((#107105,#107106,#107107,#107108,#107109),(#107110,
#107111,#107112,#107113,#107114),(#107115,#107116,#107117,#107118,#107119)),
 .UNSPECIFIED.,.F.,.F.,.F.)
B_SPLINE_SURFACE_WITH_KNOTS((2,1,2),(3,2,3),(0.709600445969953,1.,1.00289807040992),
(0.383340713901921,0.383933227114987,0.401145492974693),.UNSPECIFIED.)
GEOMETRIC_REPRESENTATION_ITEM()
RATIONAL_B_SPLINE_SURFACE(((0.988246641953811,0.988246641953811,0.988246641953811,
0.986737013496293,0.988139125479962),(0.988246641953811,0.988246641953811,
0.988246641953811,0.986737013496293,0.988139125479962),(0.988246641953811,
0.988246641953811,0.988246641953811,0.986737013496293,0.988139125479962)))
REPRESENTATION_ITEM('')
SURFACE()
);
#798=(
BOUNDED_SURFACE()
B_SPLINE_SURFACE(1,2,((#107128,#107129,#107130),(#107131,#107132,#107133)),
 .UNSPECIFIED.,.F.,.F.,.F.)
B_SPLINE_SURFACE_WITH_KNOTS((2,2),(3,3),(0.710318915640068,1.),(0.331965345783649,
0.349369696259361),.UNSPECIFIED.)
GEOMETRIC_REPRESENTATION_ITEM()
RATIONAL_B_SPLINE_SURFACE(((0.988555124858682,0.99035748704491,0.99513694090229),
(0.988555124858682,0.99035748704491,0.99513694090229)))
REPRESENTATION_ITEM('')
SURFACE()
);
#799=(
BOUNDED_SURFACE()
B_SPLINE_SURFACE(1,2,((#107135,#107136,#107137,#107138,#107139),(#107140,
#107141,#107142,#107143,#107144),(#107145,#107146,#107147,#107148,#107149)),
 .UNSPECIFIED.,.F.,.F.,.F.)
B_SPLINE_SURFACE_WITH_KNOTS((2,1,2),(3,2,3),(0.70960044597758,1.,1.00289807040992),
(0.383340713909544,0.383933227114987,0.401145492974693),.UNSPECIFIED.)
GEOMETRIC_REPRESENTATION_ITEM()
RATIONAL_B_SPLINE_SURFACE(((0.988246641953811,0.988246641953811,0.988246641953811,
0.986737013496293,0.988139125479962),(0.988246641953811,0.988246641953811,
0.988246641953811,0.986737013496293,0.988139125479962),(0.988246641953811,
0.988246641953811,0.988246641953811,0.986737013496293,0.988139125479962)))
REPRESENTATION_ITEM('')
SURFACE()
);
#800=(
BOUNDED_SURFACE()
B_SPLINE_SURFACE(1,2,((#107158,#107159,#107160),(#107161,#107162,#107163)),
 .UNSPECIFIED.,.F.,.F.,.F.)
B_SPLINE_SURFACE_WITH_KNOTS((2,2),(3,3),(0.71031891564007,1.),(0.331965345783649,
0.349369696259361),.UNSPECIFIED.)
GEOMETRIC_REPRESENTATION_ITEM()
RATIONAL_B_SPLINE_SURFACE(((0.988555124858681,0.99035748704491,0.99513694090229),
(0.988555124858681,0.99035748704491,0.99513694090229)))
REPRESENTATION_ITEM('')
SURFACE()
);
#801=(
BOUNDED_SURFACE()
B_SPLINE_SURFACE(1,2,((#107165,#107166,#107167,#107168,#107169),(#107170,
#107171,#107172,#107173,#107174),(#107175,#107176,#107177,#107178,#107179)),
 .UNSPECIFIED.,.F.,.F.,.F.)
B_SPLINE_SURFACE_WITH_KNOTS((2,1,2),(3,2,3),(0.709600445987776,1.,1.00289807040992),
(0.383340713919749,0.383933227114986,0.401145492974693),.UNSPECIFIED.)
GEOMETRIC_REPRESENTATION_ITEM()
RATIONAL_B_SPLINE_SURFACE(((0.988246641953811,0.988246641953811,0.988246641953811,
0.986737013496293,0.988139125479962),(0.988246641953811,0.988246641953811,
0.988246641953811,0.986737013496293,0.988139125479962),(0.988246641953811,
0.988246641953811,0.988246641953811,0.986737013496293,0.988139125479962)))
REPRESENTATION_ITEM('')
SURFACE()
);
#802=(
BOUNDED_SURFACE()
B_SPLINE_SURFACE(1,2,((#107188,#107189,#107190),(#107191,#107192,#107193)),
 .UNSPECIFIED.,.F.,.F.,.F.)
B_SPLINE_SURFACE_WITH_KNOTS((2,2),(3,3),(0.710318915640073,1.),(0.331965345783649,
0.349369696259361),.UNSPECIFIED.)
GEOMETRIC_REPRESENTATION_ITEM()
RATIONAL_B_SPLINE_SURFACE(((0.988555124858682,0.99035748704491,0.99513694090229),
(0.988555124858681,0.99035748704491,0.99513694090229)))
REPRESENTATION_ITEM('')
SURFACE()
);
#803=(
BOUNDED_SURFACE()
B_SPLINE_SURFACE(1,2,((#107195,#107196,#107197,#107198,#107199),(#107200,
#107201,#107202,#107203,#107204),(#107205,#107206,#107207,#107208,#107209)),
 .UNSPECIFIED.,.F.,.F.,.F.)
B_SPLINE_SURFACE_WITH_KNOTS((2,1,2),(3,2,3),(0.709600445965168,1.,1.00289807040992),
(0.383340713897137,0.383933227114987,0.401145492974693),.UNSPECIFIED.)
GEOMETRIC_REPRESENTATION_ITEM()
RATIONAL_B_SPLINE_SURFACE(((0.988246641953811,0.988246641953811,0.988246641953811,
0.986737013496293,0.988139125479962),(0.988246641953811,0.988246641953811,
0.988246641953811,0.986737013496293,0.988139125479962),(0.988246641953811,
0.988246641953811,0.988246641953811,0.986737013496293,0.988139125479962)))
REPRESENTATION_ITEM('')
SURFACE()
);
#804=(
BOUNDED_SURFACE()
B_SPLINE_SURFACE(1,2,((#107218,#107219,#107220),(#107221,#107222,#107223)),
 .UNSPECIFIED.,.F.,.F.,.F.)
B_SPLINE_SURFACE_WITH_KNOTS((2,2),(3,3),(0.71031891564008,1.),(0.331965345783649,
0.349369696259361),.UNSPECIFIED.)
GEOMETRIC_REPRESENTATION_ITEM()
RATIONAL_B_SPLINE_SURFACE(((0.988555124858681,0.99035748704491,0.99513694090229),
(0.988555124858681,0.99035748704491,0.99513694090229)))
REPRESENTATION_ITEM('')
SURFACE()
);
#805=(
BOUNDED_SURFACE()
B_SPLINE_SURFACE(1,2,((#107225,#107226,#107227,#107228,#107229),(#107230,
#107231,#107232,#107233,#107234),(#107235,#107236,#107237,#107238,#107239)),
 .UNSPECIFIED.,.F.,.F.,.F.)
B_SPLINE_SURFACE_WITH_KNOTS((2,1,2),(3,2,3),(0.709600445983969,1.,1.00289807040992),
(0.383340713915941,0.383933227114987,0.401145492974693),.UNSPECIFIED.)
GEOMETRIC_REPRESENTATION_ITEM()
RATIONAL_B_SPLINE_SURFACE(((0.988246641953811,0.988246641953811,0.988246641953811,
0.986737013496293,0.988139125479962),(0.988246641953811,0.988246641953811,
0.988246641953811,0.986737013496293,0.988139125479962),(0.988246641953811,
0.988246641953811,0.988246641953811,0.986737013496293,0.988139125479962)))
REPRESENTATION_ITEM('')
SURFACE()
);
#806=(
BOUNDED_SURFACE()
B_SPLINE_SURFACE(1,2,((#107248,#107249,#107250),(#107251,#107252,#107253)),
 .UNSPECIFIED.,.F.,.F.,.F.)
B_SPLINE_SURFACE_WITH_KNOTS((2,2),(3,3),(0.710318915640075,1.),(0.331965345783649,
0.349369696259361),.UNSPECIFIED.)
GEOMETRIC_REPRESENTATION_ITEM()
RATIONAL_B_SPLINE_SURFACE(((0.988555124858682,0.99035748704491,0.99513694090229),
(0.988555124858682,0.99035748704491,0.99513694090229)))
REPRESENTATION_ITEM('')
SURFACE()
);
#807=(
BOUNDED_SURFACE()
B_SPLINE_SURFACE(1,2,((#107255,#107256,#107257,#107258,#107259),(#107260,
#107261,#107262,#107263,#107264),(#107265,#107266,#107267,#107268,#107269)),
 .UNSPECIFIED.,.F.,.F.,.F.)
B_SPLINE_SURFACE_WITH_KNOTS((2,1,2),(3,2,3),(0.70960044599214,1.,1.00289807040992),
(0.383340713924216,0.383933227114986,0.401145492974693),.UNSPECIFIED.)
GEOMETRIC_REPRESENTATION_ITEM()
RATIONAL_B_SPLINE_SURFACE(((0.988246641953811,0.988246641953811,0.988246641953811,
0.986737013496293,0.988139125479961),(0.988246641953811,0.988246641953811,
0.988246641953811,0.986737013496293,0.988139125479961),(0.988246641953811,
0.988246641953811,0.988246641953811,0.986737013496293,0.988139125479961)))
REPRESENTATION_ITEM('')
SURFACE()
);
#808=(
BOUNDED_SURFACE()
B_SPLINE_SURFACE(1,2,((#107278,#107279,#107280),(#107281,#107282,#107283)),
 .UNSPECIFIED.,.F.,.F.,.F.)
B_SPLINE_SURFACE_WITH_KNOTS((2,2),(3,3),(0.710318915639971,1.),(0.331965345783649,
0.349369696259361),.UNSPECIFIED.)
GEOMETRIC_REPRESENTATION_ITEM()
RATIONAL_B_SPLINE_SURFACE(((0.988555124858682,0.99035748704491,0.99513694090229),
(0.988555124858682,0.99035748704491,0.99513694090229)))
REPRESENTATION_ITEM('')
SURFACE()
);
#809=(
BOUNDED_SURFACE()
B_SPLINE_SURFACE(1,2,((#107285,#107286,#107287,#107288,#107289),(#107290,
#107291,#107292,#107293,#107294),(#107295,#107296,#107297,#107298,#107299)),
 .UNSPECIFIED.,.F.,.F.,.F.)
B_SPLINE_SURFACE_WITH_KNOTS((2,1,2),(3,2,3),(0.709600445959392,1.,1.00289807040993),
(0.38334071389278,0.383933227114987,0.401145492974693),.UNSPECIFIED.)
GEOMETRIC_REPRESENTATION_ITEM()
RATIONAL_B_SPLINE_SURFACE(((0.988246641953811,0.988246641953811,0.988246641953811,
0.986737013496293,0.988139125479962),(0.988246641953811,0.988246641953811,
0.988246641953811,0.986737013496293,0.988139125479962),(0.988246641953811,
0.988246641953811,0.988246641953811,0.986737013496293,0.988139125479962)))
REPRESENTATION_ITEM('')
SURFACE()
);
#810=(
BOUNDED_SURFACE()
B_SPLINE_SURFACE(1,2,((#107308,#107309,#107310),(#107311,#107312,#107313)),
 .UNSPECIFIED.,.F.,.F.,.F.)
B_SPLINE_SURFACE_WITH_KNOTS((2,2),(3,3),(0.710318915638668,1.),(0.331965345783647,
0.349369696259361),.UNSPECIFIED.)
GEOMETRIC_REPRESENTATION_ITEM()
RATIONAL_B_SPLINE_SURFACE(((0.988555124858681,0.99035748704491,0.99513694090229),
(0.988555124858681,0.99035748704491,0.99513694090229)))
REPRESENTATION_ITEM('')
SURFACE()
);
#811=(
BOUNDED_SURFACE()
B_SPLINE_SURFACE(1,2,((#107315,#107316,#107317,#107318,#107319),(#107320,
#107321,#107322,#107323,#107324),(#107325,#107326,#107327,#107328,#107329)),
 .UNSPECIFIED.,.F.,.F.,.F.)
B_SPLINE_SURFACE_WITH_KNOTS((2,1,2),(3,2,3),(0.70960044598379,1.,1.00289807040992),
(0.383340713916011,0.383933227114987,0.401145492974693),.UNSPECIFIED.)
GEOMETRIC_REPRESENTATION_ITEM()
RATIONAL_B_SPLINE_SURFACE(((0.988246641953811,0.988246641953811,0.988246641953811,
0.986737013496293,0.988139125479961),(0.988246641953811,0.988246641953811,
0.988246641953811,0.986737013496293,0.988139125479962),(0.988246641953811,
0.988246641953811,0.988246641953811,0.986737013496293,0.988139125479962)))
REPRESENTATION_ITEM('')
SURFACE()
);
#812=(
BOUNDED_SURFACE()
B_SPLINE_SURFACE(1,2,((#107338,#107339,#107340),(#107341,#107342,#107343)),
 .UNSPECIFIED.,.F.,.F.,.F.)
B_SPLINE_SURFACE_WITH_KNOTS((2,2),(3,3),(0.710318915639827,1.),(0.331965345783647,
0.349369696259361),.UNSPECIFIED.)
GEOMETRIC_REPRESENTATION_ITEM()
RATIONAL_B_SPLINE_SURFACE(((0.988555124858681,0.99035748704491,0.99513694090229),
(0.988555124858681,0.99035748704491,0.99513694090229)))
REPRESENTATION_ITEM('')
SURFACE()
);
#813=(
BOUNDED_SURFACE()
B_SPLINE_SURFACE(1,2,((#107345,#107346,#107347,#107348,#107349),(#107350,
#107351,#107352,#107353,#107354),(#107355,#107356,#107357,#107358,#107359)),
 .UNSPECIFIED.,.F.,.F.,.F.)
B_SPLINE_SURFACE_WITH_KNOTS((2,1,2),(3,2,3),(0.709600445981835,1.,1.00289807040992),
(0.383340713913804,0.383933227114986,0.401145492974693),.UNSPECIFIED.)
GEOMETRIC_REPRESENTATION_ITEM()
RATIONAL_B_SPLINE_SURFACE(((0.988246641953811,0.988246641953811,0.988246641953811,
0.986737013496293,0.988139125479961),(0.988246641953811,0.988246641953811,
0.988246641953811,0.986737013496293,0.988139125479961),(0.988246641953811,
0.988246641953811,0.988246641953811,0.986737013496293,0.988139125479961)))
REPRESENTATION_ITEM('')
SURFACE()
);
#814=(
BOUNDED_SURFACE()
B_SPLINE_SURFACE(1,2,((#107368,#107369,#107370),(#107371,#107372,#107373)),
 .UNSPECIFIED.,.F.,.F.,.F.)
B_SPLINE_SURFACE_WITH_KNOTS((2,2),(3,3),(0.710318915640078,1.),(0.331965345783649,
0.349369696259361),.UNSPECIFIED.)
GEOMETRIC_REPRESENTATION_ITEM()
RATIONAL_B_SPLINE_SURFACE(((0.988555124858682,0.99035748704491,0.99513694090229),
(0.988555124858681,0.99035748704491,0.99513694090229)))
REPRESENTATION_ITEM('')
SURFACE()
);
#815=(
BOUNDED_SURFACE()
B_SPLINE_SURFACE(1,2,((#107375,#107376,#107377,#107378,#107379),(#107380,
#107381,#107382,#107383,#107384),(#107385,#107386,#107387,#107388,#107389)),
 .UNSPECIFIED.,.F.,.F.,.F.)
B_SPLINE_SURFACE_WITH_KNOTS((2,1,2),(3,2,3),(0.70960044599244,1.,1.00289807040992),
(0.383340713924407,0.383933227114987,0.401145492974693),.UNSPECIFIED.)
GEOMETRIC_REPRESENTATION_ITEM()
RATIONAL_B_SPLINE_SURFACE(((0.988246641953811,0.988246641953811,0.988246641953811,
0.986737013496293,0.988139125479962),(0.988246641953811,0.988246641953811,
0.988246641953811,0.986737013496293,0.988139125479962),(0.988246641953811,
0.988246641953811,0.988246641953811,0.986737013496293,0.988139125479962)))
REPRESENTATION_ITEM('')
SURFACE()
);
#816=(
BOUNDED_SURFACE()
B_SPLINE_SURFACE(1,2,((#107398,#107399,#107400),(#107401,#107402,#107403)),
 .UNSPECIFIED.,.F.,.F.,.F.)
B_SPLINE_SURFACE_WITH_KNOTS((2,2),(3,3),(0.71031891564008,1.),(0.331965345783647,
0.349369696259361),.UNSPECIFIED.)
GEOMETRIC_REPRESENTATION_ITEM()
RATIONAL_B_SPLINE_SURFACE(((0.988555124858681,0.99035748704491,0.99513694090229),
(0.988555124858681,0.99035748704491,0.99513694090229)))
REPRESENTATION_ITEM('')
SURFACE()
);
#817=(
BOUNDED_SURFACE()
B_SPLINE_SURFACE(1,2,((#107405,#107406,#107407,#107408,#107409),(#107410,
#107411,#107412,#107413,#107414),(#107415,#107416,#107417,#107418,#107419)),
 .UNSPECIFIED.,.F.,.F.,.F.)
B_SPLINE_SURFACE_WITH_KNOTS((2,1,2),(3,2,3),(0.709600445973141,1.,1.00289807040992),
(0.383340713905106,0.383933227114987,0.401145492974693),.UNSPECIFIED.)
GEOMETRIC_REPRESENTATION_ITEM()
RATIONAL_B_SPLINE_SURFACE(((0.988246641953811,0.988246641953811,0.988246641953811,
0.986737013496293,0.988139125479961),(0.988246641953811,0.988246641953811,
0.988246641953811,0.986737013496293,0.988139125479961),(0.988246641953811,
0.988246641953811,0.988246641953811,0.986737013496293,0.988139125479961)))
REPRESENTATION_ITEM('')
SURFACE()
);
#818=(
BOUNDED_SURFACE()
B_SPLINE_SURFACE(1,2,((#107428,#107429,#107430),(#107431,#107432,#107433)),
 .UNSPECIFIED.,.F.,.F.,.F.)
B_SPLINE_SURFACE_WITH_KNOTS((2,2),(3,3),(0.710318915640081,1.),(0.331965345783647,
0.349369696259361),.UNSPECIFIED.)
GEOMETRIC_REPRESENTATION_ITEM()
RATIONAL_B_SPLINE_SURFACE(((0.988555124858681,0.99035748704491,0.99513694090229),
(0.988555124858681,0.99035748704491,0.99513694090229)))
REPRESENTATION_ITEM('')
SURFACE()
);
#819=(
BOUNDED_SURFACE()
B_SPLINE_SURFACE(1,2,((#107435,#107436,#107437,#107438,#107439),(#107440,
#107441,#107442,#107443,#107444),(#107445,#107446,#107447,#107448,#107449)),
 .UNSPECIFIED.,.F.,.F.,.F.)
B_SPLINE_SURFACE_WITH_KNOTS((2,1,2),(3,2,3),(0.709600445966216,1.,1.00289807040992),
(0.383340713898184,0.383933227114987,0.401145492974693),.UNSPECIFIED.)
GEOMETRIC_REPRESENTATION_ITEM()
RATIONAL_B_SPLINE_SURFACE(((0.988246641953811,0.988246641953811,0.988246641953811,
0.986737013496293,0.988139125479962),(0.988246641953811,0.988246641953811,
0.988246641953811,0.986737013496293,0.988139125479962),(0.988246641953811,
0.988246641953811,0.988246641953811,0.986737013496293,0.988139125479962)))
REPRESENTATION_ITEM('')
SURFACE()
);
#820=(
BOUNDED_SURFACE()
B_SPLINE_SURFACE(1,2,((#107458,#107459,#107460),(#107461,#107462,#107463)),
 .UNSPECIFIED.,.F.,.F.,.F.)
B_SPLINE_SURFACE_WITH_KNOTS((2,2),(3,3),(0.710318915640083,1.),(0.331965345783647,
0.349369696259361),.UNSPECIFIED.)
GEOMETRIC_REPRESENTATION_ITEM()
RATIONAL_B_SPLINE_SURFACE(((0.988555124858681,0.99035748704491,0.99513694090229),
(0.988555124858681,0.99035748704491,0.99513694090229)))
REPRESENTATION_ITEM('')
SURFACE()
);
#821=(
BOUNDED_SURFACE()
B_SPLINE_SURFACE(1,2,((#107465,#107466,#107467,#107468,#107469),(#107470,
#107471,#107472,#107473,#107474),(#107475,#107476,#107477,#107478,#107479)),
 .UNSPECIFIED.,.F.,.F.,.F.)
B_SPLINE_SURFACE_WITH_KNOTS((2,1,2),(3,2,3),(0.70960044597391,1.,1.00289807040992),
(0.383340713905879,0.383933227114987,0.401145492974693),.UNSPECIFIED.)
GEOMETRIC_REPRESENTATION_ITEM()
RATIONAL_B_SPLINE_SURFACE(((0.988246641953811,0.988246641953811,0.988246641953811,
0.986737013496293,0.988139125479962),(0.988246641953811,0.988246641953811,
0.988246641953811,0.986737013496293,0.988139125479962),(0.988246641953811,
0.988246641953811,0.988246641953811,0.986737013496293,0.988139125479962)))
REPRESENTATION_ITEM('')
SURFACE()
);
#822=(
BOUNDED_SURFACE()
B_SPLINE_SURFACE(1,2,((#107488,#107489,#107490),(#107491,#107492,#107493)),
 .UNSPECIFIED.,.F.,.F.,.F.)
B_SPLINE_SURFACE_WITH_KNOTS((2,2),(3,3),(0.710318915640079,1.),(0.331965345783649,
0.349369696259361),.UNSPECIFIED.)
GEOMETRIC_REPRESENTATION_ITEM()
RATIONAL_B_SPLINE_SURFACE(((0.988555124858681,0.99035748704491,0.99513694090229),
(0.988555124858681,0.99035748704491,0.99513694090229)))
REPRESENTATION_ITEM('')
SURFACE()
);
#823=(
BOUNDED_SURFACE()
B_SPLINE_SURFACE(1,2,((#107495,#107496,#107497,#107498,#107499),(#107500,
#107501,#107502,#107503,#107504),(#107505,#107506,#107507,#107508,#107509)),
 .UNSPECIFIED.,.F.,.F.,.F.)
B_SPLINE_SURFACE_WITH_KNOTS((2,1,2),(3,2,3),(0.709600445962162,1.,1.00289807040992),
(0.383340713894442,0.383933227114983,0.401145492974692),.UNSPECIFIED.)
GEOMETRIC_REPRESENTATION_ITEM()
RATIONAL_B_SPLINE_SURFACE(((0.988246641953811,0.988246641953811,0.988246641953811,
0.986737013496293,0.988139125479961),(0.988246641953811,0.988246641953811,
0.988246641953811,0.986737013496293,0.988139125479961),(0.988246641953811,
0.988246641953811,0.988246641953811,0.986737013496293,0.988139125479961)))
REPRESENTATION_ITEM('')
SURFACE()
);
#824=(
BOUNDED_SURFACE()
B_SPLINE_SURFACE(1,2,((#107518,#107519,#107520),(#107521,#107522,#107523)),
 .UNSPECIFIED.,.F.,.F.,.F.)
B_SPLINE_SURFACE_WITH_KNOTS((2,2),(3,3),(0.710318915639765,1.),(0.331965345783648,
0.349369696259362),.UNSPECIFIED.)
GEOMETRIC_REPRESENTATION_ITEM()
RATIONAL_B_SPLINE_SURFACE(((0.988555124858681,0.99035748704491,0.99513694090229),
(0.988555124858681,0.99035748704491,0.995136940902291)))
REPRESENTATION_ITEM('')
SURFACE()
);
#825=(
BOUNDED_SURFACE()
B_SPLINE_SURFACE(1,2,((#107525,#107526,#107527,#107528,#107529),(#107530,
#107531,#107532,#107533,#107534),(#107535,#107536,#107537,#107538,#107539)),
 .UNSPECIFIED.,.F.,.F.,.F.)
B_SPLINE_SURFACE_WITH_KNOTS((2,1,2),(3,2,3),(0.709600445962641,1.,1.00289807040992),
(0.383340713894891,0.383933227114985,0.401145492974692),.UNSPECIFIED.)
GEOMETRIC_REPRESENTATION_ITEM()
RATIONAL_B_SPLINE_SURFACE(((0.988246641953811,0.988246641953811,0.988246641953811,
0.986737013496293,0.988139125479961),(0.988246641953811,0.988246641953811,
0.988246641953811,0.986737013496293,0.988139125479961),(0.988246641953811,
0.988246641953811,0.988246641953811,0.986737013496293,0.988139125479961)))
REPRESENTATION_ITEM('')
SURFACE()
);
#826=(
BOUNDED_SURFACE()
B_SPLINE_SURFACE(1,2,((#107548,#107549,#107550),(#107551,#107552,#107553)),
 .UNSPECIFIED.,.F.,.F.,.F.)
B_SPLINE_SURFACE_WITH_KNOTS((2,2),(3,3),(0.7103189156398,1.),(0.331965345783649,
0.349369696259361),.UNSPECIFIED.)
GEOMETRIC_REPRESENTATION_ITEM()
RATIONAL_B_SPLINE_SURFACE(((0.988555124858681,0.99035748704491,0.99513694090229),
(0.988555124858682,0.990357487044911,0.99513694090229)))
REPRESENTATION_ITEM('')
SURFACE()
);
#827=(
BOUNDED_SURFACE()
B_SPLINE_SURFACE(1,2,((#107555,#107556,#107557,#107558,#107559),(#107560,
#107561,#107562,#107563,#107564),(#107565,#107566,#107567,#107568,#107569)),
 .UNSPECIFIED.,.F.,.F.,.F.)
B_SPLINE_SURFACE_WITH_KNOTS((2,1,2),(3,2,3),(0.709600445972273,1.,1.00289807040992),
(0.383340713904703,0.383933227114987,0.401145492974693),.UNSPECIFIED.)
GEOMETRIC_REPRESENTATION_ITEM()
RATIONAL_B_SPLINE_SURFACE(((0.988246641953811,0.988246641953811,0.988246641953811,
0.986737013496293,0.988139125479962),(0.988246641953811,0.988246641953811,
0.988246641953811,0.986737013496293,0.988139125479962),(0.988246641953811,
0.988246641953811,0.988246641953811,0.986737013496293,0.988139125479962)))
REPRESENTATION_ITEM('')
SURFACE()
);
#828=(
BOUNDED_SURFACE()
B_SPLINE_SURFACE(1,2,((#107578,#107579,#107580),(#107581,#107582,#107583)),
 .UNSPECIFIED.,.F.,.F.,.F.)
B_SPLINE_SURFACE_WITH_KNOTS((2,2),(3,3),(0.710318915639619,1.),(0.331965345783649,
0.349369696259361),.UNSPECIFIED.)
GEOMETRIC_REPRESENTATION_ITEM()
RATIONAL_B_SPLINE_SURFACE(((0.988555124858681,0.99035748704491,0.99513694090229),
(0.988555124858681,0.99035748704491,0.99513694090229)))
REPRESENTATION_ITEM('')
SURFACE()
);
#829=(
BOUNDED_SURFACE()
B_SPLINE_SURFACE(1,2,((#107585,#107586,#107587,#107588,#107589),(#107590,
#107591,#107592,#107593,#107594),(#107595,#107596,#107597,#107598,#107599)),
 .UNSPECIFIED.,.F.,.F.,.F.)
B_SPLINE_SURFACE_WITH_KNOTS((2,1,2),(3,2,3),(0.709600445979013,1.,1.00289807040992),
(0.383340713911408,0.383933227114987,0.401145492974693),.UNSPECIFIED.)
GEOMETRIC_REPRESENTATION_ITEM()
RATIONAL_B_SPLINE_SURFACE(((0.988246641953811,0.988246641953811,0.988246641953811,
0.986737013496293,0.988139125479962),(0.988246641953811,0.988246641953811,
0.988246641953811,0.986737013496293,0.988139125479962),(0.988246641953811,
0.988246641953811,0.988246641953811,0.986737013496293,0.988139125479962)))
REPRESENTATION_ITEM('')
SURFACE()
);
#830=(
BOUNDED_SURFACE()
B_SPLINE_SURFACE(1,2,((#107608,#107609,#107610),(#107611,#107612,#107613)),
 .UNSPECIFIED.,.F.,.F.,.F.)
B_SPLINE_SURFACE_WITH_KNOTS((2,2),(3,3),(0.71031891563966,1.),(0.331965345783649,
0.349369696259361),.UNSPECIFIED.)
GEOMETRIC_REPRESENTATION_ITEM()
RATIONAL_B_SPLINE_SURFACE(((0.988555124858681,0.99035748704491,0.99513694090229),
(0.988555124858681,0.99035748704491,0.99513694090229)))
REPRESENTATION_ITEM('')
SURFACE()
);
#831=(
BOUNDED_SURFACE()
B_SPLINE_SURFACE(1,2,((#107615,#107616,#107617,#107618,#107619),(#107620,
#107621,#107622,#107623,#107624),(#107625,#107626,#107627,#107628,#107629)),
 .UNSPECIFIED.,.F.,.F.,.F.)
B_SPLINE_SURFACE_WITH_KNOTS((2,1,2),(3,2,3),(0.709600445963461,1.,1.00289807040992),
(0.383340713895831,0.383933227114987,0.401145492974693),.UNSPECIFIED.)
GEOMETRIC_REPRESENTATION_ITEM()
RATIONAL_B_SPLINE_SURFACE(((0.988246641953811,0.988246641953811,0.988246641953811,
0.986737013496293,0.988139125479962),(0.988246641953811,0.988246641953811,
0.988246641953811,0.986737013496293,0.988139125479962),(0.988246641953811,
0.988246641953811,0.988246641953811,0.986737013496293,0.988139125479962)))
REPRESENTATION_ITEM('')
SURFACE()
);
#832=(
BOUNDED_SURFACE()
B_SPLINE_SURFACE(1,2,((#107631,#107632,#107633),(#107634,#107635,#107636)),
 .UNSPECIFIED.,.F.,.F.,.F.)
B_SPLINE_SURFACE_WITH_KNOTS((2,2),(3,3),(0.,0.289807040992854),(0.435775021682558,
0.453027768259469),.UNSPECIFIED.)
GEOMETRIC_REPRESENTATION_ITEM()
RATIONAL_B_SPLINE_SURFACE(((0.995452950231099,0.990618550266721,0.988709602819327),
(0.995452950231099,0.990618550266721,0.988709602819327)))
REPRESENTATION_ITEM('')
SURFACE()
);
#833=(
BOUNDED_SURFACE()
B_SPLINE_SURFACE(1,2,((#107645,#107646,#107647,#107648,#107649),(#107650,
#107651,#107652,#107653,#107654)),.UNSPECIFIED.,.F.,.F.,.F.)
B_SPLINE_SURFACE_WITH_KNOTS((2,2),(3,2,3),(0.,0.289681084360052),(0.280328542633766,
0.285714285714286,0.297856505190614),.UNSPECIFIED.)
GEOMETRIC_REPRESENTATION_ITEM()
RATIONAL_B_SPLINE_SURFACE(((0.996504189652447,0.998109554471267,1.,0.995737968897747,
0.992924952273132),(0.996504189652447,0.998109554471267,1.,0.995737968897747,
0.992924952273132)))
REPRESENTATION_ITEM('')
SURFACE()
);
#834=(
BOUNDED_SURFACE()
B_SPLINE_SURFACE(1,2,((#107672,#107673,#107674),(#107675,#107676,#107677)),
 .UNSPECIFIED.,.F.,.F.,.F.)
B_SPLINE_SURFACE_WITH_KNOTS((2,2),(3,3),(0.,0.289807040991561),(0.435775021682621,
0.453027768259468),.UNSPECIFIED.)
GEOMETRIC_REPRESENTATION_ITEM()
RATIONAL_B_SPLINE_SURFACE(((0.995452950231064,0.990618550266715,0.988709602819327),
(0.995452950231064,0.990618550266715,0.988709602819327)))
REPRESENTATION_ITEM('')
SURFACE()
);
#835=(
BOUNDED_SURFACE()
B_SPLINE_SURFACE(1,2,((#107679,#107680,#107681,#107682,#107683),(#107684,
#107685,#107686,#107687,#107688)),.UNSPECIFIED.,.F.,.F.,.F.)
B_SPLINE_SURFACE_WITH_KNOTS((2,2),(3,2,3),(0.,0.289681084359918),(0.280328542633766,
0.285714285714286,0.297856505190615),.UNSPECIFIED.)
GEOMETRIC_REPRESENTATION_ITEM()
RATIONAL_B_SPLINE_SURFACE(((0.996504189652447,0.998109554471267,1.,0.995737968897747,
0.992924952273131),(0.996504189652447,0.998109554471267,1.,0.995737968897747,
0.992924952273131)))
REPRESENTATION_ITEM('')
SURFACE()
);
#836=(
BOUNDED_SURFACE()
B_SPLINE_SURFACE(1,2,((#107706,#107707,#107708),(#107709,#107710,#107711)),
 .UNSPECIFIED.,.F.,.F.,.F.)
B_SPLINE_SURFACE_WITH_KNOTS((2,2),(3,3),(0.,0.289807040991557),(0.435775021682621,
0.453027768259468),.UNSPECIFIED.)
GEOMETRIC_REPRESENTATION_ITEM()
RATIONAL_B_SPLINE_SURFACE(((0.995452950231064,0.990618550266715,0.988709602819327),
(0.995452950231064,0.990618550266715,0.988709602819327)))
REPRESENTATION_ITEM('')
SURFACE()
);
#837=(
BOUNDED_SURFACE()
B_SPLINE_SURFACE(1,2,((#107713,#107714,#107715,#107716,#107717),(#107718,
#107719,#107720,#107721,#107722)),.UNSPECIFIED.,.F.,.F.,.F.)
B_SPLINE_SURFACE_WITH_KNOTS((2,2),(3,2,3),(0.,0.289681084360338),(0.280328542633766,
0.285714285714286,0.297856505190615),.UNSPECIFIED.)
GEOMETRIC_REPRESENTATION_ITEM()
RATIONAL_B_SPLINE_SURFACE(((0.996504189652447,0.998109554471267,1.,0.995737968897747,
0.992924952273132),(0.996504189652447,0.998109554471267,1.,0.995737968897747,
0.992924952273132)))
REPRESENTATION_ITEM('')
SURFACE()
);
#838=(
BOUNDED_SURFACE()
B_SPLINE_SURFACE(1,2,((#107740,#107741,#107742),(#107743,#107744,#107745)),
 .UNSPECIFIED.,.F.,.F.,.F.)
B_SPLINE_SURFACE_WITH_KNOTS((2,2),(3,3),(0.,0.28980704099156),(0.435775021682621,
0.453027768259468),.UNSPECIFIED.)
GEOMETRIC_REPRESENTATION_ITEM()
RATIONAL_B_SPLINE_SURFACE(((0.995452950231064,0.990618550266715,0.988709602819327),
(0.995452950231064,0.990618550266715,0.988709602819327)))
REPRESENTATION_ITEM('')
SURFACE()
);
#839=(
BOUNDED_SURFACE()
B_SPLINE_SURFACE(1,2,((#107747,#107748,#107749,#107750,#107751),(#107752,
#107753,#107754,#107755,#107756)),.UNSPECIFIED.,.F.,.F.,.F.)
B_SPLINE_SURFACE_WITH_KNOTS((2,2),(3,2,3),(0.,0.289681084359927),(0.280328542633766,
0.285714285714286,0.297856505190615),.UNSPECIFIED.)
GEOMETRIC_REPRESENTATION_ITEM()
RATIONAL_B_SPLINE_SURFACE(((0.996504189652447,0.998109554471267,1.,0.995737968897747,
0.992924952273131),(0.996504189652447,0.998109554471267,1.,0.995737968897747,
0.992924952273131)))
REPRESENTATION_ITEM('')
SURFACE()
);
#840=(
BOUNDED_SURFACE()
B_SPLINE_SURFACE(1,2,((#107774,#107775,#107776),(#107777,#107778,#107779)),
 .UNSPECIFIED.,.F.,.F.,.F.)
B_SPLINE_SURFACE_WITH_KNOTS((2,2),(3,3),(0.,0.289807040991564),(0.435775021682621,
0.453027768259468),.UNSPECIFIED.)
GEOMETRIC_REPRESENTATION_ITEM()
RATIONAL_B_SPLINE_SURFACE(((0.995452950231064,0.990618550266715,0.988709602819327),
(0.995452950231064,0.990618550266715,0.988709602819327)))
REPRESENTATION_ITEM('')
SURFACE()
);
#841=(
BOUNDED_SURFACE()
B_SPLINE_SURFACE(1,2,((#107781,#107782,#107783,#107784,#107785),(#107786,
#107787,#107788,#107789,#107790)),.UNSPECIFIED.,.F.,.F.,.F.)
B_SPLINE_SURFACE_WITH_KNOTS((2,2),(3,2,3),(0.,0.289681084359916),(0.280328542633766,
0.285714285714286,0.297856505190615),.UNSPECIFIED.)
GEOMETRIC_REPRESENTATION_ITEM()
RATIONAL_B_SPLINE_SURFACE(((0.996504189652447,0.998109554471267,1.,0.995737968897747,
0.992924952273131),(0.996504189652447,0.998109554471267,1.,0.995737968897747,
0.992924952273131)))
REPRESENTATION_ITEM('')
SURFACE()
);
#842=(
BOUNDED_SURFACE()
B_SPLINE_SURFACE(1,2,((#107808,#107809,#107810),(#107811,#107812,#107813)),
 .UNSPECIFIED.,.F.,.F.,.F.)
B_SPLINE_SURFACE_WITH_KNOTS((2,2),(3,3),(0.,0.289807040991642),(0.435775021682622,
0.453027768259468),.UNSPECIFIED.)
GEOMETRIC_REPRESENTATION_ITEM()
RATIONAL_B_SPLINE_SURFACE(((0.995452950231063,0.990618550266715,0.988709602819327),
(0.995452950231063,0.990618550266715,0.988709602819327)))
REPRESENTATION_ITEM('')
SURFACE()
);
#843=(
BOUNDED_SURFACE()
B_SPLINE_SURFACE(1,2,((#107815,#107816,#107817,#107818,#107819),(#107820,
#107821,#107822,#107823,#107824)),.UNSPECIFIED.,.F.,.F.,.F.)
B_SPLINE_SURFACE_WITH_KNOTS((2,2),(3,2,3),(0.,0.28968108436033),(0.280328542633765,
0.285714285714286,0.297856505190614),.UNSPECIFIED.)
GEOMETRIC_REPRESENTATION_ITEM()
RATIONAL_B_SPLINE_SURFACE(((0.996504189652447,0.998109554471267,1.,0.995737968897747,
0.992924952273132),(0.996504189652447,0.998109554471267,1.,0.995737968897747,
0.992924952273132)))
REPRESENTATION_ITEM('')
SURFACE()
);
#844=(
BOUNDED_SURFACE()
B_SPLINE_SURFACE(1,2,((#107842,#107843,#107844),(#107845,#107846,#107847)),
 .UNSPECIFIED.,.F.,.F.,.F.)
B_SPLINE_SURFACE_WITH_KNOTS((2,2),(3,3),(0.,0.289807040991638),(0.435775021682622,
0.453027768259469),.UNSPECIFIED.)
GEOMETRIC_REPRESENTATION_ITEM()
RATIONAL_B_SPLINE_SURFACE(((0.995452950231063,0.990618550266714,0.988709602819327),
(0.995452950231063,0.990618550266714,0.988709602819327)))
REPRESENTATION_ITEM('')
SURFACE()
);
#845=(
BOUNDED_SURFACE()
B_SPLINE_SURFACE(1,2,((#107849,#107850,#107851,#107852,#107853),(#107854,
#107855,#107856,#107857,#107858)),.UNSPECIFIED.,.F.,.F.,.F.)
B_SPLINE_SURFACE_WITH_KNOTS((2,2),(3,2,3),(0.,0.289681084359919),(0.280328542633765,
0.285714285714286,0.297856505190614),.UNSPECIFIED.)
GEOMETRIC_REPRESENTATION_ITEM()
RATIONAL_B_SPLINE_SURFACE(((0.996504189652447,0.998109554471267,1.,0.995737968897747,
0.992924952273132),(0.996504189652447,0.998109554471267,1.,0.995737968897747,
0.992924952273132)))
REPRESENTATION_ITEM('')
SURFACE()
);
#846=(
BOUNDED_SURFACE()
B_SPLINE_SURFACE(1,2,((#107876,#107877,#107878),(#107879,#107880,#107881)),
 .UNSPECIFIED.,.F.,.F.,.F.)
B_SPLINE_SURFACE_WITH_KNOTS((2,2),(3,3),(0.,0.28980704099164),(0.435775021682622,
0.453027768259469),.UNSPECIFIED.)
GEOMETRIC_REPRESENTATION_ITEM()
RATIONAL_B_SPLINE_SURFACE(((0.995452950231063,0.990618550266714,0.988709602819327),
(0.995452950231063,0.990618550266714,0.988709602819327)))
REPRESENTATION_ITEM('')
SURFACE()
);
#847=(
BOUNDED_SURFACE()
B_SPLINE_SURFACE(1,2,((#107883,#107884,#107885,#107886,#107887),(#107888,
#107889,#107890,#107891,#107892)),.UNSPECIFIED.,.F.,.F.,.F.)
B_SPLINE_SURFACE_WITH_KNOTS((2,2),(3,2,3),(0.,0.289681084359922),(0.280328542633765,
0.285714285714286,0.297856505190614),.UNSPECIFIED.)
GEOMETRIC_REPRESENTATION_ITEM()
RATIONAL_B_SPLINE_SURFACE(((0.996504189652447,0.998109554471267,1.,0.995737968897747,
0.992924952273132),(0.996504189652447,0.998109554471267,1.,0.995737968897747,
0.992924952273132)))
REPRESENTATION_ITEM('')
SURFACE()
);
#848=(
BOUNDED_SURFACE()
B_SPLINE_SURFACE(1,2,((#107910,#107911,#107912),(#107913,#107914,#107915)),
 .UNSPECIFIED.,.F.,.F.,.F.)
B_SPLINE_SURFACE_WITH_KNOTS((2,2),(3,3),(0.,0.289807040991643),(0.435775021682622,
0.453027768259469),.UNSPECIFIED.)
GEOMETRIC_REPRESENTATION_ITEM()
RATIONAL_B_SPLINE_SURFACE(((0.995452950231063,0.990618550266714,0.988709602819327),
(0.995452950231063,0.990618550266714,0.988709602819327)))
REPRESENTATION_ITEM('')
SURFACE()
);
#849=(
BOUNDED_SURFACE()
B_SPLINE_SURFACE(1,2,((#107917,#107918,#107919,#107920,#107921),(#107922,
#107923,#107924,#107925,#107926)),.UNSPECIFIED.,.F.,.F.,.F.)
B_SPLINE_SURFACE_WITH_KNOTS((2,2),(3,2,3),(0.,0.289681084360311),(0.280328542633765,
0.285714285714286,0.297856505190614),.UNSPECIFIED.)
GEOMETRIC_REPRESENTATION_ITEM()
RATIONAL_B_SPLINE_SURFACE(((0.996504189652447,0.998109554471267,1.,0.995737968897747,
0.992924952273132),(0.996504189652447,0.998109554471267,1.,0.995737968897747,
0.992924952273132)))
REPRESENTATION_ITEM('')
SURFACE()
);
#850=(
BOUNDED_SURFACE()
B_SPLINE_SURFACE(1,2,((#107944,#107945,#107946),(#107947,#107948,#107949)),
 .UNSPECIFIED.,.F.,.F.,.F.)
B_SPLINE_SURFACE_WITH_KNOTS((2,2),(3,3),(0.,0.289807040991563),(0.435775021682622,
0.453027768259469),.UNSPECIFIED.)
GEOMETRIC_REPRESENTATION_ITEM()
RATIONAL_B_SPLINE_SURFACE(((0.995452950231063,0.990618550266714,0.988709602819327),
(0.995452950231063,0.990618550266714,0.988709602819327)))
REPRESENTATION_ITEM('')
SURFACE()
);
#851=(
BOUNDED_SURFACE()
B_SPLINE_SURFACE(1,2,((#107951,#107952,#107953,#107954,#107955),(#107956,
#107957,#107958,#107959,#107960)),.UNSPECIFIED.,.F.,.F.,.F.)
B_SPLINE_SURFACE_WITH_KNOTS((2,2),(3,2,3),(0.,0.289681084359919),(0.280328542633765,
0.285714285714286,0.297856505190614),.UNSPECIFIED.)
GEOMETRIC_REPRESENTATION_ITEM()
RATIONAL_B_SPLINE_SURFACE(((0.996504189652447,0.998109554471267,1.,0.995737968897747,
0.992924952273132),(0.996504189652447,0.998109554471267,1.,0.995737968897747,
0.992924952273132)))
REPRESENTATION_ITEM('')
SURFACE()
);
#852=(
BOUNDED_SURFACE()
B_SPLINE_SURFACE(1,2,((#107978,#107979,#107980),(#107981,#107982,#107983)),
 .UNSPECIFIED.,.F.,.F.,.F.)
B_SPLINE_SURFACE_WITH_KNOTS((2,2),(3,3),(0.,0.289807040991651),(0.435775021682622,
0.453027768259469),.UNSPECIFIED.)
GEOMETRIC_REPRESENTATION_ITEM()
RATIONAL_B_SPLINE_SURFACE(((0.995452950231063,0.990618550266714,0.988709602819327),
(0.995452950231063,0.990618550266714,0.988709602819327)))
REPRESENTATION_ITEM('')
SURFACE()
);
#853=(
BOUNDED_SURFACE()
B_SPLINE_SURFACE(1,2,((#107985,#107986,#107987,#107988,#107989),(#107990,
#107991,#107992,#107993,#107994)),.UNSPECIFIED.,.F.,.F.,.F.)
B_SPLINE_SURFACE_WITH_KNOTS((2,2),(3,2,3),(0.,0.289681084359921),(0.280328542633765,
0.285714285714286,0.297856505190614),.UNSPECIFIED.)
GEOMETRIC_REPRESENTATION_ITEM()
RATIONAL_B_SPLINE_SURFACE(((0.996504189652447,0.998109554471267,1.,0.995737968897747,
0.992924952273132),(0.996504189652447,0.998109554471267,1.,0.995737968897747,
0.992924952273132)))
REPRESENTATION_ITEM('')
SURFACE()
);
#854=(
BOUNDED_SURFACE()
B_SPLINE_SURFACE(1,2,((#108012,#108013,#108014),(#108015,#108016,#108017)),
 .UNSPECIFIED.,.F.,.F.,.F.)
B_SPLINE_SURFACE_WITH_KNOTS((2,2),(3,3),(0.,0.28980704099156),(0.435775021682622,
0.453027768259469),.UNSPECIFIED.)
GEOMETRIC_REPRESENTATION_ITEM()
RATIONAL_B_SPLINE_SURFACE(((0.995452950231063,0.990618550266714,0.988709602819327),
(0.995452950231063,0.990618550266714,0.988709602819327)))
REPRESENTATION_ITEM('')
SURFACE()
);
#855=(
BOUNDED_SURFACE()
B_SPLINE_SURFACE(1,2,((#108019,#108020,#108021,#108022,#108023),(#108024,
#108025,#108026,#108027,#108028)),.UNSPECIFIED.,.F.,.F.,.F.)
B_SPLINE_SURFACE_WITH_KNOTS((2,2),(3,2,3),(0.,0.289681084360324),(0.280328542633765,
0.285714285714286,0.297856505190614),.UNSPECIFIED.)
GEOMETRIC_REPRESENTATION_ITEM()
RATIONAL_B_SPLINE_SURFACE(((0.996504189652447,0.998109554471267,1.,0.995737968897747,
0.992924952273132),(0.996504189652447,0.998109554471267,1.,0.995737968897747,
0.992924952273132)))
REPRESENTATION_ITEM('')
SURFACE()
);
#856=(
BOUNDED_SURFACE()
B_SPLINE_SURFACE(1,2,((#108046,#108047,#108048),(#108049,#108050,#108051)),
 .UNSPECIFIED.,.F.,.F.,.F.)
B_SPLINE_SURFACE_WITH_KNOTS((2,2),(3,3),(0.,0.289807040991919),(0.435775021682622,
0.453027768259469),.UNSPECIFIED.)
GEOMETRIC_REPRESENTATION_ITEM()
RATIONAL_B_SPLINE_SURFACE(((0.995452950231063,0.990618550266714,0.988709602819327),
(0.995452950231063,0.990618550266714,0.988709602819327)))
REPRESENTATION_ITEM('')
SURFACE()
);
#857=(
BOUNDED_SURFACE()
B_SPLINE_SURFACE(1,2,((#108053,#108054,#108055,#108056,#108057),(#108058,
#108059,#108060,#108061,#108062)),.UNSPECIFIED.,.F.,.F.,.F.)
B_SPLINE_SURFACE_WITH_KNOTS((2,2),(3,2,3),(0.,0.289681084359923),(0.280328542633765,
0.285714285714286,0.297856505190614),.UNSPECIFIED.)
GEOMETRIC_REPRESENTATION_ITEM()
RATIONAL_B_SPLINE_SURFACE(((0.996504189652447,0.998109554471267,1.,0.995737968897747,
0.992924952273132),(0.996504189652447,0.998109554471267,1.,0.995737968897747,
0.992924952273132)))
REPRESENTATION_ITEM('')
SURFACE()
);
#858=(
BOUNDED_SURFACE()
B_SPLINE_SURFACE(1,2,((#108080,#108081,#108082),(#108083,#108084,#108085)),
 .UNSPECIFIED.,.F.,.F.,.F.)
B_SPLINE_SURFACE_WITH_KNOTS((2,2),(3,3),(0.,0.289807040992968),(0.435775021682622,
0.453027768259469),.UNSPECIFIED.)
GEOMETRIC_REPRESENTATION_ITEM()
RATIONAL_B_SPLINE_SURFACE(((0.995452950231063,0.990618550266714,0.988709602819327),
(0.995452950231063,0.990618550266714,0.988709602819327)))
REPRESENTATION_ITEM('')
SURFACE()
);
#859=(
BOUNDED_SURFACE()
B_SPLINE_SURFACE(1,2,((#108087,#108088,#108089,#108090,#108091),(#108092,
#108093,#108094,#108095,#108096)),.UNSPECIFIED.,.F.,.F.,.F.)
B_SPLINE_SURFACE_WITH_KNOTS((2,2),(3,2,3),(0.,0.289681084359921),(0.280328542633765,
0.285714285714286,0.297856505190614),.UNSPECIFIED.)
GEOMETRIC_REPRESENTATION_ITEM()
RATIONAL_B_SPLINE_SURFACE(((0.996504189652447,0.998109554471267,1.,0.995737968897747,
0.992924952273132),(0.996504189652447,0.998109554471267,1.,0.995737968897747,
0.992924952273132)))
REPRESENTATION_ITEM('')
SURFACE()
);
#860=(
BOUNDED_SURFACE()
B_SPLINE_SURFACE(1,2,((#108114,#108115,#108116),(#108117,#108118,#108119)),
 .UNSPECIFIED.,.F.,.F.,.F.)
B_SPLINE_SURFACE_WITH_KNOTS((2,2),(3,3),(0.,0.289807040991685),(0.435775021682461,
0.45302776825947),.UNSPECIFIED.)
GEOMETRIC_REPRESENTATION_ITEM()
RATIONAL_B_SPLINE_SURFACE(((0.995452950231154,0.990618550266732,0.988709602819327),
(0.995452950231154,0.990618550266732,0.988709602819327)))
REPRESENTATION_ITEM('')
SURFACE()
);
#861=(
BOUNDED_SURFACE()
B_SPLINE_SURFACE(1,2,((#108121,#108122,#108123,#108124,#108125),(#108126,
#108127,#108128,#108129,#108130)),.UNSPECIFIED.,.F.,.F.,.F.)
B_SPLINE_SURFACE_WITH_KNOTS((2,2),(3,2,3),(0.,0.289681084359926),(0.280328542633765,
0.285714285714286,0.297856505190614),.UNSPECIFIED.)
GEOMETRIC_REPRESENTATION_ITEM()
RATIONAL_B_SPLINE_SURFACE(((0.996504189652447,0.998109554471267,1.,0.995737968897747,
0.992924952273132),(0.996504189652447,0.998109554471267,1.,0.995737968897747,
0.992924952273132)))
REPRESENTATION_ITEM('')
SURFACE()
);
#862=(
BOUNDED_SURFACE()
B_SPLINE_SURFACE(1,2,((#108148,#108149,#108150),(#108151,#108152,#108153)),
 .UNSPECIFIED.,.F.,.F.,.F.)
B_SPLINE_SURFACE_WITH_KNOTS((2,2),(3,3),(0.,0.289807040991565),(0.435775021682622,
0.453027768259469),.UNSPECIFIED.)
GEOMETRIC_REPRESENTATION_ITEM()
RATIONAL_B_SPLINE_SURFACE(((0.995452950231063,0.990618550266714,0.988709602819327),
(0.995452950231063,0.990618550266714,0.988709602819327)))
REPRESENTATION_ITEM('')
SURFACE()
);
#863=(
BOUNDED_SURFACE()
B_SPLINE_SURFACE(1,2,((#108155,#108156,#108157,#108158,#108159),(#108160,
#108161,#108162,#108163,#108164)),.UNSPECIFIED.,.F.,.F.,.F.)
B_SPLINE_SURFACE_WITH_KNOTS((2,2),(3,2,3),(0.,0.289681084360124),(0.280328542633765,
0.285714285714286,0.297856505190614),.UNSPECIFIED.)
GEOMETRIC_REPRESENTATION_ITEM()
RATIONAL_B_SPLINE_SURFACE(((0.996504189652447,0.998109554471267,1.,0.995737968897747,
0.992924952273132),(0.996504189652447,0.998109554471267,1.,0.995737968897747,
0.992924952273132)))
REPRESENTATION_ITEM('')
SURFACE()
);
#864=(
BOUNDED_SURFACE()
B_SPLINE_SURFACE(1,2,((#108182,#108183,#108184),(#108185,#108186,#108187)),
 .UNSPECIFIED.,.F.,.F.,.F.)
B_SPLINE_SURFACE_WITH_KNOTS((2,2),(3,3),(0.,0.289807040991792),(0.435775021682622,
0.453027768259469),.UNSPECIFIED.)
GEOMETRIC_REPRESENTATION_ITEM()
RATIONAL_B_SPLINE_SURFACE(((0.995452950231063,0.990618550266714,0.988709602819327),
(0.995452950231063,0.990618550266714,0.988709602819327)))
REPRESENTATION_ITEM('')
SURFACE()
);
#865=(
BOUNDED_SURFACE()
B_SPLINE_SURFACE(1,2,((#108189,#108190,#108191,#108192,#108193),(#108194,
#108195,#108196,#108197,#108198)),.UNSPECIFIED.,.F.,.F.,.F.)
B_SPLINE_SURFACE_WITH_KNOTS((2,2),(3,2,3),(0.,0.289681084359926),(0.280328542633765,
0.285714285714286,0.297856505190614),.UNSPECIFIED.)
GEOMETRIC_REPRESENTATION_ITEM()
RATIONAL_B_SPLINE_SURFACE(((0.996504189652447,0.998109554471267,1.,0.995737968897747,
0.992924952273132),(0.996504189652447,0.998109554471267,1.,0.995737968897747,
0.992924952273132)))
REPRESENTATION_ITEM('')
SURFACE()
);
#866=(
BOUNDED_SURFACE()
B_SPLINE_SURFACE(1,2,((#108216,#108217,#108218),(#108219,#108220,#108221)),
 .UNSPECIFIED.,.F.,.F.,.F.)
B_SPLINE_SURFACE_WITH_KNOTS((2,2),(3,3),(0.,0.289807040991559),(0.435775021682622,
0.453027768259469),.UNSPECIFIED.)
GEOMETRIC_REPRESENTATION_ITEM()
RATIONAL_B_SPLINE_SURFACE(((0.995452950231063,0.990618550266714,0.988709602819327),
(0.995452950231063,0.990618550266714,0.988709602819327)))
REPRESENTATION_ITEM('')
SURFACE()
);
#867=(
BOUNDED_SURFACE()
B_SPLINE_SURFACE(1,2,((#108223,#108224,#108225,#108226,#108227),(#108228,
#108229,#108230,#108231,#108232)),.UNSPECIFIED.,.F.,.F.,.F.)
B_SPLINE_SURFACE_WITH_KNOTS((2,2),(3,2,3),(0.,0.289681084359928),(0.280328542633765,
0.285714285714286,0.297856505190614),.UNSPECIFIED.)
GEOMETRIC_REPRESENTATION_ITEM()
RATIONAL_B_SPLINE_SURFACE(((0.996504189652446,0.998109554471267,1.,0.995737968897747,
0.992924952273132),(0.996504189652446,0.998109554471267,1.,0.995737968897747,
0.992924952273132)))
REPRESENTATION_ITEM('')
SURFACE()
);
#868=(
BOUNDED_SURFACE()
B_SPLINE_SURFACE(1,2,((#108250,#108251,#108252),(#108253,#108254,#108255)),
 .UNSPECIFIED.,.F.,.F.,.F.)
B_SPLINE_SURFACE_WITH_KNOTS((2,2),(3,3),(0.,0.289807040992696),(0.435775021682622,
0.453027768259469),.UNSPECIFIED.)
GEOMETRIC_REPRESENTATION_ITEM()
RATIONAL_B_SPLINE_SURFACE(((0.995452950231063,0.990618550266714,0.988709602819327),
(0.995452950231063,0.990618550266714,0.988709602819327)))
REPRESENTATION_ITEM('')
SURFACE()
);
#869=(
BOUNDED_SURFACE()
B_SPLINE_SURFACE(1,2,((#108257,#108258,#108259,#108260,#108261),(#108262,
#108263,#108264,#108265,#108266)),.UNSPECIFIED.,.F.,.F.,.F.)
B_SPLINE_SURFACE_WITH_KNOTS((2,2),(3,2,3),(0.,0.289681084360402),(0.280328542633765,
0.285714285714286,0.297856505190614),.UNSPECIFIED.)
GEOMETRIC_REPRESENTATION_ITEM()
RATIONAL_B_SPLINE_SURFACE(((0.996504189652447,0.998109554471267,1.,0.995737968897747,
0.992924952273132),(0.996504189652447,0.998109554471267,1.,0.995737968897747,
0.992924952273132)))
REPRESENTATION_ITEM('')
SURFACE()
);
#870=(
BOUNDED_SURFACE()
B_SPLINE_SURFACE(1,2,((#108284,#108285,#108286),(#108287,#108288,#108289)),
 .UNSPECIFIED.,.F.,.F.,.F.)
B_SPLINE_SURFACE_WITH_KNOTS((2,2),(3,3),(0.,0.289807040992538),(0.435775021682116,
0.453027768259472),.UNSPECIFIED.)
GEOMETRIC_REPRESENTATION_ITEM()
RATIONAL_B_SPLINE_SURFACE(((0.995452950231347,0.990618550266769,0.988709602819326),
(0.995452950231347,0.990618550266769,0.988709602819326)))
REPRESENTATION_ITEM('')
SURFACE()
);
#871=(
BOUNDED_SURFACE()
B_SPLINE_SURFACE(1,2,((#108291,#108292,#108293,#108294,#108295),(#108296,
#108297,#108298,#108299,#108300)),.UNSPECIFIED.,.F.,.F.,.F.)
B_SPLINE_SURFACE_WITH_KNOTS((2,2),(3,2,3),(0.,0.289681084359924),(0.280328542633765,
0.285714285714286,0.297856505190614),.UNSPECIFIED.)
GEOMETRIC_REPRESENTATION_ITEM()
RATIONAL_B_SPLINE_SURFACE(((0.996504189652447,0.998109554471267,1.,0.995737968897747,
0.992924952273132),(0.996504189652447,0.998109554471267,1.,0.995737968897747,
0.992924952273132)))
REPRESENTATION_ITEM('')
SURFACE()
);
#872=(
BOUNDED_SURFACE()
B_SPLINE_SURFACE(1,2,((#108318,#108319,#108320),(#108321,#108322,#108323)),
 .UNSPECIFIED.,.F.,.F.,.F.)
B_SPLINE_SURFACE_WITH_KNOTS((2,2),(3,3),(0.,0.289807040992669),(0.435775021682251,
0.453027768259471),.UNSPECIFIED.)
GEOMETRIC_REPRESENTATION_ITEM()
RATIONAL_B_SPLINE_SURFACE(((0.995452950231271,0.990618550266755,0.988709602819326),
(0.995452950231271,0.990618550266755,0.988709602819326)))
REPRESENTATION_ITEM('')
SURFACE()
);
#873=(
BOUNDED_SURFACE()
B_SPLINE_SURFACE(1,2,((#108325,#108326,#108327,#108328,#108329),(#108330,
#108331,#108332,#108333,#108334)),.UNSPECIFIED.,.F.,.F.,.F.)
B_SPLINE_SURFACE_WITH_KNOTS((2,2),(3,2,3),(0.,0.289681084360136),(0.280328542633765,
0.285714285714286,0.297856505190614),.UNSPECIFIED.)
GEOMETRIC_REPRESENTATION_ITEM()
RATIONAL_B_SPLINE_SURFACE(((0.996504189652447,0.998109554471267,1.,0.995737968897747,
0.992924952273132),(0.996504189652447,0.998109554471267,1.,0.995737968897747,
0.992924952273132)))
REPRESENTATION_ITEM('')
SURFACE()
);
#874=(
BOUNDED_SURFACE()
B_SPLINE_SURFACE(1,2,((#108352,#108353,#108354),(#108355,#108356,#108357)),
 .UNSPECIFIED.,.F.,.F.,.F.)
B_SPLINE_SURFACE_WITH_KNOTS((2,2),(3,3),(0.,0.289807040991763),(0.435775021682622,
0.453027768259469),.UNSPECIFIED.)
GEOMETRIC_REPRESENTATION_ITEM()
RATIONAL_B_SPLINE_SURFACE(((0.995452950231063,0.990618550266714,0.988709602819327),
(0.995452950231063,0.990618550266714,0.988709602819327)))
REPRESENTATION_ITEM('')
SURFACE()
);
#875=(
BOUNDED_SURFACE()
B_SPLINE_SURFACE(1,2,((#108359,#108360,#108361,#108362,#108363),(#108364,
#108365,#108366,#108367,#108368)),.UNSPECIFIED.,.F.,.F.,.F.)
B_SPLINE_SURFACE_WITH_KNOTS((2,2),(3,2,3),(0.,0.289681084359923),(0.280328542633765,
0.285714285714286,0.297856505190614),.UNSPECIFIED.)
GEOMETRIC_REPRESENTATION_ITEM()
RATIONAL_B_SPLINE_SURFACE(((0.996504189652446,0.998109554471267,1.,0.995737968897747,
0.992924952273132),(0.996504189652446,0.998109554471267,1.,0.995737968897747,
0.992924952273132)))
REPRESENTATION_ITEM('')
SURFACE()
);
#876=(
BOUNDED_SURFACE()
B_SPLINE_SURFACE(1,2,((#108386,#108387,#108388),(#108389,#108390,#108391)),
 .UNSPECIFIED.,.F.,.F.,.F.)
B_SPLINE_SURFACE_WITH_KNOTS((2,2),(3,3),(0.,0.289807040993048),(0.435775021682622,
0.453027768259469),.UNSPECIFIED.)
GEOMETRIC_REPRESENTATION_ITEM()
RATIONAL_B_SPLINE_SURFACE(((0.995452950231063,0.990618550266714,0.988709602819327),
(0.995452950231063,0.990618550266714,0.988709602819327)))
REPRESENTATION_ITEM('')
SURFACE()
);
#877=(
BOUNDED_SURFACE()
B_SPLINE_SURFACE(1,2,((#108393,#108394,#108395,#108396,#108397),(#108398,
#108399,#108400,#108401,#108402)),.UNSPECIFIED.,.F.,.F.,.F.)
B_SPLINE_SURFACE_WITH_KNOTS((2,2),(3,2,3),(0.,0.289681084359929),(0.280328542633765,
0.285714285714286,0.297856505190614),.UNSPECIFIED.)
GEOMETRIC_REPRESENTATION_ITEM()
RATIONAL_B_SPLINE_SURFACE(((0.996504189652446,0.998109554471267,1.,0.995737968897747,
0.992924952273132),(0.996504189652446,0.998109554471267,1.,0.995737968897747,
0.992924952273132)))
REPRESENTATION_ITEM('')
SURFACE()
);
#878=(
BOUNDED_SURFACE()
B_SPLINE_SURFACE(1,2,((#108420,#108421,#108422),(#108423,#108424,#108425)),
 .UNSPECIFIED.,.F.,.F.,.F.)
B_SPLINE_SURFACE_WITH_KNOTS((2,2),(3,3),(0.,0.289807040992795),(0.435775021682622,
0.453027768259469),.UNSPECIFIED.)
GEOMETRIC_REPRESENTATION_ITEM()
RATIONAL_B_SPLINE_SURFACE(((0.995452950231063,0.990618550266714,0.988709602819327),
(0.995452950231063,0.990618550266714,0.988709602819327)))
REPRESENTATION_ITEM('')
SURFACE()
);
#879=(
BOUNDED_SURFACE()
B_SPLINE_SURFACE(1,2,((#108427,#108428,#108429,#108430,#108431),(#108432,
#108433,#108434,#108435,#108436)),.UNSPECIFIED.,.F.,.F.,.F.)
B_SPLINE_SURFACE_WITH_KNOTS((2,2),(3,2,3),(0.,0.289681084360214),(0.280328542633765,
0.285714285714286,0.297856505190614),.UNSPECIFIED.)
GEOMETRIC_REPRESENTATION_ITEM()
RATIONAL_B_SPLINE_SURFACE(((0.996504189652446,0.998109554471267,1.,0.995737968897747,
0.992924952273132),(0.996504189652446,0.998109554471267,1.,0.995737968897747,
0.992924952273132)))
REPRESENTATION_ITEM('')
SURFACE()
);
#880=(
BOUNDED_SURFACE()
B_SPLINE_SURFACE(1,2,((#108454,#108455,#108456),(#108457,#108458,#108459)),
 .UNSPECIFIED.,.F.,.F.,.F.)
B_SPLINE_SURFACE_WITH_KNOTS((2,2),(3,3),(0.,0.289807040992557),(0.435775021682307,
0.453027768259471),.UNSPECIFIED.)
GEOMETRIC_REPRESENTATION_ITEM()
RATIONAL_B_SPLINE_SURFACE(((0.99545295023124,0.990618550266749,0.988709602819327),
(0.99545295023124,0.990618550266749,0.988709602819327)))
REPRESENTATION_ITEM('')
SURFACE()
);
#881=(
BOUNDED_SURFACE()
B_SPLINE_SURFACE(1,2,((#108461,#108462,#108463,#108464,#108465),(#108466,
#108467,#108468,#108469,#108470)),.UNSPECIFIED.,.F.,.F.,.F.)
B_SPLINE_SURFACE_WITH_KNOTS((2,2),(3,2,3),(0.,0.289681084360026),(0.280328542633765,
0.285714285714286,0.297856505190614),.UNSPECIFIED.)
GEOMETRIC_REPRESENTATION_ITEM()
RATIONAL_B_SPLINE_SURFACE(((0.996504189652447,0.998109554471267,1.,0.995737968897747,
0.992924952273132),(0.996504189652447,0.998109554471267,1.,0.995737968897747,
0.992924952273132)))
REPRESENTATION_ITEM('')
SURFACE()
);
#882=(
BOUNDED_SURFACE()
B_SPLINE_SURFACE(1,2,((#108488,#108489,#108490),(#108491,#108492,#108493)),
 .UNSPECIFIED.,.F.,.F.,.F.)
B_SPLINE_SURFACE_WITH_KNOTS((2,2),(3,3),(0.,0.289807040992487),(0.435775021682621,
0.453027768259469),.UNSPECIFIED.)
GEOMETRIC_REPRESENTATION_ITEM()
RATIONAL_B_SPLINE_SURFACE(((0.995452950231063,0.990618550266714,0.988709602819327),
(0.995452950231063,0.990618550266714,0.988709602819327)))
REPRESENTATION_ITEM('')
SURFACE()
);
#883=(
BOUNDED_SURFACE()
B_SPLINE_SURFACE(1,2,((#108495,#108496,#108497,#108498,#108499),(#108500,
#108501,#108502,#108503,#108504)),.UNSPECIFIED.,.F.,.F.,.F.)
B_SPLINE_SURFACE_WITH_KNOTS((2,2),(3,2,3),(0.,0.28968108436023),(0.280328542633765,
0.285714285714286,0.297856505190614),.UNSPECIFIED.)
GEOMETRIC_REPRESENTATION_ITEM()
RATIONAL_B_SPLINE_SURFACE(((0.996504189652447,0.998109554471267,1.,0.995737968897747,
0.992924952273132),(0.996504189652447,0.998109554471267,1.,0.995737968897747,
0.992924952273132)))
REPRESENTATION_ITEM('')
SURFACE()
);
#884=(
BOUNDED_SURFACE()
B_SPLINE_SURFACE(1,2,((#108522,#108523,#108524),(#108525,#108526,#108527)),
 .UNSPECIFIED.,.F.,.F.,.F.)
B_SPLINE_SURFACE_WITH_KNOTS((2,2),(3,3),(0.,0.289807040992805),(0.435775021682253,
0.453027768259471),.UNSPECIFIED.)
GEOMETRIC_REPRESENTATION_ITEM()
RATIONAL_B_SPLINE_SURFACE(((0.99545295023127,0.990618550266755,0.988709602819327),
(0.99545295023127,0.990618550266755,0.988709602819327)))
REPRESENTATION_ITEM('')
SURFACE()
);
#885=(
BOUNDED_SURFACE()
B_SPLINE_SURFACE(1,2,((#108529,#108530,#108531,#108532,#108533),(#108534,
#108535,#108536,#108537,#108538)),.UNSPECIFIED.,.F.,.F.,.F.)
B_SPLINE_SURFACE_WITH_KNOTS((2,2),(3,2,3),(0.,0.28968108435992),(0.280328542633765,
0.285714285714286,0.297856505190614),.UNSPECIFIED.)
GEOMETRIC_REPRESENTATION_ITEM()
RATIONAL_B_SPLINE_SURFACE(((0.996504189652447,0.998109554471267,1.,0.995737968897747,
0.992924952273132),(0.996504189652447,0.998109554471267,1.,0.995737968897747,
0.992924952273132)))
REPRESENTATION_ITEM('')
SURFACE()
);
#886=(
BOUNDED_SURFACE()
B_SPLINE_SURFACE(1,2,((#108556,#108557,#108558),(#108559,#108560,#108561)),
 .UNSPECIFIED.,.F.,.F.,.F.)
B_SPLINE_SURFACE_WITH_KNOTS((2,2),(3,3),(0.,0.28980704099266),(0.435775021682484,
0.45302776825947),.UNSPECIFIED.)
GEOMETRIC_REPRESENTATION_ITEM()
RATIONAL_B_SPLINE_SURFACE(((0.99545295023114,0.990618550266729,0.988709602819327),
(0.99545295023114,0.990618550266729,0.988709602819327)))
REPRESENTATION_ITEM('')
SURFACE()
);
#887=(
BOUNDED_SURFACE()
B_SPLINE_SURFACE(1,2,((#108563,#108564,#108565,#108566,#108567),(#108568,
#108569,#108570,#108571,#108572)),.UNSPECIFIED.,.F.,.F.,.F.)
B_SPLINE_SURFACE_WITH_KNOTS((2,2),(3,2,3),(0.,0.289681084359924),(0.280328542633765,
0.285714285714286,0.297856505190614),.UNSPECIFIED.)
GEOMETRIC_REPRESENTATION_ITEM()
RATIONAL_B_SPLINE_SURFACE(((0.996504189652446,0.998109554471267,1.,0.995737968897747,
0.992924952273132),(0.996504189652446,0.998109554471267,1.,0.995737968897747,
0.992924952273132)))
REPRESENTATION_ITEM('')
SURFACE()
);
#888=(
BOUNDED_SURFACE()
B_SPLINE_SURFACE(1,2,((#108590,#108591,#108592),(#108593,#108594,#108595)),
 .UNSPECIFIED.,.F.,.F.,.F.)
B_SPLINE_SURFACE_WITH_KNOTS((2,2),(3,3),(0.,0.289807040992677),(0.43577502168217,
0.453027768259471),.UNSPECIFIED.)
GEOMETRIC_REPRESENTATION_ITEM()
RATIONAL_B_SPLINE_SURFACE(((0.995452950231316,0.990618550266764,0.988709602819327),
(0.995452950231316,0.990618550266764,0.988709602819327)))
REPRESENTATION_ITEM('')
SURFACE()
);
#889=(
BOUNDED_SURFACE()
B_SPLINE_SURFACE(1,2,((#108597,#108598,#108599,#108600,#108601),(#108602,
#108603,#108604,#108605,#108606)),.UNSPECIFIED.,.F.,.F.,.F.)
B_SPLINE_SURFACE_WITH_KNOTS((2,2),(3,2,3),(0.,0.289681084359919),(0.280328542633765,
0.285714285714286,0.297856505190614),.UNSPECIFIED.)
GEOMETRIC_REPRESENTATION_ITEM()
RATIONAL_B_SPLINE_SURFACE(((0.996504189652446,0.998109554471267,1.,0.995737968897747,
0.992924952273132),(0.996504189652446,0.998109554471267,1.,0.995737968897747,
0.992924952273132)))
REPRESENTATION_ITEM('')
SURFACE()
);
#890=(
BOUNDED_SURFACE()
B_SPLINE_SURFACE(1,2,((#108612,#108613,#108614,#108615,#108616),(#108617,
#108618,#108619,#108620,#108621)),.UNSPECIFIED.,.F.,.F.,.F.)
B_SPLINE_SURFACE_WITH_KNOTS((2,2),(3,2,3),(0.,0.290406045058907),(0.331470144818563,
0.332069149066804,0.349473499542517),.UNSPECIFIED.)
GEOMETRIC_REPRESENTATION_ITEM()
RATIONAL_B_SPLINE_SURFACE(((0.988576730109495,0.988576730109495,0.988576730109495,
0.990396848309667,0.99519405818099),(0.988576730109495,0.988576730109495,
0.988576730109495,0.990396848309667,0.99519405818099)))
REPRESENTATION_ITEM('')
SURFACE()
);
#891=(
BOUNDED_SURFACE()
B_SPLINE_SURFACE(1,2,((#108638,#108639,#108640),(#108641,#108642,#108643),
(#108644,#108645,#108646)),.UNSPECIFIED.,.F.,.F.,.F.)
B_SPLINE_SURFACE_WITH_KNOTS((2,1,2),(3,3),(0.,0.289681084359929,0.292577895203529),
(0.383830569465723,0.401042835325579),.UNSPECIFIED.)
GEOMETRIC_REPRESENTATION_ITEM()
RATIONAL_B_SPLINE_SURFACE(((0.988264753026337,0.98673775832363,0.988122504062159),
(0.988264753026337,0.98673775832363,0.988122504062159),(0.988264753026337,
0.98673775832363,0.988122504062159)))
REPRESENTATION_ITEM('')
SURFACE()
);
#892=(
BOUNDED_SURFACE()
B_SPLINE_SURFACE(1,2,((#108648,#108649,#108650,#108651,#108652),(#108653,
#108654,#108655,#108656,#108657)),.UNSPECIFIED.,.F.,.F.,.F.)
B_SPLINE_SURFACE_WITH_KNOTS((2,2),(3,2,3),(0.,0.290406045025257),(0.331470144821685,
0.332069149066804,0.349473499542519),.UNSPECIFIED.)
GEOMETRIC_REPRESENTATION_ITEM()
RATIONAL_B_SPLINE_SURFACE(((0.988576730109495,0.988576730109495,0.988576730109495,
0.990396848309667,0.995194058180991),(0.988576730109495,0.988576730109495,
0.988576730109495,0.990396848309667,0.995194058180991)))
REPRESENTATION_ITEM('')
SURFACE()
);
#893=(
BOUNDED_SURFACE()
B_SPLINE_SURFACE(1,2,((#108674,#108675,#108676),(#108677,#108678,#108679),
(#108680,#108681,#108682)),.UNSPECIFIED.,.F.,.F.,.F.)
B_SPLINE_SURFACE_WITH_KNOTS((2,1,2),(3,3),(0.,0.289681084359929,0.292577895203529),
(0.383830569465724,0.401042835325431),.UNSPECIFIED.)
GEOMETRIC_REPRESENTATION_ITEM()
RATIONAL_B_SPLINE_SURFACE(((0.988264753026337,0.986737758323643,0.988122504062135),
(0.988264753026337,0.986737758323643,0.988122504062135),(0.988264753026337,
0.986737758323643,0.988122504062135)))
REPRESENTATION_ITEM('')
SURFACE()
);
#894=(
BOUNDED_SURFACE()
B_SPLINE_SURFACE(1,2,((#108684,#108685,#108686,#108687,#108688),(#108689,
#108690,#108691,#108692,#108693)),.UNSPECIFIED.,.F.,.F.,.F.)
B_SPLINE_SURFACE_WITH_KNOTS((2,2),(3,2,3),(0.,0.290406045000865),(0.331470144846541,
0.332069149066804,0.349473499542523),.UNSPECIFIED.)
GEOMETRIC_REPRESENTATION_ITEM()
RATIONAL_B_SPLINE_SURFACE(((0.988576730109495,0.988576730109495,0.988576730109495,
0.990396848309668,0.995194058180993),(0.988576730109495,0.988576730109495,
0.988576730109495,0.990396848309668,0.995194058180993)))
REPRESENTATION_ITEM('')
SURFACE()
);
#895=(
BOUNDED_SURFACE()
B_SPLINE_SURFACE(1,2,((#108710,#108711,#108712),(#108713,#108714,#108715),
(#108716,#108717,#108718)),.UNSPECIFIED.,.F.,.F.,.F.)
B_SPLINE_SURFACE_WITH_KNOTS((2,1,2),(3,3),(0.,0.289681084359919,0.292577895203518),
(0.383830569465724,0.401042835325431),.UNSPECIFIED.)
GEOMETRIC_REPRESENTATION_ITEM()
RATIONAL_B_SPLINE_SURFACE(((0.988264753026337,0.986737758323643,0.988122504062135),
(0.988264753026337,0.986737758323643,0.988122504062135),(0.988264753026337,
0.986737758323643,0.988122504062135)))
REPRESENTATION_ITEM('')
SURFACE()
);
#896=(
BOUNDED_SURFACE()
B_SPLINE_SURFACE(1,2,((#108720,#108721,#108722,#108723,#108724),(#108725,
#108726,#108727,#108728,#108729)),.UNSPECIFIED.,.F.,.F.,.F.)
B_SPLINE_SURFACE_WITH_KNOTS((2,2),(3,2,3),(0.,0.290406045022049),(0.331470144825657,
0.332069149066802,0.349473499542516),.UNSPECIFIED.)
GEOMETRIC_REPRESENTATION_ITEM()
RATIONAL_B_SPLINE_SURFACE(((0.988576730109495,0.988576730109495,0.988576730109495,
0.990396848309667,0.99519405818099),(0.988576730109495,0.988576730109495,
0.988576730109495,0.990396848309667,0.99519405818099)))
REPRESENTATION_ITEM('')
SURFACE()
);
#897=(
BOUNDED_SURFACE()
B_SPLINE_SURFACE(1,2,((#108746,#108747,#108748),(#108749,#108750,#108751),
(#108752,#108753,#108754)),.UNSPECIFIED.,.F.,.F.,.F.)
B_SPLINE_SURFACE_WITH_KNOTS((2,1,2),(3,3),(0.,0.289681084359923,0.292577895203522),
(0.383830569465724,0.401042835325431),.UNSPECIFIED.)
GEOMETRIC_REPRESENTATION_ITEM()
RATIONAL_B_SPLINE_SURFACE(((0.988264753026337,0.986737758323643,0.988122504062135),
(0.988264753026337,0.986737758323643,0.988122504062135),(0.988264753026337,
0.986737758323643,0.988122504062135)))
REPRESENTATION_ITEM('')
SURFACE()
);
#898=(
BOUNDED_SURFACE()
B_SPLINE_SURFACE(1,2,((#108756,#108757,#108758,#108759,#108760),(#108761,
#108762,#108763,#108764,#108765)),.UNSPECIFIED.,.F.,.F.,.F.)
B_SPLINE_SURFACE_WITH_KNOTS((2,2),(3,2,3),(0.,0.290406045027367),(0.331470144820027,
0.332069149066804,0.349473499542516),.UNSPECIFIED.)
GEOMETRIC_REPRESENTATION_ITEM()
RATIONAL_B_SPLINE_SURFACE(((0.988576730109495,0.988576730109495,0.988576730109495,
0.990396848309667,0.99519405818099),(0.988576730109495,0.988576730109495,
0.988576730109495,0.990396848309667,0.99519405818099)))
REPRESENTATION_ITEM('')
SURFACE()
);
#899=(
BOUNDED_SURFACE()
B_SPLINE_SURFACE(1,2,((#108782,#108783,#108784),(#108785,#108786,#108787),
(#108788,#108789,#108790)),.UNSPECIFIED.,.F.,.F.,.F.)
B_SPLINE_SURFACE_WITH_KNOTS((2,1,2),(3,3),(0.,0.289681084359917,0.292577895203516),
(0.383830569465724,0.401042835325431),.UNSPECIFIED.)
GEOMETRIC_REPRESENTATION_ITEM()
RATIONAL_B_SPLINE_SURFACE(((0.988264753026337,0.986737758323643,0.988122504062135),
(0.988264753026337,0.986737758323643,0.988122504062135),(0.988264753026337,
0.986737758323643,0.988122504062135)))
REPRESENTATION_ITEM('')
SURFACE()
);
#900=(
BOUNDED_SURFACE()
B_SPLINE_SURFACE(1,2,((#108792,#108793,#108794,#108795,#108796),(#108797,
#108798,#108799,#108800,#108801)),.UNSPECIFIED.,.F.,.F.,.F.)
B_SPLINE_SURFACE_WITH_KNOTS((2,2),(3,2,3),(0.,0.290406045052955),(0.331470144825287,
0.332069149066804,0.349473499542498),.UNSPECIFIED.)
GEOMETRIC_REPRESENTATION_ITEM()
RATIONAL_B_SPLINE_SURFACE(((0.988576730109495,0.988576730109495,0.988576730109495,
0.990396848309665,0.99519405818098),(0.988576730109495,0.988576730109495,
0.988576730109495,0.990396848309665,0.99519405818098)))
REPRESENTATION_ITEM('')
SURFACE()
);
#901=(
BOUNDED_SURFACE()
B_SPLINE_SURFACE(1,2,((#108818,#108819,#108820),(#108821,#108822,#108823),
(#108824,#108825,#108826)),.UNSPECIFIED.,.F.,.F.,.F.)
B_SPLINE_SURFACE_WITH_KNOTS((2,1,2),(3,3),(0.,0.289681084359922,0.292577895203521),
(0.383830569465707,0.401042835325431),.UNSPECIFIED.)
GEOMETRIC_REPRESENTATION_ITEM()
RATIONAL_B_SPLINE_SURFACE(((0.98826475302634,0.986737758323642,0.988122504062136),
(0.98826475302634,0.986737758323642,0.988122504062136),(0.98826475302634,
0.986737758323642,0.988122504062136)))
REPRESENTATION_ITEM('')
SURFACE()
);
#902=(
BOUNDED_SURFACE()
B_SPLINE_SURFACE(1,2,((#108828,#108829,#108830,#108831,#108832),(#108833,
#108834,#108835,#108836,#108837)),.UNSPECIFIED.,.F.,.F.,.F.)
B_SPLINE_SURFACE_WITH_KNOTS((2,2),(3,2,3),(0.,0.290406045005485),(0.331470144841198,
0.332069149066804,0.349473499542501),.UNSPECIFIED.)
GEOMETRIC_REPRESENTATION_ITEM()
RATIONAL_B_SPLINE_SURFACE(((0.988576730109495,0.988576730109495,0.988576730109495,
0.990396848309665,0.995194058180981),(0.988576730109495,0.988576730109495,
0.988576730109495,0.990396848309665,0.995194058180981)))
REPRESENTATION_ITEM('')
SURFACE()
);
#903=(
BOUNDED_SURFACE()
B_SPLINE_SURFACE(1,2,((#108854,#108855,#108856),(#108857,#108858,#108859),
(#108860,#108861,#108862)),.UNSPECIFIED.,.F.,.F.,.F.)
B_SPLINE_SURFACE_WITH_KNOTS((2,1,2),(3,3),(0.,0.289681084359922,0.292577895203521),
(0.383830569465707,0.401042835325431),.UNSPECIFIED.)
GEOMETRIC_REPRESENTATION_ITEM()
RATIONAL_B_SPLINE_SURFACE(((0.98826475302634,0.986737758323642,0.988122504062136),
(0.98826475302634,0.986737758323642,0.988122504062136),(0.98826475302634,
0.986737758323642,0.988122504062136)))
REPRESENTATION_ITEM('')
SURFACE()
);
#904=(
BOUNDED_SURFACE()
B_SPLINE_SURFACE(1,2,((#108864,#108865,#108866,#108867,#108868),(#108869,
#108870,#108871,#108872,#108873)),.UNSPECIFIED.,.F.,.F.,.F.)
B_SPLINE_SURFACE_WITH_KNOTS((2,2),(3,2,3),(0.,0.290406045032764),(0.331470144844551,
0.332069149066802,0.349473499542498),.UNSPECIFIED.)
GEOMETRIC_REPRESENTATION_ITEM()
RATIONAL_B_SPLINE_SURFACE(((0.988576730109495,0.988576730109495,0.988576730109495,
0.990396848309664,0.99519405818098),(0.988576730109495,0.988576730109495,
0.988576730109495,0.990396848309664,0.99519405818098)))
REPRESENTATION_ITEM('')
SURFACE()
);
#905=(
BOUNDED_SURFACE()
B_SPLINE_SURFACE(1,2,((#108890,#108891,#108892),(#108893,#108894,#108895),
(#108896,#108897,#108898)),.UNSPECIFIED.,.F.,.F.,.F.)
B_SPLINE_SURFACE_WITH_KNOTS((2,1,2),(3,3),(0.,0.289681084359926,0.292577895203525),
(0.383830569465707,0.401042835325431),.UNSPECIFIED.)
GEOMETRIC_REPRESENTATION_ITEM()
RATIONAL_B_SPLINE_SURFACE(((0.98826475302634,0.986737758323642,0.988122504062136),
(0.98826475302634,0.986737758323642,0.988122504062136),(0.98826475302634,
0.986737758323642,0.988122504062136)))
REPRESENTATION_ITEM('')
SURFACE()
);
#906=(
BOUNDED_SURFACE()
B_SPLINE_SURFACE(1,2,((#108900,#108901,#108902,#108903,#108904),(#108905,
#108906,#108907,#108908,#108909)),.UNSPECIFIED.,.F.,.F.,.F.)
B_SPLINE_SURFACE_WITH_KNOTS((2,2),(3,2,3),(0.,0.290406045042011),(0.331470144835407,
0.332069149066802,0.349473499542498),.UNSPECIFIED.)
GEOMETRIC_REPRESENTATION_ITEM()
RATIONAL_B_SPLINE_SURFACE(((0.988576730109495,0.988576730109495,0.988576730109495,
0.990396848309665,0.99519405818098),(0.988576730109495,0.988576730109495,
0.988576730109495,0.990396848309665,0.99519405818098)))
REPRESENTATION_ITEM('')
SURFACE()
);
#907=(
BOUNDED_SURFACE()
B_SPLINE_SURFACE(1,2,((#108926,#108927,#108928),(#108929,#108930,#108931),
(#108932,#108933,#108934)),.UNSPECIFIED.,.F.,.F.,.F.)
B_SPLINE_SURFACE_WITH_KNOTS((2,1,2),(3,3),(0.,0.289681084359927,0.292577895203526),
(0.383830569465707,0.401042835325431),.UNSPECIFIED.)
GEOMETRIC_REPRESENTATION_ITEM()
RATIONAL_B_SPLINE_SURFACE(((0.98826475302634,0.986737758323642,0.988122504062136),
(0.98826475302634,0.986737758323642,0.988122504062136),(0.98826475302634,
0.986737758323642,0.988122504062136)))
REPRESENTATION_ITEM('')
SURFACE()
);
#908=(
BOUNDED_SURFACE()
B_SPLINE_SURFACE(1,2,((#108936,#108937,#108938,#108939,#108940),(#108941,
#108942,#108943,#108944,#108945)),.UNSPECIFIED.,.F.,.F.,.F.)
B_SPLINE_SURFACE_WITH_KNOTS((2,2),(3,2,3),(0.,0.290406045022594),(0.331470144824454,
0.332069149066802,0.349473499542517),.UNSPECIFIED.)
GEOMETRIC_REPRESENTATION_ITEM()
RATIONAL_B_SPLINE_SURFACE(((0.988576730109495,0.988576730109495,0.988576730109495,
0.990396848309666,0.99519405818099),(0.988576730109495,0.988576730109495,
0.988576730109495,0.990396848309666,0.99519405818099)))
REPRESENTATION_ITEM('')
SURFACE()
);
#909=(
BOUNDED_SURFACE()
B_SPLINE_SURFACE(1,2,((#108962,#108963,#108964),(#108965,#108966,#108967),
(#108968,#108969,#108970)),.UNSPECIFIED.,.F.,.F.,.F.)
B_SPLINE_SURFACE_WITH_KNOTS((2,1,2),(3,3),(0.,0.289681084359921,0.29257789520352),
(0.383830569465723,0.401042835325579),.UNSPECIFIED.)
GEOMETRIC_REPRESENTATION_ITEM()
RATIONAL_B_SPLINE_SURFACE(((0.988264753026337,0.98673775832363,0.98812250406216),
(0.988264753026337,0.98673775832363,0.98812250406216),(0.988264753026337,
0.98673775832363,0.98812250406216)))
REPRESENTATION_ITEM('')
SURFACE()
);
#910=(
BOUNDED_SURFACE()
B_SPLINE_SURFACE(1,2,((#108972,#108973,#108974,#108975,#108976),(#108977,
#108978,#108979,#108980,#108981)),.UNSPECIFIED.,.F.,.F.,.F.)
B_SPLINE_SURFACE_WITH_KNOTS((2,2),(3,2,3),(0.,0.290406045013778),(0.33147014483302,
0.332069149066802,0.349473499542517),.UNSPECIFIED.)
GEOMETRIC_REPRESENTATION_ITEM()
RATIONAL_B_SPLINE_SURFACE(((0.988576730109495,0.988576730109495,0.988576730109495,
0.990396848309666,0.99519405818099),(0.988576730109495,0.988576730109495,
0.988576730109495,0.990396848309666,0.99519405818099)))
REPRESENTATION_ITEM('')
SURFACE()
);
#911=(
BOUNDED_SURFACE()
B_SPLINE_SURFACE(1,2,((#108998,#108999,#109000),(#109001,#109002,#109003),
(#109004,#109005,#109006)),.UNSPECIFIED.,.F.,.F.,.F.)
B_SPLINE_SURFACE_WITH_KNOTS((2,1,2),(3,3),(0.,0.289681084359917,0.292577895203516),
(0.383830569465724,0.401042835325432),.UNSPECIFIED.)
GEOMETRIC_REPRESENTATION_ITEM()
RATIONAL_B_SPLINE_SURFACE(((0.988264753026337,0.986737758323643,0.988122504062136),
(0.988264753026337,0.986737758323643,0.988122504062136),(0.988264753026337,
0.986737758323643,0.988122504062136)))
REPRESENTATION_ITEM('')
SURFACE()
);
#912=(
BOUNDED_SURFACE()
B_SPLINE_SURFACE(1,2,((#109008,#109009,#109010,#109011,#109012),(#109013,
#109014,#109015,#109016,#109017)),.UNSPECIFIED.,.F.,.F.,.F.)
B_SPLINE_SURFACE_WITH_KNOTS((2,2),(3,2,3),(0.,0.290406045030811),(0.33147014484647,
0.332069149066802,0.349473499542517),.UNSPECIFIED.)
GEOMETRIC_REPRESENTATION_ITEM()
RATIONAL_B_SPLINE_SURFACE(((0.988576730109495,0.988576730109495,0.988576730109495,
0.990396848309666,0.99519405818099),(0.988576730109495,0.988576730109495,
0.988576730109495,0.990396848309667,0.99519405818099)))
REPRESENTATION_ITEM('')
SURFACE()
);
#913=(
BOUNDED_SURFACE()
B_SPLINE_SURFACE(1,2,((#109034,#109035,#109036),(#109037,#109038,#109039),
(#109040,#109041,#109042)),.UNSPECIFIED.,.F.,.F.,.F.)
B_SPLINE_SURFACE_WITH_KNOTS((2,1,2),(3,3),(0.,0.289681084359925,0.292577895203524),
(0.383830569465724,0.401042835325431),.UNSPECIFIED.)
GEOMETRIC_REPRESENTATION_ITEM()
RATIONAL_B_SPLINE_SURFACE(((0.988264753026337,0.986737758323643,0.988122504062136),
(0.988264753026337,0.986737758323643,0.988122504062135),(0.988264753026337,
0.986737758323643,0.988122504062135)))
REPRESENTATION_ITEM('')
SURFACE()
);
#914=(
BOUNDED_SURFACE()
B_SPLINE_SURFACE(1,2,((#109044,#109045,#109046,#109047,#109048),(#109049,
#109050,#109051,#109052,#109053)),.UNSPECIFIED.,.F.,.F.,.F.)
B_SPLINE_SURFACE_WITH_KNOTS((2,2),(3,2,3),(0.,0.290406045030277),(0.331470144846858,
0.332069149066804,0.349473499542517),.UNSPECIFIED.)
GEOMETRIC_REPRESENTATION_ITEM()
RATIONAL_B_SPLINE_SURFACE(((0.988576730109495,0.988576730109495,0.988576730109495,
0.990396848309667,0.99519405818099),(0.988576730109495,0.988576730109495,
0.988576730109495,0.990396848309667,0.99519405818099)))
REPRESENTATION_ITEM('')
SURFACE()
);
#915=(
BOUNDED_SURFACE()
B_SPLINE_SURFACE(1,2,((#109070,#109071,#109072),(#109073,#109074,#109075),
(#109076,#109077,#109078)),.UNSPECIFIED.,.F.,.F.,.F.)
B_SPLINE_SURFACE_WITH_KNOTS((2,1,2),(3,3),(0.,0.289681084359927,0.292577895203526),
(0.383830569465724,0.401042835325431),.UNSPECIFIED.)
GEOMETRIC_REPRESENTATION_ITEM()
RATIONAL_B_SPLINE_SURFACE(((0.988264753026337,0.986737758323643,0.988122504062136),
(0.988264753026337,0.986737758323643,0.988122504062136),(0.988264753026337,
0.986737758323643,0.988122504062136)))
REPRESENTATION_ITEM('')
SURFACE()
);
#916=(
BOUNDED_SURFACE()
B_SPLINE_SURFACE(1,2,((#109080,#109081,#109082,#109083,#109084),(#109085,
#109086,#109087,#109088,#109089)),.UNSPECIFIED.,.F.,.F.,.F.)
B_SPLINE_SURFACE_WITH_KNOTS((2,2),(3,2,3),(0.,0.290406045030895),(0.331470144814642,
0.332069149066804,0.349473499542517),.UNSPECIFIED.)
GEOMETRIC_REPRESENTATION_ITEM()
RATIONAL_B_SPLINE_SURFACE(((0.988576730109495,0.988576730109495,0.988576730109495,
0.990396848309667,0.99519405818099),(0.988576730109495,0.988576730109495,
0.988576730109495,0.990396848309667,0.99519405818099)))
REPRESENTATION_ITEM('')
SURFACE()
);
#917=(
BOUNDED_SURFACE()
B_SPLINE_SURFACE(1,2,((#109106,#109107,#109108),(#109109,#109110,#109111),
(#109112,#109113,#109114)),.UNSPECIFIED.,.F.,.F.,.F.)
B_SPLINE_SURFACE_WITH_KNOTS((2,1,2),(3,3),(0.,0.289681084359927,0.292577895203526),
(0.383830569465724,0.401042835325431),.UNSPECIFIED.)
GEOMETRIC_REPRESENTATION_ITEM()
RATIONAL_B_SPLINE_SURFACE(((0.988264753026337,0.986737758323643,0.988122504062136),
(0.988264753026337,0.986737758323643,0.988122504062136),(0.988264753026337,
0.986737758323643,0.988122504062136)))
REPRESENTATION_ITEM('')
SURFACE()
);
#918=(
BOUNDED_SURFACE()
B_SPLINE_SURFACE(1,2,((#109116,#109117,#109118,#109119,#109120),(#109121,
#109122,#109123,#109124,#109125)),.UNSPECIFIED.,.F.,.F.,.F.)
B_SPLINE_SURFACE_WITH_KNOTS((2,2),(3,2,3),(0.,0.290038889744793),(0.331837300100696,
0.332069149066804,0.349473499542517),.UNSPECIFIED.)
GEOMETRIC_REPRESENTATION_ITEM()
RATIONAL_B_SPLINE_SURFACE(((0.988576730109495,0.988576730109495,0.988576730109495,
0.990396848309667,0.99519405818099),(0.988576730109495,0.988576730109495,
0.988576730109495,0.990396848309667,0.99519405818099)))
REPRESENTATION_ITEM('')
SURFACE()
);
#919=(
BOUNDED_SURFACE()
B_SPLINE_SURFACE(1,2,((#109133,#109134,#109135),(#109136,#109137,#109138),
(#109139,#109140,#109141)),.UNSPECIFIED.,.F.,.F.,.F.)
B_SPLINE_SURFACE_WITH_KNOTS((2,1,2),(3,3),(0.,0.289681084359933,0.292577895203533),
(0.383830569465724,0.401042835325431),.UNSPECIFIED.)
GEOMETRIC_REPRESENTATION_ITEM()
RATIONAL_B_SPLINE_SURFACE(((0.988264753026337,0.986737758323643,0.988122504062136),
(0.988264753026337,0.986737758323643,0.988122504062136),(0.988264753026337,
0.986737758323643,0.988122504062136)))
REPRESENTATION_ITEM('')
SURFACE()
);
#920=(
BOUNDED_SURFACE()
B_SPLINE_SURFACE(1,2,((#109143,#109144,#109145,#109146,#109147),(#109148,
#109149,#109150,#109151,#109152)),.UNSPECIFIED.,.F.,.F.,.F.)
B_SPLINE_SURFACE_WITH_KNOTS((2,2),(3,2,3),(0.,0.290406045005544),(0.331470144840714,
0.332069149066804,0.349473499542517),.UNSPECIFIED.)
GEOMETRIC_REPRESENTATION_ITEM()
RATIONAL_B_SPLINE_SURFACE(((0.988576730109495,0.988576730109495,0.988576730109495,
0.990396848309667,0.99519405818099),(0.988576730109495,0.988576730109495,
0.988576730109495,0.990396848309667,0.99519405818099)))
REPRESENTATION_ITEM('')
SURFACE()
);
#921=(
BOUNDED_SURFACE()
B_SPLINE_SURFACE(1,2,((#109169,#109170,#109171),(#109172,#109173,#109174),
(#109175,#109176,#109177)),.UNSPECIFIED.,.F.,.F.,.F.)
B_SPLINE_SURFACE_WITH_KNOTS((2,1,2),(3,3),(0.,0.289681084359918,0.292577895203517),
(0.383830569465724,0.401042835325432),.UNSPECIFIED.)
GEOMETRIC_REPRESENTATION_ITEM()
RATIONAL_B_SPLINE_SURFACE(((0.988264753026337,0.986737758323643,0.988122504062136),
(0.988264753026337,0.986737758323643,0.988122504062136),(0.988264753026337,
0.986737758323643,0.988122504062136)))
REPRESENTATION_ITEM('')
SURFACE()
);
#922=(
BOUNDED_SURFACE()
B_SPLINE_SURFACE(1,2,((#109179,#109180,#109181,#109182,#109183),(#109184,
#109185,#109186,#109187,#109188)),.UNSPECIFIED.,.F.,.F.,.F.)
B_SPLINE_SURFACE_WITH_KNOTS((2,2),(3,2,3),(0.,0.29040604502067),(0.331470144826036,
0.332069149066804,0.349473499542517),.UNSPECIFIED.)
GEOMETRIC_REPRESENTATION_ITEM()
RATIONAL_B_SPLINE_SURFACE(((0.988576730109495,0.988576730109495,0.988576730109495,
0.990396848309667,0.99519405818099),(0.988576730109495,0.988576730109495,
0.988576730109495,0.990396848309667,0.99519405818099)))
REPRESENTATION_ITEM('')
SURFACE()
);
#923=(
BOUNDED_SURFACE()
B_SPLINE_SURFACE(1,2,((#109205,#109206,#109207),(#109208,#109209,#109210),
(#109211,#109212,#109213)),.UNSPECIFIED.,.F.,.F.,.F.)
B_SPLINE_SURFACE_WITH_KNOTS((2,1,2),(3,3),(0.,0.289681084359923,0.292577895203522),
(0.383830569465724,0.401042835325432),.UNSPECIFIED.)
GEOMETRIC_REPRESENTATION_ITEM()
RATIONAL_B_SPLINE_SURFACE(((0.988264753026337,0.986737758323643,0.988122504062136),
(0.988264753026337,0.986737758323643,0.988122504062136),(0.988264753026337,
0.986737758323643,0.988122504062136)))
REPRESENTATION_ITEM('')
SURFACE()
);
#924=(
BOUNDED_SURFACE()
B_SPLINE_SURFACE(1,2,((#109215,#109216,#109217,#109218,#109219),(#109220,
#109221,#109222,#109223,#109224)),.UNSPECIFIED.,.F.,.F.,.F.)
B_SPLINE_SURFACE_WITH_KNOTS((2,2),(3,2,3),(0.,0.290406045013821),(0.331470144832401,
0.332069149066804,0.349473499542517),.UNSPECIFIED.)
GEOMETRIC_REPRESENTATION_ITEM()
RATIONAL_B_SPLINE_SURFACE(((0.988576730109495,0.988576730109495,0.988576730109495,
0.990396848309667,0.99519405818099),(0.988576730109495,0.988576730109495,
0.988576730109495,0.990396848309667,0.99519405818099)))
REPRESENTATION_ITEM('')
SURFACE()
);
#925=(
BOUNDED_SURFACE()
B_SPLINE_SURFACE(1,2,((#109241,#109242,#109243),(#109244,#109245,#109246),
(#109247,#109248,#109249)),.UNSPECIFIED.,.F.,.F.,.F.)
B_SPLINE_SURFACE_WITH_KNOTS((2,1,2),(3,3),(0.,0.289681084359923,0.292577895203522),
(0.383830569465724,0.401042835325432),.UNSPECIFIED.)
GEOMETRIC_REPRESENTATION_ITEM()
RATIONAL_B_SPLINE_SURFACE(((0.988264753026337,0.986737758323643,0.988122504062136),
(0.988264753026337,0.986737758323643,0.988122504062136),(0.988264753026337,
0.986737758323643,0.988122504062136)))
REPRESENTATION_ITEM('')
SURFACE()
);
#926=(
BOUNDED_SURFACE()
B_SPLINE_SURFACE(1,2,((#109251,#109252,#109253,#109254,#109255),(#109256,
#109257,#109258,#109259,#109260)),.UNSPECIFIED.,.F.,.F.,.F.)
B_SPLINE_SURFACE_WITH_KNOTS((2,2),(3,2,3),(0.,0.2904060450347),(0.331470144843839,
0.332069149066802,0.349473499542517),.UNSPECIFIED.)
GEOMETRIC_REPRESENTATION_ITEM()
RATIONAL_B_SPLINE_SURFACE(((0.988576730109495,0.988576730109495,0.988576730109495,
0.990396848309667,0.99519405818099),(0.988576730109495,0.988576730109495,
0.988576730109495,0.990396848309667,0.99519405818099)))
REPRESENTATION_ITEM('')
SURFACE()
);
#927=(
BOUNDED_SURFACE()
B_SPLINE_SURFACE(1,2,((#109277,#109278,#109279),(#109280,#109281,#109282),
(#109283,#109284,#109285)),.UNSPECIFIED.,.F.,.F.,.F.)
B_SPLINE_SURFACE_WITH_KNOTS((2,1,2),(3,3),(0.,0.289681084359922,0.292577895203521),
(0.383830569465724,0.401042835325431),.UNSPECIFIED.)
GEOMETRIC_REPRESENTATION_ITEM()
RATIONAL_B_SPLINE_SURFACE(((0.988264753026337,0.986737758323643,0.988122504062136),
(0.988264753026337,0.986737758323643,0.988122504062136),(0.988264753026337,
0.986737758323643,0.988122504062136)))
REPRESENTATION_ITEM('')
SURFACE()
);
#928=(
BOUNDED_SURFACE()
B_SPLINE_SURFACE(1,2,((#109287,#109288,#109289,#109290,#109291),(#109292,
#109293,#109294,#109295,#109296)),.UNSPECIFIED.,.F.,.F.,.F.)
B_SPLINE_SURFACE_WITH_KNOTS((2,2),(3,2,3),(0.,0.290406045030005),(0.331470144816454,
0.332069149066802,0.349473499542517),.UNSPECIFIED.)
GEOMETRIC_REPRESENTATION_ITEM()
RATIONAL_B_SPLINE_SURFACE(((0.988576730109495,0.988576730109495,0.988576730109495,
0.990396848309667,0.99519405818099),(0.988576730109495,0.988576730109495,
0.988576730109495,0.990396848309667,0.99519405818099)))
REPRESENTATION_ITEM('')
SURFACE()
);
#929=(
BOUNDED_SURFACE()
B_SPLINE_SURFACE(1,2,((#109313,#109314,#109315),(#109316,#109317,#109318),
(#109319,#109320,#109321)),.UNSPECIFIED.,.F.,.F.,.F.)
B_SPLINE_SURFACE_WITH_KNOTS((2,1,2),(3,3),(0.,0.289681084359921,0.29257789520352),
(0.383830569465724,0.401042835325431),.UNSPECIFIED.)
GEOMETRIC_REPRESENTATION_ITEM()
RATIONAL_B_SPLINE_SURFACE(((0.988264753026337,0.986737758323643,0.988122504062136),
(0.988264753026337,0.986737758323643,0.988122504062136),(0.988264753026337,
0.986737758323643,0.988122504062136)))
REPRESENTATION_ITEM('')
SURFACE()
);
#930=(
BOUNDED_SURFACE()
B_SPLINE_SURFACE(1,2,((#109323,#109324,#109325,#109326,#109327),(#109328,
#109329,#109330,#109331,#109332)),.UNSPECIFIED.,.F.,.F.,.F.)
B_SPLINE_SURFACE_WITH_KNOTS((2,2),(3,2,3),(0.,0.290406045012658),(0.331470144833921,
0.332069149066804,0.349473499542517),.UNSPECIFIED.)
GEOMETRIC_REPRESENTATION_ITEM()
RATIONAL_B_SPLINE_SURFACE(((0.988576730109495,0.988576730109495,0.988576730109495,
0.990396848309667,0.99519405818099),(0.988576730109495,0.988576730109495,
0.988576730109495,0.990396848309667,0.99519405818099)))
REPRESENTATION_ITEM('')
SURFACE()
);
#931=(
BOUNDED_SURFACE()
B_SPLINE_SURFACE(1,2,((#109349,#109350,#109351),(#109352,#109353,#109354),
(#109355,#109356,#109357)),.UNSPECIFIED.,.F.,.F.,.F.)
B_SPLINE_SURFACE_WITH_KNOTS((2,1,2),(3,3),(0.,0.289681084359924,0.292577895203523),
(0.383830569465724,0.401042835325431),.UNSPECIFIED.)
GEOMETRIC_REPRESENTATION_ITEM()
RATIONAL_B_SPLINE_SURFACE(((0.988264753026337,0.986737758323643,0.988122504062136),
(0.988264753026337,0.986737758323643,0.988122504062135),(0.988264753026337,
0.986737758323643,0.988122504062135)))
REPRESENTATION_ITEM('')
SURFACE()
);
#932=(
BOUNDED_SURFACE()
B_SPLINE_SURFACE(1,2,((#109359,#109360,#109361,#109362,#109363),(#109364,
#109365,#109366,#109367,#109368)),.UNSPECIFIED.,.F.,.F.,.F.)
B_SPLINE_SURFACE_WITH_KNOTS((2,2),(3,2,3),(0.,0.29040604502366),(0.331470144822577,
0.332069149066802,0.349473499542517),.UNSPECIFIED.)
GEOMETRIC_REPRESENTATION_ITEM()
RATIONAL_B_SPLINE_SURFACE(((0.988576730109495,0.988576730109495,0.988576730109495,
0.990396848309667,0.99519405818099),(0.988576730109495,0.988576730109495,
0.988576730109495,0.990396848309667,0.99519405818099)))
REPRESENTATION_ITEM('')
SURFACE()
);
#933=(
BOUNDED_SURFACE()
B_SPLINE_SURFACE(1,2,((#109385,#109386,#109387),(#109388,#109389,#109390),
(#109391,#109392,#109393)),.UNSPECIFIED.,.F.,.F.,.F.)
B_SPLINE_SURFACE_WITH_KNOTS((2,1,2),(3,3),(0.,0.289681084359919,0.292577895203518),
(0.383830569465724,0.401042835325431),.UNSPECIFIED.)
GEOMETRIC_REPRESENTATION_ITEM()
RATIONAL_B_SPLINE_SURFACE(((0.988264753026337,0.986737758323643,0.988122504062136),
(0.988264753026337,0.986737758323643,0.988122504062135),(0.988264753026337,
0.986737758323643,0.988122504062135)))
REPRESENTATION_ITEM('')
SURFACE()
);
#934=(
BOUNDED_SURFACE()
B_SPLINE_SURFACE(1,2,((#109395,#109396,#109397,#109398,#109399),(#109400,
#109401,#109402,#109403,#109404)),.UNSPECIFIED.,.F.,.F.,.F.)
B_SPLINE_SURFACE_WITH_KNOTS((2,2),(3,2,3),(0.,0.290406045042354),(0.33147014480446,
0.332069149066802,0.349473499542517),.UNSPECIFIED.)
GEOMETRIC_REPRESENTATION_ITEM()
RATIONAL_B_SPLINE_SURFACE(((0.988576730109495,0.988576730109495,0.988576730109495,
0.990396848309667,0.99519405818099),(0.988576730109495,0.988576730109495,
0.988576730109495,0.990396848309666,0.99519405818099)))
REPRESENTATION_ITEM('')
SURFACE()
);
#935=(
BOUNDED_SURFACE()
B_SPLINE_SURFACE(1,2,((#109421,#109422,#109423),(#109424,#109425,#109426),
(#109427,#109428,#109429)),.UNSPECIFIED.,.F.,.F.,.F.)
B_SPLINE_SURFACE_WITH_KNOTS((2,1,2),(3,3),(0.,0.289681084359919,0.292577895203518),
(0.383830569465724,0.401042835325431),.UNSPECIFIED.)
GEOMETRIC_REPRESENTATION_ITEM()
RATIONAL_B_SPLINE_SURFACE(((0.988264753026337,0.986737758323643,0.988122504062136),
(0.988264753026337,0.986737758323643,0.988122504062136),(0.988264753026337,
0.986737758323643,0.988122504062136)))
REPRESENTATION_ITEM('')
SURFACE()
);
#936=(
BOUNDED_SURFACE()
B_SPLINE_SURFACE(1,2,((#109431,#109432,#109433,#109434,#109435),(#109436,
#109437,#109438,#109439,#109440)),.UNSPECIFIED.,.F.,.F.,.F.)
B_SPLINE_SURFACE_WITH_KNOTS((2,2),(3,2,3),(0.,0.290406045004334),(0.331470144841729,
0.332069149066802,0.349473499542517),.UNSPECIFIED.)
GEOMETRIC_REPRESENTATION_ITEM()
RATIONAL_B_SPLINE_SURFACE(((0.988576730109495,0.988576730109495,0.988576730109495,
0.990396848309667,0.99519405818099),(0.988576730109495,0.988576730109495,
0.988576730109495,0.990396848309666,0.99519405818099)))
REPRESENTATION_ITEM('')
SURFACE()
);
#937=(
BOUNDED_SURFACE()
B_SPLINE_SURFACE(1,2,((#109451,#109452,#109453),(#109454,#109455,#109456),
(#109457,#109458,#109459)),.UNSPECIFIED.,.F.,.F.,.F.)
B_SPLINE_SURFACE_WITH_KNOTS((2,1,2),(3,3),(0.,0.289681084359924,0.292577895203523),
(0.383830569465724,0.401042835325431),.UNSPECIFIED.)
GEOMETRIC_REPRESENTATION_ITEM()
RATIONAL_B_SPLINE_SURFACE(((0.988264753026337,0.986737758323643,0.988122504062136),
(0.988264753026337,0.986737758323643,0.988122504062136),(0.988264753026337,
0.986737758323643,0.988122504062136)))
REPRESENTATION_ITEM('')
SURFACE()
);
#938=(
BOUNDED_SURFACE()
B_SPLINE_SURFACE(1,2,((#109467,#109468,#109469,#109470,#109471),(#109472,
#109473,#109474,#109475,#109476)),.UNSPECIFIED.,.F.,.F.,.F.)
B_SPLINE_SURFACE_WITH_KNOTS((2,2),(3,2,3),(0.,0.290406045008831),(0.331470144837565,
0.332069149066804,0.349473499542517),.UNSPECIFIED.)
GEOMETRIC_REPRESENTATION_ITEM()
RATIONAL_B_SPLINE_SURFACE(((0.988576730109495,0.988576730109495,0.988576730109495,
0.990396848309667,0.99519405818099),(0.988576730109495,0.988576730109495,
0.988576730109495,0.990396848309667,0.99519405818099)))
REPRESENTATION_ITEM('')
SURFACE()
);
#939=(
BOUNDED_SURFACE()
B_SPLINE_SURFACE(1,2,((#109493,#109494,#109495),(#109496,#109497,#109498),
(#109499,#109500,#109501)),.UNSPECIFIED.,.F.,.F.,.F.)
B_SPLINE_SURFACE_WITH_KNOTS((2,1,2),(3,3),(0.,0.289681084359917,0.292577895203516),
(0.38383056946572,0.401042835325487),.UNSPECIFIED.)
GEOMETRIC_REPRESENTATION_ITEM()
RATIONAL_B_SPLINE_SURFACE(((0.988264753026338,0.986737758323638,0.988122504062145),
(0.988264753026338,0.986737758323638,0.988122504062145),(0.988264753026338,
0.986737758323638,0.988122504062145)))
REPRESENTATION_ITEM('')
SURFACE()
);
#940=(
BOUNDED_SURFACE()
B_SPLINE_SURFACE(1,2,((#109503,#109504,#109505,#109506,#109507),(#109508,
#109509,#109510,#109511,#109512)),.UNSPECIFIED.,.F.,.F.,.F.)
B_SPLINE_SURFACE_WITH_KNOTS((2,2),(3,2,3),(0.,0.290406045002945),(0.331470144843635,
0.332069149066803,0.349473499542518),.UNSPECIFIED.)
GEOMETRIC_REPRESENTATION_ITEM()
RATIONAL_B_SPLINE_SURFACE(((0.988576730109495,0.988576730109495,0.988576730109495,
0.990396848309667,0.995194058180991),(0.988576730109495,0.988576730109495,
0.988576730109495,0.990396848309667,0.995194058180991)))
REPRESENTATION_ITEM('')
SURFACE()
);
#941=(
BOUNDED_SURFACE()
B_SPLINE_SURFACE(1,2,((#109529,#109530,#109531),(#109532,#109533,#109534),
(#109535,#109536,#109537)),.UNSPECIFIED.,.F.,.F.,.F.)
B_SPLINE_SURFACE_WITH_KNOTS((2,1,2),(3,3),(0.,0.289681084359926,0.292577895203525),
(0.383830569465722,0.40104283532548),.UNSPECIFIED.)
GEOMETRIC_REPRESENTATION_ITEM()
RATIONAL_B_SPLINE_SURFACE(((0.988264753026337,0.986737758323638,0.988122504062143),
(0.988264753026337,0.986737758323638,0.988122504062143),(0.988264753026337,
0.986737758323638,0.988122504062143)))
REPRESENTATION_ITEM('')
SURFACE()
);
#942=(
BOUNDED_SURFACE()
B_SPLINE_SURFACE(1,2,((#109539,#109540,#109541,#109542,#109543),(#109544,
#109545,#109546,#109547,#109548)),.UNSPECIFIED.,.F.,.F.,.F.)
B_SPLINE_SURFACE_WITH_KNOTS((2,2),(3,2,3),(0.,0.290406045028382),(0.331470144849026,
0.332069149066805,0.349473499542517),.UNSPECIFIED.)
GEOMETRIC_REPRESENTATION_ITEM()
RATIONAL_B_SPLINE_SURFACE(((0.988576730109495,0.988576730109495,0.988576730109495,
0.990396848309667,0.99519405818099),(0.988576730109495,0.988576730109495,
0.988576730109495,0.990396848309667,0.99519405818099)))
REPRESENTATION_ITEM('')
SURFACE()
);
#943=(
BOUNDED_SURFACE()
B_SPLINE_SURFACE(1,2,((#109565,#109566,#109567),(#109568,#109569,#109570),
(#109571,#109572,#109573)),.UNSPECIFIED.,.F.,.F.,.F.)
B_SPLINE_SURFACE_WITH_KNOTS((2,1,2),(3,3),(0.,0.289681084359917,0.292577895203516),
(0.383830569465723,0.40104283532558),.UNSPECIFIED.)
GEOMETRIC_REPRESENTATION_ITEM()
RATIONAL_B_SPLINE_SURFACE(((0.988264753026337,0.98673775832363,0.98812250406216),
(0.988264753026337,0.98673775832363,0.98812250406216),(0.988264753026337,
0.98673775832363,0.98812250406216)))
REPRESENTATION_ITEM('')
SURFACE()
);
#944=(
BOUNDED_SURFACE()
B_SPLINE_SURFACE(1,2,((#109575,#109576,#109577,#109578,#109579),(#109580,
#109581,#109582,#109583,#109584)),.UNSPECIFIED.,.F.,.F.,.F.)
B_SPLINE_SURFACE_WITH_KNOTS((2,2),(3,2,3),(0.,0.290406045018038),(0.331470144859553,
0.332069149066804,0.349473499542517),.UNSPECIFIED.)
GEOMETRIC_REPRESENTATION_ITEM()
RATIONAL_B_SPLINE_SURFACE(((0.988576730109495,0.988576730109495,0.988576730109495,
0.990396848309667,0.99519405818099),(0.988576730109495,0.988576730109495,
0.988576730109495,0.990396848309667,0.99519405818099)))
REPRESENTATION_ITEM('')
SURFACE()
);
#945=(
BOUNDED_SURFACE()
B_SPLINE_SURFACE(1,2,((#109601,#109602,#109603),(#109604,#109605,#109606),
(#109607,#109608,#109609)),.UNSPECIFIED.,.F.,.F.,.F.)
B_SPLINE_SURFACE_WITH_KNOTS((2,1,2),(3,3),(0.,0.289681084359936,0.292577895203535),
(0.383830569465723,0.40104283532558),.UNSPECIFIED.)
GEOMETRIC_REPRESENTATION_ITEM()
RATIONAL_B_SPLINE_SURFACE(((0.988264753026337,0.986737758323629,0.988122504062159),
(0.988264753026337,0.986737758323629,0.988122504062159),(0.988264753026337,
0.986737758323629,0.988122504062159)))
REPRESENTATION_ITEM('')
SURFACE()
);
#946=(
BOUNDED_SURFACE()
B_SPLINE_SURFACE(1,2,((#109611,#109612,#109613,#109614,#109615),(#109616,
#109617,#109618,#109619,#109620)),.UNSPECIFIED.,.F.,.F.,.F.)
B_SPLINE_SURFACE_WITH_KNOTS((2,2),(3,2,3),(0.,0.290406045046641),(0.331470144830908,
0.332069149066804,0.349473499542517),.UNSPECIFIED.)
GEOMETRIC_REPRESENTATION_ITEM()
RATIONAL_B_SPLINE_SURFACE(((0.988576730109495,0.988576730109495,0.988576730109495,
0.990396848309667,0.99519405818099),(0.988576730109495,0.988576730109495,
0.988576730109495,0.990396848309667,0.99519405818099)))
REPRESENTATION_ITEM('')
SURFACE()
);
#947=(
BOUNDED_SURFACE()
B_SPLINE_SURFACE(1,2,((#109637,#109638,#109639),(#109640,#109641,#109642),
(#109643,#109644,#109645)),.UNSPECIFIED.,.F.,.F.,.F.)
B_SPLINE_SURFACE_WITH_KNOTS((2,1,2),(3,3),(0.,0.289681084359927,0.292577895203526),
(0.383830569465723,0.401042835325579),.UNSPECIFIED.)
GEOMETRIC_REPRESENTATION_ITEM()
RATIONAL_B_SPLINE_SURFACE(((0.988264753026337,0.98673775832363,0.988122504062159),
(0.988264753026337,0.98673775832363,0.988122504062159),(0.988264753026337,
0.98673775832363,0.988122504062159)))
REPRESENTATION_ITEM('')
SURFACE()
);
#948=(
BOUNDED_SURFACE()
B_SPLINE_SURFACE(1,2,((#109647,#109648,#109649),(#109650,#109651,#109652)),
 .UNSPECIFIED.,.F.,.F.,.F.)
B_SPLINE_SURFACE_WITH_KNOTS((2,2),(3,3),(0.710318915638199,1.),(0.435672122597606,
0.452924869174518),.UNSPECIFIED.)
GEOMETRIC_REPRESENTATION_ITEM()
RATIONAL_B_SPLINE_SURFACE(((0.995510721093658,0.99065887310234,0.988732477628005),
(0.995510721093658,0.99065887310234,0.988732477628005)))
REPRESENTATION_ITEM('')
SURFACE()
);
#949=(
BOUNDED_SURFACE()
B_SPLINE_SURFACE(1,2,((#109663,#109664,#109665,#109666,#109667,#109668,
#109669),(#109670,#109671,#109672,#109673,#109674,#109675,#109676)),
 .UNSPECIFIED.,.F.,.F.,.F.)
B_SPLINE_SURFACE_WITH_KNOTS((2,2),(3,2,2,3),(0.710192959006552,1.),(0.280257803540346,
0.280433083165914,0.285714285714286,0.297961045722742),.UNSPECIFIED.)
GEOMETRIC_REPRESENTATION_ITEM()
RATIONAL_B_SPLINE_SURFACE(((0.996566619267864,0.996566619267864,0.996566619267864,
0.998146249162903,1.,0.995701274206118,0.992876621380151),(0.996566619267864,
0.996566619267864,0.996566619267864,0.998146249162903,1.,0.995701274206118,
0.992876621380151)))
REPRESENTATION_ITEM('')
SURFACE()
);
#950=(
BOUNDED_SURFACE()
B_SPLINE_SURFACE(1,2,((#109690,#109691,#109692),(#109693,#109694,#109695)),
 .UNSPECIFIED.,.F.,.F.,.F.)
B_SPLINE_SURFACE_WITH_KNOTS((2,2),(3,3),(0.710318915640079,1.),(0.43567212259767,
0.452924869174517),.UNSPECIFIED.)
GEOMETRIC_REPRESENTATION_ITEM()
RATIONAL_B_SPLINE_SURFACE(((0.995510721093622,0.990658873102333,0.988732477628005),
(0.995510721093622,0.990658873102333,0.988732477628005)))
REPRESENTATION_ITEM('')
SURFACE()
);
#951=(
BOUNDED_SURFACE()
B_SPLINE_SURFACE(1,2,((#109706,#109707,#109708,#109709,#109710,#109711,
#109712),(#109713,#109714,#109715,#109716,#109717,#109718,#109719)),
 .UNSPECIFIED.,.F.,.F.,.F.)
B_SPLINE_SURFACE_WITH_KNOTS((2,2),(3,2,2,3),(0.710192959008442,1.),(0.280257803540343,
0.280433083165911,0.285714285714286,0.297961045722763),.UNSPECIFIED.)
GEOMETRIC_REPRESENTATION_ITEM()
RATIONAL_B_SPLINE_SURFACE(((0.996566619267862,0.996566619267862,0.996566619267862,
0.998146249162902,1.,0.995701274206111,0.992876621380142),(0.996566619267862,
0.996566619267862,0.996566619267862,0.998146249162902,1.,0.995701274206111,
0.992876621380142)))
REPRESENTATION_ITEM('')
SURFACE()
);
#952=(
BOUNDED_SURFACE()
B_SPLINE_SURFACE(1,2,((#109733,#109734,#109735),(#109736,#109737,#109738)),
 .UNSPECIFIED.,.F.,.F.,.F.)
B_SPLINE_SURFACE_WITH_KNOTS((2,2),(3,3),(0.710318915639502,1.),(0.43567212259767,
0.452924869174517),.UNSPECIFIED.)
GEOMETRIC_REPRESENTATION_ITEM()
RATIONAL_B_SPLINE_SURFACE(((0.995510721093622,0.990658873102333,0.988732477628006),
(0.995510721093622,0.990658873102333,0.988732477628006)))
REPRESENTATION_ITEM('')
SURFACE()
);
#953=(
BOUNDED_SURFACE()
B_SPLINE_SURFACE(1,2,((#109749,#109750,#109751,#109752,#109753,#109754,
#109755),(#109756,#109757,#109758,#109759,#109760,#109761,#109762)),
 .UNSPECIFIED.,.F.,.F.,.F.)
B_SPLINE_SURFACE_WITH_KNOTS((2,2),(3,2,2,3),(0.710192959007859,1.),(0.280257803540345,
0.280433083165913,0.285714285714286,0.297961045722763),.UNSPECIFIED.)
GEOMETRIC_REPRESENTATION_ITEM()
RATIONAL_B_SPLINE_SURFACE(((0.996566619267863,0.996566619267863,0.996566619267863,
0.998146249162903,1.,0.995701274206111,0.992876621380141),(0.996566619267863,
0.996566619267863,0.996566619267863,0.998146249162903,1.,0.995701274206111,
0.992876621380141)))
REPRESENTATION_ITEM('')
SURFACE()
);
#954=(
BOUNDED_SURFACE()
B_SPLINE_SURFACE(1,2,((#109776,#109777,#109778),(#109779,#109780,#109781)),
 .UNSPECIFIED.,.F.,.F.,.F.)
B_SPLINE_SURFACE_WITH_KNOTS((2,2),(3,3),(0.710318915640078,1.),(0.43567212259767,
0.452924869174517),.UNSPECIFIED.)
GEOMETRIC_REPRESENTATION_ITEM()
RATIONAL_B_SPLINE_SURFACE(((0.995510721093622,0.990658873102333,0.988732477628005),
(0.995510721093622,0.990658873102333,0.988732477628005)))
REPRESENTATION_ITEM('')
SURFACE()
);
#955=(
BOUNDED_SURFACE()
B_SPLINE_SURFACE(1,2,((#109792,#109793,#109794,#109795,#109796,#109797,
#109798),(#109799,#109800,#109801,#109802,#109803,#109804,#109805)),
 .UNSPECIFIED.,.F.,.F.,.F.)
B_SPLINE_SURFACE_WITH_KNOTS((2,2),(3,2,2,3),(0.710192959008441,1.),(0.280257803540345,
0.280433083165913,0.285714285714286,0.297961045722763),.UNSPECIFIED.)
GEOMETRIC_REPRESENTATION_ITEM()
RATIONAL_B_SPLINE_SURFACE(((0.996566619267863,0.996566619267863,0.996566619267863,
0.998146249162903,1.,0.995701274206111,0.992876621380142),(0.996566619267863,
0.996566619267863,0.996566619267863,0.998146249162903,1.,0.995701274206111,
0.992876621380142)))
REPRESENTATION_ITEM('')
SURFACE()
);
#956=(
BOUNDED_SURFACE()
B_SPLINE_SURFACE(1,2,((#109819,#109820,#109821),(#109822,#109823,#109824)),
 .UNSPECIFIED.,.F.,.F.,.F.)
B_SPLINE_SURFACE_WITH_KNOTS((2,2),(3,3),(0.710318915639499,1.),(0.43567212259767,
0.452924869174517),.UNSPECIFIED.)
GEOMETRIC_REPRESENTATION_ITEM()
RATIONAL_B_SPLINE_SURFACE(((0.995510721093622,0.990658873102333,0.988732477628005),
(0.995510721093622,0.990658873102333,0.988732477628005)))
REPRESENTATION_ITEM('')
SURFACE()
);
#957=(
BOUNDED_SURFACE()
B_SPLINE_SURFACE(1,2,((#109835,#109836,#109837,#109838,#109839,#109840,
#109841),(#109842,#109843,#109844,#109845,#109846,#109847,#109848)),
 .UNSPECIFIED.,.F.,.F.,.F.)
B_SPLINE_SURFACE_WITH_KNOTS((2,2),(3,2,2,3),(0.710192959007862,1.),(0.280257803540345,
0.280433083165913,0.285714285714286,0.297961045722763),.UNSPECIFIED.)
GEOMETRIC_REPRESENTATION_ITEM()
RATIONAL_B_SPLINE_SURFACE(((0.996566619267863,0.996566619267863,0.996566619267863,
0.998146249162903,1.,0.995701274206111,0.992876621380142),(0.996566619267863,
0.996566619267863,0.996566619267863,0.998146249162903,1.,0.995701274206111,
0.992876621380142)))
REPRESENTATION_ITEM('')
SURFACE()
);
#958=(
BOUNDED_SURFACE()
B_SPLINE_SURFACE(1,2,((#109862,#109863,#109864),(#109865,#109866,#109867)),
 .UNSPECIFIED.,.F.,.F.,.F.)
B_SPLINE_SURFACE_WITH_KNOTS((2,2),(3,3),(0.710318915640002,1.),(0.435672122597671,
0.452924869174517),.UNSPECIFIED.)
GEOMETRIC_REPRESENTATION_ITEM()
RATIONAL_B_SPLINE_SURFACE(((0.995510721093621,0.990658873102333,0.988732477628005),
(0.995510721093621,0.990658873102333,0.988732477628005)))
REPRESENTATION_ITEM('')
SURFACE()
);
#959=(
BOUNDED_SURFACE()
B_SPLINE_SURFACE(1,2,((#109878,#109879,#109880,#109881,#109882,#109883,
#109884),(#109885,#109886,#109887,#109888,#109889,#109890,#109891)),
 .UNSPECIFIED.,.F.,.F.,.F.)
B_SPLINE_SURFACE_WITH_KNOTS((2,2),(3,2,2,3),(0.710192959008361,1.),(0.280257803540343,
0.280433083165911,0.285714285714286,0.297961045722762),.UNSPECIFIED.)
GEOMETRIC_REPRESENTATION_ITEM()
RATIONAL_B_SPLINE_SURFACE(((0.996566619267862,0.996566619267862,0.996566619267862,
0.998146249162902,1.,0.995701274206111,0.992876621380142),(0.996566619267862,
0.996566619267862,0.996566619267862,0.998146249162902,1.,0.995701274206111,
0.992876621380142)))
REPRESENTATION_ITEM('')
SURFACE()
);
#960=(
BOUNDED_SURFACE()
B_SPLINE_SURFACE(1,2,((#109905,#109906,#109907),(#109908,#109909,#109910)),
 .UNSPECIFIED.,.F.,.F.,.F.)
B_SPLINE_SURFACE_WITH_KNOTS((2,2),(3,3),(0.710318915640002,1.),(0.435672122597671,
0.452924869174518),.UNSPECIFIED.)
GEOMETRIC_REPRESENTATION_ITEM()
RATIONAL_B_SPLINE_SURFACE(((0.995510721093621,0.990658873102333,0.988732477628005),
(0.995510721093621,0.990658873102333,0.988732477628005)))
REPRESENTATION_ITEM('')
SURFACE()
);
#961=(
BOUNDED_SURFACE()
B_SPLINE_SURFACE(1,2,((#109921,#109922,#109923,#109924,#109925,#109926,
#109927),(#109928,#109929,#109930,#109931,#109932,#109933,#109934)),
 .UNSPECIFIED.,.F.,.F.,.F.)
B_SPLINE_SURFACE_WITH_KNOTS((2,2),(3,2,2,3),(0.710192959008365,1.),(0.280257803540344,
0.280433083165912,0.285714285714286,0.297961045722762),.UNSPECIFIED.)
GEOMETRIC_REPRESENTATION_ITEM()
RATIONAL_B_SPLINE_SURFACE(((0.996566619267863,0.996566619267863,0.996566619267863,
0.998146249162903,1.,0.995701274206111,0.992876621380142),(0.996566619267863,
0.996566619267863,0.996566619267863,0.998146249162903,1.,0.995701274206111,
0.992876621380142)))
REPRESENTATION_ITEM('')
SURFACE()
);
#962=(
BOUNDED_SURFACE()
B_SPLINE_SURFACE(1,2,((#109948,#109949,#109950),(#109951,#109952,#109953)),
 .UNSPECIFIED.,.F.,.F.,.F.)
B_SPLINE_SURFACE_WITH_KNOTS((2,2),(3,3),(0.71031891563941,1.),(0.435672122597671,
0.452924869174518),.UNSPECIFIED.)
GEOMETRIC_REPRESENTATION_ITEM()
RATIONAL_B_SPLINE_SURFACE(((0.995510721093621,0.990658873102333,0.988732477628005),
(0.995510721093621,0.990658873102333,0.988732477628005)))
REPRESENTATION_ITEM('')
SURFACE()
);
#963=(
BOUNDED_SURFACE()
B_SPLINE_SURFACE(1,2,((#109964,#109965,#109966,#109967,#109968,#109969,
#109970),(#109971,#109972,#109973,#109974,#109975,#109976,#109977)),
 .UNSPECIFIED.,.F.,.F.,.F.)
B_SPLINE_SURFACE_WITH_KNOTS((2,2),(3,2,2,3),(0.71019295900777,1.),(0.280257803540344,
0.280433083165912,0.285714285714286,0.297961045722762),.UNSPECIFIED.)
GEOMETRIC_REPRESENTATION_ITEM()
RATIONAL_B_SPLINE_SURFACE(((0.996566619267863,0.996566619267863,0.996566619267863,
0.998146249162903,1.,0.995701274206111,0.992876621380142),(0.996566619267863,
0.996566619267863,0.996566619267863,0.998146249162903,1.,0.995701274206111,
0.992876621380142)))
REPRESENTATION_ITEM('')
SURFACE()
);
#964=(
BOUNDED_SURFACE()
B_SPLINE_SURFACE(1,2,((#109991,#109992,#109993),(#109994,#109995,#109996)),
 .UNSPECIFIED.,.F.,.F.,.F.)
B_SPLINE_SURFACE_WITH_KNOTS((2,2),(3,3),(0.710318915639997,1.),(0.435672122597671,
0.452924869174518),.UNSPECIFIED.)
GEOMETRIC_REPRESENTATION_ITEM()
RATIONAL_B_SPLINE_SURFACE(((0.995510721093621,0.990658873102333,0.988732477628005),
(0.995510721093621,0.990658873102333,0.988732477628005)))
REPRESENTATION_ITEM('')
SURFACE()
);
#965=(
BOUNDED_SURFACE()
B_SPLINE_SURFACE(1,2,((#110007,#110008,#110009,#110010,#110011,#110012,
#110013),(#110014,#110015,#110016,#110017,#110018,#110019,#110020)),
 .UNSPECIFIED.,.F.,.F.,.F.)
B_SPLINE_SURFACE_WITH_KNOTS((2,2),(3,2,2,3),(0.710192959008358,1.),(0.280257803540343,
0.280433083165911,0.285714285714286,0.297961045722762),.UNSPECIFIED.)
GEOMETRIC_REPRESENTATION_ITEM()
RATIONAL_B_SPLINE_SURFACE(((0.996566619267862,0.996566619267862,0.996566619267862,
0.998146249162902,1.,0.995701274206111,0.992876621380142),(0.996566619267862,
0.996566619267862,0.996566619267862,0.998146249162902,1.,0.995701274206111,
0.992876621380142)))
REPRESENTATION_ITEM('')
SURFACE()
);
#966=(
BOUNDED_SURFACE()
B_SPLINE_SURFACE(1,2,((#110034,#110035,#110036),(#110037,#110038,#110039)),
 .UNSPECIFIED.,.F.,.F.,.F.)
B_SPLINE_SURFACE_WITH_KNOTS((2,2),(3,3),(0.710318915639496,1.),(0.435672122597671,
0.452924869174518),.UNSPECIFIED.)
GEOMETRIC_REPRESENTATION_ITEM()
RATIONAL_B_SPLINE_SURFACE(((0.995510721093621,0.990658873102333,0.988732477628005),
(0.995510721093621,0.990658873102333,0.988732477628005)))
REPRESENTATION_ITEM('')
SURFACE()
);
#967=(
BOUNDED_SURFACE()
B_SPLINE_SURFACE(1,2,((#110050,#110051,#110052,#110053,#110054,#110055,
#110056),(#110057,#110058,#110059,#110060,#110061,#110062,#110063)),
 .UNSPECIFIED.,.F.,.F.,.F.)
B_SPLINE_SURFACE_WITH_KNOTS((2,2),(3,2,2,3),(0.710192959007859,1.),(0.280257803540344,
0.280433083165912,0.285714285714286,0.297961045722762),.UNSPECIFIED.)
GEOMETRIC_REPRESENTATION_ITEM()
RATIONAL_B_SPLINE_SURFACE(((0.996566619267862,0.996566619267862,0.996566619267862,
0.998146249162902,1.,0.995701274206111,0.992876621380142),(0.996566619267862,
0.996566619267862,0.996566619267862,0.998146249162902,1.,0.995701274206111,
0.992876621380142)))
REPRESENTATION_ITEM('')
SURFACE()
);
#968=(
BOUNDED_SURFACE()
B_SPLINE_SURFACE(1,2,((#110077,#110078,#110079),(#110080,#110081,#110082)),
 .UNSPECIFIED.,.F.,.F.,.F.)
B_SPLINE_SURFACE_WITH_KNOTS((2,2),(3,3),(0.71031891563999,1.),(0.435672122597671,
0.452924869174518),.UNSPECIFIED.)
GEOMETRIC_REPRESENTATION_ITEM()
RATIONAL_B_SPLINE_SURFACE(((0.995510721093621,0.990658873102333,0.988732477628005),
(0.995510721093621,0.990658873102333,0.988732477628005)))
REPRESENTATION_ITEM('')
SURFACE()
);
#969=(
BOUNDED_SURFACE()
B_SPLINE_SURFACE(1,2,((#110093,#110094,#110095,#110096,#110097,#110098,
#110099),(#110100,#110101,#110102,#110103,#110104,#110105,#110106)),
 .UNSPECIFIED.,.F.,.F.,.F.)
B_SPLINE_SURFACE_WITH_KNOTS((2,2),(3,2,2,3),(0.710192959008352,1.),(0.280257803540344,
0.280433083165912,0.285714285714286,0.297961045722762),.UNSPECIFIED.)
GEOMETRIC_REPRESENTATION_ITEM()
RATIONAL_B_SPLINE_SURFACE(((0.996566619267863,0.996566619267863,0.996566619267863,
0.998146249162902,1.,0.995701274206111,0.992876621380142),(0.996566619267863,
0.996566619267863,0.996566619267863,0.998146249162902,1.,0.995701274206111,
0.992876621380142)))
REPRESENTATION_ITEM('')
SURFACE()
);
#970=(
BOUNDED_SURFACE()
B_SPLINE_SURFACE(1,2,((#110120,#110121,#110122),(#110123,#110124,#110125)),
 .UNSPECIFIED.,.F.,.F.,.F.)
B_SPLINE_SURFACE_WITH_KNOTS((2,2),(3,3),(0.710318915639497,1.),(0.435672122597671,
0.452924869174518),.UNSPECIFIED.)
GEOMETRIC_REPRESENTATION_ITEM()
RATIONAL_B_SPLINE_SURFACE(((0.995510721093621,0.990658873102333,0.988732477628005),
(0.995510721093621,0.990658873102333,0.988732477628005)))
REPRESENTATION_ITEM('')
SURFACE()
);
#971=(
BOUNDED_SURFACE()
B_SPLINE_SURFACE(1,2,((#110136,#110137,#110138,#110139,#110140,#110141,
#110142),(#110143,#110144,#110145,#110146,#110147,#110148,#110149)),
 .UNSPECIFIED.,.F.,.F.,.F.)
B_SPLINE_SURFACE_WITH_KNOTS((2,2),(3,2,2,3),(0.710192959007853,1.),(0.280257803540344,
0.280433083165912,0.285714285714286,0.297961045722762),.UNSPECIFIED.)
GEOMETRIC_REPRESENTATION_ITEM()
RATIONAL_B_SPLINE_SURFACE(((0.996566619267863,0.996566619267863,0.996566619267863,
0.998146249162902,1.,0.995701274206111,0.992876621380142),(0.996566619267863,
0.996566619267863,0.996566619267863,0.998146249162902,1.,0.995701274206111,
0.992876621380142)))
REPRESENTATION_ITEM('')
SURFACE()
);
#972=(
BOUNDED_SURFACE()
B_SPLINE_SURFACE(1,2,((#110163,#110164,#110165),(#110166,#110167,#110168)),
 .UNSPECIFIED.,.F.,.F.,.F.)
B_SPLINE_SURFACE_WITH_KNOTS((2,2),(3,3),(0.710318915639716,1.),(0.435672122597671,
0.452924869174518),.UNSPECIFIED.)
GEOMETRIC_REPRESENTATION_ITEM()
RATIONAL_B_SPLINE_SURFACE(((0.995510721093621,0.990658873102333,0.988732477628005),
(0.995510721093621,0.990658873102333,0.988732477628005)))
REPRESENTATION_ITEM('')
SURFACE()
);
#973=(
BOUNDED_SURFACE()
B_SPLINE_SURFACE(1,2,((#110179,#110180,#110181,#110182,#110183,#110184,
#110185),(#110186,#110187,#110188,#110189,#110190,#110191,#110192)),
 .UNSPECIFIED.,.F.,.F.,.F.)
B_SPLINE_SURFACE_WITH_KNOTS((2,2),(3,2,2,3),(0.71019295900808,1.),(0.280257803540343,
0.280433083165911,0.285714285714286,0.297961045722762),.UNSPECIFIED.)
GEOMETRIC_REPRESENTATION_ITEM()
RATIONAL_B_SPLINE_SURFACE(((0.996566619267862,0.996566619267862,0.996566619267862,
0.998146249162902,1.,0.995701274206111,0.992876621380142),(0.996566619267862,
0.996566619267862,0.996566619267862,0.998146249162902,1.,0.995701274206111,
0.992876621380142)))
REPRESENTATION_ITEM('')
SURFACE()
);
#974=(
BOUNDED_SURFACE()
B_SPLINE_SURFACE(1,2,((#110206,#110207,#110208),(#110209,#110210,#110211)),
 .UNSPECIFIED.,.F.,.F.,.F.)
B_SPLINE_SURFACE_WITH_KNOTS((2,2),(3,3),(0.710318915638671,1.),(0.435672122597671,
0.452924869174518),.UNSPECIFIED.)
GEOMETRIC_REPRESENTATION_ITEM()
RATIONAL_B_SPLINE_SURFACE(((0.995510721093621,0.990658873102333,0.988732477628005),
(0.995510721093621,0.990658873102333,0.988732477628005)))
REPRESENTATION_ITEM('')
SURFACE()
);
#975=(
BOUNDED_SURFACE()
B_SPLINE_SURFACE(1,2,((#110222,#110223,#110224,#110225,#110226,#110227,
#110228),(#110229,#110230,#110231,#110232,#110233,#110234,#110235)),
 .UNSPECIFIED.,.F.,.F.,.F.)
B_SPLINE_SURFACE_WITH_KNOTS((2,2),(3,2,2,3),(0.710192959007032,1.),(0.280257803540344,
0.280433083165912,0.285714285714286,0.297961045722762),.UNSPECIFIED.)
GEOMETRIC_REPRESENTATION_ITEM()
RATIONAL_B_SPLINE_SURFACE(((0.996566619267863,0.996566619267863,0.996566619267863,
0.998146249162902,1.,0.995701274206111,0.992876621380142),(0.996566619267863,
0.996566619267863,0.996566619267863,0.998146249162902,1.,0.995701274206111,
0.992876621380142)))
REPRESENTATION_ITEM('')
SURFACE()
);
#976=(
BOUNDED_SURFACE()
B_SPLINE_SURFACE(1,2,((#110249,#110250,#110251),(#110252,#110253,#110254)),
 .UNSPECIFIED.,.F.,.F.,.F.)
B_SPLINE_SURFACE_WITH_KNOTS((2,2),(3,3),(0.710318915639955,1.),(0.435672122597508,
0.452924869174518),.UNSPECIFIED.)
GEOMETRIC_REPRESENTATION_ITEM()
RATIONAL_B_SPLINE_SURFACE(((0.995510721093713,0.990658873102351,0.988732477628005),
(0.995510721093713,0.990658873102351,0.988732477628005)))
REPRESENTATION_ITEM('')
SURFACE()
);
#977=(
BOUNDED_SURFACE()
B_SPLINE_SURFACE(1,2,((#110265,#110266,#110267,#110268,#110269,#110270,
#110271),(#110272,#110273,#110274,#110275,#110276,#110277,#110278)),
 .UNSPECIFIED.,.F.,.F.,.F.)
B_SPLINE_SURFACE_WITH_KNOTS((2,2),(3,2,2,3),(0.710192959008314,1.),(0.280257803540344,
0.280433083165912,0.285714285714286,0.29796104572276),.UNSPECIFIED.)
GEOMETRIC_REPRESENTATION_ITEM()
RATIONAL_B_SPLINE_SURFACE(((0.996566619267863,0.996566619267863,0.996566619267863,
0.998146249162903,1.,0.995701274206112,0.992876621380143),(0.996566619267863,
0.996566619267863,0.996566619267863,0.998146249162903,1.,0.995701274206112,
0.992876621380143)))
REPRESENTATION_ITEM('')
SURFACE()
);
#978=(
BOUNDED_SURFACE()
B_SPLINE_SURFACE(1,2,((#110292,#110293,#110294),(#110295,#110296,#110297)),
 .UNSPECIFIED.,.F.,.F.,.F.)
B_SPLINE_SURFACE_WITH_KNOTS((2,2),(3,3),(0.710318915640075,1.),(0.435672122597671,
0.452924869174518),.UNSPECIFIED.)
GEOMETRIC_REPRESENTATION_ITEM()
RATIONAL_B_SPLINE_SURFACE(((0.995510721093621,0.990658873102333,0.988732477628005),
(0.995510721093621,0.990658873102333,0.988732477628005)))
REPRESENTATION_ITEM('')
SURFACE()
);
#979=(
BOUNDED_SURFACE()
B_SPLINE_SURFACE(1,2,((#110308,#110309,#110310,#110311,#110312,#110313,
#110314),(#110315,#110316,#110317,#110318,#110319,#110320,#110321)),
 .UNSPECIFIED.,.F.,.F.,.F.)
B_SPLINE_SURFACE_WITH_KNOTS((2,2),(3,2,2,3),(0.710192959008435,1.),(0.280257803540343,
0.280433083165911,0.285714285714286,0.297961045722762),.UNSPECIFIED.)
GEOMETRIC_REPRESENTATION_ITEM()
RATIONAL_B_SPLINE_SURFACE(((0.996566619267862,0.996566619267862,0.996566619267862,
0.998146249162902,1.,0.995701274206111,0.992876621380142),(0.996566619267862,
0.996566619267862,0.996566619267862,0.998146249162902,1.,0.995701274206111,
0.992876621380142)))
REPRESENTATION_ITEM('')
SURFACE()
);
#980=(
BOUNDED_SURFACE()
B_SPLINE_SURFACE(1,2,((#110335,#110336,#110337),(#110338,#110339,#110340)),
 .UNSPECIFIED.,.F.,.F.,.F.)
B_SPLINE_SURFACE_WITH_KNOTS((2,2),(3,3),(0.710318915639446,1.),(0.4356721225975,
0.452924869174518),.UNSPECIFIED.)
GEOMETRIC_REPRESENTATION_ITEM()
RATIONAL_B_SPLINE_SURFACE(((0.995510721093717,0.990658873102352,0.988732477628005),
(0.995510721093717,0.990658873102352,0.988732477628005)))
REPRESENTATION_ITEM('')
SURFACE()
);
#981=(
BOUNDED_SURFACE()
B_SPLINE_SURFACE(1,2,((#110351,#110352,#110353,#110354,#110355,#110356,
#110357),(#110358,#110359,#110360,#110361,#110362,#110363,#110364)),
 .UNSPECIFIED.,.F.,.F.,.F.)
B_SPLINE_SURFACE_WITH_KNOTS((2,2),(3,2,2,3),(0.710192959007802,1.),(0.280257803540344,
0.280433083165912,0.285714285714286,0.297961045722762),.UNSPECIFIED.)
GEOMETRIC_REPRESENTATION_ITEM()
RATIONAL_B_SPLINE_SURFACE(((0.996566619267863,0.996566619267863,0.996566619267863,
0.998146249162902,1.,0.995701274206111,0.992876621380142),(0.996566619267863,
0.996566619267863,0.996566619267863,0.998146249162902,1.,0.995701274206111,
0.992876621380142)))
REPRESENTATION_ITEM('')
SURFACE()
);
#982=(
BOUNDED_SURFACE()
B_SPLINE_SURFACE(1,2,((#110378,#110379,#110380),(#110381,#110382,#110383)),
 .UNSPECIFIED.,.F.,.F.,.F.)
B_SPLINE_SURFACE_WITH_KNOTS((2,2),(3,3),(0.71031891564008,1.),(0.435672122597573,
0.452924869174518),.UNSPECIFIED.)
GEOMETRIC_REPRESENTATION_ITEM()
RATIONAL_B_SPLINE_SURFACE(((0.995510721093677,0.990658873102344,0.988732477628005),
(0.995510721093677,0.990658873102344,0.988732477628005)))
REPRESENTATION_ITEM('')
SURFACE()
);
#983=(
BOUNDED_SURFACE()
B_SPLINE_SURFACE(1,2,((#110394,#110395,#110396,#110397,#110398,#110399,
#110400),(#110401,#110402,#110403,#110404,#110405,#110406,#110407)),
 .UNSPECIFIED.,.F.,.F.,.F.)
B_SPLINE_SURFACE_WITH_KNOTS((2,2),(3,2,2,3),(0.710192959008442,1.),(0.280257803540345,
0.280433083165913,0.285714285714286,0.297961045722762),.UNSPECIFIED.)
GEOMETRIC_REPRESENTATION_ITEM()
RATIONAL_B_SPLINE_SURFACE(((0.996566619267863,0.996566619267863,0.996566619267863,
0.998146249162903,1.,0.995701274206111,0.992876621380142),(0.996566619267863,
0.996566619267863,0.996566619267863,0.998146249162903,1.,0.995701274206111,
0.992876621380142)))
REPRESENTATION_ITEM('')
SURFACE()
);
#984=(
BOUNDED_SURFACE()
B_SPLINE_SURFACE(1,2,((#110421,#110422,#110423),(#110424,#110425,#110426)),
 .UNSPECIFIED.,.F.,.F.,.F.)
B_SPLINE_SURFACE_WITH_KNOTS((2,2),(3,3),(0.710318915638947,1.),(0.435672122597671,
0.452924869174518),.UNSPECIFIED.)
GEOMETRIC_REPRESENTATION_ITEM()
RATIONAL_B_SPLINE_SURFACE(((0.995510721093621,0.990658873102333,0.988732477628005),
(0.995510721093621,0.990658873102333,0.988732477628005)))
REPRESENTATION_ITEM('')
SURFACE()
);
#985=(
BOUNDED_SURFACE()
B_SPLINE_SURFACE(1,2,((#110437,#110438,#110439,#110440,#110441,#110442,
#110443),(#110444,#110445,#110446,#110447,#110448,#110449,#110450)),
 .UNSPECIFIED.,.F.,.F.,.F.)
B_SPLINE_SURFACE_WITH_KNOTS((2,2),(3,2,2,3),(0.710192959007306,1.),(0.280257803540345,
0.280433083165913,0.285714285714286,0.297961045722762),.UNSPECIFIED.)
GEOMETRIC_REPRESENTATION_ITEM()
RATIONAL_B_SPLINE_SURFACE(((0.996566619267863,0.996566619267863,0.996566619267863,
0.998146249162903,1.,0.995701274206111,0.992876621380142),(0.996566619267863,
0.996566619267863,0.996566619267863,0.998146249162903,1.,0.995701274206111,
0.992876621380142)))
REPRESENTATION_ITEM('')
SURFACE()
);
#986=(
BOUNDED_SURFACE()
B_SPLINE_SURFACE(1,2,((#110464,#110465,#110466),(#110467,#110468,#110469)),
 .UNSPECIFIED.,.F.,.F.,.F.)
B_SPLINE_SURFACE_WITH_KNOTS((2,2),(3,3),(0.710318915639103,1.),(0.435672122597161,
0.452924869174518),.UNSPECIFIED.)
GEOMETRIC_REPRESENTATION_ITEM()
RATIONAL_B_SPLINE_SURFACE(((0.995510721093908,0.99065887310239,0.988732477628006),
(0.995510721093908,0.99065887310239,0.988732477628006)))
REPRESENTATION_ITEM('')
SURFACE()
);
#987=(
BOUNDED_SURFACE()
B_SPLINE_SURFACE(1,2,((#110480,#110481,#110482,#110483,#110484,#110485,
#110486),(#110487,#110488,#110489,#110490,#110491,#110492,#110493)),
 .UNSPECIFIED.,.F.,.F.,.F.)
B_SPLINE_SURFACE_WITH_KNOTS((2,2),(3,2,2,3),(0.710192959007465,1.),(0.280257803540345,
0.280433083165913,0.285714285714286,0.29796104572276),.UNSPECIFIED.)
GEOMETRIC_REPRESENTATION_ITEM()
RATIONAL_B_SPLINE_SURFACE(((0.996566619267863,0.996566619267863,0.996566619267863,
0.998146249162903,1.,0.995701274206112,0.992876621380143),(0.996566619267863,
0.996566619267863,0.996566619267863,0.998146249162903,1.,0.995701274206112,
0.992876621380143)))
REPRESENTATION_ITEM('')
SURFACE()
);
#988=(
BOUNDED_SURFACE()
B_SPLINE_SURFACE(1,2,((#110507,#110508,#110509),(#110510,#110511,#110512)),
 .UNSPECIFIED.,.F.,.F.,.F.)
B_SPLINE_SURFACE_WITH_KNOTS((2,2),(3,3),(0.710318915638374,1.),(0.435672122597297,
0.452924869174625),.UNSPECIFIED.)
GEOMETRIC_REPRESENTATION_ITEM()
RATIONAL_B_SPLINE_SURFACE(((0.995510721093831,0.990658873102344,0.988732477627981),
(0.995510721093832,0.990658873102344,0.988732477627981)))
REPRESENTATION_ITEM('')
SURFACE()
);
#989=(
BOUNDED_SURFACE()
B_SPLINE_SURFACE(1,2,((#110523,#110524,#110525,#110526,#110527,#110528,
#110529),(#110530,#110531,#110532,#110533,#110534,#110535,#110536)),
 .UNSPECIFIED.,.F.,.F.,.F.)
B_SPLINE_SURFACE_WITH_KNOTS((2,2),(3,2,2,3),(0.710192959006739,1.),(0.280257803540345,
0.280433083165913,0.285714285714286,0.29796104572276),.UNSPECIFIED.)
GEOMETRIC_REPRESENTATION_ITEM()
RATIONAL_B_SPLINE_SURFACE(((0.996566619267863,0.996566619267863,0.996566619267863,
0.998146249162903,1.,0.995701274206112,0.992876621380143),(0.996566619267863,
0.996566619267863,0.996566619267863,0.998146249162903,1.,0.995701274206112,
0.992876621380143)))
REPRESENTATION_ITEM('')
SURFACE()
);
#990=(
BOUNDED_SURFACE()
B_SPLINE_SURFACE(1,2,((#110550,#110551,#110552),(#110553,#110554,#110555)),
 .UNSPECIFIED.,.F.,.F.,.F.)
B_SPLINE_SURFACE_WITH_KNOTS((2,2),(3,3),(0.710318915639878,1.),(0.435672122597669,
0.452924869174794),.UNSPECIFIED.)
GEOMETRIC_REPRESENTATION_ITEM()
RATIONAL_B_SPLINE_SURFACE(((0.995510721093622,0.990658873102255,0.988732477627944),
(0.995510721093622,0.990658873102255,0.988732477627944)))
REPRESENTATION_ITEM('')
SURFACE()
);
#991=(
BOUNDED_SURFACE()
B_SPLINE_SURFACE(1,2,((#110566,#110567,#110568,#110569,#110570,#110571,
#110572),(#110573,#110574,#110575,#110576,#110577,#110578,#110579)),
 .UNSPECIFIED.,.F.,.F.,.F.)
B_SPLINE_SURFACE_WITH_KNOTS((2,2),(3,2,2,3),(0.710192959008237,1.),(0.280257803540345,
0.280433083165913,0.285714285714286,0.297961045722762),.UNSPECIFIED.)
GEOMETRIC_REPRESENTATION_ITEM()
RATIONAL_B_SPLINE_SURFACE(((0.996566619267863,0.996566619267863,0.996566619267863,
0.998146249162903,1.,0.995701274206111,0.992876621380142),(0.996566619267863,
0.996566619267863,0.996566619267863,0.998146249162903,1.,0.995701274206111,
0.992876621380142)))
REPRESENTATION_ITEM('')
SURFACE()
);
#992=(
BOUNDED_SURFACE()
B_SPLINE_SURFACE(1,2,((#110593,#110594,#110595),(#110596,#110597,#110598)),
 .UNSPECIFIED.,.F.,.F.,.F.)
B_SPLINE_SURFACE_WITH_KNOTS((2,2),(3,3),(0.710318915638592,1.),(0.435672122597671,
0.452924869174518),.UNSPECIFIED.)
GEOMETRIC_REPRESENTATION_ITEM()
RATIONAL_B_SPLINE_SURFACE(((0.995510721093621,0.990658873102333,0.988732477628005),
(0.995510721093621,0.990658873102333,0.988732477628005)))
REPRESENTATION_ITEM('')
SURFACE()
);
#993=(
BOUNDED_SURFACE()
B_SPLINE_SURFACE(1,2,((#110609,#110610,#110611,#110612,#110613,#110614,
#110615),(#110616,#110617,#110618,#110619,#110620,#110621,#110622)),
 .UNSPECIFIED.,.F.,.F.,.F.)
B_SPLINE_SURFACE_WITH_KNOTS((2,2),(3,2,2,3),(0.710192959006951,1.),(0.280257803540345,
0.280433083165913,0.285714285714286,0.297961045722762),.UNSPECIFIED.)
GEOMETRIC_REPRESENTATION_ITEM()
RATIONAL_B_SPLINE_SURFACE(((0.996566619267863,0.996566619267863,0.996566619267863,
0.998146249162903,1.,0.995701274206111,0.992876621380142),(0.996566619267863,
0.996566619267863,0.996566619267863,0.998146249162903,1.,0.995701274206111,
0.992876621380142)))
REPRESENTATION_ITEM('')
SURFACE()
);
#994=(
BOUNDED_SURFACE()
B_SPLINE_SURFACE(1,2,((#110636,#110637,#110638),(#110639,#110640,#110641)),
 .UNSPECIFIED.,.F.,.F.,.F.)
B_SPLINE_SURFACE_WITH_KNOTS((2,2),(3,3),(0.710318915638846,1.),(0.435672122597539,
0.452924869174518),.UNSPECIFIED.)
GEOMETRIC_REPRESENTATION_ITEM()
RATIONAL_B_SPLINE_SURFACE(((0.995510721093696,0.990658873102347,0.988732477628005),
(0.995510721093696,0.990658873102347,0.988732477628005)))
REPRESENTATION_ITEM('')
SURFACE()
);
#995=(
BOUNDED_SURFACE()
B_SPLINE_SURFACE(1,2,((#110652,#110653,#110654,#110655,#110656,#110657,
#110658),(#110659,#110660,#110661,#110662,#110663,#110664,#110665)),
 .UNSPECIFIED.,.F.,.F.,.F.)
B_SPLINE_SURFACE_WITH_KNOTS((2,2),(3,2,2,3),(0.710192959007199,1.),(0.280257803540345,
0.280433083165913,0.285714285714286,0.297961045722762),.UNSPECIFIED.)
GEOMETRIC_REPRESENTATION_ITEM()
RATIONAL_B_SPLINE_SURFACE(((0.996566619267863,0.996566619267863,0.996566619267863,
0.998146249162903,1.,0.995701274206111,0.992876621380142),(0.996566619267863,
0.996566619267863,0.996566619267863,0.998146249162903,1.,0.995701274206111,
0.992876621380142)))
REPRESENTATION_ITEM('')
SURFACE()
);
#996=(
BOUNDED_SURFACE()
B_SPLINE_SURFACE(1,2,((#110679,#110680,#110681),(#110682,#110683,#110684)),
 .UNSPECIFIED.,.F.,.F.,.F.)
B_SPLINE_SURFACE_WITH_KNOTS((2,2),(3,3),(0.710318915639085,1.),(0.435672122597353,
0.452924869174518),.UNSPECIFIED.)
GEOMETRIC_REPRESENTATION_ITEM()
RATIONAL_B_SPLINE_SURFACE(((0.9955107210938,0.990658873102368,0.988732477628005),
(0.9955107210938,0.990658873102368,0.988732477628005)))
REPRESENTATION_ITEM('')
SURFACE()
);
#997=(
BOUNDED_SURFACE()
B_SPLINE_SURFACE(1,2,((#110695,#110696,#110697,#110698,#110699,#110700,
#110701),(#110702,#110703,#110704,#110705,#110706,#110707,#110708)),
 .UNSPECIFIED.,.F.,.F.,.F.)
B_SPLINE_SURFACE_WITH_KNOTS((2,2),(3,2,2,3),(0.71019295900744,1.),(0.280257803540346,
0.280433083165913,0.285714285714286,0.297961045722604),.UNSPECIFIED.)
GEOMETRIC_REPRESENTATION_ITEM()
RATIONAL_B_SPLINE_SURFACE(((0.996566619267863,0.996566619267863,0.996566619267863,
0.998146249162903,1.,0.995701274206166,0.992876621380215),(0.996566619267863,
0.996566619267863,0.996566619267863,0.998146249162903,1.,0.995701274206166,
0.992876621380215)))
REPRESENTATION_ITEM('')
SURFACE()
);
#998=(
BOUNDED_SURFACE()
B_SPLINE_SURFACE(1,2,((#110722,#110723,#110724),(#110725,#110726,#110727)),
 .UNSPECIFIED.,.F.,.F.,.F.)
B_SPLINE_SURFACE_WITH_KNOTS((2,2),(3,3),(0.710318915639152,1.),(0.435672122597622,
0.452924869174518),.UNSPECIFIED.)
GEOMETRIC_REPRESENTATION_ITEM()
RATIONAL_B_SPLINE_SURFACE(((0.995510721093649,0.990658873102338,0.988732477628005),
(0.995510721093649,0.990658873102338,0.988732477628005)))
REPRESENTATION_ITEM('')
SURFACE()
);
#999=(
BOUNDED_SURFACE()
B_SPLINE_SURFACE(1,2,((#110738,#110739,#110740,#110741,#110742,#110743,
#110744),(#110745,#110746,#110747,#110748,#110749,#110750,#110751)),
 .UNSPECIFIED.,.F.,.F.,.F.)
B_SPLINE_SURFACE_WITH_KNOTS((2,2),(3,2,2,3),(0.710192959007518,1.),(0.280257803540345,
0.280433083165913,0.285714285714286,0.297961045722762),.UNSPECIFIED.)
GEOMETRIC_REPRESENTATION_ITEM()
RATIONAL_B_SPLINE_SURFACE(((0.996566619267863,0.996566619267863,0.996566619267863,
0.998146249162903,1.,0.995701274206111,0.992876621380142),(0.996566619267863,
0.996566619267863,0.996566619267863,0.998146249162903,1.,0.995701274206111,
0.992876621380142)))
REPRESENTATION_ITEM('')
SURFACE()
);
#1000=(
BOUNDED_SURFACE()
B_SPLINE_SURFACE(1,2,((#110765,#110766,#110767),(#110768,#110769,#110770)),
 .UNSPECIFIED.,.F.,.F.,.F.)
B_SPLINE_SURFACE_WITH_KNOTS((2,2),(3,3),(0.710318915638835,1.),(0.4356721225973,
0.452924869174518),.UNSPECIFIED.)
GEOMETRIC_REPRESENTATION_ITEM()
RATIONAL_B_SPLINE_SURFACE(((0.99551072109383,0.990658873102374,0.988732477628005),
(0.99551072109383,0.990658873102374,0.988732477628005)))
REPRESENTATION_ITEM('')
SURFACE()
);
#1001=(
BOUNDED_SURFACE()
B_SPLINE_SURFACE(1,2,((#110781,#110782,#110783,#110784,#110785,#110786,
#110787),(#110788,#110789,#110790,#110791,#110792,#110793,#110794)),
 .UNSPECIFIED.,.F.,.F.,.F.)
B_SPLINE_SURFACE_WITH_KNOTS((2,2),(3,2,2,3),(0.710192959006289,1.),(0.280257803540335,
0.280433083165902,0.285714285714286,0.297961045722673),.UNSPECIFIED.)
GEOMETRIC_REPRESENTATION_ITEM()
RATIONAL_B_SPLINE_SURFACE(((0.996566619267857,0.996566619267857,0.996566619267857,
0.998146249162899,1.,0.995701274206142,0.992876621380183),(0.996566619267857,
0.996566619267857,0.996566619267857,0.998146249162899,1.,0.995701274206142,
0.992876621380183)))
REPRESENTATION_ITEM('')
SURFACE()
);
#1002=(
BOUNDED_SURFACE()
B_SPLINE_SURFACE(1,2,((#110808,#110809,#110810),(#110811,#110812,#110813)),
 .UNSPECIFIED.,.F.,.F.,.F.)
B_SPLINE_SURFACE_WITH_KNOTS((2,2),(3,3),(0.710318915638985,1.),(0.435672122597532,
0.452924869174518),.UNSPECIFIED.)
GEOMETRIC_REPRESENTATION_ITEM()
RATIONAL_B_SPLINE_SURFACE(((0.9955107210937,0.990658873102348,0.988732477628005),
(0.9955107210937,0.990658873102348,0.988732477628005)))
REPRESENTATION_ITEM('')
SURFACE()
);
#1003=(
BOUNDED_SURFACE()
B_SPLINE_SURFACE(1,2,((#110824,#110825,#110826,#110827,#110828,#110829,
#110830),(#110831,#110832,#110833,#110834,#110835,#110836,#110837)),
 .UNSPECIFIED.,.F.,.F.,.F.)
B_SPLINE_SURFACE_WITH_KNOTS((2,2),(3,2,2,3),(0.710192959007348,1.),(0.280257803540345,
0.280433083165913,0.285714285714286,0.29796104572276),.UNSPECIFIED.)
GEOMETRIC_REPRESENTATION_ITEM()
RATIONAL_B_SPLINE_SURFACE(((0.996566619267863,0.996566619267863,0.996566619267863,
0.998146249162903,1.,0.995701274206112,0.992876621380143),(0.996566619267863,
0.996566619267863,0.996566619267863,0.998146249162903,1.,0.995701274206112,
0.992876621380143)))
REPRESENTATION_ITEM('')
SURFACE()
);
#1004=(
BOUNDED_SURFACE()
B_SPLINE_SURFACE(1,2,((#110851,#110852,#110853),(#110854,#110855,#110856)),
 .UNSPECIFIED.,.F.,.F.,.F.)
B_SPLINE_SURFACE_WITH_KNOTS((2,2),(3,3),(0.710318915638962,1.),(0.435672122597216,
0.452924869174518),.UNSPECIFIED.)
GEOMETRIC_REPRESENTATION_ITEM()
RATIONAL_B_SPLINE_SURFACE(((0.995510721093877,0.990658873102383,0.988732477628005),
(0.995510721093877,0.990658873102383,0.988732477628005)))
REPRESENTATION_ITEM('')
SURFACE()
);
#1005=(
BOUNDED_SURFACE()
B_SPLINE_SURFACE(1,2,((#110867,#110868,#110869,#110870,#110871,#110872,
#110873),(#110874,#110875,#110876,#110877,#110878,#110879,#110880)),
 .UNSPECIFIED.,.F.,.F.,.F.)
B_SPLINE_SURFACE_WITH_KNOTS((2,2),(3,2,2,3),(0.710192959007327,1.),(0.280257803540346,
0.280433083165913,0.285714285714286,0.297961045722661),.UNSPECIFIED.)
GEOMETRIC_REPRESENTATION_ITEM()
RATIONAL_B_SPLINE_SURFACE(((0.996566619267863,0.996566619267863,0.996566619267863,
0.998146249162903,1.,0.995701274206146,0.992876621380189),(0.996566619267863,
0.996566619267863,0.996566619267863,0.998146249162903,1.,0.995701274206146,
0.992876621380189)))
REPRESENTATION_ITEM('')
SURFACE()
);
#1006=(
BOUNDED_SURFACE()
B_SPLINE_SURFACE(1,2,((#110894,#110895,#110896,#110897,#110898),(#110899,
#110900,#110901,#110902,#110903)),.UNSPECIFIED.,.F.,.F.,.F.)
B_SPLINE_SURFACE_WITH_KNOTS((2,2),(3,2,3),(0.709594768913623,1.),(0.40044464506204,
0.401042835325431,0.418415696246127),.UNSPECIFIED.)
GEOMETRIC_REPRESENTATION_ITEM()
RATIONAL_B_SPLINE_SURFACE(((0.988122504062136,0.988122504062136,0.988122504062136,
0.989520169850094,0.993884164197535),(0.988122504062136,0.988122504062136,
0.988122504062136,0.989520169850094,0.993884164197535)))
REPRESENTATION_ITEM('')
SURFACE()
);
#1007=(
BOUNDED_SURFACE()
B_SPLINE_SURFACE(1,2,((#110912,#110913,#110914),(#110915,#110916,#110917)),
 .UNSPECIFIED.,.F.,.F.,.F.)
B_SPLINE_SURFACE_WITH_KNOTS((2,2),(3,3),(0.710318915639747,1.),(0.314840108491245,
0.332069149066961),.UNSPECIFIED.)
GEOMETRIC_REPRESENTATION_ITEM()
RATIONAL_B_SPLINE_SURFACE(((0.98789057959819,0.986774945528852,0.988576730109528),
(0.98789057959819,0.986774945528852,0.988576730109528)))
REPRESENTATION_ITEM('')
SURFACE()
);
#1008=(
BOUNDED_SURFACE()
B_SPLINE_SURFACE(1,2,((#110919,#110920,#110921,#110922,#110923),(#110924,
#110925,#110926,#110927,#110928)),.UNSPECIFIED.,.F.,.F.,.F.)
B_SPLINE_SURFACE_WITH_KNOTS((2,2),(3,2,3),(0.709594768940214,1.),(0.400444645034863,
0.401042835325431,0.418415696246122),.UNSPECIFIED.)
GEOMETRIC_REPRESENTATION_ITEM()
RATIONAL_B_SPLINE_SURFACE(((0.988122504062136,0.988122504062136,0.988122504062136,
0.989520169850094,0.993884164197532),(0.988122504062136,0.988122504062136,
0.988122504062136,0.989520169850094,0.993884164197532)))
REPRESENTATION_ITEM('')
SURFACE()
);
#1009=(
BOUNDED_SURFACE()
B_SPLINE_SURFACE(1,2,((#110937,#110938,#110939),(#110940,#110941,#110942)),
 .UNSPECIFIED.,.F.,.F.,.F.)
B_SPLINE_SURFACE_WITH_KNOTS((2,2),(3,3),(0.710318915639637,1.),(0.314840108491246,
0.332069149066804),.UNSPECIFIED.)
GEOMETRIC_REPRESENTATION_ITEM()
RATIONAL_B_SPLINE_SURFACE(((0.98789057959819,0.986774945528862,0.988576730109495),
(0.98789057959819,0.986774945528862,0.988576730109495)))
REPRESENTATION_ITEM('')
SURFACE()
);
#1010=(
BOUNDED_SURFACE()
B_SPLINE_SURFACE(1,2,((#110944,#110945,#110946,#110947,#110948),(#110949,
#110950,#110951,#110952,#110953)),.UNSPECIFIED.,.F.,.F.,.F.)
B_SPLINE_SURFACE_WITH_KNOTS((2,2),(3,2,3),(0.709594768922229,1.),(0.400444645017343,
0.40104283532543,0.418415696246122),.UNSPECIFIED.)
GEOMETRIC_REPRESENTATION_ITEM()
RATIONAL_B_SPLINE_SURFACE(((0.988122504062135,0.988122504062135,0.988122504062135,
0.989520169850094,0.993884164197532),(0.988122504062135,0.988122504062135,
0.988122504062135,0.989520169850094,0.993884164197532)))
REPRESENTATION_ITEM('')
SURFACE()
);
#1011=(
BOUNDED_SURFACE()
B_SPLINE_SURFACE(1,2,((#110962,#110963,#110964),(#110965,#110966,#110967)),
 .UNSPECIFIED.,.F.,.F.,.F.)
B_SPLINE_SURFACE_WITH_KNOTS((2,2),(3,3),(0.710318915638961,1.),(0.314840108491246,
0.332069149066804),.UNSPECIFIED.)
GEOMETRIC_REPRESENTATION_ITEM()
RATIONAL_B_SPLINE_SURFACE(((0.98789057959819,0.986774945528862,0.988576730109495),
(0.98789057959819,0.986774945528862,0.988576730109495)))
REPRESENTATION_ITEM('')
SURFACE()
);
#1012=(
BOUNDED_SURFACE()
B_SPLINE_SURFACE(1,2,((#110969,#110970,#110971,#110972,#110973),(#110974,
#110975,#110976,#110977,#110978)),.UNSPECIFIED.,.F.,.F.,.F.)
B_SPLINE_SURFACE_WITH_KNOTS((2,2),(3,2,3),(0.709594768914856,1.),(0.400444645010268,
0.401042835325429,0.418415696246123),.UNSPECIFIED.)
GEOMETRIC_REPRESENTATION_ITEM()
RATIONAL_B_SPLINE_SURFACE(((0.988122504062135,0.988122504062135,0.988122504062135,
0.989520169850093,0.993884164197532),(0.988122504062135,0.988122504062135,
0.988122504062135,0.989520169850093,0.993884164197532)))
REPRESENTATION_ITEM('')
SURFACE()
);
#1013=(
BOUNDED_SURFACE()
B_SPLINE_SURFACE(1,2,((#110987,#110988,#110989),(#110990,#110991,#110992)),
 .UNSPECIFIED.,.F.,.F.,.F.)
B_SPLINE_SURFACE_WITH_KNOTS((2,2),(3,3),(0.710318915639114,1.),(0.314840108491246,
0.332069149066804),.UNSPECIFIED.)
GEOMETRIC_REPRESENTATION_ITEM()
RATIONAL_B_SPLINE_SURFACE(((0.98789057959819,0.986774945528862,0.988576730109495),
(0.98789057959819,0.986774945528862,0.988576730109495)))
REPRESENTATION_ITEM('')
SURFACE()
);
#1014=(
BOUNDED_SURFACE()
B_SPLINE_SURFACE(1,2,((#110994,#110995,#110996,#110997,#110998),(#110999,
#111000,#111001,#111002,#111003)),.UNSPECIFIED.,.F.,.F.,.F.)
B_SPLINE_SURFACE_WITH_KNOTS((2,2),(3,2,3),(0.70959476892646,1.),(0.40044464502156,
0.40104283532543,0.418415696246148),.UNSPECIFIED.)
GEOMETRIC_REPRESENTATION_ITEM()
RATIONAL_B_SPLINE_SURFACE(((0.988122504062136,0.988122504062136,0.988122504062136,
0.989520169850096,0.993884164197545),(0.988122504062135,0.988122504062135,
0.988122504062135,0.989520169850095,0.993884164197545)))
REPRESENTATION_ITEM('')
SURFACE()
);
#1015=(
BOUNDED_SURFACE()
B_SPLINE_SURFACE(1,2,((#111012,#111013,#111014),(#111015,#111016,#111017)),
 .UNSPECIFIED.,.F.,.F.,.F.)
B_SPLINE_SURFACE_WITH_KNOTS((2,2),(3,3),(0.710318915639138,1.),(0.314840108491246,
0.332069149066804),.UNSPECIFIED.)
GEOMETRIC_REPRESENTATION_ITEM()
RATIONAL_B_SPLINE_SURFACE(((0.98789057959819,0.986774945528862,0.988576730109495),
(0.98789057959819,0.986774945528862,0.988576730109495)))
REPRESENTATION_ITEM('')
SURFACE()
);
#1016=(
BOUNDED_SURFACE()
B_SPLINE_SURFACE(1,2,((#111019,#111020,#111021,#111022,#111023),(#111024,
#111025,#111026,#111027,#111028)),.UNSPECIFIED.,.F.,.F.,.F.)
B_SPLINE_SURFACE_WITH_KNOTS((2,2),(3,2,3),(0.709594768882625,1.),(0.400444645032233,
0.401042835325431,0.418415696246122),.UNSPECIFIED.)
GEOMETRIC_REPRESENTATION_ITEM()
RATIONAL_B_SPLINE_SURFACE(((0.988122504062136,0.988122504062136,0.988122504062136,
0.989520169850094,0.993884164197532),(0.988122504062136,0.988122504062136,
0.988122504062136,0.989520169850094,0.993884164197532)))
REPRESENTATION_ITEM('')
SURFACE()
);
#1017=(
BOUNDED_SURFACE()
B_SPLINE_SURFACE(1,2,((#111037,#111038,#111039),(#111040,#111041,#111042)),
 .UNSPECIFIED.,.F.,.F.,.F.)
B_SPLINE_SURFACE_WITH_KNOTS((2,2),(3,3),(0.710318915638967,1.),(0.314840108491246,
0.332069149066804),.UNSPECIFIED.)
GEOMETRIC_REPRESENTATION_ITEM()
RATIONAL_B_SPLINE_SURFACE(((0.98789057959819,0.986774945528862,0.988576730109495),
(0.98789057959819,0.986774945528862,0.988576730109495)))
REPRESENTATION_ITEM('')
SURFACE()
);
#1018=(
BOUNDED_SURFACE()
B_SPLINE_SURFACE(1,2,((#111044,#111045,#111046,#111047,#111048),(#111049,
#111050,#111051,#111052,#111053)),.UNSPECIFIED.,.F.,.F.,.F.)
B_SPLINE_SURFACE_WITH_KNOTS((2,2),(3,2,3),(0.709594768927658,1.),(0.40044464502204,
0.401042835325431,0.418415696246123),.UNSPECIFIED.)
GEOMETRIC_REPRESENTATION_ITEM()
RATIONAL_B_SPLINE_SURFACE(((0.988122504062135,0.988122504062135,0.988122504062135,
0.989520169850094,0.993884164197532),(0.988122504062136,0.988122504062136,
0.988122504062136,0.989520169850094,0.993884164197532)))
REPRESENTATION_ITEM('')
SURFACE()
);
#1019=(
BOUNDED_SURFACE()
B_SPLINE_SURFACE(1,2,((#111062,#111063,#111064),(#111065,#111066,#111067)),
 .UNSPECIFIED.,.F.,.F.,.F.)
B_SPLINE_SURFACE_WITH_KNOTS((2,2),(3,3),(0.710318915639904,1.),(0.314840108491246,
0.332069149066804),.UNSPECIFIED.)
GEOMETRIC_REPRESENTATION_ITEM()
RATIONAL_B_SPLINE_SURFACE(((0.98789057959819,0.986774945528862,0.988576730109495),
(0.98789057959819,0.986774945528862,0.988576730109495)))
REPRESENTATION_ITEM('')
SURFACE()
);
#1020=(
BOUNDED_SURFACE()
B_SPLINE_SURFACE(1,2,((#111069,#111070,#111071,#111072,#111073),(#111074,
#111075,#111076,#111077,#111078)),.UNSPECIFIED.,.F.,.F.,.F.)
B_SPLINE_SURFACE_WITH_KNOTS((2,2),(3,2,3),(0.709594768892998,1.),(0.400444645041438,
0.401042835325428,0.418415696246122),.UNSPECIFIED.)
GEOMETRIC_REPRESENTATION_ITEM()
RATIONAL_B_SPLINE_SURFACE(((0.988122504062135,0.988122504062135,0.988122504062135,
0.989520169850093,0.993884164197532),(0.988122504062135,0.988122504062135,
0.988122504062135,0.989520169850093,0.993884164197532)))
REPRESENTATION_ITEM('')
SURFACE()
);
#1021=(
BOUNDED_SURFACE()
B_SPLINE_SURFACE(1,2,((#111087,#111088,#111089),(#111090,#111091,#111092)),
 .UNSPECIFIED.,.F.,.F.,.F.)
B_SPLINE_SURFACE_WITH_KNOTS((2,2),(3,3),(0.710318915639899,1.),(0.314840108491246,
0.332069149066804),.UNSPECIFIED.)
GEOMETRIC_REPRESENTATION_ITEM()
RATIONAL_B_SPLINE_SURFACE(((0.98789057959819,0.986774945528862,0.988576730109495),
(0.98789057959819,0.986774945528862,0.988576730109495)))
REPRESENTATION_ITEM('')
SURFACE()
);
#1022=(
BOUNDED_SURFACE()
B_SPLINE_SURFACE(1,2,((#111094,#111095,#111096,#111097,#111098),(#111099,
#111100,#111101,#111102,#111103)),.UNSPECIFIED.,.F.,.F.,.F.)
B_SPLINE_SURFACE_WITH_KNOTS((2,2),(3,2,3),(0.709594768879046,1.),(0.400444645027766,
0.401042835325429,0.418415696246122),.UNSPECIFIED.)
GEOMETRIC_REPRESENTATION_ITEM()
RATIONAL_B_SPLINE_SURFACE(((0.988122504062135,0.988122504062135,0.988122504062135,
0.989520169850093,0.993884164197532),(0.988122504062135,0.988122504062135,
0.988122504062135,0.989520169850093,0.993884164197532)))
REPRESENTATION_ITEM('')
SURFACE()
);
#1023=(
BOUNDED_SURFACE()
B_SPLINE_SURFACE(1,2,((#111112,#111113,#111114),(#111115,#111116,#111117)),
 .UNSPECIFIED.,.F.,.F.,.F.)
B_SPLINE_SURFACE_WITH_KNOTS((2,2),(3,3),(0.710318915639792,1.),(0.314840108491246,
0.332069149066804),.UNSPECIFIED.)
GEOMETRIC_REPRESENTATION_ITEM()
RATIONAL_B_SPLINE_SURFACE(((0.98789057959819,0.986774945528862,0.988576730109495),
(0.98789057959819,0.986774945528862,0.988576730109495)))
REPRESENTATION_ITEM('')
SURFACE()
);
#1024=(
BOUNDED_SURFACE()
B_SPLINE_SURFACE(1,2,((#111119,#111120,#111121,#111122,#111123),(#111124,
#111125,#111126,#111127,#111128)),.UNSPECIFIED.,.F.,.F.,.F.)
B_SPLINE_SURFACE_WITH_KNOTS((2,2),(3,2,3),(0.709594768914364,1.),(0.400444645009116,
0.401042835325428,0.418415696246123),.UNSPECIFIED.)
GEOMETRIC_REPRESENTATION_ITEM()
RATIONAL_B_SPLINE_SURFACE(((0.988122504062135,0.988122504062135,0.988122504062135,
0.989520169850093,0.993884164197532),(0.988122504062135,0.988122504062135,
0.988122504062135,0.989520169850093,0.993884164197532)))
REPRESENTATION_ITEM('')
SURFACE()
);
#1025=(
BOUNDED_SURFACE()
B_SPLINE_SURFACE(1,2,((#111137,#111138,#111139),(#111140,#111141,#111142)),
 .UNSPECIFIED.,.F.,.F.,.F.)
B_SPLINE_SURFACE_WITH_KNOTS((2,2),(3,3),(0.710318915639852,1.),(0.314840108491245,
0.332069149066961),.UNSPECIFIED.)
GEOMETRIC_REPRESENTATION_ITEM()
RATIONAL_B_SPLINE_SURFACE(((0.98789057959819,0.986774945528852,0.988576730109528),
(0.98789057959819,0.986774945528852,0.988576730109528)))
REPRESENTATION_ITEM('')
SURFACE()
);
#1026=(
BOUNDED_SURFACE()
B_SPLINE_SURFACE(1,2,((#111144,#111145,#111146,#111147,#111148),(#111149,
#111150,#111151,#111152,#111153)),.UNSPECIFIED.,.F.,.F.,.F.)
B_SPLINE_SURFACE_WITH_KNOTS((2,2),(3,2,3),(0.709594768913958,1.),(0.40044464500846,
0.401042835325429,0.418415696246123),.UNSPECIFIED.)
GEOMETRIC_REPRESENTATION_ITEM()
RATIONAL_B_SPLINE_SURFACE(((0.988122504062135,0.988122504062135,0.988122504062135,
0.989520169850093,0.993884164197532),(0.988122504062135,0.988122504062135,
0.988122504062135,0.989520169850093,0.993884164197532)))
REPRESENTATION_ITEM('')
SURFACE()
);
#1027=(
BOUNDED_SURFACE()
B_SPLINE_SURFACE(1,2,((#111162,#111163,#111164),(#111165,#111166,#111167)),
 .UNSPECIFIED.,.F.,.F.,.F.)
B_SPLINE_SURFACE_WITH_KNOTS((2,2),(3,3),(0.710318915639882,1.),(0.314840108491246,
0.332069149066805),.UNSPECIFIED.)
GEOMETRIC_REPRESENTATION_ITEM()
RATIONAL_B_SPLINE_SURFACE(((0.98789057959819,0.986774945528862,0.988576730109495),
(0.98789057959819,0.986774945528862,0.988576730109495)))
REPRESENTATION_ITEM('')
SURFACE()
);
#1028=(
BOUNDED_SURFACE()
B_SPLINE_SURFACE(1,2,((#111169,#111170,#111171,#111172,#111173),(#111174,
#111175,#111176,#111177,#111178)),.UNSPECIFIED.,.F.,.F.,.F.)
B_SPLINE_SURFACE_WITH_KNOTS((2,2),(3,2,3),(0.709594768896135,1.),(0.400444645043879,
0.401042835325428,0.418415696246123),.UNSPECIFIED.)
GEOMETRIC_REPRESENTATION_ITEM()
RATIONAL_B_SPLINE_SURFACE(((0.988122504062135,0.988122504062135,0.988122504062135,
0.989520169850093,0.993884164197532),(0.988122504062135,0.988122504062135,
0.988122504062135,0.989520169850093,0.993884164197532)))
REPRESENTATION_ITEM('')
SURFACE()
);
#1029=(
BOUNDED_SURFACE()
B_SPLINE_SURFACE(1,2,((#111187,#111188,#111189),(#111190,#111191,#111192)),
 .UNSPECIFIED.,.F.,.F.,.F.)
B_SPLINE_SURFACE_WITH_KNOTS((2,2),(3,3),(0.710318915639927,1.),(0.314840108491246,
0.332069149066805),.UNSPECIFIED.)
GEOMETRIC_REPRESENTATION_ITEM()
RATIONAL_B_SPLINE_SURFACE(((0.98789057959819,0.986774945528862,0.988576730109495),
(0.98789057959819,0.986774945528862,0.988576730109495)))
REPRESENTATION_ITEM('')
SURFACE()
);
#1030=(
BOUNDED_SURFACE()
B_SPLINE_SURFACE(1,2,((#111194,#111195,#111196,#111197,#111198),(#111199,
#111200,#111201,#111202,#111203)),.UNSPECIFIED.,.F.,.F.,.F.)
B_SPLINE_SURFACE_WITH_KNOTS((2,2),(3,2,3),(0.709594768891415,1.),(0.400444645039748,
0.401042835325431,0.418415696246122),.UNSPECIFIED.)
GEOMETRIC_REPRESENTATION_ITEM()
RATIONAL_B_SPLINE_SURFACE(((0.988122504062136,0.988122504062136,0.988122504062136,
0.989520169850094,0.993884164197532),(0.988122504062136,0.988122504062136,
0.988122504062136,0.989520169850094,0.993884164197532)))
REPRESENTATION_ITEM('')
SURFACE()
);
#1031=(
BOUNDED_SURFACE()
B_SPLINE_SURFACE(1,2,((#111212,#111213,#111214),(#111215,#111216,#111217)),
 .UNSPECIFIED.,.F.,.F.,.F.)
B_SPLINE_SURFACE_WITH_KNOTS((2,2),(3,3),(0.710318915640067,1.),(0.314840108491246,
0.332069149066804),.UNSPECIFIED.)
GEOMETRIC_REPRESENTATION_ITEM()
RATIONAL_B_SPLINE_SURFACE(((0.98789057959819,0.986774945528862,0.988576730109495),
(0.98789057959819,0.986774945528862,0.988576730109495)))
REPRESENTATION_ITEM('')
SURFACE()
);
#1032=(
BOUNDED_SURFACE()
B_SPLINE_SURFACE(1,2,((#111219,#111220,#111221,#111222,#111223),(#111224,
#111225,#111226,#111227,#111228)),.UNSPECIFIED.,.F.,.F.,.F.)
B_SPLINE_SURFACE_WITH_KNOTS((2,2),(3,2,3),(0.709594768879615,1.),(0.400444644973927,
0.40104283532543,0.418415696246122),.UNSPECIFIED.)
GEOMETRIC_REPRESENTATION_ITEM()
RATIONAL_B_SPLINE_SURFACE(((0.988122504062136,0.988122504062136,0.988122504062136,
0.989520169850094,0.993884164197532),(0.988122504062135,0.988122504062135,
0.988122504062135,0.989520169850094,0.993884164197532)))
REPRESENTATION_ITEM('')
SURFACE()
);
#1033=(
BOUNDED_SURFACE()
B_SPLINE_SURFACE(1,2,((#111237,#111238,#111239),(#111240,#111241,#111242)),
 .UNSPECIFIED.,.F.,.F.,.F.)
B_SPLINE_SURFACE_WITH_KNOTS((2,2),(3,3),(0.710318915640078,1.),(0.314840108491246,
0.332069149066804),.UNSPECIFIED.)
GEOMETRIC_REPRESENTATION_ITEM()
RATIONAL_B_SPLINE_SURFACE(((0.98789057959819,0.986774945528862,0.988576730109495),
(0.98789057959819,0.986774945528862,0.988576730109495)))
REPRESENTATION_ITEM('')
SURFACE()
);
#1034=(
BOUNDED_SURFACE()
B_SPLINE_SURFACE(1,2,((#111244,#111245,#111246,#111247,#111248),(#111249,
#111250,#111251,#111252,#111253)),.UNSPECIFIED.,.F.,.F.,.F.)
B_SPLINE_SURFACE_WITH_KNOTS((2,2),(3,2,3),(0.709961012046059,1.),(0.400810888140328,
0.401042835325431,0.418415696246122),.UNSPECIFIED.)
GEOMETRIC_REPRESENTATION_ITEM()
RATIONAL_B_SPLINE_SURFACE(((0.988122504062135,0.988122504062135,0.988122504062135,
0.989520169850094,0.993884164197532),(0.988122504062135,0.988122504062135,
0.988122504062135,0.989520169850094,0.993884164197532)))
REPRESENTATION_ITEM('')
SURFACE()
);
#1035=(
BOUNDED_SURFACE()
B_SPLINE_SURFACE(1,2,((#111262,#111263,#111264),(#111265,#111266,#111267)),
 .UNSPECIFIED.,.F.,.F.,.F.)
B_SPLINE_SURFACE_WITH_KNOTS((2,2),(3,3),(0.710318915640071,1.),(0.314840108491246,
0.332069149066804),.UNSPECIFIED.)
GEOMETRIC_REPRESENTATION_ITEM()
RATIONAL_B_SPLINE_SURFACE(((0.98789057959819,0.986774945528862,0.988576730109495),
(0.98789057959819,0.986774945528862,0.988576730109495)))
REPRESENTATION_ITEM('')
SURFACE()
);
#1036=(
BOUNDED_SURFACE()
B_SPLINE_SURFACE(1,2,((#111269,#111270,#111271,#111272,#111273),(#111274,
#111275,#111276,#111277,#111278)),.UNSPECIFIED.,.F.,.F.,.F.)
B_SPLINE_SURFACE_WITH_KNOTS((2,2),(3,2,3),(0.709594768954711,1.),(0.400444645048674,
0.401042835325431,0.418415696246122),.UNSPECIFIED.)
GEOMETRIC_REPRESENTATION_ITEM()
RATIONAL_B_SPLINE_SURFACE(((0.988122504062136,0.988122504062136,0.988122504062136,
0.989520169850094,0.993884164197532),(0.988122504062135,0.988122504062135,
0.988122504062135,0.989520169850094,0.993884164197532)))
REPRESENTATION_ITEM('')
SURFACE()
);
#1037=(
BOUNDED_SURFACE()
B_SPLINE_SURFACE(1,2,((#111287,#111288,#111289),(#111290,#111291,#111292)),
 .UNSPECIFIED.,.F.,.F.,.F.)
B_SPLINE_SURFACE_WITH_KNOTS((2,2),(3,3),(0.71031891564008,1.),(0.314840108491246,
0.332069149066805),.UNSPECIFIED.)
GEOMETRIC_REPRESENTATION_ITEM()
RATIONAL_B_SPLINE_SURFACE(((0.98789057959819,0.986774945528862,0.988576730109495),
(0.98789057959819,0.986774945528862,0.988576730109495)))
REPRESENTATION_ITEM('')
SURFACE()
);
#1038=(
BOUNDED_SURFACE()
B_SPLINE_SURFACE(1,2,((#111294,#111295,#111296,#111297,#111298),(#111299,
#111300,#111301,#111302,#111303)),.UNSPECIFIED.,.F.,.F.,.F.)
B_SPLINE_SURFACE_WITH_KNOTS((2,2),(3,2,3),(0.709594768929927,1.),(0.400444645024341,
0.401042835325431,0.418415696246123),.UNSPECIFIED.)
GEOMETRIC_REPRESENTATION_ITEM()
RATIONAL_B_SPLINE_SURFACE(((0.988122504062136,0.988122504062136,0.988122504062136,
0.989520169850094,0.993884164197532),(0.988122504062136,0.988122504062136,
0.988122504062136,0.989520169850094,0.993884164197532)))
REPRESENTATION_ITEM('')
SURFACE()
);
#1039=(
BOUNDED_SURFACE()
B_SPLINE_SURFACE(1,2,((#111312,#111313,#111314),(#111315,#111316,#111317)),
 .UNSPECIFIED.,.F.,.F.,.F.)
B_SPLINE_SURFACE_WITH_KNOTS((2,2),(3,3),(0.710318915640074,1.),(0.314840108491246,
0.332069149066805),.UNSPECIFIED.)
GEOMETRIC_REPRESENTATION_ITEM()
RATIONAL_B_SPLINE_SURFACE(((0.98789057959819,0.986774945528862,0.988576730109495),
(0.98789057959819,0.986774945528862,0.988576730109495)))
REPRESENTATION_ITEM('')
SURFACE()
);
#1040=(
BOUNDED_SURFACE()
B_SPLINE_SURFACE(1,2,((#111319,#111320,#111321,#111322,#111323),(#111324,
#111325,#111326,#111327,#111328)),.UNSPECIFIED.,.F.,.F.,.F.)
B_SPLINE_SURFACE_WITH_KNOTS((2,2),(3,2,3),(0.709594768925206,1.),(0.400444645019135,
0.401042835325431,0.418415696246122),.UNSPECIFIED.)
GEOMETRIC_REPRESENTATION_ITEM()
RATIONAL_B_SPLINE_SURFACE(((0.988122504062136,0.988122504062136,0.988122504062136,
0.989520169850094,0.993884164197532),(0.988122504062136,0.988122504062136,
0.988122504062136,0.989520169850094,0.993884164197532)))
REPRESENTATION_ITEM('')
SURFACE()
);
#1041=(
BOUNDED_SURFACE()
B_SPLINE_SURFACE(1,2,((#111337,#111338,#111339),(#111340,#111341,#111342)),
 .UNSPECIFIED.,.F.,.F.,.F.)
B_SPLINE_SURFACE_WITH_KNOTS((2,2),(3,3),(0.71031891563997,1.),(0.314840108491246,
0.332069149066805),.UNSPECIFIED.)
GEOMETRIC_REPRESENTATION_ITEM()
RATIONAL_B_SPLINE_SURFACE(((0.98789057959819,0.986774945528862,0.988576730109495),
(0.98789057959819,0.986774945528862,0.988576730109495)))
REPRESENTATION_ITEM('')
SURFACE()
);
#1042=(
BOUNDED_SURFACE()
B_SPLINE_SURFACE(1,2,((#111344,#111345,#111346,#111347,#111348),(#111349,
#111350,#111351,#111352,#111353)),.UNSPECIFIED.,.F.,.F.,.F.)
B_SPLINE_SURFACE_WITH_KNOTS((2,2),(3,2,3),(0.70959476887014,1.),(0.40044464501961,
0.401042835325428,0.418415696246123),.UNSPECIFIED.)
GEOMETRIC_REPRESENTATION_ITEM()
RATIONAL_B_SPLINE_SURFACE(((0.988122504062135,0.988122504062135,0.988122504062135,
0.989520169850093,0.993884164197532),(0.988122504062135,0.988122504062135,
0.988122504062135,0.989520169850093,0.993884164197532)))
REPRESENTATION_ITEM('')
SURFACE()
);
#1043=(
BOUNDED_SURFACE()
B_SPLINE_SURFACE(1,2,((#111362,#111363,#111364),(#111365,#111366,#111367)),
 .UNSPECIFIED.,.F.,.F.,.F.)
B_SPLINE_SURFACE_WITH_KNOTS((2,2),(3,3),(0.710318915638668,1.),(0.314840108491246,
0.332069149066805),.UNSPECIFIED.)
GEOMETRIC_REPRESENTATION_ITEM()
RATIONAL_B_SPLINE_SURFACE(((0.98789057959819,0.986774945528862,0.988576730109495),
(0.98789057959819,0.986774945528862,0.988576730109495)))
REPRESENTATION_ITEM('')
SURFACE()
);
#1044=(
BOUNDED_SURFACE()
B_SPLINE_SURFACE(1,2,((#111369,#111370,#111371,#111372,#111373),(#111374,
#111375,#111376,#111377,#111378)),.UNSPECIFIED.,.F.,.F.,.F.)
B_SPLINE_SURFACE_WITH_KNOTS((2,2),(3,2,3),(0.709594768915212,1.),(0.400444645009376,
0.401042835325429,0.418415696246122),.UNSPECIFIED.)
GEOMETRIC_REPRESENTATION_ITEM()
RATIONAL_B_SPLINE_SURFACE(((0.988122504062135,0.988122504062135,0.988122504062135,
0.989520169850093,0.993884164197532),(0.988122504062135,0.988122504062135,
0.988122504062135,0.989520169850093,0.993884164197532)))
REPRESENTATION_ITEM('')
SURFACE()
);
#1045=(
BOUNDED_SURFACE()
B_SPLINE_SURFACE(1,2,((#111387,#111388,#111389),(#111390,#111391,#111392)),
 .UNSPECIFIED.,.F.,.F.,.F.)
B_SPLINE_SURFACE_WITH_KNOTS((2,2),(3,3),(0.710318915639828,1.),(0.314840108491246,
0.332069149066805),.UNSPECIFIED.)
GEOMETRIC_REPRESENTATION_ITEM()
RATIONAL_B_SPLINE_SURFACE(((0.98789057959819,0.986774945528862,0.988576730109495),
(0.98789057959819,0.986774945528862,0.988576730109495)))
REPRESENTATION_ITEM('')
SURFACE()
);
#1046=(
BOUNDED_SURFACE()
B_SPLINE_SURFACE(1,2,((#111394,#111395,#111396,#111397,#111398),(#111399,
#111400,#111401,#111402,#111403)),.UNSPECIFIED.,.F.,.F.,.F.)
B_SPLINE_SURFACE_WITH_KNOTS((2,2),(3,2,3),(0.709594768950057,1.),(0.400444645044343,
0.401042835325431,0.418415696246123),.UNSPECIFIED.)
GEOMETRIC_REPRESENTATION_ITEM()
RATIONAL_B_SPLINE_SURFACE(((0.988122504062135,0.988122504062135,0.988122504062135,
0.989520169850094,0.993884164197532),(0.988122504062135,0.988122504062135,
0.988122504062135,0.989520169850094,0.993884164197532)))
REPRESENTATION_ITEM('')
SURFACE()
);
#1047=(
BOUNDED_SURFACE()
B_SPLINE_SURFACE(1,2,((#111412,#111413,#111414),(#111415,#111416,#111417)),
 .UNSPECIFIED.,.F.,.F.,.F.)
B_SPLINE_SURFACE_WITH_KNOTS((2,2),(3,3),(0.710318915640079,1.),(0.314840108491246,
0.332069149066805),.UNSPECIFIED.)
GEOMETRIC_REPRESENTATION_ITEM()
RATIONAL_B_SPLINE_SURFACE(((0.98789057959819,0.986774945528862,0.988576730109495),
(0.98789057959819,0.986774945528862,0.988576730109495)))
REPRESENTATION_ITEM('')
SURFACE()
);
#1048=(
BOUNDED_SURFACE()
B_SPLINE_SURFACE(1,2,((#111419,#111420,#111421,#111422,#111423),(#111424,
#111425,#111426,#111427,#111428)),.UNSPECIFIED.,.F.,.F.,.F.)
B_SPLINE_SURFACE_WITH_KNOTS((2,2),(3,2,3),(0.709594768954782,1.),(0.400444645048726,
0.401042835325429,0.418415696246123),.UNSPECIFIED.)
GEOMETRIC_REPRESENTATION_ITEM()
RATIONAL_B_SPLINE_SURFACE(((0.988122504062135,0.988122504062135,0.988122504062135,
0.989520169850093,0.993884164197532),(0.988122504062135,0.988122504062135,
0.988122504062135,0.989520169850093,0.993884164197532)))
REPRESENTATION_ITEM('')
SURFACE()
);
#1049=(
BOUNDED_SURFACE()
B_SPLINE_SURFACE(1,2,((#111437,#111438,#111439),(#111440,#111441,#111442)),
 .UNSPECIFIED.,.F.,.F.,.F.)
B_SPLINE_SURFACE_WITH_KNOTS((2,2),(3,3),(0.710318915640079,1.),(0.314840108491246,
0.332069149066805),.UNSPECIFIED.)
GEOMETRIC_REPRESENTATION_ITEM()
RATIONAL_B_SPLINE_SURFACE(((0.98789057959819,0.986774945528862,0.988576730109495),
(0.98789057959819,0.986774945528862,0.988576730109495)))
REPRESENTATION_ITEM('')
SURFACE()
);
#1050=(
BOUNDED_SURFACE()
B_SPLINE_SURFACE(1,2,((#111444,#111445,#111446,#111447,#111448),(#111449,
#111450,#111451,#111452,#111453)),.UNSPECIFIED.,.F.,.F.,.F.)
B_SPLINE_SURFACE_WITH_KNOTS((2,2),(3,2,3),(0.709594768915967,1.),(0.400444645010483,
0.401042835325429,0.418415696246123),.UNSPECIFIED.)
GEOMETRIC_REPRESENTATION_ITEM()
RATIONAL_B_SPLINE_SURFACE(((0.988122504062135,0.988122504062135,0.988122504062135,
0.989520169850093,0.993884164197532),(0.988122504062135,0.988122504062135,
0.988122504062135,0.989520169850093,0.993884164197532)))
REPRESENTATION_ITEM('')
SURFACE()
);
#1051=(
BOUNDED_SURFACE()
B_SPLINE_SURFACE(1,2,((#111462,#111463,#111464),(#111465,#111466,#111467)),
 .UNSPECIFIED.,.F.,.F.,.F.)
B_SPLINE_SURFACE_WITH_KNOTS((2,2),(3,3),(0.71031891564008,1.),(0.314840108491246,
0.332069149066805),.UNSPECIFIED.)
GEOMETRIC_REPRESENTATION_ITEM()
RATIONAL_B_SPLINE_SURFACE(((0.98789057959819,0.986774945528862,0.988576730109495),
(0.98789057959819,0.986774945528862,0.988576730109495)))
REPRESENTATION_ITEM('')
SURFACE()
);
#1052=(
BOUNDED_SURFACE()
B_SPLINE_SURFACE(1,2,((#111469,#111470,#111471,#111472,#111473),(#111474,
#111475,#111476,#111477,#111478)),.UNSPECIFIED.,.F.,.F.,.F.)
B_SPLINE_SURFACE_WITH_KNOTS((2,2),(3,2,3),(0.709594768949808,1.),(0.400444645043581,
0.401042835325428,0.418415696246123),.UNSPECIFIED.)
GEOMETRIC_REPRESENTATION_ITEM()
RATIONAL_B_SPLINE_SURFACE(((0.988122504062135,0.988122504062135,0.988122504062135,
0.989520169850093,0.993884164197532),(0.988122504062135,0.988122504062135,
0.988122504062135,0.989520169850093,0.993884164197532)))
REPRESENTATION_ITEM('')
SURFACE()
);
#1053=(
BOUNDED_SURFACE()
B_SPLINE_SURFACE(1,2,((#111487,#111488,#111489),(#111490,#111491,#111492)),
 .UNSPECIFIED.,.F.,.F.,.F.)
B_SPLINE_SURFACE_WITH_KNOTS((2,2),(3,3),(0.710318915640075,1.),(0.314840108491246,
0.332069149066804),.UNSPECIFIED.)
GEOMETRIC_REPRESENTATION_ITEM()
RATIONAL_B_SPLINE_SURFACE(((0.98789057959819,0.986774945528862,0.988576730109495),
(0.98789057959819,0.986774945528862,0.988576730109495)))
REPRESENTATION_ITEM('')
SURFACE()
);
#1054=(
BOUNDED_SURFACE()
B_SPLINE_SURFACE(1,2,((#111494,#111495,#111496,#111497,#111498),(#111499,
#111500,#111501,#111502,#111503)),.UNSPECIFIED.,.F.,.F.,.F.)
B_SPLINE_SURFACE_WITH_KNOTS((2,2),(3,2,3),(0.709594768917399,1.),(0.400444645011763,
0.401042835325431,0.418415696246121),.UNSPECIFIED.)
GEOMETRIC_REPRESENTATION_ITEM()
RATIONAL_B_SPLINE_SURFACE(((0.988122504062135,0.988122504062135,0.988122504062135,
0.989520169850093,0.993884164197532),(0.988122504062135,0.988122504062135,
0.988122504062135,0.989520169850093,0.993884164197532)))
REPRESENTATION_ITEM('')
SURFACE()
);
#1055=(
BOUNDED_SURFACE()
B_SPLINE_SURFACE(1,2,((#111512,#111513,#111514),(#111515,#111516,#111517)),
 .UNSPECIFIED.,.F.,.F.,.F.)
B_SPLINE_SURFACE_WITH_KNOTS((2,2),(3,3),(0.710318915639816,1.),(0.314840108491247,
0.332069149066865),.UNSPECIFIED.)
GEOMETRIC_REPRESENTATION_ITEM()
RATIONAL_B_SPLINE_SURFACE(((0.98789057959819,0.986774945528858,0.988576730109508),
(0.98789057959819,0.986774945528858,0.988576730109508)))
REPRESENTATION_ITEM('')
SURFACE()
);
#1056=(
BOUNDED_SURFACE()
B_SPLINE_SURFACE(1,2,((#111519,#111520,#111521,#111522,#111523),(#111524,
#111525,#111526,#111527,#111528)),.UNSPECIFIED.,.F.,.F.,.F.)
B_SPLINE_SURFACE_WITH_KNOTS((2,2),(3,2,3),(0.709594768924498,1.),(0.400444645018782,
0.401042835325428,0.418415696246121),.UNSPECIFIED.)
GEOMETRIC_REPRESENTATION_ITEM()
RATIONAL_B_SPLINE_SURFACE(((0.988122504062135,0.988122504062135,0.988122504062135,
0.989520169850093,0.993884164197532),(0.988122504062135,0.988122504062135,
0.988122504062135,0.989520169850093,0.993884164197532)))
REPRESENTATION_ITEM('')
SURFACE()
);
#1057=(
BOUNDED_SURFACE()
B_SPLINE_SURFACE(1,2,((#111537,#111538,#111539),(#111540,#111541,#111542)),
 .UNSPECIFIED.,.F.,.F.,.F.)
B_SPLINE_SURFACE_WITH_KNOTS((2,2),(3,3),(0.71031891563976,1.),(0.314840108491247,
0.332069149066858),.UNSPECIFIED.)
GEOMETRIC_REPRESENTATION_ITEM()
RATIONAL_B_SPLINE_SURFACE(((0.98789057959819,0.986774945528858,0.988576730109506),
(0.98789057959819,0.986774945528858,0.988576730109506)))
REPRESENTATION_ITEM('')
SURFACE()
);
#1058=(
BOUNDED_SURFACE()
B_SPLINE_SURFACE(1,2,((#111544,#111545,#111546,#111547,#111548),(#111549,
#111550,#111551,#111552,#111553)),.UNSPECIFIED.,.F.,.F.,.F.)
B_SPLINE_SURFACE_WITH_KNOTS((2,2),(3,2,3),(0.709594768872521,1.),(0.400444645020776,
0.401042835325429,0.418415696246121),.UNSPECIFIED.)
GEOMETRIC_REPRESENTATION_ITEM()
RATIONAL_B_SPLINE_SURFACE(((0.988122504062135,0.988122504062135,0.988122504062135,
0.989520169850093,0.993884164197532),(0.988122504062135,0.988122504062135,
0.988122504062135,0.989520169850093,0.993884164197532)))
REPRESENTATION_ITEM('')
SURFACE()
);
#1059=(
BOUNDED_SURFACE()
B_SPLINE_SURFACE(1,2,((#111562,#111563,#111564),(#111565,#111566,#111567)),
 .UNSPECIFIED.,.F.,.F.,.F.)
B_SPLINE_SURFACE_WITH_KNOTS((2,2),(3,3),(0.710318915639801,1.),(0.314840108491246,
0.332069149066961),.UNSPECIFIED.)
GEOMETRIC_REPRESENTATION_ITEM()
RATIONAL_B_SPLINE_SURFACE(((0.98789057959819,0.986774945528852,0.988576730109528),
(0.98789057959819,0.986774945528852,0.988576730109528)))
REPRESENTATION_ITEM('')
SURFACE()
);
#1060=(
BOUNDED_SURFACE()
B_SPLINE_SURFACE(1,2,((#111569,#111570,#111571,#111572,#111573),(#111574,
#111575,#111576,#111577,#111578)),.UNSPECIFIED.,.F.,.F.,.F.)
B_SPLINE_SURFACE_WITH_KNOTS((2,2),(3,2,3),(0.709594768860568,1.),(0.400444645009416,
0.40104283532543,0.418415696246122),.UNSPECIFIED.)
GEOMETRIC_REPRESENTATION_ITEM()
RATIONAL_B_SPLINE_SURFACE(((0.988122504062135,0.988122504062135,0.988122504062135,
0.989520169850094,0.993884164197532),(0.988122504062135,0.988122504062135,
0.988122504062135,0.989520169850094,0.993884164197532)))
REPRESENTATION_ITEM('')
SURFACE()
);
#1061=(
BOUNDED_SURFACE()
B_SPLINE_SURFACE(1,2,((#111587,#111588,#111589),(#111590,#111591,#111592)),
 .UNSPECIFIED.,.F.,.F.,.F.)
B_SPLINE_SURFACE_WITH_KNOTS((2,2),(3,3),(0.710318915639618,1.),(0.314840108491245,
0.332069149066961),.UNSPECIFIED.)
GEOMETRIC_REPRESENTATION_ITEM()
RATIONAL_B_SPLINE_SURFACE(((0.98789057959819,0.986774945528851,0.988576730109528),
(0.98789057959819,0.986774945528852,0.988576730109528)))
REPRESENTATION_ITEM('')
SURFACE()
);
#1062=(
BOUNDED_SURFACE()
B_SPLINE_SURFACE(1,2,((#111594,#111595,#111596,#111597,#111598),(#111599,
#111600,#111601,#111602,#111603)),.UNSPECIFIED.,.F.,.F.,.F.)
B_SPLINE_SURFACE_WITH_KNOTS((2,2),(3,2,3),(0.709594768894549,1.),(0.400444645043085,
0.401042835325431,0.418415696246122),.UNSPECIFIED.)
GEOMETRIC_REPRESENTATION_ITEM()
RATIONAL_B_SPLINE_SURFACE(((0.988122504062135,0.988122504062135,0.988122504062135,
0.989520169850094,0.993884164197532),(0.988122504062135,0.988122504062135,
0.988122504062135,0.989520169850094,0.993884164197532)))
REPRESENTATION_ITEM('')
SURFACE()
);
#1063=(
BOUNDED_SURFACE()
B_SPLINE_SURFACE(1,2,((#111612,#111613,#111614),(#111615,#111616,#111617)),
 .UNSPECIFIED.,.F.,.F.,.F.)
B_SPLINE_SURFACE_WITH_KNOTS((2,2),(3,3),(0.71031891563966,1.),(0.314840108491245,
0.332069149066961),.UNSPECIFIED.)
GEOMETRIC_REPRESENTATION_ITEM()
RATIONAL_B_SPLINE_SURFACE(((0.98789057959819,0.986774945528852,0.988576730109528),
(0.98789057959819,0.986774945528852,0.988576730109528)))
REPRESENTATION_ITEM('')
SURFACE()
);
#1064=(
BOUNDED_SURFACE()
B_SPLINE_SURFACE(1,2,((#111619,#111620,#111621),(#111622,#111623,#111624)),
 .UNSPECIFIED.,.F.,.F.,.F.)
B_SPLINE_SURFACE_WITH_KNOTS((2,2),(3,3),(0.,0.28968108435992),(0.262994994770444,
0.280433083165913),.UNSPECIFIED.)
GEOMETRIC_REPRESENTATION_ITEM()
RATIONAL_B_SPLINE_SURFACE(((0.989123653000983,0.991350813683904,0.996566619267863),
(0.989123653000983,0.991350813683904,0.996566619267863)))
REPRESENTATION_ITEM('')
SURFACE()
);
#1065=(
BOUNDED_SURFACE()
B_SPLINE_SURFACE(1,2,((#111633,#111634,#111635,#111636,#111637),(#111638,
#111639,#111640,#111641,#111642)),.UNSPECIFIED.,.F.,.F.,.F.)
B_SPLINE_SURFACE_WITH_KNOTS((2,2),(3,2,3),(0.,0.29039866515125),(0.452333244852708,
0.452924869174517,0.470122329512317),.UNSPECIFIED.)
GEOMETRIC_REPRESENTATION_ITEM()
RATIONAL_B_SPLINE_SURFACE(((0.988732477628006,0.988732477628006,0.988732477628006,
0.986812255267055,0.987798766302166),(0.988732477628006,0.988732477628006,
0.988732477628006,0.986812255267055,0.987798766302166)))
REPRESENTATION_ITEM('')
SURFACE()
);
#1066=(
BOUNDED_SURFACE()
B_SPLINE_SURFACE(1,2,((#111644,#111645,#111646),(#111647,#111648,#111649)),
 .UNSPECIFIED.,.F.,.F.,.F.)
B_SPLINE_SURFACE_WITH_KNOTS((2,2),(3,3),(0.,0.289681084359921),(0.262994994770445,
0.280433083165915),.UNSPECIFIED.)
GEOMETRIC_REPRESENTATION_ITEM()
RATIONAL_B_SPLINE_SURFACE(((0.989123653000983,0.991350813683905,0.996566619267864),
(0.989123653000983,0.991350813683905,0.996566619267864)))
REPRESENTATION_ITEM('')
SURFACE()
);
#1067=(
BOUNDED_SURFACE()
B_SPLINE_SURFACE(1,2,((#111658,#111659,#111660,#111661,#111662),(#111663,
#111664,#111665,#111666,#111667)),.UNSPECIFIED.,.F.,.F.,.F.)
B_SPLINE_SURFACE_WITH_KNOTS((2,2),(3,2,3),(0.,0.290398665170194),(0.452333244833745,
0.452924869174514,0.470122329512317),.UNSPECIFIED.)
GEOMETRIC_REPRESENTATION_ITEM()
RATIONAL_B_SPLINE_SURFACE(((0.988732477628006,0.988732477628006,0.988732477628006,
0.986812255267055,0.987798766302166),(0.988732477628006,0.988732477628006,
0.988732477628006,0.986812255267055,0.987798766302166)))
REPRESENTATION_ITEM('')
SURFACE()
);
#1068=(
BOUNDED_SURFACE()
B_SPLINE_SURFACE(1,2,((#111669,#111670,#111671),(#111672,#111673,#111674)),
 .UNSPECIFIED.,.F.,.F.,.F.)
B_SPLINE_SURFACE_WITH_KNOTS((2,2),(3,3),(0.,0.289681084359918),(0.262994994770445,
0.280433083165914),.UNSPECIFIED.)
GEOMETRIC_REPRESENTATION_ITEM()
RATIONAL_B_SPLINE_SURFACE(((0.989123653000983,0.991350813683905,0.996566619267864),
(0.989123653000983,0.991350813683905,0.996566619267864)))
REPRESENTATION_ITEM('')
SURFACE()
);
#1069=(
BOUNDED_SURFACE()
B_SPLINE_SURFACE(1,2,((#111683,#111684,#111685,#111686,#111687),(#111688,
#111689,#111690,#111691,#111692)),.UNSPECIFIED.,.F.,.F.,.F.)
B_SPLINE_SURFACE_WITH_KNOTS((2,2),(3,2,3),(0.,0.290398665162971),(0.452333244841549,
0.452924869174515,0.470122329512317),.UNSPECIFIED.)
GEOMETRIC_REPRESENTATION_ITEM()
RATIONAL_B_SPLINE_SURFACE(((0.988732477628006,0.988732477628006,0.988732477628006,
0.986812255267055,0.987798766302166),(0.988732477628006,0.988732477628006,
0.988732477628006,0.986812255267055,0.987798766302166)))
REPRESENTATION_ITEM('')
SURFACE()
);
#1070=(
BOUNDED_SURFACE()
B_SPLINE_SURFACE(1,2,((#111694,#111695,#111696),(#111697,#111698,#111699)),
 .UNSPECIFIED.,.F.,.F.,.F.)
B_SPLINE_SURFACE_WITH_KNOTS((2,2),(3,3),(0.,0.289681084359921),(0.262994994770445,
0.280433083165914),.UNSPECIFIED.)
GEOMETRIC_REPRESENTATION_ITEM()
RATIONAL_B_SPLINE_SURFACE(((0.989123653000983,0.991350813683905,0.996566619267864),
(0.989123653000983,0.991350813683905,0.996566619267864)))
REPRESENTATION_ITEM('')
SURFACE()
);
#1071=(
BOUNDED_SURFACE()
B_SPLINE_SURFACE(1,2,((#111708,#111709,#111710,#111711,#111712),(#111713,
#111714,#111715,#111716,#111717)),.UNSPECIFIED.,.F.,.F.,.F.)
B_SPLINE_SURFACE_WITH_KNOTS((2,2),(3,2,3),(0.,0.290398665157545),(0.452333244846396,
0.452924869174515,0.470122329512317),.UNSPECIFIED.)
GEOMETRIC_REPRESENTATION_ITEM()
RATIONAL_B_SPLINE_SURFACE(((0.988732477628006,0.988732477628006,0.988732477628006,
0.986812255267055,0.987798766302166),(0.988732477628006,0.988732477628006,
0.988732477628006,0.986812255267055,0.987798766302166)))
REPRESENTATION_ITEM('')
SURFACE()
);
#1072=(
BOUNDED_SURFACE()
B_SPLINE_SURFACE(1,2,((#111719,#111720,#111721),(#111722,#111723,#111724)),
 .UNSPECIFIED.,.F.,.F.,.F.)
B_SPLINE_SURFACE_WITH_KNOTS((2,2),(3,3),(0.,0.289681084359921),(0.262994994770445,
0.280433083165914),.UNSPECIFIED.)
GEOMETRIC_REPRESENTATION_ITEM()
RATIONAL_B_SPLINE_SURFACE(((0.989123653000983,0.991350813683905,0.996566619267864),
(0.989123653000983,0.991350813683905,0.996566619267864)))
REPRESENTATION_ITEM('')
SURFACE()
);
#1073=(
BOUNDED_SURFACE()
B_SPLINE_SURFACE(1,2,((#111733,#111734,#111735,#111736,#111737),(#111738,
#111739,#111740,#111741,#111742)),.UNSPECIFIED.,.F.,.F.,.F.)
B_SPLINE_SURFACE_WITH_KNOTS((2,2),(3,2,3),(0.,0.29039866515236),(0.452333244852162,
0.452924869174515,0.470122329512317),.UNSPECIFIED.)
GEOMETRIC_REPRESENTATION_ITEM()
RATIONAL_B_SPLINE_SURFACE(((0.988732477628006,0.988732477628006,0.988732477628006,
0.986812255267055,0.987798766302166),(0.988732477628006,0.988732477628006,
0.988732477628006,0.986812255267055,0.987798766302166)))
REPRESENTATION_ITEM('')
SURFACE()
);
#1074=(
BOUNDED_SURFACE()
B_SPLINE_SURFACE(1,2,((#111744,#111745,#111746),(#111747,#111748,#111749)),
 .UNSPECIFIED.,.F.,.F.,.F.)
B_SPLINE_SURFACE_WITH_KNOTS((2,2),(3,3),(0.,0.289681084359916),(0.262994994770445,
0.280433083165914),.UNSPECIFIED.)
GEOMETRIC_REPRESENTATION_ITEM()
RATIONAL_B_SPLINE_SURFACE(((0.989123653000983,0.991350813683905,0.996566619267864),
(0.989123653000983,0.991350813683905,0.996566619267864)))
REPRESENTATION_ITEM('')
SURFACE()
);
#1075=(
BOUNDED_SURFACE()
B_SPLINE_SURFACE(1,2,((#111758,#111759,#111760,#111761,#111762),(#111763,
#111764,#111765,#111766,#111767)),.UNSPECIFIED.,.F.,.F.,.F.)
B_SPLINE_SURFACE_WITH_KNOTS((2,2),(3,2,3),(0.,0.290398665167829),(0.452333244836186,
0.452924869174516,0.470122329512317),.UNSPECIFIED.)
GEOMETRIC_REPRESENTATION_ITEM()
RATIONAL_B_SPLINE_SURFACE(((0.988732477628006,0.988732477628006,0.988732477628006,
0.986812255267055,0.987798766302166),(0.988732477628006,0.988732477628006,
0.988732477628006,0.986812255267055,0.987798766302166)))
REPRESENTATION_ITEM('')
SURFACE()
);
#1076=(
BOUNDED_SURFACE()
B_SPLINE_SURFACE(1,2,((#111769,#111770,#111771),(#111772,#111773,#111774)),
 .UNSPECIFIED.,.F.,.F.,.F.)
B_SPLINE_SURFACE_WITH_KNOTS((2,2),(3,3),(0.,0.289681084359922),(0.262994994770443,
0.280433083165913),.UNSPECIFIED.)
GEOMETRIC_REPRESENTATION_ITEM()
RATIONAL_B_SPLINE_SURFACE(((0.989123653000983,0.991350813683904,0.996566619267864),
(0.989123653000983,0.991350813683904,0.996566619267864)))
REPRESENTATION_ITEM('')
SURFACE()
);
#1077=(
BOUNDED_SURFACE()
B_SPLINE_SURFACE(1,2,((#111783,#111784,#111785,#111786,#111787),(#111788,
#111789,#111790,#111791,#111792)),.UNSPECIFIED.,.F.,.F.,.F.)
B_SPLINE_SURFACE_WITH_KNOTS((2,2),(3,2,3),(0.,0.290398665157212),(0.452333244846804,
0.452924869174517,0.470122329512318),.UNSPECIFIED.)
GEOMETRIC_REPRESENTATION_ITEM()
RATIONAL_B_SPLINE_SURFACE(((0.988732477628006,0.988732477628006,0.988732477628006,
0.986812255267055,0.987798766302167),(0.988732477628006,0.988732477628006,
0.988732477628006,0.986812255267055,0.987798766302167)))
REPRESENTATION_ITEM('')
SURFACE()
);
#1078=(
BOUNDED_SURFACE()
B_SPLINE_SURFACE(1,2,((#111794,#111795,#111796),(#111797,#111798,#111799)),
 .UNSPECIFIED.,.F.,.F.,.F.)
B_SPLINE_SURFACE_WITH_KNOTS((2,2),(3,3),(0.,0.289681084359917),(0.262994994770443,
0.280433083165913),.UNSPECIFIED.)
GEOMETRIC_REPRESENTATION_ITEM()
RATIONAL_B_SPLINE_SURFACE(((0.989123653000983,0.991350813683904,0.996566619267863),
(0.989123653000983,0.991350813683904,0.996566619267863)))
REPRESENTATION_ITEM('')
SURFACE()
);
#1079=(
BOUNDED_SURFACE()
B_SPLINE_SURFACE(1,2,((#111808,#111809,#111810,#111811,#111812),(#111813,
#111814,#111815,#111816,#111817)),.UNSPECIFIED.,.F.,.F.,.F.)
B_SPLINE_SURFACE_WITH_KNOTS((2,2),(3,2,3),(0.,0.290398665177456),(0.45233324482716,
0.452924869174517,0.470122329512318),.UNSPECIFIED.)
GEOMETRIC_REPRESENTATION_ITEM()
RATIONAL_B_SPLINE_SURFACE(((0.988732477628005,0.988732477628005,0.988732477628005,
0.986812255267055,0.987798766302166),(0.988732477628005,0.988732477628005,
0.988732477628005,0.986812255267055,0.987798766302166)))
REPRESENTATION_ITEM('')
SURFACE()
);
#1080=(
BOUNDED_SURFACE()
B_SPLINE_SURFACE(1,2,((#111819,#111820,#111821),(#111822,#111823,#111824)),
 .UNSPECIFIED.,.F.,.F.,.F.)
B_SPLINE_SURFACE_WITH_KNOTS((2,2),(3,3),(0.,0.289681084359919),(0.262994994770443,
0.280433083165913),.UNSPECIFIED.)
GEOMETRIC_REPRESENTATION_ITEM()
RATIONAL_B_SPLINE_SURFACE(((0.989123653000983,0.991350813683904,0.996566619267864),
(0.989123653000983,0.991350813683904,0.996566619267864)))
REPRESENTATION_ITEM('')
SURFACE()
);
#1081=(
BOUNDED_SURFACE()
B_SPLINE_SURFACE(1,2,((#111833,#111834,#111835,#111836,#111837),(#111838,
#111839,#111840,#111841,#111842)),.UNSPECIFIED.,.F.,.F.,.F.)
B_SPLINE_SURFACE_WITH_KNOTS((2,2),(3,2,3),(0.,0.290398665175405),(0.452333244828615,
0.452924869174516,0.470122329512318),.UNSPECIFIED.)
GEOMETRIC_REPRESENTATION_ITEM()
RATIONAL_B_SPLINE_SURFACE(((0.988732477628006,0.988732477628006,0.988732477628006,
0.986812255267055,0.987798766302166),(0.988732477628006,0.988732477628006,
0.988732477628006,0.986812255267055,0.987798766302166)))
REPRESENTATION_ITEM('')
SURFACE()
);
#1082=(
BOUNDED_SURFACE()
B_SPLINE_SURFACE(1,2,((#111844,#111845,#111846),(#111847,#111848,#111849)),
 .UNSPECIFIED.,.F.,.F.,.F.)
B_SPLINE_SURFACE_WITH_KNOTS((2,2),(3,3),(0.,0.289681084359922),(0.262994994770443,
0.280433083165913),.UNSPECIFIED.)
GEOMETRIC_REPRESENTATION_ITEM()
RATIONAL_B_SPLINE_SURFACE(((0.989123653000983,0.991350813683904,0.996566619267863),
(0.989123653000983,0.991350813683904,0.996566619267863)))
REPRESENTATION_ITEM('')
SURFACE()
);
#1083=(
BOUNDED_SURFACE()
B_SPLINE_SURFACE(1,2,((#111858,#111859,#111860,#111861,#111862),(#111863,
#111864,#111865,#111866,#111867)),.UNSPECIFIED.,.F.,.F.,.F.)
B_SPLINE_SURFACE_WITH_KNOTS((2,2),(3,2,3),(0.,0.290398665173023),(0.452333244831502,
0.452924869174516,0.470122329512318),.UNSPECIFIED.)
GEOMETRIC_REPRESENTATION_ITEM()
RATIONAL_B_SPLINE_SURFACE(((0.988732477628006,0.988732477628006,0.988732477628006,
0.986812255267055,0.987798766302167),(0.988732477628006,0.988732477628006,
0.988732477628006,0.986812255267055,0.987798766302167)))
REPRESENTATION_ITEM('')
SURFACE()
);
#1084=(
BOUNDED_SURFACE()
B_SPLINE_SURFACE(1,2,((#111869,#111870,#111871),(#111872,#111873,#111874)),
 .UNSPECIFIED.,.F.,.F.,.F.)
B_SPLINE_SURFACE_WITH_KNOTS((2,2),(3,3),(0.,0.289681084359919),(0.262994994770443,
0.280433083165913),.UNSPECIFIED.)
GEOMETRIC_REPRESENTATION_ITEM()
RATIONAL_B_SPLINE_SURFACE(((0.989123653000983,0.991350813683904,0.996566619267864),
(0.989123653000983,0.991350813683904,0.996566619267864)))
REPRESENTATION_ITEM('')
SURFACE()
);
#1085=(
BOUNDED_SURFACE()
B_SPLINE_SURFACE(1,2,((#111883,#111884,#111885,#111886,#111887),(#111888,
#111889,#111890,#111891,#111892)),.UNSPECIFIED.,.F.,.F.,.F.)
B_SPLINE_SURFACE_WITH_KNOTS((2,2),(3,2,3),(0.,0.290398665142381),(0.452333244861645,
0.452924869174517,0.470122329512318),.UNSPECIFIED.)
GEOMETRIC_REPRESENTATION_ITEM()
RATIONAL_B_SPLINE_SURFACE(((0.988732477628006,0.988732477628006,0.988732477628006,
0.986812255267055,0.987798766302167),(0.988732477628006,0.988732477628006,
0.988732477628006,0.986812255267055,0.987798766302167)))
REPRESENTATION_ITEM('')
SURFACE()
);
#1086=(
BOUNDED_SURFACE()
B_SPLINE_SURFACE(1,2,((#111894,#111895,#111896),(#111897,#111898,#111899)),
 .UNSPECIFIED.,.F.,.F.,.F.)
B_SPLINE_SURFACE_WITH_KNOTS((2,2),(3,3),(0.,0.289681084359921),(0.262994994770443,
0.280433083165913),.UNSPECIFIED.)
GEOMETRIC_REPRESENTATION_ITEM()
RATIONAL_B_SPLINE_SURFACE(((0.989123653000983,0.991350813683904,0.996566619267864),
(0.989123653000983,0.991350813683904,0.996566619267864)))
REPRESENTATION_ITEM('')
SURFACE()
);
#1087=(
BOUNDED_SURFACE()
B_SPLINE_SURFACE(1,2,((#111908,#111909,#111910,#111911,#111912),(#111913,
#111914,#111915,#111916,#111917)),.UNSPECIFIED.,.F.,.F.,.F.)
B_SPLINE_SURFACE_WITH_KNOTS((2,2),(3,2,3),(0.,0.290398665147505),(0.452333244857022,
0.452924869174516,0.470122329512318),.UNSPECIFIED.)
GEOMETRIC_REPRESENTATION_ITEM()
RATIONAL_B_SPLINE_SURFACE(((0.988732477628006,0.988732477628006,0.988732477628006,
0.986812255267055,0.987798766302166),(0.988732477628006,0.988732477628006,
0.988732477628006,0.986812255267055,0.987798766302166)))
REPRESENTATION_ITEM('')
SURFACE()
);
#1088=(
BOUNDED_SURFACE()
B_SPLINE_SURFACE(1,2,((#111919,#111920,#111921),(#111922,#111923,#111924)),
 .UNSPECIFIED.,.F.,.F.,.F.)
B_SPLINE_SURFACE_WITH_KNOTS((2,2),(3,3),(0.,0.289681084359921),(0.262994994770444,
0.280433083165913),.UNSPECIFIED.)
GEOMETRIC_REPRESENTATION_ITEM()
RATIONAL_B_SPLINE_SURFACE(((0.989123653000983,0.991350813683904,0.996566619267863),
(0.989123653000983,0.991350813683904,0.996566619267863)))
REPRESENTATION_ITEM('')
SURFACE()
);
#1089=(
BOUNDED_SURFACE()
B_SPLINE_SURFACE(1,2,((#111933,#111934,#111935,#111936,#111937),(#111938,
#111939,#111940,#111941,#111942)),.UNSPECIFIED.,.F.,.F.,.F.)
B_SPLINE_SURFACE_WITH_KNOTS((2,2),(3,2,3),(0.,0.290398665150954),(0.452333244853345,
0.452924869174516,0.470122329512318),.UNSPECIFIED.)
GEOMETRIC_REPRESENTATION_ITEM()
RATIONAL_B_SPLINE_SURFACE(((0.988732477628006,0.988732477628006,0.988732477628006,
0.986812255267055,0.987798766302166),(0.988732477628006,0.988732477628006,
0.988732477628006,0.986812255267055,0.987798766302166)))
REPRESENTATION_ITEM('')
SURFACE()
);
#1090=(
BOUNDED_SURFACE()
B_SPLINE_SURFACE(1,2,((#111944,#111945,#111946),(#111947,#111948,#111949)),
 .UNSPECIFIED.,.F.,.F.,.F.)
B_SPLINE_SURFACE_WITH_KNOTS((2,2),(3,3),(0.,0.289681084359921),(0.262994994770444,
0.280433083165913),.UNSPECIFIED.)
GEOMETRIC_REPRESENTATION_ITEM()
RATIONAL_B_SPLINE_SURFACE(((0.989123653000983,0.991350813683904,0.996566619267864),
(0.989123653000983,0.991350813683904,0.996566619267864)))
REPRESENTATION_ITEM('')
SURFACE()
);
#1091=(
BOUNDED_SURFACE()
B_SPLINE_SURFACE(1,2,((#111958,#111959,#111960,#111961,#111962),(#111963,
#111964,#111965,#111966,#111967)),.UNSPECIFIED.,.F.,.F.,.F.)
B_SPLINE_SURFACE_WITH_KNOTS((2,2),(3,2,3),(0.,0.290398665158173),(0.45233324484718,
0.452924869174516,0.470122329512318),.UNSPECIFIED.)
GEOMETRIC_REPRESENTATION_ITEM()
RATIONAL_B_SPLINE_SURFACE(((0.988732477628006,0.988732477628006,0.988732477628006,
0.986812255267055,0.987798766302167),(0.988732477628006,0.988732477628006,
0.988732477628006,0.986812255267055,0.987798766302166)))
REPRESENTATION_ITEM('')
SURFACE()
);
#1092=(
BOUNDED_SURFACE()
B_SPLINE_SURFACE(1,2,((#111969,#111970,#111971),(#111972,#111973,#111974)),
 .UNSPECIFIED.,.F.,.F.,.F.)
B_SPLINE_SURFACE_WITH_KNOTS((2,2),(3,3),(0.,0.289681084359921),(0.262994994770444,
0.280433083165913),.UNSPECIFIED.)
GEOMETRIC_REPRESENTATION_ITEM()
RATIONAL_B_SPLINE_SURFACE(((0.989123653000983,0.991350813683904,0.996566619267864),
(0.989123653000983,0.991350813683904,0.996566619267864)))
REPRESENTATION_ITEM('')
SURFACE()
);
#1093=(
BOUNDED_SURFACE()
B_SPLINE_SURFACE(1,2,((#111983,#111984,#111985,#111986,#111987),(#111988,
#111989,#111990,#111991,#111992)),.UNSPECIFIED.,.F.,.F.,.F.)
B_SPLINE_SURFACE_WITH_KNOTS((2,2),(3,2,3),(0.,0.290398665174958),(0.452333244829107,
0.452924869174517,0.470122329512318),.UNSPECIFIED.)
GEOMETRIC_REPRESENTATION_ITEM()
RATIONAL_B_SPLINE_SURFACE(((0.988732477628005,0.988732477628005,0.988732477628005,
0.986812255267055,0.987798766302167),(0.988732477628005,0.988732477628005,
0.988732477628005,0.986812255267055,0.987798766302167)))
REPRESENTATION_ITEM('')
SURFACE()
);
#1094=(
BOUNDED_SURFACE()
B_SPLINE_SURFACE(1,2,((#111994,#111995,#111996),(#111997,#111998,#111999)),
 .UNSPECIFIED.,.F.,.F.,.F.)
B_SPLINE_SURFACE_WITH_KNOTS((2,2),(3,3),(0.,0.28968108435993),(0.262994994770444,
0.280433083165913),.UNSPECIFIED.)
GEOMETRIC_REPRESENTATION_ITEM()
RATIONAL_B_SPLINE_SURFACE(((0.989123653000983,0.991350813683904,0.996566619267864),
(0.989123653000983,0.991350813683904,0.996566619267864)))
REPRESENTATION_ITEM('')
SURFACE()
);
#1095=(
BOUNDED_SURFACE()
B_SPLINE_SURFACE(1,2,((#112008,#112009,#112010,#112011,#112012),(#112013,
#112014,#112015,#112016,#112017)),.UNSPECIFIED.,.F.,.F.,.F.)
B_SPLINE_SURFACE_WITH_KNOTS((2,2),(3,2,3),(0.,0.290398665152165),(0.452333244851786,
0.452924869174515,0.470122329512318),.UNSPECIFIED.)
GEOMETRIC_REPRESENTATION_ITEM()
RATIONAL_B_SPLINE_SURFACE(((0.988732477628006,0.988732477628006,0.988732477628006,
0.986812255267055,0.987798766302166),(0.988732477628006,0.988732477628006,
0.988732477628006,0.986812255267055,0.987798766302166)))
REPRESENTATION_ITEM('')
SURFACE()
);
#1096=(
BOUNDED_SURFACE()
B_SPLINE_SURFACE(1,2,((#112019,#112020,#112021),(#112022,#112023,#112024)),
 .UNSPECIFIED.,.F.,.F.,.F.)
B_SPLINE_SURFACE_WITH_KNOTS((2,2),(3,3),(0.,0.289681084359921),(0.262994994770443,
0.280433083165913),.UNSPECIFIED.)
GEOMETRIC_REPRESENTATION_ITEM()
RATIONAL_B_SPLINE_SURFACE(((0.989123653000983,0.991350813683904,0.996566619267863),
(0.989123653000983,0.991350813683904,0.996566619267863)))
REPRESENTATION_ITEM('')
SURFACE()
);
#1097=(
BOUNDED_SURFACE()
B_SPLINE_SURFACE(1,2,((#112033,#112034,#112035,#112036,#112037),(#112038,
#112039,#112040,#112041,#112042)),.UNSPECIFIED.,.F.,.F.,.F.)
B_SPLINE_SURFACE_WITH_KNOTS((2,2),(3,2,3),(0.,0.290398665180164),(0.452333244824412,
0.452924869174517,0.470122329512318),.UNSPECIFIED.)
GEOMETRIC_REPRESENTATION_ITEM()
RATIONAL_B_SPLINE_SURFACE(((0.988732477628006,0.988732477628006,0.988732477628006,
0.986812255267055,0.987798766302167),(0.988732477628006,0.988732477628006,
0.988732477628006,0.986812255267055,0.987798766302167)))
REPRESENTATION_ITEM('')
SURFACE()
);
#1098=(
BOUNDED_SURFACE()
B_SPLINE_SURFACE(1,2,((#112044,#112045,#112046),(#112047,#112048,#112049)),
 .UNSPECIFIED.,.F.,.F.,.F.)
B_SPLINE_SURFACE_WITH_KNOTS((2,2),(3,3),(0.,0.289681084359926),(0.262994994770443,
0.280433083165913),.UNSPECIFIED.)
GEOMETRIC_REPRESENTATION_ITEM()
RATIONAL_B_SPLINE_SURFACE(((0.989123653000983,0.991350813683904,0.996566619267863),
(0.989123653000983,0.991350813683904,0.996566619267863)))
REPRESENTATION_ITEM('')
SURFACE()
);
#1099=(
BOUNDED_SURFACE()
B_SPLINE_SURFACE(1,2,((#112058,#112059,#112060,#112061,#112062),(#112063,
#112064,#112065,#112066,#112067)),.UNSPECIFIED.,.F.,.F.,.F.)
B_SPLINE_SURFACE_WITH_KNOTS((2,2),(3,2,3),(0.,0.290398665174101),(0.45233324482984,
0.452924869174517,0.470122329512318),.UNSPECIFIED.)
GEOMETRIC_REPRESENTATION_ITEM()
RATIONAL_B_SPLINE_SURFACE(((0.988732477628005,0.988732477628005,0.988732477628005,
0.986812255267055,0.987798766302166),(0.988732477628005,0.988732477628005,
0.988732477628005,0.986812255267055,0.987798766302166)))
REPRESENTATION_ITEM('')
SURFACE()
);
#1100=(
BOUNDED_SURFACE()
B_SPLINE_SURFACE(1,2,((#112069,#112070,#112071),(#112072,#112073,#112074)),
 .UNSPECIFIED.,.F.,.F.,.F.)
B_SPLINE_SURFACE_WITH_KNOTS((2,2),(3,3),(0.,0.289681084359926),(0.262994994770443,
0.280433083165913),.UNSPECIFIED.)
GEOMETRIC_REPRESENTATION_ITEM()
RATIONAL_B_SPLINE_SURFACE(((0.989123653000983,0.991350813683904,0.996566619267864),
(0.989123653000983,0.991350813683904,0.996566619267864)))
REPRESENTATION_ITEM('')
SURFACE()
);
#1101=(
BOUNDED_SURFACE()
B_SPLINE_SURFACE(1,2,((#112083,#112084,#112085,#112086,#112087),(#112088,
#112089,#112090,#112091,#112092)),.UNSPECIFIED.,.F.,.F.,.F.)
B_SPLINE_SURFACE_WITH_KNOTS((2,2),(3,2,3),(0.,0.29039866517598),(0.452333244829113,
0.452924869174518,0.470122329512318),.UNSPECIFIED.)
GEOMETRIC_REPRESENTATION_ITEM()
RATIONAL_B_SPLINE_SURFACE(((0.988732477628005,0.988732477628005,0.988732477628005,
0.986812255267055,0.987798766302166),(0.988732477628005,0.988732477628005,
0.988732477628005,0.986812255267055,0.987798766302166)))
REPRESENTATION_ITEM('')
SURFACE()
);
#1102=(
BOUNDED_SURFACE()
B_SPLINE_SURFACE(1,2,((#112094,#112095,#112096),(#112097,#112098,#112099)),
 .UNSPECIFIED.,.F.,.F.,.F.)
B_SPLINE_SURFACE_WITH_KNOTS((2,2),(3,3),(0.,0.289681084359929),(0.262994994770443,
0.280433083165913),.UNSPECIFIED.)
GEOMETRIC_REPRESENTATION_ITEM()
RATIONAL_B_SPLINE_SURFACE(((0.989123653000983,0.991350813683904,0.996566619267863),
(0.989123653000983,0.991350813683904,0.996566619267863)))
REPRESENTATION_ITEM('')
SURFACE()
);
#1103=(
BOUNDED_SURFACE()
B_SPLINE_SURFACE(1,2,((#112108,#112109,#112110,#112111,#112112),(#112113,
#112114,#112115,#112116,#112117)),.UNSPECIFIED.,.F.,.F.,.F.)
B_SPLINE_SURFACE_WITH_KNOTS((2,2),(3,2,3),(0.,0.290398665149643),(0.452333244855286,
0.452924869174518,0.470122329512318),.UNSPECIFIED.)
GEOMETRIC_REPRESENTATION_ITEM()
RATIONAL_B_SPLINE_SURFACE(((0.988732477628005,0.988732477628005,0.988732477628005,
0.986812255267055,0.987798766302167),(0.988732477628005,0.988732477628005,
0.988732477628005,0.986812255267055,0.987798766302167)))
REPRESENTATION_ITEM('')
SURFACE()
);
#1104=(
BOUNDED_SURFACE()
B_SPLINE_SURFACE(1,2,((#112119,#112120,#112121),(#112122,#112123,#112124)),
 .UNSPECIFIED.,.F.,.F.,.F.)
B_SPLINE_SURFACE_WITH_KNOTS((2,2),(3,3),(0.,0.289681084359926),(0.262994994770443,
0.280433083166016),.UNSPECIFIED.)
GEOMETRIC_REPRESENTATION_ITEM()
RATIONAL_B_SPLINE_SURFACE(((0.989123653000982,0.991350813683917,0.996566619267925),
(0.989123653000982,0.991350813683917,0.996566619267925)))
REPRESENTATION_ITEM('')
SURFACE()
);
#1105=(
BOUNDED_SURFACE()
B_SPLINE_SURFACE(1,2,((#112133,#112134,#112135,#112136,#112137),(#112138,
#112139,#112140,#112141,#112142)),.UNSPECIFIED.,.F.,.F.,.F.)
B_SPLINE_SURFACE_WITH_KNOTS((2,2),(3,2,3),(0.,0.290398665156825),(0.452333244848833,
0.452924869174518,0.470122329512318),.UNSPECIFIED.)
GEOMETRIC_REPRESENTATION_ITEM()
RATIONAL_B_SPLINE_SURFACE(((0.988732477628005,0.988732477628005,0.988732477628005,
0.986812255267055,0.987798766302166),(0.988732477628005,0.988732477628005,
0.988732477628005,0.986812255267055,0.987798766302166)))
REPRESENTATION_ITEM('')
SURFACE()
);
#1106=(
BOUNDED_SURFACE()
B_SPLINE_SURFACE(1,2,((#112144,#112145,#112146),(#112147,#112148,#112149)),
 .UNSPECIFIED.,.F.,.F.,.F.)
B_SPLINE_SURFACE_WITH_KNOTS((2,2),(3,3),(0.,0.289681084359918),(0.262994994770442,
0.280433083166178),.UNSPECIFIED.)
GEOMETRIC_REPRESENTATION_ITEM()
RATIONAL_B_SPLINE_SURFACE(((0.989123653000982,0.991350813683937,0.996566619268022),
(0.989123653000982,0.991350813683937,0.996566619268022)))
REPRESENTATION_ITEM('')
SURFACE()
);
#1107=(
BOUNDED_SURFACE()
B_SPLINE_SURFACE(1,2,((#112158,#112159,#112160,#112161,#112162),(#112163,
#112164,#112165,#112166,#112167)),.UNSPECIFIED.,.F.,.F.,.F.)
B_SPLINE_SURFACE_WITH_KNOTS((2,2),(3,2,3),(0.,0.290398665150478),(0.45233324485367,
0.452924869174517,0.470122329512318),.UNSPECIFIED.)
GEOMETRIC_REPRESENTATION_ITEM()
RATIONAL_B_SPLINE_SURFACE(((0.988732477628005,0.988732477628005,0.988732477628005,
0.986812255267055,0.987798766302167),(0.988732477628005,0.988732477628005,
0.988732477628005,0.986812255267055,0.987798766302167)))
REPRESENTATION_ITEM('')
SURFACE()
);
#1108=(
BOUNDED_SURFACE()
B_SPLINE_SURFACE(1,2,((#112169,#112170,#112171),(#112172,#112173,#112174)),
 .UNSPECIFIED.,.F.,.F.,.F.)
B_SPLINE_SURFACE_WITH_KNOTS((2,2),(3,3),(0.,0.289681084359922),(0.262994994770443,
0.280433083165913),.UNSPECIFIED.)
GEOMETRIC_REPRESENTATION_ITEM()
RATIONAL_B_SPLINE_SURFACE(((0.989123653000983,0.991350813683904,0.996566619267863),
(0.989123653000983,0.991350813683904,0.996566619267863)))
REPRESENTATION_ITEM('')
SURFACE()
);
#1109=(
BOUNDED_SURFACE()
B_SPLINE_SURFACE(1,2,((#112183,#112184,#112185,#112186,#112187),(#112188,
#112189,#112190,#112191,#112192)),.UNSPECIFIED.,.F.,.F.,.F.)
B_SPLINE_SURFACE_WITH_KNOTS((2,2),(3,2,3),(0.,0.290398665153931),(0.452333244851512,
0.452924869174518,0.470122329512318),.UNSPECIFIED.)
GEOMETRIC_REPRESENTATION_ITEM()
RATIONAL_B_SPLINE_SURFACE(((0.988732477628005,0.988732477628005,0.988732477628005,
0.986812255267055,0.987798766302167),(0.988732477628005,0.988732477628005,
0.988732477628005,0.986812255267055,0.987798766302167)))
REPRESENTATION_ITEM('')
SURFACE()
);
#1110=(
BOUNDED_SURFACE()
B_SPLINE_SURFACE(1,2,((#112194,#112195,#112196),(#112197,#112198,#112199)),
 .UNSPECIFIED.,.F.,.F.,.F.)
B_SPLINE_SURFACE_WITH_KNOTS((2,2),(3,3),(0.,0.289681084359929),(0.262994994770444,
0.280433083165913),.UNSPECIFIED.)
GEOMETRIC_REPRESENTATION_ITEM()
RATIONAL_B_SPLINE_SURFACE(((0.989123653000983,0.991350813683904,0.996566619267863),
(0.989123653000983,0.991350813683904,0.996566619267863)))
REPRESENTATION_ITEM('')
SURFACE()
);
#1111=(
BOUNDED_SURFACE()
B_SPLINE_SURFACE(1,2,((#112208,#112209,#112210,#112211,#112212),(#112213,
#112214,#112215,#112216,#112217)),.UNSPECIFIED.,.F.,.F.,.F.)
B_SPLINE_SURFACE_WITH_KNOTS((2,2),(3,2,3),(0.,0.290398665157378),(0.452333244847814,
0.452924869174518,0.470122329512321),.UNSPECIFIED.)
GEOMETRIC_REPRESENTATION_ITEM()
RATIONAL_B_SPLINE_SURFACE(((0.988732477628005,0.988732477628005,0.988732477628005,
0.986812255267055,0.987798766302167),(0.988732477628005,0.988732477628005,
0.988732477628005,0.986812255267055,0.987798766302167)))
REPRESENTATION_ITEM('')
SURFACE()
);
#1112=(
BOUNDED_SURFACE()
B_SPLINE_SURFACE(1,2,((#112219,#112220,#112221),(#112222,#112223,#112224)),
 .UNSPECIFIED.,.F.,.F.,.F.)
B_SPLINE_SURFACE_WITH_KNOTS((2,2),(3,3),(0.,0.289681084359937),(0.262994994770443,
0.280433083165913),.UNSPECIFIED.)
GEOMETRIC_REPRESENTATION_ITEM()
RATIONAL_B_SPLINE_SURFACE(((0.989123653000983,0.991350813683904,0.996566619267863),
(0.989123653000983,0.991350813683904,0.996566619267863)))
REPRESENTATION_ITEM('')
SURFACE()
);
#1113=(
BOUNDED_SURFACE()
B_SPLINE_SURFACE(1,2,((#112233,#112234,#112235,#112236,#112237),(#112238,
#112239,#112240,#112241,#112242)),.UNSPECIFIED.,.F.,.F.,.F.)
B_SPLINE_SURFACE_WITH_KNOTS((2,2),(3,2,3),(0.,0.290398665156934),(0.452333244848014,
0.452924869174518,0.470122329512319),.UNSPECIFIED.)
GEOMETRIC_REPRESENTATION_ITEM()
RATIONAL_B_SPLINE_SURFACE(((0.988732477628005,0.988732477628005,0.988732477628005,
0.986812255267055,0.987798766302166),(0.988732477628005,0.988732477628005,
0.988732477628005,0.986812255267055,0.987798766302166)))
REPRESENTATION_ITEM('')
SURFACE()
);
#1114=(
BOUNDED_SURFACE()
B_SPLINE_SURFACE(1,2,((#112244,#112245,#112246),(#112247,#112248,#112249)),
 .UNSPECIFIED.,.F.,.F.,.F.)
B_SPLINE_SURFACE_WITH_KNOTS((2,2),(3,3),(0.,0.289681084359929),(0.262994994770443,
0.280433083165913),.UNSPECIFIED.)
GEOMETRIC_REPRESENTATION_ITEM()
RATIONAL_B_SPLINE_SURFACE(((0.989123653000983,0.991350813683904,0.996566619267863),
(0.989123653000983,0.991350813683904,0.996566619267863)))
REPRESENTATION_ITEM('')
SURFACE()
);
#1115=(
BOUNDED_SURFACE()
B_SPLINE_SURFACE(1,2,((#112258,#112259,#112260,#112261,#112262),(#112263,
#112264,#112265,#112266,#112267)),.UNSPECIFIED.,.F.,.F.,.F.)
B_SPLINE_SURFACE_WITH_KNOTS((2,2),(3,2,3),(0.,0.29039866515975),(0.452333244845127,
0.452924869174518,0.470122329512318),.UNSPECIFIED.)
GEOMETRIC_REPRESENTATION_ITEM()
RATIONAL_B_SPLINE_SURFACE(((0.988732477628005,0.988732477628005,0.988732477628005,
0.986812255267055,0.987798766302166),(0.988732477628005,0.988732477628005,
0.988732477628005,0.986812255267055,0.987798766302167)))
REPRESENTATION_ITEM('')
SURFACE()
);
#1116=(
BOUNDED_SURFACE()
B_SPLINE_SURFACE(1,2,((#112269,#112270,#112271),(#112272,#112273,#112274)),
 .UNSPECIFIED.,.F.,.F.,.F.)
B_SPLINE_SURFACE_WITH_KNOTS((2,2),(3,3),(0.,0.289681084359923),(0.262994994770443,
0.280433083165913),.UNSPECIFIED.)
GEOMETRIC_REPRESENTATION_ITEM()
RATIONAL_B_SPLINE_SURFACE(((0.989123653000983,0.991350813683904,0.996566619267863),
(0.989123653000983,0.991350813683904,0.996566619267863)))
REPRESENTATION_ITEM('')
SURFACE()
);
#1117=(
BOUNDED_SURFACE()
B_SPLINE_SURFACE(1,2,((#112283,#112284,#112285,#112286,#112287),(#112288,
#112289,#112290,#112291,#112292)),.UNSPECIFIED.,.F.,.F.,.F.)
B_SPLINE_SURFACE_WITH_KNOTS((2,2),(3,2,3),(0.,0.29039866518354),(0.452333244822635,
0.452924869174506,0.470122329512318),.UNSPECIFIED.)
GEOMETRIC_REPRESENTATION_ITEM()
RATIONAL_B_SPLINE_SURFACE(((0.988732477628008,0.988732477628008,0.988732477628008,
0.986812255267055,0.987798766302166),(0.988732477628008,0.988732477628008,
0.988732477628008,0.986812255267054,0.987798766302166)))
REPRESENTATION_ITEM('')
SURFACE()
);
#1118=(
BOUNDED_SURFACE()
B_SPLINE_SURFACE(1,2,((#112294,#112295,#112296),(#112297,#112298,#112299)),
 .UNSPECIFIED.,.F.,.F.,.F.)
B_SPLINE_SURFACE_WITH_KNOTS((2,2),(3,3),(0.,0.289681084359921),(0.262994994770443,
0.280433083165913),.UNSPECIFIED.)
GEOMETRIC_REPRESENTATION_ITEM()
RATIONAL_B_SPLINE_SURFACE(((0.989123653000983,0.991350813683904,0.996566619267864),
(0.989123653000983,0.991350813683904,0.996566619267864)))
REPRESENTATION_ITEM('')
SURFACE()
);
#1119=(
BOUNDED_SURFACE()
B_SPLINE_SURFACE(1,2,((#112308,#112309,#112310,#112311,#112312),(#112313,
#112314,#112315,#112316,#112317)),.UNSPECIFIED.,.F.,.F.,.F.)
B_SPLINE_SURFACE_WITH_KNOTS((2,2),(3,2,3),(0.,0.290398665168458),(0.452333244836591,
0.452924869174517,0.470122329512318),.UNSPECIFIED.)
GEOMETRIC_REPRESENTATION_ITEM()
RATIONAL_B_SPLINE_SURFACE(((0.988732477628005,0.988732477628005,0.988732477628005,
0.986812255267055,0.987798766302167),(0.988732477628005,0.988732477628005,
0.988732477628005,0.986812255267055,0.987798766302167)))
REPRESENTATION_ITEM('')
SURFACE()
);
#1120=(
BOUNDED_SURFACE()
B_SPLINE_SURFACE(1,2,((#112319,#112320,#112321),(#112322,#112323,#112324)),
 .UNSPECIFIED.,.F.,.F.,.F.)
B_SPLINE_SURFACE_WITH_KNOTS((2,2),(3,3),(0.,0.289681084359922),(0.262994994770443,
0.280433083165913),.UNSPECIFIED.)
GEOMETRIC_REPRESENTATION_ITEM()
RATIONAL_B_SPLINE_SURFACE(((0.989123653000983,0.991350813683904,0.996566619267863),
(0.989123653000983,0.991350813683904,0.996566619267863)))
REPRESENTATION_ITEM('')
SURFACE()
);
#1121=(
BOUNDED_SURFACE()
B_SPLINE_SURFACE(1,2,((#112333,#112334,#112335,#112336,#112337),(#112338,
#112339,#112340,#112341,#112342)),.UNSPECIFIED.,.F.,.F.,.F.)
B_SPLINE_SURFACE_WITH_KNOTS((2,2),(3,2,3),(0.,0.290398665166776),(0.452333244838288,
0.452924869174517,0.470122329512318),.UNSPECIFIED.)
GEOMETRIC_REPRESENTATION_ITEM()
RATIONAL_B_SPLINE_SURFACE(((0.988732477628005,0.988732477628005,0.988732477628005,
0.986812255267055,0.987798766302166),(0.988732477628005,0.988732477628005,
0.988732477628005,0.986812255267055,0.987798766302166)))
REPRESENTATION_ITEM('')
SURFACE()
);
#1122=(
BOUNDED_SURFACE()
B_SPLINE_SURFACE(1,2,((#112344,#112345,#112346,#112347,#112348),(#112349,
#112350,#112351,#112352,#112353)),.UNSPECIFIED.,.F.,.F.,.F.)
B_SPLINE_SURFACE_WITH_KNOTS((2,2),(3,2,3),(0.,0.289681084359925),(0.400939219852743,
0.418312080773439,0.418485809382646),.UNSPECIFIED.)
GEOMETRIC_REPRESENTATION_ITEM()
RATIONAL_B_SPLINE_SURFACE(((0.988105937622242,0.989485911589766,0.993832214116773,
0.993832214116773,0.993832214116773),(0.988105937622242,0.989485911589766,
0.993832214116773,0.993832214116773,0.993832214116773)))
REPRESENTATION_ITEM('')
SURFACE()
);
#1123=(
BOUNDED_SURFACE()
B_SPLINE_SURFACE(1,2,((#112364,#112365,#112366,#112367,#112368),(#112369,
#112370,#112371,#112372,#112373)),.UNSPECIFIED.,.F.,.F.,.F.)
B_SPLINE_SURFACE_WITH_KNOTS((2,2),(3,2,3),(0.,0.289807040991894),(0.314770575782761,
0.314942866188516,0.332171906764074),.UNSPECIFIED.)
GEOMETRIC_REPRESENTATION_ITEM()
RATIONAL_B_SPLINE_SURFACE(((0.987877375613931,0.987877375613931,0.987877375613931,
0.986779141655835,0.988598326347701),(0.987877375613931,0.987877375613931,
0.987877375613931,0.986779141655835,0.988598326347701)))
REPRESENTATION_ITEM('')
SURFACE()
);
#1124=(
BOUNDED_SURFACE()
B_SPLINE_SURFACE(1,2,((#112399,#112400,#112401,#112402,#112403),(#112404,
#112405,#112406,#112407,#112408)),.UNSPECIFIED.,.F.,.F.,.F.)
B_SPLINE_SURFACE_WITH_KNOTS((2,2),(3,2,3),(0.,0.289681084359929),(0.400939219852743,
0.418312080773434,0.418485809382641),.UNSPECIFIED.)
GEOMETRIC_REPRESENTATION_ITEM()
RATIONAL_B_SPLINE_SURFACE(((0.988105937622242,0.989485911589766,0.99383221411677,
0.99383221411677,0.99383221411677),(0.988105937622242,0.989485911589766,
0.99383221411677,0.99383221411677,0.99383221411677)))
REPRESENTATION_ITEM('')
SURFACE()
);
#1125=(
BOUNDED_SURFACE()
B_SPLINE_SURFACE(1,2,((#112410,#112411,#112412,#112413,#112414),(#112415,
#112416,#112417,#112418,#112419)),.UNSPECIFIED.,.F.,.F.,.F.)
B_SPLINE_SURFACE_WITH_KNOTS((2,2),(3,2,3),(0.,0.289807040992009),(0.314770575782761,
0.314942866188516,0.332171906764074),.UNSPECIFIED.)
GEOMETRIC_REPRESENTATION_ITEM()
RATIONAL_B_SPLINE_SURFACE(((0.987877375613931,0.987877375613931,0.987877375613931,
0.986779141655835,0.988598326347701),(0.987877375613931,0.987877375613931,
0.987877375613931,0.986779141655835,0.988598326347701)))
REPRESENTATION_ITEM('')
SURFACE()
);
#1126=(
BOUNDED_SURFACE()
B_SPLINE_SURFACE(1,2,((#112445,#112446,#112447,#112448,#112449),(#112450,
#112451,#112452,#112453,#112454)),.UNSPECIFIED.,.F.,.F.,.F.)
B_SPLINE_SURFACE_WITH_KNOTS((2,2),(3,2,3),(0.,0.289681084359929),(0.400939219852742,
0.418312080773434,0.418485809382641),.UNSPECIFIED.)
GEOMETRIC_REPRESENTATION_ITEM()
RATIONAL_B_SPLINE_SURFACE(((0.988105937622242,0.989485911589766,0.99383221411677,
0.99383221411677,0.99383221411677),(0.988105937622242,0.989485911589766,
0.99383221411677,0.99383221411677,0.99383221411677)))
REPRESENTATION_ITEM('')
SURFACE()
);
#1127=(
BOUNDED_SURFACE()
B_SPLINE_SURFACE(1,2,((#112456,#112457,#112458,#112459,#112460),(#112461,
#112462,#112463,#112464,#112465)),.UNSPECIFIED.,.F.,.F.,.F.)
B_SPLINE_SURFACE_WITH_KNOTS((2,2),(3,2,3),(0.,0.289807040993042),(0.314770575782756,
0.314942866188511,0.332171906764072),.UNSPECIFIED.)
GEOMETRIC_REPRESENTATION_ITEM()
RATIONAL_B_SPLINE_SURFACE(((0.987877375613932,0.987877375613932,0.987877375613932,
0.986779141655835,0.988598326347701),(0.987877375613932,0.987877375613932,
0.987877375613932,0.986779141655835,0.988598326347701)))
REPRESENTATION_ITEM('')
SURFACE()
);
#1128=(
BOUNDED_SURFACE()
B_SPLINE_SURFACE(1,2,((#112491,#112492,#112493,#112494,#112495),(#112496,
#112497,#112498,#112499,#112500)),.UNSPECIFIED.,.F.,.F.,.F.)
B_SPLINE_SURFACE_WITH_KNOTS((2,2),(3,2,3),(0.,0.289681084359915),(0.40093921985274,
0.418312080773435,0.418485809382642),.UNSPECIFIED.)
GEOMETRIC_REPRESENTATION_ITEM()
RATIONAL_B_SPLINE_SURFACE(((0.988105937622242,0.989485911589765,0.99383221411677,
0.99383221411677,0.99383221411677),(0.988105937622242,0.989485911589765,
0.99383221411677,0.99383221411677,0.99383221411677)))
REPRESENTATION_ITEM('')
SURFACE()
);
#1129=(
BOUNDED_SURFACE()
B_SPLINE_SURFACE(1,2,((#112502,#112503,#112504,#112505,#112506),(#112507,
#112508,#112509,#112510,#112511)),.UNSPECIFIED.,.F.,.F.,.F.)
B_SPLINE_SURFACE_WITH_KNOTS((2,2),(3,2,3),(0.,0.289807040992772),(0.314770575782758,
0.314942866188513,0.332171906764074),.UNSPECIFIED.)
GEOMETRIC_REPRESENTATION_ITEM()
RATIONAL_B_SPLINE_SURFACE(((0.987877375613932,0.987877375613932,0.987877375613932,
0.986779141655835,0.988598326347701),(0.987877375613932,0.987877375613932,
0.987877375613932,0.986779141655835,0.988598326347701)))
REPRESENTATION_ITEM('')
SURFACE()
);
#1130=(
BOUNDED_SURFACE()
B_SPLINE_SURFACE(1,2,((#112537,#112538,#112539,#112540,#112541),(#112542,
#112543,#112544,#112545,#112546)),.UNSPECIFIED.,.F.,.F.,.F.)
B_SPLINE_SURFACE_WITH_KNOTS((2,2),(3,2,3),(0.,0.289681084359922),(0.400939219852742,
0.41831208077346,0.418485809382667),.UNSPECIFIED.)
GEOMETRIC_REPRESENTATION_ITEM()
RATIONAL_B_SPLINE_SURFACE(((0.988105937622242,0.989485911589768,0.993832214116783,
0.993832214116783,0.993832214116783),(0.988105937622242,0.989485911589768,
0.993832214116783,0.993832214116783,0.993832214116783)))
REPRESENTATION_ITEM('')
SURFACE()
);
#1131=(
BOUNDED_SURFACE()
B_SPLINE_SURFACE(1,2,((#112548,#112549,#112550,#112551,#112552),(#112553,
#112554,#112555,#112556,#112557)),.UNSPECIFIED.,.F.,.F.,.F.)
B_SPLINE_SURFACE_WITH_KNOTS((2,2),(3,2,3),(0.,0.2898070409925),(0.314770575782761,
0.314942866188516,0.332171906764074),.UNSPECIFIED.)
GEOMETRIC_REPRESENTATION_ITEM()
RATIONAL_B_SPLINE_SURFACE(((0.987877375613931,0.987877375613931,0.987877375613931,
0.986779141655835,0.988598326347701),(0.987877375613931,0.987877375613931,
0.987877375613931,0.986779141655835,0.988598326347701)))
REPRESENTATION_ITEM('')
SURFACE()
);
#1132=(
BOUNDED_SURFACE()
B_SPLINE_SURFACE(1,2,((#112583,#112584,#112585,#112586,#112587),(#112588,
#112589,#112590,#112591,#112592)),.UNSPECIFIED.,.F.,.F.,.F.)
B_SPLINE_SURFACE_WITH_KNOTS((2,2),(3,2,3),(0.,0.289681084359915),(0.400939219852743,
0.418312080773434,0.418485809382641),.UNSPECIFIED.)
GEOMETRIC_REPRESENTATION_ITEM()
RATIONAL_B_SPLINE_SURFACE(((0.988105937622242,0.989485911589766,0.99383221411677,
0.99383221411677,0.99383221411677),(0.988105937622242,0.989485911589766,
0.99383221411677,0.99383221411677,0.99383221411677)))
REPRESENTATION_ITEM('')
SURFACE()
);
#1133=(
BOUNDED_SURFACE()
B_SPLINE_SURFACE(1,2,((#112594,#112595,#112596,#112597,#112598),(#112599,
#112600,#112601,#112602,#112603)),.UNSPECIFIED.,.F.,.F.,.F.)
B_SPLINE_SURFACE_WITH_KNOTS((2,2),(3,2,3),(0.,0.289807040992675),(0.314770575782761,
0.314942866188516,0.332171906764074),.UNSPECIFIED.)
GEOMETRIC_REPRESENTATION_ITEM()
RATIONAL_B_SPLINE_SURFACE(((0.987877375613931,0.987877375613931,0.987877375613931,
0.986779141655835,0.988598326347701),(0.987877375613931,0.987877375613931,
0.987877375613931,0.986779141655835,0.988598326347701)))
REPRESENTATION_ITEM('')
SURFACE()
);
#1134=(
BOUNDED_SURFACE()
B_SPLINE_SURFACE(1,2,((#112629,#112630,#112631,#112632,#112633),(#112634,
#112635,#112636,#112637,#112638)),.UNSPECIFIED.,.F.,.F.,.F.)
B_SPLINE_SURFACE_WITH_KNOTS((2,2),(3,2,3),(0.,0.289681084359923),(0.400939219852743,
0.418312080773434,0.418485809382641),.UNSPECIFIED.)
GEOMETRIC_REPRESENTATION_ITEM()
RATIONAL_B_SPLINE_SURFACE(((0.988105937622242,0.989485911589766,0.99383221411677,
0.99383221411677,0.99383221411677),(0.988105937622242,0.989485911589766,
0.99383221411677,0.99383221411677,0.99383221411677)))
REPRESENTATION_ITEM('')
SURFACE()
);
#1135=(
BOUNDED_SURFACE()
B_SPLINE_SURFACE(1,2,((#112640,#112641,#112642,#112643,#112644),(#112645,
#112646,#112647,#112648,#112649)),.UNSPECIFIED.,.F.,.F.,.F.)
B_SPLINE_SURFACE_WITH_KNOTS((2,2),(3,2,3),(0.,0.289807040991735),(0.314770575782761,
0.314942866188516,0.332171906764071),.UNSPECIFIED.)
GEOMETRIC_REPRESENTATION_ITEM()
RATIONAL_B_SPLINE_SURFACE(((0.987877375613931,0.987877375613931,0.987877375613931,
0.986779141655835,0.9885983263477),(0.987877375613931,0.987877375613931,
0.987877375613931,0.986779141655835,0.9885983263477)))
REPRESENTATION_ITEM('')
SURFACE()
);
#1136=(
BOUNDED_SURFACE()
B_SPLINE_SURFACE(1,2,((#112657,#112658,#112659,#112660,#112661),(#112662,
#112663,#112664,#112665,#112666)),.UNSPECIFIED.,.F.,.F.,.F.)
B_SPLINE_SURFACE_WITH_KNOTS((2,2),(3,2,3),(0.,0.289681084359923),(0.40093921985274,
0.418312080773434,0.418485809382641),.UNSPECIFIED.)
GEOMETRIC_REPRESENTATION_ITEM()
RATIONAL_B_SPLINE_SURFACE(((0.988105937622241,0.989485911589765,0.99383221411677,
0.99383221411677,0.99383221411677),(0.988105937622241,0.989485911589765,
0.99383221411677,0.99383221411677,0.99383221411677)))
REPRESENTATION_ITEM('')
SURFACE()
);
#1137=(
BOUNDED_SURFACE()
B_SPLINE_SURFACE(1,2,((#112668,#112669,#112670,#112671,#112672),(#112673,
#112674,#112675,#112676,#112677)),.UNSPECIFIED.,.F.,.F.,.F.)
B_SPLINE_SURFACE_WITH_KNOTS((2,2),(3,2,3),(0.,0.289807040991743),(0.314770575782761,
0.314942866188516,0.332171906764072),.UNSPECIFIED.)
GEOMETRIC_REPRESENTATION_ITEM()
RATIONAL_B_SPLINE_SURFACE(((0.987877375613931,0.987877375613931,0.987877375613931,
0.986779141655835,0.9885983263477),(0.987877375613931,0.987877375613931,
0.987877375613931,0.986779141655835,0.9885983263477)))
REPRESENTATION_ITEM('')
SURFACE()
);
#1138=(
BOUNDED_SURFACE()
B_SPLINE_SURFACE(1,2,((#112703,#112704,#112705,#112706,#112707),(#112708,
#112709,#112710,#112711,#112712)),.UNSPECIFIED.,.F.,.F.,.F.)
B_SPLINE_SURFACE_WITH_KNOTS((2,2),(3,2,3),(0.,0.289681084359925),(0.40093921985274,
0.418312080773435,0.418485809382642),.UNSPECIFIED.)
GEOMETRIC_REPRESENTATION_ITEM()
RATIONAL_B_SPLINE_SURFACE(((0.988105937622242,0.989485911589765,0.99383221411677,
0.99383221411677,0.99383221411677),(0.988105937622242,0.989485911589765,
0.99383221411677,0.99383221411677,0.99383221411677)))
REPRESENTATION_ITEM('')
SURFACE()
);
#1139=(
BOUNDED_SURFACE()
B_SPLINE_SURFACE(1,2,((#112714,#112715,#112716,#112717,#112718),(#112719,
#112720,#112721,#112722,#112723)),.UNSPECIFIED.,.F.,.F.,.F.)
B_SPLINE_SURFACE_WITH_KNOTS((2,2),(3,2,3),(0.,0.289807040991848),(0.314770575782761,
0.314942866188516,0.332171906764071),.UNSPECIFIED.)
GEOMETRIC_REPRESENTATION_ITEM()
RATIONAL_B_SPLINE_SURFACE(((0.987877375613931,0.987877375613931,0.987877375613931,
0.986779141655835,0.9885983263477),(0.987877375613931,0.987877375613931,
0.987877375613931,0.986779141655835,0.9885983263477)))
REPRESENTATION_ITEM('')
SURFACE()
);
#1140=(
BOUNDED_SURFACE()
B_SPLINE_SURFACE(1,2,((#112749,#112750,#112751,#112752,#112753),(#112754,
#112755,#112756,#112757,#112758)),.UNSPECIFIED.,.F.,.F.,.F.)
B_SPLINE_SURFACE_WITH_KNOTS((2,2),(3,2,3),(0.,0.28968108435993),(0.40093921985274,
0.418312080773434,0.418485809382641),.UNSPECIFIED.)
GEOMETRIC_REPRESENTATION_ITEM()
RATIONAL_B_SPLINE_SURFACE(((0.988105937622242,0.989485911589765,0.99383221411677,
0.99383221411677,0.99383221411677),(0.988105937622241,0.989485911589765,
0.99383221411677,0.99383221411677,0.99383221411677)))
REPRESENTATION_ITEM('')
SURFACE()
);
#1141=(
BOUNDED_SURFACE()
B_SPLINE_SURFACE(1,2,((#112760,#112761,#112762,#112763,#112764),(#112765,
#112766,#112767,#112768,#112769)),.UNSPECIFIED.,.F.,.F.,.F.)
B_SPLINE_SURFACE_WITH_KNOTS((2,2),(3,2,3),(0.,0.289807040991791),(0.314770575782761,
0.314942866188516,0.332171906764072),.UNSPECIFIED.)
GEOMETRIC_REPRESENTATION_ITEM()
RATIONAL_B_SPLINE_SURFACE(((0.987877375613931,0.987877375613931,0.987877375613931,
0.986779141655835,0.988598326347701),(0.987877375613931,0.987877375613931,
0.987877375613931,0.986779141655836,0.988598326347701)))
REPRESENTATION_ITEM('')
SURFACE()
);
#1142=(
BOUNDED_SURFACE()
B_SPLINE_SURFACE(1,2,((#112795,#112796,#112797,#112798,#112799),(#112800,
#112801,#112802,#112803,#112804)),.UNSPECIFIED.,.F.,.F.,.F.)
B_SPLINE_SURFACE_WITH_KNOTS((2,2),(3,2,3),(0.,0.289681084359921),(0.400939219852741,
0.418312080773434,0.418485809382641),.UNSPECIFIED.)
GEOMETRIC_REPRESENTATION_ITEM()
RATIONAL_B_SPLINE_SURFACE(((0.988105937622242,0.989485911589765,0.99383221411677,
0.99383221411677,0.99383221411677),(0.988105937622242,0.989485911589765,
0.99383221411677,0.99383221411677,0.99383221411677)))
REPRESENTATION_ITEM('')
SURFACE()
);
#1143=(
BOUNDED_SURFACE()
B_SPLINE_SURFACE(1,2,((#112806,#112807,#112808,#112809,#112810),(#112811,
#112812,#112813,#112814,#112815)),.UNSPECIFIED.,.F.,.F.,.F.)
B_SPLINE_SURFACE_WITH_KNOTS((2,2),(3,2,3),(0.,0.289807040991756),(0.314770575782761,
0.314942866188516,0.332171906764071),.UNSPECIFIED.)
GEOMETRIC_REPRESENTATION_ITEM()
RATIONAL_B_SPLINE_SURFACE(((0.987877375613931,0.987877375613931,0.987877375613931,
0.986779141655835,0.9885983263477),(0.987877375613931,0.987877375613931,
0.987877375613931,0.986779141655835,0.9885983263477)))
REPRESENTATION_ITEM('')
SURFACE()
);
#1144=(
BOUNDED_SURFACE()
B_SPLINE_SURFACE(1,2,((#112841,#112842,#112843,#112844,#112845),(#112846,
#112847,#112848,#112849,#112850)),.UNSPECIFIED.,.F.,.F.,.F.)
B_SPLINE_SURFACE_WITH_KNOTS((2,2),(3,2,3),(0.,0.289681084359919),(0.40093921985274,
0.418312080773434,0.418485809382641),.UNSPECIFIED.)
GEOMETRIC_REPRESENTATION_ITEM()
RATIONAL_B_SPLINE_SURFACE(((0.988105937622242,0.989485911589765,0.99383221411677,
0.99383221411677,0.99383221411677),(0.988105937622241,0.989485911589765,
0.99383221411677,0.99383221411677,0.99383221411677)))
REPRESENTATION_ITEM('')
SURFACE()
);
#1145=(
BOUNDED_SURFACE()
B_SPLINE_SURFACE(1,2,((#112852,#112853,#112854,#112855,#112856),(#112857,
#112858,#112859,#112860,#112861)),.UNSPECIFIED.,.F.,.F.,.F.)
B_SPLINE_SURFACE_WITH_KNOTS((2,2),(3,2,3),(0.,0.289807040991712),(0.314770575782761,
0.314942866188516,0.332171906764074),.UNSPECIFIED.)
GEOMETRIC_REPRESENTATION_ITEM()
RATIONAL_B_SPLINE_SURFACE(((0.987877375613931,0.987877375613931,0.987877375613931,
0.986779141655835,0.988598326347701),(0.987877375613931,0.987877375613931,
0.987877375613931,0.986779141655835,0.988598326347701)))
REPRESENTATION_ITEM('')
SURFACE()
);
#1146=(
BOUNDED_SURFACE()
B_SPLINE_SURFACE(1,2,((#112887,#112888,#112889,#112890,#112891),(#112892,
#112893,#112894,#112895,#112896)),.UNSPECIFIED.,.F.,.F.,.F.)
B_SPLINE_SURFACE_WITH_KNOTS((2,2),(3,2,3),(0.,0.289681084359925),(0.400939219852743,
0.418312080773434,0.418485809382641),.UNSPECIFIED.)
GEOMETRIC_REPRESENTATION_ITEM()
RATIONAL_B_SPLINE_SURFACE(((0.988105937622242,0.989485911589766,0.99383221411677,
0.99383221411677,0.99383221411677),(0.988105937622242,0.989485911589766,
0.99383221411677,0.99383221411677,0.99383221411677)))
REPRESENTATION_ITEM('')
SURFACE()
);
#1147=(
BOUNDED_SURFACE()
B_SPLINE_SURFACE(1,2,((#112898,#112899,#112900,#112901,#112902),(#112903,
#112904,#112905,#112906,#112907)),.UNSPECIFIED.,.F.,.F.,.F.)
B_SPLINE_SURFACE_WITH_KNOTS((2,2),(3,2,3),(0.,0.289807040991569),(0.314770575782761,
0.314942866188516,0.332171906764074),.UNSPECIFIED.)
GEOMETRIC_REPRESENTATION_ITEM()
RATIONAL_B_SPLINE_SURFACE(((0.987877375613931,0.987877375613931,0.987877375613931,
0.986779141655835,0.988598326347701),(0.987877375613931,0.987877375613931,
0.987877375613931,0.986779141655835,0.988598326347701)))
REPRESENTATION_ITEM('')
SURFACE()
);
#1148=(
BOUNDED_SURFACE()
B_SPLINE_SURFACE(1,2,((#112933,#112934,#112935,#112936,#112937),(#112938,
#112939,#112940,#112941,#112942)),.UNSPECIFIED.,.F.,.F.,.F.)
B_SPLINE_SURFACE_WITH_KNOTS((2,2),(3,2,3),(0.,0.289681084359925),(0.400939219852742,
0.418312080773434,0.418485809382641),.UNSPECIFIED.)
GEOMETRIC_REPRESENTATION_ITEM()
RATIONAL_B_SPLINE_SURFACE(((0.988105937622242,0.989485911589766,0.99383221411677,
0.99383221411677,0.99383221411677),(0.988105937622242,0.989485911589766,
0.99383221411677,0.99383221411677,0.99383221411677)))
REPRESENTATION_ITEM('')
SURFACE()
);
#1149=(
BOUNDED_SURFACE()
B_SPLINE_SURFACE(1,2,((#112944,#112945,#112946,#112947,#112948),(#112949,
#112950,#112951,#112952,#112953)),.UNSPECIFIED.,.F.,.F.,.F.)
B_SPLINE_SURFACE_WITH_KNOTS((2,2),(3,2,3),(0.,0.289807040991565),(0.314770575782761,
0.314942866188516,0.332171906764074),.UNSPECIFIED.)
GEOMETRIC_REPRESENTATION_ITEM()
RATIONAL_B_SPLINE_SURFACE(((0.987877375613931,0.987877375613931,0.987877375613931,
0.986779141655835,0.988598326347701),(0.987877375613931,0.987877375613931,
0.987877375613931,0.986779141655835,0.988598326347701)))
REPRESENTATION_ITEM('')
SURFACE()
);
#1150=(
BOUNDED_SURFACE()
B_SPLINE_SURFACE(1,2,((#112979,#112980,#112981,#112982,#112983),(#112984,
#112985,#112986,#112987,#112988)),.UNSPECIFIED.,.F.,.F.,.F.)
B_SPLINE_SURFACE_WITH_KNOTS((2,2),(3,2,3),(0.,0.289681084359926),(0.400939219852743,
0.418312080773434,0.418485809382641),.UNSPECIFIED.)
GEOMETRIC_REPRESENTATION_ITEM()
RATIONAL_B_SPLINE_SURFACE(((0.988105937622242,0.989485911589766,0.99383221411677,
0.99383221411677,0.99383221411677),(0.988105937622242,0.989485911589766,
0.99383221411677,0.99383221411677,0.99383221411677)))
REPRESENTATION_ITEM('')
SURFACE()
);
#1151=(
BOUNDED_SURFACE()
B_SPLINE_SURFACE(1,2,((#112990,#112991,#112992,#112993,#112994),(#112995,
#112996,#112997,#112998,#112999)),.UNSPECIFIED.,.F.,.F.,.F.)
B_SPLINE_SURFACE_WITH_KNOTS((2,2),(3,2,3),(0.,0.289807040991566),(0.314770575782761,
0.314942866188516,0.332171906764074),.UNSPECIFIED.)
GEOMETRIC_REPRESENTATION_ITEM()
RATIONAL_B_SPLINE_SURFACE(((0.987877375613931,0.987877375613931,0.987877375613931,
0.986779141655835,0.988598326347701),(0.987877375613931,0.987877375613931,
0.987877375613931,0.986779141655835,0.988598326347701)))
REPRESENTATION_ITEM('')
SURFACE()
);
#1152=(
BOUNDED_SURFACE()
B_SPLINE_SURFACE(1,2,((#113025,#113026,#113027,#113028,#113029),(#113030,
#113031,#113032,#113033,#113034)),.UNSPECIFIED.,.F.,.F.,.F.)
B_SPLINE_SURFACE_WITH_KNOTS((2,2),(3,2,3),(0.,0.289681084359931),(0.400939219852743,
0.418312080773435,0.418485809382642),.UNSPECIFIED.)
GEOMETRIC_REPRESENTATION_ITEM()
RATIONAL_B_SPLINE_SURFACE(((0.988105937622242,0.989485911589766,0.993832214116771,
0.993832214116771,0.993832214116771),(0.988105937622242,0.989485911589766,
0.993832214116771,0.993832214116771,0.993832214116771)))
REPRESENTATION_ITEM('')
SURFACE()
);
#1153=(
BOUNDED_SURFACE()
B_SPLINE_SURFACE(1,2,((#113036,#113037,#113038,#113039,#113040),(#113041,
#113042,#113043,#113044,#113045)),.UNSPECIFIED.,.F.,.F.,.F.)
B_SPLINE_SURFACE_WITH_KNOTS((2,2),(3,2,3),(0.,0.289807040991562),(0.314770575782761,
0.314942866188516,0.332171906764074),.UNSPECIFIED.)
GEOMETRIC_REPRESENTATION_ITEM()
RATIONAL_B_SPLINE_SURFACE(((0.987877375613931,0.987877375613931,0.987877375613931,
0.986779141655835,0.988598326347701),(0.987877375613931,0.987877375613931,
0.987877375613931,0.986779141655835,0.988598326347701)))
REPRESENTATION_ITEM('')
SURFACE()
);
#1154=(
BOUNDED_SURFACE()
B_SPLINE_SURFACE(1,2,((#113071,#113072,#113073,#113074,#113075),(#113076,
#113077,#113078,#113079,#113080)),.UNSPECIFIED.,.F.,.F.,.F.)
B_SPLINE_SURFACE_WITH_KNOTS((2,2),(3,2,3),(0.,0.289681084359919),(0.400939219852743,
0.418312080773434,0.418485809382641),.UNSPECIFIED.)
GEOMETRIC_REPRESENTATION_ITEM()
RATIONAL_B_SPLINE_SURFACE(((0.988105937622242,0.989485911589766,0.99383221411677,
0.99383221411677,0.99383221411677),(0.988105937622242,0.989485911589766,
0.99383221411677,0.99383221411677,0.99383221411677)))
REPRESENTATION_ITEM('')
SURFACE()
);
#1155=(
BOUNDED_SURFACE()
B_SPLINE_SURFACE(1,2,((#113082,#113083,#113084,#113085,#113086),(#113087,
#113088,#113089,#113090,#113091)),.UNSPECIFIED.,.F.,.F.,.F.)
B_SPLINE_SURFACE_WITH_KNOTS((2,2),(3,2,3),(0.,0.289807040991562),(0.314770575782761,
0.314942866188516,0.332171906764074),.UNSPECIFIED.)
GEOMETRIC_REPRESENTATION_ITEM()
RATIONAL_B_SPLINE_SURFACE(((0.987877375613931,0.987877375613931,0.987877375613931,
0.986779141655835,0.988598326347701),(0.987877375613931,0.987877375613931,
0.987877375613931,0.986779141655835,0.988598326347701)))
REPRESENTATION_ITEM('')
SURFACE()
);
#1156=(
BOUNDED_SURFACE()
B_SPLINE_SURFACE(1,2,((#113117,#113118,#113119,#113120,#113121),(#113122,
#113123,#113124,#113125,#113126)),.UNSPECIFIED.,.F.,.F.,.F.)
B_SPLINE_SURFACE_WITH_KNOTS((2,2),(3,2,3),(0.,0.28968108435992),(0.400939219852743,
0.418312080773434,0.418485809382641),.UNSPECIFIED.)
GEOMETRIC_REPRESENTATION_ITEM()
RATIONAL_B_SPLINE_SURFACE(((0.988105937622242,0.989485911589766,0.99383221411677,
0.99383221411677,0.99383221411677),(0.988105937622242,0.989485911589766,
0.99383221411677,0.99383221411677,0.99383221411677)))
REPRESENTATION_ITEM('')
SURFACE()
);
#1157=(
BOUNDED_SURFACE()
B_SPLINE_SURFACE(1,2,((#113128,#113129,#113130,#113131,#113132),(#113133,
#113134,#113135,#113136,#113137)),.UNSPECIFIED.,.F.,.F.,.F.)
B_SPLINE_SURFACE_WITH_KNOTS((2,2),(3,2,3),(0.,0.289807040991671),(0.314770575782761,
0.314942866188516,0.332171906764072),.UNSPECIFIED.)
GEOMETRIC_REPRESENTATION_ITEM()
RATIONAL_B_SPLINE_SURFACE(((0.987877375613931,0.987877375613931,0.987877375613931,
0.986779141655835,0.9885983263477),(0.987877375613931,0.987877375613931,
0.987877375613931,0.986779141655836,0.988598326347701)))
REPRESENTATION_ITEM('')
SURFACE()
);
#1158=(
BOUNDED_SURFACE()
B_SPLINE_SURFACE(1,2,((#113163,#113164,#113165,#113166,#113167),(#113168,
#113169,#113170,#113171,#113172)),.UNSPECIFIED.,.F.,.F.,.F.)
B_SPLINE_SURFACE_WITH_KNOTS((2,2),(3,2,3),(0.,0.289681084359922),(0.40093921985274,
0.418312080773434,0.418485809382641),.UNSPECIFIED.)
GEOMETRIC_REPRESENTATION_ITEM()
RATIONAL_B_SPLINE_SURFACE(((0.988105937622242,0.989485911589765,0.99383221411677,
0.99383221411677,0.99383221411677),(0.988105937622242,0.989485911589765,
0.99383221411677,0.99383221411677,0.99383221411677)))
REPRESENTATION_ITEM('')
SURFACE()
);
#1159=(
BOUNDED_SURFACE()
B_SPLINE_SURFACE(1,2,((#113174,#113175,#113176,#113177,#113178),(#113179,
#113180,#113181,#113182,#113183)),.UNSPECIFIED.,.F.,.F.,.F.)
B_SPLINE_SURFACE_WITH_KNOTS((2,2),(3,2,3),(0.,0.289807040992971),(0.314770575782761,
0.314942866188516,0.332171906764072),.UNSPECIFIED.)
GEOMETRIC_REPRESENTATION_ITEM()
RATIONAL_B_SPLINE_SURFACE(((0.987877375613931,0.987877375613931,0.987877375613931,
0.986779141655835,0.9885983263477),(0.987877375613931,0.987877375613931,
0.987877375613931,0.986779141655835,0.9885983263477)))
REPRESENTATION_ITEM('')
SURFACE()
);
#1160=(
BOUNDED_SURFACE()
B_SPLINE_SURFACE(1,2,((#113209,#113210,#113211,#113212,#113213),(#113214,
#113215,#113216,#113217,#113218)),.UNSPECIFIED.,.F.,.F.,.F.)
B_SPLINE_SURFACE_WITH_KNOTS((2,2),(3,2,3),(0.,0.28968108435992),(0.40093921985274,
0.418312080773434,0.418485809382641),.UNSPECIFIED.)
GEOMETRIC_REPRESENTATION_ITEM()
RATIONAL_B_SPLINE_SURFACE(((0.988105937622242,0.989485911589765,0.99383221411677,
0.99383221411677,0.99383221411677),(0.988105937622242,0.989485911589765,
0.99383221411677,0.99383221411677,0.99383221411677)))
REPRESENTATION_ITEM('')
SURFACE()
);
#1161=(
BOUNDED_SURFACE()
B_SPLINE_SURFACE(1,2,((#113220,#113221,#113222,#113223,#113224),(#113225,
#113226,#113227,#113228,#113229)),.UNSPECIFIED.,.F.,.F.,.F.)
B_SPLINE_SURFACE_WITH_KNOTS((2,2),(3,2,3),(0.,0.289807040991813),(0.314770575782761,
0.314942866188516,0.332171906764074),.UNSPECIFIED.)
GEOMETRIC_REPRESENTATION_ITEM()
RATIONAL_B_SPLINE_SURFACE(((0.987877375613931,0.987877375613931,0.987877375613931,
0.986779141655835,0.988598326347701),(0.987877375613931,0.987877375613931,
0.987877375613931,0.986779141655835,0.988598326347701)))
REPRESENTATION_ITEM('')
SURFACE()
);
#1162=(
BOUNDED_SURFACE()
B_SPLINE_SURFACE(1,2,((#113255,#113256,#113257,#113258,#113259),(#113260,
#113261,#113262,#113263,#113264)),.UNSPECIFIED.,.F.,.F.,.F.)
B_SPLINE_SURFACE_WITH_KNOTS((2,2),(3,2,3),(0.,0.289681084359921),(0.400939219852743,
0.418312080773434,0.418485809382641),.UNSPECIFIED.)
GEOMETRIC_REPRESENTATION_ITEM()
RATIONAL_B_SPLINE_SURFACE(((0.988105937622242,0.989485911589766,0.99383221411677,
0.99383221411677,0.99383221411677),(0.988105937622242,0.989485911589766,
0.99383221411677,0.99383221411677,0.99383221411677)))
REPRESENTATION_ITEM('')
SURFACE()
);
#1163=(
BOUNDED_SURFACE()
B_SPLINE_SURFACE(1,2,((#113266,#113267,#113268,#113269,#113270),(#113271,
#113272,#113273,#113274,#113275)),.UNSPECIFIED.,.F.,.F.,.F.)
B_SPLINE_SURFACE_WITH_KNOTS((2,2),(3,2,3),(0.,0.28980704099156),(0.314770575782761,
0.314942866188516,0.332171906764072),.UNSPECIFIED.)
GEOMETRIC_REPRESENTATION_ITEM()
RATIONAL_B_SPLINE_SURFACE(((0.987877375613931,0.987877375613931,0.987877375613931,
0.986779141655835,0.9885983263477),(0.987877375613931,0.987877375613931,
0.987877375613931,0.986779141655835,0.9885983263477)))
REPRESENTATION_ITEM('')
SURFACE()
);
#1164=(
BOUNDED_SURFACE()
B_SPLINE_SURFACE(1,2,((#113301,#113302,#113303,#113304,#113305),(#113306,
#113307,#113308,#113309,#113310)),.UNSPECIFIED.,.F.,.F.,.F.)
B_SPLINE_SURFACE_WITH_KNOTS((2,2),(3,2,3),(0.,0.289681084359923),(0.400939219852741,
0.418312080773434,0.418485809382641),.UNSPECIFIED.)
GEOMETRIC_REPRESENTATION_ITEM()
RATIONAL_B_SPLINE_SURFACE(((0.988105937622242,0.989485911589765,0.99383221411677,
0.99383221411677,0.99383221411677),(0.988105937622242,0.989485911589765,
0.99383221411677,0.99383221411677,0.99383221411677)))
REPRESENTATION_ITEM('')
SURFACE()
);
#1165=(
BOUNDED_SURFACE()
B_SPLINE_SURFACE(1,2,((#113312,#113313,#113314,#113315,#113316),(#113317,
#113318,#113319,#113320,#113321)),.UNSPECIFIED.,.F.,.F.,.F.)
B_SPLINE_SURFACE_WITH_KNOTS((2,2),(3,2,3),(0.,0.28980704099156),(0.314770575782761,
0.314942866188516,0.332171906764072),.UNSPECIFIED.)
GEOMETRIC_REPRESENTATION_ITEM()
RATIONAL_B_SPLINE_SURFACE(((0.987877375613931,0.987877375613931,0.987877375613931,
0.986779141655835,0.988598326347701),(0.987877375613931,0.987877375613931,
0.987877375613931,0.986779141655836,0.988598326347701)))
REPRESENTATION_ITEM('')
SURFACE()
);
#1166=(
BOUNDED_SURFACE()
B_SPLINE_SURFACE(1,2,((#113347,#113348,#113349,#113350,#113351),(#113352,
#113353,#113354,#113355,#113356)),.UNSPECIFIED.,.F.,.F.,.F.)
B_SPLINE_SURFACE_WITH_KNOTS((2,2),(3,2,3),(0.,0.289681084359917),(0.40093921985274,
0.418312080773434,0.418485809382641),.UNSPECIFIED.)
GEOMETRIC_REPRESENTATION_ITEM()
RATIONAL_B_SPLINE_SURFACE(((0.988105937622242,0.989485911589765,0.99383221411677,
0.99383221411677,0.99383221411677),(0.988105937622242,0.989485911589765,
0.99383221411677,0.99383221411677,0.99383221411677)))
REPRESENTATION_ITEM('')
SURFACE()
);
#1167=(
BOUNDED_SURFACE()
B_SPLINE_SURFACE(1,2,((#113358,#113359,#113360,#113361,#113362),(#113363,
#113364,#113365,#113366,#113367)),.UNSPECIFIED.,.F.,.F.,.F.)
B_SPLINE_SURFACE_WITH_KNOTS((2,2),(3,2,3),(0.,0.289807040991559),(0.314770575782761,
0.314942866188516,0.332171906764072),.UNSPECIFIED.)
GEOMETRIC_REPRESENTATION_ITEM()
RATIONAL_B_SPLINE_SURFACE(((0.987877375613931,0.987877375613931,0.987877375613931,
0.986779141655835,0.9885983263477),(0.987877375613931,0.987877375613931,
0.987877375613931,0.986779141655835,0.9885983263477)))
REPRESENTATION_ITEM('')
SURFACE()
);
#1168=(
BOUNDED_SURFACE()
B_SPLINE_SURFACE(1,2,((#113378,#113379,#113380,#113381,#113382),(#113383,
#113384,#113385,#113386,#113387)),.UNSPECIFIED.,.F.,.F.,.F.)
B_SPLINE_SURFACE_WITH_KNOTS((2,2),(3,2,3),(0.,0.289681084359918),(0.40093921985274,
0.418312080773435,0.418485809382642),.UNSPECIFIED.)
GEOMETRIC_REPRESENTATION_ITEM()
RATIONAL_B_SPLINE_SURFACE(((0.988105937622242,0.989485911589765,0.99383221411677,
0.99383221411677,0.99383221411677),(0.988105937622242,0.989485911589765,
0.99383221411677,0.99383221411677,0.99383221411677)))
REPRESENTATION_ITEM('')
SURFACE()
);
#1169=(
BOUNDED_SURFACE()
B_SPLINE_SURFACE(1,2,((#113404,#113405,#113406,#113407,#113408),(#113409,
#113410,#113411,#113412,#113413)),.UNSPECIFIED.,.F.,.F.,.F.)
B_SPLINE_SURFACE_WITH_KNOTS((2,2),(3,2,3),(0.,0.28980704099156),(0.314770575782761,
0.314942866188516,0.332171906764074),.UNSPECIFIED.)
GEOMETRIC_REPRESENTATION_ITEM()
RATIONAL_B_SPLINE_SURFACE(((0.987877375613931,0.987877375613931,0.987877375613931,
0.986779141655835,0.988598326347701),(0.987877375613931,0.987877375613931,
0.987877375613931,0.986779141655835,0.988598326347701)))
REPRESENTATION_ITEM('')
SURFACE()
);
#1170=(
BOUNDED_SURFACE()
B_SPLINE_SURFACE(1,2,((#113439,#113440,#113441,#113442,#113443),(#113444,
#113445,#113446,#113447,#113448)),.UNSPECIFIED.,.F.,.F.,.F.)
B_SPLINE_SURFACE_WITH_KNOTS((2,2),(3,2,3),(0.,0.289681084359927),(0.400939219852743,
0.418312080773433,0.41848580938264),.UNSPECIFIED.)
GEOMETRIC_REPRESENTATION_ITEM()
RATIONAL_B_SPLINE_SURFACE(((0.988105937622242,0.989485911589766,0.99383221411677,
0.99383221411677,0.99383221411677),(0.988105937622242,0.989485911589766,
0.99383221411677,0.99383221411677,0.99383221411677)))
REPRESENTATION_ITEM('')
SURFACE()
);
#1171=(
BOUNDED_SURFACE()
B_SPLINE_SURFACE(1,2,((#113450,#113451,#113452,#113453,#113454),(#113455,
#113456,#113457,#113458,#113459)),.UNSPECIFIED.,.F.,.F.,.F.)
B_SPLINE_SURFACE_WITH_KNOTS((2,2),(3,2,3),(0.,0.289807040991823),(0.314770575782762,
0.314942866188517,0.332171906764075),.UNSPECIFIED.)
GEOMETRIC_REPRESENTATION_ITEM()
RATIONAL_B_SPLINE_SURFACE(((0.987877375613931,0.987877375613931,0.987877375613931,
0.986779141655835,0.988598326347701),(0.987877375613931,0.987877375613931,
0.987877375613931,0.986779141655835,0.988598326347701)))
REPRESENTATION_ITEM('')
SURFACE()
);
#1172=(
BOUNDED_SURFACE()
B_SPLINE_SURFACE(1,2,((#113485,#113486,#113487,#113488,#113489),(#113490,
#113491,#113492,#113493,#113494)),.UNSPECIFIED.,.F.,.F.,.F.)
B_SPLINE_SURFACE_WITH_KNOTS((2,2),(3,2,3),(0.,0.289681084359918),(0.400939219852739,
0.418312080773433,0.41848580938264),.UNSPECIFIED.)
GEOMETRIC_REPRESENTATION_ITEM()
RATIONAL_B_SPLINE_SURFACE(((0.988105937622241,0.989485911589765,0.99383221411677,
0.99383221411677,0.99383221411677),(0.988105937622241,0.989485911589765,
0.99383221411677,0.99383221411677,0.99383221411677)))
REPRESENTATION_ITEM('')
SURFACE()
);
#1173=(
BOUNDED_SURFACE()
B_SPLINE_SURFACE(1,2,((#113496,#113497,#113498,#113499,#113500),(#113501,
#113502,#113503,#113504,#113505)),.UNSPECIFIED.,.F.,.F.,.F.)
B_SPLINE_SURFACE_WITH_KNOTS((2,2),(3,2,3),(0.,0.289807040991884),(0.314770575782762,
0.314942866188517,0.332171906764075),.UNSPECIFIED.)
GEOMETRIC_REPRESENTATION_ITEM()
RATIONAL_B_SPLINE_SURFACE(((0.987877375613931,0.987877375613931,0.987877375613931,
0.986779141655835,0.988598326347701),(0.987877375613931,0.987877375613931,
0.987877375613931,0.986779141655835,0.988598326347701)))
REPRESENTATION_ITEM('')
SURFACE()
);
#1174=(
BOUNDED_SURFACE()
B_SPLINE_SURFACE(1,2,((#113531,#113532,#113533,#113534,#113535),(#113536,
#113537,#113538,#113539,#113540)),.UNSPECIFIED.,.F.,.F.,.F.)
B_SPLINE_SURFACE_WITH_KNOTS((2,2),(3,2,3),(0.,0.289681084359927),(0.400939219852741,
0.418312080773433,0.41848580938264),.UNSPECIFIED.)
GEOMETRIC_REPRESENTATION_ITEM()
RATIONAL_B_SPLINE_SURFACE(((0.988105937622242,0.989485911589765,0.99383221411677,
0.99383221411677,0.99383221411677),(0.988105937622242,0.989485911589765,
0.99383221411677,0.99383221411677,0.99383221411677)))
REPRESENTATION_ITEM('')
SURFACE()
);
#1175=(
BOUNDED_SURFACE()
B_SPLINE_SURFACE(1,2,((#113542,#113543,#113544,#113545,#113546),(#113547,
#113548,#113549,#113550,#113551)),.UNSPECIFIED.,.F.,.F.,.F.)
B_SPLINE_SURFACE_WITH_KNOTS((2,2),(3,2,3),(0.,0.289807040991838),(0.314770575782762,
0.314942866188517,0.332171906764074),.UNSPECIFIED.)
GEOMETRIC_REPRESENTATION_ITEM()
RATIONAL_B_SPLINE_SURFACE(((0.987877375613931,0.987877375613931,0.987877375613931,
0.986779141655835,0.988598326347701),(0.987877375613931,0.987877375613931,
0.987877375613931,0.986779141655835,0.988598326347701)))
REPRESENTATION_ITEM('')
SURFACE()
);
#1176=(
BOUNDED_SURFACE()
B_SPLINE_SURFACE(1,2,((#113577,#113578,#113579,#113580,#113581),(#113582,
#113583,#113584,#113585,#113586)),.UNSPECIFIED.,.F.,.F.,.F.)
B_SPLINE_SURFACE_WITH_KNOTS((2,2),(3,2,3),(0.,0.289681084359916),(0.400939219852742,
0.418312080773434,0.418485809382641),.UNSPECIFIED.)
GEOMETRIC_REPRESENTATION_ITEM()
RATIONAL_B_SPLINE_SURFACE(((0.988105937622242,0.989485911589766,0.99383221411677,
0.99383221411677,0.99383221411677),(0.988105937622242,0.989485911589766,
0.99383221411677,0.99383221411677,0.99383221411677)))
REPRESENTATION_ITEM('')
SURFACE()
);
#1177=(
BOUNDED_SURFACE()
B_SPLINE_SURFACE(1,2,((#113588,#113589,#113590,#113591,#113592),(#113593,
#113594,#113595,#113596,#113597)),.UNSPECIFIED.,.F.,.F.,.F.)
B_SPLINE_SURFACE_WITH_KNOTS((2,2),(3,2,3),(0.,0.289807040992021),(0.314770575782761,
0.314942866188516,0.332171906764074),.UNSPECIFIED.)
GEOMETRIC_REPRESENTATION_ITEM()
RATIONAL_B_SPLINE_SURFACE(((0.987877375613931,0.987877375613931,0.987877375613931,
0.986779141655835,0.988598326347701),(0.987877375613931,0.987877375613931,
0.987877375613931,0.986779141655835,0.988598326347701)))
REPRESENTATION_ITEM('')
SURFACE()
);
#1178=(
BOUNDED_SURFACE()
B_SPLINE_SURFACE(1,2,((#113623,#113624,#113625,#113626,#113627),(#113628,
#113629,#113630,#113631,#113632)),.UNSPECIFIED.,.F.,.F.,.F.)
B_SPLINE_SURFACE_WITH_KNOTS((2,2),(3,2,3),(0.,0.289681084359935),(0.400939219852743,
0.418312080773434,0.418485809382641),.UNSPECIFIED.)
GEOMETRIC_REPRESENTATION_ITEM()
RATIONAL_B_SPLINE_SURFACE(((0.988105937622242,0.989485911589766,0.99383221411677,
0.99383221411677,0.99383221411677),(0.988105937622242,0.989485911589766,
0.99383221411677,0.99383221411677,0.99383221411677)))
REPRESENTATION_ITEM('')
SURFACE()
);
#1179=(
BOUNDED_SURFACE()
B_SPLINE_SURFACE(1,2,((#113649,#113650,#113651,#113652,#113653),(#113654,
#113655,#113656,#113657,#113658)),.UNSPECIFIED.,.F.,.F.,.F.)
B_SPLINE_SURFACE_WITH_KNOTS((2,2),(3,2,3),(0.,0.289807040991979),(0.314770575782761,
0.314942866188516,0.332171906764074),.UNSPECIFIED.)
GEOMETRIC_REPRESENTATION_ITEM()
RATIONAL_B_SPLINE_SURFACE(((0.987877375613931,0.987877375613931,0.987877375613931,
0.986779141655835,0.988598326347701),(0.987877375613931,0.987877375613931,
0.987877375613931,0.986779141655835,0.988598326347701)))
REPRESENTATION_ITEM('')
SURFACE()
);
#1180=(
BOUNDED_SURFACE()
B_SPLINE_SURFACE(1,2,((#113660,#113661,#113662,#113663,#113664),(#113665,
#113666,#113667,#113668,#113669)),.UNSPECIFIED.,.F.,.F.,.F.)
B_SPLINE_SURFACE_WITH_KNOTS((2,2),(3,2,3),(0.710192959007329,1.),(0.262924618389842,
0.263098999273797,0.280537087669266),.UNSPECIFIED.)
GEOMETRIC_REPRESENTATION_ITEM()
RATIONAL_B_SPLINE_SURFACE(((0.989150325841653,0.989150325841653,0.989150325841653,
0.991395311444462,0.996628941948308),(0.989150325841653,0.989150325841653,
0.989150325841653,0.991395311444462,0.996628941948308)))
REPRESENTATION_ITEM('')
SURFACE()
);
#1181=(
BOUNDED_SURFACE()
B_SPLINE_SURFACE(1,2,((#113680,#113681,#113682),(#113683,#113684,#113685)),
 .UNSPECIFIED.,.F.,.F.,.F.)
B_SPLINE_SURFACE_WITH_KNOTS((2,2),(3,3),(0.710318915640079,1.),(0.452822299828563,
0.470019760166384),.UNSPECIFIED.)
GEOMETRIC_REPRESENTATION_ITEM()
RATIONAL_B_SPLINE_SURFACE(((0.988755486262821,0.986817927519784,0.987787102172816),
(0.988755486262821,0.986817927519784,0.987787102172816)))
REPRESENTATION_ITEM('')
SURFACE()
);
#1182=(
BOUNDED_SURFACE()
B_SPLINE_SURFACE(1,2,((#113696,#113697,#113698,#113699,#113700),(#113701,
#113702,#113703,#113704,#113705)),.UNSPECIFIED.,.F.,.F.,.F.)
B_SPLINE_SURFACE_WITH_KNOTS((2,2),(3,2,3),(0.710192959008441,1.),(0.262924618389842,
0.263098999273797,0.280537087669267),.UNSPECIFIED.)
GEOMETRIC_REPRESENTATION_ITEM()
RATIONAL_B_SPLINE_SURFACE(((0.989150325841653,0.989150325841653,0.989150325841653,
0.991395311444462,0.996628941948308),(0.989150325841653,0.989150325841653,
0.989150325841653,0.991395311444462,0.996628941948308)))
REPRESENTATION_ITEM('')
SURFACE()
);
#1183=(
BOUNDED_SURFACE()
B_SPLINE_SURFACE(1,2,((#113713,#113714,#113715),(#113716,#113717,#113718)),
 .UNSPECIFIED.,.F.,.F.,.F.)
B_SPLINE_SURFACE_WITH_KNOTS((2,2),(3,3),(0.710318915640082,1.),(0.452822299828565,
0.470019760166366),.UNSPECIFIED.)
GEOMETRIC_REPRESENTATION_ITEM()
RATIONAL_B_SPLINE_SURFACE(((0.988755486262821,0.986817927519786,0.987787102172814),
(0.988755486262821,0.986817927519786,0.987787102172814)))
REPRESENTATION_ITEM('')
SURFACE()
);
#1184=(
BOUNDED_SURFACE()
B_SPLINE_SURFACE(1,2,((#113729,#113730,#113731,#113732,#113733),(#113734,
#113735,#113736,#113737,#113738)),.UNSPECIFIED.,.F.,.F.,.F.)
B_SPLINE_SURFACE_WITH_KNOTS((2,2),(3,2,3),(0.710192959008439,1.),(0.262924618389842,
0.263098999273797,0.280537087669267),.UNSPECIFIED.)
GEOMETRIC_REPRESENTATION_ITEM()
RATIONAL_B_SPLINE_SURFACE(((0.989150325841653,0.989150325841653,0.989150325841653,
0.991395311444462,0.996628941948308),(0.989150325841653,0.989150325841653,
0.989150325841653,0.991395311444462,0.996628941948308)))
REPRESENTATION_ITEM('')
SURFACE()
);
#1185=(
BOUNDED_SURFACE()
B_SPLINE_SURFACE(1,2,((#113746,#113747,#113748),(#113749,#113750,#113751)),
 .UNSPECIFIED.,.F.,.F.,.F.)
B_SPLINE_SURFACE_WITH_KNOTS((2,2),(3,3),(0.710318915639499,1.),(0.452822299828566,
0.470019760166366),.UNSPECIFIED.)
GEOMETRIC_REPRESENTATION_ITEM()
RATIONAL_B_SPLINE_SURFACE(((0.98875548626282,0.986817927519786,0.987787102172814),
(0.98875548626282,0.986817927519786,0.987787102172814)))
REPRESENTATION_ITEM('')
SURFACE()
);
#1186=(
BOUNDED_SURFACE()
B_SPLINE_SURFACE(1,2,((#113762,#113763,#113764,#113765,#113766),(#113767,
#113768,#113769,#113770,#113771)),.UNSPECIFIED.,.F.,.F.,.F.)
B_SPLINE_SURFACE_WITH_KNOTS((2,2),(3,2,3),(0.709593130080989,1.),(0.26249917015916,
0.263098999273797,0.280537087669267),.UNSPECIFIED.)
GEOMETRIC_REPRESENTATION_ITEM()
RATIONAL_B_SPLINE_SURFACE(((0.989150325841653,0.989150325841653,0.989150325841653,
0.991395311444462,0.996628941948308),(0.989150325841653,0.989150325841653,
0.989150325841653,0.991395311444462,0.996628941948308)))
REPRESENTATION_ITEM('')
SURFACE()
);
#1187=(
BOUNDED_SURFACE()
B_SPLINE_SURFACE(1,2,((#113779,#113780,#113781),(#113782,#113783,#113784)),
 .UNSPECIFIED.,.F.,.F.,.F.)
B_SPLINE_SURFACE_WITH_KNOTS((2,2),(3,3),(0.710318915640079,1.),(0.452822299828565,
0.470019760166366),.UNSPECIFIED.)
GEOMETRIC_REPRESENTATION_ITEM()
RATIONAL_B_SPLINE_SURFACE(((0.98875548626282,0.986817927519786,0.987787102172814),
(0.988755486262821,0.986817927519786,0.987787102172814)))
REPRESENTATION_ITEM('')
SURFACE()
);
#1188=(
BOUNDED_SURFACE()
B_SPLINE_SURFACE(1,2,((#113795,#113796,#113797,#113798,#113799),(#113800,
#113801,#113802,#113803,#113804)),.UNSPECIFIED.,.F.,.F.,.F.)
B_SPLINE_SURFACE_WITH_KNOTS((2,2),(3,2,3),(0.709593130109806,1.),(0.262499170175398,
0.263098999273797,0.280537087669267),.UNSPECIFIED.)
GEOMETRIC_REPRESENTATION_ITEM()
RATIONAL_B_SPLINE_SURFACE(((0.989150325841653,0.989150325841653,0.989150325841653,
0.991395311444462,0.996628941948309),(0.989150325841653,0.989150325841653,
0.989150325841653,0.991395311444462,0.996628941948308)))
REPRESENTATION_ITEM('')
SURFACE()
);
#1189=(
BOUNDED_SURFACE()
B_SPLINE_SURFACE(1,2,((#113812,#113813,#113814),(#113815,#113816,#113817)),
 .UNSPECIFIED.,.F.,.F.,.F.)
B_SPLINE_SURFACE_WITH_KNOTS((2,2),(3,3),(0.710318915639495,1.),(0.452822299828565,
0.470019760166366),.UNSPECIFIED.)
GEOMETRIC_REPRESENTATION_ITEM()
RATIONAL_B_SPLINE_SURFACE(((0.98875548626282,0.986817927519786,0.987787102172814),
(0.988755486262821,0.986817927519786,0.987787102172814)))
REPRESENTATION_ITEM('')
SURFACE()
);
#1190=(
BOUNDED_SURFACE()
B_SPLINE_SURFACE(1,2,((#113828,#113829,#113830,#113831,#113832),(#113833,
#113834,#113835,#113836,#113837)),.UNSPECIFIED.,.F.,.F.,.F.)
B_SPLINE_SURFACE_WITH_KNOTS((2,2),(3,2,3),(0.709593130090909,1.),(0.262499170157079,
0.263098999273797,0.280537087669267),.UNSPECIFIED.)
GEOMETRIC_REPRESENTATION_ITEM()
RATIONAL_B_SPLINE_SURFACE(((0.989150325841653,0.989150325841653,0.989150325841653,
0.991395311444462,0.996628941948308),(0.989150325841653,0.989150325841653,
0.989150325841653,0.991395311444462,0.996628941948308)))
REPRESENTATION_ITEM('')
SURFACE()
);
#1191=(
BOUNDED_SURFACE()
B_SPLINE_SURFACE(1,2,((#113845,#113846,#113847),(#113848,#113849,#113850)),
 .UNSPECIFIED.,.F.,.F.,.F.)
B_SPLINE_SURFACE_WITH_KNOTS((2,2),(3,3),(0.710318915639997,1.),(0.452822299828567,
0.470019760166366),.UNSPECIFIED.)
GEOMETRIC_REPRESENTATION_ITEM()
RATIONAL_B_SPLINE_SURFACE(((0.98875548626282,0.986817927519786,0.987787102172814),
(0.98875548626282,0.986817927519786,0.987787102172814)))
REPRESENTATION_ITEM('')
SURFACE()
);
#1192=(
BOUNDED_SURFACE()
B_SPLINE_SURFACE(1,2,((#113861,#113862,#113863,#113864,#113865),(#113866,
#113867,#113868,#113869,#113870)),.UNSPECIFIED.,.F.,.F.,.F.)
B_SPLINE_SURFACE_WITH_KNOTS((2,2),(3,2,3),(0.709593130119578,1.),(0.262499170185248,
0.263098999273796,0.280537087669266),.UNSPECIFIED.)
GEOMETRIC_REPRESENTATION_ITEM()
RATIONAL_B_SPLINE_SURFACE(((0.989150325841653,0.989150325841653,0.989150325841653,
0.991395311444461,0.996628941948308),(0.989150325841653,0.989150325841653,
0.989150325841653,0.991395311444461,0.996628941948308)))
REPRESENTATION_ITEM('')
SURFACE()
);
#1193=(
BOUNDED_SURFACE()
B_SPLINE_SURFACE(1,2,((#113878,#113879,#113880),(#113881,#113882,#113883)),
 .UNSPECIFIED.,.F.,.F.,.F.)
B_SPLINE_SURFACE_WITH_KNOTS((2,2),(3,3),(0.710318915640003,1.),(0.452822299828567,
0.470019760166367),.UNSPECIFIED.)
GEOMETRIC_REPRESENTATION_ITEM()
RATIONAL_B_SPLINE_SURFACE(((0.98875548626282,0.986817927519786,0.987787102172814),
(0.98875548626282,0.986817927519786,0.987787102172814)))
REPRESENTATION_ITEM('')
SURFACE()
);
#1194=(
BOUNDED_SURFACE()
B_SPLINE_SURFACE(1,2,((#113894,#113895,#113896,#113897,#113898),(#113899,
#113900,#113901,#113902,#113903)),.UNSPECIFIED.,.F.,.F.,.F.)
B_SPLINE_SURFACE_WITH_KNOTS((2,2),(3,2,3),(0.710192959008368,1.),(0.262924618389841,
0.263098999273796,0.280537087669266),.UNSPECIFIED.)
GEOMETRIC_REPRESENTATION_ITEM()
RATIONAL_B_SPLINE_SURFACE(((0.989150325841653,0.989150325841653,0.989150325841653,
0.991395311444461,0.996628941948308),(0.989150325841653,0.989150325841653,
0.989150325841653,0.991395311444461,0.996628941948308)))
REPRESENTATION_ITEM('')
SURFACE()
);
#1195=(
BOUNDED_SURFACE()
B_SPLINE_SURFACE(1,2,((#113911,#113912,#113913),(#113914,#113915,#113916)),
 .UNSPECIFIED.,.F.,.F.,.F.)
B_SPLINE_SURFACE_WITH_KNOTS((2,2),(3,3),(0.710318915639408,1.),(0.452822299828567,
0.470019760166367),.UNSPECIFIED.)
GEOMETRIC_REPRESENTATION_ITEM()
RATIONAL_B_SPLINE_SURFACE(((0.98875548626282,0.986817927519786,0.987787102172814),
(0.98875548626282,0.986817927519786,0.987787102172814)))
REPRESENTATION_ITEM('')
SURFACE()
);
#1196=(
BOUNDED_SURFACE()
B_SPLINE_SURFACE(1,2,((#113927,#113928,#113929,#113930,#113931),(#113932,
#113933,#113934,#113935,#113936)),.UNSPECIFIED.,.F.,.F.,.F.)
B_SPLINE_SURFACE_WITH_KNOTS((2,2),(3,2,3),(0.710192959007765,1.),(0.262924618389841,
0.263098999273796,0.280537087669266),.UNSPECIFIED.)
GEOMETRIC_REPRESENTATION_ITEM()
RATIONAL_B_SPLINE_SURFACE(((0.989150325841653,0.989150325841653,0.989150325841653,
0.991395311444461,0.996628941948308),(0.989150325841653,0.989150325841653,
0.989150325841653,0.991395311444461,0.996628941948308)))
REPRESENTATION_ITEM('')
SURFACE()
);
#1197=(
BOUNDED_SURFACE()
B_SPLINE_SURFACE(1,2,((#113944,#113945,#113946),(#113947,#113948,#113949)),
 .UNSPECIFIED.,.F.,.F.,.F.)
B_SPLINE_SURFACE_WITH_KNOTS((2,2),(3,3),(0.710318915639996,1.),(0.452822299828567,
0.470019760166367),.UNSPECIFIED.)
GEOMETRIC_REPRESENTATION_ITEM()
RATIONAL_B_SPLINE_SURFACE(((0.98875548626282,0.986817927519786,0.987787102172814),
(0.98875548626282,0.986817927519786,0.987787102172814)))
REPRESENTATION_ITEM('')
SURFACE()
);
#1198=(
BOUNDED_SURFACE()
B_SPLINE_SURFACE(1,2,((#113960,#113961,#113962,#113963,#113964),(#113965,
#113966,#113967,#113968,#113969)),.UNSPECIFIED.,.F.,.F.,.F.)
B_SPLINE_SURFACE_WITH_KNOTS((2,2),(3,2,3),(0.710192959008356,1.),(0.262924618389841,
0.263098999273796,0.280537087669266),.UNSPECIFIED.)
GEOMETRIC_REPRESENTATION_ITEM()
RATIONAL_B_SPLINE_SURFACE(((0.989150325841653,0.989150325841653,0.989150325841653,
0.991395311444461,0.996628941948308),(0.989150325841653,0.989150325841653,
0.989150325841653,0.991395311444461,0.996628941948308)))
REPRESENTATION_ITEM('')
SURFACE()
);
#1199=(
BOUNDED_SURFACE()
B_SPLINE_SURFACE(1,2,((#113977,#113978,#113979),(#113980,#113981,#113982)),
 .UNSPECIFIED.,.F.,.F.,.F.)
B_SPLINE_SURFACE_WITH_KNOTS((2,2),(3,3),(0.710318915639494,1.),(0.452822299828567,
0.470019760166367),.UNSPECIFIED.)
GEOMETRIC_REPRESENTATION_ITEM()
RATIONAL_B_SPLINE_SURFACE(((0.98875548626282,0.986817927519786,0.987787102172814),
(0.98875548626282,0.986817927519786,0.987787102172814)))
REPRESENTATION_ITEM('')
SURFACE()
);
#1200=(
BOUNDED_SURFACE()
B_SPLINE_SURFACE(1,2,((#113993,#113994,#113995,#113996,#113997),(#113998,
#113999,#114000,#114001,#114002)),.UNSPECIFIED.,.F.,.F.,.F.)
B_SPLINE_SURFACE_WITH_KNOTS((2,2),(3,2,3),(0.710192959007858,1.),(0.262924618389841,
0.263098999273796,0.280537087669266),.UNSPECIFIED.)
GEOMETRIC_REPRESENTATION_ITEM()
RATIONAL_B_SPLINE_SURFACE(((0.989150325841653,0.989150325841653,0.989150325841653,
0.991395311444461,0.996628941948308),(0.989150325841653,0.989150325841653,
0.989150325841653,0.991395311444461,0.996628941948308)))
REPRESENTATION_ITEM('')
SURFACE()
);
#1201=(
BOUNDED_SURFACE()
B_SPLINE_SURFACE(1,2,((#114010,#114011,#114012),(#114013,#114014,#114015)),
 .UNSPECIFIED.,.F.,.F.,.F.)
B_SPLINE_SURFACE_WITH_KNOTS((2,2),(3,3),(0.710318915639993,1.),(0.452822299828567,
0.470019760166367),.UNSPECIFIED.)
GEOMETRIC_REPRESENTATION_ITEM()
RATIONAL_B_SPLINE_SURFACE(((0.98875548626282,0.986817927519786,0.987787102172814),
(0.98875548626282,0.986817927519786,0.987787102172814)))
REPRESENTATION_ITEM('')
SURFACE()
);
#1202=(
BOUNDED_SURFACE()
B_SPLINE_SURFACE(1,2,((#114026,#114027,#114028,#114029,#114030),(#114031,
#114032,#114033,#114034,#114035)),.UNSPECIFIED.,.F.,.F.,.F.)
B_SPLINE_SURFACE_WITH_KNOTS((2,2),(3,2,3),(0.709593130089926,1.),(0.262499170167511,
0.263098999273796,0.280537087669266),.UNSPECIFIED.)
GEOMETRIC_REPRESENTATION_ITEM()
RATIONAL_B_SPLINE_SURFACE(((0.989150325841653,0.989150325841653,0.989150325841653,
0.991395311444461,0.996628941948308),(0.989150325841653,0.989150325841653,
0.989150325841653,0.991395311444461,0.996628941948308)))
REPRESENTATION_ITEM('')
SURFACE()
);
#1203=(
BOUNDED_SURFACE()
B_SPLINE_SURFACE(1,2,((#114043,#114044,#114045),(#114046,#114047,#114048)),
 .UNSPECIFIED.,.F.,.F.,.F.)
B_SPLINE_SURFACE_WITH_KNOTS((2,2),(3,3),(0.710318915639495,1.),(0.452822299828567,
0.470019760166367),.UNSPECIFIED.)
GEOMETRIC_REPRESENTATION_ITEM()
RATIONAL_B_SPLINE_SURFACE(((0.98875548626282,0.986817927519786,0.987787102172814),
(0.98875548626282,0.986817927519786,0.987787102172814)))
REPRESENTATION_ITEM('')
SURFACE()
);
#1204=(
BOUNDED_SURFACE()
B_SPLINE_SURFACE(1,2,((#114059,#114060,#114061,#114062,#114063),(#114064,
#114065,#114066,#114067,#114068)),.UNSPECIFIED.,.F.,.F.,.F.)
B_SPLINE_SURFACE_WITH_KNOTS((2,2),(3,2,3),(0.709593130096317,1.),(0.262499170174355,
0.263098999273796,0.280537087669266),.UNSPECIFIED.)
GEOMETRIC_REPRESENTATION_ITEM()
RATIONAL_B_SPLINE_SURFACE(((0.989150325841653,0.989150325841653,0.989150325841653,
0.991395311444461,0.996628941948308),(0.989150325841653,0.989150325841653,
0.989150325841653,0.991395311444461,0.996628941948308)))
REPRESENTATION_ITEM('')
SURFACE()
);
#1205=(
BOUNDED_SURFACE()
B_SPLINE_SURFACE(1,2,((#114076,#114077,#114078),(#114079,#114080,#114081)),
 .UNSPECIFIED.,.F.,.F.,.F.)
B_SPLINE_SURFACE_WITH_KNOTS((2,2),(3,3),(0.710318915639721,1.),(0.452822299828567,
0.470019760166367),.UNSPECIFIED.)
GEOMETRIC_REPRESENTATION_ITEM()
RATIONAL_B_SPLINE_SURFACE(((0.98875548626282,0.986817927519786,0.987787102172814),
(0.98875548626282,0.986817927519786,0.987787102172814)))
REPRESENTATION_ITEM('')
SURFACE()
);
#1206=(
BOUNDED_SURFACE()
B_SPLINE_SURFACE(1,2,((#114092,#114093,#114094,#114095,#114096),(#114097,
#114098,#114099,#114100,#114101)),.UNSPECIFIED.,.F.,.F.,.F.)
B_SPLINE_SURFACE_WITH_KNOTS((2,2),(3,2,3),(0.709593130099464,1.),(0.262499170165416,
0.263098999273796,0.280537087669266),.UNSPECIFIED.)
GEOMETRIC_REPRESENTATION_ITEM()
RATIONAL_B_SPLINE_SURFACE(((0.989150325841653,0.989150325841653,0.989150325841653,
0.991395311444461,0.996628941948308),(0.989150325841653,0.989150325841653,
0.989150325841653,0.991395311444461,0.996628941948308)))
REPRESENTATION_ITEM('')
SURFACE()
);
#1207=(
BOUNDED_SURFACE()
B_SPLINE_SURFACE(1,2,((#114109,#114110,#114111),(#114112,#114113,#114114)),
 .UNSPECIFIED.,.F.,.F.,.F.)
B_SPLINE_SURFACE_WITH_KNOTS((2,2),(3,3),(0.710318915638678,1.),(0.452822299828567,
0.470019760166367),.UNSPECIFIED.)
GEOMETRIC_REPRESENTATION_ITEM()
RATIONAL_B_SPLINE_SURFACE(((0.98875548626282,0.986817927519786,0.987787102172814),
(0.98875548626282,0.986817927519786,0.987787102172814)))
REPRESENTATION_ITEM('')
SURFACE()
);
#1208=(
BOUNDED_SURFACE()
B_SPLINE_SURFACE(1,2,((#114122,#114123,#114124,#114125,#114126),(#114127,
#114128,#114129,#114130,#114131)),.UNSPECIFIED.,.F.,.F.,.F.)
B_SPLINE_SURFACE_WITH_KNOTS((2,2),(3,2,3),(0.71019295900703,1.),(0.262924618389841,
0.263098999273796,0.280537087669266),.UNSPECIFIED.)
GEOMETRIC_REPRESENTATION_ITEM()
RATIONAL_B_SPLINE_SURFACE(((0.989150325841653,0.989150325841653,0.989150325841653,
0.991395311444461,0.996628941948308),(0.989150325841653,0.989150325841653,
0.989150325841653,0.991395311444461,0.996628941948308)))
REPRESENTATION_ITEM('')
SURFACE()
);
#1209=(
BOUNDED_SURFACE()
B_SPLINE_SURFACE(1,2,((#114133,#114134,#114135),(#114136,#114137,#114138)),
 .UNSPECIFIED.,.F.,.F.,.F.)
B_SPLINE_SURFACE_WITH_KNOTS((2,2),(3,3),(0.710318915639959,1.),(0.452822299828567,
0.470019760166367),.UNSPECIFIED.)
GEOMETRIC_REPRESENTATION_ITEM()
RATIONAL_B_SPLINE_SURFACE(((0.98875548626282,0.986817927519786,0.987787102172814),
(0.98875548626282,0.986817927519786,0.987787102172814)))
REPRESENTATION_ITEM('')
SURFACE()
);
#1210=(
BOUNDED_SURFACE()
B_SPLINE_SURFACE(1,2,((#114149,#114150,#114151,#114152,#114153),(#114154,
#114155,#114156,#114157,#114158)),.UNSPECIFIED.,.F.,.F.,.F.)
B_SPLINE_SURFACE_WITH_KNOTS((2,2),(3,2,3),(0.710192959008315,1.),(0.262924618389841,
0.263098999273796,0.280537087669266),.UNSPECIFIED.)
GEOMETRIC_REPRESENTATION_ITEM()
RATIONAL_B_SPLINE_SURFACE(((0.989150325841653,0.989150325841653,0.989150325841653,
0.991395311444461,0.996628941948308),(0.989150325841653,0.989150325841653,
0.989150325841653,0.991395311444461,0.996628941948308)))
REPRESENTATION_ITEM('')
SURFACE()
);
#1211=(
BOUNDED_SURFACE()
B_SPLINE_SURFACE(1,2,((#114166,#114167,#114168),(#114169,#114170,#114171)),
 .UNSPECIFIED.,.F.,.F.,.F.)
B_SPLINE_SURFACE_WITH_KNOTS((2,2),(3,3),(0.710318915640075,1.),(0.452822299828567,
0.470019760166367),.UNSPECIFIED.)
GEOMETRIC_REPRESENTATION_ITEM()
RATIONAL_B_SPLINE_SURFACE(((0.98875548626282,0.986817927519786,0.987787102172814),
(0.98875548626282,0.986817927519786,0.987787102172814)))
REPRESENTATION_ITEM('')
SURFACE()
);
#1212=(
BOUNDED_SURFACE()
B_SPLINE_SURFACE(1,2,((#114182,#114183,#114184,#114185,#114186),(#114187,
#114188,#114189,#114190,#114191)),.UNSPECIFIED.,.F.,.F.,.F.)
B_SPLINE_SURFACE_WITH_KNOTS((2,2),(3,2,3),(0.710192959008434,1.),(0.262924618389841,
0.263098999273796,0.280537087669266),.UNSPECIFIED.)
GEOMETRIC_REPRESENTATION_ITEM()
RATIONAL_B_SPLINE_SURFACE(((0.989150325841653,0.989150325841653,0.989150325841653,
0.991395311444461,0.996628941948308),(0.989150325841653,0.989150325841653,
0.989150325841653,0.991395311444461,0.996628941948308)))
REPRESENTATION_ITEM('')
SURFACE()
);
#1213=(
BOUNDED_SURFACE()
B_SPLINE_SURFACE(1,2,((#114199,#114200,#114201),(#114202,#114203,#114204)),
 .UNSPECIFIED.,.F.,.F.,.F.)
B_SPLINE_SURFACE_WITH_KNOTS((2,2),(3,3),(0.710318915639447,1.),(0.452822299828566,
0.470019760166367),.UNSPECIFIED.)
GEOMETRIC_REPRESENTATION_ITEM()
RATIONAL_B_SPLINE_SURFACE(((0.98875548626282,0.986817927519786,0.987787102172814),
(0.98875548626282,0.986817927519786,0.987787102172814)))
REPRESENTATION_ITEM('')
SURFACE()
);
#1214=(
BOUNDED_SURFACE()
B_SPLINE_SURFACE(1,2,((#114215,#114216,#114217,#114218,#114219),(#114220,
#114221,#114222,#114223,#114224)),.UNSPECIFIED.,.F.,.F.,.F.)
B_SPLINE_SURFACE_WITH_KNOTS((2,2),(3,2,3),(0.710192959007799,1.),(0.262924618389841,
0.263098999273796,0.280537087669266),.UNSPECIFIED.)
GEOMETRIC_REPRESENTATION_ITEM()
RATIONAL_B_SPLINE_SURFACE(((0.989150325841653,0.989150325841653,0.989150325841653,
0.991395311444461,0.996628941948308),(0.989150325841653,0.989150325841653,
0.989150325841653,0.991395311444461,0.996628941948308)))
REPRESENTATION_ITEM('')
SURFACE()
);
#1215=(
BOUNDED_SURFACE()
B_SPLINE_SURFACE(1,2,((#114232,#114233,#114234),(#114235,#114236,#114237)),
 .UNSPECIFIED.,.F.,.F.,.F.)
B_SPLINE_SURFACE_WITH_KNOTS((2,2),(3,3),(0.71031891564008,1.),(0.452822299828566,
0.470019760166367),.UNSPECIFIED.)
GEOMETRIC_REPRESENTATION_ITEM()
RATIONAL_B_SPLINE_SURFACE(((0.98875548626282,0.986817927519786,0.987787102172814),
(0.98875548626282,0.986817927519786,0.987787102172814)))
REPRESENTATION_ITEM('')
SURFACE()
);
#1216=(
BOUNDED_SURFACE()
B_SPLINE_SURFACE(1,2,((#114248,#114249,#114250,#114251,#114252),(#114253,
#114254,#114255,#114256,#114257)),.UNSPECIFIED.,.F.,.F.,.F.)
B_SPLINE_SURFACE_WITH_KNOTS((2,2),(3,2,3),(0.709593130092405,1.),(0.262499170169975,
0.263098999273796,0.280537087669266),.UNSPECIFIED.)
GEOMETRIC_REPRESENTATION_ITEM()
RATIONAL_B_SPLINE_SURFACE(((0.989150325841653,0.989150325841653,0.989150325841653,
0.991395311444461,0.996628941948308),(0.989150325841653,0.989150325841653,
0.989150325841653,0.991395311444461,0.996628941948308)))
REPRESENTATION_ITEM('')
SURFACE()
);
#1217=(
BOUNDED_SURFACE()
B_SPLINE_SURFACE(1,2,((#114265,#114266,#114267),(#114268,#114269,#114270)),
 .UNSPECIFIED.,.F.,.F.,.F.)
B_SPLINE_SURFACE_WITH_KNOTS((2,2),(3,3),(0.710318915638944,1.),(0.452822299828567,
0.470019760166367),.UNSPECIFIED.)
GEOMETRIC_REPRESENTATION_ITEM()
RATIONAL_B_SPLINE_SURFACE(((0.98875548626282,0.986817927519786,0.987787102172814),
(0.98875548626282,0.986817927519786,0.987787102172814)))
REPRESENTATION_ITEM('')
SURFACE()
);
#1218=(
BOUNDED_SURFACE()
B_SPLINE_SURFACE(1,2,((#114281,#114282,#114283,#114284,#114285),(#114286,
#114287,#114288,#114289,#114290)),.UNSPECIFIED.,.F.,.F.,.F.)
B_SPLINE_SURFACE_WITH_KNOTS((2,2),(3,2,3),(0.70959313010765,1.),(0.262499170174373,
0.263098999273796,0.280537087669266),.UNSPECIFIED.)
GEOMETRIC_REPRESENTATION_ITEM()
RATIONAL_B_SPLINE_SURFACE(((0.989150325841653,0.989150325841653,0.989150325841653,
0.991395311444461,0.996628941948308),(0.989150325841653,0.989150325841653,
0.989150325841653,0.991395311444461,0.996628941948308)))
REPRESENTATION_ITEM('')
SURFACE()
);
#1219=(
BOUNDED_SURFACE()
B_SPLINE_SURFACE(1,2,((#114298,#114299,#114300),(#114301,#114302,#114303)),
 .UNSPECIFIED.,.F.,.F.,.F.)
B_SPLINE_SURFACE_WITH_KNOTS((2,2),(3,3),(0.710318915639103,1.),(0.452822299828567,
0.470019760166367),.UNSPECIFIED.)
GEOMETRIC_REPRESENTATION_ITEM()
RATIONAL_B_SPLINE_SURFACE(((0.98875548626282,0.986817927519786,0.987787102172814),
(0.98875548626282,0.986817927519786,0.987787102172814)))
REPRESENTATION_ITEM('')
SURFACE()
);
#1220=(
BOUNDED_SURFACE()
B_SPLINE_SURFACE(1,2,((#114314,#114315,#114316,#114317,#114318),(#114319,
#114320,#114321,#114322,#114323)),.UNSPECIFIED.,.F.,.F.,.F.)
B_SPLINE_SURFACE_WITH_KNOTS((2,2),(3,2,3),(0.709593130086774,1.),(0.262499170165146,
0.263098999273796,0.280537087669266),.UNSPECIFIED.)
GEOMETRIC_REPRESENTATION_ITEM()
RATIONAL_B_SPLINE_SURFACE(((0.989150325841653,0.989150325841653,0.989150325841653,
0.991395311444461,0.996628941948308),(0.989150325841653,0.989150325841653,
0.989150325841653,0.991395311444461,0.996628941948308)))
REPRESENTATION_ITEM('')
SURFACE()
);
#1221=(
BOUNDED_SURFACE()
B_SPLINE_SURFACE(1,2,((#114331,#114332,#114333),(#114334,#114335,#114336)),
 .UNSPECIFIED.,.F.,.F.,.F.)
B_SPLINE_SURFACE_WITH_KNOTS((2,2),(3,3),(0.710318915638382,1.),(0.452822299828567,
0.470019760166367),.UNSPECIFIED.)
GEOMETRIC_REPRESENTATION_ITEM()
RATIONAL_B_SPLINE_SURFACE(((0.98875548626282,0.986817927519786,0.987787102172814),
(0.98875548626282,0.986817927519786,0.987787102172814)))
REPRESENTATION_ITEM('')
SURFACE()
);
#1222=(
BOUNDED_SURFACE()
B_SPLINE_SURFACE(1,2,((#114347,#114348,#114349,#114350,#114351),(#114352,
#114353,#114354,#114355,#114356)),.UNSPECIFIED.,.F.,.F.,.F.)
B_SPLINE_SURFACE_WITH_KNOTS((2,2),(3,2,3),(0.709593130097478,1.),(0.262499170176673,
0.263098999273796,0.280537087669266),.UNSPECIFIED.)
GEOMETRIC_REPRESENTATION_ITEM()
RATIONAL_B_SPLINE_SURFACE(((0.989150325841653,0.989150325841653,0.989150325841653,
0.991395311444461,0.996628941948308),(0.989150325841653,0.989150325841653,
0.989150325841653,0.991395311444461,0.996628941948308)))
REPRESENTATION_ITEM('')
SURFACE()
);
#1223=(
BOUNDED_SURFACE()
B_SPLINE_SURFACE(1,2,((#114364,#114365,#114366),(#114367,#114368,#114369)),
 .UNSPECIFIED.,.F.,.F.,.F.)
B_SPLINE_SURFACE_WITH_KNOTS((2,2),(3,3),(0.71031891563988,1.),(0.452822299828566,
0.470019760166367),.UNSPECIFIED.)
GEOMETRIC_REPRESENTATION_ITEM()
RATIONAL_B_SPLINE_SURFACE(((0.98875548626282,0.986817927519786,0.987787102172814),
(0.98875548626282,0.986817927519786,0.987787102172814)))
REPRESENTATION_ITEM('')
SURFACE()
);
#1224=(
BOUNDED_SURFACE()
B_SPLINE_SURFACE(1,2,((#114380,#114381,#114382,#114383,#114384),(#114385,
#114386,#114387,#114388,#114389)),.UNSPECIFIED.,.F.,.F.,.F.)
B_SPLINE_SURFACE_WITH_KNOTS((2,2),(3,2,3),(0.710192959008239,1.),(0.262924618389841,
0.263098999273796,0.280537087669266),.UNSPECIFIED.)
GEOMETRIC_REPRESENTATION_ITEM()
RATIONAL_B_SPLINE_SURFACE(((0.989150325841653,0.989150325841653,0.989150325841653,
0.991395311444461,0.996628941948308),(0.989150325841653,0.989150325841653,
0.989150325841653,0.991395311444461,0.996628941948308)))
REPRESENTATION_ITEM('')
SURFACE()
);
#1225=(
BOUNDED_SURFACE()
B_SPLINE_SURFACE(1,2,((#114397,#114398,#114399),(#114400,#114401,#114402)),
 .UNSPECIFIED.,.F.,.F.,.F.)
B_SPLINE_SURFACE_WITH_KNOTS((2,2),(3,3),(0.710318915638594,1.),(0.452822299828566,
0.470019760166367),.UNSPECIFIED.)
GEOMETRIC_REPRESENTATION_ITEM()
RATIONAL_B_SPLINE_SURFACE(((0.98875548626282,0.986817927519787,0.987787102172814),
(0.98875548626282,0.986817927519786,0.987787102172814)))
REPRESENTATION_ITEM('')
SURFACE()
);
#1226=(
BOUNDED_SURFACE()
B_SPLINE_SURFACE(1,2,((#114413,#114414,#114415,#114416,#114417),(#114418,
#114419,#114420,#114421,#114422)),.UNSPECIFIED.,.F.,.F.,.F.)
B_SPLINE_SURFACE_WITH_KNOTS((2,2),(3,2,3),(0.710192959006949,1.),(0.262924618389841,
0.263098999273796,0.280537087669266),.UNSPECIFIED.)
GEOMETRIC_REPRESENTATION_ITEM()
RATIONAL_B_SPLINE_SURFACE(((0.989150325841653,0.989150325841653,0.989150325841653,
0.991395311444461,0.996628941948308),(0.989150325841653,0.989150325841653,
0.989150325841653,0.991395311444461,0.996628941948308)))
REPRESENTATION_ITEM('')
SURFACE()
);
#1227=(
BOUNDED_SURFACE()
B_SPLINE_SURFACE(1,2,((#114430,#114431,#114432),(#114433,#114434,#114435)),
 .UNSPECIFIED.,.F.,.F.,.F.)
B_SPLINE_SURFACE_WITH_KNOTS((2,2),(3,3),(0.710318915638842,1.),(0.452822299828566,
0.47001976016637),.UNSPECIFIED.)
GEOMETRIC_REPRESENTATION_ITEM()
RATIONAL_B_SPLINE_SURFACE(((0.98875548626282,0.986817927519786,0.987787102172814),
(0.98875548626282,0.986817927519786,0.987787102172814)))
REPRESENTATION_ITEM('')
SURFACE()
);
#1228=(
BOUNDED_SURFACE()
B_SPLINE_SURFACE(1,2,((#114446,#114447,#114448,#114449,#114450),(#114451,
#114452,#114453,#114454,#114455)),.UNSPECIFIED.,.F.,.F.,.F.)
B_SPLINE_SURFACE_WITH_KNOTS((2,2),(3,2,3),(0.710192959007197,1.),(0.262924618389841,
0.263098999273796,0.280537087669266),.UNSPECIFIED.)
GEOMETRIC_REPRESENTATION_ITEM()
RATIONAL_B_SPLINE_SURFACE(((0.989150325841653,0.989150325841653,0.989150325841653,
0.991395311444461,0.996628941948308),(0.989150325841653,0.989150325841653,
0.989150325841653,0.991395311444461,0.996628941948308)))
REPRESENTATION_ITEM('')
SURFACE()
);
#1229=(
BOUNDED_SURFACE()
B_SPLINE_SURFACE(1,2,((#114463,#114464,#114465),(#114466,#114467,#114468)),
 .UNSPECIFIED.,.F.,.F.,.F.)
B_SPLINE_SURFACE_WITH_KNOTS((2,2),(3,3),(0.71031891563908,1.),(0.452822299828567,
0.470019760166368),.UNSPECIFIED.)
GEOMETRIC_REPRESENTATION_ITEM()
RATIONAL_B_SPLINE_SURFACE(((0.98875548626282,0.986817927519786,0.987787102172814),
(0.98875548626282,0.986817927519786,0.987787102172814)))
REPRESENTATION_ITEM('')
SURFACE()
);
#1230=(
BOUNDED_SURFACE()
B_SPLINE_SURFACE(1,2,((#114479,#114480,#114481,#114482,#114483),(#114484,
#114485,#114486,#114487,#114488)),.UNSPECIFIED.,.F.,.F.,.F.)
B_SPLINE_SURFACE_WITH_KNOTS((2,2),(3,2,3),(0.709593130094452,1.),(0.262499170161042,
0.263098999273796,0.280537087669266),.UNSPECIFIED.)
GEOMETRIC_REPRESENTATION_ITEM()
RATIONAL_B_SPLINE_SURFACE(((0.989150325841653,0.989150325841653,0.989150325841653,
0.991395311444461,0.996628941948308),(0.989150325841653,0.989150325841653,
0.989150325841653,0.991395311444461,0.996628941948308)))
REPRESENTATION_ITEM('')
SURFACE()
);
#1231=(
BOUNDED_SURFACE()
B_SPLINE_SURFACE(1,2,((#114496,#114497,#114498),(#114499,#114500,#114501)),
 .UNSPECIFIED.,.F.,.F.,.F.)
B_SPLINE_SURFACE_WITH_KNOTS((2,2),(3,3),(0.710318915639153,1.),(0.452822299828566,
0.470019760166367),.UNSPECIFIED.)
GEOMETRIC_REPRESENTATION_ITEM()
RATIONAL_B_SPLINE_SURFACE(((0.98875548626282,0.986817927519786,0.987787102172814),
(0.98875548626282,0.986817927519786,0.987787102172814)))
REPRESENTATION_ITEM('')
SURFACE()
);
#1232=(
BOUNDED_SURFACE()
B_SPLINE_SURFACE(1,2,((#114512,#114513,#114514,#114515,#114516),(#114517,
#114518,#114519,#114520,#114521)),.UNSPECIFIED.,.F.,.F.,.F.)
B_SPLINE_SURFACE_WITH_KNOTS((2,2),(3,2,3),(0.70959313010617,1.),(0.262499170172683,
0.263098999273796,0.280537087669266),.UNSPECIFIED.)
GEOMETRIC_REPRESENTATION_ITEM()
RATIONAL_B_SPLINE_SURFACE(((0.989150325841653,0.989150325841653,0.989150325841653,
0.991395311444461,0.996628941948308),(0.989150325841653,0.989150325841653,
0.989150325841653,0.991395311444461,0.996628941948308)))
REPRESENTATION_ITEM('')
SURFACE()
);
#1233=(
BOUNDED_SURFACE()
B_SPLINE_SURFACE(1,2,((#114529,#114530,#114531),(#114532,#114533,#114534)),
 .UNSPECIFIED.,.F.,.F.,.F.)
B_SPLINE_SURFACE_WITH_KNOTS((2,2),(3,3),(0.710318915638837,1.),(0.452822299828566,
0.470019760166367),.UNSPECIFIED.)
GEOMETRIC_REPRESENTATION_ITEM()
RATIONAL_B_SPLINE_SURFACE(((0.98875548626282,0.986817927519786,0.987787102172814),
(0.98875548626282,0.986817927519786,0.987787102172814)))
REPRESENTATION_ITEM('')
SURFACE()
);
#1234=(
BOUNDED_SURFACE()
B_SPLINE_SURFACE(1,2,((#114545,#114546,#114547,#114548,#114549),(#114550,
#114551,#114552,#114553,#114554)),.UNSPECIFIED.,.F.,.F.,.F.)
B_SPLINE_SURFACE_WITH_KNOTS((2,2),(3,2,3),(0.709593130114102,1.),(0.262499170180933,
0.263098999273796,0.280537087669266),.UNSPECIFIED.)
GEOMETRIC_REPRESENTATION_ITEM()
RATIONAL_B_SPLINE_SURFACE(((0.989150325841653,0.989150325841653,0.989150325841653,
0.991395311444461,0.996628941948308),(0.989150325841653,0.989150325841653,
0.989150325841653,0.991395311444461,0.996628941948308)))
REPRESENTATION_ITEM('')
SURFACE()
);
#1235=(
BOUNDED_SURFACE()
B_SPLINE_SURFACE(1,2,((#114562,#114563,#114564),(#114565,#114566,#114567)),
 .UNSPECIFIED.,.F.,.F.,.F.)
B_SPLINE_SURFACE_WITH_KNOTS((2,2),(3,3),(0.710318915638982,1.),(0.452822299828566,
0.470019760166367),.UNSPECIFIED.)
GEOMETRIC_REPRESENTATION_ITEM()
RATIONAL_B_SPLINE_SURFACE(((0.98875548626282,0.986817927519786,0.987787102172814),
(0.98875548626282,0.986817927519786,0.987787102172814)))
REPRESENTATION_ITEM('')
SURFACE()
);
#1236=(
BOUNDED_SURFACE()
B_SPLINE_SURFACE(1,2,((#114578,#114579,#114580,#114581,#114582),(#114583,
#114584,#114585,#114586,#114587)),.UNSPECIFIED.,.F.,.F.,.F.)
B_SPLINE_SURFACE_WITH_KNOTS((2,2),(3,2,3),(0.709593130112758,1.),(0.262499170191214,
0.263098999273796,0.280537087669266),.UNSPECIFIED.)
GEOMETRIC_REPRESENTATION_ITEM()
RATIONAL_B_SPLINE_SURFACE(((0.989150325841653,0.989150325841653,0.989150325841653,
0.991395311444461,0.996628941948308),(0.989150325841653,0.989150325841653,
0.989150325841653,0.991395311444461,0.996628941948308)))
REPRESENTATION_ITEM('')
SURFACE()
);
#1237=(
BOUNDED_SURFACE()
B_SPLINE_SURFACE(1,2,((#114601,#114602,#114603),(#114604,#114605,#114606)),
 .UNSPECIFIED.,.F.,.F.,.F.)
B_SPLINE_SURFACE_WITH_KNOTS((2,2),(3,3),(0.710318915638967,1.),(0.452822299828566,
0.470019760166367),.UNSPECIFIED.)
GEOMETRIC_REPRESENTATION_ITEM()
RATIONAL_B_SPLINE_SURFACE(((0.98875548626282,0.986817927519786,0.987787102172814),
(0.98875548626282,0.986817927519786,0.987787102172814)))
REPRESENTATION_ITEM('')
SURFACE()
);
#1238=(
BOUNDED_SURFACE()
B_SPLINE_SURFACE(1,2,((#114608,#114609,#114610),(#114611,#114612,#114613)),
 .UNSPECIFIED.,.F.,.F.,.F.)
B_SPLINE_SURFACE_WITH_KNOTS((2,2),(3,3),(0.710318915639666,1.),(0.297753987024626,
0.314942866188521),.UNSPECIFIED.)
GEOMETRIC_REPRESENTATION_ITEM()
RATIONAL_B_SPLINE_SURFACE(((0.992972556818501,0.988973049555645,0.987877375613931),
(0.992972556818501,0.988973049555645,0.987877375613931)))
REPRESENTATION_ITEM('')
SURFACE()
);
#1239=(
BOUNDED_SURFACE()
B_SPLINE_SURFACE(1,2,((#114622,#114623,#114624,#114625,#114626),(#114627,
#114628,#114629,#114630,#114631)),.UNSPECIFIED.,.F.,.F.,.F.)
B_SPLINE_SURFACE_WITH_KNOTS((2,2),(3,2,3),(0.710192959008103,1.),(0.418312080773434,
0.428571428571429,0.435879799328077),.UNSPECIFIED.)
GEOMETRIC_REPRESENTATION_ITEM()
RATIONAL_B_SPLINE_SURFACE(((0.99383221411677,0.996398874234721,1.,0.997434694412141,
0.995394338545807),(0.99383221411677,0.996398874234721,1.,0.997434694412141,
0.995394338545807)))
REPRESENTATION_ITEM('')
SURFACE()
);
#1240=(
BOUNDED_SURFACE()
B_SPLINE_SURFACE(1,2,((#114646,#114647,#114648),(#114649,#114650,#114651)),
 .UNSPECIFIED.,.F.,.F.,.F.)
B_SPLINE_SURFACE_WITH_KNOTS((2,2),(3,3),(0.710318915639748,1.),(0.297753987024626,
0.314942866188516),.UNSPECIFIED.)
GEOMETRIC_REPRESENTATION_ITEM()
RATIONAL_B_SPLINE_SURFACE(((0.992972556818501,0.988973049555646,0.987877375613931),
(0.992972556818501,0.988973049555646,0.987877375613931)))
REPRESENTATION_ITEM('')
SURFACE()
);
#1241=(
BOUNDED_SURFACE()
B_SPLINE_SURFACE(1,2,((#114653,#114654,#114655,#114656,#114657),(#114658,
#114659,#114660,#114661,#114662)),.UNSPECIFIED.,.F.,.F.,.F.)
B_SPLINE_SURFACE_WITH_KNOTS((2,2),(3,2,3),(0.710192959007989,1.),(0.418312080773434,
0.428571428571429,0.435879799327622),.UNSPECIFIED.)
GEOMETRIC_REPRESENTATION_ITEM()
RATIONAL_B_SPLINE_SURFACE(((0.99383221411677,0.996398874234721,1.,0.997434694412301,
0.995394338546061),(0.99383221411677,0.996398874234721,1.,0.997434694412301,
0.995394338546061)))
REPRESENTATION_ITEM('')
SURFACE()
);
#1242=(
BOUNDED_SURFACE()
B_SPLINE_SURFACE(1,2,((#114677,#114678,#114679),(#114680,#114681,#114682)),
 .UNSPECIFIED.,.F.,.F.,.F.)
B_SPLINE_SURFACE_WITH_KNOTS((2,2),(3,3),(0.710318915639632,1.),(0.297753987024127,
0.314942866188516),.UNSPECIFIED.)
GEOMETRIC_REPRESENTATION_ITEM()
RATIONAL_B_SPLINE_SURFACE(((0.992972556818734,0.988973049555678,0.987877375613931),
(0.992972556818734,0.988973049555678,0.987877375613931)))
REPRESENTATION_ITEM('')
SURFACE()
);
#1243=(
BOUNDED_SURFACE()
B_SPLINE_SURFACE(1,2,((#114684,#114685,#114686,#114687,#114688),(#114689,
#114690,#114691,#114692,#114693)),.UNSPECIFIED.,.F.,.F.,.F.)
B_SPLINE_SURFACE_WITH_KNOTS((2,2),(3,2,3),(0.710192959006973,1.),(0.41831208077343,
0.428571428571429,0.435879799328077),.UNSPECIFIED.)
GEOMETRIC_REPRESENTATION_ITEM()
RATIONAL_B_SPLINE_SURFACE(((0.993832214116768,0.996398874234719,1.,0.997434694412141,
0.995394338545807),(0.993832214116768,0.996398874234719,1.,0.997434694412141,
0.995394338545807)))
REPRESENTATION_ITEM('')
SURFACE()
);
#1244=(
BOUNDED_SURFACE()
B_SPLINE_SURFACE(1,2,((#114708,#114709,#114710),(#114711,#114712,#114713)),
 .UNSPECIFIED.,.F.,.F.,.F.)
B_SPLINE_SURFACE_WITH_KNOTS((2,2),(3,3),(0.71031891563896,1.),(0.297753987024626,
0.314942866188516),.UNSPECIFIED.)
GEOMETRIC_REPRESENTATION_ITEM()
RATIONAL_B_SPLINE_SURFACE(((0.992972556818501,0.988973049555646,0.987877375613931),
(0.992972556818501,0.988973049555646,0.987877375613931)))
REPRESENTATION_ITEM('')
SURFACE()
);
#1245=(
BOUNDED_SURFACE()
B_SPLINE_SURFACE(1,2,((#114715,#114716,#114717,#114718,#114719),(#114720,
#114721,#114722,#114723,#114724)),.UNSPECIFIED.,.F.,.F.,.F.)
B_SPLINE_SURFACE_WITH_KNOTS((2,2),(3,2,3),(0.710192959007242,1.),(0.418312080773432,
0.428571428571429,0.435879799328077),.UNSPECIFIED.)
GEOMETRIC_REPRESENTATION_ITEM()
RATIONAL_B_SPLINE_SURFACE(((0.993832214116769,0.99639887423472,1.,0.997434694412141,
0.995394338545807),(0.993832214116769,0.99639887423472,1.,0.997434694412141,
0.995394338545807)))
REPRESENTATION_ITEM('')
SURFACE()
);
#1246=(
BOUNDED_SURFACE()
B_SPLINE_SURFACE(1,2,((#114739,#114740,#114741),(#114742,#114743,#114744)),
 .UNSPECIFIED.,.F.,.F.,.F.)
B_SPLINE_SURFACE_WITH_KNOTS((2,2),(3,3),(0.710318915639108,1.),(0.297753987024626,
0.314942866188543),.UNSPECIFIED.)
GEOMETRIC_REPRESENTATION_ITEM()
RATIONAL_B_SPLINE_SURFACE(((0.992972556818502,0.98897304955564,0.987877375613928),
(0.992972556818501,0.98897304955564,0.987877375613928)))
REPRESENTATION_ITEM('')
SURFACE()
);
#1247=(
BOUNDED_SURFACE()
B_SPLINE_SURFACE(1,2,((#114746,#114747,#114748,#114749,#114750),(#114751,
#114752,#114753,#114754,#114755)),.UNSPECIFIED.,.F.,.F.,.F.)
B_SPLINE_SURFACE_WITH_KNOTS((2,2),(3,2,3),(0.710192959007502,1.),(0.418312080773435,
0.428571428571429,0.435879799328077),.UNSPECIFIED.)
GEOMETRIC_REPRESENTATION_ITEM()
RATIONAL_B_SPLINE_SURFACE(((0.99383221411677,0.996398874234721,1.,0.997434694412141,
0.995394338545807),(0.99383221411677,0.996398874234721,1.,0.997434694412141,
0.995394338545807)))
REPRESENTATION_ITEM('')
SURFACE()
);
#1248=(
BOUNDED_SURFACE()
B_SPLINE_SURFACE(1,2,((#114770,#114771,#114772),(#114773,#114774,#114775)),
 .UNSPECIFIED.,.F.,.F.,.F.)
B_SPLINE_SURFACE_WITH_KNOTS((2,2),(3,3),(0.710318915639139,1.),(0.297753987024626,
0.314942866188516),.UNSPECIFIED.)
GEOMETRIC_REPRESENTATION_ITEM()
RATIONAL_B_SPLINE_SURFACE(((0.992972556818501,0.988973049555646,0.987877375613931),
(0.992972556818501,0.988973049555646,0.987877375613931)))
REPRESENTATION_ITEM('')
SURFACE()
);
#1249=(
BOUNDED_SURFACE()
B_SPLINE_SURFACE(1,2,((#114777,#114778,#114779,#114780,#114781),(#114782,
#114783,#114784,#114785,#114786)),.UNSPECIFIED.,.F.,.F.,.F.)
B_SPLINE_SURFACE_WITH_KNOTS((2,2),(3,2,3),(0.710192959007329,1.),(0.418312080773434,
0.428571428571429,0.435879799328077),.UNSPECIFIED.)
GEOMETRIC_REPRESENTATION_ITEM()
RATIONAL_B_SPLINE_SURFACE(((0.99383221411677,0.996398874234721,1.,0.997434694412141,
0.995394338545807),(0.99383221411677,0.996398874234721,1.,0.997434694412141,
0.995394338545807)))
REPRESENTATION_ITEM('')
SURFACE()
);
#1250=(
BOUNDED_SURFACE()
B_SPLINE_SURFACE(1,2,((#114801,#114802,#114803),(#114804,#114805,#114806)),
 .UNSPECIFIED.,.F.,.F.,.F.)
B_SPLINE_SURFACE_WITH_KNOTS((2,2),(3,3),(0.710318915638972,1.),(0.297753987024626,
0.314942866188516),.UNSPECIFIED.)
GEOMETRIC_REPRESENTATION_ITEM()
RATIONAL_B_SPLINE_SURFACE(((0.992972556818502,0.988973049555647,0.987877375613931),
(0.992972556818502,0.988973049555647,0.987877375613931)))
REPRESENTATION_ITEM('')
SURFACE()
);
#1251=(
BOUNDED_SURFACE()
B_SPLINE_SURFACE(1,2,((#114808,#114809,#114810,#114811,#114812),(#114813,
#114814,#114815,#114816,#114817)),.UNSPECIFIED.,.F.,.F.,.F.)
B_SPLINE_SURFACE_WITH_KNOTS((2,2),(3,2,3),(0.710192959008261,1.),(0.418312080773434,
0.428571428571429,0.435879799328077),.UNSPECIFIED.)
GEOMETRIC_REPRESENTATION_ITEM()
RATIONAL_B_SPLINE_SURFACE(((0.99383221411677,0.996398874234721,1.,0.997434694412141,
0.995394338545807),(0.99383221411677,0.996398874234721,1.,0.997434694412141,
0.995394338545807)))
REPRESENTATION_ITEM('')
SURFACE()
);
#1252=(
BOUNDED_SURFACE()
B_SPLINE_SURFACE(1,2,((#114832,#114833,#114834),(#114835,#114836,#114837)),
 .UNSPECIFIED.,.F.,.F.,.F.)
B_SPLINE_SURFACE_WITH_KNOTS((2,2),(3,3),(0.710318915639903,1.),(0.297753987024626,
0.314942866188516),.UNSPECIFIED.)
GEOMETRIC_REPRESENTATION_ITEM()
RATIONAL_B_SPLINE_SURFACE(((0.992972556818501,0.988973049555646,0.987877375613931),
(0.992972556818501,0.988973049555646,0.987877375613931)))
REPRESENTATION_ITEM('')
SURFACE()
);
#1253=(
BOUNDED_SURFACE()
B_SPLINE_SURFACE(1,2,((#114839,#114840,#114841,#114842,#114843),(#114844,
#114845,#114846,#114847,#114848)),.UNSPECIFIED.,.F.,.F.,.F.)
B_SPLINE_SURFACE_WITH_KNOTS((2,2),(3,2,3),(0.71019295900825,1.),(0.418312080773434,
0.428571428571429,0.435879799328077),.UNSPECIFIED.)
GEOMETRIC_REPRESENTATION_ITEM()
RATIONAL_B_SPLINE_SURFACE(((0.99383221411677,0.996398874234721,1.,0.997434694412141,
0.995394338545807),(0.99383221411677,0.996398874234721,1.,0.997434694412141,
0.995394338545807)))
REPRESENTATION_ITEM('')
SURFACE()
);
#1254=(
BOUNDED_SURFACE()
B_SPLINE_SURFACE(1,2,((#114863,#114864,#114865),(#114866,#114867,#114868)),
 .UNSPECIFIED.,.F.,.F.,.F.)
B_SPLINE_SURFACE_WITH_KNOTS((2,2),(3,3),(0.710318915639894,1.),(0.297753987024626,
0.314942866188516),.UNSPECIFIED.)
GEOMETRIC_REPRESENTATION_ITEM()
RATIONAL_B_SPLINE_SURFACE(((0.992972556818502,0.988973049555647,0.987877375613931),
(0.992972556818502,0.988973049555647,0.987877375613931)))
REPRESENTATION_ITEM('')
SURFACE()
);
#1255=(
BOUNDED_SURFACE()
B_SPLINE_SURFACE(1,2,((#114870,#114871,#114872,#114873,#114874),(#114875,
#114876,#114877,#114878,#114879)),.UNSPECIFIED.,.F.,.F.,.F.)
B_SPLINE_SURFACE_WITH_KNOTS((2,2),(3,2,3),(0.710192959008146,1.),(0.418312080773434,
0.428571428571429,0.435879799328077),.UNSPECIFIED.)
GEOMETRIC_REPRESENTATION_ITEM()
RATIONAL_B_SPLINE_SURFACE(((0.99383221411677,0.996398874234721,1.,0.997434694412141,
0.995394338545807),(0.99383221411677,0.996398874234721,1.,0.997434694412141,
0.995394338545807)))
REPRESENTATION_ITEM('')
SURFACE()
);
#1256=(
BOUNDED_SURFACE()
B_SPLINE_SURFACE(1,2,((#114894,#114895,#114896),(#114897,#114898,#114899)),
 .UNSPECIFIED.,.F.,.F.,.F.)
B_SPLINE_SURFACE_WITH_KNOTS((2,2),(3,3),(0.710318915639792,1.),(0.29775398702454,
0.314942866188516),.UNSPECIFIED.)
GEOMETRIC_REPRESENTATION_ITEM()
RATIONAL_B_SPLINE_SURFACE(((0.992972556818541,0.988973049555652,0.987877375613931),
(0.992972556818541,0.988973049555652,0.987877375613931)))
REPRESENTATION_ITEM('')
SURFACE()
);
#1257=(
BOUNDED_SURFACE()
B_SPLINE_SURFACE(1,2,((#114901,#114902,#114903,#114904,#114905),(#114906,
#114907,#114908,#114909,#114910)),.UNSPECIFIED.,.F.,.F.,.F.)
B_SPLINE_SURFACE_WITH_KNOTS((2,2),(3,2,3),(0.710192959008211,1.),(0.418312080773434,
0.428571428571429,0.435879799328077),.UNSPECIFIED.)
GEOMETRIC_REPRESENTATION_ITEM()
RATIONAL_B_SPLINE_SURFACE(((0.99383221411677,0.996398874234721,1.,0.997434694412141,
0.995394338545807),(0.99383221411677,0.996398874234721,1.,0.997434694412141,
0.995394338545807)))
REPRESENTATION_ITEM('')
SURFACE()
);
#1258=(
BOUNDED_SURFACE()
B_SPLINE_SURFACE(1,2,((#114925,#114926,#114927),(#114928,#114929,#114930)),
 .UNSPECIFIED.,.F.,.F.,.F.)
B_SPLINE_SURFACE_WITH_KNOTS((2,2),(3,3),(0.710318915639852,1.),(0.297753987024605,
0.314942866188516),.UNSPECIFIED.)
GEOMETRIC_REPRESENTATION_ITEM()
RATIONAL_B_SPLINE_SURFACE(((0.992972556818511,0.988973049555648,0.987877375613931),
(0.992972556818511,0.988973049555648,0.987877375613931)))
REPRESENTATION_ITEM('')
SURFACE()
);
#1259=(
BOUNDED_SURFACE()
B_SPLINE_SURFACE(1,2,((#114932,#114933,#114934,#114935,#114936),(#114937,
#114938,#114939,#114940,#114941)),.UNSPECIFIED.,.F.,.F.,.F.)
B_SPLINE_SURFACE_WITH_KNOTS((2,2),(3,2,3),(0.710192959008243,1.),(0.418312080773434,
0.428571428571429,0.435879799328077),.UNSPECIFIED.)
GEOMETRIC_REPRESENTATION_ITEM()
RATIONAL_B_SPLINE_SURFACE(((0.99383221411677,0.996398874234721,1.,0.997434694412141,
0.995394338545807),(0.99383221411677,0.996398874234721,1.,0.997434694412141,
0.995394338545807)))
REPRESENTATION_ITEM('')
SURFACE()
);
#1260=(
BOUNDED_SURFACE()
B_SPLINE_SURFACE(1,2,((#114956,#114957,#114958),(#114959,#114960,#114961)),
 .UNSPECIFIED.,.F.,.F.,.F.)
B_SPLINE_SURFACE_WITH_KNOTS((2,2),(3,3),(0.71031891563988,1.),(0.297753987024518,
0.314942866188516),.UNSPECIFIED.)
GEOMETRIC_REPRESENTATION_ITEM()
RATIONAL_B_SPLINE_SURFACE(((0.992972556818552,0.988973049555653,0.987877375613931),
(0.992972556818552,0.988973049555653,0.987877375613931)))
REPRESENTATION_ITEM('')
SURFACE()
);
#1261=(
BOUNDED_SURFACE()
B_SPLINE_SURFACE(1,2,((#114963,#114964,#114965,#114966,#114967),(#114968,
#114969,#114970,#114971,#114972)),.UNSPECIFIED.,.F.,.F.,.F.)
B_SPLINE_SURFACE_WITH_KNOTS((2,2),(3,2,3),(0.71019295900829,1.),(0.418312080773434,
0.428571428571429,0.435879799328077),.UNSPECIFIED.)
GEOMETRIC_REPRESENTATION_ITEM()
RATIONAL_B_SPLINE_SURFACE(((0.99383221411677,0.996398874234721,1.,0.997434694412141,
0.995394338545807),(0.99383221411677,0.996398874234721,1.,0.997434694412141,
0.995394338545807)))
REPRESENTATION_ITEM('')
SURFACE()
);
#1262=(
BOUNDED_SURFACE()
B_SPLINE_SURFACE(1,2,((#114987,#114988,#114989),(#114990,#114991,#114992)),
 .UNSPECIFIED.,.F.,.F.,.F.)
B_SPLINE_SURFACE_WITH_KNOTS((2,2),(3,3),(0.710318915639924,1.),(0.297753987024626,
0.314942866188516),.UNSPECIFIED.)
GEOMETRIC_REPRESENTATION_ITEM()
RATIONAL_B_SPLINE_SURFACE(((0.992972556818502,0.988973049555646,0.987877375613931),
(0.992972556818502,0.988973049555646,0.987877375613931)))
REPRESENTATION_ITEM('')
SURFACE()
);
#1263=(
BOUNDED_SURFACE()
B_SPLINE_SURFACE(1,2,((#114994,#114995,#114996,#114997,#114998),(#114999,
#115000,#115001,#115002,#115003)),.UNSPECIFIED.,.F.,.F.,.F.)
B_SPLINE_SURFACE_WITH_KNOTS((2,2),(3,2,3),(0.710192959008442,1.),(0.418312080773434,
0.428571428571429,0.435879799328077),.UNSPECIFIED.)
GEOMETRIC_REPRESENTATION_ITEM()
RATIONAL_B_SPLINE_SURFACE(((0.99383221411677,0.996398874234721,1.,0.997434694412141,
0.995394338545807),(0.99383221411677,0.996398874234721,1.,0.997434694412141,
0.995394338545807)))
REPRESENTATION_ITEM('')
SURFACE()
);
#1264=(
BOUNDED_SURFACE()
B_SPLINE_SURFACE(1,2,((#115018,#115019,#115020),(#115021,#115022,#115023)),
 .UNSPECIFIED.,.F.,.F.,.F.)
B_SPLINE_SURFACE_WITH_KNOTS((2,2),(3,3),(0.710318915640075,1.),(0.297753987024626,
0.314942866188516),.UNSPECIFIED.)
GEOMETRIC_REPRESENTATION_ITEM()
RATIONAL_B_SPLINE_SURFACE(((0.992972556818502,0.988973049555646,0.987877375613931),
(0.992972556818502,0.988973049555646,0.987877375613931)))
REPRESENTATION_ITEM('')
SURFACE()
);
#1265=(
BOUNDED_SURFACE()
B_SPLINE_SURFACE(1,2,((#115025,#115026,#115027,#115028,#115029),(#115030,
#115031,#115032,#115033,#115034)),.UNSPECIFIED.,.F.,.F.,.F.)
B_SPLINE_SURFACE_WITH_KNOTS((2,2),(3,2,3),(0.710192959008442,1.),(0.418312080773434,
0.428571428571429,0.435879799328077),.UNSPECIFIED.)
GEOMETRIC_REPRESENTATION_ITEM()
RATIONAL_B_SPLINE_SURFACE(((0.99383221411677,0.996398874234721,1.,0.997434694412141,
0.995394338545807),(0.99383221411677,0.996398874234721,1.,0.997434694412141,
0.995394338545807)))
REPRESENTATION_ITEM('')
SURFACE()
);
#1266=(
BOUNDED_SURFACE()
B_SPLINE_SURFACE(1,2,((#115049,#115050,#115051),(#115052,#115053,#115054)),
 .UNSPECIFIED.,.F.,.F.,.F.)
B_SPLINE_SURFACE_WITH_KNOTS((2,2),(3,3),(0.710318915640075,1.),(0.297753987024626,
0.314942866188516),.UNSPECIFIED.)
GEOMETRIC_REPRESENTATION_ITEM()
RATIONAL_B_SPLINE_SURFACE(((0.992972556818501,0.988973049555646,0.987877375613931),
(0.992972556818501,0.988973049555646,0.987877375613931)))
REPRESENTATION_ITEM('')
SURFACE()
);
#1267=(
BOUNDED_SURFACE()
B_SPLINE_SURFACE(1,2,((#115056,#115057,#115058,#115059,#115060),(#115061,
#115062,#115063,#115064,#115065)),.UNSPECIFIED.,.F.,.F.,.F.)
B_SPLINE_SURFACE_WITH_KNOTS((2,2),(3,2,3),(0.710192959008435,1.),(0.418312080773434,
0.428571428571429,0.435879799328077),.UNSPECIFIED.)
GEOMETRIC_REPRESENTATION_ITEM()
RATIONAL_B_SPLINE_SURFACE(((0.99383221411677,0.996398874234721,1.,0.997434694412141,
0.995394338545807),(0.99383221411677,0.996398874234721,1.,0.997434694412141,
0.995394338545807)))
REPRESENTATION_ITEM('')
SURFACE()
);
#1268=(
BOUNDED_SURFACE()
B_SPLINE_SURFACE(1,2,((#115080,#115081,#115082),(#115083,#115084,#115085)),
 .UNSPECIFIED.,.F.,.F.,.F.)
B_SPLINE_SURFACE_WITH_KNOTS((2,2),(3,3),(0.710318915640074,1.),(0.297753987024626,
0.314942866188517),.UNSPECIFIED.)
GEOMETRIC_REPRESENTATION_ITEM()
RATIONAL_B_SPLINE_SURFACE(((0.992972556818502,0.988973049555646,0.987877375613931),
(0.992972556818502,0.988973049555646,0.987877375613931)))
REPRESENTATION_ITEM('')
SURFACE()
);
#1269=(
BOUNDED_SURFACE()
B_SPLINE_SURFACE(1,2,((#115087,#115088,#115089,#115090,#115091),(#115092,
#115093,#115094,#115095,#115096)),.UNSPECIFIED.,.F.,.F.,.F.)
B_SPLINE_SURFACE_WITH_KNOTS((2,2),(3,2,3),(0.710192959008438,1.),(0.418312080773434,
0.428571428571429,0.435879799328077),.UNSPECIFIED.)
GEOMETRIC_REPRESENTATION_ITEM()
RATIONAL_B_SPLINE_SURFACE(((0.99383221411677,0.996398874234721,1.,0.997434694412141,
0.995394338545807),(0.99383221411677,0.996398874234721,1.,0.997434694412141,
0.995394338545807)))
REPRESENTATION_ITEM('')
SURFACE()
);
#1270=(
BOUNDED_SURFACE()
B_SPLINE_SURFACE(1,2,((#115111,#115112,#115113),(#115114,#115115,#115116)),
 .UNSPECIFIED.,.F.,.F.,.F.)
B_SPLINE_SURFACE_WITH_KNOTS((2,2),(3,3),(0.710318915640078,1.),(0.297753987024626,
0.314942866188516),.UNSPECIFIED.)
GEOMETRIC_REPRESENTATION_ITEM()
RATIONAL_B_SPLINE_SURFACE(((0.992972556818502,0.988973049555647,0.987877375613931),
(0.992972556818502,0.988973049555646,0.987877375613931)))
REPRESENTATION_ITEM('')
SURFACE()
);
#1271=(
BOUNDED_SURFACE()
B_SPLINE_SURFACE(1,2,((#115118,#115119,#115120,#115121,#115122),(#115123,
#115124,#115125,#115126,#115127)),.UNSPECIFIED.,.F.,.F.,.F.)
B_SPLINE_SURFACE_WITH_KNOTS((2,2),(3,2,3),(0.710192959008439,1.),(0.418312080773434,
0.428571428571429,0.435879799328077),.UNSPECIFIED.)
GEOMETRIC_REPRESENTATION_ITEM()
RATIONAL_B_SPLINE_SURFACE(((0.99383221411677,0.996398874234721,1.,0.997434694412141,
0.995394338545807),(0.99383221411677,0.996398874234721,1.,0.997434694412141,
0.995394338545807)))
REPRESENTATION_ITEM('')
SURFACE()
);
#1272=(
BOUNDED_SURFACE()
B_SPLINE_SURFACE(1,2,((#115142,#115143,#115144),(#115145,#115146,#115147)),
 .UNSPECIFIED.,.F.,.F.,.F.)
B_SPLINE_SURFACE_WITH_KNOTS((2,2),(3,3),(0.710318915640077,1.),(0.297753987024626,
0.314942866188516),.UNSPECIFIED.)
GEOMETRIC_REPRESENTATION_ITEM()
RATIONAL_B_SPLINE_SURFACE(((0.992972556818502,0.988973049555646,0.987877375613931),
(0.992972556818502,0.988973049555646,0.987877375613931)))
REPRESENTATION_ITEM('')
SURFACE()
);
#1273=(
BOUNDED_SURFACE()
B_SPLINE_SURFACE(1,2,((#115149,#115150,#115151,#115152,#115153),(#115154,
#115155,#115156,#115157,#115158)),.UNSPECIFIED.,.F.,.F.,.F.)
B_SPLINE_SURFACE_WITH_KNOTS((2,2),(3,2,3),(0.710192959008327,1.),(0.418312080773434,
0.428571428571429,0.435879799328077),.UNSPECIFIED.)
GEOMETRIC_REPRESENTATION_ITEM()
RATIONAL_B_SPLINE_SURFACE(((0.99383221411677,0.996398874234721,1.,0.997434694412141,
0.995394338545807),(0.99383221411677,0.996398874234721,1.,0.997434694412141,
0.995394338545807)))
REPRESENTATION_ITEM('')
SURFACE()
);
#1274=(
BOUNDED_SURFACE()
B_SPLINE_SURFACE(1,2,((#115173,#115174,#115175),(#115176,#115177,#115178)),
 .UNSPECIFIED.,.F.,.F.,.F.)
B_SPLINE_SURFACE_WITH_KNOTS((2,2),(3,3),(0.710318915639967,1.),(0.297753987024626,
0.314942866188516),.UNSPECIFIED.)
GEOMETRIC_REPRESENTATION_ITEM()
RATIONAL_B_SPLINE_SURFACE(((0.992972556818502,0.988973049555646,0.987877375613931),
(0.992972556818502,0.988973049555646,0.987877375613931)))
REPRESENTATION_ITEM('')
SURFACE()
);
#1275=(
BOUNDED_SURFACE()
B_SPLINE_SURFACE(1,2,((#115180,#115181,#115182,#115183,#115184),(#115185,
#115186,#115187,#115188,#115189)),.UNSPECIFIED.,.F.,.F.,.F.)
B_SPLINE_SURFACE_WITH_KNOTS((2,2),(3,2,3),(0.71019295900703,1.),(0.418312080773434,
0.428571428571429,0.435879799328077),.UNSPECIFIED.)
GEOMETRIC_REPRESENTATION_ITEM()
RATIONAL_B_SPLINE_SURFACE(((0.99383221411677,0.996398874234721,1.,0.997434694412141,
0.995394338545807),(0.99383221411677,0.996398874234721,1.,0.997434694412141,
0.995394338545807)))
REPRESENTATION_ITEM('')
SURFACE()
);
#1276=(
BOUNDED_SURFACE()
B_SPLINE_SURFACE(1,2,((#115204,#115205,#115206),(#115207,#115208,#115209)),
 .UNSPECIFIED.,.F.,.F.,.F.)
B_SPLINE_SURFACE_WITH_KNOTS((2,2),(3,3),(0.71031891563867,1.),(0.297753987024626,
0.314942866188516),.UNSPECIFIED.)
GEOMETRIC_REPRESENTATION_ITEM()
RATIONAL_B_SPLINE_SURFACE(((0.992972556818502,0.988973049555647,0.987877375613931),
(0.992972556818502,0.988973049555647,0.987877375613931)))
REPRESENTATION_ITEM('')
SURFACE()
);
#1277=(
BOUNDED_SURFACE()
B_SPLINE_SURFACE(1,2,((#115211,#115212,#115213,#115214,#115215),(#115216,
#115217,#115218,#115219,#115220)),.UNSPECIFIED.,.F.,.F.,.F.)
B_SPLINE_SURFACE_WITH_KNOTS((2,2),(3,2,3),(0.710192959008186,1.),(0.418312080773434,
0.428571428571429,0.435879799328077),.UNSPECIFIED.)
GEOMETRIC_REPRESENTATION_ITEM()
RATIONAL_B_SPLINE_SURFACE(((0.99383221411677,0.996398874234721,1.,0.997434694412141,
0.995394338545807),(0.99383221411677,0.996398874234721,1.,0.997434694412141,
0.995394338545807)))
REPRESENTATION_ITEM('')
SURFACE()
);
#1278=(
BOUNDED_SURFACE()
B_SPLINE_SURFACE(1,2,((#115235,#115236,#115237),(#115238,#115239,#115240)),
 .UNSPECIFIED.,.F.,.F.,.F.)
B_SPLINE_SURFACE_WITH_KNOTS((2,2),(3,3),(0.710318915639825,1.),(0.297753987024626,
0.314942866188516),.UNSPECIFIED.)
GEOMETRIC_REPRESENTATION_ITEM()
RATIONAL_B_SPLINE_SURFACE(((0.992972556818502,0.988973049555647,0.987877375613931),
(0.992972556818502,0.988973049555647,0.987877375613931)))
REPRESENTATION_ITEM('')
SURFACE()
);
#1279=(
BOUNDED_SURFACE()
B_SPLINE_SURFACE(1,2,((#115242,#115243,#115244,#115245,#115246),(#115247,
#115248,#115249,#115250,#115251)),.UNSPECIFIED.,.F.,.F.,.F.)
B_SPLINE_SURFACE_WITH_KNOTS((2,2),(3,2,3),(0.710192959008442,1.),(0.418312080773434,
0.428571428571429,0.435879799328077),.UNSPECIFIED.)
GEOMETRIC_REPRESENTATION_ITEM()
RATIONAL_B_SPLINE_SURFACE(((0.99383221411677,0.996398874234721,1.,0.997434694412141,
0.995394338545807),(0.99383221411677,0.996398874234721,1.,0.997434694412141,
0.995394338545807)))
REPRESENTATION_ITEM('')
SURFACE()
);
#1280=(
BOUNDED_SURFACE()
B_SPLINE_SURFACE(1,2,((#115266,#115267,#115268),(#115269,#115270,#115271)),
 .UNSPECIFIED.,.F.,.F.,.F.)
B_SPLINE_SURFACE_WITH_KNOTS((2,2),(3,3),(0.710318915640081,1.),(0.297753987024626,
0.314942866188516),.UNSPECIFIED.)
GEOMETRIC_REPRESENTATION_ITEM()
RATIONAL_B_SPLINE_SURFACE(((0.992972556818501,0.988973049555646,0.987877375613931),
(0.992972556818501,0.988973049555646,0.987877375613931)))
REPRESENTATION_ITEM('')
SURFACE()
);
#1281=(
BOUNDED_SURFACE()
B_SPLINE_SURFACE(1,2,((#115273,#115274,#115275,#115276,#115277),(#115278,
#115279,#115280,#115281,#115282)),.UNSPECIFIED.,.F.,.F.,.F.)
B_SPLINE_SURFACE_WITH_KNOTS((2,2),(3,2,3),(0.71019295900844,1.),(0.418312080773434,
0.428571428571429,0.435879799328077),.UNSPECIFIED.)
GEOMETRIC_REPRESENTATION_ITEM()
RATIONAL_B_SPLINE_SURFACE(((0.99383221411677,0.996398874234721,1.,0.997434694412141,
0.995394338545807),(0.99383221411677,0.996398874234721,1.,0.997434694412141,
0.995394338545807)))
REPRESENTATION_ITEM('')
SURFACE()
);
#1282=(
BOUNDED_SURFACE()
B_SPLINE_SURFACE(1,2,((#115297,#115298,#115299),(#115300,#115301,#115302)),
 .UNSPECIFIED.,.F.,.F.,.F.)
B_SPLINE_SURFACE_WITH_KNOTS((2,2),(3,3),(0.710318915640086,1.),(0.297753987024626,
0.314942866188516),.UNSPECIFIED.)
GEOMETRIC_REPRESENTATION_ITEM()
RATIONAL_B_SPLINE_SURFACE(((0.992972556818502,0.988973049555646,0.987877375613931),
(0.992972556818502,0.988973049555646,0.987877375613931)))
REPRESENTATION_ITEM('')
SURFACE()
);
#1283=(
BOUNDED_SURFACE()
B_SPLINE_SURFACE(1,2,((#115304,#115305,#115306,#115307,#115308),(#115309,
#115310,#115311,#115312,#115313)),.UNSPECIFIED.,.F.,.F.,.F.)
B_SPLINE_SURFACE_WITH_KNOTS((2,2),(3,2,3),(0.710192959008441,1.),(0.418312080773434,
0.428571428571429,0.435879799328077),.UNSPECIFIED.)
GEOMETRIC_REPRESENTATION_ITEM()
RATIONAL_B_SPLINE_SURFACE(((0.99383221411677,0.996398874234721,1.,0.997434694412141,
0.995394338545807),(0.99383221411677,0.996398874234721,1.,0.997434694412141,
0.995394338545807)))
REPRESENTATION_ITEM('')
SURFACE()
);
#1284=(
BOUNDED_SURFACE()
B_SPLINE_SURFACE(1,2,((#115328,#115329,#115330),(#115331,#115332,#115333)),
 .UNSPECIFIED.,.F.,.F.,.F.)
B_SPLINE_SURFACE_WITH_KNOTS((2,2),(3,3),(0.710318915640077,1.),(0.297753987024626,
0.314942866188516),.UNSPECIFIED.)
GEOMETRIC_REPRESENTATION_ITEM()
RATIONAL_B_SPLINE_SURFACE(((0.992972556818502,0.988973049555646,0.987877375613931),
(0.992972556818502,0.988973049555646,0.987877375613931)))
REPRESENTATION_ITEM('')
SURFACE()
);
#1285=(
BOUNDED_SURFACE()
B_SPLINE_SURFACE(1,2,((#115335,#115336,#115337,#115338,#115339),(#115340,
#115341,#115342,#115343,#115344)),.UNSPECIFIED.,.F.,.F.,.F.)
B_SPLINE_SURFACE_WITH_KNOTS((2,2),(3,2,3),(0.71019295900772,1.),(0.418312080773434,
0.428571428571429,0.435879799328076),.UNSPECIFIED.)
GEOMETRIC_REPRESENTATION_ITEM()
RATIONAL_B_SPLINE_SURFACE(((0.99383221411677,0.996398874234721,1.,0.997434694412141,
0.995394338545808),(0.99383221411677,0.996398874234721,1.,0.997434694412141,
0.995394338545808)))
REPRESENTATION_ITEM('')
SURFACE()
);
#1286=(
BOUNDED_SURFACE()
B_SPLINE_SURFACE(1,2,((#115359,#115360,#115361),(#115362,#115363,#115364)),
 .UNSPECIFIED.,.F.,.F.,.F.)
B_SPLINE_SURFACE_WITH_KNOTS((2,2),(3,3),(0.710318915639364,1.),(0.297753987024627,
0.314942866188517),.UNSPECIFIED.)
GEOMETRIC_REPRESENTATION_ITEM()
RATIONAL_B_SPLINE_SURFACE(((0.992972556818501,0.988973049555646,0.987877375613931),
(0.992972556818501,0.988973049555646,0.987877375613931)))
REPRESENTATION_ITEM('')
SURFACE()
);
#1287=(
BOUNDED_SURFACE()
B_SPLINE_SURFACE(1,2,((#115366,#115367,#115368,#115369,#115370),(#115371,
#115372,#115373,#115374,#115375)),.UNSPECIFIED.,.F.,.F.,.F.)
B_SPLINE_SURFACE_WITH_KNOTS((2,2),(3,2,3),(0.710192959008172,1.),(0.418312080773433,
0.428571428571429,0.435879799328076),.UNSPECIFIED.)
GEOMETRIC_REPRESENTATION_ITEM()
RATIONAL_B_SPLINE_SURFACE(((0.993832214116769,0.99639887423472,1.,0.997434694412141,
0.995394338545808),(0.993832214116769,0.99639887423472,1.,0.997434694412141,
0.995394338545808)))
REPRESENTATION_ITEM('')
SURFACE()
);
#1288=(
BOUNDED_SURFACE()
B_SPLINE_SURFACE(1,2,((#115390,#115391,#115392),(#115393,#115394,#115395)),
 .UNSPECIFIED.,.F.,.F.,.F.)
B_SPLINE_SURFACE_WITH_KNOTS((2,2),(3,3),(0.710318915639813,1.),(0.297753987024418,
0.314942866188517),.UNSPECIFIED.)
GEOMETRIC_REPRESENTATION_ITEM()
RATIONAL_B_SPLINE_SURFACE(((0.992972556818598,0.988973049555659,0.987877375613931),
(0.992972556818598,0.988973049555659,0.987877375613931)))
REPRESENTATION_ITEM('')
SURFACE()
);
#1289=(
BOUNDED_SURFACE()
B_SPLINE_SURFACE(1,2,((#115397,#115398,#115399,#115400,#115401),(#115402,
#115403,#115404,#115405,#115406)),.UNSPECIFIED.,.F.,.F.,.F.)
B_SPLINE_SURFACE_WITH_KNOTS((2,2),(3,2,3),(0.710192959008117,1.),(0.418312080773433,
0.428571428571429,0.435879799328042),.UNSPECIFIED.)
GEOMETRIC_REPRESENTATION_ITEM()
RATIONAL_B_SPLINE_SURFACE(((0.99383221411677,0.99639887423472,1.,0.997434694412154,
0.995394338545827),(0.99383221411677,0.99639887423472,1.,0.997434694412154,
0.995394338545827)))
REPRESENTATION_ITEM('')
SURFACE()
);
#1290=(
BOUNDED_SURFACE()
B_SPLINE_SURFACE(1,2,((#115421,#115422,#115423),(#115424,#115425,#115426)),
 .UNSPECIFIED.,.F.,.F.,.F.)
B_SPLINE_SURFACE_WITH_KNOTS((2,2),(3,3),(0.710318915639757,1.),(0.297753987024401,
0.314942866188517),.UNSPECIFIED.)
GEOMETRIC_REPRESENTATION_ITEM()
RATIONAL_B_SPLINE_SURFACE(((0.992972556818606,0.98897304955566,0.987877375613931),
(0.992972556818606,0.98897304955566,0.987877375613931)))
REPRESENTATION_ITEM('')
SURFACE()
);
#1291=(
BOUNDED_SURFACE()
B_SPLINE_SURFACE(1,2,((#115428,#115429,#115430,#115431,#115432),(#115433,
#115434,#115435,#115436,#115437)),.UNSPECIFIED.,.F.,.F.,.F.)
B_SPLINE_SURFACE_WITH_KNOTS((2,2),(3,2,3),(0.710192959008159,1.),(0.418312080773433,
0.428571428571429,0.435879799328077),.UNSPECIFIED.)
GEOMETRIC_REPRESENTATION_ITEM()
RATIONAL_B_SPLINE_SURFACE(((0.993832214116769,0.99639887423472,1.,0.997434694412141,
0.995394338545807),(0.993832214116769,0.99639887423472,1.,0.997434694412141,
0.995394338545807)))
REPRESENTATION_ITEM('')
SURFACE()
);
#1292=(
BOUNDED_SURFACE()
B_SPLINE_SURFACE(1,2,((#115452,#115453,#115454),(#115455,#115456,#115457)),
 .UNSPECIFIED.,.F.,.F.,.F.)
B_SPLINE_SURFACE_WITH_KNOTS((2,2),(3,3),(0.710318915639801,1.),(0.297753987024479,
0.314942866188516),.UNSPECIFIED.)
GEOMETRIC_REPRESENTATION_ITEM()
RATIONAL_B_SPLINE_SURFACE(((0.99297255681857,0.988973049555656,0.987877375613931),
(0.99297255681857,0.988973049555656,0.987877375613931)))
REPRESENTATION_ITEM('')
SURFACE()
);
#1293=(
BOUNDED_SURFACE()
B_SPLINE_SURFACE(1,2,((#115459,#115460,#115461,#115462,#115463),(#115464,
#115465,#115466,#115467,#115468)),.UNSPECIFIED.,.F.,.F.,.F.)
B_SPLINE_SURFACE_WITH_KNOTS((2,2),(3,2,3),(0.71019295900798,1.),(0.418312080773434,
0.428571428571429,0.435879799328079),.UNSPECIFIED.)
GEOMETRIC_REPRESENTATION_ITEM()
RATIONAL_B_SPLINE_SURFACE(((0.99383221411677,0.996398874234721,1.,0.997434694412141,
0.995394338545806),(0.99383221411677,0.996398874234721,1.,0.997434694412141,
0.995394338545806)))
REPRESENTATION_ITEM('')
SURFACE()
);
#1294=(
BOUNDED_SURFACE()
B_SPLINE_SURFACE(1,2,((#115483,#115484,#115485),(#115486,#115487,#115488)),
 .UNSPECIFIED.,.F.,.F.,.F.)
B_SPLINE_SURFACE_WITH_KNOTS((2,2),(3,3),(0.710318915639618,1.),(0.297753987024626,
0.314942866188516),.UNSPECIFIED.)
GEOMETRIC_REPRESENTATION_ITEM()
RATIONAL_B_SPLINE_SURFACE(((0.992972556818502,0.988973049555647,0.987877375613931),
(0.992972556818502,0.988973049555647,0.987877375613931)))
REPRESENTATION_ITEM('')
SURFACE()
);
#1295=(
BOUNDED_SURFACE()
B_SPLINE_SURFACE(1,2,((#115490,#115491,#115492,#115493,#115494),(#115495,
#115496,#115497,#115498,#115499)),.UNSPECIFIED.,.F.,.F.,.F.)
B_SPLINE_SURFACE_WITH_KNOTS((2,2),(3,2,3),(0.710192959008018,1.),(0.418312080773434,
0.428571428571429,0.435879799328077),.UNSPECIFIED.)
GEOMETRIC_REPRESENTATION_ITEM()
RATIONAL_B_SPLINE_SURFACE(((0.99383221411677,0.996398874234721,1.,0.997434694412141,
0.995394338545807),(0.99383221411677,0.996398874234721,1.,0.997434694412141,
0.995394338545807)))
REPRESENTATION_ITEM('')
SURFACE()
);
#1296=(
BOUNDED_SURFACE()
B_SPLINE_SURFACE(1,2,((#115507,#115508,#115509,#115510,#115511),(#115512,
#115513,#115514,#115515,#115516)),.UNSPECIFIED.,.F.,.F.,.F.)
B_SPLINE_SURFACE_WITH_KNOTS((2,2),(3,2,3),(0.,0.28980704099156),(0.469846324360764,
0.470019760166365,0.487363340726489),.UNSPECIFIED.)
GEOMETRIC_REPRESENTATION_ITEM()
RATIONAL_B_SPLINE_SURFACE(((0.987787102172814,0.987787102172814,0.987787102172814,
0.988764511531024,0.992698258926487),(0.987787102172814,0.987787102172814,
0.987787102172814,0.988764511531024,0.992698258926487)))
REPRESENTATION_ITEM('')
SURFACE()
);
#1297=(
BOUNDED_SURFACE()
B_SPLINE_SURFACE(1,2,((#115525,#115526,#115527),(#115528,#115529,#115530)),
 .UNSPECIFIED.,.F.,.F.,.F.)
B_SPLINE_SURFACE_WITH_KNOTS((2,2),(3,3),(0.,0.289681084359914),(0.245851183393691,
0.263098999273814),.UNSPECIFIED.)
GEOMETRIC_REPRESENTATION_ITEM()
RATIONAL_B_SPLINE_SURFACE(((0.987633126750593,0.986929835989061,0.989150325841658),
(0.987633126750593,0.986929835989061,0.989150325841658)))
REPRESENTATION_ITEM('')
SURFACE()
);
#1298=(
BOUNDED_SURFACE()
B_SPLINE_SURFACE(1,2,((#115539,#115540,#115541,#115542,#115543),(#115544,
#115545,#115546,#115547,#115548)),.UNSPECIFIED.,.F.,.F.,.F.)
B_SPLINE_SURFACE_WITH_KNOTS((2,2),(3,2,3),(0.,0.289807040991555),(0.469846324360765,
0.470019760166366,0.487363340726489),.UNSPECIFIED.)
GEOMETRIC_REPRESENTATION_ITEM()
RATIONAL_B_SPLINE_SURFACE(((0.987787102172814,0.987787102172814,0.987787102172814,
0.988764511531023,0.992698258926487),(0.987787102172814,0.987787102172814,
0.987787102172814,0.988764511531023,0.992698258926487)))
REPRESENTATION_ITEM('')
SURFACE()
);
#1299=(
BOUNDED_SURFACE()
B_SPLINE_SURFACE(1,2,((#115550,#115551,#115552),(#115553,#115554,#115555)),
 .UNSPECIFIED.,.F.,.F.,.F.)
B_SPLINE_SURFACE_WITH_KNOTS((2,2),(3,3),(0.,0.289681084359923),(0.245851183393691,
0.263098999273798),.UNSPECIFIED.)
GEOMETRIC_REPRESENTATION_ITEM()
RATIONAL_B_SPLINE_SURFACE(((0.987633126750593,0.986929835989062,0.989150325841653),
(0.987633126750593,0.986929835989062,0.989150325841653)))
REPRESENTATION_ITEM('')
SURFACE()
);
#1300=(
BOUNDED_SURFACE()
B_SPLINE_SURFACE(1,2,((#115564,#115565,#115566,#115567,#115568),(#115569,
#115570,#115571,#115572,#115573)),.UNSPECIFIED.,.F.,.F.,.F.)
B_SPLINE_SURFACE_WITH_KNOTS((2,2),(3,2,3),(0.,0.289807040991561),(0.469846324360764,
0.470019760166365,0.487363340726489),.UNSPECIFIED.)
GEOMETRIC_REPRESENTATION_ITEM()
RATIONAL_B_SPLINE_SURFACE(((0.987787102172814,0.987787102172814,0.987787102172814,
0.988764511531024,0.992698258926487),(0.987787102172814,0.987787102172814,
0.987787102172814,0.988764511531024,0.992698258926487)))
REPRESENTATION_ITEM('')
SURFACE()
);
#1301=(
BOUNDED_SURFACE()
B_SPLINE_SURFACE(1,2,((#115575,#115576,#115577),(#115578,#115579,#115580)),
 .UNSPECIFIED.,.F.,.F.,.F.)
B_SPLINE_SURFACE_WITH_KNOTS((2,2),(3,3),(0.,0.289681084359918),(0.245851183393691,
0.263098999273798),.UNSPECIFIED.)
GEOMETRIC_REPRESENTATION_ITEM()
RATIONAL_B_SPLINE_SURFACE(((0.987633126750594,0.986929835989062,0.989150325841653),
(0.987633126750594,0.986929835989062,0.989150325841653)))
REPRESENTATION_ITEM('')
SURFACE()
);
#1302=(
BOUNDED_SURFACE()
B_SPLINE_SURFACE(1,2,((#115589,#115590,#115591,#115592,#115593),(#115594,
#115595,#115596,#115597,#115598)),.UNSPECIFIED.,.F.,.F.,.F.)
B_SPLINE_SURFACE_WITH_KNOTS((2,2),(3,2,3),(0.,0.290404426476257),(0.469422374491981,
0.470019760166365,0.487363340726489),.UNSPECIFIED.)
GEOMETRIC_REPRESENTATION_ITEM()
RATIONAL_B_SPLINE_SURFACE(((0.987787102172814,0.987787102172814,0.987787102172814,
0.988764511531023,0.992698258926487),(0.987787102172814,0.987787102172814,
0.987787102172814,0.988764511531023,0.992698258926487)))
REPRESENTATION_ITEM('')
SURFACE()
);
#1303=(
BOUNDED_SURFACE()
B_SPLINE_SURFACE(1,2,((#115600,#115601,#115602),(#115603,#115604,#115605)),
 .UNSPECIFIED.,.F.,.F.,.F.)
B_SPLINE_SURFACE_WITH_KNOTS((2,2),(3,3),(0.,0.289681084359921),(0.245851183393691,
0.263098999273798),.UNSPECIFIED.)
GEOMETRIC_REPRESENTATION_ITEM()
RATIONAL_B_SPLINE_SURFACE(((0.987633126750593,0.986929835989062,0.989150325841653),
(0.987633126750593,0.986929835989062,0.989150325841653)))
REPRESENTATION_ITEM('')
SURFACE()
);
#1304=(
BOUNDED_SURFACE()
B_SPLINE_SURFACE(1,2,((#115614,#115615,#115616,#115617,#115618),(#115619,
#115620,#115621,#115622,#115623)),.UNSPECIFIED.,.F.,.F.,.F.)
B_SPLINE_SURFACE_WITH_KNOTS((2,2),(3,2,3),(0.,0.290404426466868),(0.469422374491797,
0.470019760166365,0.487363340726489),.UNSPECIFIED.)
GEOMETRIC_REPRESENTATION_ITEM()
RATIONAL_B_SPLINE_SURFACE(((0.987787102172814,0.987787102172814,0.987787102172814,
0.988764511531023,0.992698258926487),(0.987787102172814,0.987787102172814,
0.987787102172814,0.988764511531023,0.992698258926487)))
REPRESENTATION_ITEM('')
SURFACE()
);
#1305=(
BOUNDED_SURFACE()
B_SPLINE_SURFACE(1,2,((#115625,#115626,#115627),(#115628,#115629,#115630)),
 .UNSPECIFIED.,.F.,.F.,.F.)
B_SPLINE_SURFACE_WITH_KNOTS((2,2),(3,3),(0.,0.289681084359923),(0.245851183393691,
0.263098999273798),.UNSPECIFIED.)
GEOMETRIC_REPRESENTATION_ITEM()
RATIONAL_B_SPLINE_SURFACE(((0.987633126750594,0.986929835989062,0.989150325841653),
(0.987633126750594,0.986929835989062,0.989150325841653)))
REPRESENTATION_ITEM('')
SURFACE()
);
#1306=(
BOUNDED_SURFACE()
B_SPLINE_SURFACE(1,2,((#115639,#115640,#115641,#115642,#115643),(#115644,
#115645,#115646,#115647,#115648)),.UNSPECIFIED.,.F.,.F.,.F.)
B_SPLINE_SURFACE_WITH_KNOTS((2,2),(3,2,3),(0.,0.290404426468995),(0.469422374490255,
0.470019760166365,0.487363340726489),.UNSPECIFIED.)
GEOMETRIC_REPRESENTATION_ITEM()
RATIONAL_B_SPLINE_SURFACE(((0.987787102172814,0.987787102172814,0.987787102172814,
0.988764511531023,0.992698258926487),(0.987787102172814,0.987787102172814,
0.987787102172814,0.988764511531023,0.992698258926487)))
REPRESENTATION_ITEM('')
SURFACE()
);
#1307=(
BOUNDED_SURFACE()
B_SPLINE_SURFACE(1,2,((#115650,#115651,#115652),(#115653,#115654,#115655)),
 .UNSPECIFIED.,.F.,.F.,.F.)
B_SPLINE_SURFACE_WITH_KNOTS((2,2),(3,3),(0.,0.289681084359914),(0.245851183393691,
0.263098999273798),.UNSPECIFIED.)
GEOMETRIC_REPRESENTATION_ITEM()
RATIONAL_B_SPLINE_SURFACE(((0.987633126750593,0.986929835989062,0.989150325841653),
(0.987633126750593,0.986929835989062,0.989150325841653)))
REPRESENTATION_ITEM('')
SURFACE()
);
#1308=(
BOUNDED_SURFACE()
B_SPLINE_SURFACE(1,2,((#115664,#115665,#115666,#115667,#115668),(#115669,
#115670,#115671,#115672,#115673)),.UNSPECIFIED.,.F.,.F.,.F.)
B_SPLINE_SURFACE_WITH_KNOTS((2,2),(3,2,3),(0.,0.290404426439913),(0.469422374518831,
0.470019760166367,0.487363340726489),.UNSPECIFIED.)
GEOMETRIC_REPRESENTATION_ITEM()
RATIONAL_B_SPLINE_SURFACE(((0.987787102172814,0.987787102172814,0.987787102172814,
0.988764511531024,0.992698258926487),(0.987787102172814,0.987787102172814,
0.987787102172814,0.988764511531024,0.992698258926487)))
REPRESENTATION_ITEM('')
SURFACE()
);
#1309=(
BOUNDED_SURFACE()
B_SPLINE_SURFACE(1,2,((#115675,#115676,#115677),(#115678,#115679,#115680)),
 .UNSPECIFIED.,.F.,.F.,.F.)
B_SPLINE_SURFACE_WITH_KNOTS((2,2),(3,3),(0.,0.289681084359922),(0.24585118339369,
0.263098999273797),.UNSPECIFIED.)
GEOMETRIC_REPRESENTATION_ITEM()
RATIONAL_B_SPLINE_SURFACE(((0.987633126750593,0.986929835989062,0.989150325841653),
(0.987633126750593,0.986929835989062,0.989150325841653)))
REPRESENTATION_ITEM('')
SURFACE()
);
#1310=(
BOUNDED_SURFACE()
B_SPLINE_SURFACE(1,2,((#115689,#115690,#115691,#115692,#115693),(#115694,
#115695,#115696,#115697,#115698)),.UNSPECIFIED.,.F.,.F.,.F.)
B_SPLINE_SURFACE_WITH_KNOTS((2,2),(3,2,3),(0.,0.289807040991635),(0.469846324360766,
0.470019760166367,0.48736334072649),.UNSPECIFIED.)
GEOMETRIC_REPRESENTATION_ITEM()
RATIONAL_B_SPLINE_SURFACE(((0.987787102172814,0.987787102172814,0.987787102172814,
0.988764511531024,0.992698258926488),(0.987787102172814,0.987787102172814,
0.987787102172814,0.988764511531024,0.992698258926488)))
REPRESENTATION_ITEM('')
SURFACE()
);
#1311=(
BOUNDED_SURFACE()
B_SPLINE_SURFACE(1,2,((#115700,#115701,#115702),(#115703,#115704,#115705)),
 .UNSPECIFIED.,.F.,.F.,.F.)
B_SPLINE_SURFACE_WITH_KNOTS((2,2),(3,3),(0.,0.289681084359916),(0.24585118339369,
0.263098999273797),.UNSPECIFIED.)
GEOMETRIC_REPRESENTATION_ITEM()
RATIONAL_B_SPLINE_SURFACE(((0.987633126750594,0.986929835989062,0.989150325841653),
(0.987633126750594,0.986929835989062,0.989150325841653)))
REPRESENTATION_ITEM('')
SURFACE()
);
#1312=(
BOUNDED_SURFACE()
B_SPLINE_SURFACE(1,2,((#115714,#115715,#115716,#115717,#115718),(#115719,
#115720,#115721,#115722,#115723)),.UNSPECIFIED.,.F.,.F.,.F.)
B_SPLINE_SURFACE_WITH_KNOTS((2,2),(3,2,3),(0.,0.289807040992233),(0.469846324360766,
0.470019760166367,0.48736334072649),.UNSPECIFIED.)
GEOMETRIC_REPRESENTATION_ITEM()
RATIONAL_B_SPLINE_SURFACE(((0.987787102172814,0.987787102172814,0.987787102172814,
0.988764511531024,0.992698258926488),(0.987787102172814,0.987787102172814,
0.987787102172814,0.988764511531024,0.992698258926488)))
REPRESENTATION_ITEM('')
SURFACE()
);
#1313=(
BOUNDED_SURFACE()
B_SPLINE_SURFACE(1,2,((#115725,#115726,#115727),(#115728,#115729,#115730)),
 .UNSPECIFIED.,.F.,.F.,.F.)
B_SPLINE_SURFACE_WITH_KNOTS((2,2),(3,3),(0.,0.289681084359921),(0.24585118339369,
0.263098999273797),.UNSPECIFIED.)
GEOMETRIC_REPRESENTATION_ITEM()
RATIONAL_B_SPLINE_SURFACE(((0.987633126750594,0.986929835989062,0.989150325841653),
(0.987633126750594,0.986929835989062,0.989150325841653)))
REPRESENTATION_ITEM('')
SURFACE()
);
#1314=(
BOUNDED_SURFACE()
B_SPLINE_SURFACE(1,2,((#115739,#115740,#115741,#115742,#115743),(#115744,
#115745,#115746,#115747,#115748)),.UNSPECIFIED.,.F.,.F.,.F.)
B_SPLINE_SURFACE_WITH_KNOTS((2,2),(3,2,3),(0.,0.289807040991645),(0.469846324360766,
0.470019760166367,0.48736334072649),.UNSPECIFIED.)
GEOMETRIC_REPRESENTATION_ITEM()
RATIONAL_B_SPLINE_SURFACE(((0.987787102172814,0.987787102172814,0.987787102172814,
0.988764511531024,0.992698258926488),(0.987787102172814,0.987787102172814,
0.987787102172814,0.988764511531024,0.992698258926488)))
REPRESENTATION_ITEM('')
SURFACE()
);
#1315=(
BOUNDED_SURFACE()
B_SPLINE_SURFACE(1,2,((#115750,#115751,#115752),(#115753,#115754,#115755)),
 .UNSPECIFIED.,.F.,.F.,.F.)
B_SPLINE_SURFACE_WITH_KNOTS((2,2),(3,3),(0.,0.28968108435992),(0.24585118339369,
0.263098999273797),.UNSPECIFIED.)
GEOMETRIC_REPRESENTATION_ITEM()
RATIONAL_B_SPLINE_SURFACE(((0.987633126750594,0.986929835989062,0.989150325841653),
(0.987633126750594,0.986929835989062,0.989150325841653)))
REPRESENTATION_ITEM('')
SURFACE()
);
#1316=(
BOUNDED_SURFACE()
B_SPLINE_SURFACE(1,2,((#115764,#115765,#115766,#115767,#115768),(#115769,
#115770,#115771,#115772,#115773)),.UNSPECIFIED.,.F.,.F.,.F.)
B_SPLINE_SURFACE_WITH_KNOTS((2,2),(3,2,3),(0.,0.289807040992142),(0.469846324360766,
0.470019760166367,0.48736334072649),.UNSPECIFIED.)
GEOMETRIC_REPRESENTATION_ITEM()
RATIONAL_B_SPLINE_SURFACE(((0.987787102172814,0.987787102172814,0.987787102172814,
0.988764511531024,0.992698258926488),(0.987787102172814,0.987787102172814,
0.987787102172814,0.988764511531024,0.992698258926488)))
REPRESENTATION_ITEM('')
SURFACE()
);
#1317=(
BOUNDED_SURFACE()
B_SPLINE_SURFACE(1,2,((#115775,#115776,#115777),(#115778,#115779,#115780)),
 .UNSPECIFIED.,.F.,.F.,.F.)
B_SPLINE_SURFACE_WITH_KNOTS((2,2),(3,3),(0.,0.28968108435992),(0.24585118339369,
0.263098999273797),.UNSPECIFIED.)
GEOMETRIC_REPRESENTATION_ITEM()
RATIONAL_B_SPLINE_SURFACE(((0.987633126750594,0.986929835989062,0.989150325841653),
(0.987633126750594,0.986929835989062,0.989150325841653)))
REPRESENTATION_ITEM('')
SURFACE()
);
#1318=(
BOUNDED_SURFACE()
B_SPLINE_SURFACE(1,2,((#115789,#115790,#115791,#115792,#115793),(#115794,
#115795,#115796,#115797,#115798)),.UNSPECIFIED.,.F.,.F.,.F.)
B_SPLINE_SURFACE_WITH_KNOTS((2,2),(3,2,3),(0.,0.290404426498244),(0.469422374469413,
0.470019760166367,0.48736334072649),.UNSPECIFIED.)
GEOMETRIC_REPRESENTATION_ITEM()
RATIONAL_B_SPLINE_SURFACE(((0.987787102172814,0.987787102172814,0.987787102172814,
0.988764511531024,0.992698258926488),(0.987787102172814,0.987787102172814,
0.987787102172814,0.988764511531024,0.992698258926488)))
REPRESENTATION_ITEM('')
SURFACE()
);
#1319=(
BOUNDED_SURFACE()
B_SPLINE_SURFACE(1,2,((#115800,#115801,#115802),(#115803,#115804,#115805)),
 .UNSPECIFIED.,.F.,.F.,.F.)
B_SPLINE_SURFACE_WITH_KNOTS((2,2),(3,3),(0.,0.289681084359923),(0.24585118339369,
0.263098999273797),.UNSPECIFIED.)
GEOMETRIC_REPRESENTATION_ITEM()
RATIONAL_B_SPLINE_SURFACE(((0.987633126750594,0.986929835989062,0.989150325841653),
(0.987633126750594,0.986929835989062,0.989150325841653)))
REPRESENTATION_ITEM('')
SURFACE()
);
#1320=(
BOUNDED_SURFACE()
B_SPLINE_SURFACE(1,2,((#115814,#115815,#115816,#115817,#115818),(#115819,
#115820,#115821,#115822,#115823)),.UNSPECIFIED.,.F.,.F.,.F.)
B_SPLINE_SURFACE_WITH_KNOTS((2,2),(3,2,3),(0.,0.290404426464598),(0.469422374503515,
0.470019760166367,0.48736334072649),.UNSPECIFIED.)
GEOMETRIC_REPRESENTATION_ITEM()
RATIONAL_B_SPLINE_SURFACE(((0.987787102172814,0.987787102172814,0.987787102172814,
0.988764511531024,0.992698258926488),(0.987787102172814,0.987787102172814,
0.987787102172814,0.988764511531024,0.992698258926488)))
REPRESENTATION_ITEM('')
SURFACE()
);
#1321=(
BOUNDED_SURFACE()
B_SPLINE_SURFACE(1,2,((#115825,#115826,#115827),(#115828,#115829,#115830)),
 .UNSPECIFIED.,.F.,.F.,.F.)
B_SPLINE_SURFACE_WITH_KNOTS((2,2),(3,3),(0.,0.289681084359922),(0.24585118339369,
0.263098999273797),.UNSPECIFIED.)
GEOMETRIC_REPRESENTATION_ITEM()
RATIONAL_B_SPLINE_SURFACE(((0.987633126750594,0.986929835989062,0.989150325841653),
(0.987633126750594,0.986929835989062,0.989150325841653)))
REPRESENTATION_ITEM('')
SURFACE()
);
#1322=(
BOUNDED_SURFACE()
B_SPLINE_SURFACE(1,2,((#115839,#115840,#115841,#115842,#115843),(#115844,
#115845,#115846,#115847,#115848)),.UNSPECIFIED.,.F.,.F.,.F.)
B_SPLINE_SURFACE_WITH_KNOTS((2,2),(3,2,3),(0.,0.290404426443499),(0.469422374515526,
0.470019760166367,0.48736334072649),.UNSPECIFIED.)
GEOMETRIC_REPRESENTATION_ITEM()
RATIONAL_B_SPLINE_SURFACE(((0.987787102172814,0.987787102172814,0.987787102172814,
0.988764511531024,0.992698258926488),(0.987787102172814,0.987787102172814,
0.987787102172814,0.988764511531024,0.992698258926488)))
REPRESENTATION_ITEM('')
SURFACE()
);
#1323=(
BOUNDED_SURFACE()
B_SPLINE_SURFACE(1,2,((#115850,#115851,#115852),(#115853,#115854,#115855)),
 .UNSPECIFIED.,.F.,.F.,.F.)
B_SPLINE_SURFACE_WITH_KNOTS((2,2),(3,3),(0.,0.289681084359924),(0.24585118339369,
0.263098999273797),.UNSPECIFIED.)
GEOMETRIC_REPRESENTATION_ITEM()
RATIONAL_B_SPLINE_SURFACE(((0.987633126750593,0.986929835989062,0.989150325841653),
(0.987633126750593,0.986929835989062,0.989150325841653)))
REPRESENTATION_ITEM('')
SURFACE()
);
#1324=(
BOUNDED_SURFACE()
B_SPLINE_SURFACE(1,2,((#115864,#115865,#115866,#115867,#115868),(#115869,
#115870,#115871,#115872,#115873)),.UNSPECIFIED.,.F.,.F.,.F.)
B_SPLINE_SURFACE_WITH_KNOTS((2,2),(3,2,3),(0.,0.289807040992967),(0.469846324360766,
0.470019760166367,0.48736334072649),.UNSPECIFIED.)
GEOMETRIC_REPRESENTATION_ITEM()
RATIONAL_B_SPLINE_SURFACE(((0.987787102172814,0.987787102172814,0.987787102172814,
0.988764511531024,0.992698258926488),(0.987787102172814,0.987787102172814,
0.987787102172814,0.988764511531024,0.992698258926488)))
REPRESENTATION_ITEM('')
SURFACE()
);
#1325=(
BOUNDED_SURFACE()
B_SPLINE_SURFACE(1,2,((#115875,#115876,#115877),(#115878,#115879,#115880)),
 .UNSPECIFIED.,.F.,.F.,.F.)
B_SPLINE_SURFACE_WITH_KNOTS((2,2),(3,3),(0.,0.289681084359922),(0.24585118339369,
0.263098999273797),.UNSPECIFIED.)
GEOMETRIC_REPRESENTATION_ITEM()
RATIONAL_B_SPLINE_SURFACE(((0.987633126750594,0.986929835989062,0.989150325841653),
(0.987633126750594,0.986929835989062,0.989150325841653)))
REPRESENTATION_ITEM('')
SURFACE()
);
#1326=(
BOUNDED_SURFACE()
B_SPLINE_SURFACE(1,2,((#115889,#115890,#115891,#115892,#115893),(#115894,
#115895,#115896,#115897,#115898)),.UNSPECIFIED.,.F.,.F.,.F.)
B_SPLINE_SURFACE_WITH_KNOTS((2,2),(3,2,3),(0.,0.289807040991681),(0.469846324360766,
0.470019760166367,0.48736334072649),.UNSPECIFIED.)
GEOMETRIC_REPRESENTATION_ITEM()
RATIONAL_B_SPLINE_SURFACE(((0.987787102172814,0.987787102172814,0.987787102172814,
0.988764511531024,0.992698258926488),(0.987787102172814,0.987787102172814,
0.987787102172814,0.988764511531024,0.992698258926488)))
REPRESENTATION_ITEM('')
SURFACE()
);
#1327=(
BOUNDED_SURFACE()
B_SPLINE_SURFACE(1,2,((#115900,#115901,#115902),(#115903,#115904,#115905)),
 .UNSPECIFIED.,.F.,.F.,.F.)
B_SPLINE_SURFACE_WITH_KNOTS((2,2),(3,3),(0.,0.289681084359928),(0.24585118339369,
0.263098999273797),.UNSPECIFIED.)
GEOMETRIC_REPRESENTATION_ITEM()
RATIONAL_B_SPLINE_SURFACE(((0.987633126750594,0.986929835989062,0.989150325841653),
(0.987633126750594,0.986929835989062,0.989150325841653)))
REPRESENTATION_ITEM('')
SURFACE()
);
#1328=(
BOUNDED_SURFACE()
B_SPLINE_SURFACE(1,2,((#115914,#115915,#115916,#115917,#115918),(#115919,
#115920,#115921,#115922,#115923)),.UNSPECIFIED.,.F.,.F.,.F.)
B_SPLINE_SURFACE_WITH_KNOTS((2,2),(3,2,3),(0.,0.289807040991564),(0.469846324360766,
0.470019760166367,0.48736334072649),.UNSPECIFIED.)
GEOMETRIC_REPRESENTATION_ITEM()
RATIONAL_B_SPLINE_SURFACE(((0.987787102172814,0.987787102172814,0.987787102172814,
0.988764511531024,0.992698258926488),(0.987787102172814,0.987787102172814,
0.987787102172814,0.988764511531024,0.992698258926488)))
REPRESENTATION_ITEM('')
SURFACE()
);
#1329=(
BOUNDED_SURFACE()
B_SPLINE_SURFACE(1,2,((#115925,#115926,#115927),(#115928,#115929,#115930)),
 .UNSPECIFIED.,.F.,.F.,.F.)
B_SPLINE_SURFACE_WITH_KNOTS((2,2),(3,3),(0.,0.289681084359921),(0.24585118339369,
0.263098999273796),.UNSPECIFIED.)
GEOMETRIC_REPRESENTATION_ITEM()
RATIONAL_B_SPLINE_SURFACE(((0.987633126750594,0.986929835989062,0.989150325841653),
(0.987633126750594,0.986929835989062,0.989150325841653)))
REPRESENTATION_ITEM('')
SURFACE()
);
#1330=(
BOUNDED_SURFACE()
B_SPLINE_SURFACE(1,2,((#115939,#115940,#115941,#115942,#115943),(#115944,
#115945,#115946,#115947,#115948)),.UNSPECIFIED.,.F.,.F.,.F.)
B_SPLINE_SURFACE_WITH_KNOTS((2,2),(3,2,3),(0.,0.289807040992195),(0.469846324360765,
0.470019760166366,0.48736334072649),.UNSPECIFIED.)
GEOMETRIC_REPRESENTATION_ITEM()
RATIONAL_B_SPLINE_SURFACE(((0.987787102172814,0.987787102172814,0.987787102172814,
0.988764511531024,0.992698258926488),(0.987787102172814,0.987787102172814,
0.987787102172814,0.988764511531024,0.992698258926488)))
REPRESENTATION_ITEM('')
SURFACE()
);
#1331=(
BOUNDED_SURFACE()
B_SPLINE_SURFACE(1,2,((#115950,#115951,#115952),(#115953,#115954,#115955)),
 .UNSPECIFIED.,.F.,.F.,.F.)
B_SPLINE_SURFACE_WITH_KNOTS((2,2),(3,3),(0.,0.289681084359926),(0.24585118339369,
0.263098999273796),.UNSPECIFIED.)
GEOMETRIC_REPRESENTATION_ITEM()
RATIONAL_B_SPLINE_SURFACE(((0.987633126750594,0.986929835989062,0.989150325841653),
(0.987633126750594,0.986929835989062,0.989150325841653)))
REPRESENTATION_ITEM('')
SURFACE()
);
#1332=(
BOUNDED_SURFACE()
B_SPLINE_SURFACE(1,2,((#115964,#115965,#115966,#115967,#115968),(#115969,
#115970,#115971,#115972,#115973)),.UNSPECIFIED.,.F.,.F.,.F.)
B_SPLINE_SURFACE_WITH_KNOTS((2,2),(3,2,3),(0.,0.290404426475224),(0.469422374492427,
0.470019760166367,0.48736334072649),.UNSPECIFIED.)
GEOMETRIC_REPRESENTATION_ITEM()
RATIONAL_B_SPLINE_SURFACE(((0.987787102172814,0.987787102172814,0.987787102172814,
0.988764511531024,0.992698258926488),(0.987787102172814,0.987787102172814,
0.987787102172814,0.988764511531024,0.992698258926488)))
REPRESENTATION_ITEM('')
SURFACE()
);
#1333=(
BOUNDED_SURFACE()
B_SPLINE_SURFACE(1,2,((#115975,#115976,#115977),(#115978,#115979,#115980)),
 .UNSPECIFIED.,.F.,.F.,.F.)
B_SPLINE_SURFACE_WITH_KNOTS((2,2),(3,3),(0.,0.289681084359927),(0.24585118339369,
0.263098999273796),.UNSPECIFIED.)
GEOMETRIC_REPRESENTATION_ITEM()
RATIONAL_B_SPLINE_SURFACE(((0.987633126750594,0.986929835989062,0.989150325841653),
(0.987633126750594,0.986929835989062,0.989150325841653)))
REPRESENTATION_ITEM('')
SURFACE()
);
#1334=(
BOUNDED_SURFACE()
B_SPLINE_SURFACE(1,2,((#115989,#115990,#115991,#115992,#115993),(#115994,
#115995,#115996,#115997,#115998)),.UNSPECIFIED.,.F.,.F.,.F.)
B_SPLINE_SURFACE_WITH_KNOTS((2,2),(3,2,3),(0.,0.290404426435714),(0.469422374524091,
0.470019760166367,0.48736334072649),.UNSPECIFIED.)
GEOMETRIC_REPRESENTATION_ITEM()
RATIONAL_B_SPLINE_SURFACE(((0.987787102172814,0.987787102172814,0.987787102172814,
0.988764511531024,0.992698258926488),(0.987787102172814,0.987787102172814,
0.987787102172814,0.988764511531024,0.992698258926488)))
REPRESENTATION_ITEM('')
SURFACE()
);
#1335=(
BOUNDED_SURFACE()
B_SPLINE_SURFACE(1,2,((#116000,#116001,#116002),(#116003,#116004,#116005)),
 .UNSPECIFIED.,.F.,.F.,.F.)
B_SPLINE_SURFACE_WITH_KNOTS((2,2),(3,3),(0.,0.289681084359928),(0.24585118339369,
0.263098999273796),.UNSPECIFIED.)
GEOMETRIC_REPRESENTATION_ITEM()
RATIONAL_B_SPLINE_SURFACE(((0.987633126750594,0.986929835989062,0.989150325841653),
(0.987633126750594,0.986929835989062,0.989150325841653)))
REPRESENTATION_ITEM('')
SURFACE()
);
#1336=(
BOUNDED_SURFACE()
B_SPLINE_SURFACE(1,2,((#116014,#116015,#116016,#116017,#116018),(#116019,
#116020,#116021,#116022,#116023)),.UNSPECIFIED.,.F.,.F.,.F.)
B_SPLINE_SURFACE_WITH_KNOTS((2,2),(3,2,3),(0.,0.290404426476923),(0.469422374491519,
0.470019760166367,0.48736334072649),.UNSPECIFIED.)
GEOMETRIC_REPRESENTATION_ITEM()
RATIONAL_B_SPLINE_SURFACE(((0.987787102172814,0.987787102172814,0.987787102172814,
0.988764511531024,0.992698258926488),(0.987787102172814,0.987787102172814,
0.987787102172814,0.988764511531024,0.992698258926488)))
REPRESENTATION_ITEM('')
SURFACE()
);
#1337=(
BOUNDED_SURFACE()
B_SPLINE_SURFACE(1,2,((#116025,#116026,#116027),(#116028,#116029,#116030)),
 .UNSPECIFIED.,.F.,.F.,.F.)
B_SPLINE_SURFACE_WITH_KNOTS((2,2),(3,3),(0.,0.289681084359926),(0.24585118339369,
0.263098999273796),.UNSPECIFIED.)
GEOMETRIC_REPRESENTATION_ITEM()
RATIONAL_B_SPLINE_SURFACE(((0.987633126750594,0.986929835989062,0.989150325841653),
(0.987633126750594,0.986929835989062,0.989150325841653)))
REPRESENTATION_ITEM('')
SURFACE()
);
#1338=(
BOUNDED_SURFACE()
B_SPLINE_SURFACE(1,2,((#116039,#116040,#116041,#116042,#116043),(#116044,
#116045,#116046,#116047,#116048)),.UNSPECIFIED.,.F.,.F.,.F.)
B_SPLINE_SURFACE_WITH_KNOTS((2,2),(3,2,3),(0.,0.290404426447106),(0.469422374522161,
0.470019760166367,0.48736334072649),.UNSPECIFIED.)
GEOMETRIC_REPRESENTATION_ITEM()
RATIONAL_B_SPLINE_SURFACE(((0.987787102172814,0.987787102172814,0.987787102172814,
0.988764511531024,0.992698258926488),(0.987787102172814,0.987787102172814,
0.987787102172814,0.988764511531024,0.992698258926488)))
REPRESENTATION_ITEM('')
SURFACE()
);
#1339=(
BOUNDED_SURFACE()
B_SPLINE_SURFACE(1,2,((#116050,#116051,#116052),(#116053,#116054,#116055)),
 .UNSPECIFIED.,.F.,.F.,.F.)
B_SPLINE_SURFACE_WITH_KNOTS((2,2),(3,3),(0.,0.28968108435992),(0.24585118339369,
0.263098999273796),.UNSPECIFIED.)
GEOMETRIC_REPRESENTATION_ITEM()
RATIONAL_B_SPLINE_SURFACE(((0.987633126750594,0.986929835989062,0.989150325841653),
(0.987633126750594,0.986929835989062,0.989150325841653)))
REPRESENTATION_ITEM('')
SURFACE()
);
#1340=(
BOUNDED_SURFACE()
B_SPLINE_SURFACE(1,2,((#116064,#116065,#116066,#116067,#116068),(#116069,
#116070,#116071,#116072,#116073)),.UNSPECIFIED.,.F.,.F.,.F.)
B_SPLINE_SURFACE_WITH_KNOTS((2,2),(3,2,3),(0.,0.28980704099176),(0.469846324360766,
0.470019760166367,0.48736334072649),.UNSPECIFIED.)
GEOMETRIC_REPRESENTATION_ITEM()
RATIONAL_B_SPLINE_SURFACE(((0.987787102172814,0.987787102172814,0.987787102172814,
0.988764511531024,0.992698258926488),(0.987787102172814,0.987787102172814,
0.987787102172814,0.988764511531024,0.992698258926488)))
REPRESENTATION_ITEM('')
SURFACE()
);
#1341=(
BOUNDED_SURFACE()
B_SPLINE_SURFACE(1,2,((#116075,#116076,#116077),(#116078,#116079,#116080)),
 .UNSPECIFIED.,.F.,.F.,.F.)
B_SPLINE_SURFACE_WITH_KNOTS((2,2),(3,3),(0.,0.289681084359922),(0.24585118339369,
0.263098999273796),.UNSPECIFIED.)
GEOMETRIC_REPRESENTATION_ITEM()
RATIONAL_B_SPLINE_SURFACE(((0.987633126750594,0.986929835989062,0.989150325841653),
(0.987633126750594,0.986929835989062,0.989150325841653)))
REPRESENTATION_ITEM('')
SURFACE()
);
#1342=(
BOUNDED_SURFACE()
B_SPLINE_SURFACE(1,2,((#116089,#116090,#116091,#116092,#116093),(#116094,
#116095,#116096,#116097,#116098)),.UNSPECIFIED.,.F.,.F.,.F.)
B_SPLINE_SURFACE_WITH_KNOTS((2,2),(3,2,3),(0.,0.289807040993049),(0.469846324360766,
0.470019760166367,0.48736334072649),.UNSPECIFIED.)
GEOMETRIC_REPRESENTATION_ITEM()
RATIONAL_B_SPLINE_SURFACE(((0.987787102172814,0.987787102172814,0.987787102172814,
0.988764511531024,0.992698258926488),(0.987787102172814,0.987787102172814,
0.987787102172814,0.988764511531024,0.992698258926488)))
REPRESENTATION_ITEM('')
SURFACE()
);
#1343=(
BOUNDED_SURFACE()
B_SPLINE_SURFACE(1,2,((#116100,#116101,#116102),(#116103,#116104,#116105)),
 .UNSPECIFIED.,.F.,.F.,.F.)
B_SPLINE_SURFACE_WITH_KNOTS((2,2),(3,3),(0.,0.289681084359929),(0.24585118339369,
0.2630989992738),.UNSPECIFIED.)
GEOMETRIC_REPRESENTATION_ITEM()
RATIONAL_B_SPLINE_SURFACE(((0.987633126750594,0.986929835989062,0.989150325841654),
(0.987633126750594,0.986929835989062,0.989150325841654)))
REPRESENTATION_ITEM('')
SURFACE()
);
#1344=(
BOUNDED_SURFACE()
B_SPLINE_SURFACE(1,2,((#116114,#116115,#116116,#116117,#116118),(#116119,
#116120,#116121,#116122,#116123)),.UNSPECIFIED.,.F.,.F.,.F.)
B_SPLINE_SURFACE_WITH_KNOTS((2,2),(3,2,3),(0.,0.289807040992803),(0.469846324360765,
0.470019760166366,0.48736334072649),.UNSPECIFIED.)
GEOMETRIC_REPRESENTATION_ITEM()
RATIONAL_B_SPLINE_SURFACE(((0.987787102172814,0.987787102172814,0.987787102172814,
0.988764511531024,0.992698258926488),(0.987787102172814,0.987787102172814,
0.987787102172814,0.988764511531024,0.992698258926488)))
REPRESENTATION_ITEM('')
SURFACE()
);
#1345=(
BOUNDED_SURFACE()
B_SPLINE_SURFACE(1,2,((#116125,#116126,#116127),(#116128,#116129,#116130)),
 .UNSPECIFIED.,.F.,.F.,.F.)
B_SPLINE_SURFACE_WITH_KNOTS((2,2),(3,3),(0.,0.289681084359935),(0.24585118339369,
0.263098999273798),.UNSPECIFIED.)
GEOMETRIC_REPRESENTATION_ITEM()
RATIONAL_B_SPLINE_SURFACE(((0.987633126750594,0.986929835989062,0.989150325841653),
(0.987633126750594,0.986929835989062,0.989150325841653)))
REPRESENTATION_ITEM('')
SURFACE()
);
#1346=(
BOUNDED_SURFACE()
B_SPLINE_SURFACE(1,2,((#116139,#116140,#116141,#116142,#116143),(#116144,
#116145,#116146,#116147,#116148)),.UNSPECIFIED.,.F.,.F.,.F.)
B_SPLINE_SURFACE_WITH_KNOTS((2,2),(3,2,3),(0.,0.290404426453367),(0.469422374506297,
0.470019760166367,0.48736334072649),.UNSPECIFIED.)
GEOMETRIC_REPRESENTATION_ITEM()
RATIONAL_B_SPLINE_SURFACE(((0.987787102172814,0.987787102172814,0.987787102172814,
0.988764511531024,0.992698258926488),(0.987787102172814,0.987787102172814,
0.987787102172814,0.988764511531024,0.992698258926488)))
REPRESENTATION_ITEM('')
SURFACE()
);
#1347=(
BOUNDED_SURFACE()
B_SPLINE_SURFACE(1,2,((#116150,#116151,#116152),(#116153,#116154,#116155)),
 .UNSPECIFIED.,.F.,.F.,.F.)
B_SPLINE_SURFACE_WITH_KNOTS((2,2),(3,3),(0.,0.289681084359929),(0.24585118339369,
0.263098999273796),.UNSPECIFIED.)
GEOMETRIC_REPRESENTATION_ITEM()
RATIONAL_B_SPLINE_SURFACE(((0.987633126750594,0.986929835989062,0.989150325841653),
(0.987633126750594,0.986929835989062,0.989150325841653)))
REPRESENTATION_ITEM('')
SURFACE()
);
#1348=(
BOUNDED_SURFACE()
B_SPLINE_SURFACE(1,2,((#116164,#116165,#116166,#116167,#116168),(#116169,
#116170,#116171,#116172,#116173)),.UNSPECIFIED.,.F.,.F.,.F.)
B_SPLINE_SURFACE_WITH_KNOTS((2,2),(3,2,3),(0.,0.290404426459532),(0.46942237450006,
0.470019760166366,0.48736334072649),.UNSPECIFIED.)
GEOMETRIC_REPRESENTATION_ITEM()
RATIONAL_B_SPLINE_SURFACE(((0.987787102172814,0.987787102172814,0.987787102172814,
0.988764511531024,0.992698258926488),(0.987787102172814,0.987787102172814,
0.987787102172814,0.988764511531024,0.992698258926488)))
REPRESENTATION_ITEM('')
SURFACE()
);
#1349=(
BOUNDED_SURFACE()
B_SPLINE_SURFACE(1,2,((#116175,#116176,#116177),(#116178,#116179,#116180)),
 .UNSPECIFIED.,.F.,.F.,.F.)
B_SPLINE_SURFACE_WITH_KNOTS((2,2),(3,3),(0.,0.289681084359924),(0.24585118339369,
0.263098999273796),.UNSPECIFIED.)
GEOMETRIC_REPRESENTATION_ITEM()
RATIONAL_B_SPLINE_SURFACE(((0.987633126750594,0.986929835989062,0.989150325841653),
(0.987633126750594,0.986929835989062,0.989150325841653)))
REPRESENTATION_ITEM('')
SURFACE()
);
#1350=(
BOUNDED_SURFACE()
B_SPLINE_SURFACE(1,2,((#116189,#116190,#116191,#116192,#116193),(#116194,
#116195,#116196,#116197,#116198)),.UNSPECIFIED.,.F.,.F.,.F.)
B_SPLINE_SURFACE_WITH_KNOTS((2,2),(3,2,3),(0.,0.290404426466932),(0.469422374492982,
0.470019760166367,0.487363340726492),.UNSPECIFIED.)
GEOMETRIC_REPRESENTATION_ITEM()
RATIONAL_B_SPLINE_SURFACE(((0.987787102172814,0.987787102172814,0.987787102172814,
0.988764511531024,0.992698258926488),(0.987787102172814,0.987787102172814,
0.987787102172814,0.988764511531024,0.992698258926488)))
REPRESENTATION_ITEM('')
SURFACE()
);
#1351=(
BOUNDED_SURFACE()
B_SPLINE_SURFACE(1,2,((#116200,#116201,#116202),(#116203,#116204,#116205)),
 .UNSPECIFIED.,.F.,.F.,.F.)
B_SPLINE_SURFACE_WITH_KNOTS((2,2),(3,3),(0.,0.289681084359922),(0.245851183393682,
0.263098999273796),.UNSPECIFIED.)
GEOMETRIC_REPRESENTATION_ITEM()
RATIONAL_B_SPLINE_SURFACE(((0.987633126750594,0.986929835989061,0.989150325841653),
(0.987633126750594,0.986929835989061,0.989150325841653)))
REPRESENTATION_ITEM('')
SURFACE()
);
#1352=(
BOUNDED_SURFACE()
B_SPLINE_SURFACE(1,2,((#116214,#116215,#116216,#116217,#116218),(#116219,
#116220,#116221,#116222,#116223)),.UNSPECIFIED.,.F.,.F.,.F.)
B_SPLINE_SURFACE_WITH_KNOTS((2,2),(3,2,3),(0.,0.290404426475473),(0.469422374493052,
0.470019760166366,0.48736334072649),.UNSPECIFIED.)
GEOMETRIC_REPRESENTATION_ITEM()
RATIONAL_B_SPLINE_SURFACE(((0.987787102172814,0.987787102172814,0.987787102172814,
0.988764511531024,0.992698258926488),(0.987787102172814,0.987787102172814,
0.987787102172814,0.988764511531024,0.992698258926488)))
REPRESENTATION_ITEM('')
SURFACE()
);
#1353=(
BOUNDED_SURFACE()
B_SPLINE_SURFACE(1,2,((#116225,#116226,#116227),(#116228,#116229,#116230)),
 .UNSPECIFIED.,.F.,.F.,.F.)
B_SPLINE_SURFACE_WITH_KNOTS((2,2),(3,3),(0.,0.289681084359924),(0.245851183393691,
0.263098999273796),.UNSPECIFIED.)
GEOMETRIC_REPRESENTATION_ITEM()
RATIONAL_B_SPLINE_SURFACE(((0.987633126750594,0.986929835989062,0.989150325841653),
(0.987633126750594,0.986929835989062,0.989150325841653)))
REPRESENTATION_ITEM('')
SURFACE()
);
#1354=(
BOUNDED_SURFACE()
B_SPLINE_SURFACE(1,2,((#116232,#116233,#116234,#116235,#116236),(#116237,
#116238,#116239,#116240,#116241)),.UNSPECIFIED.,.F.,.F.,.F.)
B_SPLINE_SURFACE_WITH_KNOTS((2,2),(3,2,3),(0.,0.289807040991971),(0.297684616398974,
0.297856505190613,0.315045384354509),.UNSPECIFIED.)
GEOMETRIC_REPRESENTATION_ITEM()
RATIONAL_B_SPLINE_SURFACE(((0.992924952273132,0.992924952273132,0.992924952273132,
0.98894276409569,0.98786440923939),(0.992924952273132,0.992924952273132,
0.992924952273132,0.98894276409569,0.98786440923939)))
REPRESENTATION_ITEM('')
SURFACE()
);
#1355=(
BOUNDED_SURFACE()
B_SPLINE_SURFACE(1,2,((#116264,#116265,#116266,#116267,#116268,#116269,
#116270),(#116271,#116272,#116273,#116274,#116275,#116276,#116277)),
 .UNSPECIFIED.,.F.,.F.,.F.)
B_SPLINE_SURFACE_WITH_KNOTS((2,2),(3,2,2,3),(0.,0.289681084359924),(0.418207303127979,
0.428571428571429,0.435775021682622,0.435950698868169),.UNSPECIFIED.)
GEOMETRIC_REPRESENTATION_ITEM()
RATIONAL_B_SPLINE_SURFACE(((0.993779895952495,0.996362096314125,1.,0.997471472332736,
0.995452950231063,0.995452950231063,0.995452950231063),(0.993779895952495,
0.996362096314125,1.,0.997471472332736,0.995452950231063,0.995452950231063,
0.995452950231063)))
REPRESENTATION_ITEM('')
SURFACE()
);
#1356=(
BOUNDED_SURFACE()
B_SPLINE_SURFACE(1,2,((#116279,#116280,#116281,#116282,#116283),(#116284,
#116285,#116286,#116287,#116288)),.UNSPECIFIED.,.F.,.F.,.F.)
B_SPLINE_SURFACE_WITH_KNOTS((2,2),(3,2,3),(0.,0.289807040991893),(0.297684616398974,
0.297856505190613,0.315045384354503),.UNSPECIFIED.)
GEOMETRIC_REPRESENTATION_ITEM()
RATIONAL_B_SPLINE_SURFACE(((0.992924952273132,0.992924952273132,0.992924952273132,
0.988942764095691,0.987864409239391),(0.992924952273132,0.992924952273132,
0.992924952273132,0.988942764095691,0.987864409239391)))
REPRESENTATION_ITEM('')
SURFACE()
);
#1357=(
BOUNDED_SURFACE()
B_SPLINE_SURFACE(1,2,((#116311,#116312,#116313,#116314,#116315,#116316,
#116317),(#116318,#116319,#116320,#116321,#116322,#116323,#116324)),
 .UNSPECIFIED.,.F.,.F.,.F.)
B_SPLINE_SURFACE_WITH_KNOTS((2,2),(3,2,2,3),(0.,0.289681084359928),(0.418207303127979,
0.428571428571429,0.435775021682622,0.435950698868169),.UNSPECIFIED.)
GEOMETRIC_REPRESENTATION_ITEM()
RATIONAL_B_SPLINE_SURFACE(((0.993779895952495,0.996362096314125,1.,0.997471472332736,
0.995452950231063,0.995452950231063,0.995452950231063),(0.993779895952495,
0.996362096314125,1.,0.997471472332736,0.995452950231063,0.995452950231063,
0.995452950231063)))
REPRESENTATION_ITEM('')
SURFACE()
);
#1358=(
BOUNDED_SURFACE()
B_SPLINE_SURFACE(1,2,((#116326,#116327,#116328,#116329,#116330),(#116331,
#116332,#116333,#116334,#116335)),.UNSPECIFIED.,.F.,.F.,.F.)
B_SPLINE_SURFACE_WITH_KNOTS((2,2),(3,2,3),(0.,0.289807040992008),(0.297684616398473,
0.297856505190117,0.315045384354506),.UNSPECIFIED.)
GEOMETRIC_REPRESENTATION_ITEM()
RATIONAL_B_SPLINE_SURFACE(((0.992924952273362,0.992924952273362,0.992924952273362,
0.988942764095722,0.98786440923939),(0.992924952273362,0.992924952273362,
0.992924952273362,0.988942764095722,0.98786440923939)))
REPRESENTATION_ITEM('')
SURFACE()
);
#1359=(
BOUNDED_SURFACE()
B_SPLINE_SURFACE(1,2,((#116358,#116359,#116360,#116361,#116362,#116363,
#116364),(#116365,#116366,#116367,#116368,#116369,#116370,#116371)),
 .UNSPECIFIED.,.F.,.F.,.F.)
B_SPLINE_SURFACE_WITH_KNOTS((2,2),(3,2,2,3),(0.,0.289681084359928),(0.418207303127979,
0.428571428571429,0.435775021682622,0.435950698868169),.UNSPECIFIED.)
GEOMETRIC_REPRESENTATION_ITEM()
RATIONAL_B_SPLINE_SURFACE(((0.993779895952495,0.996362096314125,1.,0.997471472332736,
0.995452950231063,0.995452950231063,0.995452950231063),(0.993779895952495,
0.996362096314125,1.,0.997471472332736,0.995452950231063,0.995452950231063,
0.995452950231063)))
REPRESENTATION_ITEM('')
SURFACE()
);
#1360=(
BOUNDED_SURFACE()
B_SPLINE_SURFACE(1,2,((#116373,#116374,#116375,#116376,#116377),(#116378,
#116379,#116380,#116381,#116382)),.UNSPECIFIED.,.F.,.F.,.F.)
B_SPLINE_SURFACE_WITH_KNOTS((2,2),(3,2,3),(0.,0.289807040992683),(0.297684616398974,
0.297856505190613,0.315045384354503),.UNSPECIFIED.)
GEOMETRIC_REPRESENTATION_ITEM()
RATIONAL_B_SPLINE_SURFACE(((0.992924952273132,0.992924952273132,0.992924952273132,
0.988942764095691,0.98786440923939),(0.992924952273132,0.992924952273132,
0.992924952273132,0.988942764095691,0.98786440923939)))
REPRESENTATION_ITEM('')
SURFACE()
);
#1361=(
BOUNDED_SURFACE()
B_SPLINE_SURFACE(1,2,((#116405,#116406,#116407,#116408,#116409,#116410,
#116411),(#116412,#116413,#116414,#116415,#116416,#116417,#116418)),
 .UNSPECIFIED.,.F.,.F.,.F.)
B_SPLINE_SURFACE_WITH_KNOTS((2,2),(3,2,2,3),(0.,0.289681084360555),(0.418207303127979,
0.428571428571429,0.435775021682622,0.435950698868169),.UNSPECIFIED.)
GEOMETRIC_REPRESENTATION_ITEM()
RATIONAL_B_SPLINE_SURFACE(((0.993779895952495,0.996362096314125,1.,0.997471472332736,
0.995452950231063,0.995452950231063,0.995452950231063),(0.993779895952495,
0.996362096314125,1.,0.997471472332736,0.995452950231063,0.995452950231063,
0.995452950231063)))
REPRESENTATION_ITEM('')
SURFACE()
);
#1362=(
BOUNDED_SURFACE()
B_SPLINE_SURFACE(1,2,((#116420,#116421,#116422,#116423,#116424),(#116425,
#116426,#116427,#116428,#116429)),.UNSPECIFIED.,.F.,.F.,.F.)
B_SPLINE_SURFACE_WITH_KNOTS((2,2),(3,2,3),(0.,0.289807040992536),(0.297684616398974,
0.297856505190613,0.31504538435453),.UNSPECIFIED.)
GEOMETRIC_REPRESENTATION_ITEM()
RATIONAL_B_SPLINE_SURFACE(((0.992924952273132,0.992924952273132,0.992924952273132,
0.988942764095685,0.987864409239387),(0.992924952273132,0.992924952273132,
0.992924952273132,0.988942764095685,0.987864409239387)))
REPRESENTATION_ITEM('')
SURFACE()
);
#1363=(
BOUNDED_SURFACE()
B_SPLINE_SURFACE(1,2,((#116452,#116453,#116454,#116455,#116456,#116457,
#116458),(#116459,#116460,#116461,#116462,#116463,#116464,#116465)),
 .UNSPECIFIED.,.F.,.F.,.F.)
B_SPLINE_SURFACE_WITH_KNOTS((2,2),(3,2,2,3),(0.,0.289681084360345),(0.41820730312798,
0.428571428571429,0.435775021682622,0.435950698868169),.UNSPECIFIED.)
GEOMETRIC_REPRESENTATION_ITEM()
RATIONAL_B_SPLINE_SURFACE(((0.993779895952495,0.996362096314126,1.,0.997471472332736,
0.995452950231063,0.995452950231063,0.995452950231063),(0.993779895952495,
0.996362096314126,1.,0.997471472332736,0.995452950231063,0.995452950231063,
0.995452950231063)))
REPRESENTATION_ITEM('')
SURFACE()
);
#1364=(
BOUNDED_SURFACE()
B_SPLINE_SURFACE(1,2,((#116467,#116468,#116469,#116470,#116471),(#116472,
#116473,#116474,#116475,#116476)),.UNSPECIFIED.,.F.,.F.,.F.)
B_SPLINE_SURFACE_WITH_KNOTS((2,2),(3,2,3),(0.,0.289807040992501),(0.297684616398974,
0.297856505190613,0.315045384354503),.UNSPECIFIED.)
GEOMETRIC_REPRESENTATION_ITEM()
RATIONAL_B_SPLINE_SURFACE(((0.992924952273132,0.992924952273132,0.992924952273132,
0.988942764095691,0.98786440923939),(0.992924952273132,0.992924952273132,
0.992924952273132,0.988942764095691,0.987864409239391)))
REPRESENTATION_ITEM('')
SURFACE()
);
#1365=(
BOUNDED_SURFACE()
B_SPLINE_SURFACE(1,2,((#116499,#116500,#116501,#116502,#116503,#116504,
#116505),(#116506,#116507,#116508,#116509,#116510,#116511,#116512)),
 .UNSPECIFIED.,.F.,.F.,.F.)
B_SPLINE_SURFACE_WITH_KNOTS((2,2),(3,2,2,3),(0.,0.289681084359914),(0.418207303127979,
0.428571428571429,0.435775021682622,0.435950698868169),.UNSPECIFIED.)
GEOMETRIC_REPRESENTATION_ITEM()
RATIONAL_B_SPLINE_SURFACE(((0.993779895952495,0.996362096314125,1.,0.997471472332736,
0.995452950231063,0.995452950231063,0.995452950231063),(0.993779895952495,
0.996362096314125,1.,0.997471472332736,0.995452950231063,0.995452950231063,
0.995452950231063)))
REPRESENTATION_ITEM('')
SURFACE()
);
#1366=(
BOUNDED_SURFACE()
B_SPLINE_SURFACE(1,2,((#116514,#116515,#116516,#116517,#116518),(#116519,
#116520,#116521,#116522,#116523)),.UNSPECIFIED.,.F.,.F.,.F.)
B_SPLINE_SURFACE_WITH_KNOTS((2,2),(3,2,3),(0.,0.289807040992673),(0.297684616398974,
0.297856505190613,0.315045384354503),.UNSPECIFIED.)
GEOMETRIC_REPRESENTATION_ITEM()
RATIONAL_B_SPLINE_SURFACE(((0.992924952273132,0.992924952273132,0.992924952273132,
0.988942764095691,0.98786440923939),(0.992924952273132,0.992924952273132,
0.992924952273132,0.988942764095691,0.98786440923939)))
REPRESENTATION_ITEM('')
SURFACE()
);
#1367=(
BOUNDED_SURFACE()
B_SPLINE_SURFACE(1,2,((#116546,#116547,#116548,#116549,#116550,#116551,
#116552),(#116553,#116554,#116555,#116556,#116557,#116558,#116559)),
 .UNSPECIFIED.,.F.,.F.,.F.)
B_SPLINE_SURFACE_WITH_KNOTS((2,2),(3,2,2,3),(0.,0.28968108435992),(0.418207303127979,
0.428571428571429,0.435775021682622,0.435950698868169),.UNSPECIFIED.)
GEOMETRIC_REPRESENTATION_ITEM()
RATIONAL_B_SPLINE_SURFACE(((0.993779895952495,0.996362096314125,1.,0.997471472332736,
0.995452950231063,0.995452950231063,0.995452950231063),(0.993779895952495,
0.996362096314125,1.,0.997471472332736,0.995452950231063,0.995452950231063,
0.995452950231063)))
REPRESENTATION_ITEM('')
SURFACE()
);
#1368=(
BOUNDED_SURFACE()
B_SPLINE_SURFACE(1,2,((#116561,#116562,#116563,#116564,#116565),(#116566,
#116567,#116568,#116569,#116570)),.UNSPECIFIED.,.F.,.F.,.F.)
B_SPLINE_SURFACE_WITH_KNOTS((2,2),(3,2,3),(0.,0.289807040991738),(0.297684616398974,
0.297856505190613,0.315045384354503),.UNSPECIFIED.)
GEOMETRIC_REPRESENTATION_ITEM()
RATIONAL_B_SPLINE_SURFACE(((0.992924952273132,0.992924952273132,0.992924952273132,
0.988942764095691,0.98786440923939),(0.992924952273132,0.992924952273132,
0.992924952273132,0.988942764095691,0.98786440923939)))
REPRESENTATION_ITEM('')
SURFACE()
);
#1369=(
BOUNDED_SURFACE()
B_SPLINE_SURFACE(1,2,((#116593,#116594,#116595,#116596,#116597,#116598,
#116599),(#116600,#116601,#116602,#116603,#116604,#116605,#116606)),
 .UNSPECIFIED.,.F.,.F.,.F.)
B_SPLINE_SURFACE_WITH_KNOTS((2,2),(3,2,2,3),(0.,0.289681084359925),(0.418207303127979,
0.428571428571429,0.435775021682622,0.435950698868169),.UNSPECIFIED.)
GEOMETRIC_REPRESENTATION_ITEM()
RATIONAL_B_SPLINE_SURFACE(((0.993779895952495,0.996362096314125,1.,0.997471472332736,
0.995452950231063,0.995452950231063,0.995452950231063),(0.993779895952495,
0.996362096314125,1.,0.997471472332736,0.995452950231063,0.995452950231063,
0.995452950231063)))
REPRESENTATION_ITEM('')
SURFACE()
);
#1370=(
BOUNDED_SURFACE()
B_SPLINE_SURFACE(1,2,((#116608,#116609,#116610,#116611,#116612),(#116613,
#116614,#116615,#116616,#116617)),.UNSPECIFIED.,.F.,.F.,.F.)
B_SPLINE_SURFACE_WITH_KNOTS((2,2),(3,2,3),(0.,0.289807040991744),(0.297684616398974,
0.297856505190613,0.315045384354503),.UNSPECIFIED.)
GEOMETRIC_REPRESENTATION_ITEM()
RATIONAL_B_SPLINE_SURFACE(((0.992924952273132,0.992924952273132,0.992924952273132,
0.988942764095691,0.98786440923939),(0.992924952273132,0.992924952273132,
0.992924952273132,0.988942764095691,0.98786440923939)))
REPRESENTATION_ITEM('')
SURFACE()
);
#1371=(
BOUNDED_SURFACE()
B_SPLINE_SURFACE(1,2,((#116640,#116641,#116642,#116643,#116644,#116645,
#116646),(#116647,#116648,#116649,#116650,#116651,#116652,#116653)),
 .UNSPECIFIED.,.F.,.F.,.F.)
B_SPLINE_SURFACE_WITH_KNOTS((2,2),(3,2,2,3),(0.,0.289681084359988),(0.418207303127979,
0.428571428571429,0.435775021682622,0.435950698868169),.UNSPECIFIED.)
GEOMETRIC_REPRESENTATION_ITEM()
RATIONAL_B_SPLINE_SURFACE(((0.993779895952495,0.996362096314125,1.,0.997471472332736,
0.995452950231063,0.995452950231063,0.995452950231063),(0.993779895952495,
0.996362096314125,1.,0.997471472332736,0.995452950231063,0.995452950231063,
0.995452950231063)))
REPRESENTATION_ITEM('')
SURFACE()
);
#1372=(
BOUNDED_SURFACE()
B_SPLINE_SURFACE(1,2,((#116655,#116656,#116657,#116658,#116659),(#116660,
#116661,#116662,#116663,#116664)),.UNSPECIFIED.,.F.,.F.,.F.)
B_SPLINE_SURFACE_WITH_KNOTS((2,2),(3,2,3),(0.,0.289807040991851),(0.297684616398974,
0.297856505190613,0.315045384354503),.UNSPECIFIED.)
GEOMETRIC_REPRESENTATION_ITEM()
RATIONAL_B_SPLINE_SURFACE(((0.992924952273132,0.992924952273132,0.992924952273132,
0.988942764095691,0.98786440923939),(0.992924952273132,0.992924952273132,
0.992924952273132,0.988942764095691,0.98786440923939)))
REPRESENTATION_ITEM('')
SURFACE()
);
#1373=(
BOUNDED_SURFACE()
B_SPLINE_SURFACE(1,2,((#116687,#116688,#116689,#116690,#116691,#116692,
#116693),(#116694,#116695,#116696,#116697,#116698,#116699,#116700)),
 .UNSPECIFIED.,.F.,.F.,.F.)
B_SPLINE_SURFACE_WITH_KNOTS((2,2),(3,2,2,3),(0.,0.289681084360646),(0.418207303127979,
0.428571428571429,0.435775021682622,0.435950698868169),.UNSPECIFIED.)
GEOMETRIC_REPRESENTATION_ITEM()
RATIONAL_B_SPLINE_SURFACE(((0.993779895952495,0.996362096314125,1.,0.997471472332736,
0.995452950231063,0.995452950231063,0.995452950231063),(0.993779895952495,
0.996362096314125,1.,0.997471472332736,0.995452950231063,0.995452950231063,
0.995452950231063)))
REPRESENTATION_ITEM('')
SURFACE()
);
#1374=(
BOUNDED_SURFACE()
B_SPLINE_SURFACE(1,2,((#116702,#116703,#116704,#116705,#116706),(#116707,
#116708,#116709,#116710,#116711)),.UNSPECIFIED.,.F.,.F.,.F.)
B_SPLINE_SURFACE_WITH_KNOTS((2,2),(3,2,3),(0.,0.289807040991787),(0.297684616398974,
0.297856505190613,0.315045384354503),.UNSPECIFIED.)
GEOMETRIC_REPRESENTATION_ITEM()
RATIONAL_B_SPLINE_SURFACE(((0.992924952273132,0.992924952273132,0.992924952273132,
0.988942764095691,0.98786440923939),(0.992924952273132,0.992924952273132,
0.992924952273132,0.988942764095691,0.98786440923939)))
REPRESENTATION_ITEM('')
SURFACE()
);
#1375=(
BOUNDED_SURFACE()
B_SPLINE_SURFACE(1,2,((#116734,#116735,#116736,#116737,#116738,#116739,
#116740),(#116741,#116742,#116743,#116744,#116745,#116746,#116747)),
 .UNSPECIFIED.,.F.,.F.,.F.)
B_SPLINE_SURFACE_WITH_KNOTS((2,2),(3,2,2,3),(0.,0.289681084359924),(0.418207303127979,
0.428571428571429,0.435775021682622,0.435950698868169),.UNSPECIFIED.)
GEOMETRIC_REPRESENTATION_ITEM()
RATIONAL_B_SPLINE_SURFACE(((0.993779895952495,0.996362096314125,1.,0.997471472332736,
0.995452950231063,0.995452950231063,0.995452950231063),(0.993779895952495,
0.996362096314125,1.,0.997471472332736,0.995452950231063,0.995452950231063,
0.995452950231063)))
REPRESENTATION_ITEM('')
SURFACE()
);
#1376=(
BOUNDED_SURFACE()
B_SPLINE_SURFACE(1,2,((#116749,#116750,#116751,#116752,#116753),(#116754,
#116755,#116756,#116757,#116758)),.UNSPECIFIED.,.F.,.F.,.F.)
B_SPLINE_SURFACE_WITH_KNOTS((2,2),(3,2,3),(0.,0.289807040991759),(0.297684616398974,
0.297856505190613,0.315045384354503),.UNSPECIFIED.)
GEOMETRIC_REPRESENTATION_ITEM()
RATIONAL_B_SPLINE_SURFACE(((0.992924952273132,0.992924952273132,0.992924952273132,
0.988942764095691,0.98786440923939),(0.992924952273132,0.992924952273132,
0.992924952273132,0.988942764095691,0.98786440923939)))
REPRESENTATION_ITEM('')
SURFACE()
);
#1377=(
BOUNDED_SURFACE()
B_SPLINE_SURFACE(1,2,((#116781,#116782,#116783,#116784,#116785,#116786,
#116787),(#116788,#116789,#116790,#116791,#116792,#116793,#116794)),
 .UNSPECIFIED.,.F.,.F.,.F.)
B_SPLINE_SURFACE_WITH_KNOTS((2,2),(3,2,2,3),(0.,0.289681084359918),(0.418207303127979,
0.428571428571429,0.435775021682622,0.435950698868169),.UNSPECIFIED.)
GEOMETRIC_REPRESENTATION_ITEM()
RATIONAL_B_SPLINE_SURFACE(((0.993779895952495,0.996362096314125,1.,0.997471472332736,
0.995452950231063,0.995452950231063,0.995452950231063),(0.993779895952495,
0.996362096314125,1.,0.997471472332736,0.995452950231063,0.995452950231063,
0.995452950231063)))
REPRESENTATION_ITEM('')
SURFACE()
);
#1378=(
BOUNDED_SURFACE()
B_SPLINE_SURFACE(1,2,((#116796,#116797,#116798,#116799,#116800),(#116801,
#116802,#116803,#116804,#116805)),.UNSPECIFIED.,.F.,.F.,.F.)
B_SPLINE_SURFACE_WITH_KNOTS((2,2),(3,2,3),(0.,0.289807040991714),(0.297684616398974,
0.297856505190613,0.315045384354503),.UNSPECIFIED.)
GEOMETRIC_REPRESENTATION_ITEM()
RATIONAL_B_SPLINE_SURFACE(((0.992924952273132,0.992924952273132,0.992924952273132,
0.988942764095691,0.98786440923939),(0.992924952273132,0.992924952273132,
0.992924952273132,0.988942764095691,0.98786440923939)))
REPRESENTATION_ITEM('')
SURFACE()
);
#1379=(
BOUNDED_SURFACE()
B_SPLINE_SURFACE(1,2,((#116828,#116829,#116830,#116831,#116832,#116833,
#116834),(#116835,#116836,#116837,#116838,#116839,#116840,#116841)),
 .UNSPECIFIED.,.F.,.F.,.F.)
B_SPLINE_SURFACE_WITH_KNOTS((2,2),(3,2,2,3),(0.,0.289681084359924),(0.418207303127979,
0.428571428571429,0.435775021682622,0.435950698868169),.UNSPECIFIED.)
GEOMETRIC_REPRESENTATION_ITEM()
RATIONAL_B_SPLINE_SURFACE(((0.993779895952495,0.996362096314125,1.,0.997471472332736,
0.995452950231063,0.995452950231063,0.995452950231063),(0.993779895952495,
0.996362096314125,1.,0.997471472332736,0.995452950231063,0.995452950231063,
0.995452950231063)))
REPRESENTATION_ITEM('')
SURFACE()
);
#1380=(
BOUNDED_SURFACE()
B_SPLINE_SURFACE(1,2,((#116843,#116844,#116845,#116846,#116847),(#116848,
#116849,#116850,#116851,#116852)),.UNSPECIFIED.,.F.,.F.,.F.)
B_SPLINE_SURFACE_WITH_KNOTS((2,2),(3,2,3),(0.,0.289807040991564),(0.297684616398974,
0.297856505190613,0.315045384354503),.UNSPECIFIED.)
GEOMETRIC_REPRESENTATION_ITEM()
RATIONAL_B_SPLINE_SURFACE(((0.992924952273132,0.992924952273132,0.992924952273132,
0.988942764095691,0.98786440923939),(0.992924952273132,0.992924952273132,
0.992924952273132,0.988942764095691,0.98786440923939)))
REPRESENTATION_ITEM('')
SURFACE()
);
#1381=(
BOUNDED_SURFACE()
B_SPLINE_SURFACE(1,2,((#116875,#116876,#116877,#116878,#116879,#116880,
#116881),(#116882,#116883,#116884,#116885,#116886,#116887,#116888)),
 .UNSPECIFIED.,.F.,.F.,.F.)
B_SPLINE_SURFACE_WITH_KNOTS((2,2),(3,2,2,3),(0.,0.289681084359924),(0.418207303127979,
0.428571428571429,0.435775021682622,0.435950698868169),.UNSPECIFIED.)
GEOMETRIC_REPRESENTATION_ITEM()
RATIONAL_B_SPLINE_SURFACE(((0.993779895952495,0.996362096314125,1.,0.997471472332736,
0.995452950231063,0.995452950231063,0.995452950231063),(0.993779895952495,
0.996362096314125,1.,0.997471472332736,0.995452950231063,0.995452950231063,
0.995452950231063)))
REPRESENTATION_ITEM('')
SURFACE()
);
#1382=(
BOUNDED_SURFACE()
B_SPLINE_SURFACE(1,2,((#116890,#116891,#116892,#116893,#116894),(#116895,
#116896,#116897,#116898,#116899)),.UNSPECIFIED.,.F.,.F.,.F.)
B_SPLINE_SURFACE_WITH_KNOTS((2,2),(3,2,3),(0.,0.289807040991565),(0.297684616398974,
0.297856505190613,0.315045384354503),.UNSPECIFIED.)
GEOMETRIC_REPRESENTATION_ITEM()
RATIONAL_B_SPLINE_SURFACE(((0.992924952273132,0.992924952273132,0.992924952273132,
0.988942764095691,0.98786440923939),(0.992924952273132,0.992924952273132,
0.992924952273132,0.988942764095691,0.98786440923939)))
REPRESENTATION_ITEM('')
SURFACE()
);
#1383=(
BOUNDED_SURFACE()
B_SPLINE_SURFACE(1,2,((#116907,#116908,#116909,#116910,#116911,#116912,
#116913),(#116914,#116915,#116916,#116917,#116918,#116919,#116920)),
 .UNSPECIFIED.,.F.,.F.,.F.)
B_SPLINE_SURFACE_WITH_KNOTS((2,2),(3,2,2,3),(0.,0.289681084359926),(0.418207303127979,
0.428571428571429,0.435775021682622,0.435950698868169),.UNSPECIFIED.)
GEOMETRIC_REPRESENTATION_ITEM()
RATIONAL_B_SPLINE_SURFACE(((0.993779895952495,0.996362096314125,1.,0.997471472332736,
0.995452950231063,0.995452950231063,0.995452950231063),(0.993779895952495,
0.996362096314125,1.,0.997471472332736,0.995452950231063,0.995452950231063,
0.995452950231063)))
REPRESENTATION_ITEM('')
SURFACE()
);
#1384=(
BOUNDED_SURFACE()
B_SPLINE_SURFACE(1,2,((#116922,#116923,#116924,#116925,#116926),(#116927,
#116928,#116929,#116930,#116931)),.UNSPECIFIED.,.F.,.F.,.F.)
B_SPLINE_SURFACE_WITH_KNOTS((2,2),(3,2,3),(0.,0.289807040991568),(0.297684616398974,
0.297856505190613,0.315045384354503),.UNSPECIFIED.)
GEOMETRIC_REPRESENTATION_ITEM()
RATIONAL_B_SPLINE_SURFACE(((0.992924952273132,0.992924952273132,0.992924952273132,
0.988942764095691,0.98786440923939),(0.992924952273132,0.992924952273132,
0.992924952273132,0.988942764095691,0.98786440923939)))
REPRESENTATION_ITEM('')
SURFACE()
);
#1385=(
BOUNDED_SURFACE()
B_SPLINE_SURFACE(1,2,((#116954,#116955,#116956,#116957,#116958,#116959,
#116960),(#116961,#116962,#116963,#116964,#116965,#116966,#116967)),
 .UNSPECIFIED.,.F.,.F.,.F.)
B_SPLINE_SURFACE_WITH_KNOTS((2,2),(3,2,2,3),(0.,0.289681084359931),(0.418207303127979,
0.428571428571429,0.435775021682622,0.435950698868169),.UNSPECIFIED.)
GEOMETRIC_REPRESENTATION_ITEM()
RATIONAL_B_SPLINE_SURFACE(((0.993779895952495,0.996362096314125,1.,0.997471472332736,
0.995452950231063,0.995452950231063,0.995452950231063),(0.993779895952495,
0.996362096314125,1.,0.997471472332736,0.995452950231063,0.995452950231063,
0.995452950231063)))
REPRESENTATION_ITEM('')
SURFACE()
);
#1386=(
BOUNDED_SURFACE()
B_SPLINE_SURFACE(1,2,((#116969,#116970,#116971,#116972,#116973),(#116974,
#116975,#116976,#116977,#116978)),.UNSPECIFIED.,.F.,.F.,.F.)
B_SPLINE_SURFACE_WITH_KNOTS((2,2),(3,2,3),(0.,0.289807040991561),(0.297684616398974,
0.297856505190613,0.315045384354503),.UNSPECIFIED.)
GEOMETRIC_REPRESENTATION_ITEM()
RATIONAL_B_SPLINE_SURFACE(((0.992924952273132,0.992924952273132,0.992924952273132,
0.988942764095691,0.98786440923939),(0.992924952273132,0.992924952273132,
0.992924952273132,0.988942764095691,0.98786440923939)))
REPRESENTATION_ITEM('')
SURFACE()
);
#1387=(
BOUNDED_SURFACE()
B_SPLINE_SURFACE(1,2,((#117001,#117002,#117003,#117004,#117005,#117006,
#117007),(#117008,#117009,#117010,#117011,#117012,#117013,#117014)),
 .UNSPECIFIED.,.F.,.F.,.F.)
B_SPLINE_SURFACE_WITH_KNOTS((2,2),(3,2,2,3),(0.,0.289681084359919),(0.418207303127979,
0.428571428571429,0.435775021682622,0.435950698868169),.UNSPECIFIED.)
GEOMETRIC_REPRESENTATION_ITEM()
RATIONAL_B_SPLINE_SURFACE(((0.993779895952495,0.996362096314125,1.,0.997471472332736,
0.995452950231063,0.995452950231063,0.995452950231063),(0.993779895952495,
0.996362096314125,1.,0.997471472332736,0.995452950231063,0.995452950231063,
0.995452950231063)))
REPRESENTATION_ITEM('')
SURFACE()
);
#1388=(
BOUNDED_SURFACE()
B_SPLINE_SURFACE(1,2,((#117016,#117017,#117018,#117019,#117020),(#117021,
#117022,#117023,#117024,#117025)),.UNSPECIFIED.,.F.,.F.,.F.)
B_SPLINE_SURFACE_WITH_KNOTS((2,2),(3,2,3),(0.,0.289807040991558),(0.297684616398974,
0.297856505190613,0.315045384354503),.UNSPECIFIED.)
GEOMETRIC_REPRESENTATION_ITEM()
RATIONAL_B_SPLINE_SURFACE(((0.992924952273132,0.992924952273132,0.992924952273132,
0.988942764095691,0.98786440923939),(0.992924952273132,0.992924952273132,
0.992924952273132,0.988942764095691,0.98786440923939)))
REPRESENTATION_ITEM('')
SURFACE()
);
#1389=(
BOUNDED_SURFACE()
B_SPLINE_SURFACE(1,2,((#117048,#117049,#117050,#117051,#117052,#117053,
#117054),(#117055,#117056,#117057,#117058,#117059,#117060,#117061)),
 .UNSPECIFIED.,.F.,.F.,.F.)
B_SPLINE_SURFACE_WITH_KNOTS((2,2),(3,2,2,3),(0.,0.289681084359921),(0.418207303127979,
0.428571428571429,0.435775021682622,0.435950698868169),.UNSPECIFIED.)
GEOMETRIC_REPRESENTATION_ITEM()
RATIONAL_B_SPLINE_SURFACE(((0.993779895952495,0.996362096314125,1.,0.997471472332736,
0.995452950231063,0.995452950231063,0.995452950231063),(0.993779895952495,
0.996362096314125,1.,0.997471472332736,0.995452950231063,0.995452950231063,
0.995452950231063)))
REPRESENTATION_ITEM('')
SURFACE()
);
#1390=(
BOUNDED_SURFACE()
B_SPLINE_SURFACE(1,2,((#117063,#117064,#117065,#117066,#117067),(#117068,
#117069,#117070,#117071,#117072)),.UNSPECIFIED.,.F.,.F.,.F.)
B_SPLINE_SURFACE_WITH_KNOTS((2,2),(3,2,3),(0.,0.289807040991672),(0.297684616398974,
0.297856505190613,0.315045384354503),.UNSPECIFIED.)
GEOMETRIC_REPRESENTATION_ITEM()
RATIONAL_B_SPLINE_SURFACE(((0.992924952273132,0.992924952273132,0.992924952273132,
0.988942764095691,0.98786440923939),(0.992924952273132,0.992924952273132,
0.992924952273132,0.988942764095691,0.98786440923939)))
REPRESENTATION_ITEM('')
SURFACE()
);
#1391=(
BOUNDED_SURFACE()
B_SPLINE_SURFACE(1,2,((#117095,#117096,#117097,#117098,#117099,#117100,
#117101),(#117102,#117103,#117104,#117105,#117106,#117107,#117108)),
 .UNSPECIFIED.,.F.,.F.,.F.)
B_SPLINE_SURFACE_WITH_KNOTS((2,2),(3,2,2,3),(0.,0.289681084359923),(0.418207303127979,
0.428571428571429,0.435775021682622,0.435950698868169),.UNSPECIFIED.)
GEOMETRIC_REPRESENTATION_ITEM()
RATIONAL_B_SPLINE_SURFACE(((0.993779895952495,0.996362096314125,1.,0.997471472332736,
0.995452950231063,0.995452950231063,0.995452950231063),(0.993779895952495,
0.996362096314125,1.,0.997471472332736,0.995452950231063,0.995452950231063,
0.995452950231063)))
REPRESENTATION_ITEM('')
SURFACE()
);
#1392=(
BOUNDED_SURFACE()
B_SPLINE_SURFACE(1,2,((#117110,#117111,#117112,#117113,#117114),(#117115,
#117116,#117117,#117118,#117119)),.UNSPECIFIED.,.F.,.F.,.F.)
B_SPLINE_SURFACE_WITH_KNOTS((2,2),(3,2,3),(0.,0.289807040992966),(0.297684616398974,
0.297856505190613,0.315045384354503),.UNSPECIFIED.)
GEOMETRIC_REPRESENTATION_ITEM()
RATIONAL_B_SPLINE_SURFACE(((0.992924952273132,0.992924952273132,0.992924952273132,
0.988942764095691,0.98786440923939),(0.992924952273132,0.992924952273132,
0.992924952273132,0.988942764095691,0.98786440923939)))
REPRESENTATION_ITEM('')
SURFACE()
);
#1393=(
BOUNDED_SURFACE()
B_SPLINE_SURFACE(1,2,((#117142,#117143,#117144,#117145,#117146,#117147,
#117148),(#117149,#117150,#117151,#117152,#117153,#117154,#117155)),
 .UNSPECIFIED.,.F.,.F.,.F.)
B_SPLINE_SURFACE_WITH_KNOTS((2,2),(3,2,2,3),(0.,0.28968108435992),(0.418207303127979,
0.428571428571429,0.435775021682622,0.435950698868169),.UNSPECIFIED.)
GEOMETRIC_REPRESENTATION_ITEM()
RATIONAL_B_SPLINE_SURFACE(((0.993779895952495,0.996362096314125,1.,0.997471472332736,
0.995452950231063,0.995452950231063,0.995452950231063),(0.993779895952495,
0.996362096314125,1.,0.997471472332736,0.995452950231063,0.995452950231063,
0.995452950231063)))
REPRESENTATION_ITEM('')
SURFACE()
);
#1394=(
BOUNDED_SURFACE()
B_SPLINE_SURFACE(1,2,((#117157,#117158,#117159,#117160,#117161),(#117162,
#117163,#117164,#117165,#117166)),.UNSPECIFIED.,.F.,.F.,.F.)
B_SPLINE_SURFACE_WITH_KNOTS((2,2),(3,2,3),(0.,0.289807040991817),(0.297684616398974,
0.297856505190613,0.315045384354503),.UNSPECIFIED.)
GEOMETRIC_REPRESENTATION_ITEM()
RATIONAL_B_SPLINE_SURFACE(((0.992924952273132,0.992924952273132,0.992924952273132,
0.988942764095691,0.98786440923939),(0.992924952273132,0.992924952273132,
0.992924952273132,0.988942764095691,0.987864409239391)))
REPRESENTATION_ITEM('')
SURFACE()
);
#1395=(
BOUNDED_SURFACE()
B_SPLINE_SURFACE(1,2,((#117189,#117190,#117191,#117192,#117193,#117194,
#117195),(#117196,#117197,#117198,#117199,#117200,#117201,#117202)),
 .UNSPECIFIED.,.F.,.F.,.F.)
B_SPLINE_SURFACE_WITH_KNOTS((2,2),(3,2,2,3),(0.,0.28968108435992),(0.418207303127979,
0.428571428571429,0.435775021682622,0.435950698868169),.UNSPECIFIED.)
GEOMETRIC_REPRESENTATION_ITEM()
RATIONAL_B_SPLINE_SURFACE(((0.993779895952495,0.996362096314125,1.,0.997471472332736,
0.995452950231063,0.995452950231063,0.995452950231063),(0.993779895952495,
0.996362096314125,1.,0.997471472332736,0.995452950231063,0.995452950231063,
0.995452950231063)))
REPRESENTATION_ITEM('')
SURFACE()
);
#1396=(
BOUNDED_SURFACE()
B_SPLINE_SURFACE(1,2,((#117204,#117205,#117206,#117207,#117208),(#117209,
#117210,#117211,#117212,#117213)),.UNSPECIFIED.,.F.,.F.,.F.)
B_SPLINE_SURFACE_WITH_KNOTS((2,2),(3,2,3),(0.,0.28980704099156),(0.297684616398974,
0.297856505190613,0.315045384354503),.UNSPECIFIED.)
GEOMETRIC_REPRESENTATION_ITEM()
RATIONAL_B_SPLINE_SURFACE(((0.992924952273132,0.992924952273132,0.992924952273132,
0.988942764095691,0.98786440923939),(0.992924952273132,0.992924952273132,
0.992924952273132,0.988942764095691,0.98786440923939)))
REPRESENTATION_ITEM('')
SURFACE()
);
#1397=(
BOUNDED_SURFACE()
B_SPLINE_SURFACE(1,2,((#117236,#117237,#117238,#117239,#117240,#117241,
#117242),(#117243,#117244,#117245,#117246,#117247,#117248,#117249)),
 .UNSPECIFIED.,.F.,.F.,.F.)
B_SPLINE_SURFACE_WITH_KNOTS((2,2),(3,2,2,3),(0.,0.28968108435992),(0.418207303127979,
0.428571428571429,0.435775021682622,0.435950698868169),.UNSPECIFIED.)
GEOMETRIC_REPRESENTATION_ITEM()
RATIONAL_B_SPLINE_SURFACE(((0.993779895952495,0.996362096314125,1.,0.997471472332736,
0.995452950231063,0.995452950231063,0.995452950231063),(0.993779895952495,
0.996362096314125,1.,0.997471472332736,0.995452950231063,0.995452950231063,
0.995452950231063)))
REPRESENTATION_ITEM('')
SURFACE()
);
#1398=(
BOUNDED_SURFACE()
B_SPLINE_SURFACE(1,2,((#117251,#117252,#117253,#117254,#117255),(#117256,
#117257,#117258,#117259,#117260)),.UNSPECIFIED.,.F.,.F.,.F.)
B_SPLINE_SURFACE_WITH_KNOTS((2,2),(3,2,3),(0.,0.289807040991555),(0.297684616398974,
0.297856505190613,0.315045384354503),.UNSPECIFIED.)
GEOMETRIC_REPRESENTATION_ITEM()
RATIONAL_B_SPLINE_SURFACE(((0.992924952273132,0.992924952273132,0.992924952273132,
0.988942764095691,0.98786440923939),(0.992924952273132,0.992924952273132,
0.992924952273132,0.988942764095691,0.98786440923939)))
REPRESENTATION_ITEM('')
SURFACE()
);
#1399=(
BOUNDED_SURFACE()
B_SPLINE_SURFACE(1,2,((#117271,#117272,#117273,#117274,#117275,#117276,
#117277),(#117278,#117279,#117280,#117281,#117282,#117283,#117284)),
 .UNSPECIFIED.,.F.,.F.,.F.)
B_SPLINE_SURFACE_WITH_KNOTS((2,2),(3,2,2,3),(0.,0.289681084359917),(0.418207303127979,
0.428571428571429,0.435775021682622,0.435950698868169),.UNSPECIFIED.)
GEOMETRIC_REPRESENTATION_ITEM()
RATIONAL_B_SPLINE_SURFACE(((0.993779895952495,0.996362096314125,1.,0.997471472332736,
0.995452950231063,0.995452950231063,0.995452950231063),(0.993779895952495,
0.996362096314125,1.,0.997471472332736,0.995452950231063,0.995452950231063,
0.995452950231063)))
REPRESENTATION_ITEM('')
SURFACE()
);
#1400=(
BOUNDED_SURFACE()
B_SPLINE_SURFACE(1,2,((#117298,#117299,#117300,#117301,#117302),(#117303,
#117304,#117305,#117306,#117307)),.UNSPECIFIED.,.F.,.F.,.F.)
B_SPLINE_SURFACE_WITH_KNOTS((2,2),(3,2,3),(0.,0.289807040991562),(0.297684616398974,
0.297856505190613,0.315045384354503),.UNSPECIFIED.)
GEOMETRIC_REPRESENTATION_ITEM()
RATIONAL_B_SPLINE_SURFACE(((0.992924952273132,0.992924952273132,0.992924952273132,
0.988942764095691,0.98786440923939),(0.992924952273132,0.992924952273132,
0.992924952273132,0.988942764095691,0.98786440923939)))
REPRESENTATION_ITEM('')
SURFACE()
);
#1401=(
BOUNDED_SURFACE()
B_SPLINE_SURFACE(1,2,((#117330,#117331,#117332,#117333,#117334,#117335,
#117336),(#117337,#117338,#117339,#117340,#117341,#117342,#117343)),
 .UNSPECIFIED.,.F.,.F.,.F.)
B_SPLINE_SURFACE_WITH_KNOTS((2,2),(3,2,2,3),(0.,0.289681084359921),(0.418207303127979,
0.428571428571429,0.435775021682621,0.435950698868168),.UNSPECIFIED.)
GEOMETRIC_REPRESENTATION_ITEM()
RATIONAL_B_SPLINE_SURFACE(((0.993779895952495,0.996362096314125,1.,0.997471472332737,
0.995452950231064,0.995452950231064,0.995452950231064),(0.993779895952495,
0.996362096314125,1.,0.997471472332737,0.995452950231063,0.995452950231063,
0.995452950231063)))
REPRESENTATION_ITEM('')
SURFACE()
);
#1402=(
BOUNDED_SURFACE()
B_SPLINE_SURFACE(1,2,((#117345,#117346,#117347,#117348,#117349),(#117350,
#117351,#117352,#117353,#117354)),.UNSPECIFIED.,.F.,.F.,.F.)
B_SPLINE_SURFACE_WITH_KNOTS((2,2),(3,2,3),(0.,0.289807040991634),(0.297684616398489,
0.297856505190132,0.315045384354507),.UNSPECIFIED.)
GEOMETRIC_REPRESENTATION_ITEM()
RATIONAL_B_SPLINE_SURFACE(((0.992924952273355,0.992924952273355,0.992924952273355,
0.988942764095721,0.98786440923939),(0.992924952273355,0.992924952273355,
0.992924952273355,0.988942764095721,0.98786440923939)))
REPRESENTATION_ITEM('')
SURFACE()
);
#1403=(
BOUNDED_SURFACE()
B_SPLINE_SURFACE(1,2,((#117377,#117378,#117379,#117380,#117381,#117382,
#117383),(#117384,#117385,#117386,#117387,#117388,#117389,#117390)),
 .UNSPECIFIED.,.F.,.F.,.F.)
B_SPLINE_SURFACE_WITH_KNOTS((2,2),(3,2,2,3),(0.,0.289681084359999),(0.418207303127978,
0.428571428571429,0.435775021682621,0.435950698868168),.UNSPECIFIED.)
GEOMETRIC_REPRESENTATION_ITEM()
RATIONAL_B_SPLINE_SURFACE(((0.993779895952495,0.996362096314125,1.,0.997471472332737,
0.995452950231063,0.995452950231063,0.995452950231063),(0.993779895952495,
0.996362096314125,1.,0.997471472332737,0.995452950231063,0.995452950231063,
0.995452950231063)))
REPRESENTATION_ITEM('')
SURFACE()
);
#1404=(
BOUNDED_SURFACE()
B_SPLINE_SURFACE(1,2,((#117392,#117393,#117394,#117395,#117396),(#117397,
#117398,#117399,#117400,#117401)),.UNSPECIFIED.,.F.,.F.,.F.)
B_SPLINE_SURFACE_WITH_KNOTS((2,2),(3,2,3),(0.,0.289807040991643),(0.297684616398975,
0.297856505190614,0.315045384354505),.UNSPECIFIED.)
GEOMETRIC_REPRESENTATION_ITEM()
RATIONAL_B_SPLINE_SURFACE(((0.992924952273132,0.992924952273132,0.992924952273132,
0.988942764095691,0.98786440923939),(0.992924952273132,0.992924952273132,
0.992924952273132,0.988942764095691,0.98786440923939)))
REPRESENTATION_ITEM('')
SURFACE()
);
#1405=(
BOUNDED_SURFACE()
B_SPLINE_SURFACE(1,2,((#117424,#117425,#117426,#117427,#117428,#117429,
#117430),(#117431,#117432,#117433,#117434,#117435,#117436,#117437)),
 .UNSPECIFIED.,.F.,.F.,.F.)
B_SPLINE_SURFACE_WITH_KNOTS((2,2),(3,2,2,3),(0.,0.28968108436),(0.418207303127978,
0.428571428571429,0.435775021682621,0.435950698868168),.UNSPECIFIED.)
GEOMETRIC_REPRESENTATION_ITEM()
RATIONAL_B_SPLINE_SURFACE(((0.993779895952495,0.996362096314125,1.,0.997471472332737,
0.995452950231063,0.995452950231063,0.995452950231063),(0.993779895952495,
0.996362096314125,1.,0.997471472332737,0.995452950231063,0.995452950231063,
0.995452950231063)))
REPRESENTATION_ITEM('')
SURFACE()
);
#1406=(
BOUNDED_SURFACE()
B_SPLINE_SURFACE(1,2,((#117439,#117440,#117441,#117442,#117443),(#117444,
#117445,#117446,#117447,#117448)),.UNSPECIFIED.,.F.,.F.,.F.)
B_SPLINE_SURFACE_WITH_KNOTS((2,2),(3,2,3),(0.,0.289807040991662),(0.29768461639894,
0.297856505190579,0.315045384354505),.UNSPECIFIED.)
GEOMETRIC_REPRESENTATION_ITEM()
RATIONAL_B_SPLINE_SURFACE(((0.992924952273148,0.992924952273148,0.992924952273148,
0.988942764095693,0.98786440923939),(0.992924952273148,0.992924952273148,
0.992924952273148,0.988942764095693,0.98786440923939)))
REPRESENTATION_ITEM('')
SURFACE()
);
#1407=(
BOUNDED_SURFACE()
B_SPLINE_SURFACE(1,2,((#117471,#117472,#117473,#117474,#117475,#117476,
#117477),(#117478,#117479,#117480,#117481,#117482,#117483,#117484)),
 .UNSPECIFIED.,.F.,.F.,.F.)
B_SPLINE_SURFACE_WITH_KNOTS((2,2),(3,2,2,3),(0.,0.289681084360011),(0.418207303127978,
0.428571428571429,0.435775021682622,0.435950698868169),.UNSPECIFIED.)
GEOMETRIC_REPRESENTATION_ITEM()
RATIONAL_B_SPLINE_SURFACE(((0.993779895952495,0.996362096314125,1.,0.997471472332736,
0.995452950231063,0.995452950231063,0.995452950231063),(0.993779895952495,
0.996362096314125,1.,0.997471472332736,0.995452950231063,0.995452950231063,
0.995452950231063)))
REPRESENTATION_ITEM('')
SURFACE()
);
#1408=(
BOUNDED_SURFACE()
B_SPLINE_SURFACE(1,2,((#117486,#117487,#117488,#117489,#117490),(#117491,
#117492,#117493,#117494,#117495)),.UNSPECIFIED.,.F.,.F.,.F.)
B_SPLINE_SURFACE_WITH_KNOTS((2,2),(3,2,3),(0.,0.289807040991655),(0.297684616398975,
0.297856505190614,0.315045384354503),.UNSPECIFIED.)
GEOMETRIC_REPRESENTATION_ITEM()
RATIONAL_B_SPLINE_SURFACE(((0.992924952273132,0.992924952273132,0.992924952273132,
0.988942764095691,0.98786440923939),(0.992924952273132,0.992924952273132,
0.992924952273132,0.988942764095691,0.98786440923939)))
REPRESENTATION_ITEM('')
SURFACE()
);
#1409=(
BOUNDED_SURFACE()
B_SPLINE_SURFACE(1,2,((#117518,#117519,#117520,#117521,#117522,#117523,
#117524),(#117525,#117526,#117527,#117528,#117529,#117530,#117531)),
 .UNSPECIFIED.,.F.,.F.,.F.)
B_SPLINE_SURFACE_WITH_KNOTS((2,2),(3,2,2,3),(0.,0.289681084359918),(0.418207303127979,
0.428571428571429,0.435775021682624,0.435950698868171),.UNSPECIFIED.)
GEOMETRIC_REPRESENTATION_ITEM()
RATIONAL_B_SPLINE_SURFACE(((0.993779895952495,0.996362096314125,1.,0.997471472332736,
0.995452950231062,0.995452950231062,0.995452950231062),(0.993779895952495,
0.996362096314125,1.,0.997471472332736,0.995452950231062,0.995452950231062,
0.995452950231062)))
REPRESENTATION_ITEM('')
SURFACE()
);
#1410=(
BOUNDED_SURFACE()
B_SPLINE_SURFACE(1,2,((#117533,#117534,#117535,#117536,#117537),(#117538,
#117539,#117540,#117541,#117542)),.UNSPECIFIED.,.F.,.F.,.F.)
B_SPLINE_SURFACE_WITH_KNOTS((2,2),(3,2,3),(0.,0.289807040992022),(0.297684616398974,
0.297856505190613,0.315045384354503),.UNSPECIFIED.)
GEOMETRIC_REPRESENTATION_ITEM()
RATIONAL_B_SPLINE_SURFACE(((0.992924952273132,0.992924952273132,0.992924952273132,
0.988942764095691,0.98786440923939),(0.992924952273132,0.992924952273132,
0.992924952273132,0.988942764095691,0.98786440923939)))
REPRESENTATION_ITEM('')
SURFACE()
);
#1411=(
BOUNDED_SURFACE()
B_SPLINE_SURFACE(1,2,((#117565,#117566,#117567,#117568,#117569,#117570,
#117571),(#117572,#117573,#117574,#117575,#117576,#117577,#117578)),
 .UNSPECIFIED.,.F.,.F.,.F.)
B_SPLINE_SURFACE_WITH_KNOTS((2,2),(3,2,2,3),(0.,0.289681084359936),(0.418207303127979,
0.428571428571429,0.435775021682622,0.435950698868169),.UNSPECIFIED.)
GEOMETRIC_REPRESENTATION_ITEM()
RATIONAL_B_SPLINE_SURFACE(((0.993779895952495,0.996362096314125,1.,0.997471472332736,
0.995452950231063,0.995452950231063,0.995452950231063),(0.993779895952495,
0.996362096314125,1.,0.997471472332736,0.995452950231063,0.995452950231063,
0.995452950231063)))
REPRESENTATION_ITEM('')
SURFACE()
);
#1412=(
BOUNDED_SURFACE()
B_SPLINE_SURFACE(1,2,((#117580,#117581,#117582,#117583,#117584),(#117585,
#117586,#117587,#117588,#117589)),.UNSPECIFIED.,.F.,.F.,.F.)
B_SPLINE_SURFACE_WITH_KNOTS((2,2),(3,2,3),(0.710318915640079,1.),(0.469916319328035,
0.487259899888158,0.487433335693759),.UNSPECIFIED.)
GEOMETRIC_REPRESENTATION_ITEM()
RATIONAL_B_SPLINE_SURFACE(((0.987775548376701,0.988735325500096,0.992651440660745,
0.992651440660745,0.992651440660745),(0.987775548376701,0.988735325500096,
0.992651440660745,0.992651440660745,0.992651440660745)))
REPRESENTATION_ITEM('')
SURFACE()
);
#1413=(
BOUNDED_SURFACE()
B_SPLINE_SURFACE(1,2,((#117600,#117601,#117602,#117603,#117604),(#117605,
#117606,#117607,#117608,#117609)),.UNSPECIFIED.,.F.,.F.,.F.)
B_SPLINE_SURFACE_WITH_KNOTS((2,2),(3,2,3),(0.709598828809336,1.),(0.245359920965979,
0.245954053070908,0.263201868951015),.UNSPECIFIED.)
GEOMETRIC_REPRESENTATION_ITEM()
RATIONAL_B_SPLINE_SURFACE(((0.987624841600687,0.987624841600687,0.987624841600687,
0.986938988894507,0.989176916802452),(0.987624841600687,0.987624841600687,
0.987624841600687,0.986938988894507,0.989176916802452)))
REPRESENTATION_ITEM('')
SURFACE()
);
#1414=(
BOUNDED_SURFACE()
B_SPLINE_SURFACE(1,2,((#117617,#117618,#117619,#117620,#117621),(#117622,
#117623,#117624,#117625,#117626)),.UNSPECIFIED.,.F.,.F.,.F.)
B_SPLINE_SURFACE_WITH_KNOTS((2,2),(3,2,3),(0.710318915640086,1.),(0.469916319328035,
0.487259899888158,0.487433335693759),.UNSPECIFIED.)
GEOMETRIC_REPRESENTATION_ITEM()
RATIONAL_B_SPLINE_SURFACE(((0.987775548376701,0.988735325500096,0.992651440660745,
0.992651440660745,0.992651440660745),(0.987775548376701,0.988735325500096,
0.992651440660745,0.992651440660745,0.992651440660745)))
REPRESENTATION_ITEM('')
SURFACE()
);
#1415=(
BOUNDED_SURFACE()
B_SPLINE_SURFACE(1,2,((#117637,#117638,#117639,#117640,#117641),(#117642,
#117643,#117644,#117645,#117646)),.UNSPECIFIED.,.F.,.F.,.F.)
B_SPLINE_SURFACE_WITH_KNOTS((2,2),(3,2,3),(0.709598828760674,1.),(0.245359920917525,
0.245954053070909,0.263201868951015),.UNSPECIFIED.)
GEOMETRIC_REPRESENTATION_ITEM()
RATIONAL_B_SPLINE_SURFACE(((0.987624841600687,0.987624841600687,0.987624841600687,
0.986938988894508,0.989176916802452),(0.987624841600687,0.987624841600687,
0.987624841600687,0.986938988894508,0.989176916802452)))
REPRESENTATION_ITEM('')
SURFACE()
);
#1416=(
BOUNDED_SURFACE()
B_SPLINE_SURFACE(1,2,((#117654,#117655,#117656,#117657,#117658),(#117659,
#117660,#117661,#117662,#117663)),.UNSPECIFIED.,.F.,.F.,.F.)
B_SPLINE_SURFACE_WITH_KNOTS((2,2),(3,2,3),(0.710318915640078,1.),(0.469916319328035,
0.487259899888158,0.487433335693759),.UNSPECIFIED.)
GEOMETRIC_REPRESENTATION_ITEM()
RATIONAL_B_SPLINE_SURFACE(((0.987775548376701,0.988735325500096,0.992651440660745,
0.992651440660745,0.992651440660745),(0.987775548376701,0.988735325500096,
0.992651440660745,0.992651440660745,0.992651440660745)))
REPRESENTATION_ITEM('')
SURFACE()
);
#1417=(
BOUNDED_SURFACE()
B_SPLINE_SURFACE(1,2,((#117674,#117675,#117676,#117677,#117678),(#117679,
#117680,#117681,#117682,#117683)),.UNSPECIFIED.,.F.,.F.,.F.)
B_SPLINE_SURFACE_WITH_KNOTS((2,2),(3,2,3),(0.709598828789182,1.),(0.245359920945796,
0.245954053070908,0.263201868951015),.UNSPECIFIED.)
GEOMETRIC_REPRESENTATION_ITEM()
RATIONAL_B_SPLINE_SURFACE(((0.987624841600687,0.987624841600687,0.987624841600687,
0.986938988894507,0.989176916802452),(0.987624841600687,0.987624841600687,
0.987624841600687,0.986938988894508,0.989176916802452)))
REPRESENTATION_ITEM('')
SURFACE()
);
#1418=(
BOUNDED_SURFACE()
B_SPLINE_SURFACE(1,2,((#117691,#117692,#117693,#117694,#117695),(#117696,
#117697,#117698,#117699,#117700)),.UNSPECIFIED.,.F.,.F.,.F.)
B_SPLINE_SURFACE_WITH_KNOTS((2,2),(3,2,3),(0.710318915639496,1.),(0.469916319328035,
0.487259899888158,0.487433335693759),.UNSPECIFIED.)
GEOMETRIC_REPRESENTATION_ITEM()
RATIONAL_B_SPLINE_SURFACE(((0.987775548376701,0.988735325500096,0.992651440660745,
0.992651440660745,0.992651440660745),(0.987775548376701,0.988735325500096,
0.992651440660745,0.992651440660745,0.992651440660745)))
REPRESENTATION_ITEM('')
SURFACE()
);
#1419=(
BOUNDED_SURFACE()
B_SPLINE_SURFACE(1,2,((#117711,#117712,#117713,#117714,#117715),(#117716,
#117717,#117718,#117719,#117720)),.UNSPECIFIED.,.F.,.F.,.F.)
B_SPLINE_SURFACE_WITH_KNOTS((2,2),(3,2,3),(0.709598828802843,1.),(0.245359920959965,
0.245954053070909,0.263201868951015),.UNSPECIFIED.)
GEOMETRIC_REPRESENTATION_ITEM()
RATIONAL_B_SPLINE_SURFACE(((0.987624841600687,0.987624841600687,0.987624841600687,
0.986938988894508,0.989176916802452),(0.987624841600687,0.987624841600687,
0.987624841600687,0.986938988894508,0.989176916802452)))
REPRESENTATION_ITEM('')
SURFACE()
);
#1420=(
BOUNDED_SURFACE()
B_SPLINE_SURFACE(1,2,((#117728,#117729,#117730,#117731,#117732),(#117733,
#117734,#117735,#117736,#117737)),.UNSPECIFIED.,.F.,.F.,.F.)
B_SPLINE_SURFACE_WITH_KNOTS((2,2),(3,2,3),(0.710318915640075,1.),(0.469916319328035,
0.487259899888158,0.487433335693759),.UNSPECIFIED.)
GEOMETRIC_REPRESENTATION_ITEM()
RATIONAL_B_SPLINE_SURFACE(((0.987775548376701,0.988735325500096,0.992651440660745,
0.992651440660745,0.992651440660745),(0.987775548376701,0.988735325500096,
0.992651440660745,0.992651440660745,0.992651440660745)))
REPRESENTATION_ITEM('')
SURFACE()
);
#1421=(
BOUNDED_SURFACE()
B_SPLINE_SURFACE(1,2,((#117748,#117749,#117750,#117751,#117752),(#117753,
#117754,#117755,#117756,#117757)),.UNSPECIFIED.,.F.,.F.,.F.)
B_SPLINE_SURFACE_WITH_KNOTS((2,2),(3,2,3),(0.709598828791051,1.),(0.245359920947667,
0.245954053070909,0.263201868951015),.UNSPECIFIED.)
GEOMETRIC_REPRESENTATION_ITEM()
RATIONAL_B_SPLINE_SURFACE(((0.987624841600687,0.987624841600687,0.987624841600687,
0.986938988894508,0.989176916802452),(0.987624841600687,0.987624841600687,
0.987624841600687,0.986938988894508,0.989176916802452)))
REPRESENTATION_ITEM('')
SURFACE()
);
#1422=(
BOUNDED_SURFACE()
B_SPLINE_SURFACE(1,2,((#117765,#117766,#117767,#117768,#117769),(#117770,
#117771,#117772,#117773,#117774)),.UNSPECIFIED.,.F.,.F.,.F.)
B_SPLINE_SURFACE_WITH_KNOTS((2,2),(3,2,3),(0.710318915639492,1.),(0.469916319328035,
0.487259899888158,0.487433335693759),.UNSPECIFIED.)
GEOMETRIC_REPRESENTATION_ITEM()
RATIONAL_B_SPLINE_SURFACE(((0.987775548376701,0.988735325500096,0.992651440660745,
0.992651440660745,0.992651440660745),(0.987775548376701,0.988735325500096,
0.992651440660745,0.992651440660745,0.992651440660745)))
REPRESENTATION_ITEM('')
SURFACE()
);
#1423=(
BOUNDED_SURFACE()
B_SPLINE_SURFACE(1,2,((#117785,#117786,#117787,#117788,#117789),(#117790,
#117791,#117792,#117793,#117794)),.UNSPECIFIED.,.F.,.F.,.F.)
B_SPLINE_SURFACE_WITH_KNOTS((2,2),(3,2,3),(0.709598828800151,1.),(0.245359920957343,
0.245954053070909,0.263201868951015),.UNSPECIFIED.)
GEOMETRIC_REPRESENTATION_ITEM()
RATIONAL_B_SPLINE_SURFACE(((0.987624841600687,0.987624841600687,0.987624841600687,
0.986938988894508,0.989176916802452),(0.987624841600687,0.987624841600687,
0.987624841600687,0.986938988894508,0.989176916802452)))
REPRESENTATION_ITEM('')
SURFACE()
);
#1424=(
BOUNDED_SURFACE()
B_SPLINE_SURFACE(1,2,((#117802,#117803,#117804,#117805,#117806),(#117807,
#117808,#117809,#117810,#117811)),.UNSPECIFIED.,.F.,.F.,.F.)
B_SPLINE_SURFACE_WITH_KNOTS((2,2),(3,2,3),(0.710318915640001,1.),(0.469916319328036,
0.487259899888158,0.487433335693759),.UNSPECIFIED.)
GEOMETRIC_REPRESENTATION_ITEM()
RATIONAL_B_SPLINE_SURFACE(((0.987775548376701,0.988735325500096,0.992651440660745,
0.992651440660745,0.992651440660745),(0.987775548376701,0.988735325500096,
0.992651440660745,0.992651440660745,0.992651440660745)))
REPRESENTATION_ITEM('')
SURFACE()
);
#1425=(
BOUNDED_SURFACE()
B_SPLINE_SURFACE(1,2,((#117822,#117823,#117824,#117825,#117826),(#117827,
#117828,#117829,#117830,#117831)),.UNSPECIFIED.,.F.,.F.,.F.)
B_SPLINE_SURFACE_WITH_KNOTS((2,2),(3,2,3),(0.709598828766692,1.),(0.245359920923563,
0.245954053070907,0.263201868951014),.UNSPECIFIED.)
GEOMETRIC_REPRESENTATION_ITEM()
RATIONAL_B_SPLINE_SURFACE(((0.987624841600687,0.987624841600687,0.987624841600687,
0.986938988894508,0.989176916802452),(0.987624841600687,0.987624841600687,
0.987624841600687,0.986938988894508,0.989176916802452)))
REPRESENTATION_ITEM('')
SURFACE()
);
#1426=(
BOUNDED_SURFACE()
B_SPLINE_SURFACE(1,2,((#117839,#117840,#117841,#117842,#117843),(#117844,
#117845,#117846,#117847,#117848)),.UNSPECIFIED.,.F.,.F.,.F.)
B_SPLINE_SURFACE_WITH_KNOTS((2,2),(3,2,3),(0.710318915640006,1.),(0.469916319328036,
0.487259899888159,0.48743333569376),.UNSPECIFIED.)
GEOMETRIC_REPRESENTATION_ITEM()
RATIONAL_B_SPLINE_SURFACE(((0.987775548376701,0.988735325500096,0.992651440660746,
0.992651440660746,0.992651440660746),(0.987775548376701,0.988735325500096,
0.992651440660746,0.992651440660746,0.992651440660746)))
REPRESENTATION_ITEM('')
SURFACE()
);
#1427=(
BOUNDED_SURFACE()
B_SPLINE_SURFACE(1,2,((#117859,#117860,#117861,#117862,#117863),(#117864,
#117865,#117866,#117867,#117868)),.UNSPECIFIED.,.F.,.F.,.F.)
B_SPLINE_SURFACE_WITH_KNOTS((2,2),(3,2,3),(0.70959882880507,1.),(0.245359920961868,
0.245954053070908,0.263201868951014),.UNSPECIFIED.)
GEOMETRIC_REPRESENTATION_ITEM()
RATIONAL_B_SPLINE_SURFACE(((0.987624841600687,0.987624841600687,0.987624841600687,
0.986938988894508,0.989176916802451),(0.987624841600687,0.987624841600687,
0.987624841600687,0.986938988894508,0.989176916802451)))
REPRESENTATION_ITEM('')
SURFACE()
);
#1428=(
BOUNDED_SURFACE()
B_SPLINE_SURFACE(1,2,((#117876,#117877,#117878,#117879,#117880),(#117881,
#117882,#117883,#117884,#117885)),.UNSPECIFIED.,.F.,.F.,.F.)
B_SPLINE_SURFACE_WITH_KNOTS((2,2),(3,2,3),(0.710318915639408,1.),(0.469916319328036,
0.487259899888159,0.48743333569376),.UNSPECIFIED.)
GEOMETRIC_REPRESENTATION_ITEM()
RATIONAL_B_SPLINE_SURFACE(((0.987775548376701,0.988735325500096,0.992651440660746,
0.992651440660746,0.992651440660746),(0.987775548376701,0.988735325500096,
0.992651440660746,0.992651440660746,0.992651440660746)))
REPRESENTATION_ITEM('')
SURFACE()
);
#1429=(
BOUNDED_SURFACE()
B_SPLINE_SURFACE(1,2,((#117896,#117897,#117898,#117899,#117900),(#117901,
#117902,#117903,#117904,#117905)),.UNSPECIFIED.,.F.,.F.,.F.)
B_SPLINE_SURFACE_WITH_KNOTS((2,2),(3,2,3),(0.709598828765639,1.),(0.245359920923153,
0.245954053070907,0.263201868951014),.UNSPECIFIED.)
GEOMETRIC_REPRESENTATION_ITEM()
RATIONAL_B_SPLINE_SURFACE(((0.987624841600687,0.987624841600687,0.987624841600687,
0.986938988894508,0.989176916802452),(0.987624841600687,0.987624841600687,
0.987624841600687,0.986938988894508,0.989176916802452)))
REPRESENTATION_ITEM('')
SURFACE()
);
#1430=(
BOUNDED_SURFACE()
B_SPLINE_SURFACE(1,2,((#117913,#117914,#117915,#117916,#117917),(#117918,
#117919,#117920,#117921,#117922)),.UNSPECIFIED.,.F.,.F.,.F.)
B_SPLINE_SURFACE_WITH_KNOTS((2,2),(3,2,3),(0.710318915639994,1.),(0.469916319328036,
0.487259899888159,0.48743333569376),.UNSPECIFIED.)
GEOMETRIC_REPRESENTATION_ITEM()
RATIONAL_B_SPLINE_SURFACE(((0.987775548376701,0.988735325500096,0.992651440660746,
0.992651440660746,0.992651440660746),(0.987775548376701,0.988735325500096,
0.992651440660746,0.992651440660746,0.992651440660746)))
REPRESENTATION_ITEM('')
SURFACE()
);
#1431=(
BOUNDED_SURFACE()
B_SPLINE_SURFACE(1,2,((#117933,#117934,#117935,#117936,#117937),(#117938,
#117939,#117940,#117941,#117942)),.UNSPECIFIED.,.F.,.F.,.F.)
B_SPLINE_SURFACE_WITH_KNOTS((2,2),(3,2,3),(0.709598828795369,1.),(0.245359920952099,
0.245954053070907,0.263201868951014),.UNSPECIFIED.)
GEOMETRIC_REPRESENTATION_ITEM()
RATIONAL_B_SPLINE_SURFACE(((0.987624841600687,0.987624841600687,0.987624841600687,
0.986938988894507,0.989176916802451),(0.987624841600687,0.987624841600687,
0.987624841600687,0.986938988894507,0.989176916802451)))
REPRESENTATION_ITEM('')
SURFACE()
);
#1432=(
BOUNDED_SURFACE()
B_SPLINE_SURFACE(1,2,((#117950,#117951,#117952,#117953,#117954),(#117955,
#117956,#117957,#117958,#117959)),.UNSPECIFIED.,.F.,.F.,.F.)
B_SPLINE_SURFACE_WITH_KNOTS((2,2),(3,2,3),(0.710318915639496,1.),(0.469916319328036,
0.487259899888159,0.48743333569376),.UNSPECIFIED.)
GEOMETRIC_REPRESENTATION_ITEM()
RATIONAL_B_SPLINE_SURFACE(((0.987775548376701,0.988735325500096,0.992651440660745,
0.992651440660745,0.992651440660745),(0.987775548376701,0.988735325500096,
0.992651440660745,0.992651440660745,0.992651440660745)))
REPRESENTATION_ITEM('')
SURFACE()
);
#1433=(
BOUNDED_SURFACE()
B_SPLINE_SURFACE(1,2,((#117970,#117971,#117972,#117973,#117974),(#117975,
#117976,#117977,#117978,#117979)),.UNSPECIFIED.,.F.,.F.,.F.)
B_SPLINE_SURFACE_WITH_KNOTS((2,2),(3,2,3),(0.709598828793834,1.),(0.245359920950977,
0.245954053070907,0.263201868951014),.UNSPECIFIED.)
GEOMETRIC_REPRESENTATION_ITEM()
RATIONAL_B_SPLINE_SURFACE(((0.987624841600687,0.987624841600687,0.987624841600687,
0.986938988894507,0.989176916802451),(0.987624841600687,0.987624841600687,
0.987624841600687,0.986938988894507,0.989176916802451)))
REPRESENTATION_ITEM('')
SURFACE()
);
#1434=(
BOUNDED_SURFACE()
B_SPLINE_SURFACE(1,2,((#117987,#117988,#117989,#117990,#117991),(#117992,
#117993,#117994,#117995,#117996)),.UNSPECIFIED.,.F.,.F.,.F.)
B_SPLINE_SURFACE_WITH_KNOTS((2,2),(3,2,3),(0.71031891563999,1.),(0.469916319328036,
0.48725989988816,0.487433335693761),.UNSPECIFIED.)
GEOMETRIC_REPRESENTATION_ITEM()
RATIONAL_B_SPLINE_SURFACE(((0.987775548376701,0.988735325500096,0.992651440660746,
0.992651440660746,0.992651440660746),(0.987775548376701,0.988735325500096,
0.992651440660746,0.992651440660746,0.992651440660746)))
REPRESENTATION_ITEM('')
SURFACE()
);
#1435=(
BOUNDED_SURFACE()
B_SPLINE_SURFACE(1,2,((#118007,#118008,#118009,#118010,#118011),(#118012,
#118013,#118014,#118015,#118016)),.UNSPECIFIED.,.F.,.F.,.F.)
B_SPLINE_SURFACE_WITH_KNOTS((2,2),(3,2,3),(0.709598828771055,1.),(0.245359920927963,
0.245954053070907,0.263201868951014),.UNSPECIFIED.)
GEOMETRIC_REPRESENTATION_ITEM()
RATIONAL_B_SPLINE_SURFACE(((0.987624841600687,0.987624841600687,0.987624841600687,
0.986938988894508,0.989176916802452),(0.987624841600687,0.987624841600687,
0.987624841600687,0.986938988894508,0.989176916802452)))
REPRESENTATION_ITEM('')
SURFACE()
);
#1436=(
BOUNDED_SURFACE()
B_SPLINE_SURFACE(1,2,((#118024,#118025,#118026,#118027,#118028),(#118029,
#118030,#118031,#118032,#118033)),.UNSPECIFIED.,.F.,.F.,.F.)
B_SPLINE_SURFACE_WITH_KNOTS((2,2),(3,2,3),(0.710318915639492,1.),(0.469916319328036,
0.487259899888159,0.48743333569376),.UNSPECIFIED.)
GEOMETRIC_REPRESENTATION_ITEM()
RATIONAL_B_SPLINE_SURFACE(((0.987775548376701,0.988735325500096,0.992651440660745,
0.992651440660745,0.992651440660745),(0.987775548376701,0.988735325500096,
0.992651440660745,0.992651440660745,0.992651440660745)))
REPRESENTATION_ITEM('')
SURFACE()
);
#1437=(
BOUNDED_SURFACE()
B_SPLINE_SURFACE(1,2,((#118044,#118045,#118046,#118047,#118048),(#118049,
#118050,#118051,#118052,#118053)),.UNSPECIFIED.,.F.,.F.,.F.)
B_SPLINE_SURFACE_WITH_KNOTS((2,2),(3,2,3),(0.709598828793346,1.),(0.2453599209506,
0.245954053070908,0.263201868951014),.UNSPECIFIED.)
GEOMETRIC_REPRESENTATION_ITEM()
RATIONAL_B_SPLINE_SURFACE(((0.987624841600687,0.987624841600687,0.987624841600687,
0.986938988894507,0.989176916802451),(0.987624841600687,0.987624841600687,
0.987624841600687,0.986938988894507,0.989176916802451)))
REPRESENTATION_ITEM('')
SURFACE()
);
#1438=(
BOUNDED_SURFACE()
B_SPLINE_SURFACE(1,2,((#118061,#118062,#118063,#118064,#118065),(#118066,
#118067,#118068,#118069,#118070)),.UNSPECIFIED.,.F.,.F.,.F.)
B_SPLINE_SURFACE_WITH_KNOTS((2,2),(3,2,3),(0.71031891563972,1.),(0.469916319328036,
0.487259899888159,0.48743333569376),.UNSPECIFIED.)
GEOMETRIC_REPRESENTATION_ITEM()
RATIONAL_B_SPLINE_SURFACE(((0.987775548376701,0.988735325500096,0.992651440660746,
0.992651440660746,0.992651440660746),(0.987775548376701,0.988735325500096,
0.992651440660746,0.992651440660746,0.992651440660746)))
REPRESENTATION_ITEM('')
SURFACE()
);
#1439=(
BOUNDED_SURFACE()
B_SPLINE_SURFACE(1,2,((#118081,#118082,#118083,#118084,#118085),(#118086,
#118087,#118088,#118089,#118090)),.UNSPECIFIED.,.F.,.F.,.F.)
B_SPLINE_SURFACE_WITH_KNOTS((2,2),(3,2,3),(0.709598828778751,1.),(0.24535992093593,
0.245954053070907,0.263201868951014),.UNSPECIFIED.)
GEOMETRIC_REPRESENTATION_ITEM()
RATIONAL_B_SPLINE_SURFACE(((0.987624841600687,0.987624841600687,0.987624841600687,
0.986938988894508,0.989176916802452),(0.987624841600687,0.987624841600687,
0.987624841600687,0.986938988894508,0.989176916802452)))
REPRESENTATION_ITEM('')
SURFACE()
);
#1440=(
BOUNDED_SURFACE()
B_SPLINE_SURFACE(1,2,((#118098,#118099,#118100,#118101,#118102),(#118103,
#118104,#118105,#118106,#118107)),.UNSPECIFIED.,.F.,.F.,.F.)
B_SPLINE_SURFACE_WITH_KNOTS((2,2),(3,2,3),(0.710318915638677,1.),(0.469916319328036,
0.487259899888159,0.48743333569376),.UNSPECIFIED.)
GEOMETRIC_REPRESENTATION_ITEM()
RATIONAL_B_SPLINE_SURFACE(((0.987775548376701,0.988735325500096,0.992651440660746,
0.992651440660746,0.992651440660746),(0.987775548376701,0.988735325500096,
0.992651440660746,0.992651440660746,0.992651440660746)))
REPRESENTATION_ITEM('')
SURFACE()
);
#1441=(
BOUNDED_SURFACE()
B_SPLINE_SURFACE(1,2,((#118118,#118119,#118120,#118121,#118122),(#118123,
#118124,#118125,#118126,#118127)),.UNSPECIFIED.,.F.,.F.,.F.)
B_SPLINE_SURFACE_WITH_KNOTS((2,2),(3,2,3),(0.709598828786485,1.),(0.245359920944462,
0.245954053070907,0.263201868951014),.UNSPECIFIED.)
GEOMETRIC_REPRESENTATION_ITEM()
RATIONAL_B_SPLINE_SURFACE(((0.987624841600687,0.987624841600687,0.987624841600687,
0.986938988894508,0.989176916802452),(0.987624841600687,0.987624841600687,
0.987624841600687,0.986938988894507,0.989176916802451)))
REPRESENTATION_ITEM('')
SURFACE()
);
#1442=(
BOUNDED_SURFACE()
B_SPLINE_SURFACE(1,2,((#118135,#118136,#118137,#118138,#118139),(#118140,
#118141,#118142,#118143,#118144)),.UNSPECIFIED.,.F.,.F.,.F.)
B_SPLINE_SURFACE_WITH_KNOTS((2,2),(3,2,3),(0.710318915639962,1.),(0.469916319328036,
0.487259899888159,0.48743333569376),.UNSPECIFIED.)
GEOMETRIC_REPRESENTATION_ITEM()
RATIONAL_B_SPLINE_SURFACE(((0.987775548376701,0.988735325500096,0.992651440660746,
0.992651440660746,0.992651440660746),(0.987775548376701,0.988735325500096,
0.992651440660746,0.992651440660746,0.992651440660746)))
REPRESENTATION_ITEM('')
SURFACE()
);
#1443=(
BOUNDED_SURFACE()
B_SPLINE_SURFACE(1,2,((#118155,#118156,#118157,#118158,#118159),(#118160,
#118161,#118162,#118163,#118164)),.UNSPECIFIED.,.F.,.F.,.F.)
B_SPLINE_SURFACE_WITH_KNOTS((2,2),(3,2,3),(0.709598828781523,1.),(0.245359920938325,
0.245954053070907,0.263201868951014),.UNSPECIFIED.)
GEOMETRIC_REPRESENTATION_ITEM()
RATIONAL_B_SPLINE_SURFACE(((0.987624841600687,0.987624841600687,0.987624841600687,
0.986938988894508,0.989176916802452),(0.987624841600687,0.987624841600687,
0.987624841600687,0.986938988894508,0.989176916802452)))
REPRESENTATION_ITEM('')
SURFACE()
);
#1444=(
BOUNDED_SURFACE()
B_SPLINE_SURFACE(1,2,((#118172,#118173,#118174,#118175,#118176),(#118177,
#118178,#118179,#118180,#118181)),.UNSPECIFIED.,.F.,.F.,.F.)
B_SPLINE_SURFACE_WITH_KNOTS((2,2),(3,2,3),(0.710318915640078,1.),(0.469916319328036,
0.487259899888159,0.48743333569376),.UNSPECIFIED.)
GEOMETRIC_REPRESENTATION_ITEM()
RATIONAL_B_SPLINE_SURFACE(((0.987775548376701,0.988735325500096,0.992651440660746,
0.992651440660746,0.992651440660746),(0.987775548376701,0.988735325500096,
0.992651440660746,0.992651440660746,0.992651440660746)))
REPRESENTATION_ITEM('')
SURFACE()
);
#1445=(
BOUNDED_SURFACE()
B_SPLINE_SURFACE(1,2,((#118192,#118193,#118194,#118195,#118196),(#118197,
#118198,#118199,#118200,#118201)),.UNSPECIFIED.,.F.,.F.,.F.)
B_SPLINE_SURFACE_WITH_KNOTS((2,2),(3,2,3),(0.70959882878374,1.),(0.245359920940315,
0.245954053070907,0.263201868951014),.UNSPECIFIED.)
GEOMETRIC_REPRESENTATION_ITEM()
RATIONAL_B_SPLINE_SURFACE(((0.987624841600687,0.987624841600687,0.987624841600687,
0.986938988894507,0.989176916802451),(0.987624841600687,0.987624841600687,
0.987624841600687,0.986938988894507,0.989176916802451)))
REPRESENTATION_ITEM('')
SURFACE()
);
#1446=(
BOUNDED_SURFACE()
B_SPLINE_SURFACE(1,2,((#118209,#118210,#118211,#118212,#118213),(#118214,
#118215,#118216,#118217,#118218)),.UNSPECIFIED.,.F.,.F.,.F.)
B_SPLINE_SURFACE_WITH_KNOTS((2,2),(3,2,3),(0.710318915639442,1.),(0.469916319328036,
0.487259899888159,0.48743333569376),.UNSPECIFIED.)
GEOMETRIC_REPRESENTATION_ITEM()
RATIONAL_B_SPLINE_SURFACE(((0.987775548376701,0.988735325500096,0.992651440660746,
0.992651440660746,0.992651440660746),(0.987775548376701,0.988735325500096,
0.992651440660746,0.992651440660746,0.992651440660746)))
REPRESENTATION_ITEM('')
SURFACE()
);
#1447=(
BOUNDED_SURFACE()
B_SPLINE_SURFACE(1,2,((#118229,#118230,#118231,#118232,#118233),(#118234,
#118235,#118236,#118237,#118238)),.UNSPECIFIED.,.F.,.F.,.F.)
B_SPLINE_SURFACE_WITH_KNOTS((2,2),(3,2,3),(0.70959882881485,1.),(0.245359920972021,
0.245954053070907,0.263201868951014),.UNSPECIFIED.)
GEOMETRIC_REPRESENTATION_ITEM()
RATIONAL_B_SPLINE_SURFACE(((0.987624841600687,0.987624841600687,0.987624841600687,
0.986938988894507,0.989176916802451),(0.987624841600687,0.987624841600687,
0.987624841600687,0.986938988894507,0.989176916802451)))
REPRESENTATION_ITEM('')
SURFACE()
);
#1448=(
BOUNDED_SURFACE()
B_SPLINE_SURFACE(1,2,((#118246,#118247,#118248,#118249,#118250),(#118251,
#118252,#118253,#118254,#118255)),.UNSPECIFIED.,.F.,.F.,.F.)
B_SPLINE_SURFACE_WITH_KNOTS((2,2),(3,2,3),(0.710318915640074,1.),(0.469916319328036,
0.487259899888159,0.48743333569376),.UNSPECIFIED.)
GEOMETRIC_REPRESENTATION_ITEM()
RATIONAL_B_SPLINE_SURFACE(((0.987775548376701,0.988735325500096,0.992651440660746,
0.992651440660746,0.992651440660746),(0.987775548376701,0.988735325500096,
0.992651440660746,0.992651440660746,0.992651440660746)))
REPRESENTATION_ITEM('')
SURFACE()
);
#1449=(
BOUNDED_SURFACE()
B_SPLINE_SURFACE(1,2,((#118266,#118267,#118268,#118269,#118270),(#118271,
#118272,#118273,#118274,#118275)),.UNSPECIFIED.,.F.,.F.,.F.)
B_SPLINE_SURFACE_WITH_KNOTS((2,2),(3,2,3),(0.709598828775925,1.),(0.245359920932689,
0.245954053070907,0.263201868951013),.UNSPECIFIED.)
GEOMETRIC_REPRESENTATION_ITEM()
RATIONAL_B_SPLINE_SURFACE(((0.987624841600687,0.987624841600687,0.987624841600687,
0.986938988894507,0.989176916802451),(0.987624841600687,0.987624841600687,
0.987624841600687,0.986938988894507,0.989176916802451)))
REPRESENTATION_ITEM('')
SURFACE()
);
#1450=(
BOUNDED_SURFACE()
B_SPLINE_SURFACE(1,2,((#118283,#118284,#118285,#118286,#118287),(#118288,
#118289,#118290,#118291,#118292)),.UNSPECIFIED.,.F.,.F.,.F.)
B_SPLINE_SURFACE_WITH_KNOTS((2,2),(3,2,3),(0.710318915638945,1.),(0.469916319328036,
0.487259899888159,0.48743333569376),.UNSPECIFIED.)
GEOMETRIC_REPRESENTATION_ITEM()
RATIONAL_B_SPLINE_SURFACE(((0.987775548376701,0.988735325500096,0.992651440660746,
0.992651440660746,0.992651440660746),(0.987775548376701,0.988735325500096,
0.992651440660746,0.992651440660746,0.992651440660746)))
REPRESENTATION_ITEM('')
SURFACE()
);
#1451=(
BOUNDED_SURFACE()
B_SPLINE_SURFACE(1,2,((#118303,#118304,#118305,#118306,#118307),(#118308,
#118309,#118310,#118311,#118312)),.UNSPECIFIED.,.F.,.F.,.F.)
B_SPLINE_SURFACE_WITH_KNOTS((2,2),(3,2,3),(0.709598828783652,1.),(0.245359920941388,
0.245954053070907,0.263201868951014),.UNSPECIFIED.)
GEOMETRIC_REPRESENTATION_ITEM()
RATIONAL_B_SPLINE_SURFACE(((0.987624841600687,0.987624841600687,0.987624841600687,
0.986938988894507,0.989176916802451),(0.987624841600687,0.987624841600687,
0.987624841600687,0.986938988894507,0.989176916802451)))
REPRESENTATION_ITEM('')
SURFACE()
);
#1452=(
BOUNDED_SURFACE()
B_SPLINE_SURFACE(1,2,((#118320,#118321,#118322,#118323,#118324),(#118325,
#118326,#118327,#118328,#118329)),.UNSPECIFIED.,.F.,.F.,.F.)
B_SPLINE_SURFACE_WITH_KNOTS((2,2),(3,2,3),(0.710318915639109,1.),(0.469916319328036,
0.487259899888159,0.48743333569376),.UNSPECIFIED.)
GEOMETRIC_REPRESENTATION_ITEM()
RATIONAL_B_SPLINE_SURFACE(((0.987775548376701,0.988735325500096,0.992651440660746,
0.992651440660746,0.992651440660746),(0.987775548376701,0.988735325500096,
0.992651440660746,0.992651440660746,0.992651440660746)))
REPRESENTATION_ITEM('')
SURFACE()
);
#1453=(
BOUNDED_SURFACE()
B_SPLINE_SURFACE(1,2,((#118340,#118341,#118342,#118343,#118344),(#118345,
#118346,#118347,#118348,#118349)),.UNSPECIFIED.,.F.,.F.,.F.)
B_SPLINE_SURFACE_WITH_KNOTS((2,2),(3,2,3),(0.709598828772429,1.),(0.245359920930035,
0.245954053070907,0.263201868951013),.UNSPECIFIED.)
GEOMETRIC_REPRESENTATION_ITEM()
RATIONAL_B_SPLINE_SURFACE(((0.987624841600687,0.987624841600687,0.987624841600687,
0.986938988894508,0.989176916802452),(0.987624841600687,0.987624841600687,
0.987624841600687,0.986938988894508,0.989176916802452)))
REPRESENTATION_ITEM('')
SURFACE()
);
#1454=(
BOUNDED_SURFACE()
B_SPLINE_SURFACE(1,2,((#118357,#118358,#118359,#118360,#118361),(#118362,
#118363,#118364,#118365,#118366)),.UNSPECIFIED.,.F.,.F.,.F.)
B_SPLINE_SURFACE_WITH_KNOTS((2,2),(3,2,3),(0.710318915638385,1.),(0.469916319328036,
0.487259899888159,0.48743333569376),.UNSPECIFIED.)
GEOMETRIC_REPRESENTATION_ITEM()
RATIONAL_B_SPLINE_SURFACE(((0.987775548376701,0.988735325500096,0.992651440660746,
0.992651440660746,0.992651440660746),(0.987775548376701,0.988735325500096,
0.992651440660746,0.992651440660746,0.992651440660746)))
REPRESENTATION_ITEM('')
SURFACE()
);
#1455=(
BOUNDED_SURFACE()
B_SPLINE_SURFACE(1,2,((#118374,#118375,#118376,#118377,#118378),(#118379,
#118380,#118381,#118382,#118383)),.UNSPECIFIED.,.F.,.F.,.F.)
B_SPLINE_SURFACE_WITH_KNOTS((2,2),(3,2,3),(0.709598828798267,1.),(0.245359920956622,
0.245954053070907,0.263201868951013),.UNSPECIFIED.)
GEOMETRIC_REPRESENTATION_ITEM()
RATIONAL_B_SPLINE_SURFACE(((0.987624841600687,0.987624841600687,0.987624841600687,
0.986938988894507,0.989176916802451),(0.987624841600687,0.987624841600687,
0.987624841600687,0.986938988894507,0.989176916802451)))
REPRESENTATION_ITEM('')
SURFACE()
);
#1456=(
BOUNDED_SURFACE()
B_SPLINE_SURFACE(1,2,((#118385,#118386,#118387,#118388,#118389),(#118390,
#118391,#118392,#118393,#118394)),.UNSPECIFIED.,.F.,.F.,.F.)
B_SPLINE_SURFACE_WITH_KNOTS((2,2),(3,2,3),(0.71031891563988,1.),(0.469916319328036,
0.487259899888159,0.48743333569376),.UNSPECIFIED.)
GEOMETRIC_REPRESENTATION_ITEM()
RATIONAL_B_SPLINE_SURFACE(((0.987775548376701,0.988735325500096,0.992651440660746,
0.992651440660746,0.992651440660746),(0.987775548376701,0.988735325500096,
0.992651440660746,0.992651440660746,0.992651440660746)))
REPRESENTATION_ITEM('')
SURFACE()
);
#1457=(
BOUNDED_SURFACE()
B_SPLINE_SURFACE(1,2,((#118405,#118406,#118407,#118408,#118409),(#118410,
#118411,#118412,#118413,#118414)),.UNSPECIFIED.,.F.,.F.,.F.)
B_SPLINE_SURFACE_WITH_KNOTS((2,2),(3,2,3),(0.70959882880242,1.),(0.245359920959295,
0.245954053070907,0.263201868951013),.UNSPECIFIED.)
GEOMETRIC_REPRESENTATION_ITEM()
RATIONAL_B_SPLINE_SURFACE(((0.987624841600687,0.987624841600687,0.987624841600687,
0.986938988894507,0.989176916802451),(0.987624841600687,0.987624841600687,
0.987624841600687,0.986938988894507,0.989176916802451)))
REPRESENTATION_ITEM('')
SURFACE()
);
#1458=(
BOUNDED_SURFACE()
B_SPLINE_SURFACE(1,2,((#118422,#118423,#118424,#118425,#118426),(#118427,
#118428,#118429,#118430,#118431)),.UNSPECIFIED.,.F.,.F.,.F.)
B_SPLINE_SURFACE_WITH_KNOTS((2,2),(3,2,3),(0.710318915638591,1.),(0.469916319328036,
0.487259899888159,0.48743333569376),.UNSPECIFIED.)
GEOMETRIC_REPRESENTATION_ITEM()
RATIONAL_B_SPLINE_SURFACE(((0.987775548376701,0.988735325500096,0.992651440660746,
0.992651440660746,0.992651440660746),(0.987775548376701,0.988735325500096,
0.992651440660746,0.992651440660746,0.992651440660746)))
REPRESENTATION_ITEM('')
SURFACE()
);
#1459=(
BOUNDED_SURFACE()
B_SPLINE_SURFACE(1,2,((#118442,#118443,#118444,#118445,#118446),(#118447,
#118448,#118449,#118450,#118451)),.UNSPECIFIED.,.F.,.F.,.F.)
B_SPLINE_SURFACE_WITH_KNOTS((2,2),(3,2,3),(0.709598828781214,1.),(0.245359920939413,
0.245954053070907,0.263201868951017),.UNSPECIFIED.)
GEOMETRIC_REPRESENTATION_ITEM()
RATIONAL_B_SPLINE_SURFACE(((0.987624841600687,0.987624841600687,0.987624841600687,
0.986938988894507,0.989176916802452),(0.987624841600687,0.987624841600687,
0.987624841600687,0.986938988894507,0.989176916802452)))
REPRESENTATION_ITEM('')
SURFACE()
);
#1460=(
BOUNDED_SURFACE()
B_SPLINE_SURFACE(1,2,((#118459,#118460,#118461,#118462,#118463),(#118464,
#118465,#118466,#118467,#118468)),.UNSPECIFIED.,.F.,.F.,.F.)
B_SPLINE_SURFACE_WITH_KNOTS((2,2),(3,2,3),(0.710318915638836,1.),(0.469916319328036,
0.487259899888159,0.48743333569376),.UNSPECIFIED.)
GEOMETRIC_REPRESENTATION_ITEM()
RATIONAL_B_SPLINE_SURFACE(((0.987775548376701,0.988735325500096,0.992651440660746,
0.992651440660746,0.992651440660746),(0.987775548376701,0.988735325500096,
0.992651440660746,0.992651440660746,0.992651440660746)))
REPRESENTATION_ITEM('')
SURFACE()
);
#1461=(
BOUNDED_SURFACE()
B_SPLINE_SURFACE(1,2,((#118479,#118480,#118481,#118482,#118483),(#118484,
#118485,#118486,#118487,#118488)),.UNSPECIFIED.,.F.,.F.,.F.)
B_SPLINE_SURFACE_WITH_KNOTS((2,2),(3,2,3),(0.709598828784904,1.),(0.245359920942991,
0.245954053070907,0.263201868951015),.UNSPECIFIED.)
GEOMETRIC_REPRESENTATION_ITEM()
RATIONAL_B_SPLINE_SURFACE(((0.987624841600687,0.987624841600687,0.987624841600687,
0.986938988894507,0.989176916802452),(0.987624841600687,0.987624841600687,
0.987624841600687,0.986938988894507,0.989176916802452)))
REPRESENTATION_ITEM('')
SURFACE()
);
#1462=(
BOUNDED_SURFACE()
B_SPLINE_SURFACE(1,2,((#118496,#118497,#118498,#118499,#118500),(#118501,
#118502,#118503,#118504,#118505)),.UNSPECIFIED.,.F.,.F.,.F.)
B_SPLINE_SURFACE_WITH_KNOTS((2,2),(3,2,3),(0.710318915639086,1.),(0.469916319328036,
0.487259899888159,0.48743333569376),.UNSPECIFIED.)
GEOMETRIC_REPRESENTATION_ITEM()
RATIONAL_B_SPLINE_SURFACE(((0.987775548376701,0.988735325500096,0.992651440660746,
0.992651440660746,0.992651440660746),(0.987775548376701,0.988735325500096,
0.992651440660746,0.992651440660746,0.992651440660746)))
REPRESENTATION_ITEM('')
SURFACE()
);
#1463=(
BOUNDED_SURFACE()
B_SPLINE_SURFACE(1,2,((#118516,#118517,#118518,#118519,#118520),(#118521,
#118522,#118523,#118524,#118525)),.UNSPECIFIED.,.F.,.F.,.F.)
B_SPLINE_SURFACE_WITH_KNOTS((2,2),(3,2,3),(0.709598828779162,1.),(0.245359920936906,
0.245954053070907,0.263201868951013),.UNSPECIFIED.)
GEOMETRIC_REPRESENTATION_ITEM()
RATIONAL_B_SPLINE_SURFACE(((0.987624841600687,0.987624841600687,0.987624841600687,
0.986938988894507,0.989176916802451),(0.987624841600687,0.987624841600687,
0.987624841600687,0.986938988894507,0.989176916802451)))
REPRESENTATION_ITEM('')
SURFACE()
);
#1464=(
BOUNDED_SURFACE()
B_SPLINE_SURFACE(1,2,((#118533,#118534,#118535,#118536,#118537),(#118538,
#118539,#118540,#118541,#118542)),.UNSPECIFIED.,.F.,.F.,.F.)
B_SPLINE_SURFACE_WITH_KNOTS((2,2),(3,2,3),(0.710318915639156,1.),(0.469916319328036,
0.487259899888159,0.48743333569376),.UNSPECIFIED.)
GEOMETRIC_REPRESENTATION_ITEM()
RATIONAL_B_SPLINE_SURFACE(((0.987775548376701,0.988735325500096,0.992651440660746,
0.992651440660746,0.992651440660746),(0.987775548376701,0.988735325500096,
0.992651440660746,0.992651440660746,0.992651440660746)))
REPRESENTATION_ITEM('')
SURFACE()
);
#1465=(
BOUNDED_SURFACE()
B_SPLINE_SURFACE(1,2,((#118553,#118554,#118555,#118556,#118557),(#118558,
#118559,#118560,#118561,#118562)),.UNSPECIFIED.,.F.,.F.,.F.)
B_SPLINE_SURFACE_WITH_KNOTS((2,2),(3,2,3),(0.709598828805424,1.),(0.245359920963013,
0.245954053070908,0.263201868951014),.UNSPECIFIED.)
GEOMETRIC_REPRESENTATION_ITEM()
RATIONAL_B_SPLINE_SURFACE(((0.987624841600687,0.987624841600687,0.987624841600687,
0.986938988894508,0.989176916802451),(0.987624841600687,0.987624841600687,
0.987624841600687,0.986938988894508,0.989176916802451)))
REPRESENTATION_ITEM('')
SURFACE()
);
#1466=(
BOUNDED_SURFACE()
B_SPLINE_SURFACE(1,2,((#118570,#118571,#118572,#118573,#118574),(#118575,
#118576,#118577,#118578,#118579)),.UNSPECIFIED.,.F.,.F.,.F.)
B_SPLINE_SURFACE_WITH_KNOTS((2,2),(3,2,3),(0.71031891563883,1.),(0.469916319328036,
0.487259899888161,0.487433335693762),.UNSPECIFIED.)
GEOMETRIC_REPRESENTATION_ITEM()
RATIONAL_B_SPLINE_SURFACE(((0.987775548376701,0.988735325500096,0.992651440660746,
0.992651440660746,0.992651440660746),(0.987775548376701,0.988735325500096,
0.992651440660746,0.992651440660746,0.992651440660746)))
REPRESENTATION_ITEM('')
SURFACE()
);
#1467=(
BOUNDED_SURFACE()
B_SPLINE_SURFACE(1,2,((#118590,#118591,#118592,#118593,#118594),(#118595,
#118596,#118597,#118598,#118599)),.UNSPECIFIED.,.F.,.F.,.F.)
B_SPLINE_SURFACE_WITH_KNOTS((2,2),(3,2,3),(0.709598828788555,1.),(0.24535992094641,
0.245954053070899,0.263201868951014),.UNSPECIFIED.)
GEOMETRIC_REPRESENTATION_ITEM()
RATIONAL_B_SPLINE_SURFACE(((0.987624841600687,0.987624841600687,0.987624841600687,
0.986938988894506,0.989176916802451),(0.987624841600687,0.987624841600687,
0.987624841600687,0.986938988894506,0.989176916802451)))
REPRESENTATION_ITEM('')
SURFACE()
);
#1468=(
BOUNDED_SURFACE()
B_SPLINE_SURFACE(1,2,((#118607,#118608,#118609,#118610,#118611),(#118612,
#118613,#118614,#118615,#118616)),.UNSPECIFIED.,.F.,.F.,.F.)
B_SPLINE_SURFACE_WITH_KNOTS((2,2),(3,2,3),(0.710318915638989,1.),(0.469916319328036,
0.487259899888159,0.48743333569376),.UNSPECIFIED.)
GEOMETRIC_REPRESENTATION_ITEM()
RATIONAL_B_SPLINE_SURFACE(((0.987775548376701,0.988735325500096,0.992651440660746,
0.992651440660746,0.992651440660746),(0.987775548376701,0.988735325500096,
0.992651440660746,0.992651440660746,0.992651440660746)))
REPRESENTATION_ITEM('')
SURFACE()
);
#1469=(
BOUNDED_SURFACE()
B_SPLINE_SURFACE(1,2,((#118627,#118628,#118629,#118630,#118631),(#118632,
#118633,#118634,#118635,#118636)),.UNSPECIFIED.,.F.,.F.,.F.)
B_SPLINE_SURFACE_WITH_KNOTS((2,2),(3,2,3),(0.709598828800189,1.),(0.24535992095796,
0.245954053070909,0.263201868951013),.UNSPECIFIED.)
GEOMETRIC_REPRESENTATION_ITEM()
RATIONAL_B_SPLINE_SURFACE(((0.987624841600687,0.987624841600687,0.987624841600687,
0.986938988894508,0.989176916802452),(0.987624841600687,0.987624841600687,
0.987624841600687,0.986938988894508,0.989176916802452)))
REPRESENTATION_ITEM('')
SURFACE()
);
#1470=(
BOUNDED_SURFACE()
B_SPLINE_SURFACE(1,2,((#118644,#118645,#118646),(#118647,#118648,#118649)),
 .UNSPECIFIED.,.F.,.F.,.F.)
B_SPLINE_SURFACE_WITH_KNOTS((2,2),(3,3),(0.710192959008021,1.),(0.435775021682622,
0.453027768259469),.UNSPECIFIED.)
GEOMETRIC_REPRESENTATION_ITEM()
RATIONAL_B_SPLINE_SURFACE(((0.995452950231063,0.990618550266714,0.988709602819327),
(0.995452950231063,0.990618550266714,0.988709602819327)))
REPRESENTATION_ITEM('')
SURFACE()
);
#1471=(
BOUNDED_SURFACE()
B_SPLINE_SURFACE(1,2,((#118658,#118659,#118660,#118661,#118662),(#118663,
#118664,#118665,#118666,#118667)),.UNSPECIFIED.,.F.,.F.,.F.)
B_SPLINE_SURFACE_WITH_KNOTS((2,2),(3,2,3),(0.710318915639671,1.),(0.280328542633765,
0.285714285714286,0.297856505190614),.UNSPECIFIED.)
GEOMETRIC_REPRESENTATION_ITEM()
RATIONAL_B_SPLINE_SURFACE(((0.996504189652446,0.998109554471267,1.,0.995737968897747,
0.992924952273132),(0.996504189652447,0.998109554471267,1.,0.995737968897747,
0.992924952273132)))
REPRESENTATION_ITEM('')
SURFACE()
);
#1472=(
BOUNDED_SURFACE()
B_SPLINE_SURFACE(1,2,((#118678,#118679,#118680),(#118681,#118682,#118683)),
 .UNSPECIFIED.,.F.,.F.,.F.)
B_SPLINE_SURFACE_WITH_KNOTS((2,2),(3,3),(0.710192959008101,1.),(0.435775021682622,
0.453027768259469),.UNSPECIFIED.)
GEOMETRIC_REPRESENTATION_ITEM()
RATIONAL_B_SPLINE_SURFACE(((0.995452950231063,0.990618550266714,0.988709602819327),
(0.995452950231063,0.990618550266714,0.988709602819327)))
REPRESENTATION_ITEM('')
SURFACE()
);
#1473=(
BOUNDED_SURFACE()
B_SPLINE_SURFACE(1,2,((#118692,#118693,#118694,#118695,#118696),(#118697,
#118698,#118699,#118700,#118701)),.UNSPECIFIED.,.F.,.F.,.F.)
B_SPLINE_SURFACE_WITH_KNOTS((2,2),(3,2,3),(0.710318915639747,1.),(0.280328542633765,
0.285714285714286,0.297856505190613),.UNSPECIFIED.)
GEOMETRIC_REPRESENTATION_ITEM()
RATIONAL_B_SPLINE_SURFACE(((0.996504189652446,0.998109554471267,1.,0.995737968897747,
0.992924952273132),(0.996504189652447,0.998109554471267,1.,0.995737968897747,
0.992924952273132)))
REPRESENTATION_ITEM('')
SURFACE()
);
#1474=(
BOUNDED_SURFACE()
B_SPLINE_SURFACE(1,2,((#118712,#118713,#118714),(#118715,#118716,#118717)),
 .UNSPECIFIED.,.F.,.F.,.F.)
B_SPLINE_SURFACE_WITH_KNOTS((2,2),(3,3),(0.71019295900799,1.),(0.43577502168215,
0.453027768259472),.UNSPECIFIED.)
GEOMETRIC_REPRESENTATION_ITEM()
RATIONAL_B_SPLINE_SURFACE(((0.995452950231328,0.990618550266766,0.988709602819326),
(0.995452950231328,0.990618550266766,0.988709602819326)))
REPRESENTATION_ITEM('')
SURFACE()
);
#1475=(
BOUNDED_SURFACE()
B_SPLINE_SURFACE(1,2,((#118726,#118727,#118728,#118729,#118730),(#118731,
#118732,#118733,#118734,#118735)),.UNSPECIFIED.,.F.,.F.,.F.)
B_SPLINE_SURFACE_WITH_KNOTS((2,2),(3,2,3),(0.710318915639631,1.),(0.280328542633765,
0.285714285714286,0.297856505190614),.UNSPECIFIED.)
GEOMETRIC_REPRESENTATION_ITEM()
RATIONAL_B_SPLINE_SURFACE(((0.996504189652446,0.998109554471267,1.,0.995737968897747,
0.992924952273132),(0.996504189652446,0.998109554471267,1.,0.995737968897747,
0.992924952273132)))
REPRESENTATION_ITEM('')
SURFACE()
);
#1476=(
BOUNDED_SURFACE()
B_SPLINE_SURFACE(1,2,((#118746,#118747,#118748),(#118749,#118750,#118751)),
 .UNSPECIFIED.,.F.,.F.,.F.)
B_SPLINE_SURFACE_WITH_KNOTS((2,2),(3,3),(0.710192959007314,1.),(0.435775021682621,
0.453027768259469),.UNSPECIFIED.)
GEOMETRIC_REPRESENTATION_ITEM()
RATIONAL_B_SPLINE_SURFACE(((0.995452950231063,0.990618550266714,0.988709602819327),
(0.995452950231063,0.990618550266714,0.988709602819327)))
REPRESENTATION_ITEM('')
SURFACE()
);
#1477=(
BOUNDED_SURFACE()
B_SPLINE_SURFACE(1,2,((#118760,#118761,#118762,#118763,#118764),(#118765,
#118766,#118767,#118768,#118769)),.UNSPECIFIED.,.F.,.F.,.F.)
B_SPLINE_SURFACE_WITH_KNOTS((2,2),(3,2,3),(0.710318915638957,1.),(0.280328542633765,
0.285714285714286,0.297856505190614),.UNSPECIFIED.)
GEOMETRIC_REPRESENTATION_ITEM()
RATIONAL_B_SPLINE_SURFACE(((0.996504189652447,0.998109554471267,1.,0.995737968897747,
0.992924952273132),(0.996504189652447,0.998109554471267,1.,0.995737968897747,
0.992924952273132)))
REPRESENTATION_ITEM('')
SURFACE()
);
#1478=(
BOUNDED_SURFACE()
B_SPLINE_SURFACE(1,2,((#118780,#118781,#118782),(#118783,#118784,#118785)),
 .UNSPECIFIED.,.F.,.F.,.F.)
B_SPLINE_SURFACE_WITH_KNOTS((2,2),(3,3),(0.710192959007467,1.),(0.435775021682622,
0.453027768259469),.UNSPECIFIED.)
GEOMETRIC_REPRESENTATION_ITEM()
RATIONAL_B_SPLINE_SURFACE(((0.995452950231063,0.990618550266714,0.988709602819327),
(0.995452950231063,0.990618550266714,0.988709602819327)))
REPRESENTATION_ITEM('')
SURFACE()
);
#1479=(
BOUNDED_SURFACE()
B_SPLINE_SURFACE(1,2,((#118794,#118795,#118796,#118797,#118798),(#118799,
#118800,#118801,#118802,#118803)),.UNSPECIFIED.,.F.,.F.,.F.)
B_SPLINE_SURFACE_WITH_KNOTS((2,2),(3,2,3),(0.710318915639107,1.),(0.280328542633765,
0.285714285714286,0.297856505190614),.UNSPECIFIED.)
GEOMETRIC_REPRESENTATION_ITEM()
RATIONAL_B_SPLINE_SURFACE(((0.996504189652447,0.998109554471267,1.,0.995737968897747,
0.992924952273132),(0.996504189652447,0.998109554471267,1.,0.995737968897747,
0.992924952273132)))
REPRESENTATION_ITEM('')
SURFACE()
);
#1480=(
BOUNDED_SURFACE()
B_SPLINE_SURFACE(1,2,((#118814,#118815,#118816),(#118817,#118818,#118819)),
 .UNSPECIFIED.,.F.,.F.,.F.)
B_SPLINE_SURFACE_WITH_KNOTS((2,2),(3,3),(0.710192959007502,1.),(0.435775021682622,
0.453027768259469),.UNSPECIFIED.)
GEOMETRIC_REPRESENTATION_ITEM()
RATIONAL_B_SPLINE_SURFACE(((0.995452950231063,0.990618550266714,0.988709602819327),
(0.995452950231063,0.990618550266714,0.988709602819327)))
REPRESENTATION_ITEM('')
SURFACE()
);
#1481=(
BOUNDED_SURFACE()
B_SPLINE_SURFACE(1,2,((#118828,#118829,#118830,#118831,#118832),(#118833,
#118834,#118835,#118836,#118837)),.UNSPECIFIED.,.F.,.F.,.F.)
B_SPLINE_SURFACE_WITH_KNOTS((2,2),(3,2,3),(0.710318915639146,1.),(0.280328542633765,
0.285714285714286,0.297856505190614),.UNSPECIFIED.)
GEOMETRIC_REPRESENTATION_ITEM()
RATIONAL_B_SPLINE_SURFACE(((0.996504189652446,0.998109554471267,1.,0.995737968897747,
0.992924952273132),(0.996504189652446,0.998109554471267,1.,0.995737968897747,
0.992924952273132)))
REPRESENTATION_ITEM('')
SURFACE()
);
#1482=(
BOUNDED_SURFACE()
B_SPLINE_SURFACE(1,2,((#118848,#118849,#118850),(#118851,#118852,#118853)),
 .UNSPECIFIED.,.F.,.F.,.F.)
B_SPLINE_SURFACE_WITH_KNOTS((2,2),(3,3),(0.710192959007325,1.),(0.435775021682622,
0.453027768259469),.UNSPECIFIED.)
GEOMETRIC_REPRESENTATION_ITEM()
RATIONAL_B_SPLINE_SURFACE(((0.995452950231063,0.990618550266714,0.988709602819327),
(0.995452950231063,0.990618550266714,0.988709602819327)))
REPRESENTATION_ITEM('')
SURFACE()
);
#1483=(
BOUNDED_SURFACE()
B_SPLINE_SURFACE(1,2,((#118862,#118863,#118864,#118865,#118866),(#118867,
#118868,#118869,#118870,#118871)),.UNSPECIFIED.,.F.,.F.,.F.)
B_SPLINE_SURFACE_WITH_KNOTS((2,2),(3,2,3),(0.710318915638968,1.),(0.280328542633765,
0.285714285714286,0.297856505190614),.UNSPECIFIED.)
GEOMETRIC_REPRESENTATION_ITEM()
RATIONAL_B_SPLINE_SURFACE(((0.996504189652446,0.998109554471267,1.,0.995737968897747,
0.992924952273132),(0.996504189652446,0.998109554471267,1.,0.995737968897747,
0.992924952273132)))
REPRESENTATION_ITEM('')
SURFACE()
);
#1484=(
BOUNDED_SURFACE()
B_SPLINE_SURFACE(1,2,((#118882,#118883,#118884),(#118885,#118886,#118887)),
 .UNSPECIFIED.,.F.,.F.,.F.)
B_SPLINE_SURFACE_WITH_KNOTS((2,2),(3,3),(0.710192959008261,1.),(0.435775021682622,
0.453027768259469),.UNSPECIFIED.)
GEOMETRIC_REPRESENTATION_ITEM()
RATIONAL_B_SPLINE_SURFACE(((0.995452950231063,0.990618550266714,0.988709602819327),
(0.995452950231063,0.990618550266714,0.988709602819327)))
REPRESENTATION_ITEM('')
SURFACE()
);
#1485=(
BOUNDED_SURFACE()
B_SPLINE_SURFACE(1,2,((#118896,#118897,#118898,#118899,#118900),(#118901,
#118902,#118903,#118904,#118905)),.UNSPECIFIED.,.F.,.F.,.F.)
B_SPLINE_SURFACE_WITH_KNOTS((2,2),(3,2,3),(0.7103189156399,1.),(0.280328542633765,
0.285714285714286,0.297856505190614),.UNSPECIFIED.)
GEOMETRIC_REPRESENTATION_ITEM()
RATIONAL_B_SPLINE_SURFACE(((0.996504189652446,0.998109554471267,1.,0.995737968897747,
0.992924952273132),(0.996504189652446,0.998109554471267,1.,0.995737968897747,
0.992924952273132)))
REPRESENTATION_ITEM('')
SURFACE()
);
#1486=(
BOUNDED_SURFACE()
B_SPLINE_SURFACE(1,2,((#118916,#118917,#118918),(#118919,#118920,#118921)),
 .UNSPECIFIED.,.F.,.F.,.F.)
B_SPLINE_SURFACE_WITH_KNOTS((2,2),(3,3),(0.710192959008251,1.),(0.435775021682622,
0.453027768259469),.UNSPECIFIED.)
GEOMETRIC_REPRESENTATION_ITEM()
RATIONAL_B_SPLINE_SURFACE(((0.995452950231063,0.990618550266714,0.988709602819327),
(0.995452950231063,0.990618550266714,0.988709602819327)))
REPRESENTATION_ITEM('')
SURFACE()
);
#1487=(
BOUNDED_SURFACE()
B_SPLINE_SURFACE(1,2,((#118930,#118931,#118932,#118933,#118934),(#118935,
#118936,#118937,#118938,#118939)),.UNSPECIFIED.,.F.,.F.,.F.)
B_SPLINE_SURFACE_WITH_KNOTS((2,2),(3,2,3),(0.710318915639895,1.),(0.280328542633765,
0.285714285714286,0.297856505190614),.UNSPECIFIED.)
GEOMETRIC_REPRESENTATION_ITEM()
RATIONAL_B_SPLINE_SURFACE(((0.996504189652446,0.998109554471267,1.,0.995737968897747,
0.992924952273132),(0.996504189652446,0.998109554471267,1.,0.995737968897747,
0.992924952273132)))
REPRESENTATION_ITEM('')
SURFACE()
);
#1488=(
BOUNDED_SURFACE()
B_SPLINE_SURFACE(1,2,((#118950,#118951,#118952),(#118953,#118954,#118955)),
 .UNSPECIFIED.,.F.,.F.,.F.)
B_SPLINE_SURFACE_WITH_KNOTS((2,2),(3,3),(0.710192959008144,1.),(0.435775021682622,
0.453027768259469),.UNSPECIFIED.)
GEOMETRIC_REPRESENTATION_ITEM()
RATIONAL_B_SPLINE_SURFACE(((0.995452950231063,0.990618550266714,0.988709602819327),
(0.995452950231063,0.990618550266714,0.988709602819327)))
REPRESENTATION_ITEM('')
SURFACE()
);
#1489=(
BOUNDED_SURFACE()
B_SPLINE_SURFACE(1,2,((#118964,#118965,#118966,#118967,#118968),(#118969,
#118970,#118971,#118972,#118973)),.UNSPECIFIED.,.F.,.F.,.F.)
B_SPLINE_SURFACE_WITH_KNOTS((2,2),(3,2,3),(0.710318915639317,1.),(0.280328542633765,
0.285714285714286,0.297856505190614),.UNSPECIFIED.)
GEOMETRIC_REPRESENTATION_ITEM()
RATIONAL_B_SPLINE_SURFACE(((0.996504189652446,0.998109554471267,1.,0.995737968897747,
0.992924952273132),(0.996504189652446,0.998109554471267,1.,0.995737968897747,
0.992924952273132)))
REPRESENTATION_ITEM('')
SURFACE()
);
#1490=(
BOUNDED_SURFACE()
B_SPLINE_SURFACE(1,2,((#118984,#118985,#118986),(#118987,#118988,#118989)),
 .UNSPECIFIED.,.F.,.F.,.F.)
B_SPLINE_SURFACE_WITH_KNOTS((2,2),(3,3),(0.710192959008211,1.),(0.435775021682622,
0.453027768259469),.UNSPECIFIED.)
GEOMETRIC_REPRESENTATION_ITEM()
RATIONAL_B_SPLINE_SURFACE(((0.995452950231063,0.990618550266714,0.988709602819327),
(0.995452950231063,0.990618550266714,0.988709602819327)))
REPRESENTATION_ITEM('')
SURFACE()
);
#1491=(
BOUNDED_SURFACE()
B_SPLINE_SURFACE(1,2,((#118998,#118999,#119000,#119001,#119002),(#119003,
#119004,#119005,#119006,#119007)),.UNSPECIFIED.,.F.,.F.,.F.)
B_SPLINE_SURFACE_WITH_KNOTS((2,2),(3,2,3),(0.710318915639847,1.),(0.280328542633765,
0.285714285714286,0.297856505190614),.UNSPECIFIED.)
GEOMETRIC_REPRESENTATION_ITEM()
RATIONAL_B_SPLINE_SURFACE(((0.996504189652446,0.998109554471267,1.,0.995737968897747,
0.992924952273132),(0.996504189652446,0.998109554471267,1.,0.995737968897747,
0.992924952273132)))
REPRESENTATION_ITEM('')
SURFACE()
);
#1492=(
BOUNDED_SURFACE()
B_SPLINE_SURFACE(1,2,((#119018,#119019,#119020),(#119021,#119022,#119023)),
 .UNSPECIFIED.,.F.,.F.,.F.)
B_SPLINE_SURFACE_WITH_KNOTS((2,2),(3,3),(0.710192959008243,1.),(0.435775021682622,
0.453027768259469),.UNSPECIFIED.)
GEOMETRIC_REPRESENTATION_ITEM()
RATIONAL_B_SPLINE_SURFACE(((0.995452950231063,0.990618550266714,0.988709602819327),
(0.995452950231063,0.990618550266714,0.988709602819327)))
REPRESENTATION_ITEM('')
SURFACE()
);
#1493=(
BOUNDED_SURFACE()
B_SPLINE_SURFACE(1,2,((#119032,#119033,#119034,#119035,#119036),(#119037,
#119038,#119039,#119040,#119041)),.UNSPECIFIED.,.F.,.F.,.F.)
B_SPLINE_SURFACE_WITH_KNOTS((2,2),(3,2,3),(0.710318915639875,1.),(0.280328542633765,
0.285714285714286,0.297856505190614),.UNSPECIFIED.)
GEOMETRIC_REPRESENTATION_ITEM()
RATIONAL_B_SPLINE_SURFACE(((0.996504189652446,0.998109554471267,1.,0.995737968897747,
0.992924952273132),(0.996504189652446,0.998109554471267,1.,0.995737968897747,
0.992924952273132)))
REPRESENTATION_ITEM('')
SURFACE()
);
#1494=(
BOUNDED_SURFACE()
B_SPLINE_SURFACE(1,2,((#119052,#119053,#119054),(#119055,#119056,#119057)),
 .UNSPECIFIED.,.F.,.F.,.F.)
B_SPLINE_SURFACE_WITH_KNOTS((2,2),(3,3),(0.71019295900829,1.),(0.435775021682622,
0.453027768259469),.UNSPECIFIED.)
GEOMETRIC_REPRESENTATION_ITEM()
RATIONAL_B_SPLINE_SURFACE(((0.995452950231063,0.990618550266714,0.988709602819327),
(0.995452950231063,0.990618550266714,0.988709602819327)))
REPRESENTATION_ITEM('')
SURFACE()
);
#1495=(
BOUNDED_SURFACE()
B_SPLINE_SURFACE(1,2,((#119066,#119067,#119068,#119069,#119070),(#119071,
#119072,#119073,#119074,#119075)),.UNSPECIFIED.,.F.,.F.,.F.)
B_SPLINE_SURFACE_WITH_KNOTS((2,2),(3,2,3),(0.710318915639929,1.),(0.280328542633765,
0.285714285714286,0.297856505190614),.UNSPECIFIED.)
GEOMETRIC_REPRESENTATION_ITEM()
RATIONAL_B_SPLINE_SURFACE(((0.996504189652446,0.998109554471267,1.,0.995737968897747,
0.992924952273132),(0.996504189652447,0.998109554471267,1.,0.995737968897747,
0.992924952273132)))
REPRESENTATION_ITEM('')
SURFACE()
);
#1496=(
BOUNDED_SURFACE()
B_SPLINE_SURFACE(1,2,((#119086,#119087,#119088),(#119089,#119090,#119091)),
 .UNSPECIFIED.,.F.,.F.,.F.)
B_SPLINE_SURFACE_WITH_KNOTS((2,2),(3,3),(0.710192959008439,1.),(0.435775021682622,
0.453027768259469),.UNSPECIFIED.)
GEOMETRIC_REPRESENTATION_ITEM()
RATIONAL_B_SPLINE_SURFACE(((0.995452950231063,0.990618550266714,0.988709602819327),
(0.995452950231063,0.990618550266714,0.988709602819327)))
REPRESENTATION_ITEM('')
SURFACE()
);
#1497=(
BOUNDED_SURFACE()
B_SPLINE_SURFACE(1,2,((#119100,#119101,#119102,#119103,#119104),(#119105,
#119106,#119107,#119108,#119109)),.UNSPECIFIED.,.F.,.F.,.F.)
B_SPLINE_SURFACE_WITH_KNOTS((2,2),(3,2,3),(0.710318915640072,1.),(0.280328542633765,
0.285714285714286,0.297856505190614),.UNSPECIFIED.)
GEOMETRIC_REPRESENTATION_ITEM()
RATIONAL_B_SPLINE_SURFACE(((0.996504189652447,0.998109554471267,1.,0.995737968897747,
0.992924952273132),(0.996504189652447,0.998109554471267,1.,0.995737968897747,
0.992924952273132)))
REPRESENTATION_ITEM('')
SURFACE()
);
#1498=(
BOUNDED_SURFACE()
B_SPLINE_SURFACE(1,2,((#119120,#119121,#119122),(#119123,#119124,#119125)),
 .UNSPECIFIED.,.F.,.F.,.F.)
B_SPLINE_SURFACE_WITH_KNOTS((2,2),(3,3),(0.710192959008441,1.),(0.435775021682622,
0.453027768259469),.UNSPECIFIED.)
GEOMETRIC_REPRESENTATION_ITEM()
RATIONAL_B_SPLINE_SURFACE(((0.995452950231063,0.990618550266714,0.988709602819327),
(0.995452950231063,0.990618550266714,0.988709602819327)))
REPRESENTATION_ITEM('')
SURFACE()
);
#1499=(
BOUNDED_SURFACE()
B_SPLINE_SURFACE(1,2,((#119134,#119135,#119136,#119137,#119138),(#119139,
#119140,#119141,#119142,#119143)),.UNSPECIFIED.,.F.,.F.,.F.)
B_SPLINE_SURFACE_WITH_KNOTS((2,2),(3,2,3),(0.710318915640079,1.),(0.280328542633765,
0.285714285714286,0.297856505190614),.UNSPECIFIED.)
GEOMETRIC_REPRESENTATION_ITEM()
RATIONAL_B_SPLINE_SURFACE(((0.996504189652446,0.998109554471267,1.,0.995737968897747,
0.992924952273132),(0.996504189652447,0.998109554471267,1.,0.995737968897747,
0.992924952273132)))
REPRESENTATION_ITEM('')
SURFACE()
);
#1500=(
BOUNDED_SURFACE()
B_SPLINE_SURFACE(1,2,((#119154,#119155,#119156),(#119157,#119158,#119159)),
 .UNSPECIFIED.,.F.,.F.,.F.)
B_SPLINE_SURFACE_WITH_KNOTS((2,2),(3,3),(0.710192959008438,1.),(0.435775021682622,
0.453027768259469),.UNSPECIFIED.)
GEOMETRIC_REPRESENTATION_ITEM()
RATIONAL_B_SPLINE_SURFACE(((0.995452950231063,0.990618550266714,0.988709602819327),
(0.995452950231063,0.990618550266714,0.988709602819327)))
REPRESENTATION_ITEM('')
SURFACE()
);
#1501=(
BOUNDED_SURFACE()
B_SPLINE_SURFACE(1,2,((#119168,#119169,#119170,#119171,#119172),(#119173,
#119174,#119175,#119176,#119177)),.UNSPECIFIED.,.F.,.F.,.F.)
B_SPLINE_SURFACE_WITH_KNOTS((2,2),(3,2,3),(0.710318915640069,1.),(0.280328542633765,
0.285714285714286,0.297856505190614),.UNSPECIFIED.)
GEOMETRIC_REPRESENTATION_ITEM()
RATIONAL_B_SPLINE_SURFACE(((0.996504189652446,0.998109554471267,1.,0.995737968897747,
0.992924952273132),(0.996504189652446,0.998109554471267,1.,0.995737968897747,
0.992924952273132)))
REPRESENTATION_ITEM('')
SURFACE()
);
#1502=(
BOUNDED_SURFACE()
B_SPLINE_SURFACE(1,2,((#119188,#119189,#119190),(#119191,#119192,#119193)),
 .UNSPECIFIED.,.F.,.F.,.F.)
B_SPLINE_SURFACE_WITH_KNOTS((2,2),(3,3),(0.710192959008439,1.),(0.435775021682622,
0.453027768259469),.UNSPECIFIED.)
GEOMETRIC_REPRESENTATION_ITEM()
RATIONAL_B_SPLINE_SURFACE(((0.995452950231063,0.990618550266714,0.988709602819327),
(0.995452950231063,0.990618550266714,0.988709602819327)))
REPRESENTATION_ITEM('')
SURFACE()
);
#1503=(
BOUNDED_SURFACE()
B_SPLINE_SURFACE(1,2,((#119202,#119203,#119204,#119205,#119206),(#119207,
#119208,#119209,#119210,#119211)),.UNSPECIFIED.,.F.,.F.,.F.)
B_SPLINE_SURFACE_WITH_KNOTS((2,2),(3,2,3),(0.710318915640078,1.),(0.280328542633765,
0.285714285714286,0.297856505190614),.UNSPECIFIED.)
GEOMETRIC_REPRESENTATION_ITEM()
RATIONAL_B_SPLINE_SURFACE(((0.996504189652446,0.998109554471267,1.,0.995737968897747,
0.992924952273132),(0.996504189652446,0.998109554471267,1.,0.995737968897747,
0.992924952273132)))
REPRESENTATION_ITEM('')
SURFACE()
);
#1504=(
BOUNDED_SURFACE()
B_SPLINE_SURFACE(1,2,((#119222,#119223,#119224),(#119225,#119226,#119227)),
 .UNSPECIFIED.,.F.,.F.,.F.)
B_SPLINE_SURFACE_WITH_KNOTS((2,2),(3,3),(0.710192959008441,1.),(0.435775021682622,
0.453027768259469),.UNSPECIFIED.)
GEOMETRIC_REPRESENTATION_ITEM()
RATIONAL_B_SPLINE_SURFACE(((0.995452950231063,0.990618550266714,0.988709602819327),
(0.995452950231063,0.990618550266714,0.988709602819327)))
REPRESENTATION_ITEM('')
SURFACE()
);
#1505=(
BOUNDED_SURFACE()
B_SPLINE_SURFACE(1,2,((#119236,#119237,#119238,#119239,#119240),(#119241,
#119242,#119243,#119244,#119245)),.UNSPECIFIED.,.F.,.F.,.F.)
B_SPLINE_SURFACE_WITH_KNOTS((2,2),(3,2,3),(0.710318915640079,1.),(0.280328542633765,
0.285714285714286,0.297856505190614),.UNSPECIFIED.)
GEOMETRIC_REPRESENTATION_ITEM()
RATIONAL_B_SPLINE_SURFACE(((0.996504189652446,0.998109554471267,1.,0.995737968897747,
0.992924952273132),(0.996504189652447,0.998109554471267,1.,0.995737968897747,
0.992924952273132)))
REPRESENTATION_ITEM('')
SURFACE()
);
#1506=(
BOUNDED_SURFACE()
B_SPLINE_SURFACE(1,2,((#119256,#119257,#119258),(#119259,#119260,#119261)),
 .UNSPECIFIED.,.F.,.F.,.F.)
B_SPLINE_SURFACE_WITH_KNOTS((2,2),(3,3),(0.710192959008329,1.),(0.435775021682622,
0.453027768259469),.UNSPECIFIED.)
GEOMETRIC_REPRESENTATION_ITEM()
RATIONAL_B_SPLINE_SURFACE(((0.995452950231063,0.990618550266714,0.988709602819327),
(0.995452950231063,0.990618550266714,0.988709602819327)))
REPRESENTATION_ITEM('')
SURFACE()
);
#1507=(
BOUNDED_SURFACE()
B_SPLINE_SURFACE(1,2,((#119270,#119271,#119272,#119273,#119274),(#119275,
#119276,#119277,#119278,#119279)),.UNSPECIFIED.,.F.,.F.,.F.)
B_SPLINE_SURFACE_WITH_KNOTS((2,2),(3,2,3),(0.710318915639972,1.),(0.280328542633765,
0.285714285714286,0.297856505190614),.UNSPECIFIED.)
GEOMETRIC_REPRESENTATION_ITEM()
RATIONAL_B_SPLINE_SURFACE(((0.996504189652447,0.998109554471267,1.,0.995737968897747,
0.992924952273132),(0.996504189652447,0.998109554471267,1.,0.995737968897747,
0.992924952273132)))
REPRESENTATION_ITEM('')
SURFACE()
);
#1508=(
BOUNDED_SURFACE()
B_SPLINE_SURFACE(1,2,((#119290,#119291,#119292),(#119293,#119294,#119295)),
 .UNSPECIFIED.,.F.,.F.,.F.)
B_SPLINE_SURFACE_WITH_KNOTS((2,2),(3,3),(0.710192959007031,1.),(0.435775021682622,
0.453027768259469),.UNSPECIFIED.)
GEOMETRIC_REPRESENTATION_ITEM()
RATIONAL_B_SPLINE_SURFACE(((0.995452950231063,0.990618550266714,0.988709602819327),
(0.995452950231063,0.990618550266714,0.988709602819327)))
REPRESENTATION_ITEM('')
SURFACE()
);
#1509=(
BOUNDED_SURFACE()
B_SPLINE_SURFACE(1,2,((#119304,#119305,#119306,#119307,#119308),(#119309,
#119310,#119311,#119312,#119313)),.UNSPECIFIED.,.F.,.F.,.F.)
B_SPLINE_SURFACE_WITH_KNOTS((2,2),(3,2,3),(0.710318915638671,1.),(0.280328542633765,
0.285714285714286,0.297856505190614),.UNSPECIFIED.)
GEOMETRIC_REPRESENTATION_ITEM()
RATIONAL_B_SPLINE_SURFACE(((0.996504189652446,0.998109554471267,1.,0.995737968897747,
0.992924952273132),(0.996504189652446,0.998109554471267,1.,0.995737968897747,
0.992924952273132)))
REPRESENTATION_ITEM('')
SURFACE()
);
#1510=(
BOUNDED_SURFACE()
B_SPLINE_SURFACE(1,2,((#119324,#119325,#119326),(#119327,#119328,#119329)),
 .UNSPECIFIED.,.F.,.F.,.F.)
B_SPLINE_SURFACE_WITH_KNOTS((2,2),(3,3),(0.710192959008183,1.),(0.435775021682622,
0.453027768259469),.UNSPECIFIED.)
GEOMETRIC_REPRESENTATION_ITEM()
RATIONAL_B_SPLINE_SURFACE(((0.995452950231063,0.990618550266714,0.988709602819327),
(0.995452950231063,0.990618550266714,0.988709602819327)))
REPRESENTATION_ITEM('')
SURFACE()
);
#1511=(
BOUNDED_SURFACE()
B_SPLINE_SURFACE(1,2,((#119338,#119339,#119340,#119341,#119342),(#119343,
#119344,#119345,#119346,#119347)),.UNSPECIFIED.,.F.,.F.,.F.)
B_SPLINE_SURFACE_WITH_KNOTS((2,2),(3,2,3),(0.710318915639824,1.),(0.280328542633765,
0.285714285714286,0.297856505190614),.UNSPECIFIED.)
GEOMETRIC_REPRESENTATION_ITEM()
RATIONAL_B_SPLINE_SURFACE(((0.996504189652447,0.998109554471267,1.,0.995737968897747,
0.992924952273132),(0.996504189652447,0.998109554471267,1.,0.995737968897747,
0.992924952273132)))
REPRESENTATION_ITEM('')
SURFACE()
);
#1512=(
BOUNDED_SURFACE()
B_SPLINE_SURFACE(1,2,((#119358,#119359,#119360),(#119361,#119362,#119363)),
 .UNSPECIFIED.,.F.,.F.,.F.)
B_SPLINE_SURFACE_WITH_KNOTS((2,2),(3,3),(0.710192959008437,1.),(0.435775021682622,
0.453027768259469),.UNSPECIFIED.)
GEOMETRIC_REPRESENTATION_ITEM()
RATIONAL_B_SPLINE_SURFACE(((0.995452950231063,0.990618550266714,0.988709602819327),
(0.995452950231063,0.990618550266714,0.988709602819327)))
REPRESENTATION_ITEM('')
SURFACE()
);
#1513=(
BOUNDED_SURFACE()
B_SPLINE_SURFACE(1,2,((#119372,#119373,#119374,#119375,#119376),(#119377,
#119378,#119379,#119380,#119381)),.UNSPECIFIED.,.F.,.F.,.F.)
B_SPLINE_SURFACE_WITH_KNOTS((2,2),(3,2,3),(0.710318915640082,1.),(0.280328542633765,
0.285714285714286,0.297856505190614),.UNSPECIFIED.)
GEOMETRIC_REPRESENTATION_ITEM()
RATIONAL_B_SPLINE_SURFACE(((0.996504189652447,0.998109554471267,1.,0.995737968897747,
0.992924952273132),(0.996504189652447,0.998109554471267,1.,0.995737968897747,
0.992924952273132)))
REPRESENTATION_ITEM('')
SURFACE()
);
#1514=(
BOUNDED_SURFACE()
B_SPLINE_SURFACE(1,2,((#119392,#119393,#119394),(#119395,#119396,#119397)),
 .UNSPECIFIED.,.F.,.F.,.F.)
B_SPLINE_SURFACE_WITH_KNOTS((2,2),(3,3),(0.71019295900844,1.),(0.435775021682622,
0.453027768259469),.UNSPECIFIED.)
GEOMETRIC_REPRESENTATION_ITEM()
RATIONAL_B_SPLINE_SURFACE(((0.995452950231063,0.990618550266714,0.988709602819327),
(0.995452950231063,0.990618550266714,0.988709602819327)))
REPRESENTATION_ITEM('')
SURFACE()
);
#1515=(
BOUNDED_SURFACE()
B_SPLINE_SURFACE(1,2,((#119406,#119407,#119408,#119409,#119410),(#119411,
#119412,#119413,#119414,#119415)),.UNSPECIFIED.,.F.,.F.,.F.)
B_SPLINE_SURFACE_WITH_KNOTS((2,2),(3,2,3),(0.710318915640079,1.),(0.280328542633765,
0.285714285714286,0.297856505190614),.UNSPECIFIED.)
GEOMETRIC_REPRESENTATION_ITEM()
RATIONAL_B_SPLINE_SURFACE(((0.996504189652446,0.998109554471267,1.,0.995737968897747,
0.992924952273132),(0.996504189652447,0.998109554471267,1.,0.995737968897747,
0.992924952273132)))
REPRESENTATION_ITEM('')
SURFACE()
);
#1516=(
BOUNDED_SURFACE()
B_SPLINE_SURFACE(1,2,((#119426,#119427,#119428),(#119429,#119430,#119431)),
 .UNSPECIFIED.,.F.,.F.,.F.)
B_SPLINE_SURFACE_WITH_KNOTS((2,2),(3,3),(0.710192959008364,1.),(0.435775021682622,
0.453027768259468),.UNSPECIFIED.)
GEOMETRIC_REPRESENTATION_ITEM()
RATIONAL_B_SPLINE_SURFACE(((0.995452950231063,0.990618550266715,0.988709602819327),
(0.995452950231063,0.990618550266715,0.988709602819327)))
REPRESENTATION_ITEM('')
SURFACE()
);
#1517=(
BOUNDED_SURFACE()
B_SPLINE_SURFACE(1,2,((#119440,#119441,#119442,#119443,#119444),(#119445,
#119446,#119447,#119448,#119449)),.UNSPECIFIED.,.F.,.F.,.F.)
B_SPLINE_SURFACE_WITH_KNOTS((2,2),(3,2,3),(0.710318915640008,1.),(0.280328542633766,
0.285714285714286,0.297856505190615),.UNSPECIFIED.)
GEOMETRIC_REPRESENTATION_ITEM()
RATIONAL_B_SPLINE_SURFACE(((0.996504189652447,0.998109554471267,1.,0.995737968897747,
0.992924952273131),(0.996504189652447,0.998109554471267,1.,0.995737968897747,
0.992924952273131)))
REPRESENTATION_ITEM('')
SURFACE()
);
#1518=(
BOUNDED_SURFACE()
B_SPLINE_SURFACE(1,2,((#119460,#119461,#119462),(#119463,#119464,#119465)),
 .UNSPECIFIED.,.F.,.F.,.F.)
B_SPLINE_SURFACE_WITH_KNOTS((2,2),(3,3),(0.710192959007759,1.),(0.435775021682136,
0.453027768259471),.UNSPECIFIED.)
GEOMETRIC_REPRESENTATION_ITEM()
RATIONAL_B_SPLINE_SURFACE(((0.995452950231336,0.990618550266768,0.988709602819327),
(0.995452950231336,0.990618550266768,0.988709602819327)))
REPRESENTATION_ITEM('')
SURFACE()
);
#1519=(
BOUNDED_SURFACE()
B_SPLINE_SURFACE(1,2,((#119474,#119475,#119476,#119477,#119478),(#119479,
#119480,#119481,#119482,#119483)),.UNSPECIFIED.,.F.,.F.,.F.)
B_SPLINE_SURFACE_WITH_KNOTS((2,2),(3,2,3),(0.710318915639399,1.),(0.280328542633766,
0.285714285714286,0.297856505190615),.UNSPECIFIED.)
GEOMETRIC_REPRESENTATION_ITEM()
RATIONAL_B_SPLINE_SURFACE(((0.996504189652447,0.998109554471267,1.,0.995737968897747,
0.992924952273131),(0.996504189652447,0.998109554471267,1.,0.995737968897747,
0.992924952273131)))
REPRESENTATION_ITEM('')
SURFACE()
);
#1520=(
BOUNDED_SURFACE()
B_SPLINE_SURFACE(1,2,((#119494,#119495,#119496),(#119497,#119498,#119499)),
 .UNSPECIFIED.,.F.,.F.,.F.)
B_SPLINE_SURFACE_WITH_KNOTS((2,2),(3,3),(0.710192959008366,1.),(0.435775021682621,
0.453027768259468),.UNSPECIFIED.)
GEOMETRIC_REPRESENTATION_ITEM()
RATIONAL_B_SPLINE_SURFACE(((0.995452950231064,0.990618550266715,0.988709602819327),
(0.995452950231064,0.990618550266715,0.988709602819327)))
REPRESENTATION_ITEM('')
SURFACE()
);
#1521=(
BOUNDED_SURFACE()
B_SPLINE_SURFACE(1,2,((#119508,#119509,#119510,#119511,#119512),(#119513,
#119514,#119515,#119516,#119517)),.UNSPECIFIED.,.F.,.F.,.F.)
B_SPLINE_SURFACE_WITH_KNOTS((2,2),(3,2,3),(0.710318915640004,1.),(0.280328542633766,
0.285714285714286,0.297856505190615),.UNSPECIFIED.)
GEOMETRIC_REPRESENTATION_ITEM()
RATIONAL_B_SPLINE_SURFACE(((0.996504189652447,0.998109554471267,1.,0.995737968897746,
0.992924952273131),(0.996504189652447,0.998109554471267,1.,0.995737968897746,
0.992924952273131)))
REPRESENTATION_ITEM('')
SURFACE()
);
#1522=(
BOUNDED_SURFACE()
B_SPLINE_SURFACE(1,2,((#119528,#119529,#119530),(#119531,#119532,#119533)),
 .UNSPECIFIED.,.F.,.F.,.F.)
B_SPLINE_SURFACE_WITH_KNOTS((2,2),(3,3),(0.710192959008342,1.),(0.435775021682587,
0.453027768259468),.UNSPECIFIED.)
GEOMETRIC_REPRESENTATION_ITEM()
RATIONAL_B_SPLINE_SURFACE(((0.995452950231083,0.990618550266718,0.988709602819327),
(0.995452950231083,0.990618550266718,0.988709602819327)))
REPRESENTATION_ITEM('')
SURFACE()
);
#1523=(
BOUNDED_SURFACE()
B_SPLINE_SURFACE(1,2,((#119542,#119543,#119544,#119545,#119546),(#119547,
#119548,#119549,#119550,#119551)),.UNSPECIFIED.,.F.,.F.,.F.)
B_SPLINE_SURFACE_WITH_KNOTS((2,2),(3,2,3),(0.710318915639979,1.),(0.280328542633766,
0.285714285714286,0.297856505190616),.UNSPECIFIED.)
GEOMETRIC_REPRESENTATION_ITEM()
RATIONAL_B_SPLINE_SURFACE(((0.996504189652447,0.998109554471267,1.,0.995737968897746,
0.992924952273131),(0.996504189652447,0.998109554471267,1.,0.995737968897746,
0.992924952273131)))
REPRESENTATION_ITEM('')
SURFACE()
);
#1524=(
BOUNDED_SURFACE()
B_SPLINE_SURFACE(1,2,((#119562,#119563,#119564),(#119565,#119566,#119567)),
 .UNSPECIFIED.,.F.,.F.,.F.)
B_SPLINE_SURFACE_WITH_KNOTS((2,2),(3,3),(0.710192959008342,1.),(0.435775021682621,
0.453027768259468),.UNSPECIFIED.)
GEOMETRIC_REPRESENTATION_ITEM()
RATIONAL_B_SPLINE_SURFACE(((0.995452950231064,0.990618550266715,0.988709602819327),
(0.995452950231064,0.990618550266715,0.988709602819327)))
REPRESENTATION_ITEM('')
SURFACE()
);
#1525=(
BOUNDED_SURFACE()
B_SPLINE_SURFACE(1,2,((#119576,#119577,#119578,#119579,#119580),(#119581,
#119582,#119583,#119584,#119585)),.UNSPECIFIED.,.F.,.F.,.F.)
B_SPLINE_SURFACE_WITH_KNOTS((2,2),(3,2,3),(0.710318915639981,1.),(0.280328542633766,
0.285714285714286,0.297856505190615),.UNSPECIFIED.)
GEOMETRIC_REPRESENTATION_ITEM()
RATIONAL_B_SPLINE_SURFACE(((0.996504189652447,0.998109554471267,1.,0.995737968897746,
0.992924952273131),(0.996504189652447,0.998109554471267,1.,0.995737968897746,
0.992924952273131)))
REPRESENTATION_ITEM('')
SURFACE()
);
#1526=(
BOUNDED_SURFACE()
B_SPLINE_SURFACE(1,2,((#119596,#119597,#119598),(#119599,#119600,#119601)),
 .UNSPECIFIED.,.F.,.F.,.F.)
B_SPLINE_SURFACE_WITH_KNOTS((2,2),(3,3),(0.710192959007979,1.),(0.435775021682622,
0.453027768259469),.UNSPECIFIED.)
GEOMETRIC_REPRESENTATION_ITEM()
RATIONAL_B_SPLINE_SURFACE(((0.995452950231063,0.990618550266714,0.988709602819327),
(0.995452950231063,0.990618550266714,0.988709602819327)))
REPRESENTATION_ITEM('')
SURFACE()
);
#1527=(
BOUNDED_SURFACE()
B_SPLINE_SURFACE(1,2,((#119610,#119611,#119612,#119613,#119614),(#119615,
#119616,#119617,#119618,#119619)),.UNSPECIFIED.,.F.,.F.,.F.)
B_SPLINE_SURFACE_WITH_KNOTS((2,2),(3,2,3),(0.710318915639623,1.),(0.280328542633765,
0.285714285714286,0.297856505190614),.UNSPECIFIED.)
GEOMETRIC_REPRESENTATION_ITEM()
RATIONAL_B_SPLINE_SURFACE(((0.996504189652446,0.998109554471267,1.,0.995737968897747,
0.992924952273132),(0.996504189652446,0.998109554471267,1.,0.995737968897747,
0.992924952273132)))
REPRESENTATION_ITEM('')
SURFACE()
);
#1528=(
BOUNDED_SURFACE()
B_SPLINE_SURFACE(1,2,((#119630,#119631,#119632),(#119633,#119634,#119635)),
 .UNSPECIFIED.,.F.,.F.,.F.)
B_SPLINE_SURFACE_WITH_KNOTS((2,2),(3,3),(0.,0.289681084359915),(0.228780950825311,
0.245954053070909),.UNSPECIFIED.)
GEOMETRIC_REPRESENTATION_ITEM()
RATIONAL_B_SPLINE_SURFACE(((0.991889110260683,0.988307723348179,0.987624841600687),
(0.991889110260683,0.988307723348179,0.987624841600687)))
REPRESENTATION_ITEM('')
SURFACE()
);
#1529=(
BOUNDED_SURFACE()
B_SPLINE_SURFACE(1,2,((#119648,#119649,#119650,#119651,#119652),(#119653,
#119654,#119655,#119656,#119657)),.UNSPECIFIED.,.F.,.F.,.F.)
B_SPLINE_SURFACE_WITH_KNOTS((2,2),(3,2,3),(0.,0.289807040991556),(0.487259899888157,
0.5,0.504824515313955),.UNSPECIFIED.)
GEOMETRIC_REPRESENTATION_ITEM()
RATIONAL_B_SPLINE_SURFACE(((0.992651440660745,0.995528107276569,1.,0.998306550597157,
0.996841863226483),(0.992651440660745,0.995528107276569,1.,0.998306550597157,
0.996841863226483)))
REPRESENTATION_ITEM('')
SURFACE()
);
#1530=(
BOUNDED_SURFACE()
B_SPLINE_SURFACE(1,2,((#119668,#119669,#119670),(#119671,#119672,#119673)),
 .UNSPECIFIED.,.F.,.F.,.F.)
B_SPLINE_SURFACE_WITH_KNOTS((2,2),(3,3),(0.,0.289681084359919),(0.228780950825311,
0.245954053070909),.UNSPECIFIED.)
GEOMETRIC_REPRESENTATION_ITEM()
RATIONAL_B_SPLINE_SURFACE(((0.991889110260684,0.988307723348179,0.987624841600686),
(0.991889110260683,0.988307723348179,0.987624841600686)))
REPRESENTATION_ITEM('')
SURFACE()
);
#1531=(
BOUNDED_SURFACE()
B_SPLINE_SURFACE(1,2,((#119686,#119687,#119688,#119689,#119690),(#119691,
#119692,#119693,#119694,#119695)),.UNSPECIFIED.,.F.,.F.,.F.)
B_SPLINE_SURFACE_WITH_KNOTS((2,2),(3,2,3),(0.,0.289807040991562),(0.487259899888158,
0.5,0.504824515313955),.UNSPECIFIED.)
GEOMETRIC_REPRESENTATION_ITEM()
RATIONAL_B_SPLINE_SURFACE(((0.992651440660745,0.995528107276569,1.,0.998306550597157,
0.996841863226483),(0.992651440660745,0.995528107276569,1.,0.998306550597157,
0.996841863226483)))
REPRESENTATION_ITEM('')
SURFACE()
);
#1532=(
BOUNDED_SURFACE()
B_SPLINE_SURFACE(1,2,((#119706,#119707,#119708),(#119709,#119710,#119711)),
 .UNSPECIFIED.,.F.,.F.,.F.)
B_SPLINE_SURFACE_WITH_KNOTS((2,2),(3,3),(0.,0.289681084359922),(0.228780950825753,
0.245954053070909),.UNSPECIFIED.)
GEOMETRIC_REPRESENTATION_ITEM()
RATIONAL_B_SPLINE_SURFACE(((0.991889110260499,0.988307723348161,0.987624841600687),
(0.991889110260499,0.988307723348161,0.987624841600687)))
REPRESENTATION_ITEM('')
SURFACE()
);
#1533=(
BOUNDED_SURFACE()
B_SPLINE_SURFACE(1,2,((#119724,#119725,#119726,#119727,#119728),(#119729,
#119730,#119731,#119732,#119733)),.UNSPECIFIED.,.F.,.F.,.F.)
B_SPLINE_SURFACE_WITH_KNOTS((2,2),(3,2,3),(0.,0.289807040991561),(0.487259899888157,
0.5,0.504824515313955),.UNSPECIFIED.)
GEOMETRIC_REPRESENTATION_ITEM()
RATIONAL_B_SPLINE_SURFACE(((0.992651440660745,0.995528107276569,1.,0.998306550597157,
0.996841863226483),(0.992651440660745,0.995528107276569,1.,0.998306550597157,
0.996841863226483)))
REPRESENTATION_ITEM('')
SURFACE()
);
#1534=(
BOUNDED_SURFACE()
B_SPLINE_SURFACE(1,2,((#119744,#119745,#119746),(#119747,#119748,#119749)),
 .UNSPECIFIED.,.F.,.F.,.F.)
B_SPLINE_SURFACE_WITH_KNOTS((2,2),(3,3),(0.,0.289681084359919),(0.228780950825753,
0.245954053070909),.UNSPECIFIED.)
GEOMETRIC_REPRESENTATION_ITEM()
RATIONAL_B_SPLINE_SURFACE(((0.991889110260499,0.988307723348161,0.987624841600687),
(0.991889110260499,0.988307723348161,0.987624841600687)))
REPRESENTATION_ITEM('')
SURFACE()
);
#1535=(
BOUNDED_SURFACE()
B_SPLINE_SURFACE(1,2,((#119762,#119763,#119764,#119765,#119766),(#119767,
#119768,#119769,#119770,#119771)),.UNSPECIFIED.,.F.,.F.,.F.)
B_SPLINE_SURFACE_WITH_KNOTS((2,2),(3,2,3),(0.,0.289807040992138),(0.487259899888158,
0.5,0.504824515313955),.UNSPECIFIED.)
GEOMETRIC_REPRESENTATION_ITEM()
RATIONAL_B_SPLINE_SURFACE(((0.992651440660745,0.995528107276569,1.,0.998306550597157,
0.996841863226483),(0.992651440660745,0.995528107276569,1.,0.998306550597157,
0.996841863226483)))
REPRESENTATION_ITEM('')
SURFACE()
);
#1536=(
BOUNDED_SURFACE()
B_SPLINE_SURFACE(1,2,((#119782,#119783,#119784),(#119785,#119786,#119787)),
 .UNSPECIFIED.,.F.,.F.,.F.)
B_SPLINE_SURFACE_WITH_KNOTS((2,2),(3,3),(0.,0.289681084359922),(0.228780950825753,
0.245954053070909),.UNSPECIFIED.)
GEOMETRIC_REPRESENTATION_ITEM()
RATIONAL_B_SPLINE_SURFACE(((0.991889110260499,0.988307723348161,0.987624841600687),
(0.991889110260499,0.988307723348161,0.987624841600687)))
REPRESENTATION_ITEM('')
SURFACE()
);
#1537=(
BOUNDED_SURFACE()
B_SPLINE_SURFACE(1,2,((#119800,#119801,#119802,#119803,#119804),(#119805,
#119806,#119807,#119808,#119809)),.UNSPECIFIED.,.F.,.F.,.F.)
B_SPLINE_SURFACE_WITH_KNOTS((2,2),(3,2,3),(0.,0.28980704099156),(0.487259899888158,
0.5,0.504824515313955),.UNSPECIFIED.)
GEOMETRIC_REPRESENTATION_ITEM()
RATIONAL_B_SPLINE_SURFACE(((0.992651440660745,0.995528107276569,1.,0.998306550597157,
0.996841863226483),(0.992651440660745,0.995528107276569,1.,0.998306550597157,
0.996841863226483)))
REPRESENTATION_ITEM('')
SURFACE()
);
#1538=(
BOUNDED_SURFACE()
B_SPLINE_SURFACE(1,2,((#119820,#119821,#119822),(#119823,#119824,#119825)),
 .UNSPECIFIED.,.F.,.F.,.F.)
B_SPLINE_SURFACE_WITH_KNOTS((2,2),(3,3),(0.,0.289681084359924),(0.228780950825753,
0.245954053070909),.UNSPECIFIED.)
GEOMETRIC_REPRESENTATION_ITEM()
RATIONAL_B_SPLINE_SURFACE(((0.991889110260499,0.988307723348161,0.987624841600687),
(0.991889110260499,0.988307723348161,0.987624841600687)))
REPRESENTATION_ITEM('')
SURFACE()
);
#1539=(
BOUNDED_SURFACE()
B_SPLINE_SURFACE(1,2,((#119838,#119839,#119840,#119841,#119842),(#119843,
#119844,#119845,#119846,#119847)),.UNSPECIFIED.,.F.,.F.,.F.)
B_SPLINE_SURFACE_WITH_KNOTS((2,2),(3,2,3),(0.,0.289807040992146),(0.487259899888158,
0.5,0.504824515313955),.UNSPECIFIED.)
GEOMETRIC_REPRESENTATION_ITEM()
RATIONAL_B_SPLINE_SURFACE(((0.992651440660745,0.995528107276569,1.,0.998306550597157,
0.996841863226483),(0.992651440660745,0.995528107276569,1.,0.998306550597157,
0.996841863226483)))
REPRESENTATION_ITEM('')
SURFACE()
);
#1540=(
BOUNDED_SURFACE()
B_SPLINE_SURFACE(1,2,((#119858,#119859,#119860),(#119861,#119862,#119863)),
 .UNSPECIFIED.,.F.,.F.,.F.)
B_SPLINE_SURFACE_WITH_KNOTS((2,2),(3,3),(0.,0.289681084359919),(0.228780950825753,
0.245954053070909),.UNSPECIFIED.)
GEOMETRIC_REPRESENTATION_ITEM()
RATIONAL_B_SPLINE_SURFACE(((0.991889110260499,0.988307723348161,0.987624841600687),
(0.991889110260499,0.988307723348161,0.987624841600687)))
REPRESENTATION_ITEM('')
SURFACE()
);
#1541=(
BOUNDED_SURFACE()
B_SPLINE_SURFACE(1,2,((#119876,#119877,#119878,#119879,#119880),(#119881,
#119882,#119883,#119884,#119885)),.UNSPECIFIED.,.F.,.F.,.F.)
B_SPLINE_SURFACE_WITH_KNOTS((2,2),(3,2,3),(0.,0.28980704099164),(0.487259899888159,
0.5,0.504824515313955),.UNSPECIFIED.)
GEOMETRIC_REPRESENTATION_ITEM()
RATIONAL_B_SPLINE_SURFACE(((0.992651440660745,0.99552810727657,1.,0.998306550597157,
0.996841863226483),(0.992651440660745,0.99552810727657,1.,0.998306550597157,
0.996841863226483)))
REPRESENTATION_ITEM('')
SURFACE()
);
#1542=(
BOUNDED_SURFACE()
B_SPLINE_SURFACE(1,2,((#119896,#119897,#119898),(#119899,#119900,#119901)),
 .UNSPECIFIED.,.F.,.F.,.F.)
B_SPLINE_SURFACE_WITH_KNOTS((2,2),(3,3),(0.,0.289681084359925),(0.228780950825752,
0.245954053070908),.UNSPECIFIED.)
GEOMETRIC_REPRESENTATION_ITEM()
RATIONAL_B_SPLINE_SURFACE(((0.991889110260499,0.988307723348161,0.987624841600687),
(0.991889110260499,0.988307723348161,0.987624841600687)))
REPRESENTATION_ITEM('')
SURFACE()
);
#1543=(
BOUNDED_SURFACE()
B_SPLINE_SURFACE(1,2,((#119914,#119915,#119916,#119917,#119918),(#119919,
#119920,#119921,#119922,#119923)),.UNSPECIFIED.,.F.,.F.,.F.)
B_SPLINE_SURFACE_WITH_KNOTS((2,2),(3,2,3),(0.,0.289807040991634),(0.487259899888159,
0.5,0.504824515313956),.UNSPECIFIED.)
GEOMETRIC_REPRESENTATION_ITEM()
RATIONAL_B_SPLINE_SURFACE(((0.992651440660745,0.99552810727657,1.,0.998306550597157,
0.996841863226482),(0.992651440660745,0.99552810727657,1.,0.998306550597157,
0.996841863226482)))
REPRESENTATION_ITEM('')
SURFACE()
);
#1544=(
BOUNDED_SURFACE()
B_SPLINE_SURFACE(1,2,((#119934,#119935,#119936),(#119937,#119938,#119939)),
 .UNSPECIFIED.,.F.,.F.,.F.)
B_SPLINE_SURFACE_WITH_KNOTS((2,2),(3,3),(0.,0.289681084361937),(0.22878095082531,
0.245954053070933),.UNSPECIFIED.)
GEOMETRIC_REPRESENTATION_ITEM()
RATIONAL_B_SPLINE_SURFACE(((0.991889110260684,0.988307723348174,0.987624841600685),
(0.991889110260684,0.988307723348174,0.987624841600685)))
REPRESENTATION_ITEM('')
SURFACE()
);
#1545=(
BOUNDED_SURFACE()
B_SPLINE_SURFACE(1,2,((#119952,#119953,#119954,#119955,#119956),(#119957,
#119958,#119959,#119960,#119961)),.UNSPECIFIED.,.F.,.F.,.F.)
B_SPLINE_SURFACE_WITH_KNOTS((2,2),(3,2,3),(0.,0.289807040992233),(0.487259899888159,
0.5,0.504824515313956),.UNSPECIFIED.)
GEOMETRIC_REPRESENTATION_ITEM()
RATIONAL_B_SPLINE_SURFACE(((0.992651440660745,0.99552810727657,1.,0.998306550597157,
0.996841863226482),(0.992651440660745,0.99552810727657,1.,0.998306550597157,
0.996841863226482)))
REPRESENTATION_ITEM('')
SURFACE()
);
#1546=(
BOUNDED_SURFACE()
B_SPLINE_SURFACE(1,2,((#119972,#119973,#119974),(#119975,#119976,#119977)),
 .UNSPECIFIED.,.F.,.F.,.F.)
B_SPLINE_SURFACE_WITH_KNOTS((2,2),(3,3),(0.,0.289681084359923),(0.228780950825308,
0.245954053070908),.UNSPECIFIED.)
GEOMETRIC_REPRESENTATION_ITEM()
RATIONAL_B_SPLINE_SURFACE(((0.991889110260685,0.988307723348179,0.987624841600687),
(0.991889110260685,0.988307723348179,0.987624841600687)))
REPRESENTATION_ITEM('')
SURFACE()
);
#1547=(
BOUNDED_SURFACE()
B_SPLINE_SURFACE(1,2,((#119990,#119991,#119992,#119993,#119994),(#119995,
#119996,#119997,#119998,#119999)),.UNSPECIFIED.,.F.,.F.,.F.)
B_SPLINE_SURFACE_WITH_KNOTS((2,2),(3,2,3),(0.,0.289807040991645),(0.487259899888159,
0.5,0.504824515313956),.UNSPECIFIED.)
GEOMETRIC_REPRESENTATION_ITEM()
RATIONAL_B_SPLINE_SURFACE(((0.992651440660745,0.99552810727657,1.,0.998306550597157,
0.996841863226482),(0.992651440660745,0.99552810727657,1.,0.998306550597157,
0.996841863226482)))
REPRESENTATION_ITEM('')
SURFACE()
);
#1548=(
BOUNDED_SURFACE()
B_SPLINE_SURFACE(1,2,((#120010,#120011,#120012),(#120013,#120014,#120015)),
 .UNSPECIFIED.,.F.,.F.,.F.)
B_SPLINE_SURFACE_WITH_KNOTS((2,2),(3,3),(0.,0.289681084359923),(0.228780950825302,
0.245954053070908),.UNSPECIFIED.)
GEOMETRIC_REPRESENTATION_ITEM()
RATIONAL_B_SPLINE_SURFACE(((0.991889110260687,0.98830772334818,0.987624841600687),
(0.991889110260687,0.98830772334818,0.987624841600687)))
REPRESENTATION_ITEM('')
SURFACE()
);
#1549=(
BOUNDED_SURFACE()
B_SPLINE_SURFACE(1,2,((#120028,#120029,#120030,#120031,#120032),(#120033,
#120034,#120035,#120036,#120037)),.UNSPECIFIED.,.F.,.F.,.F.)
B_SPLINE_SURFACE_WITH_KNOTS((2,2),(3,2,3),(0.,0.289807040992145),(0.487259899888159,
0.5,0.504824515313956),.UNSPECIFIED.)
GEOMETRIC_REPRESENTATION_ITEM()
RATIONAL_B_SPLINE_SURFACE(((0.992651440660745,0.99552810727657,1.,0.998306550597157,
0.996841863226482),(0.992651440660745,0.99552810727657,1.,0.998306550597157,
0.996841863226482)))
REPRESENTATION_ITEM('')
SURFACE()
);
#1550=(
BOUNDED_SURFACE()
B_SPLINE_SURFACE(1,2,((#120048,#120049,#120050),(#120051,#120052,#120053)),
 .UNSPECIFIED.,.F.,.F.,.F.)
B_SPLINE_SURFACE_WITH_KNOTS((2,2),(3,3),(0.,0.289681084359918),(0.228780950825752,
0.245954053070908),.UNSPECIFIED.)
GEOMETRIC_REPRESENTATION_ITEM()
RATIONAL_B_SPLINE_SURFACE(((0.991889110260499,0.988307723348161,0.987624841600687),
(0.991889110260499,0.988307723348162,0.987624841600687)))
REPRESENTATION_ITEM('')
SURFACE()
);
#1551=(
BOUNDED_SURFACE()
B_SPLINE_SURFACE(1,2,((#120066,#120067,#120068,#120069,#120070),(#120071,
#120072,#120073,#120074,#120075)),.UNSPECIFIED.,.F.,.F.,.F.)
B_SPLINE_SURFACE_WITH_KNOTS((2,2),(3,2,3),(0.,0.289807040991646),(0.487259899888158,
0.5,0.504824515313956),.UNSPECIFIED.)
GEOMETRIC_REPRESENTATION_ITEM()
RATIONAL_B_SPLINE_SURFACE(((0.992651440660745,0.99552810727657,1.,0.998306550597157,
0.996841863226482),(0.992651440660745,0.99552810727657,1.,0.998306550597157,
0.996841863226482)))
REPRESENTATION_ITEM('')
SURFACE()
);
#1552=(
BOUNDED_SURFACE()
B_SPLINE_SURFACE(1,2,((#120086,#120087,#120088),(#120089,#120090,#120091)),
 .UNSPECIFIED.,.F.,.F.,.F.)
B_SPLINE_SURFACE_WITH_KNOTS((2,2),(3,3),(0.,0.289681084359922),(0.228780950825302,
0.245954053070908),.UNSPECIFIED.)
GEOMETRIC_REPRESENTATION_ITEM()
RATIONAL_B_SPLINE_SURFACE(((0.991889110260687,0.98830772334818,0.987624841600687),
(0.991889110260687,0.98830772334818,0.987624841600687)))
REPRESENTATION_ITEM('')
SURFACE()
);
#1553=(
BOUNDED_SURFACE()
B_SPLINE_SURFACE(1,2,((#120104,#120105,#120106,#120107,#120108),(#120109,
#120110,#120111,#120112,#120113)),.UNSPECIFIED.,.F.,.F.,.F.)
B_SPLINE_SURFACE_WITH_KNOTS((2,2),(3,2,3),(0.,0.289807040992144),(0.487259899888159,
0.5,0.504824515313956),.UNSPECIFIED.)
GEOMETRIC_REPRESENTATION_ITEM()
RATIONAL_B_SPLINE_SURFACE(((0.992651440660745,0.99552810727657,1.,0.998306550597157,
0.996841863226482),(0.992651440660745,0.99552810727657,1.,0.998306550597157,
0.996841863226482)))
REPRESENTATION_ITEM('')
SURFACE()
);
#1554=(
BOUNDED_SURFACE()
B_SPLINE_SURFACE(1,2,((#120124,#120125,#120126),(#120127,#120128,#120129)),
 .UNSPECIFIED.,.F.,.F.,.F.)
B_SPLINE_SURFACE_WITH_KNOTS((2,2),(3,3),(0.,0.289681084359919),(0.228780950825305,
0.245954053070908),.UNSPECIFIED.)
GEOMETRIC_REPRESENTATION_ITEM()
RATIONAL_B_SPLINE_SURFACE(((0.991889110260686,0.988307723348179,0.987624841600687),
(0.991889110260686,0.988307723348179,0.987624841600687)))
REPRESENTATION_ITEM('')
SURFACE()
);
#1555=(
BOUNDED_SURFACE()
B_SPLINE_SURFACE(1,2,((#120142,#120143,#120144,#120145,#120146),(#120147,
#120148,#120149,#120150,#120151)),.UNSPECIFIED.,.F.,.F.,.F.)
B_SPLINE_SURFACE_WITH_KNOTS((2,2),(3,2,3),(0.,0.289807040991922),(0.487259899888159,
0.5,0.504824515313956),.UNSPECIFIED.)
GEOMETRIC_REPRESENTATION_ITEM()
RATIONAL_B_SPLINE_SURFACE(((0.992651440660745,0.99552810727657,1.,0.998306550597157,
0.996841863226482),(0.992651440660745,0.99552810727657,1.,0.998306550597157,
0.996841863226482)))
REPRESENTATION_ITEM('')
SURFACE()
);
#1556=(
BOUNDED_SURFACE()
B_SPLINE_SURFACE(1,2,((#120162,#120163,#120164),(#120165,#120166,#120167)),
 .UNSPECIFIED.,.F.,.F.,.F.)
B_SPLINE_SURFACE_WITH_KNOTS((2,2),(3,3),(0.,0.28968108435992),(0.228780950825309,
0.245954053070908),.UNSPECIFIED.)
GEOMETRIC_REPRESENTATION_ITEM()
RATIONAL_B_SPLINE_SURFACE(((0.991889110260684,0.988307723348179,0.987624841600687),
(0.991889110260684,0.988307723348179,0.987624841600687)))
REPRESENTATION_ITEM('')
SURFACE()
);
#1557=(
BOUNDED_SURFACE()
B_SPLINE_SURFACE(1,2,((#120180,#120181,#120182,#120183,#120184),(#120185,
#120186,#120187,#120188,#120189)),.UNSPECIFIED.,.F.,.F.,.F.)
B_SPLINE_SURFACE_WITH_KNOTS((2,2),(3,2,3),(0.,0.289807040992964),(0.487259899888159,
0.5,0.504824515313956),.UNSPECIFIED.)
GEOMETRIC_REPRESENTATION_ITEM()
RATIONAL_B_SPLINE_SURFACE(((0.992651440660745,0.99552810727657,1.,0.998306550597157,
0.996841863226482),(0.992651440660745,0.99552810727657,1.,0.998306550597157,
0.996841863226482)))
REPRESENTATION_ITEM('')
SURFACE()
);
#1558=(
BOUNDED_SURFACE()
B_SPLINE_SURFACE(1,2,((#120200,#120201,#120202),(#120203,#120204,#120205)),
 .UNSPECIFIED.,.F.,.F.,.F.)
B_SPLINE_SURFACE_WITH_KNOTS((2,2),(3,3),(0.,0.289681084359923),(0.228780950825313,
0.245954053070908),.UNSPECIFIED.)
GEOMETRIC_REPRESENTATION_ITEM()
RATIONAL_B_SPLINE_SURFACE(((0.991889110260683,0.988307723348179,0.987624841600687),
(0.991889110260683,0.988307723348179,0.987624841600687)))
REPRESENTATION_ITEM('')
SURFACE()
);
#1559=(
BOUNDED_SURFACE()
B_SPLINE_SURFACE(1,2,((#120218,#120219,#120220,#120221,#120222),(#120223,
#120224,#120225,#120226,#120227)),.UNSPECIFIED.,.F.,.F.,.F.)
B_SPLINE_SURFACE_WITH_KNOTS((2,2),(3,2,3),(0.,0.289807040991679),(0.487259899888159,
0.5,0.504824515313956),.UNSPECIFIED.)
GEOMETRIC_REPRESENTATION_ITEM()
RATIONAL_B_SPLINE_SURFACE(((0.992651440660745,0.99552810727657,1.,0.998306550597157,
0.996841863226482),(0.992651440660745,0.99552810727657,1.,0.998306550597157,
0.996841863226482)))
REPRESENTATION_ITEM('')
SURFACE()
);
#1560=(
BOUNDED_SURFACE()
B_SPLINE_SURFACE(1,2,((#120238,#120239,#120240),(#120241,#120242,#120243)),
 .UNSPECIFIED.,.F.,.F.,.F.)
B_SPLINE_SURFACE_WITH_KNOTS((2,2),(3,3),(0.,0.289681084359926),(0.228780950825752,
0.245954053070908),.UNSPECIFIED.)
GEOMETRIC_REPRESENTATION_ITEM()
RATIONAL_B_SPLINE_SURFACE(((0.991889110260499,0.988307723348161,0.987624841600687),
(0.991889110260499,0.988307723348161,0.987624841600687)))
REPRESENTATION_ITEM('')
SURFACE()
);
#1561=(
BOUNDED_SURFACE()
B_SPLINE_SURFACE(1,2,((#120256,#120257,#120258,#120259,#120260),(#120261,
#120262,#120263,#120264,#120265)),.UNSPECIFIED.,.F.,.F.,.F.)
B_SPLINE_SURFACE_WITH_KNOTS((2,2),(3,2,3),(0.,0.289807040991562),(0.487259899888159,
0.5,0.504824515313956),.UNSPECIFIED.)
GEOMETRIC_REPRESENTATION_ITEM()
RATIONAL_B_SPLINE_SURFACE(((0.992651440660745,0.99552810727657,1.,0.998306550597157,
0.996841863226482),(0.992651440660745,0.99552810727657,1.,0.998306550597157,
0.996841863226482)))
REPRESENTATION_ITEM('')
SURFACE()
);
#1562=(
BOUNDED_SURFACE()
B_SPLINE_SURFACE(1,2,((#120276,#120277,#120278),(#120279,#120280,#120281)),
 .UNSPECIFIED.,.F.,.F.,.F.)
B_SPLINE_SURFACE_WITH_KNOTS((2,2),(3,3),(0.,0.289681084359922),(0.22878095082551,
0.245954053070908),.UNSPECIFIED.)
GEOMETRIC_REPRESENTATION_ITEM()
RATIONAL_B_SPLINE_SURFACE(((0.9918891102606,0.988307723348171,0.987624841600687),
(0.9918891102606,0.988307723348171,0.987624841600687)))
REPRESENTATION_ITEM('')
SURFACE()
);
#1563=(
BOUNDED_SURFACE()
B_SPLINE_SURFACE(1,2,((#120294,#120295,#120296,#120297,#120298),(#120299,
#120300,#120301,#120302,#120303)),.UNSPECIFIED.,.F.,.F.,.F.)
B_SPLINE_SURFACE_WITH_KNOTS((2,2),(3,2,3),(0.,0.289807040992201),(0.487259899888159,
0.5,0.504824515313956),.UNSPECIFIED.)
GEOMETRIC_REPRESENTATION_ITEM()
RATIONAL_B_SPLINE_SURFACE(((0.992651440660745,0.99552810727657,1.,0.998306550597157,
0.996841863226482),(0.992651440660745,0.99552810727657,1.,0.998306550597157,
0.996841863226482)))
REPRESENTATION_ITEM('')
SURFACE()
);
#1564=(
BOUNDED_SURFACE()
B_SPLINE_SURFACE(1,2,((#120314,#120315,#120316),(#120317,#120318,#120319)),
 .UNSPECIFIED.,.F.,.F.,.F.)
B_SPLINE_SURFACE_WITH_KNOTS((2,2),(3,3),(0.,0.289681084359927),(0.22878095082532,
0.245954053070908),.UNSPECIFIED.)
GEOMETRIC_REPRESENTATION_ITEM()
RATIONAL_B_SPLINE_SURFACE(((0.99188911026068,0.988307723348179,0.987624841600687),
(0.99188911026068,0.988307723348179,0.987624841600687)))
REPRESENTATION_ITEM('')
SURFACE()
);
#1565=(
BOUNDED_SURFACE()
B_SPLINE_SURFACE(1,2,((#120332,#120333,#120334,#120335,#120336),(#120337,
#120338,#120339,#120340,#120341)),.UNSPECIFIED.,.F.,.F.,.F.)
B_SPLINE_SURFACE_WITH_KNOTS((2,2),(3,2,3),(0.,0.289807040991564),(0.487259899888159,
0.5,0.504824515313681),.UNSPECIFIED.)
GEOMETRIC_REPRESENTATION_ITEM()
RATIONAL_B_SPLINE_SURFACE(((0.992651440660745,0.99552810727657,1.,0.998306550597253,
0.996841863226649),(0.992651440660745,0.99552810727657,1.,0.998306550597253,
0.996841863226649)))
REPRESENTATION_ITEM('')
SURFACE()
);
#1566=(
BOUNDED_SURFACE()
B_SPLINE_SURFACE(1,2,((#120352,#120353,#120354),(#120355,#120356,#120357)),
 .UNSPECIFIED.,.F.,.F.,.F.)
B_SPLINE_SURFACE_WITH_KNOTS((2,2),(3,3),(0.,0.289681084359927),(0.228780950825606,
0.245954053070908),.UNSPECIFIED.)
GEOMETRIC_REPRESENTATION_ITEM()
RATIONAL_B_SPLINE_SURFACE(((0.991889110260561,0.988307723348167,0.987624841600687),
(0.991889110260561,0.988307723348168,0.987624841600687)))
REPRESENTATION_ITEM('')
SURFACE()
);
#1567=(
BOUNDED_SURFACE()
B_SPLINE_SURFACE(1,2,((#120370,#120371,#120372,#120373,#120374),(#120375,
#120376,#120377,#120378,#120379)),.UNSPECIFIED.,.F.,.F.,.F.)
B_SPLINE_SURFACE_WITH_KNOTS((2,2),(3,2,3),(0.,0.289807040992693),(0.487259899888159,
0.5,0.504824515313956),.UNSPECIFIED.)
GEOMETRIC_REPRESENTATION_ITEM()
RATIONAL_B_SPLINE_SURFACE(((0.992651440660745,0.99552810727657,1.,0.998306550597157,
0.996841863226482),(0.992651440660745,0.99552810727657,1.,0.998306550597157,
0.996841863226482)))
REPRESENTATION_ITEM('')
SURFACE()
);
#1568=(
BOUNDED_SURFACE()
B_SPLINE_SURFACE(1,2,((#120390,#120391,#120392),(#120393,#120394,#120395)),
 .UNSPECIFIED.,.F.,.F.,.F.)
B_SPLINE_SURFACE_WITH_KNOTS((2,2),(3,3),(0.,0.289681084359929),(0.228780950825752,
0.245954053070908),.UNSPECIFIED.)
GEOMETRIC_REPRESENTATION_ITEM()
RATIONAL_B_SPLINE_SURFACE(((0.991889110260499,0.988307723348162,0.987624841600687),
(0.991889110260499,0.988307723348162,0.987624841600687)))
REPRESENTATION_ITEM('')
SURFACE()
);
#1569=(
BOUNDED_SURFACE()
B_SPLINE_SURFACE(1,2,((#120408,#120409,#120410,#120411,#120412),(#120413,
#120414,#120415,#120416,#120417)),.UNSPECIFIED.,.F.,.F.,.F.)
B_SPLINE_SURFACE_WITH_KNOTS((2,2),(3,2,3),(0.,0.289807040992531),(0.487259899888159,
0.5,0.504824515313956),.UNSPECIFIED.)
GEOMETRIC_REPRESENTATION_ITEM()
RATIONAL_B_SPLINE_SURFACE(((0.992651440660745,0.99552810727657,1.,0.998306550597157,
0.996841863226482),(0.992651440660745,0.99552810727657,1.,0.998306550597157,
0.996841863226482)))
REPRESENTATION_ITEM('')
SURFACE()
);
#1570=(
BOUNDED_SURFACE()
B_SPLINE_SURFACE(1,2,((#120428,#120429,#120430),(#120431,#120432,#120433)),
 .UNSPECIFIED.,.F.,.F.,.F.)
B_SPLINE_SURFACE_WITH_KNOTS((2,2),(3,3),(0.,0.289681084359926),(0.228780950825465,
0.245954053070908),.UNSPECIFIED.)
GEOMETRIC_REPRESENTATION_ITEM()
RATIONAL_B_SPLINE_SURFACE(((0.991889110260619,0.988307723348173,0.987624841600687),
(0.991889110260619,0.988307723348173,0.987624841600687)))
REPRESENTATION_ITEM('')
SURFACE()
);
#1571=(
BOUNDED_SURFACE()
B_SPLINE_SURFACE(1,2,((#120446,#120447,#120448,#120449,#120450),(#120451,
#120452,#120453,#120454,#120455)),.UNSPECIFIED.,.F.,.F.,.F.)
B_SPLINE_SURFACE_WITH_KNOTS((2,2),(3,2,3),(0.,0.289807040993255),(0.487259899888159,
0.5,0.504824515313827),.UNSPECIFIED.)
GEOMETRIC_REPRESENTATION_ITEM()
RATIONAL_B_SPLINE_SURFACE(((0.992651440660745,0.99552810727657,1.,0.998306550597202,
0.99684186322656),(0.992651440660745,0.99552810727657,1.,0.998306550597202,
0.99684186322656)))
REPRESENTATION_ITEM('')
SURFACE()
);
#1572=(
BOUNDED_SURFACE()
B_SPLINE_SURFACE(1,2,((#120466,#120467,#120468),(#120469,#120470,#120471)),
 .UNSPECIFIED.,.F.,.F.,.F.)
B_SPLINE_SURFACE_WITH_KNOTS((2,2),(3,3),(0.,0.289681084359919),(0.228780950825422,
0.245954053070908),.UNSPECIFIED.)
GEOMETRIC_REPRESENTATION_ITEM()
RATIONAL_B_SPLINE_SURFACE(((0.991889110260637,0.988307723348175,0.987624841600687),
(0.991889110260637,0.988307723348175,0.987624841600687)))
REPRESENTATION_ITEM('')
SURFACE()
);
#1573=(
BOUNDED_SURFACE()
B_SPLINE_SURFACE(1,2,((#120484,#120485,#120486,#120487,#120488),(#120489,
#120490,#120491,#120492,#120493)),.UNSPECIFIED.,.F.,.F.,.F.)
B_SPLINE_SURFACE_WITH_KNOTS((2,2),(3,2,3),(0.,0.289807040991761),(0.487259899888159,
0.5,0.504824515313794),.UNSPECIFIED.)
GEOMETRIC_REPRESENTATION_ITEM()
RATIONAL_B_SPLINE_SURFACE(((0.992651440660745,0.99552810727657,1.,0.998306550597214,
0.99684186322658),(0.992651440660745,0.99552810727657,1.,0.998306550597214,
0.99684186322658)))
REPRESENTATION_ITEM('')
SURFACE()
);
#1574=(
BOUNDED_SURFACE()
B_SPLINE_SURFACE(1,2,((#120504,#120505,#120506),(#120507,#120508,#120509)),
 .UNSPECIFIED.,.F.,.F.,.F.)
B_SPLINE_SURFACE_WITH_KNOTS((2,2),(3,3),(0.,0.28968108435992),(0.228780950825549,
0.245954053070908),.UNSPECIFIED.)
GEOMETRIC_REPRESENTATION_ITEM()
RATIONAL_B_SPLINE_SURFACE(((0.991889110260584,0.98830772334817,0.987624841600687),
(0.991889110260584,0.98830772334817,0.987624841600687)))
REPRESENTATION_ITEM('')
SURFACE()
);
#1575=(
BOUNDED_SURFACE()
B_SPLINE_SURFACE(1,2,((#120522,#120523,#120524,#120525,#120526),(#120527,
#120528,#120529,#120530,#120531)),.UNSPECIFIED.,.F.,.F.,.F.)
B_SPLINE_SURFACE_WITH_KNOTS((2,2),(3,2,3),(0.,0.289807040993054),(0.487259899888159,
0.5,0.504824515313847),.UNSPECIFIED.)
GEOMETRIC_REPRESENTATION_ITEM()
RATIONAL_B_SPLINE_SURFACE(((0.992651440660745,0.99552810727657,1.,0.998306550597195,
0.996841863226548),(0.992651440660745,0.99552810727657,1.,0.998306550597195,
0.996841863226548)))
REPRESENTATION_ITEM('')
SURFACE()
);
#1576=(
BOUNDED_SURFACE()
B_SPLINE_SURFACE(1,2,((#120542,#120543,#120544),(#120545,#120546,#120547)),
 .UNSPECIFIED.,.F.,.F.,.F.)
B_SPLINE_SURFACE_WITH_KNOTS((2,2),(3,3),(0.,0.289681084359929),(0.228780950825689,
0.245954053070908),.UNSPECIFIED.)
GEOMETRIC_REPRESENTATION_ITEM()
RATIONAL_B_SPLINE_SURFACE(((0.991889110260526,0.988307723348164,0.987624841600687),
(0.991889110260526,0.988307723348164,0.987624841600687)))
REPRESENTATION_ITEM('')
SURFACE()
);
#1577=(
BOUNDED_SURFACE()
B_SPLINE_SURFACE(1,2,((#120560,#120561,#120562,#120563,#120564),(#120565,
#120566,#120567,#120568,#120569)),.UNSPECIFIED.,.F.,.F.,.F.)
B_SPLINE_SURFACE_WITH_KNOTS((2,2),(3,2,3),(0.,0.289807040992802),(0.487259899888159,
0.5,0.504824515313924),.UNSPECIFIED.)
GEOMETRIC_REPRESENTATION_ITEM()
RATIONAL_B_SPLINE_SURFACE(((0.992651440660745,0.99552810727657,1.,0.998306550597168,
0.996841863226501),(0.992651440660745,0.99552810727657,1.,0.998306550597168,
0.996841863226501)))
REPRESENTATION_ITEM('')
SURFACE()
);
#1578=(
BOUNDED_SURFACE()
B_SPLINE_SURFACE(1,2,((#120580,#120581,#120582),(#120583,#120584,#120585)),
 .UNSPECIFIED.,.F.,.F.,.F.)
B_SPLINE_SURFACE_WITH_KNOTS((2,2),(3,3),(0.,0.289681084359935),(0.228780950825721,
0.245954053070908),.UNSPECIFIED.)
GEOMETRIC_REPRESENTATION_ITEM()
RATIONAL_B_SPLINE_SURFACE(((0.991889110260513,0.988307723348163,0.987624841600687),
(0.991889110260513,0.988307723348163,0.987624841600687)))
REPRESENTATION_ITEM('')
SURFACE()
);
#1579=(
BOUNDED_SURFACE()
B_SPLINE_SURFACE(1,2,((#120598,#120599,#120600,#120601,#120602),(#120603,
#120604,#120605,#120606,#120607)),.UNSPECIFIED.,.F.,.F.,.F.)
B_SPLINE_SURFACE_WITH_KNOTS((2,2),(3,2,3),(0.,0.289807040992555),(0.487259899888159,
0.5,0.50482451531395),.UNSPECIFIED.)
GEOMETRIC_REPRESENTATION_ITEM()
RATIONAL_B_SPLINE_SURFACE(((0.992651440660745,0.99552810727657,1.,0.998306550597159,
0.996841863226485),(0.992651440660745,0.99552810727657,1.,0.998306550597159,
0.996841863226485)))
REPRESENTATION_ITEM('')
SURFACE()
);
#1580=(
BOUNDED_SURFACE()
B_SPLINE_SURFACE(1,2,((#120618,#120619,#120620),(#120621,#120622,#120623)),
 .UNSPECIFIED.,.F.,.F.,.F.)
B_SPLINE_SURFACE_WITH_KNOTS((2,2),(3,3),(0.,0.289681084359928),(0.228780950825752,
0.245954053070908),.UNSPECIFIED.)
GEOMETRIC_REPRESENTATION_ITEM()
RATIONAL_B_SPLINE_SURFACE(((0.9918891102605,0.988307723348162,0.987624841600687),
(0.9918891102605,0.988307723348162,0.987624841600687)))
REPRESENTATION_ITEM('')
SURFACE()
);
#1581=(
BOUNDED_SURFACE()
B_SPLINE_SURFACE(1,2,((#120636,#120637,#120638,#120639,#120640),(#120641,
#120642,#120643,#120644,#120645)),.UNSPECIFIED.,.F.,.F.,.F.)
B_SPLINE_SURFACE_WITH_KNOTS((2,2),(3,2,3),(0.,0.289807040992489),(0.487259899888159,
0.5,0.504824515313956),.UNSPECIFIED.)
GEOMETRIC_REPRESENTATION_ITEM()
RATIONAL_B_SPLINE_SURFACE(((0.992651440660745,0.99552810727657,1.,0.998306550597157,
0.996841863226482),(0.992651440660745,0.99552810727657,1.,0.998306550597157,
0.996841863226482)))
REPRESENTATION_ITEM('')
SURFACE()
);
#1582=(
BOUNDED_SURFACE()
B_SPLINE_SURFACE(1,2,((#120656,#120657,#120658),(#120659,#120660,#120661)),
 .UNSPECIFIED.,.F.,.F.,.F.)
B_SPLINE_SURFACE_WITH_KNOTS((2,2),(3,3),(0.,0.289681084359923),(0.228780950825752,
0.245954053070909),.UNSPECIFIED.)
GEOMETRIC_REPRESENTATION_ITEM()
RATIONAL_B_SPLINE_SURFACE(((0.9918891102605,0.988307723348161,0.987624841600687),
(0.9918891102605,0.988307723348161,0.987624841600687)))
REPRESENTATION_ITEM('')
SURFACE()
);
#1583=(
BOUNDED_SURFACE()
B_SPLINE_SURFACE(1,2,((#120674,#120675,#120676,#120677,#120678),(#120679,
#120680,#120681,#120682,#120683)),.UNSPECIFIED.,.F.,.F.,.F.)
B_SPLINE_SURFACE_WITH_KNOTS((2,2),(3,2,3),(0.,0.289807040992803),(0.48725989988815,
0.5,0.504824515313956),.UNSPECIFIED.)
GEOMETRIC_REPRESENTATION_ITEM()
RATIONAL_B_SPLINE_SURFACE(((0.992651440660741,0.995528107276567,1.,0.998306550597157,
0.996841863226482),(0.992651440660741,0.995528107276567,1.,0.998306550597157,
0.996841863226482)))
REPRESENTATION_ITEM('')
SURFACE()
);
#1584=(
BOUNDED_SURFACE()
B_SPLINE_SURFACE(1,2,((#120694,#120695,#120696),(#120697,#120698,#120699)),
 .UNSPECIFIED.,.F.,.F.,.F.)
B_SPLINE_SURFACE_WITH_KNOTS((2,2),(3,3),(0.,0.289681084359922),(0.228780950825753,
0.245954053070908),.UNSPECIFIED.)
GEOMETRIC_REPRESENTATION_ITEM()
RATIONAL_B_SPLINE_SURFACE(((0.991889110260499,0.988307723348161,0.987624841600687),
(0.991889110260499,0.988307723348161,0.987624841600687)))
REPRESENTATION_ITEM('')
SURFACE()
);
#1585=(
BOUNDED_SURFACE()
B_SPLINE_SURFACE(1,2,((#120712,#120713,#120714,#120715,#120716),(#120717,
#120718,#120719,#120720,#120721)),.UNSPECIFIED.,.F.,.F.,.F.)
B_SPLINE_SURFACE_WITH_KNOTS((2,2),(3,2,3),(0.,0.28980704099156),(0.487259899888158,
0.5,0.504824515313955),.UNSPECIFIED.)
GEOMETRIC_REPRESENTATION_ITEM()
RATIONAL_B_SPLINE_SURFACE(((0.992651440660745,0.995528107276569,1.,0.998306550597157,
0.996841863226483),(0.992651440660745,0.995528107276569,1.,0.998306550597157,
0.996841863226483)))
REPRESENTATION_ITEM('')
SURFACE()
);
#1586=(
BOUNDED_SURFACE()
B_SPLINE_SURFACE(1,2,((#120732,#120733,#120734),(#120735,#120736,#120737)),
 .UNSPECIFIED.,.F.,.F.,.F.)
B_SPLINE_SURFACE_WITH_KNOTS((2,2),(3,3),(0.,0.289681084359934),(0.43567212259767,
0.452924869174518),.UNSPECIFIED.)
GEOMETRIC_REPRESENTATION_ITEM()
RATIONAL_B_SPLINE_SURFACE(((0.995510721093622,0.990658873102333,0.988732477628005),
(0.995510721093622,0.990658873102333,0.988732477628005)))
REPRESENTATION_ITEM('')
SURFACE()
);
#1587=(
BOUNDED_SURFACE()
B_SPLINE_SURFACE(1,2,((#120748,#120749,#120750,#120751,#120752,#120753,
#120754),(#120755,#120756,#120757,#120758,#120759,#120760,#120761)),
 .UNSPECIFIED.,.F.,.F.,.F.)
B_SPLINE_SURFACE_WITH_KNOTS((2,2),(3,2,2,3),(0.,0.289807040991593),(0.280257803540345,
0.280433083165913,0.285714285714286,0.297961045722762),.UNSPECIFIED.)
GEOMETRIC_REPRESENTATION_ITEM()
RATIONAL_B_SPLINE_SURFACE(((0.996566619267863,0.996566619267863,0.996566619267863,
0.998146249162903,1.,0.995701274206111,0.992876621380142),(0.996566619267863,
0.996566619267863,0.996566619267863,0.998146249162903,1.,0.995701274206111,
0.992876621380142)))
REPRESENTATION_ITEM('')
SURFACE()
);
#1588=(
BOUNDED_SURFACE()
B_SPLINE_SURFACE(1,2,((#120784,#120785,#120786),(#120787,#120788,#120789)),
 .UNSPECIFIED.,.F.,.F.,.F.)
B_SPLINE_SURFACE_WITH_KNOTS((2,2),(3,3),(0.,0.289681084359924),(0.43567212259767,
0.452924869174518),.UNSPECIFIED.)
GEOMETRIC_REPRESENTATION_ITEM()
RATIONAL_B_SPLINE_SURFACE(((0.995510721093622,0.990658873102333,0.988732477628005),
(0.995510721093622,0.990658873102333,0.988732477628005)))
REPRESENTATION_ITEM('')
SURFACE()
);
#1589=(
BOUNDED_SURFACE()
B_SPLINE_SURFACE(1,2,((#120791,#120792,#120793,#120794,#120795,#120796,
#120797),(#120798,#120799,#120800,#120801,#120802,#120803,#120804)),
 .UNSPECIFIED.,.F.,.F.,.F.)
B_SPLINE_SURFACE_WITH_KNOTS((2,2),(3,2,2,3),(0.,0.289807040991598),(0.280257803540345,
0.280433083165913,0.285714285714286,0.297961045722761),.UNSPECIFIED.)
GEOMETRIC_REPRESENTATION_ITEM()
RATIONAL_B_SPLINE_SURFACE(((0.996566619267863,0.996566619267863,0.996566619267863,
0.998146249162903,1.,0.995701274206111,0.992876621380142),(0.996566619267863,
0.996566619267863,0.996566619267863,0.998146249162903,1.,0.995701274206111,
0.992876621380142)))
REPRESENTATION_ITEM('')
SURFACE()
);
#1590=(
BOUNDED_SURFACE()
B_SPLINE_SURFACE(1,2,((#120827,#120828,#120829),(#120830,#120831,#120832)),
 .UNSPECIFIED.,.F.,.F.,.F.)
B_SPLINE_SURFACE_WITH_KNOTS((2,2),(3,3),(0.,0.289681084359926),(0.435672122597196,
0.452924869174518),.UNSPECIFIED.)
GEOMETRIC_REPRESENTATION_ITEM()
RATIONAL_B_SPLINE_SURFACE(((0.995510721093888,0.990658873102386,0.988732477628005),
(0.995510721093888,0.990658873102386,0.988732477628005)))
REPRESENTATION_ITEM('')
SURFACE()
);
#1591=(
BOUNDED_SURFACE()
B_SPLINE_SURFACE(1,2,((#120834,#120835,#120836,#120837,#120838,#120839,
#120840),(#120841,#120842,#120843,#120844,#120845,#120846,#120847)),
 .UNSPECIFIED.,.F.,.F.,.F.)
B_SPLINE_SURFACE_WITH_KNOTS((2,2),(3,2,2,3),(0.,0.289807040991589),(0.280257803540345,
0.280433083165913,0.285714285714286,0.297961045722762),.UNSPECIFIED.)
GEOMETRIC_REPRESENTATION_ITEM()
RATIONAL_B_SPLINE_SURFACE(((0.996566619267863,0.996566619267863,0.996566619267863,
0.998146249162903,1.,0.995701274206111,0.992876621380142),(0.996566619267863,
0.996566619267863,0.996566619267863,0.998146249162903,1.,0.995701274206111,
0.992876621380142)))
REPRESENTATION_ITEM('')
SURFACE()
);
#1592=(
BOUNDED_SURFACE()
B_SPLINE_SURFACE(1,2,((#120870,#120871,#120872),(#120873,#120874,#120875)),
 .UNSPECIFIED.,.F.,.F.,.F.)
B_SPLINE_SURFACE_WITH_KNOTS((2,2),(3,3),(0.,0.289681084359925),(0.43567212259767,
0.452924869174518),.UNSPECIFIED.)
GEOMETRIC_REPRESENTATION_ITEM()
RATIONAL_B_SPLINE_SURFACE(((0.995510721093622,0.990658873102333,0.988732477628005),
(0.995510721093622,0.990658873102333,0.988732477628005)))
REPRESENTATION_ITEM('')
SURFACE()
);
#1593=(
BOUNDED_SURFACE()
B_SPLINE_SURFACE(1,2,((#120877,#120878,#120879,#120880,#120881,#120882,
#120883),(#120884,#120885,#120886,#120887,#120888,#120889,#120890)),
 .UNSPECIFIED.,.F.,.F.,.F.)
B_SPLINE_SURFACE_WITH_KNOTS((2,2),(3,2,2,3),(0.,0.289807040992543),(0.280257803540345,
0.280433083165913,0.285714285714286,0.297961045722762),.UNSPECIFIED.)
GEOMETRIC_REPRESENTATION_ITEM()
RATIONAL_B_SPLINE_SURFACE(((0.996566619267863,0.996566619267863,0.996566619267863,
0.998146249162903,1.,0.995701274206111,0.992876621380142),(0.996566619267863,
0.996566619267863,0.996566619267863,0.998146249162903,1.,0.995701274206111,
0.992876621380142)))
REPRESENTATION_ITEM('')
SURFACE()
);
#1594=(
BOUNDED_SURFACE()
B_SPLINE_SURFACE(1,2,((#120913,#120914,#120915),(#120916,#120917,#120918)),
 .UNSPECIFIED.,.F.,.F.,.F.)
B_SPLINE_SURFACE_WITH_KNOTS((2,2),(3,3),(0.,0.289681084359917),(0.43567212259767,
0.452924869174518),.UNSPECIFIED.)
GEOMETRIC_REPRESENTATION_ITEM()
RATIONAL_B_SPLINE_SURFACE(((0.995510721093622,0.990658873102333,0.988732477628005),
(0.995510721093622,0.990658873102333,0.988732477628005)))
REPRESENTATION_ITEM('')
SURFACE()
);
#1595=(
BOUNDED_SURFACE()
B_SPLINE_SURFACE(1,2,((#120920,#120921,#120922,#120923,#120924,#120925,
#120926),(#120927,#120928,#120929,#120930,#120931,#120932,#120933)),
 .UNSPECIFIED.,.F.,.F.,.F.)
B_SPLINE_SURFACE_WITH_KNOTS((2,2),(3,2,2,3),(0.,0.289807040992539),(0.280257803540345,
0.280433083165913,0.285714285714286,0.297961045722762),.UNSPECIFIED.)
GEOMETRIC_REPRESENTATION_ITEM()
RATIONAL_B_SPLINE_SURFACE(((0.996566619267863,0.996566619267863,0.996566619267863,
0.998146249162903,1.,0.995701274206111,0.992876621380142),(0.996566619267863,
0.996566619267863,0.996566619267863,0.998146249162903,1.,0.995701274206111,
0.992876621380142)))
REPRESENTATION_ITEM('')
SURFACE()
);
#1596=(
BOUNDED_SURFACE()
B_SPLINE_SURFACE(1,2,((#120956,#120957,#120958),(#120959,#120960,#120961)),
 .UNSPECIFIED.,.F.,.F.,.F.)
B_SPLINE_SURFACE_WITH_KNOTS((2,2),(3,3),(0.,0.289681084359922),(0.435672122597671,
0.452924869174518),.UNSPECIFIED.)
GEOMETRIC_REPRESENTATION_ITEM()
RATIONAL_B_SPLINE_SURFACE(((0.995510721093621,0.990658873102333,0.988732477628005),
(0.995510721093622,0.990658873102333,0.988732477628005)))
REPRESENTATION_ITEM('')
SURFACE()
);
#1597=(
BOUNDED_SURFACE()
B_SPLINE_SURFACE(1,2,((#120963,#120964,#120965,#120966,#120967,#120968,
#120969),(#120970,#120971,#120972,#120973,#120974,#120975,#120976)),
 .UNSPECIFIED.,.F.,.F.,.F.)
B_SPLINE_SURFACE_WITH_KNOTS((2,2),(3,2,2,3),(0.,0.289807040992498),(0.280257803540345,
0.280433083165913,0.285714285714286,0.297961045722762),.UNSPECIFIED.)
GEOMETRIC_REPRESENTATION_ITEM()
RATIONAL_B_SPLINE_SURFACE(((0.996566619267863,0.996566619267863,0.996566619267863,
0.998146249162903,1.,0.995701274206111,0.992876621380142),(0.996566619267863,
0.996566619267863,0.996566619267863,0.998146249162903,1.,0.995701274206111,
0.992876621380142)))
REPRESENTATION_ITEM('')
SURFACE()
);
#1598=(
BOUNDED_SURFACE()
B_SPLINE_SURFACE(1,2,((#120999,#121000,#121001),(#121002,#121003,#121004)),
 .UNSPECIFIED.,.F.,.F.,.F.)
B_SPLINE_SURFACE_WITH_KNOTS((2,2),(3,3),(0.,0.289681084359914),(0.43567212259767,
0.452924869174518),.UNSPECIFIED.)
GEOMETRIC_REPRESENTATION_ITEM()
RATIONAL_B_SPLINE_SURFACE(((0.995510721093622,0.990658873102333,0.988732477628005),
(0.995510721093622,0.990658873102333,0.988732477628005)))
REPRESENTATION_ITEM('')
SURFACE()
);
#1599=(
BOUNDED_SURFACE()
B_SPLINE_SURFACE(1,2,((#121006,#121007,#121008,#121009,#121010,#121011,
#121012),(#121013,#121014,#121015,#121016,#121017,#121018,#121019)),
 .UNSPECIFIED.,.F.,.F.,.F.)
B_SPLINE_SURFACE_WITH_KNOTS((2,2),(3,2,2,3),(0.,0.289807040992513),(0.280257803540345,
0.280433083165913,0.285714285714286,0.297961045722762),.UNSPECIFIED.)
GEOMETRIC_REPRESENTATION_ITEM()
RATIONAL_B_SPLINE_SURFACE(((0.996566619267863,0.996566619267863,0.996566619267863,
0.998146249162903,1.,0.995701274206111,0.992876621380142),(0.996566619267863,
0.996566619267863,0.996566619267863,0.998146249162903,1.,0.995701274206111,
0.992876621380142)))
REPRESENTATION_ITEM('')
SURFACE()
);
#1600=(
BOUNDED_SURFACE()
B_SPLINE_SURFACE(1,2,((#121027,#121028,#121029),(#121030,#121031,#121032)),
 .UNSPECIFIED.,.F.,.F.,.F.)
B_SPLINE_SURFACE_WITH_KNOTS((2,2),(3,3),(0.,0.289681084359923),(0.43567212259767,
0.452924869174518),.UNSPECIFIED.)
GEOMETRIC_REPRESENTATION_ITEM()
RATIONAL_B_SPLINE_SURFACE(((0.995510721093622,0.990658873102333,0.988732477628005),
(0.995510721093622,0.990658873102333,0.988732477628005)))
REPRESENTATION_ITEM('')
SURFACE()
);
#1601=(
BOUNDED_SURFACE()
B_SPLINE_SURFACE(1,2,((#121034,#121035,#121036,#121037,#121038,#121039,
#121040),(#121041,#121042,#121043,#121044,#121045,#121046,#121047)),
 .UNSPECIFIED.,.F.,.F.,.F.)
B_SPLINE_SURFACE_WITH_KNOTS((2,2),(3,2,2,3),(0.,0.289807040991561),(0.280257803540345,
0.280433083165913,0.285714285714286,0.297961045722762),.UNSPECIFIED.)
GEOMETRIC_REPRESENTATION_ITEM()
RATIONAL_B_SPLINE_SURFACE(((0.996566619267863,0.996566619267863,0.996566619267863,
0.998146249162903,1.,0.995701274206111,0.992876621380142),(0.996566619267863,
0.996566619267863,0.996566619267863,0.998146249162903,1.,0.995701274206111,
0.992876621380142)))
REPRESENTATION_ITEM('')
SURFACE()
);
#1602=(
BOUNDED_SURFACE()
B_SPLINE_SURFACE(1,2,((#121070,#121071,#121072),(#121073,#121074,#121075)),
 .UNSPECIFIED.,.F.,.F.,.F.)
B_SPLINE_SURFACE_WITH_KNOTS((2,2),(3,3),(0.,0.289681084359924),(0.43567212259767,
0.452924869174518),.UNSPECIFIED.)
GEOMETRIC_REPRESENTATION_ITEM()
RATIONAL_B_SPLINE_SURFACE(((0.995510721093622,0.990658873102333,0.988732477628005),
(0.995510721093622,0.990658873102333,0.988732477628005)))
REPRESENTATION_ITEM('')
SURFACE()
);
#1603=(
BOUNDED_SURFACE()
B_SPLINE_SURFACE(1,2,((#121077,#121078,#121079,#121080,#121081,#121082,
#121083),(#121084,#121085,#121086,#121087,#121088,#121089,#121090)),
 .UNSPECIFIED.,.F.,.F.,.F.)
B_SPLINE_SURFACE_WITH_KNOTS((2,2),(3,2,2,3),(0.,0.289807040991563),(0.280257803540345,
0.280433083165913,0.285714285714286,0.297961045722762),.UNSPECIFIED.)
GEOMETRIC_REPRESENTATION_ITEM()
RATIONAL_B_SPLINE_SURFACE(((0.996566619267863,0.996566619267863,0.996566619267863,
0.998146249162903,1.,0.995701274206111,0.992876621380142),(0.996566619267863,
0.996566619267863,0.996566619267863,0.998146249162903,1.,0.995701274206111,
0.992876621380142)))
REPRESENTATION_ITEM('')
SURFACE()
);
#1604=(
BOUNDED_SURFACE()
B_SPLINE_SURFACE(1,2,((#121113,#121114,#121115),(#121116,#121117,#121118)),
 .UNSPECIFIED.,.F.,.F.,.F.)
B_SPLINE_SURFACE_WITH_KNOTS((2,2),(3,3),(0.,0.289681084359924),(0.43567212259767,
0.452924869174518),.UNSPECIFIED.)
GEOMETRIC_REPRESENTATION_ITEM()
RATIONAL_B_SPLINE_SURFACE(((0.995510721093622,0.990658873102333,0.988732477628005),
(0.995510721093622,0.990658873102333,0.988732477628005)))
REPRESENTATION_ITEM('')
SURFACE()
);
#1605=(
BOUNDED_SURFACE()
B_SPLINE_SURFACE(1,2,((#121120,#121121,#121122,#121123,#121124,#121125,
#121126),(#121127,#121128,#121129,#121130,#121131,#121132,#121133)),
 .UNSPECIFIED.,.F.,.F.,.F.)
B_SPLINE_SURFACE_WITH_KNOTS((2,2),(3,2,2,3),(0.,0.289807040991564),(0.280257803540345,
0.280433083165913,0.285714285714286,0.297961045722762),.UNSPECIFIED.)
GEOMETRIC_REPRESENTATION_ITEM()
RATIONAL_B_SPLINE_SURFACE(((0.996566619267863,0.996566619267863,0.996566619267863,
0.998146249162903,1.,0.995701274206111,0.992876621380142),(0.996566619267863,
0.996566619267863,0.996566619267863,0.998146249162903,1.,0.995701274206111,
0.992876621380142)))
REPRESENTATION_ITEM('')
SURFACE()
);
#1606=(
BOUNDED_SURFACE()
B_SPLINE_SURFACE(1,2,((#121156,#121157,#121158),(#121159,#121160,#121161)),
 .UNSPECIFIED.,.F.,.F.,.F.)
B_SPLINE_SURFACE_WITH_KNOTS((2,2),(3,3),(0.,0.289681084359998),(0.43567212259767,
0.452924869174518),.UNSPECIFIED.)
GEOMETRIC_REPRESENTATION_ITEM()
RATIONAL_B_SPLINE_SURFACE(((0.995510721093622,0.990658873102333,0.988732477628005),
(0.995510721093622,0.990658873102333,0.988732477628005)))
REPRESENTATION_ITEM('')
SURFACE()
);
#1607=(
BOUNDED_SURFACE()
B_SPLINE_SURFACE(1,2,((#121163,#121164,#121165,#121166,#121167,#121168,
#121169),(#121170,#121171,#121172,#121173,#121174,#121175,#121176)),
 .UNSPECIFIED.,.F.,.F.,.F.)
B_SPLINE_SURFACE_WITH_KNOTS((2,2),(3,2,2,3),(0.,0.289807040991565),(0.280257803540345,
0.280433083165913,0.285714285714286,0.297961045722762),.UNSPECIFIED.)
GEOMETRIC_REPRESENTATION_ITEM()
RATIONAL_B_SPLINE_SURFACE(((0.996566619267863,0.996566619267863,0.996566619267863,
0.998146249162903,1.,0.995701274206111,0.992876621380142),(0.996566619267863,
0.996566619267863,0.996566619267863,0.998146249162903,1.,0.995701274206111,
0.992876621380142)))
REPRESENTATION_ITEM('')
SURFACE()
);
#1608=(
BOUNDED_SURFACE()
B_SPLINE_SURFACE(1,2,((#121199,#121200,#121201),(#121202,#121203,#121204)),
 .UNSPECIFIED.,.F.,.F.,.F.)
B_SPLINE_SURFACE_WITH_KNOTS((2,2),(3,3),(0.,0.28968108435992),(0.43567212259767,
0.452924869174518),.UNSPECIFIED.)
GEOMETRIC_REPRESENTATION_ITEM()
RATIONAL_B_SPLINE_SURFACE(((0.995510721093622,0.990658873102333,0.988732477628006),
(0.995510721093622,0.990658873102333,0.988732477628006)))
REPRESENTATION_ITEM('')
SURFACE()
);
#1609=(
BOUNDED_SURFACE()
B_SPLINE_SURFACE(1,2,((#121206,#121207,#121208,#121209,#121210,#121211,
#121212),(#121213,#121214,#121215,#121216,#121217,#121218,#121219)),
 .UNSPECIFIED.,.F.,.F.,.F.)
B_SPLINE_SURFACE_WITH_KNOTS((2,2),(3,2,2,3),(0.,0.289807040991563),(0.280257803540345,
0.280433083165913,0.285714285714286,0.297961045722762),.UNSPECIFIED.)
GEOMETRIC_REPRESENTATION_ITEM()
RATIONAL_B_SPLINE_SURFACE(((0.996566619267863,0.996566619267863,0.996566619267863,
0.998146249162903,1.,0.995701274206111,0.992876621380142),(0.996566619267863,
0.996566619267863,0.996566619267863,0.998146249162903,1.,0.995701274206111,
0.992876621380142)))
REPRESENTATION_ITEM('')
SURFACE()
);
#1610=(
BOUNDED_SURFACE()
B_SPLINE_SURFACE(1,2,((#121242,#121243,#121244),(#121245,#121246,#121247)),
 .UNSPECIFIED.,.F.,.F.,.F.)
B_SPLINE_SURFACE_WITH_KNOTS((2,2),(3,3),(0.,0.289681084359918),(0.43567212259767,
0.452924869174518),.UNSPECIFIED.)
GEOMETRIC_REPRESENTATION_ITEM()
RATIONAL_B_SPLINE_SURFACE(((0.995510721093622,0.990658873102333,0.988732477628005),
(0.995510721093622,0.990658873102333,0.988732477628005)))
REPRESENTATION_ITEM('')
SURFACE()
);
#1611=(
BOUNDED_SURFACE()
B_SPLINE_SURFACE(1,2,((#121249,#121250,#121251,#121252,#121253,#121254,
#121255),(#121256,#121257,#121258,#121259,#121260,#121261,#121262)),
 .UNSPECIFIED.,.F.,.F.,.F.)
B_SPLINE_SURFACE_WITH_KNOTS((2,2),(3,2,2,3),(0.,0.289807040991569),(0.280257803540345,
0.280433083165913,0.285714285714286,0.297961045722762),.UNSPECIFIED.)
GEOMETRIC_REPRESENTATION_ITEM()
RATIONAL_B_SPLINE_SURFACE(((0.996566619267863,0.996566619267863,0.996566619267863,
0.998146249162903,1.,0.995701274206111,0.992876621380142),(0.996566619267863,
0.996566619267863,0.996566619267863,0.998146249162903,1.,0.995701274206111,
0.992876621380142)))
REPRESENTATION_ITEM('')
SURFACE()
);
#1612=(
BOUNDED_SURFACE()
B_SPLINE_SURFACE(1,2,((#121285,#121286,#121287),(#121288,#121289,#121290)),
 .UNSPECIFIED.,.F.,.F.,.F.)
B_SPLINE_SURFACE_WITH_KNOTS((2,2),(3,3),(0.,0.289681084359925),(0.43567212259767,
0.452924869174518),.UNSPECIFIED.)
GEOMETRIC_REPRESENTATION_ITEM()
RATIONAL_B_SPLINE_SURFACE(((0.995510721093622,0.990658873102333,0.988732477628005),
(0.995510721093622,0.990658873102333,0.988732477628005)))
REPRESENTATION_ITEM('')
SURFACE()
);
#1613=(
BOUNDED_SURFACE()
B_SPLINE_SURFACE(1,2,((#121292,#121293,#121294,#121295,#121296,#121297,
#121298),(#121299,#121300,#121301,#121302,#121303,#121304,#121305)),
 .UNSPECIFIED.,.F.,.F.,.F.)
B_SPLINE_SURFACE_WITH_KNOTS((2,2),(3,2,2,3),(0.,0.289807040991567),(0.280257803540345,
0.280433083165913,0.285714285714286,0.297961045722762),.UNSPECIFIED.)
GEOMETRIC_REPRESENTATION_ITEM()
RATIONAL_B_SPLINE_SURFACE(((0.996566619267863,0.996566619267863,0.996566619267863,
0.998146249162903,1.,0.995701274206111,0.992876621380142),(0.996566619267863,
0.996566619267863,0.996566619267863,0.998146249162903,1.,0.995701274206111,
0.992876621380142)))
REPRESENTATION_ITEM('')
SURFACE()
);
#1614=(
BOUNDED_SURFACE()
B_SPLINE_SURFACE(1,2,((#121328,#121329,#121330),(#121331,#121332,#121333)),
 .UNSPECIFIED.,.F.,.F.,.F.)
B_SPLINE_SURFACE_WITH_KNOTS((2,2),(3,3),(0.,0.289681084359924),(0.43567212259767,
0.452924869174518),.UNSPECIFIED.)
GEOMETRIC_REPRESENTATION_ITEM()
RATIONAL_B_SPLINE_SURFACE(((0.995510721093622,0.990658873102333,0.988732477628005),
(0.995510721093622,0.990658873102333,0.988732477628005)))
REPRESENTATION_ITEM('')
SURFACE()
);
#1615=(
BOUNDED_SURFACE()
B_SPLINE_SURFACE(1,2,((#121335,#121336,#121337,#121338,#121339,#121340,
#121341),(#121342,#121343,#121344,#121345,#121346,#121347,#121348)),
 .UNSPECIFIED.,.F.,.F.,.F.)
B_SPLINE_SURFACE_WITH_KNOTS((2,2),(3,2,2,3),(0.,0.289807040991561),(0.280257803540345,
0.280433083165913,0.285714285714286,0.297961045722762),.UNSPECIFIED.)
GEOMETRIC_REPRESENTATION_ITEM()
RATIONAL_B_SPLINE_SURFACE(((0.996566619267863,0.996566619267863,0.996566619267863,
0.998146249162903,1.,0.995701274206111,0.992876621380142),(0.996566619267863,
0.996566619267863,0.996566619267863,0.998146249162903,1.,0.995701274206111,
0.992876621380142)))
REPRESENTATION_ITEM('')
SURFACE()
);
#1616=(
BOUNDED_SURFACE()
B_SPLINE_SURFACE(1,2,((#121371,#121372,#121373),(#121374,#121375,#121376)),
 .UNSPECIFIED.,.F.,.F.,.F.)
B_SPLINE_SURFACE_WITH_KNOTS((2,2),(3,3),(0.,0.289681084359921),(0.43567212259767,
0.452924869174518),.UNSPECIFIED.)
GEOMETRIC_REPRESENTATION_ITEM()
RATIONAL_B_SPLINE_SURFACE(((0.995510721093622,0.990658873102333,0.988732477628005),
(0.995510721093622,0.990658873102333,0.988732477628005)))
REPRESENTATION_ITEM('')
SURFACE()
);
#1617=(
BOUNDED_SURFACE()
B_SPLINE_SURFACE(1,2,((#121378,#121379,#121380,#121381,#121382,#121383,
#121384),(#121385,#121386,#121387,#121388,#121389,#121390,#121391)),
 .UNSPECIFIED.,.F.,.F.,.F.)
B_SPLINE_SURFACE_WITH_KNOTS((2,2),(3,2,2,3),(0.,0.289807040991566),(0.280257803540345,
0.280433083165913,0.285714285714286,0.297961045722762),.UNSPECIFIED.)
GEOMETRIC_REPRESENTATION_ITEM()
RATIONAL_B_SPLINE_SURFACE(((0.996566619267863,0.996566619267863,0.996566619267863,
0.998146249162903,1.,0.995701274206111,0.992876621380142),(0.996566619267863,
0.996566619267863,0.996566619267863,0.998146249162903,1.,0.995701274206111,
0.992876621380142)))
REPRESENTATION_ITEM('')
SURFACE()
);
#1618=(
BOUNDED_SURFACE()
B_SPLINE_SURFACE(1,2,((#121414,#121415,#121416),(#121417,#121418,#121419)),
 .UNSPECIFIED.,.F.,.F.,.F.)
B_SPLINE_SURFACE_WITH_KNOTS((2,2),(3,3),(0.,0.289681084359929),(0.43567212259767,
0.452924869174518),.UNSPECIFIED.)
GEOMETRIC_REPRESENTATION_ITEM()
RATIONAL_B_SPLINE_SURFACE(((0.995510721093622,0.990658873102333,0.988732477628005),
(0.995510721093622,0.990658873102333,0.988732477628005)))
REPRESENTATION_ITEM('')
SURFACE()
);
#1619=(
BOUNDED_SURFACE()
B_SPLINE_SURFACE(1,2,((#121421,#121422,#121423,#121424,#121425,#121426,
#121427),(#121428,#121429,#121430,#121431,#121432,#121433,#121434)),
 .UNSPECIFIED.,.F.,.F.,.F.)
B_SPLINE_SURFACE_WITH_KNOTS((2,2),(3,2,2,3),(0.,0.289807040991562),(0.280257803540345,
0.280433083165913,0.285714285714286,0.297961045722762),.UNSPECIFIED.)
GEOMETRIC_REPRESENTATION_ITEM()
RATIONAL_B_SPLINE_SURFACE(((0.996566619267863,0.996566619267863,0.996566619267863,
0.998146249162903,1.,0.995701274206111,0.992876621380142),(0.996566619267863,
0.996566619267863,0.996566619267863,0.998146249162903,1.,0.995701274206111,
0.992876621380142)))
REPRESENTATION_ITEM('')
SURFACE()
);
#1620=(
BOUNDED_SURFACE()
B_SPLINE_SURFACE(1,2,((#121457,#121458,#121459),(#121460,#121461,#121462)),
 .UNSPECIFIED.,.F.,.F.,.F.)
B_SPLINE_SURFACE_WITH_KNOTS((2,2),(3,3),(0.,0.289681084359919),(0.43567212259767,
0.452924869174518),.UNSPECIFIED.)
GEOMETRIC_REPRESENTATION_ITEM()
RATIONAL_B_SPLINE_SURFACE(((0.995510721093622,0.990658873102333,0.988732477628005),
(0.995510721093622,0.990658873102333,0.988732477628005)))
REPRESENTATION_ITEM('')
SURFACE()
);
#1621=(
BOUNDED_SURFACE()
B_SPLINE_SURFACE(1,2,((#121464,#121465,#121466,#121467,#121468,#121469,
#121470),(#121471,#121472,#121473,#121474,#121475,#121476,#121477)),
 .UNSPECIFIED.,.F.,.F.,.F.)
B_SPLINE_SURFACE_WITH_KNOTS((2,2),(3,2,2,3),(0.,0.289807040991561),(0.280257803540345,
0.280433083165913,0.285714285714286,0.297961045722762),.UNSPECIFIED.)
GEOMETRIC_REPRESENTATION_ITEM()
RATIONAL_B_SPLINE_SURFACE(((0.996566619267863,0.996566619267863,0.996566619267863,
0.998146249162903,1.,0.995701274206111,0.992876621380142),(0.996566619267863,
0.996566619267863,0.996566619267863,0.998146249162903,1.,0.995701274206111,
0.992876621380142)))
REPRESENTATION_ITEM('')
SURFACE()
);
#1622=(
BOUNDED_SURFACE()
B_SPLINE_SURFACE(1,2,((#121500,#121501,#121502),(#121503,#121504,#121505)),
 .UNSPECIFIED.,.F.,.F.,.F.)
B_SPLINE_SURFACE_WITH_KNOTS((2,2),(3,3),(0.,0.289681084359921),(0.43567212259767,
0.452924869174518),.UNSPECIFIED.)
GEOMETRIC_REPRESENTATION_ITEM()
RATIONAL_B_SPLINE_SURFACE(((0.995510721093622,0.990658873102333,0.988732477628005),
(0.995510721093622,0.990658873102333,0.988732477628005)))
REPRESENTATION_ITEM('')
SURFACE()
);
#1623=(
BOUNDED_SURFACE()
B_SPLINE_SURFACE(1,2,((#121507,#121508,#121509,#121510,#121511,#121512,
#121513),(#121514,#121515,#121516,#121517,#121518,#121519,#121520)),
 .UNSPECIFIED.,.F.,.F.,.F.)
B_SPLINE_SURFACE_WITH_KNOTS((2,2),(3,2,2,3),(0.,0.28980704099156),(0.280257803540345,
0.280433083165913,0.285714285714286,0.297961045722762),.UNSPECIFIED.)
GEOMETRIC_REPRESENTATION_ITEM()
RATIONAL_B_SPLINE_SURFACE(((0.996566619267863,0.996566619267863,0.996566619267863,
0.998146249162903,1.,0.995701274206111,0.992876621380142),(0.996566619267863,
0.996566619267863,0.996566619267863,0.998146249162903,1.,0.995701274206111,
0.992876621380142)))
REPRESENTATION_ITEM('')
SURFACE()
);
#1624=(
BOUNDED_SURFACE()
B_SPLINE_SURFACE(1,2,((#121543,#121544,#121545),(#121546,#121547,#121548)),
 .UNSPECIFIED.,.F.,.F.,.F.)
B_SPLINE_SURFACE_WITH_KNOTS((2,2),(3,3),(0.,0.289681084359922),(0.43567212259767,
0.452924869174518),.UNSPECIFIED.)
GEOMETRIC_REPRESENTATION_ITEM()
RATIONAL_B_SPLINE_SURFACE(((0.995510721093622,0.990658873102333,0.988732477628005),
(0.995510721093622,0.990658873102333,0.988732477628005)))
REPRESENTATION_ITEM('')
SURFACE()
);
#1625=(
BOUNDED_SURFACE()
B_SPLINE_SURFACE(1,2,((#121550,#121551,#121552,#121553,#121554,#121555,
#121556),(#121557,#121558,#121559,#121560,#121561,#121562,#121563)),
 .UNSPECIFIED.,.F.,.F.,.F.)
B_SPLINE_SURFACE_WITH_KNOTS((2,2),(3,2,2,3),(0.,0.289807040992967),(0.280257803540345,
0.280433083165913,0.285714285714286,0.297961045722762),.UNSPECIFIED.)
GEOMETRIC_REPRESENTATION_ITEM()
RATIONAL_B_SPLINE_SURFACE(((0.996566619267863,0.996566619267863,0.996566619267863,
0.998146249162903,1.,0.995701274206111,0.992876621380142),(0.996566619267863,
0.996566619267863,0.996566619267863,0.998146249162903,1.,0.995701274206111,
0.992876621380142)))
REPRESENTATION_ITEM('')
SURFACE()
);
#1626=(
BOUNDED_SURFACE()
B_SPLINE_SURFACE(1,2,((#121586,#121587,#121588),(#121589,#121590,#121591)),
 .UNSPECIFIED.,.F.,.F.,.F.)
B_SPLINE_SURFACE_WITH_KNOTS((2,2),(3,3),(0.,0.289681084359923),(0.43567212259767,
0.452924869174518),.UNSPECIFIED.)
GEOMETRIC_REPRESENTATION_ITEM()
RATIONAL_B_SPLINE_SURFACE(((0.995510721093622,0.990658873102333,0.988732477628005),
(0.995510721093622,0.990658873102333,0.988732477628005)))
REPRESENTATION_ITEM('')
SURFACE()
);
#1627=(
BOUNDED_SURFACE()
B_SPLINE_SURFACE(1,2,((#121593,#121594,#121595,#121596,#121597,#121598,
#121599),(#121600,#121601,#121602,#121603,#121604,#121605,#121606)),
 .UNSPECIFIED.,.F.,.F.,.F.)
B_SPLINE_SURFACE_WITH_KNOTS((2,2),(3,2,2,3),(0.,0.289807040991561),(0.280257803540345,
0.280433083165913,0.285714285714286,0.297961045722762),.UNSPECIFIED.)
GEOMETRIC_REPRESENTATION_ITEM()
RATIONAL_B_SPLINE_SURFACE(((0.996566619267863,0.996566619267863,0.996566619267863,
0.998146249162903,1.,0.995701274206111,0.992876621380142),(0.996566619267863,
0.996566619267863,0.996566619267863,0.998146249162903,1.,0.995701274206111,
0.992876621380142)))
REPRESENTATION_ITEM('')
SURFACE()
);
#1628=(
BOUNDED_SURFACE()
B_SPLINE_SURFACE(1,2,((#121629,#121630,#121631),(#121632,#121633,#121634)),
 .UNSPECIFIED.,.F.,.F.,.F.)
B_SPLINE_SURFACE_WITH_KNOTS((2,2),(3,3),(0.,0.289681084359924),(0.43567212259767,
0.452924869174518),.UNSPECIFIED.)
GEOMETRIC_REPRESENTATION_ITEM()
RATIONAL_B_SPLINE_SURFACE(((0.995510721093622,0.990658873102333,0.988732477628005),
(0.995510721093622,0.990658873102333,0.988732477628005)))
REPRESENTATION_ITEM('')
SURFACE()
);
#1629=(
BOUNDED_SURFACE()
B_SPLINE_SURFACE(1,2,((#121636,#121637,#121638,#121639,#121640,#121641,
#121642),(#121643,#121644,#121645,#121646,#121647,#121648,#121649)),
 .UNSPECIFIED.,.F.,.F.,.F.)
B_SPLINE_SURFACE_WITH_KNOTS((2,2),(3,2,2,3),(0.,0.289807040991556),(0.280257803540345,
0.280433083165913,0.285714285714286,0.297961045722762),.UNSPECIFIED.)
GEOMETRIC_REPRESENTATION_ITEM()
RATIONAL_B_SPLINE_SURFACE(((0.996566619267863,0.996566619267863,0.996566619267863,
0.998146249162903,1.,0.995701274206111,0.992876621380142),(0.996566619267863,
0.996566619267863,0.996566619267863,0.998146249162903,1.,0.995701274206111,
0.992876621380142)))
REPRESENTATION_ITEM('')
SURFACE()
);
#1630=(
BOUNDED_SURFACE()
B_SPLINE_SURFACE(1,2,((#121666,#121667,#121668),(#121669,#121670,#121671)),
 .UNSPECIFIED.,.F.,.F.,.F.)
B_SPLINE_SURFACE_WITH_KNOTS((2,2),(3,3),(0.,0.28968108435992),(0.43567212259767,
0.452924869174518),.UNSPECIFIED.)
GEOMETRIC_REPRESENTATION_ITEM()
RATIONAL_B_SPLINE_SURFACE(((0.995510721093622,0.990658873102333,0.988732477628005),
(0.995510721093622,0.990658873102333,0.988732477628005)))
REPRESENTATION_ITEM('')
SURFACE()
);
#1631=(
BOUNDED_SURFACE()
B_SPLINE_SURFACE(1,2,((#121679,#121680,#121681,#121682,#121683,#121684,
#121685),(#121686,#121687,#121688,#121689,#121690,#121691,#121692)),
 .UNSPECIFIED.,.F.,.F.,.F.)
B_SPLINE_SURFACE_WITH_KNOTS((2,2),(3,2,2,3),(0.,0.28980704099156),(0.280257803540344,
0.280433083165912,0.285714285714286,0.297961045722762),.UNSPECIFIED.)
GEOMETRIC_REPRESENTATION_ITEM()
RATIONAL_B_SPLINE_SURFACE(((0.996566619267863,0.996566619267863,0.996566619267863,
0.998146249162903,1.,0.995701274206111,0.992876621380142),(0.996566619267863,
0.996566619267863,0.996566619267863,0.998146249162903,1.,0.995701274206111,
0.992876621380142)))
REPRESENTATION_ITEM('')
SURFACE()
);
#1632=(
BOUNDED_SURFACE()
B_SPLINE_SURFACE(1,2,((#121715,#121716,#121717),(#121718,#121719,#121720)),
 .UNSPECIFIED.,.F.,.F.,.F.)
B_SPLINE_SURFACE_WITH_KNOTS((2,2),(3,3),(0.,0.289681084359921),(0.43567212259767,
0.452924869174517),.UNSPECIFIED.)
GEOMETRIC_REPRESENTATION_ITEM()
RATIONAL_B_SPLINE_SURFACE(((0.995510721093622,0.990658873102333,0.988732477628006),
(0.995510721093622,0.990658873102333,0.988732477628006)))
REPRESENTATION_ITEM('')
SURFACE()
);
#1633=(
BOUNDED_SURFACE()
B_SPLINE_SURFACE(1,2,((#121722,#121723,#121724,#121725,#121726,#121727,
#121728),(#121729,#121730,#121731,#121732,#121733,#121734,#121735)),
 .UNSPECIFIED.,.F.,.F.,.F.)
B_SPLINE_SURFACE_WITH_KNOTS((2,2),(3,2,2,3),(0.,0.289807040991633),(0.280257803540346,
0.280433083165914,0.285714285714286,0.297961045722763),.UNSPECIFIED.)
GEOMETRIC_REPRESENTATION_ITEM()
RATIONAL_B_SPLINE_SURFACE(((0.996566619267864,0.996566619267864,0.996566619267864,
0.998146249162903,1.,0.99570127420611,0.992876621380141),(0.996566619267864,
0.996566619267864,0.996566619267864,0.998146249162903,1.,0.995701274206111,
0.992876621380141)))
REPRESENTATION_ITEM('')
SURFACE()
);
#1634=(
BOUNDED_SURFACE()
B_SPLINE_SURFACE(1,2,((#121758,#121759,#121760),(#121761,#121762,#121763)),
 .UNSPECIFIED.,.F.,.F.,.F.)
B_SPLINE_SURFACE_WITH_KNOTS((2,2),(3,3),(0.,0.28968108435992),(0.435672122597669,
0.452924869174531),.UNSPECIFIED.)
GEOMETRIC_REPRESENTATION_ITEM()
RATIONAL_B_SPLINE_SURFACE(((0.995510721093622,0.990658873102329,0.988732477628002),
(0.995510721093622,0.990658873102329,0.988732477628002)))
REPRESENTATION_ITEM('')
SURFACE()
);
#1635=(
BOUNDED_SURFACE()
B_SPLINE_SURFACE(1,2,((#121765,#121766,#121767,#121768,#121769,#121770,
#121771),(#121772,#121773,#121774,#121775,#121776,#121777,#121778)),
 .UNSPECIFIED.,.F.,.F.,.F.)
B_SPLINE_SURFACE_WITH_KNOTS((2,2),(3,2,2,3),(0.,0.289807040992762),(0.28025780354034,
0.280433083165908,0.285714285714286,0.297961045722763),.UNSPECIFIED.)
GEOMETRIC_REPRESENTATION_ITEM()
RATIONAL_B_SPLINE_SURFACE(((0.99656661926786,0.99656661926786,0.99656661926786,
0.998146249162901,1.,0.995701274206111,0.992876621380141),(0.99656661926786,
0.99656661926786,0.99656661926786,0.998146249162901,1.,0.995701274206111,
0.992876621380141)))
REPRESENTATION_ITEM('')
SURFACE()
);
#1636=(
BOUNDED_SURFACE()
B_SPLINE_SURFACE(1,2,((#121801,#121802,#121803),(#121804,#121805,#121806)),
 .UNSPECIFIED.,.F.,.F.,.F.)
B_SPLINE_SURFACE_WITH_KNOTS((2,2),(3,3),(0.,0.289681084359927),(0.435672122597218,
0.452924869174574),.UNSPECIFIED.)
GEOMETRIC_REPRESENTATION_ITEM()
RATIONAL_B_SPLINE_SURFACE(((0.995510721093876,0.990658873102367,0.988732477627993),
(0.995510721093876,0.990658873102368,0.988732477627993)))
REPRESENTATION_ITEM('')
SURFACE()
);
#1637=(
BOUNDED_SURFACE()
B_SPLINE_SURFACE(1,2,((#121808,#121809,#121810,#121811,#121812,#121813,
#121814),(#121815,#121816,#121817,#121818,#121819,#121820,#121821)),
 .UNSPECIFIED.,.F.,.F.,.F.)
B_SPLINE_SURFACE_WITH_KNOTS((2,2),(3,2,2,3),(0.,0.289807040992469),(0.280257803540335,
0.280433083165903,0.285714285714286,0.297961045722763),.UNSPECIFIED.)
GEOMETRIC_REPRESENTATION_ITEM()
RATIONAL_B_SPLINE_SURFACE(((0.996566619267858,0.996566619267858,0.996566619267858,
0.998146249162899,1.,0.995701274206111,0.992876621380142),(0.996566619267858,
0.996566619267858,0.996566619267858,0.998146249162899,1.,0.995701274206111,
0.992876621380142)))
REPRESENTATION_ITEM('')
SURFACE()
);
#1638=(
BOUNDED_SURFACE()
B_SPLINE_SURFACE(1,2,((#121844,#121845,#121846),(#121847,#121848,#121849)),
 .UNSPECIFIED.,.F.,.F.,.F.)
B_SPLINE_SURFACE_WITH_KNOTS((2,2),(3,3),(0.,0.289681084359916),(0.435672122597635,
0.452924869174517),.UNSPECIFIED.)
GEOMETRIC_REPRESENTATION_ITEM()
RATIONAL_B_SPLINE_SURFACE(((0.995510721093642,0.990658873102337,0.988732477628006),
(0.995510721093642,0.990658873102337,0.988732477628006)))
REPRESENTATION_ITEM('')
SURFACE()
);
#1639=(
BOUNDED_SURFACE()
B_SPLINE_SURFACE(1,2,((#121851,#121852,#121853,#121854,#121855,#121856,
#121857),(#121858,#121859,#121860,#121861,#121862,#121863,#121864)),
 .UNSPECIFIED.,.F.,.F.,.F.)
B_SPLINE_SURFACE_WITH_KNOTS((2,2),(3,2,2,3),(0.,0.289807040992393),(0.280257803540336,
0.280433083165904,0.285714285714286,0.297961045722764),.UNSPECIFIED.)
GEOMETRIC_REPRESENTATION_ITEM()
RATIONAL_B_SPLINE_SURFACE(((0.996566619267858,0.996566619267858,0.996566619267858,
0.9981462491629,1.,0.99570127420611,0.992876621380141),(0.996566619267858,
0.996566619267858,0.996566619267858,0.9981462491629,1.,0.99570127420611,
0.992876621380141)))
REPRESENTATION_ITEM('')
SURFACE()
);
#1640=(
BOUNDED_SURFACE()
B_SPLINE_SURFACE(1,2,((#121887,#121888,#121889),(#121890,#121891,#121892)),
 .UNSPECIFIED.,.F.,.F.,.F.)
B_SPLINE_SURFACE_WITH_KNOTS((2,2),(3,3),(0.,0.289681084359926),(0.435672122597471,
0.452924869174526),.UNSPECIFIED.)
GEOMETRIC_REPRESENTATION_ITEM()
RATIONAL_B_SPLINE_SURFACE(((0.995510721093734,0.990658873102352,0.988732477628003),
(0.995510721093734,0.990658873102352,0.988732477628003)))
REPRESENTATION_ITEM('')
SURFACE()
);
#1641=(
BOUNDED_SURFACE()
B_SPLINE_SURFACE(1,2,((#121894,#121895,#121896,#121897,#121898,#121899,
#121900),(#121901,#121902,#121903,#121904,#121905,#121906,#121907)),
 .UNSPECIFIED.,.F.,.F.,.F.)
B_SPLINE_SURFACE_WITH_KNOTS((2,2),(3,2,2,3),(0.,0.289807040992293),(0.280257803540338,
0.280433083165906,0.285714285714286,0.297961045722764),.UNSPECIFIED.)
GEOMETRIC_REPRESENTATION_ITEM()
RATIONAL_B_SPLINE_SURFACE(((0.996566619267859,0.996566619267859,0.996566619267859,
0.9981462491629,1.,0.99570127420611,0.992876621380141),(0.996566619267859,
0.996566619267859,0.996566619267859,0.9981462491629,1.,0.99570127420611,
0.992876621380141)))
REPRESENTATION_ITEM('')
SURFACE()
);
#1642=(
BOUNDED_SURFACE()
B_SPLINE_SURFACE(1,2,((#121930,#121931,#121932),(#121933,#121934,#121935)),
 .UNSPECIFIED.,.F.,.F.,.F.)
B_SPLINE_SURFACE_WITH_KNOTS((2,2),(3,3),(0.,0.289681084359918),(0.43567212259767,
0.452924869174518),.UNSPECIFIED.)
GEOMETRIC_REPRESENTATION_ITEM()
RATIONAL_B_SPLINE_SURFACE(((0.995510721093622,0.990658873102333,0.988732477628005),
(0.995510721093622,0.990658873102333,0.988732477628005)))
REPRESENTATION_ITEM('')
SURFACE()
);
#1643=(
BOUNDED_SURFACE()
B_SPLINE_SURFACE(1,2,((#121949,#121950,#121951,#121952,#121953,#121954,
#121955),(#121956,#121957,#121958,#121959,#121960,#121961,#121962)),
 .UNSPECIFIED.,.F.,.F.,.F.)
B_SPLINE_SURFACE_WITH_KNOTS((2,2),(3,2,2,3),(0.,0.289807040991589),(0.280257803540345,
0.280433083165913,0.285714285714286,0.297961045722762),.UNSPECIFIED.)
GEOMETRIC_REPRESENTATION_ITEM()
RATIONAL_B_SPLINE_SURFACE(((0.996566619267863,0.996566619267863,0.996566619267863,
0.998146249162903,1.,0.995701274206111,0.992876621380142),(0.996566619267863,
0.996566619267863,0.996566619267863,0.998146249162903,1.,0.995701274206111,
0.992876621380142)))
REPRESENTATION_ITEM('')
SURFACE()
);
#1644=(
BOUNDED_SURFACE()
B_SPLINE_SURFACE(1,2,((#121964,#121965,#121966),(#121967,#121968,#121969)),
 .UNSPECIFIED.,.F.,.F.,.F.)
B_SPLINE_SURFACE_WITH_KNOTS((2,2),(3,3),(0.710192959008446,1.),(0.22888337489481,
0.246056477139965),.UNSPECIFIED.)
GEOMETRIC_REPRESENTATION_ITEM()
RATIONAL_B_SPLINE_SURFACE(((0.991846493044689,0.988282393439497,0.987616798999169),
(0.991846493044689,0.988282393439497,0.987616798999169)))
REPRESENTATION_ITEM('')
SURFACE()
);
#1645=(
BOUNDED_SURFACE()
B_SPLINE_SURFACE(1,2,((#121980,#121981,#121982,#121983,#121984),(#121985,
#121986,#121987,#121988,#121989)),.UNSPECIFIED.,.F.,.F.,.F.)
B_SPLINE_SURFACE_WITH_KNOTS((2,2),(3,2,3),(0.710318915639153,1.),(0.487155140750429,
0.5,0.504719756176226),.UNSPECIFIED.)
GEOMETRIC_REPRESENTATION_ITEM()
RATIONAL_B_SPLINE_SURFACE(((0.992604240083356,0.995491335852357,1.,0.99834332202137,
0.996905579294146),(0.992604240083356,0.995491335852357,1.,0.99834332202137,
0.996905579294146)))
REPRESENTATION_ITEM('')
SURFACE()
);
#1646=(
BOUNDED_SURFACE()
B_SPLINE_SURFACE(1,2,((#122006,#122007,#122008),(#122009,#122010,#122011)),
 .UNSPECIFIED.,.F.,.F.,.F.)
B_SPLINE_SURFACE_WITH_KNOTS((2,2),(3,3),(0.710192959007513,1.),(0.22888337489481,
0.246056477139965),.UNSPECIFIED.)
GEOMETRIC_REPRESENTATION_ITEM()
RATIONAL_B_SPLINE_SURFACE(((0.991846493044689,0.988282393439497,0.987616798999169),
(0.991846493044689,0.988282393439497,0.987616798999169)))
REPRESENTATION_ITEM('')
SURFACE()
);
#1647=(
BOUNDED_SURFACE()
B_SPLINE_SURFACE(1,2,((#122019,#122020,#122021,#122022,#122023),(#122024,
#122025,#122026,#122027,#122028)),.UNSPECIFIED.,.F.,.F.,.F.)
B_SPLINE_SURFACE_WITH_KNOTS((2,2),(3,2,3),(0.710318915639152,1.),(0.487155140750429,
0.5,0.504719756176227),.UNSPECIFIED.)
GEOMETRIC_REPRESENTATION_ITEM()
RATIONAL_B_SPLINE_SURFACE(((0.992604240083356,0.995491335852357,1.,0.99834332202137,
0.996905579294146),(0.992604240083356,0.995491335852357,1.,0.99834332202137,
0.996905579294146)))
REPRESENTATION_ITEM('')
SURFACE()
);
#1648=(
BOUNDED_SURFACE()
B_SPLINE_SURFACE(1,2,((#122045,#122046,#122047),(#122048,#122049,#122050)),
 .UNSPECIFIED.,.F.,.F.,.F.)
B_SPLINE_SURFACE_WITH_KNOTS((2,2),(3,3),(0.710192959007511,1.),(0.22888337489481,
0.246056477139965),.UNSPECIFIED.)
GEOMETRIC_REPRESENTATION_ITEM()
RATIONAL_B_SPLINE_SURFACE(((0.991846493044689,0.988282393439497,0.987616798999169),
(0.991846493044689,0.988282393439497,0.987616798999169)))
REPRESENTATION_ITEM('')
SURFACE()
);
#1649=(
BOUNDED_SURFACE()
B_SPLINE_SURFACE(1,2,((#122058,#122059,#122060,#122061,#122062),(#122063,
#122064,#122065,#122066,#122067)),.UNSPECIFIED.,.F.,.F.,.F.)
B_SPLINE_SURFACE_WITH_KNOTS((2,2),(3,2,3),(0.710318915639148,1.),(0.487155140750429,
0.5,0.504719756176227),.UNSPECIFIED.)
GEOMETRIC_REPRESENTATION_ITEM()
RATIONAL_B_SPLINE_SURFACE(((0.992604240083356,0.995491335852357,1.,0.99834332202137,
0.996905579294146),(0.992604240083356,0.995491335852357,1.,0.99834332202137,
0.996905579294146)))
REPRESENTATION_ITEM('')
SURFACE()
);
#1650=(
BOUNDED_SURFACE()
B_SPLINE_SURFACE(1,2,((#122084,#122085,#122086),(#122087,#122088,#122089)),
 .UNSPECIFIED.,.F.,.F.,.F.)
B_SPLINE_SURFACE_WITH_KNOTS((2,2),(3,3),(0.71019295900751,1.),(0.22888337489481,
0.246056477139966),.UNSPECIFIED.)
GEOMETRIC_REPRESENTATION_ITEM()
RATIONAL_B_SPLINE_SURFACE(((0.991846493044689,0.988282393439497,0.987616798999169),
(0.991846493044689,0.988282393439497,0.987616798999169)))
REPRESENTATION_ITEM('')
SURFACE()
);
#1651=(
BOUNDED_SURFACE()
B_SPLINE_SURFACE(1,2,((#122097,#122098,#122099,#122100,#122101),(#122102,
#122103,#122104,#122105,#122106)),.UNSPECIFIED.,.F.,.F.,.F.)
B_SPLINE_SURFACE_WITH_KNOTS((2,2),(3,2,3),(0.710318915638565,1.),(0.487155140750429,
0.5,0.504719756176227),.UNSPECIFIED.)
GEOMETRIC_REPRESENTATION_ITEM()
RATIONAL_B_SPLINE_SURFACE(((0.992604240083356,0.995491335852357,1.,0.99834332202137,
0.996905579294146),(0.992604240083356,0.995491335852357,1.,0.99834332202137,
0.996905579294146)))
REPRESENTATION_ITEM('')
SURFACE()
);
#1652=(
BOUNDED_SURFACE()
B_SPLINE_SURFACE(1,2,((#122123,#122124,#122125),(#122126,#122127,#122128)),
 .UNSPECIFIED.,.F.,.F.,.F.)
B_SPLINE_SURFACE_WITH_KNOTS((2,2),(3,3),(0.710192959006924,1.),(0.22888337489481,
0.246056477139965),.UNSPECIFIED.)
GEOMETRIC_REPRESENTATION_ITEM()
RATIONAL_B_SPLINE_SURFACE(((0.991846493044689,0.988282393439497,0.987616798999169),
(0.991846493044689,0.988282393439497,0.987616798999169)))
REPRESENTATION_ITEM('')
SURFACE()
);
#1653=(
BOUNDED_SURFACE()
B_SPLINE_SURFACE(1,2,((#122136,#122137,#122138,#122139,#122140),(#122141,
#122142,#122143,#122144,#122145)),.UNSPECIFIED.,.F.,.F.,.F.)
B_SPLINE_SURFACE_WITH_KNOTS((2,2),(3,2,3),(0.710318915639151,1.),(0.487155140750429,
0.5,0.504719756176227),.UNSPECIFIED.)
GEOMETRIC_REPRESENTATION_ITEM()
RATIONAL_B_SPLINE_SURFACE(((0.992604240083356,0.995491335852357,1.,0.99834332202137,
0.996905579294146),(0.992604240083356,0.995491335852357,1.,0.99834332202137,
0.996905579294146)))
REPRESENTATION_ITEM('')
SURFACE()
);
#1654=(
BOUNDED_SURFACE()
B_SPLINE_SURFACE(1,2,((#122162,#122163,#122164),(#122165,#122166,#122167)),
 .UNSPECIFIED.,.F.,.F.,.F.)
B_SPLINE_SURFACE_WITH_KNOTS((2,2),(3,3),(0.710192959007512,1.),(0.22888337489481,
0.246056477139966),.UNSPECIFIED.)
GEOMETRIC_REPRESENTATION_ITEM()
RATIONAL_B_SPLINE_SURFACE(((0.991846493044689,0.988282393439497,0.987616798999169),
(0.991846493044689,0.988282393439497,0.987616798999169)))
REPRESENTATION_ITEM('')
SURFACE()
);
#1655=(
BOUNDED_SURFACE()
B_SPLINE_SURFACE(1,2,((#122175,#122176,#122177,#122178,#122179),(#122180,
#122181,#122182,#122183,#122184)),.UNSPECIFIED.,.F.,.F.,.F.)
B_SPLINE_SURFACE_WITH_KNOTS((2,2),(3,2,3),(0.710318915638566,1.),(0.487155140750429,
0.5,0.504719756176226),.UNSPECIFIED.)
GEOMETRIC_REPRESENTATION_ITEM()
RATIONAL_B_SPLINE_SURFACE(((0.992604240083356,0.995491335852357,1.,0.99834332202137,
0.996905579294146),(0.992604240083356,0.995491335852357,1.,0.99834332202137,
0.996905579294146)))
REPRESENTATION_ITEM('')
SURFACE()
);
#1656=(
BOUNDED_SURFACE()
B_SPLINE_SURFACE(1,2,((#122201,#122202,#122203),(#122204,#122205,#122206)),
 .UNSPECIFIED.,.F.,.F.,.F.)
B_SPLINE_SURFACE_WITH_KNOTS((2,2),(3,3),(0.710192959006926,1.),(0.22888337489481,
0.246056477139965),.UNSPECIFIED.)
GEOMETRIC_REPRESENTATION_ITEM()
RATIONAL_B_SPLINE_SURFACE(((0.991846493044689,0.988282393439497,0.987616798999169),
(0.991846493044689,0.988282393439497,0.987616798999169)))
REPRESENTATION_ITEM('')
SURFACE()
);
#1657=(
BOUNDED_SURFACE()
B_SPLINE_SURFACE(1,2,((#122214,#122215,#122216,#122217,#122218),(#122219,
#122220,#122221,#122222,#122223)),.UNSPECIFIED.,.F.,.F.,.F.)
B_SPLINE_SURFACE_WITH_KNOTS((2,2),(3,2,3),(0.710318915639068,1.),(0.48715514075043,
0.5,0.504719756176227),.UNSPECIFIED.)
GEOMETRIC_REPRESENTATION_ITEM()
RATIONAL_B_SPLINE_SURFACE(((0.992604240083356,0.995491335852357,1.,0.99834332202137,
0.996905579294146),(0.992604240083356,0.995491335852357,1.,0.99834332202137,
0.996905579294146)))
REPRESENTATION_ITEM('')
SURFACE()
);
#1658=(
BOUNDED_SURFACE()
B_SPLINE_SURFACE(1,2,((#122240,#122241,#122242),(#122243,#122244,#122245)),
 .UNSPECIFIED.,.F.,.F.,.F.)
B_SPLINE_SURFACE_WITH_KNOTS((2,2),(3,3),(0.71019295900743,1.),(0.228883374894809,
0.246056477139964),.UNSPECIFIED.)
GEOMETRIC_REPRESENTATION_ITEM()
RATIONAL_B_SPLINE_SURFACE(((0.991846493044689,0.988282393439498,0.987616798999169),
(0.991846493044689,0.988282393439498,0.987616798999169)))
REPRESENTATION_ITEM('')
SURFACE()
);
#1659=(
BOUNDED_SURFACE()
B_SPLINE_SURFACE(1,2,((#122253,#122254,#122255,#122256,#122257),(#122258,
#122259,#122260,#122261,#122262)),.UNSPECIFIED.,.F.,.F.,.F.)
B_SPLINE_SURFACE_WITH_KNOTS((2,2),(3,2,3),(0.710318915639073,1.),(0.48715514075043,
0.5,0.504719756176228),.UNSPECIFIED.)
GEOMETRIC_REPRESENTATION_ITEM()
RATIONAL_B_SPLINE_SURFACE(((0.992604240083356,0.995491335852357,1.,0.998343322021369,
0.996905579294145),(0.992604240083356,0.995491335852357,1.,0.998343322021369,
0.996905579294145)))
REPRESENTATION_ITEM('')
SURFACE()
);
#1660=(
BOUNDED_SURFACE()
B_SPLINE_SURFACE(1,2,((#122279,#122280,#122281),(#122282,#122283,#122284)),
 .UNSPECIFIED.,.F.,.F.,.F.)
B_SPLINE_SURFACE_WITH_KNOTS((2,2),(3,3),(0.710192959007434,1.),(0.228883374894809,
0.246056477139964),.UNSPECIFIED.)
GEOMETRIC_REPRESENTATION_ITEM()
RATIONAL_B_SPLINE_SURFACE(((0.991846493044689,0.988282393439498,0.987616798999169),
(0.991846493044689,0.988282393439498,0.987616798999169)))
REPRESENTATION_ITEM('')
SURFACE()
);
#1661=(
BOUNDED_SURFACE()
B_SPLINE_SURFACE(1,2,((#122292,#122293,#122294,#122295,#122296),(#122297,
#122298,#122299,#122300,#122301)),.UNSPECIFIED.,.F.,.F.,.F.)
B_SPLINE_SURFACE_WITH_KNOTS((2,2),(3,2,3),(0.710318915638474,1.),(0.48715514075043,
0.5,0.504719756176228),.UNSPECIFIED.)
GEOMETRIC_REPRESENTATION_ITEM()
RATIONAL_B_SPLINE_SURFACE(((0.992604240083356,0.995491335852357,1.,0.998343322021369,
0.996905579294145),(0.992604240083356,0.995491335852357,1.,0.998343322021369,
0.996905579294145)))
REPRESENTATION_ITEM('')
SURFACE()
);
#1662=(
BOUNDED_SURFACE()
B_SPLINE_SURFACE(1,2,((#122318,#122319,#122320),(#122321,#122322,#122323)),
 .UNSPECIFIED.,.F.,.F.,.F.)
B_SPLINE_SURFACE_WITH_KNOTS((2,2),(3,3),(0.710192959006835,1.),(0.228883374894809,
0.246056477139964),.UNSPECIFIED.)
GEOMETRIC_REPRESENTATION_ITEM()
RATIONAL_B_SPLINE_SURFACE(((0.991846493044689,0.988282393439498,0.987616798999169),
(0.991846493044689,0.988282393439498,0.987616798999169)))
REPRESENTATION_ITEM('')
SURFACE()
);
#1663=(
BOUNDED_SURFACE()
B_SPLINE_SURFACE(1,2,((#122331,#122332,#122333,#122334,#122335),(#122336,
#122337,#122338,#122339,#122340)),.UNSPECIFIED.,.F.,.F.,.F.)
B_SPLINE_SURFACE_WITH_KNOTS((2,2),(3,2,3),(0.710318915639067,1.),(0.48715514075043,
0.5,0.504719756176228),.UNSPECIFIED.)
GEOMETRIC_REPRESENTATION_ITEM()
RATIONAL_B_SPLINE_SURFACE(((0.992604240083356,0.995491335852357,1.,0.998343322021369,
0.996905579294145),(0.992604240083356,0.995491335852357,1.,0.998343322021369,
0.996905579294145)))
REPRESENTATION_ITEM('')
SURFACE()
);
#1664=(
BOUNDED_SURFACE()
B_SPLINE_SURFACE(1,2,((#122357,#122358,#122359),(#122360,#122361,#122362)),
 .UNSPECIFIED.,.F.,.F.,.F.)
B_SPLINE_SURFACE_WITH_KNOTS((2,2),(3,3),(0.710192959007425,1.),(0.228883374894809,
0.246056477139964),.UNSPECIFIED.)
GEOMETRIC_REPRESENTATION_ITEM()
RATIONAL_B_SPLINE_SURFACE(((0.991846493044689,0.988282393439498,0.987616798999169),
(0.991846493044689,0.988282393439498,0.987616798999169)))
REPRESENTATION_ITEM('')
SURFACE()
);
#1665=(
BOUNDED_SURFACE()
B_SPLINE_SURFACE(1,2,((#122370,#122371,#122372,#122373,#122374),(#122375,
#122376,#122377,#122378,#122379)),.UNSPECIFIED.,.F.,.F.,.F.)
B_SPLINE_SURFACE_WITH_KNOTS((2,2),(3,2,3),(0.710318915638563,1.),(0.48715514075043,
0.5,0.504719756176228),.UNSPECIFIED.)
GEOMETRIC_REPRESENTATION_ITEM()
RATIONAL_B_SPLINE_SURFACE(((0.992604240083356,0.995491335852357,1.,0.998343322021369,
0.996905579294145),(0.992604240083356,0.995491335852357,1.,0.998343322021369,
0.996905579294145)))
REPRESENTATION_ITEM('')
SURFACE()
);
#1666=(
BOUNDED_SURFACE()
B_SPLINE_SURFACE(1,2,((#122396,#122397,#122398),(#122399,#122400,#122401)),
 .UNSPECIFIED.,.F.,.F.,.F.)
B_SPLINE_SURFACE_WITH_KNOTS((2,2),(3,3),(0.710192959006925,1.),(0.228883374894809,
0.246056477139964),.UNSPECIFIED.)
GEOMETRIC_REPRESENTATION_ITEM()
RATIONAL_B_SPLINE_SURFACE(((0.991846493044689,0.988282393439498,0.987616798999169),
(0.991846493044689,0.988282393439498,0.987616798999169)))
REPRESENTATION_ITEM('')
SURFACE()
);
#1667=(
BOUNDED_SURFACE()
B_SPLINE_SURFACE(1,2,((#122409,#122410,#122411,#122412,#122413),(#122414,
#122415,#122416,#122417,#122418)),.UNSPECIFIED.,.F.,.F.,.F.)
B_SPLINE_SURFACE_WITH_KNOTS((2,2),(3,2,3),(0.71031891563906,1.),(0.48715514075043,
0.5,0.504719756176228),.UNSPECIFIED.)
GEOMETRIC_REPRESENTATION_ITEM()
RATIONAL_B_SPLINE_SURFACE(((0.992604240083356,0.995491335852357,1.,0.998343322021369,
0.996905579294145),(0.992604240083356,0.995491335852357,1.,0.998343322021369,
0.996905579294145)))
REPRESENTATION_ITEM('')
SURFACE()
);
#1668=(
BOUNDED_SURFACE()
B_SPLINE_SURFACE(1,2,((#122435,#122436,#122437),(#122438,#122439,#122440)),
 .UNSPECIFIED.,.F.,.F.,.F.)
B_SPLINE_SURFACE_WITH_KNOTS((2,2),(3,3),(0.710192959007421,1.),(0.228883374894809,
0.246056477139964),.UNSPECIFIED.)
GEOMETRIC_REPRESENTATION_ITEM()
RATIONAL_B_SPLINE_SURFACE(((0.991846493044689,0.988282393439498,0.987616798999169),
(0.991846493044689,0.988282393439498,0.987616798999169)))
REPRESENTATION_ITEM('')
SURFACE()
);
#1669=(
BOUNDED_SURFACE()
B_SPLINE_SURFACE(1,2,((#122448,#122449,#122450,#122451,#122452),(#122453,
#122454,#122455,#122456,#122457)),.UNSPECIFIED.,.F.,.F.,.F.)
B_SPLINE_SURFACE_WITH_KNOTS((2,2),(3,2,3),(0.710318915638562,1.),(0.48715514075043,
0.5,0.504719756176228),.UNSPECIFIED.)
GEOMETRIC_REPRESENTATION_ITEM()
RATIONAL_B_SPLINE_SURFACE(((0.992604240083356,0.995491335852357,1.,0.998343322021369,
0.996905579294145),(0.992604240083356,0.995491335852357,1.,0.998343322021369,
0.996905579294145)))
REPRESENTATION_ITEM('')
SURFACE()
);
#1670=(
BOUNDED_SURFACE()
B_SPLINE_SURFACE(1,2,((#122474,#122475,#122476),(#122477,#122478,#122479)),
 .UNSPECIFIED.,.F.,.F.,.F.)
B_SPLINE_SURFACE_WITH_KNOTS((2,2),(3,3),(0.710192959006918,1.),(0.228883374894809,
0.246056477139964),.UNSPECIFIED.)
GEOMETRIC_REPRESENTATION_ITEM()
RATIONAL_B_SPLINE_SURFACE(((0.991846493044689,0.988282393439498,0.987616798999169),
(0.991846493044689,0.988282393439498,0.987616798999169)))
REPRESENTATION_ITEM('')
SURFACE()
);
#1671=(
BOUNDED_SURFACE()
B_SPLINE_SURFACE(1,2,((#122487,#122488,#122489,#122490,#122491),(#122492,
#122493,#122494,#122495,#122496)),.UNSPECIFIED.,.F.,.F.,.F.)
B_SPLINE_SURFACE_WITH_KNOTS((2,2),(3,2,3),(0.710318915638789,1.),(0.48715514075043,
0.5,0.504719756176228),.UNSPECIFIED.)
GEOMETRIC_REPRESENTATION_ITEM()
RATIONAL_B_SPLINE_SURFACE(((0.992604240083356,0.995491335852357,1.,0.998343322021369,
0.996905579294145),(0.992604240083356,0.995491335852357,1.,0.998343322021369,
0.996905579294145)))
REPRESENTATION_ITEM('')
SURFACE()
);
#1672=(
BOUNDED_SURFACE()
B_SPLINE_SURFACE(1,2,((#122504,#122505,#122506),(#122507,#122508,#122509)),
 .UNSPECIFIED.,.F.,.F.,.F.)
B_SPLINE_SURFACE_WITH_KNOTS((2,2),(3,3),(0.710192959007146,1.),(0.228883374894809,
0.246056477139964),.UNSPECIFIED.)
GEOMETRIC_REPRESENTATION_ITEM()
RATIONAL_B_SPLINE_SURFACE(((0.991846493044689,0.988282393439498,0.987616798999169),
(0.991846493044689,0.988282393439498,0.987616798999169)))
REPRESENTATION_ITEM('')
SURFACE()
);
#1673=(
BOUNDED_SURFACE()
B_SPLINE_SURFACE(1,2,((#122511,#122512,#122513,#122514,#122515),(#122516,
#122517,#122518,#122519,#122520)),.UNSPECIFIED.,.F.,.F.,.F.)
B_SPLINE_SURFACE_WITH_KNOTS((2,2),(3,2,3),(0.710318915637747,1.),(0.48715514075043,
0.5,0.504719756176228),.UNSPECIFIED.)
GEOMETRIC_REPRESENTATION_ITEM()
RATIONAL_B_SPLINE_SURFACE(((0.992604240083356,0.995491335852357,1.,0.998343322021369,
0.996905579294145),(0.992604240083356,0.995491335852357,1.,0.998343322021369,
0.996905579294145)))
REPRESENTATION_ITEM('')
SURFACE()
);
#1674=(
BOUNDED_SURFACE()
B_SPLINE_SURFACE(1,2,((#122537,#122538,#122539),(#122540,#122541,#122542)),
 .UNSPECIFIED.,.F.,.F.,.F.)
B_SPLINE_SURFACE_WITH_KNOTS((2,2),(3,3),(0.710192959006102,1.),(0.228883374894809,
0.246056477139964),.UNSPECIFIED.)
GEOMETRIC_REPRESENTATION_ITEM()
RATIONAL_B_SPLINE_SURFACE(((0.991846493044689,0.988282393439498,0.987616798999169),
(0.991846493044689,0.988282393439498,0.987616798999169)))
REPRESENTATION_ITEM('')
SURFACE()
);
#1675=(
BOUNDED_SURFACE()
B_SPLINE_SURFACE(1,2,((#122550,#122551,#122552,#122553,#122554),(#122555,
#122556,#122557,#122558,#122559)),.UNSPECIFIED.,.F.,.F.,.F.)
B_SPLINE_SURFACE_WITH_KNOTS((2,2),(3,2,3),(0.710318915639029,1.),(0.48715514075043,
0.5,0.50471975617623),.UNSPECIFIED.)
GEOMETRIC_REPRESENTATION_ITEM()
RATIONAL_B_SPLINE_SURFACE(((0.992604240083356,0.995491335852357,1.,0.998343322021369,
0.996905579294144),(0.992604240083356,0.995491335852357,1.,0.998343322021369,
0.996905579294144)))
REPRESENTATION_ITEM('')
SURFACE()
);
#1676=(
BOUNDED_SURFACE()
B_SPLINE_SURFACE(1,2,((#122576,#122577,#122578),(#122579,#122580,#122581)),
 .UNSPECIFIED.,.F.,.F.,.F.)
B_SPLINE_SURFACE_WITH_KNOTS((2,2),(3,3),(0.710192959007385,1.),(0.228883374894809,
0.246056477139964),.UNSPECIFIED.)
GEOMETRIC_REPRESENTATION_ITEM()
RATIONAL_B_SPLINE_SURFACE(((0.991846493044689,0.988282393439498,0.987616798999169),
(0.991846493044689,0.988282393439498,0.987616798999169)))
REPRESENTATION_ITEM('')
SURFACE()
);
#1677=(
BOUNDED_SURFACE()
B_SPLINE_SURFACE(1,2,((#122589,#122590,#122591,#122592,#122593),(#122594,
#122595,#122596,#122597,#122598)),.UNSPECIFIED.,.F.,.F.,.F.)
B_SPLINE_SURFACE_WITH_KNOTS((2,2),(3,2,3),(0.710318915639146,1.),(0.48715514075043,
0.5,0.504719756176228),.UNSPECIFIED.)
GEOMETRIC_REPRESENTATION_ITEM()
RATIONAL_B_SPLINE_SURFACE(((0.992604240083356,0.995491335852357,1.,0.998343322021369,
0.996905579294145),(0.992604240083356,0.995491335852357,1.,0.998343322021369,
0.996905579294145)))
REPRESENTATION_ITEM('')
SURFACE()
);
#1678=(
BOUNDED_SURFACE()
B_SPLINE_SURFACE(1,2,((#122615,#122616,#122617),(#122618,#122619,#122620)),
 .UNSPECIFIED.,.F.,.F.,.F.)
B_SPLINE_SURFACE_WITH_KNOTS((2,2),(3,3),(0.710192959007501,1.),(0.228883374894809,
0.246056477139964),.UNSPECIFIED.)
GEOMETRIC_REPRESENTATION_ITEM()
RATIONAL_B_SPLINE_SURFACE(((0.991846493044689,0.988282393439498,0.987616798999169),
(0.991846493044689,0.988282393439498,0.987616798999169)))
REPRESENTATION_ITEM('')
SURFACE()
);
#1679=(
BOUNDED_SURFACE()
B_SPLINE_SURFACE(1,2,((#122628,#122629,#122630,#122631,#122632),(#122633,
#122634,#122635,#122636,#122637)),.UNSPECIFIED.,.F.,.F.,.F.)
B_SPLINE_SURFACE_WITH_KNOTS((2,2),(3,2,3),(0.710318915638505,1.),(0.48715514075043,
0.5,0.504719756176228),.UNSPECIFIED.)
GEOMETRIC_REPRESENTATION_ITEM()
RATIONAL_B_SPLINE_SURFACE(((0.992604240083356,0.995491335852357,1.,0.998343322021369,
0.996905579294145),(0.992604240083356,0.995491335852357,1.,0.998343322021369,
0.996905579294145)))
REPRESENTATION_ITEM('')
SURFACE()
);
#1680=(
BOUNDED_SURFACE()
B_SPLINE_SURFACE(1,2,((#122654,#122655,#122656),(#122657,#122658,#122659)),
 .UNSPECIFIED.,.F.,.F.,.F.)
B_SPLINE_SURFACE_WITH_KNOTS((2,2),(3,3),(0.710192959006866,1.),(0.228883374894552,
0.246056477139966),.UNSPECIFIED.)
GEOMETRIC_REPRESENTATION_ITEM()
RATIONAL_B_SPLINE_SURFACE(((0.991846493044796,0.988282393439507,0.987616798999169),
(0.991846493044796,0.988282393439507,0.987616798999169)))
REPRESENTATION_ITEM('')
SURFACE()
);
#1681=(
BOUNDED_SURFACE()
B_SPLINE_SURFACE(1,2,((#122667,#122668,#122669,#122670,#122671),(#122672,
#122673,#122674,#122675,#122676)),.UNSPECIFIED.,.F.,.F.,.F.)
B_SPLINE_SURFACE_WITH_KNOTS((2,2),(3,2,3),(0.710318915639913,1.),(0.48715514075043,
0.5,0.504719756176227),.UNSPECIFIED.)
GEOMETRIC_REPRESENTATION_ITEM()
RATIONAL_B_SPLINE_SURFACE(((0.992604240083356,0.995491335852357,1.,0.998343322021369,
0.996905579294145),(0.992604240083356,0.995491335852357,1.,0.998343322021369,
0.996905579294145)))
REPRESENTATION_ITEM('')
SURFACE()
);
#1682=(
BOUNDED_SURFACE()
B_SPLINE_SURFACE(1,2,((#122693,#122694,#122695),(#122696,#122697,#122698)),
 .UNSPECIFIED.,.F.,.F.,.F.)
B_SPLINE_SURFACE_WITH_KNOTS((2,2),(3,3),(0.710192959008272,1.),(0.228883374894663,
0.246056477139965),.UNSPECIFIED.)
GEOMETRIC_REPRESENTATION_ITEM()
RATIONAL_B_SPLINE_SURFACE(((0.99184649304475,0.988282393439503,0.987616798999169),
(0.99184649304475,0.988282393439503,0.987616798999169)))
REPRESENTATION_ITEM('')
SURFACE()
);
#1683=(
BOUNDED_SURFACE()
B_SPLINE_SURFACE(1,2,((#122706,#122707,#122708,#122709,#122710),(#122711,
#122712,#122713,#122714,#122715)),.UNSPECIFIED.,.F.,.F.,.F.)
B_SPLINE_SURFACE_WITH_KNOTS((2,2),(3,2,3),(0.710318915638763,1.),(0.48715514075043,
0.5,0.504719756176228),.UNSPECIFIED.)
GEOMETRIC_REPRESENTATION_ITEM()
RATIONAL_B_SPLINE_SURFACE(((0.992604240083356,0.995491335852357,1.,0.998343322021369,
0.996905579294145),(0.992604240083356,0.995491335852357,1.,0.998343322021369,
0.996905579294145)))
REPRESENTATION_ITEM('')
SURFACE()
);
#1684=(
BOUNDED_SURFACE()
B_SPLINE_SURFACE(1,2,((#122732,#122733,#122734),(#122735,#122736,#122737)),
 .UNSPECIFIED.,.F.,.F.,.F.)
B_SPLINE_SURFACE_WITH_KNOTS((2,2),(3,3),(0.710192959007122,1.),(0.228883374894809,
0.246056477139964),.UNSPECIFIED.)
GEOMETRIC_REPRESENTATION_ITEM()
RATIONAL_B_SPLINE_SURFACE(((0.991846493044689,0.988282393439497,0.987616798999169),
(0.991846493044689,0.988282393439497,0.987616798999169)))
REPRESENTATION_ITEM('')
SURFACE()
);
#1685=(
BOUNDED_SURFACE()
B_SPLINE_SURFACE(1,2,((#122745,#122746,#122747,#122748,#122749),(#122750,
#122751,#122752,#122753,#122754)),.UNSPECIFIED.,.F.,.F.,.F.)
B_SPLINE_SURFACE_WITH_KNOTS((2,2),(3,2,3),(0.710318915638795,1.),(0.48715514075043,
0.5,0.504719756176228),.UNSPECIFIED.)
GEOMETRIC_REPRESENTATION_ITEM()
RATIONAL_B_SPLINE_SURFACE(((0.992604240083356,0.995491335852357,1.,0.998343322021369,
0.996905579294145),(0.992604240083356,0.995491335852357,1.,0.998343322021369,
0.996905579294145)))
REPRESENTATION_ITEM('')
SURFACE()
);
#1686=(
BOUNDED_SURFACE()
B_SPLINE_SURFACE(1,2,((#122771,#122772,#122773),(#122774,#122775,#122776)),
 .UNSPECIFIED.,.F.,.F.,.F.)
B_SPLINE_SURFACE_WITH_KNOTS((2,2),(3,3),(0.710192959007302,1.),(0.228883374894523,
0.246056477139966),.UNSPECIFIED.)
GEOMETRIC_REPRESENTATION_ITEM()
RATIONAL_B_SPLINE_SURFACE(((0.991846493044808,0.988282393439508,0.987616798999169),
(0.991846493044808,0.988282393439508,0.987616798999169)))
REPRESENTATION_ITEM('')
SURFACE()
);
#1687=(
BOUNDED_SURFACE()
B_SPLINE_SURFACE(1,2,((#122784,#122785,#122786,#122787,#122788),(#122789,
#122790,#122791,#122792,#122793)),.UNSPECIFIED.,.F.,.F.,.F.)
B_SPLINE_SURFACE_WITH_KNOTS((2,2),(3,2,3),(0.710318915638241,1.),(0.48715514075043,
0.5,0.504719756176228),.UNSPECIFIED.)
GEOMETRIC_REPRESENTATION_ITEM()
RATIONAL_B_SPLINE_SURFACE(((0.992604240083356,0.995491335852357,1.,0.998343322021369,
0.996905579294145),(0.992604240083356,0.995491335852357,1.,0.998343322021369,
0.996905579294145)))
REPRESENTATION_ITEM('')
SURFACE()
);
#1688=(
BOUNDED_SURFACE()
B_SPLINE_SURFACE(1,2,((#122810,#122811,#122812),(#122813,#122814,#122815)),
 .UNSPECIFIED.,.F.,.F.,.F.)
B_SPLINE_SURFACE_WITH_KNOTS((2,2),(3,3),(0.710192959006596,1.),(0.228883374894657,
0.246056477139965),.UNSPECIFIED.)
GEOMETRIC_REPRESENTATION_ITEM()
RATIONAL_B_SPLINE_SURFACE(((0.991846493044752,0.988282393439503,0.987616798999169),
(0.991846493044752,0.988282393439503,0.987616798999169)))
REPRESENTATION_ITEM('')
SURFACE()
);
#1689=(
BOUNDED_SURFACE()
B_SPLINE_SURFACE(1,2,((#122823,#122824,#122825,#122826,#122827),(#122828,
#122829,#122830,#122831,#122832)),.UNSPECIFIED.,.F.,.F.,.F.)
B_SPLINE_SURFACE_WITH_KNOTS((2,2),(3,2,3),(0.710318915639737,1.),(0.48715514075043,
0.5,0.504719756176228),.UNSPECIFIED.)
GEOMETRIC_REPRESENTATION_ITEM()
RATIONAL_B_SPLINE_SURFACE(((0.992604240083356,0.995491335852357,1.,0.998343322021369,
0.996905579294145),(0.992604240083356,0.995491335852357,1.,0.998343322021369,
0.996905579294145)))
REPRESENTATION_ITEM('')
SURFACE()
);
#1690=(
BOUNDED_SURFACE()
B_SPLINE_SURFACE(1,2,((#122849,#122850,#122851),(#122852,#122853,#122854)),
 .UNSPECIFIED.,.F.,.F.,.F.)
B_SPLINE_SURFACE_WITH_KNOTS((2,2),(3,3),(0.710192959008097,1.),(0.228883374894707,
0.246056477139965),.UNSPECIFIED.)
GEOMETRIC_REPRESENTATION_ITEM()
RATIONAL_B_SPLINE_SURFACE(((0.991846493044731,0.988282393439501,0.987616798999169),
(0.991846493044731,0.988282393439501,0.987616798999169)))
REPRESENTATION_ITEM('')
SURFACE()
);
#1691=(
BOUNDED_SURFACE()
B_SPLINE_SURFACE(1,2,((#122862,#122863,#122864,#122865,#122866),(#122867,
#122868,#122869,#122870,#122871)),.UNSPECIFIED.,.F.,.F.,.F.)
B_SPLINE_SURFACE_WITH_KNOTS((2,2),(3,2,3),(0.710318915638587,1.),(0.48715514075043,
0.5,0.50471975617627),.UNSPECIFIED.)
GEOMETRIC_REPRESENTATION_ITEM()
RATIONAL_B_SPLINE_SURFACE(((0.992604240083356,0.995491335852357,1.,0.998343322021354,
0.996905579294119),(0.992604240083356,0.995491335852357,1.,0.998343322021354,
0.996905579294119)))
REPRESENTATION_ITEM('')
SURFACE()
);
#1692=(
BOUNDED_SURFACE()
B_SPLINE_SURFACE(1,2,((#122888,#122889,#122890),(#122891,#122892,#122893)),
 .UNSPECIFIED.,.F.,.F.,.F.)
B_SPLINE_SURFACE_WITH_KNOTS((2,2),(3,3),(0.710192959006951,1.),(0.22888337489478,
0.246056477139965),.UNSPECIFIED.)
GEOMETRIC_REPRESENTATION_ITEM()
RATIONAL_B_SPLINE_SURFACE(((0.991846493044701,0.988282393439499,0.987616798999169),
(0.991846493044701,0.988282393439499,0.987616798999169)))
REPRESENTATION_ITEM('')
SURFACE()
);
#1693=(
BOUNDED_SURFACE()
B_SPLINE_SURFACE(1,2,((#122901,#122902,#122903,#122904,#122905),(#122906,
#122907,#122908,#122909,#122910)),.UNSPECIFIED.,.F.,.F.,.F.)
B_SPLINE_SURFACE_WITH_KNOTS((2,2),(3,2,3),(0.710318915638838,1.),(0.48715514075043,
0.5,0.504719756176235),.UNSPECIFIED.)
GEOMETRIC_REPRESENTATION_ITEM()
RATIONAL_B_SPLINE_SURFACE(((0.992604240083356,0.995491335852357,1.,0.998343322021367,
0.996905579294141),(0.992604240083356,0.995491335852357,1.,0.998343322021367,
0.996905579294141)))
REPRESENTATION_ITEM('')
SURFACE()
);
#1694=(
BOUNDED_SURFACE()
B_SPLINE_SURFACE(1,2,((#122927,#122928,#122929),(#122930,#122931,#122932)),
 .UNSPECIFIED.,.F.,.F.,.F.)
B_SPLINE_SURFACE_WITH_KNOTS((2,2),(3,3),(0.710192959007197,1.),(0.228883374894804,
0.246056477139964),.UNSPECIFIED.)
GEOMETRIC_REPRESENTATION_ITEM()
RATIONAL_B_SPLINE_SURFACE(((0.991846493044691,0.988282393439498,0.987616798999169),
(0.991846493044691,0.988282393439498,0.987616798999169)))
REPRESENTATION_ITEM('')
SURFACE()
);
#1695=(
BOUNDED_SURFACE()
B_SPLINE_SURFACE(1,2,((#122940,#122941,#122942,#122943,#122944),(#122945,
#122946,#122947,#122948,#122949)),.UNSPECIFIED.,.F.,.F.,.F.)
B_SPLINE_SURFACE_WITH_KNOTS((2,2),(3,2,3),(0.710318915639088,1.),(0.48715514075043,
0.5,0.504719756176228),.UNSPECIFIED.)
GEOMETRIC_REPRESENTATION_ITEM()
RATIONAL_B_SPLINE_SURFACE(((0.992604240083356,0.995491335852357,1.,0.998343322021369,
0.996905579294145),(0.992604240083356,0.995491335852357,1.,0.998343322021369,
0.996905579294145)))
REPRESENTATION_ITEM('')
SURFACE()
);
#1696=(
BOUNDED_SURFACE()
B_SPLINE_SURFACE(1,2,((#122966,#122967,#122968),(#122969,#122970,#122971)),
 .UNSPECIFIED.,.F.,.F.,.F.)
B_SPLINE_SURFACE_WITH_KNOTS((2,2),(3,3),(0.710192959007447,1.),(0.228883374894809,
0.246056477139964),.UNSPECIFIED.)
GEOMETRIC_REPRESENTATION_ITEM()
RATIONAL_B_SPLINE_SURFACE(((0.991846493044689,0.988282393439498,0.987616798999169),
(0.991846493044689,0.988282393439498,0.987616798999169)))
REPRESENTATION_ITEM('')
SURFACE()
);
#1697=(
BOUNDED_SURFACE()
B_SPLINE_SURFACE(1,2,((#122979,#122980,#122981,#122982,#122983),(#122984,
#122985,#122986,#122987,#122988)),.UNSPECIFIED.,.F.,.F.,.F.)
B_SPLINE_SURFACE_WITH_KNOTS((2,2),(3,2,3),(0.710318915639149,1.),(0.48715514075043,
0.5,0.504719756176302),.UNSPECIFIED.)
GEOMETRIC_REPRESENTATION_ITEM()
RATIONAL_B_SPLINE_SURFACE(((0.992604240083356,0.995491335852357,1.,0.998343322021343,
0.9969055792941),(0.992604240083356,0.995491335852357,1.,0.998343322021343,
0.9969055792941)))
REPRESENTATION_ITEM('')
SURFACE()
);
#1698=(
BOUNDED_SURFACE()
B_SPLINE_SURFACE(1,2,((#123005,#123006,#123007),(#123008,#123009,#123010)),
 .UNSPECIFIED.,.F.,.F.,.F.)
B_SPLINE_SURFACE_WITH_KNOTS((2,2),(3,3),(0.710192959007517,1.),(0.228883374894809,
0.246056477139966),.UNSPECIFIED.)
GEOMETRIC_REPRESENTATION_ITEM()
RATIONAL_B_SPLINE_SURFACE(((0.991846493044689,0.988282393439497,0.987616798999169),
(0.991846493044689,0.988282393439497,0.987616798999169)))
REPRESENTATION_ITEM('')
SURFACE()
);
#1699=(
BOUNDED_SURFACE()
B_SPLINE_SURFACE(1,2,((#123018,#123019,#123020,#123021,#123022),(#123023,
#123024,#123025,#123026,#123027)),.UNSPECIFIED.,.F.,.F.,.F.)
B_SPLINE_SURFACE_WITH_KNOTS((2,2),(3,2,3),(0.710318915637906,1.),(0.487155140750422,
0.5,0.504719756176228),.UNSPECIFIED.)
GEOMETRIC_REPRESENTATION_ITEM()
RATIONAL_B_SPLINE_SURFACE(((0.992604240083352,0.995491335852354,1.,0.998343322021369,
0.996905579294145),(0.992604240083352,0.995491335852354,1.,0.998343322021369,
0.996905579294145)))
REPRESENTATION_ITEM('')
SURFACE()
);
#1700=(
BOUNDED_SURFACE()
B_SPLINE_SURFACE(1,2,((#123044,#123045,#123046),(#123047,#123048,#123049)),
 .UNSPECIFIED.,.F.,.F.,.F.)
B_SPLINE_SURFACE_WITH_KNOTS((2,2),(3,3),(0.710192959006267,1.),(0.22888337489481,
0.246056477139964),.UNSPECIFIED.)
GEOMETRIC_REPRESENTATION_ITEM()
RATIONAL_B_SPLINE_SURFACE(((0.991846493044689,0.988282393439498,0.987616798999169),
(0.991846493044689,0.988282393439498,0.987616798999169)))
REPRESENTATION_ITEM('')
SURFACE()
);
#1701=(
BOUNDED_SURFACE()
B_SPLINE_SURFACE(1,2,((#123069,#123070,#123071,#123072,#123073),(#123074,
#123075,#123076,#123077,#123078)),.UNSPECIFIED.,.F.,.F.,.F.)
B_SPLINE_SURFACE_WITH_KNOTS((2,2),(3,2,3),(0.710318915640079,1.),(0.487155140750429,
0.5,0.504719756176227),.UNSPECIFIED.)
GEOMETRIC_REPRESENTATION_ITEM()
RATIONAL_B_SPLINE_SURFACE(((0.992604240083356,0.995491335852357,1.,0.99834332202137,
0.996905579294146),(0.992604240083356,0.995491335852357,1.,0.99834332202137,
0.996905579294146)))
REPRESENTATION_ITEM('')
SURFACE()
);
#1702=(
BOUNDED_SURFACE()
B_SPLINE_SURFACE(1,2,((#123080,#123081,#123082),(#123083,#123084,#123085)),
 .UNSPECIFIED.,.F.,.F.,.F.)
B_SPLINE_SURFACE_WITH_KNOTS((2,2),(3,3),(0.710318915640052,1.),(0.262994994770441,
0.280433083165913),.UNSPECIFIED.)
GEOMETRIC_REPRESENTATION_ITEM()
RATIONAL_B_SPLINE_SURFACE(((0.989123653000982,0.991350813683903,0.996566619267863),
(0.989123653000982,0.991350813683903,0.996566619267863)))
REPRESENTATION_ITEM('')
SURFACE()
);
#1703=(
BOUNDED_SURFACE()
B_SPLINE_SURFACE(1,2,((#123094,#123095,#123096,#123097,#123098),(#123099,
#123100,#123101,#123102,#123103)),.UNSPECIFIED.,.F.,.F.,.F.)
B_SPLINE_SURFACE_WITH_KNOTS((2,2),(3,2,3),(0.709601334832402,1.),(0.452333244836385,
0.452924869174518,0.470122329512318),.UNSPECIFIED.)
GEOMETRIC_REPRESENTATION_ITEM()
RATIONAL_B_SPLINE_SURFACE(((0.988732477628005,0.988732477628005,0.988732477628005,
0.986812255267055,0.987798766302166),(0.988732477628005,0.988732477628005,
0.988732477628005,0.986812255267055,0.987798766302166)))
REPRESENTATION_ITEM('')
SURFACE()
);
#1704=(
BOUNDED_SURFACE()
B_SPLINE_SURFACE(1,2,((#123112,#123113,#123114),(#123115,#123116,#123117)),
 .UNSPECIFIED.,.F.,.F.,.F.)
B_SPLINE_SURFACE_WITH_KNOTS((2,2),(3,3),(0.710318915640047,1.),(0.262994994770441,
0.280433083165913),.UNSPECIFIED.)
GEOMETRIC_REPRESENTATION_ITEM()
RATIONAL_B_SPLINE_SURFACE(((0.989123653000982,0.991350813683903,0.996566619267863),
(0.989123653000982,0.991350813683903,0.996566619267863)))
REPRESENTATION_ITEM('')
SURFACE()
);
#1705=(
BOUNDED_SURFACE()
B_SPLINE_SURFACE(1,2,((#123119,#123120,#123121,#123122,#123123),(#123124,
#123125,#123126,#123127,#123128)),.UNSPECIFIED.,.F.,.F.,.F.)
B_SPLINE_SURFACE_WITH_KNOTS((2,2),(3,2,3),(0.709601334818244,1.),(0.452333244822231,
0.452924869174517,0.470122329512318),.UNSPECIFIED.)
GEOMETRIC_REPRESENTATION_ITEM()
RATIONAL_B_SPLINE_SURFACE(((0.988732477628005,0.988732477628005,0.988732477628005,
0.986812255267055,0.987798766302166),(0.988732477628005,0.988732477628005,
0.988732477628005,0.986812255267055,0.987798766302167)))
REPRESENTATION_ITEM('')
SURFACE()
);
#1706=(
BOUNDED_SURFACE()
B_SPLINE_SURFACE(1,2,((#123137,#123138,#123139),(#123140,#123141,#123142)),
 .UNSPECIFIED.,.F.,.F.,.F.)
B_SPLINE_SURFACE_WITH_KNOTS((2,2),(3,3),(0.71031891564004,1.),(0.262994994770441,
0.280433083165913),.UNSPECIFIED.)
GEOMETRIC_REPRESENTATION_ITEM()
RATIONAL_B_SPLINE_SURFACE(((0.989123653000982,0.991350813683903,0.996566619267863),
(0.989123653000982,0.991350813683903,0.996566619267863)))
REPRESENTATION_ITEM('')
SURFACE()
);
#1707=(
BOUNDED_SURFACE()
B_SPLINE_SURFACE(1,2,((#123144,#123145,#123146,#123147,#123148),(#123149,
#123150,#123151,#123152,#123153)),.UNSPECIFIED.,.F.,.F.,.F.)
B_SPLINE_SURFACE_WITH_KNOTS((2,2),(3,2,3),(0.70960133484095,1.),(0.452333244844927,
0.452924869174518,0.470122329512318),.UNSPECIFIED.)
GEOMETRIC_REPRESENTATION_ITEM()
RATIONAL_B_SPLINE_SURFACE(((0.988732477628005,0.988732477628005,0.988732477628005,
0.986812255267055,0.987798766302166),(0.988732477628005,0.988732477628005,
0.988732477628005,0.986812255267055,0.987798766302166)))
REPRESENTATION_ITEM('')
SURFACE()
);
#1708=(
BOUNDED_SURFACE()
B_SPLINE_SURFACE(1,2,((#123162,#123163,#123164),(#123165,#123166,#123167)),
 .UNSPECIFIED.,.F.,.F.,.F.)
B_SPLINE_SURFACE_WITH_KNOTS((2,2),(3,3),(0.710318915640049,1.),(0.262994994770441,
0.280433083165913),.UNSPECIFIED.)
GEOMETRIC_REPRESENTATION_ITEM()
RATIONAL_B_SPLINE_SURFACE(((0.989123653000982,0.991350813683903,0.996566619267863),
(0.989123653000982,0.991350813683903,0.996566619267863)))
REPRESENTATION_ITEM('')
SURFACE()
);
#1709=(
BOUNDED_SURFACE()
B_SPLINE_SURFACE(1,2,((#123169,#123170,#123171,#123172,#123173),(#123174,
#123175,#123176,#123177,#123178)),.UNSPECIFIED.,.F.,.F.,.F.)
B_SPLINE_SURFACE_WITH_KNOTS((2,2),(3,2,3),(0.709601334842905,1.),(0.452333244847841,
0.452924869174518,0.470122329512318),.UNSPECIFIED.)
GEOMETRIC_REPRESENTATION_ITEM()
RATIONAL_B_SPLINE_SURFACE(((0.988732477628005,0.988732477628005,0.988732477628005,
0.986812255267055,0.987798766302166),(0.988732477628005,0.988732477628005,
0.988732477628005,0.986812255267055,0.987798766302166)))
REPRESENTATION_ITEM('')
SURFACE()
);
#1710=(
BOUNDED_SURFACE()
B_SPLINE_SURFACE(1,2,((#123187,#123188,#123189),(#123190,#123191,#123192)),
 .UNSPECIFIED.,.F.,.F.,.F.)
B_SPLINE_SURFACE_WITH_KNOTS((2,2),(3,3),(0.710318915639097,1.),(0.262994994770441,
0.280433083165913),.UNSPECIFIED.)
GEOMETRIC_REPRESENTATION_ITEM()
RATIONAL_B_SPLINE_SURFACE(((0.989123653000982,0.991350813683903,0.996566619267863),
(0.989123653000982,0.991350813683903,0.996566619267863)))
REPRESENTATION_ITEM('')
SURFACE()
);
#1711=(
BOUNDED_SURFACE()
B_SPLINE_SURFACE(1,2,((#123194,#123195,#123196,#123197,#123198),(#123199,
#123200,#123201,#123202,#123203)),.UNSPECIFIED.,.F.,.F.,.F.)
B_SPLINE_SURFACE_WITH_KNOTS((2,2),(3,2,3),(0.709601334842701,1.),(0.452333244847627,
0.452924869174518,0.470122329512318),.UNSPECIFIED.)
GEOMETRIC_REPRESENTATION_ITEM()
RATIONAL_B_SPLINE_SURFACE(((0.988732477628005,0.988732477628005,0.988732477628005,
0.986812255267055,0.987798766302167),(0.988732477628005,0.988732477628005,
0.988732477628005,0.986812255267055,0.987798766302166)))
REPRESENTATION_ITEM('')
SURFACE()
);
#1712=(
BOUNDED_SURFACE()
B_SPLINE_SURFACE(1,2,((#123212,#123213,#123214),(#123215,#123216,#123217)),
 .UNSPECIFIED.,.F.,.F.,.F.)
B_SPLINE_SURFACE_WITH_KNOTS((2,2),(3,3),(0.710318915639107,1.),(0.262994994770441,
0.280433083165913),.UNSPECIFIED.)
GEOMETRIC_REPRESENTATION_ITEM()
RATIONAL_B_SPLINE_SURFACE(((0.989123653000982,0.991350813683903,0.996566619267863),
(0.989123653000982,0.991350813683903,0.996566619267863)))
REPRESENTATION_ITEM('')
SURFACE()
);
#1713=(
BOUNDED_SURFACE()
B_SPLINE_SURFACE(1,2,((#123219,#123220,#123221,#123222,#123223),(#123224,
#123225,#123226,#123227,#123228)),.UNSPECIFIED.,.F.,.F.,.F.)
B_SPLINE_SURFACE_WITH_KNOTS((2,2),(3,2,3),(0.709601334846431,1.),(0.45233324485132,
0.452924869174518,0.470122329512318),.UNSPECIFIED.)
GEOMETRIC_REPRESENTATION_ITEM()
RATIONAL_B_SPLINE_SURFACE(((0.988732477628005,0.988732477628005,0.988732477628005,
0.986812255267055,0.987798766302166),(0.988732477628005,0.988732477628005,
0.988732477628005,0.986812255267055,0.987798766302166)))
REPRESENTATION_ITEM('')
SURFACE()
);
#1714=(
BOUNDED_SURFACE()
B_SPLINE_SURFACE(1,2,((#123237,#123238,#123239),(#123240,#123241,#123242)),
 .UNSPECIFIED.,.F.,.F.,.F.)
B_SPLINE_SURFACE_WITH_KNOTS((2,2),(3,3),(0.710318915639146,1.),(0.262994994770441,
0.280433083165913),.UNSPECIFIED.)
GEOMETRIC_REPRESENTATION_ITEM()
RATIONAL_B_SPLINE_SURFACE(((0.989123653000982,0.991350813683903,0.996566619267863),
(0.989123653000982,0.991350813683903,0.996566619267863)))
REPRESENTATION_ITEM('')
SURFACE()
);
#1715=(
BOUNDED_SURFACE()
B_SPLINE_SURFACE(1,2,((#123244,#123245,#123246,#123247,#123248),(#123249,
#123250,#123251,#123252,#123253)),.UNSPECIFIED.,.F.,.F.,.F.)
B_SPLINE_SURFACE_WITH_KNOTS((2,2),(3,2,3),(0.70960133484861,1.),(0.452333244853516,
0.452924869174518,0.470122329512318),.UNSPECIFIED.)
GEOMETRIC_REPRESENTATION_ITEM()
RATIONAL_B_SPLINE_SURFACE(((0.988732477628005,0.988732477628005,0.988732477628005,
0.986812255267055,0.987798766302166),(0.988732477628005,0.988732477628005,
0.988732477628005,0.986812255267055,0.987798766302166)))
REPRESENTATION_ITEM('')
SURFACE()
);
#1716=(
BOUNDED_SURFACE()
B_SPLINE_SURFACE(1,2,((#123262,#123263,#123264),(#123265,#123266,#123267)),
 .UNSPECIFIED.,.F.,.F.,.F.)
B_SPLINE_SURFACE_WITH_KNOTS((2,2),(3,3),(0.710318915639129,1.),(0.262994994770441,
0.280433083165913),.UNSPECIFIED.)
GEOMETRIC_REPRESENTATION_ITEM()
RATIONAL_B_SPLINE_SURFACE(((0.989123653000982,0.991350813683903,0.996566619267863),
(0.989123653000982,0.991350813683903,0.996566619267863)))
REPRESENTATION_ITEM('')
SURFACE()
);
#1717=(
BOUNDED_SURFACE()
B_SPLINE_SURFACE(1,2,((#123269,#123270,#123271,#123272,#123273),(#123274,
#123275,#123276,#123277,#123278)),.UNSPECIFIED.,.F.,.F.,.F.)
B_SPLINE_SURFACE_WITH_KNOTS((2,2),(3,2,3),(0.709601334844663,1.),(0.452333244848607,
0.452924869174518,0.470122329512318),.UNSPECIFIED.)
GEOMETRIC_REPRESENTATION_ITEM()
RATIONAL_B_SPLINE_SURFACE(((0.988732477628005,0.988732477628005,0.988732477628005,
0.986812255267055,0.987798766302166),(0.988732477628005,0.988732477628005,
0.988732477628005,0.986812255267055,0.987798766302166)))
REPRESENTATION_ITEM('')
SURFACE()
);
#1718=(
BOUNDED_SURFACE()
B_SPLINE_SURFACE(1,2,((#123287,#123288,#123289),(#123290,#123291,#123292)),
 .UNSPECIFIED.,.F.,.F.,.F.)
B_SPLINE_SURFACE_WITH_KNOTS((2,2),(3,3),(0.710318915640079,1.),(0.262994994770441,
0.280433083165913),.UNSPECIFIED.)
GEOMETRIC_REPRESENTATION_ITEM()
RATIONAL_B_SPLINE_SURFACE(((0.989123653000982,0.991350813683903,0.996566619267863),
(0.989123653000982,0.991350813683903,0.996566619267863)))
REPRESENTATION_ITEM('')
SURFACE()
);
#1719=(
BOUNDED_SURFACE()
B_SPLINE_SURFACE(1,2,((#123294,#123295,#123296,#123297,#123298),(#123299,
#123300,#123301,#123302,#123303)),.UNSPECIFIED.,.F.,.F.,.F.)
B_SPLINE_SURFACE_WITH_KNOTS((2,2),(3,2,3),(0.709601334851136,1.),(0.452333244855082,
0.452924869174517,0.470122329512318),.UNSPECIFIED.)
GEOMETRIC_REPRESENTATION_ITEM()
RATIONAL_B_SPLINE_SURFACE(((0.988732477628005,0.988732477628005,0.988732477628005,
0.986812255267055,0.987798766302167),(0.988732477628005,0.988732477628005,
0.988732477628005,0.986812255267055,0.987798766302167)))
REPRESENTATION_ITEM('')
SURFACE()
);
#1720=(
BOUNDED_SURFACE()
B_SPLINE_SURFACE(1,2,((#123312,#123313,#123314),(#123315,#123316,#123317)),
 .UNSPECIFIED.,.F.,.F.,.F.)
B_SPLINE_SURFACE_WITH_KNOTS((2,2),(3,3),(0.71031891564008,1.),(0.262994994770441,
0.280433083165913),.UNSPECIFIED.)
GEOMETRIC_REPRESENTATION_ITEM()
RATIONAL_B_SPLINE_SURFACE(((0.989123653000982,0.991350813683903,0.996566619267863),
(0.989123653000982,0.991350813683903,0.996566619267863)))
REPRESENTATION_ITEM('')
SURFACE()
);
#1721=(
BOUNDED_SURFACE()
B_SPLINE_SURFACE(1,2,((#123319,#123320,#123321,#123322,#123323),(#123324,
#123325,#123326,#123327,#123328)),.UNSPECIFIED.,.F.,.F.,.F.)
B_SPLINE_SURFACE_WITH_KNOTS((2,2),(3,2,3),(0.709601334824955,1.),(0.452333244828901,
0.452924869174518,0.47012232951232),.UNSPECIFIED.)
GEOMETRIC_REPRESENTATION_ITEM()
RATIONAL_B_SPLINE_SURFACE(((0.988732477628005,0.988732477628005,0.988732477628005,
0.986812255267055,0.987798766302167),(0.988732477628005,0.988732477628005,
0.988732477628005,0.986812255267055,0.987798766302167)))
REPRESENTATION_ITEM('')
SURFACE()
);
#1722=(
BOUNDED_SURFACE()
B_SPLINE_SURFACE(1,2,((#123337,#123338,#123339),(#123340,#123341,#123342)),
 .UNSPECIFIED.,.F.,.F.,.F.)
B_SPLINE_SURFACE_WITH_KNOTS((2,2),(3,3),(0.710318915639993,1.),(0.262994994770443,
0.280433083165914),.UNSPECIFIED.)
GEOMETRIC_REPRESENTATION_ITEM()
RATIONAL_B_SPLINE_SURFACE(((0.989123653000983,0.991350813683904,0.996566619267864),
(0.989123653000983,0.991350813683904,0.996566619267864)))
REPRESENTATION_ITEM('')
SURFACE()
);
#1723=(
BOUNDED_SURFACE()
B_SPLINE_SURFACE(1,2,((#123344,#123345,#123346,#123347,#123348),(#123349,
#123350,#123351,#123352,#123353)),.UNSPECIFIED.,.F.,.F.,.F.)
B_SPLINE_SURFACE_WITH_KNOTS((2,2),(3,2,3),(0.709601334825716,1.),(0.452333244829658,
0.452924869174518,0.470122329512318),.UNSPECIFIED.)
GEOMETRIC_REPRESENTATION_ITEM()
RATIONAL_B_SPLINE_SURFACE(((0.988732477628005,0.988732477628005,0.988732477628005,
0.986812255267055,0.987798766302166),(0.988732477628005,0.988732477628005,
0.988732477628005,0.986812255267055,0.987798766302166)))
REPRESENTATION_ITEM('')
SURFACE()
);
#1724=(
BOUNDED_SURFACE()
B_SPLINE_SURFACE(1,2,((#123362,#123363,#123364),(#123365,#123366,#123367)),
 .UNSPECIFIED.,.F.,.F.,.F.)
B_SPLINE_SURFACE_WITH_KNOTS((2,2),(3,3),(0.710318915640073,1.),(0.262994994770443,
0.280433083165913),.UNSPECIFIED.)
GEOMETRIC_REPRESENTATION_ITEM()
RATIONAL_B_SPLINE_SURFACE(((0.989123653000983,0.991350813683904,0.996566619267863),
(0.989123653000983,0.991350813683904,0.996566619267863)))
REPRESENTATION_ITEM('')
SURFACE()
);
#1725=(
BOUNDED_SURFACE()
B_SPLINE_SURFACE(1,2,((#123369,#123370,#123371,#123372,#123373),(#123374,
#123375,#123376,#123377,#123378)),.UNSPECIFIED.,.F.,.F.,.F.)
B_SPLINE_SURFACE_WITH_KNOTS((2,2),(3,2,3),(0.709601334819264,1.),(0.452333244823207,
0.452924869174518,0.470122329512318),.UNSPECIFIED.)
GEOMETRIC_REPRESENTATION_ITEM()
RATIONAL_B_SPLINE_SURFACE(((0.988732477628005,0.988732477628005,0.988732477628005,
0.986812255267055,0.987798766302166),(0.988732477628005,0.988732477628005,
0.988732477628005,0.986812255267055,0.987798766302166)))
REPRESENTATION_ITEM('')
SURFACE()
);
#1726=(
BOUNDED_SURFACE()
B_SPLINE_SURFACE(1,2,((#123387,#123388,#123389),(#123390,#123391,#123392)),
 .UNSPECIFIED.,.F.,.F.,.F.)
B_SPLINE_SURFACE_WITH_KNOTS((2,2),(3,3),(0.710318915640082,1.),(0.262994994770441,
0.280433083165913),.UNSPECIFIED.)
GEOMETRIC_REPRESENTATION_ITEM()
RATIONAL_B_SPLINE_SURFACE(((0.989123653000982,0.991350813683903,0.996566619267863),
(0.989123653000982,0.991350813683903,0.996566619267863)))
REPRESENTATION_ITEM('')
SURFACE()
);
#1727=(
BOUNDED_SURFACE()
B_SPLINE_SURFACE(1,2,((#123394,#123395,#123396,#123397,#123398),(#123399,
#123400,#123401,#123402,#123403)),.UNSPECIFIED.,.F.,.F.,.F.)
B_SPLINE_SURFACE_WITH_KNOTS((2,2),(3,2,3),(0.709601334846308,1.),(0.452333244850251,
0.452924869174518,0.470122329512318),.UNSPECIFIED.)
GEOMETRIC_REPRESENTATION_ITEM()
RATIONAL_B_SPLINE_SURFACE(((0.988732477628005,0.988732477628005,0.988732477628005,
0.986812255267055,0.987798766302166),(0.988732477628005,0.988732477628005,
0.988732477628005,0.986812255267055,0.987798766302166)))
REPRESENTATION_ITEM('')
SURFACE()
);
#1728=(
BOUNDED_SURFACE()
B_SPLINE_SURFACE(1,2,((#123412,#123413,#123414),(#123415,#123416,#123417)),
 .UNSPECIFIED.,.F.,.F.,.F.)
B_SPLINE_SURFACE_WITH_KNOTS((2,2),(3,3),(0.710318915640072,1.),(0.262994994770441,
0.280433083165913),.UNSPECIFIED.)
GEOMETRIC_REPRESENTATION_ITEM()
RATIONAL_B_SPLINE_SURFACE(((0.989123653000982,0.991350813683903,0.996566619267863),
(0.989123653000982,0.991350813683903,0.996566619267863)))
REPRESENTATION_ITEM('')
SURFACE()
);
#1729=(
BOUNDED_SURFACE()
B_SPLINE_SURFACE(1,2,((#123419,#123420,#123421,#123422,#123423),(#123424,
#123425,#123426,#123427,#123428)),.UNSPECIFIED.,.F.,.F.,.F.)
B_SPLINE_SURFACE_WITH_KNOTS((2,2),(3,2,3),(0.70960133482498,1.),(0.452333244828929,
0.452924869174518,0.470122329512318),.UNSPECIFIED.)
GEOMETRIC_REPRESENTATION_ITEM()
RATIONAL_B_SPLINE_SURFACE(((0.988732477628005,0.988732477628005,0.988732477628005,
0.986812255267055,0.987798766302166),(0.988732477628005,0.988732477628005,
0.988732477628005,0.986812255267055,0.987798766302166)))
REPRESENTATION_ITEM('')
SURFACE()
);
#1730=(
BOUNDED_SURFACE()
B_SPLINE_SURFACE(1,2,((#123437,#123438,#123439),(#123440,#123441,#123442)),
 .UNSPECIFIED.,.F.,.F.,.F.)
B_SPLINE_SURFACE_WITH_KNOTS((2,2),(3,3),(0.710318915640073,1.),(0.262994994770441,
0.280433083165913),.UNSPECIFIED.)
GEOMETRIC_REPRESENTATION_ITEM()
RATIONAL_B_SPLINE_SURFACE(((0.989123653000982,0.991350813683903,0.996566619267864),
(0.989123653000982,0.991350813683903,0.996566619267864)))
REPRESENTATION_ITEM('')
SURFACE()
);
#1731=(
BOUNDED_SURFACE()
B_SPLINE_SURFACE(1,2,((#123444,#123445,#123446,#123447,#123448),(#123449,
#123450,#123451,#123452,#123453)),.UNSPECIFIED.,.F.,.F.,.F.)
B_SPLINE_SURFACE_WITH_KNOTS((2,2),(3,2,3),(0.709601334843721,1.),(0.452333244847661,
0.452924869174518,0.470122329512318),.UNSPECIFIED.)
GEOMETRIC_REPRESENTATION_ITEM()
RATIONAL_B_SPLINE_SURFACE(((0.988732477628005,0.988732477628005,0.988732477628005,
0.986812255267055,0.987798766302166),(0.988732477628005,0.988732477628005,
0.988732477628005,0.986812255267055,0.987798766302166)))
REPRESENTATION_ITEM('')
SURFACE()
);
#1732=(
BOUNDED_SURFACE()
B_SPLINE_SURFACE(1,2,((#123462,#123463,#123464),(#123465,#123466,#123467)),
 .UNSPECIFIED.,.F.,.F.,.F.)
B_SPLINE_SURFACE_WITH_KNOTS((2,2),(3,3),(0.710318915640077,1.),(0.262994994770441,
0.280433083165913),.UNSPECIFIED.)
GEOMETRIC_REPRESENTATION_ITEM()
RATIONAL_B_SPLINE_SURFACE(((0.989123653000982,0.991350813683903,0.996566619267863),
(0.989123653000982,0.991350813683903,0.996566619267863)))
REPRESENTATION_ITEM('')
SURFACE()
);
#1733=(
BOUNDED_SURFACE()
B_SPLINE_SURFACE(1,2,((#123469,#123470,#123471,#123472,#123473),(#123474,
#123475,#123476,#123477,#123478)),.UNSPECIFIED.,.F.,.F.,.F.)
B_SPLINE_SURFACE_WITH_KNOTS((2,2),(3,2,3),(0.709601334848688,1.),(0.452333244852634,
0.452924869174518,0.470122329512318),.UNSPECIFIED.)
GEOMETRIC_REPRESENTATION_ITEM()
RATIONAL_B_SPLINE_SURFACE(((0.988732477628005,0.988732477628005,0.988732477628005,
0.986812255267055,0.987798766302167),(0.988732477628005,0.988732477628005,
0.988732477628005,0.986812255267055,0.987798766302167)))
REPRESENTATION_ITEM('')
SURFACE()
);
#1734=(
BOUNDED_SURFACE()
B_SPLINE_SURFACE(1,2,((#123487,#123488,#123489),(#123490,#123491,#123492)),
 .UNSPECIFIED.,.F.,.F.,.F.)
B_SPLINE_SURFACE_WITH_KNOTS((2,2),(3,3),(0.710318915640071,1.),(0.262994994770441,
0.280433083165913),.UNSPECIFIED.)
GEOMETRIC_REPRESENTATION_ITEM()
RATIONAL_B_SPLINE_SURFACE(((0.989123653000982,0.991350813683903,0.996566619267863),
(0.989123653000982,0.991350813683903,0.996566619267863)))
REPRESENTATION_ITEM('')
SURFACE()
);
#1735=(
BOUNDED_SURFACE()
B_SPLINE_SURFACE(1,2,((#123494,#123495,#123496,#123497,#123498),(#123499,
#123500,#123501,#123502,#123503)),.UNSPECIFIED.,.F.,.F.,.F.)
B_SPLINE_SURFACE_WITH_KNOTS((2,2),(3,2,3),(0.709601334852901,1.),(0.452333244856846,
0.452924869174518,0.470122329512318),.UNSPECIFIED.)
GEOMETRIC_REPRESENTATION_ITEM()
RATIONAL_B_SPLINE_SURFACE(((0.988732477628005,0.988732477628005,0.988732477628005,
0.986812255267055,0.987798766302167),(0.988732477628005,0.988732477628005,
0.988732477628005,0.986812255267055,0.987798766302167)))
REPRESENTATION_ITEM('')
SURFACE()
);
#1736=(
BOUNDED_SURFACE()
B_SPLINE_SURFACE(1,2,((#123512,#123513,#123514),(#123515,#123516,#123517)),
 .UNSPECIFIED.,.F.,.F.,.F.)
B_SPLINE_SURFACE_WITH_KNOTS((2,2),(3,3),(0.710318915640077,1.),(0.262994994770441,
0.280433083165913),.UNSPECIFIED.)
GEOMETRIC_REPRESENTATION_ITEM()
RATIONAL_B_SPLINE_SURFACE(((0.989123653000982,0.991350813683903,0.996566619267863),
(0.989123653000982,0.991350813683903,0.996566619267863)))
REPRESENTATION_ITEM('')
SURFACE()
);
#1737=(
BOUNDED_SURFACE()
B_SPLINE_SURFACE(1,2,((#123519,#123520,#123521,#123522,#123523),(#123524,
#123525,#123526,#123527,#123528)),.UNSPECIFIED.,.F.,.F.,.F.)
B_SPLINE_SURFACE_WITH_KNOTS((2,2),(3,2,3),(0.70960133485792,1.),(0.452333244861864,
0.452924869174518,0.470122329512318),.UNSPECIFIED.)
GEOMETRIC_REPRESENTATION_ITEM()
RATIONAL_B_SPLINE_SURFACE(((0.988732477628005,0.988732477628005,0.988732477628005,
0.986812255267055,0.987798766302166),(0.988732477628005,0.988732477628005,
0.988732477628005,0.986812255267055,0.987798766302166)))
REPRESENTATION_ITEM('')
SURFACE()
);
#1738=(
BOUNDED_SURFACE()
B_SPLINE_SURFACE(1,2,((#123537,#123538,#123539),(#123540,#123541,#123542)),
 .UNSPECIFIED.,.F.,.F.,.F.)
B_SPLINE_SURFACE_WITH_KNOTS((2,2),(3,3),(0.710318915640081,1.),(0.262994994770441,
0.280433083165913),.UNSPECIFIED.)
GEOMETRIC_REPRESENTATION_ITEM()
RATIONAL_B_SPLINE_SURFACE(((0.989123653000982,0.991350813683903,0.996566619267863),
(0.989123653000982,0.991350813683903,0.996566619267863)))
REPRESENTATION_ITEM('')
SURFACE()
);
#1739=(
BOUNDED_SURFACE()
B_SPLINE_SURFACE(1,2,((#123544,#123545,#123546,#123547,#123548),(#123549,
#123550,#123551,#123552,#123553)),.UNSPECIFIED.,.F.,.F.,.F.)
B_SPLINE_SURFACE_WITH_KNOTS((2,2),(3,2,3),(0.709601334827665,1.),(0.45233324483161,
0.452924869174518,0.470122329512318),.UNSPECIFIED.)
GEOMETRIC_REPRESENTATION_ITEM()
RATIONAL_B_SPLINE_SURFACE(((0.988732477628005,0.988732477628005,0.988732477628005,
0.986812255267055,0.987798766302166),(0.988732477628005,0.988732477628005,
0.988732477628005,0.986812255267055,0.987798766302166)))
REPRESENTATION_ITEM('')
SURFACE()
);
#1740=(
BOUNDED_SURFACE()
B_SPLINE_SURFACE(1,2,((#123562,#123563,#123564),(#123565,#123566,#123567)),
 .UNSPECIFIED.,.F.,.F.,.F.)
B_SPLINE_SURFACE_WITH_KNOTS((2,2),(3,3),(0.710318915640078,1.),(0.262994994770441,
0.280433083165913),.UNSPECIFIED.)
GEOMETRIC_REPRESENTATION_ITEM()
RATIONAL_B_SPLINE_SURFACE(((0.989123653000982,0.991350813683903,0.996566619267863),
(0.989123653000982,0.991350813683903,0.996566619267863)))
REPRESENTATION_ITEM('')
SURFACE()
);
#1741=(
BOUNDED_SURFACE()
B_SPLINE_SURFACE(1,2,((#123569,#123570,#123571,#123572,#123573),(#123574,
#123575,#123576,#123577,#123578)),.UNSPECIFIED.,.F.,.F.,.F.)
B_SPLINE_SURFACE_WITH_KNOTS((2,2),(3,2,3),(0.70960133482239,1.),(0.452333244827756,
0.452924869174518,0.470122329512318),.UNSPECIFIED.)
GEOMETRIC_REPRESENTATION_ITEM()
RATIONAL_B_SPLINE_SURFACE(((0.988732477628005,0.988732477628005,0.988732477628005,
0.986812255267055,0.987798766302166),(0.988732477628005,0.988732477628005,
0.988732477628005,0.986812255267055,0.987798766302166)))
REPRESENTATION_ITEM('')
SURFACE()
);
#1742=(
BOUNDED_SURFACE()
B_SPLINE_SURFACE(1,2,((#123587,#123588,#123589),(#123590,#123591,#123592)),
 .UNSPECIFIED.,.F.,.F.,.F.)
B_SPLINE_SURFACE_WITH_KNOTS((2,2),(3,3),(0.710318915638669,1.),(0.262994994770441,
0.280433083165913),.UNSPECIFIED.)
GEOMETRIC_REPRESENTATION_ITEM()
RATIONAL_B_SPLINE_SURFACE(((0.989123653000982,0.991350813683903,0.996566619267863),
(0.989123653000982,0.991350813683903,0.996566619267863)))
REPRESENTATION_ITEM('')
SURFACE()
);
#1743=(
BOUNDED_SURFACE()
B_SPLINE_SURFACE(1,2,((#123594,#123595,#123596,#123597,#123598),(#123599,
#123600,#123601,#123602,#123603)),.UNSPECIFIED.,.F.,.F.,.F.)
B_SPLINE_SURFACE_WITH_KNOTS((2,2),(3,2,3),(0.709601334823023,1.),(0.452333244826969,
0.452924869174518,0.470122329512318),.UNSPECIFIED.)
GEOMETRIC_REPRESENTATION_ITEM()
RATIONAL_B_SPLINE_SURFACE(((0.988732477628005,0.988732477628005,0.988732477628005,
0.986812255267055,0.987798766302166),(0.988732477628005,0.988732477628005,
0.988732477628005,0.986812255267055,0.987798766302166)))
REPRESENTATION_ITEM('')
SURFACE()
);
#1744=(
BOUNDED_SURFACE()
B_SPLINE_SURFACE(1,2,((#123612,#123613,#123614),(#123615,#123616,#123617)),
 .UNSPECIFIED.,.F.,.F.,.F.)
B_SPLINE_SURFACE_WITH_KNOTS((2,2),(3,3),(0.710318915640086,1.),(0.262994994770441,
0.280433083165913),.UNSPECIFIED.)
GEOMETRIC_REPRESENTATION_ITEM()
RATIONAL_B_SPLINE_SURFACE(((0.989123653000982,0.991350813683903,0.996566619267863),
(0.989123653000982,0.991350813683903,0.996566619267863)))
REPRESENTATION_ITEM('')
SURFACE()
);
#1745=(
BOUNDED_SURFACE()
B_SPLINE_SURFACE(1,2,((#123619,#123620,#123621,#123622,#123623),(#123624,
#123625,#123626,#123627,#123628)),.UNSPECIFIED.,.F.,.F.,.F.)
B_SPLINE_SURFACE_WITH_KNOTS((2,2),(3,2,3),(0.709601334842211,1.),(0.452333244846155,
0.452924869174518,0.47012232951232),.UNSPECIFIED.)
GEOMETRIC_REPRESENTATION_ITEM()
RATIONAL_B_SPLINE_SURFACE(((0.988732477628005,0.988732477628005,0.988732477628005,
0.986812255267055,0.987798766302167),(0.988732477628005,0.988732477628005,
0.988732477628005,0.986812255267055,0.987798766302167)))
REPRESENTATION_ITEM('')
SURFACE()
);
#1746=(
BOUNDED_SURFACE()
B_SPLINE_SURFACE(1,2,((#123637,#123638,#123639),(#123640,#123641,#123642)),
 .UNSPECIFIED.,.F.,.F.,.F.)
B_SPLINE_SURFACE_WITH_KNOTS((2,2),(3,3),(0.710318915640079,1.),(0.262994994770444,
0.280433083165913),.UNSPECIFIED.)
GEOMETRIC_REPRESENTATION_ITEM()
RATIONAL_B_SPLINE_SURFACE(((0.989123653000983,0.991350813683904,0.996566619267863),
(0.989123653000983,0.991350813683904,0.996566619267863)))
REPRESENTATION_ITEM('')
SURFACE()
);
#1747=(
BOUNDED_SURFACE()
B_SPLINE_SURFACE(1,2,((#123644,#123645,#123646,#123647,#123648),(#123649,
#123650,#123651,#123652,#123653)),.UNSPECIFIED.,.F.,.F.,.F.)
B_SPLINE_SURFACE_WITH_KNOTS((2,2),(3,2,3),(0.709601334832975,1.),(0.452333244836997,
0.452924869174517,0.470122329512317),.UNSPECIFIED.)
GEOMETRIC_REPRESENTATION_ITEM()
RATIONAL_B_SPLINE_SURFACE(((0.988732477628005,0.988732477628005,0.988732477628005,
0.986812255267055,0.987798766302166),(0.988732477628005,0.988732477628005,
0.988732477628005,0.986812255267055,0.987798766302166)))
REPRESENTATION_ITEM('')
SURFACE()
);
#1748=(
BOUNDED_SURFACE()
B_SPLINE_SURFACE(1,2,((#123662,#123663,#123664),(#123665,#123666,#123667)),
 .UNSPECIFIED.,.F.,.F.,.F.)
B_SPLINE_SURFACE_WITH_KNOTS((2,2),(3,3),(0.710318915640007,1.),(0.262994994770442,
0.280433083165914),.UNSPECIFIED.)
GEOMETRIC_REPRESENTATION_ITEM()
RATIONAL_B_SPLINE_SURFACE(((0.989123653000982,0.991350813683904,0.996566619267864),
(0.989123653000982,0.991350813683904,0.996566619267864)))
REPRESENTATION_ITEM('')
SURFACE()
);
#1749=(
BOUNDED_SURFACE()
B_SPLINE_SURFACE(1,2,((#123669,#123670,#123671,#123672,#123673),(#123674,
#123675,#123676,#123677,#123678)),.UNSPECIFIED.,.F.,.F.,.F.)
B_SPLINE_SURFACE_WITH_KNOTS((2,2),(3,2,3),(0.709601334848041,1.),(0.452333244852061,
0.452924869174517,0.470122329512317),.UNSPECIFIED.)
GEOMETRIC_REPRESENTATION_ITEM()
RATIONAL_B_SPLINE_SURFACE(((0.988732477628006,0.988732477628006,0.988732477628006,
0.986812255267055,0.987798766302166),(0.988732477628006,0.988732477628006,
0.988732477628006,0.986812255267055,0.987798766302166)))
REPRESENTATION_ITEM('')
SURFACE()
);
#1750=(
BOUNDED_SURFACE()
B_SPLINE_SURFACE(1,2,((#123687,#123688,#123689),(#123690,#123691,#123692)),
 .UNSPECIFIED.,.F.,.F.,.F.)
B_SPLINE_SURFACE_WITH_KNOTS((2,2),(3,3),(0.710318915640003,1.),(0.262994994770442,
0.280433083165929),.UNSPECIFIED.)
GEOMETRIC_REPRESENTATION_ITEM()
RATIONAL_B_SPLINE_SURFACE(((0.989123653000982,0.991350813683906,0.996566619267873),
(0.989123653000982,0.991350813683906,0.996566619267873)))
REPRESENTATION_ITEM('')
SURFACE()
);
#1751=(
BOUNDED_SURFACE()
B_SPLINE_SURFACE(1,2,((#123694,#123695,#123696,#123697,#123698),(#123699,
#123700,#123701,#123702,#123703)),.UNSPECIFIED.,.F.,.F.,.F.)
B_SPLINE_SURFACE_WITH_KNOTS((2,2),(3,2,3),(0.709601334840422,1.),(0.452333244845542,
0.45292486917451,0.470122329512317),.UNSPECIFIED.)
GEOMETRIC_REPRESENTATION_ITEM()
RATIONAL_B_SPLINE_SURFACE(((0.988732477628007,0.988732477628007,0.988732477628007,
0.986812255267055,0.987798766302166),(0.988732477628007,0.988732477628007,
0.988732477628007,0.986812255267055,0.987798766302166)))
REPRESENTATION_ITEM('')
SURFACE()
);
#1752=(
BOUNDED_SURFACE()
B_SPLINE_SURFACE(1,2,((#123712,#123713,#123714),(#123715,#123716,#123717)),
 .UNSPECIFIED.,.F.,.F.,.F.)
B_SPLINE_SURFACE_WITH_KNOTS((2,2),(3,3),(0.710318915639402,1.),(0.262994994770442,
0.280433083165975),.UNSPECIFIED.)
GEOMETRIC_REPRESENTATION_ITEM()
RATIONAL_B_SPLINE_SURFACE(((0.989123653000982,0.991350813683911,0.9965666192679),
(0.989123653000982,0.991350813683911,0.9965666192679)))
REPRESENTATION_ITEM('')
SURFACE()
);
#1753=(
BOUNDED_SURFACE()
B_SPLINE_SURFACE(1,2,((#123719,#123720,#123721,#123722,#123723),(#123724,
#123725,#123726,#123727,#123728)),.UNSPECIFIED.,.F.,.F.,.F.)
B_SPLINE_SURFACE_WITH_KNOTS((2,2),(3,2,3),(0.709601334835961,1.),(0.452333244840766,
0.452924869174507,0.470122329512317),.UNSPECIFIED.)
GEOMETRIC_REPRESENTATION_ITEM()
RATIONAL_B_SPLINE_SURFACE(((0.988732477628008,0.988732477628008,0.988732477628008,
0.986812255267055,0.987798766302166),(0.988732477628008,0.988732477628008,
0.988732477628008,0.986812255267055,0.987798766302166)))
REPRESENTATION_ITEM('')
SURFACE()
);
#1754=(
BOUNDED_SURFACE()
B_SPLINE_SURFACE(1,2,((#123737,#123738,#123739),(#123740,#123741,#123742)),
 .UNSPECIFIED.,.F.,.F.,.F.)
B_SPLINE_SURFACE_WITH_KNOTS((2,2),(3,3),(0.710318915640031,1.),(0.262994994770442,
0.280433083165914),.UNSPECIFIED.)
GEOMETRIC_REPRESENTATION_ITEM()
RATIONAL_B_SPLINE_SURFACE(((0.989123653000982,0.991350813683904,0.996566619267864),
(0.989123653000982,0.991350813683904,0.996566619267864)))
REPRESENTATION_ITEM('')
SURFACE()
);
#1755=(
BOUNDED_SURFACE()
B_SPLINE_SURFACE(1,2,((#123744,#123745,#123746,#123747,#123748),(#123749,
#123750,#123751,#123752,#123753)),.UNSPECIFIED.,.F.,.F.,.F.)
B_SPLINE_SURFACE_WITH_KNOTS((2,2),(3,2,3),(0.7096013348319,1.),(0.452333244836634,
0.452924869174508,0.470122329512317),.UNSPECIFIED.)
GEOMETRIC_REPRESENTATION_ITEM()
RATIONAL_B_SPLINE_SURFACE(((0.988732477628008,0.988732477628008,0.988732477628008,
0.986812255267055,0.987798766302166),(0.988732477628008,0.988732477628008,
0.988732477628008,0.986812255267055,0.987798766302166)))
REPRESENTATION_ITEM('')
SURFACE()
);
#1756=(
BOUNDED_SURFACE()
B_SPLINE_SURFACE(1,2,((#123762,#123763,#123764),(#123765,#123766,#123767)),
 .UNSPECIFIED.,.F.,.F.,.F.)
B_SPLINE_SURFACE_WITH_KNOTS((2,2),(3,3),(0.710318915640007,1.),(0.262994994770442,
0.280433083165924),.UNSPECIFIED.)
GEOMETRIC_REPRESENTATION_ITEM()
RATIONAL_B_SPLINE_SURFACE(((0.989123653000982,0.991350813683905,0.99656661926787),
(0.989123653000982,0.991350813683905,0.99656661926787)))
REPRESENTATION_ITEM('')
SURFACE()
);
#1757=(
BOUNDED_SURFACE()
B_SPLINE_SURFACE(1,2,((#123769,#123770,#123771,#123772,#123773),(#123774,
#123775,#123776,#123777,#123778)),.UNSPECIFIED.,.F.,.F.,.F.)
B_SPLINE_SURFACE_WITH_KNOTS((2,2),(3,2,3),(0.709601334846721,1.),(0.45233324485136,
0.452924869174509,0.470122329512317),.UNSPECIFIED.)
GEOMETRIC_REPRESENTATION_ITEM()
RATIONAL_B_SPLINE_SURFACE(((0.988732477628007,0.988732477628007,0.988732477628007,
0.986812255267055,0.987798766302166),(0.988732477628007,0.988732477628007,
0.988732477628007,0.986812255267055,0.987798766302166)))
REPRESENTATION_ITEM('')
SURFACE()
);
#1758=(
BOUNDED_SURFACE()
B_SPLINE_SURFACE(1,2,((#123787,#123788,#123789),(#123790,#123791,#123792)),
 .UNSPECIFIED.,.F.,.F.,.F.)
B_SPLINE_SURFACE_WITH_KNOTS((2,2),(3,3),(0.710318915640024,1.),(0.262994994770442,
0.280433083165913),.UNSPECIFIED.)
GEOMETRIC_REPRESENTATION_ITEM()
RATIONAL_B_SPLINE_SURFACE(((0.989123653000982,0.991350813683904,0.996566619267864),
(0.989123653000982,0.991350813683904,0.996566619267863)))
REPRESENTATION_ITEM('')
SURFACE()
);
#1759=(
BOUNDED_SURFACE()
B_SPLINE_SURFACE(1,2,((#123794,#123795,#123796,#123797,#123798),(#123799,
#123800,#123801,#123802,#123803)),.UNSPECIFIED.,.F.,.F.,.F.)
B_SPLINE_SURFACE_WITH_KNOTS((2,2),(3,2,3),(0.709601334834013,1.),(0.452333244838054,
0.452924869174518,0.470122329512318),.UNSPECIFIED.)
GEOMETRIC_REPRESENTATION_ITEM()
RATIONAL_B_SPLINE_SURFACE(((0.988732477628005,0.988732477628005,0.988732477628005,
0.986812255267055,0.987798766302166),(0.988732477628005,0.988732477628005,
0.988732477628005,0.986812255267055,0.987798766302166)))
REPRESENTATION_ITEM('')
SURFACE()
);
#1760=(
BOUNDED_SURFACE()
B_SPLINE_SURFACE(1,2,((#123805,#123806,#123807,#123808,#123809),(#123810,
#123811,#123812,#123813,#123814)),.UNSPECIFIED.,.F.,.F.,.F.)
B_SPLINE_SURFACE_WITH_KNOTS((2,2),(3,2,3),(0.,0.289807040992964),(0.504546746573287,
0.504719756176205,0.52202071646804),.UNSPECIFIED.)
GEOMETRIC_REPRESENTATION_ITEM()
RATIONAL_B_SPLINE_SURFACE(((0.996905579294159,0.996905579294159,0.996905579294159,
0.991635321911186,0.989306890555884),(0.996905579294159,0.996905579294159,
0.996905579294159,0.991635321911186,0.989306890555885)))
REPRESENTATION_ITEM('')
SURFACE()
);
#1761=(
BOUNDED_SURFACE()
B_SPLINE_SURFACE(1,2,((#123827,#123828,#123829,#123830,#123831,#123832,
#123833),(#123834,#123835,#123836,#123837,#123838,#123839,#123840)),
 .UNSPECIFIED.,.F.,.F.,.F.)
B_SPLINE_SURFACE_WITH_KNOTS((2,2),(3,2,2,3),(0.,0.289681084359915),(0.211398300093701,
0.214285714285714,0.22888337489481,0.229058225642821),.UNSPECIFIED.)
GEOMETRIC_REPRESENTATION_ITEM()
RATIONAL_B_SPLINE_SURFACE(((0.998054921708739,0.998986490969345,1.,0.994876086397763,
0.991846493044689,0.991846493044689,0.991846493044689),(0.998054921708739,
0.998986490969345,1.,0.994876086397763,0.991846493044689,0.991846493044689,
0.991846493044689)))
REPRESENTATION_ITEM('')
SURFACE()
);
#1762=(
BOUNDED_SURFACE()
B_SPLINE_SURFACE(1,2,((#123862,#123863,#123864,#123865,#123866),(#123867,
#123868,#123869,#123870,#123871)),.UNSPECIFIED.,.F.,.F.,.F.)
B_SPLINE_SURFACE_WITH_KNOTS((2,2),(3,2,3),(0.,0.2898070409939),(0.504546746573287,
0.504719756176205,0.52202071646804),.UNSPECIFIED.)
GEOMETRIC_REPRESENTATION_ITEM()
RATIONAL_B_SPLINE_SURFACE(((0.996905579294159,0.996905579294159,0.996905579294159,
0.991635321911186,0.989306890555885),(0.996905579294159,0.996905579294159,
0.996905579294159,0.991635321911186,0.989306890555885)))
REPRESENTATION_ITEM('')
SURFACE()
);
#1763=(
BOUNDED_SURFACE()
B_SPLINE_SURFACE(1,2,((#123873,#123874,#123875,#123876,#123877,#123878,
#123879),(#123880,#123881,#123882,#123883,#123884,#123885,#123886)),
 .UNSPECIFIED.,.F.,.F.,.F.)
B_SPLINE_SURFACE_WITH_KNOTS((2,2),(3,2,2,3),(0.,0.289681084359916),(0.211398300093701,
0.214285714285714,0.22888337489481,0.229058225642821),.UNSPECIFIED.)
GEOMETRIC_REPRESENTATION_ITEM()
RATIONAL_B_SPLINE_SURFACE(((0.998054921708739,0.998986490969345,1.,0.994876086397763,
0.991846493044689,0.991846493044689,0.991846493044689),(0.998054921708739,
0.998986490969345,1.,0.994876086397763,0.991846493044689,0.991846493044689,
0.991846493044689)))
REPRESENTATION_ITEM('')
SURFACE()
);
#1764=(
BOUNDED_SURFACE()
B_SPLINE_SURFACE(1,2,((#123903,#123904,#123905,#123906,#123907),(#123908,
#123909,#123910,#123911,#123912)),.UNSPECIFIED.,.F.,.F.,.F.)
B_SPLINE_SURFACE_WITH_KNOTS((2,2),(3,2,3),(0.,0.289807040993896),(0.504546746573287,
0.504719756176205,0.52202071646804),.UNSPECIFIED.)
GEOMETRIC_REPRESENTATION_ITEM()
RATIONAL_B_SPLINE_SURFACE(((0.996905579294159,0.996905579294159,0.996905579294159,
0.991635321911186,0.989306890555885),(0.996905579294159,0.996905579294159,
0.996905579294159,0.991635321911186,0.989306890555885)))
REPRESENTATION_ITEM('')
SURFACE()
);
#1765=(
BOUNDED_SURFACE()
B_SPLINE_SURFACE(1,2,((#123914,#123915,#123916,#123917,#123918,#123919,
#123920),(#123921,#123922,#123923,#123924,#123925,#123926,#123927)),
 .UNSPECIFIED.,.F.,.F.,.F.)
B_SPLINE_SURFACE_WITH_KNOTS((2,2),(3,2,2,3),(0.,0.289681084359925),(0.211398300093701,
0.214285714285714,0.22888337489481,0.229058225642821),.UNSPECIFIED.)
GEOMETRIC_REPRESENTATION_ITEM()
RATIONAL_B_SPLINE_SURFACE(((0.998054921708739,0.998986490969345,1.,0.994876086397763,
0.991846493044689,0.991846493044689,0.991846493044689),(0.998054921708739,
0.998986490969345,1.,0.994876086397763,0.991846493044689,0.991846493044689,
0.991846493044689)))
REPRESENTATION_ITEM('')
SURFACE()
);
#1766=(
BOUNDED_SURFACE()
B_SPLINE_SURFACE(1,2,((#123944,#123945,#123946,#123947,#123948),(#123949,
#123950,#123951,#123952,#123953)),.UNSPECIFIED.,.F.,.F.,.F.)
B_SPLINE_SURFACE_WITH_KNOTS((2,2),(3,2,3),(0.,0.289807040993898),(0.504546746573287,
0.504719756176205,0.52202071646804),.UNSPECIFIED.)
GEOMETRIC_REPRESENTATION_ITEM()
RATIONAL_B_SPLINE_SURFACE(((0.996905579294159,0.996905579294159,0.996905579294159,
0.991635321911186,0.989306890555885),(0.996905579294159,0.996905579294159,
0.996905579294159,0.991635321911186,0.989306890555885)))
REPRESENTATION_ITEM('')
SURFACE()
);
#1767=(
BOUNDED_SURFACE()
B_SPLINE_SURFACE(1,2,((#123955,#123956,#123957,#123958,#123959,#123960,
#123961),(#123962,#123963,#123964,#123965,#123966,#123967,#123968)),
 .UNSPECIFIED.,.F.,.F.,.F.)
B_SPLINE_SURFACE_WITH_KNOTS((2,2),(3,2,2,3),(0.,0.28968108435992),(0.211398300093701,
0.214285714285714,0.22888337489481,0.229058225642821),.UNSPECIFIED.)
GEOMETRIC_REPRESENTATION_ITEM()
RATIONAL_B_SPLINE_SURFACE(((0.998054921708739,0.998986490969345,1.,0.994876086397763,
0.991846493044689,0.991846493044689,0.991846493044689),(0.998054921708739,
0.998986490969345,1.,0.994876086397763,0.991846493044689,0.991846493044689,
0.991846493044689)))
REPRESENTATION_ITEM('')
SURFACE()
);
#1768=(
BOUNDED_SURFACE()
B_SPLINE_SURFACE(1,2,((#123990,#123991,#123992,#123993,#123994),(#123995,
#123996,#123997,#123998,#123999)),.UNSPECIFIED.,.F.,.F.,.F.)
B_SPLINE_SURFACE_WITH_KNOTS((2,2),(3,2,3),(0.,0.289807040994484),(0.504546746573287,
0.504719756176205,0.52202071646804),.UNSPECIFIED.)
GEOMETRIC_REPRESENTATION_ITEM()
RATIONAL_B_SPLINE_SURFACE(((0.996905579294159,0.996905579294159,0.996905579294159,
0.991635321911186,0.989306890555885),(0.996905579294159,0.996905579294159,
0.996905579294159,0.991635321911186,0.989306890555885)))
REPRESENTATION_ITEM('')
SURFACE()
);
#1769=(
BOUNDED_SURFACE()
B_SPLINE_SURFACE(1,2,((#124001,#124002,#124003,#124004,#124005,#124006,
#124007),(#124008,#124009,#124010,#124011,#124012,#124013,#124014)),
 .UNSPECIFIED.,.F.,.F.,.F.)
B_SPLINE_SURFACE_WITH_KNOTS((2,2),(3,2,2,3),(0.,0.289681084359918),(0.211398300093701,
0.214285714285714,0.22888337489481,0.229058225642821),.UNSPECIFIED.)
GEOMETRIC_REPRESENTATION_ITEM()
RATIONAL_B_SPLINE_SURFACE(((0.998054921708739,0.998986490969345,1.,0.994876086397763,
0.991846493044689,0.991846493044689,0.991846493044689),(0.998054921708739,
0.998986490969345,1.,0.994876086397763,0.991846493044689,0.991846493044689,
0.991846493044689)))
REPRESENTATION_ITEM('')
SURFACE()
);
#1770=(
BOUNDED_SURFACE()
B_SPLINE_SURFACE(1,2,((#124036,#124037,#124038,#124039,#124040),(#124041,
#124042,#124043,#124044,#124045)),.UNSPECIFIED.,.F.,.F.,.F.)
B_SPLINE_SURFACE_WITH_KNOTS((2,2),(3,2,3),(0.,0.289807040993898),(0.504546746573287,
0.504719756176205,0.52202071646804),.UNSPECIFIED.)
GEOMETRIC_REPRESENTATION_ITEM()
RATIONAL_B_SPLINE_SURFACE(((0.996905579294159,0.996905579294159,0.996905579294159,
0.991635321911186,0.989306890555885),(0.996905579294159,0.996905579294159,
0.996905579294159,0.991635321911186,0.989306890555885)))
REPRESENTATION_ITEM('')
SURFACE()
);
#1771=(
BOUNDED_SURFACE()
B_SPLINE_SURFACE(1,2,((#124047,#124048,#124049,#124050,#124051,#124052,
#124053),(#124054,#124055,#124056,#124057,#124058,#124059,#124060)),
 .UNSPECIFIED.,.F.,.F.,.F.)
B_SPLINE_SURFACE_WITH_KNOTS((2,2),(3,2,2,3),(0.,0.289681084359926),(0.211398300093701,
0.214285714285714,0.22888337489481,0.229058225642821),.UNSPECIFIED.)
GEOMETRIC_REPRESENTATION_ITEM()
RATIONAL_B_SPLINE_SURFACE(((0.998054921708739,0.998986490969345,1.,0.994876086397763,
0.991846493044689,0.991846493044689,0.991846493044689),(0.998054921708739,
0.998986490969345,1.,0.994876086397763,0.991846493044689,0.991846493044689,
0.991846493044689)))
REPRESENTATION_ITEM('')
SURFACE()
);
#1772=(
BOUNDED_SURFACE()
B_SPLINE_SURFACE(1,2,((#124077,#124078,#124079,#124080,#124081),(#124082,
#124083,#124084,#124085,#124086)),.UNSPECIFIED.,.F.,.F.,.F.)
B_SPLINE_SURFACE_WITH_KNOTS((2,2),(3,2,3),(0.,0.289807040994487),(0.504546746573287,
0.504719756176205,0.52202071646804),.UNSPECIFIED.)
GEOMETRIC_REPRESENTATION_ITEM()
RATIONAL_B_SPLINE_SURFACE(((0.996905579294159,0.996905579294159,0.996905579294159,
0.991635321911186,0.989306890555885),(0.996905579294159,0.996905579294159,
0.996905579294159,0.991635321911186,0.989306890555885)))
REPRESENTATION_ITEM('')
SURFACE()
);
#1773=(
BOUNDED_SURFACE()
B_SPLINE_SURFACE(1,2,((#124088,#124089,#124090,#124091,#124092,#124093,
#124094),(#124095,#124096,#124097,#124098,#124099,#124100,#124101)),
 .UNSPECIFIED.,.F.,.F.,.F.)
B_SPLINE_SURFACE_WITH_KNOTS((2,2),(3,2,2,3),(0.,0.289681084359916),(0.211398300093701,
0.214285714285714,0.22888337489481,0.229058225642821),.UNSPECIFIED.)
GEOMETRIC_REPRESENTATION_ITEM()
RATIONAL_B_SPLINE_SURFACE(((0.998054921708739,0.998986490969345,1.,0.994876086397763,
0.991846493044689,0.991846493044689,0.991846493044689),(0.998054921708739,
0.998986490969345,1.,0.994876086397763,0.991846493044689,0.991846493044689,
0.991846493044689)))
REPRESENTATION_ITEM('')
SURFACE()
);
#1774=(
BOUNDED_SURFACE()
B_SPLINE_SURFACE(1,2,((#124118,#124119,#124120,#124121,#124122),(#124123,
#124124,#124125,#124126,#124127)),.UNSPECIFIED.,.F.,.F.,.F.)
B_SPLINE_SURFACE_WITH_KNOTS((2,2),(3,2,3),(0.,0.289807040993979),(0.504546746573288,
0.504719756176206,0.52202071646804),.UNSPECIFIED.)
GEOMETRIC_REPRESENTATION_ITEM()
RATIONAL_B_SPLINE_SURFACE(((0.996905579294159,0.996905579294159,0.996905579294159,
0.991635321911186,0.989306890555885),(0.996905579294159,0.996905579294159,
0.996905579294159,0.991635321911186,0.989306890555885)))
REPRESENTATION_ITEM('')
SURFACE()
);
#1775=(
BOUNDED_SURFACE()
B_SPLINE_SURFACE(1,2,((#124129,#124130,#124131,#124132,#124133,#124134,
#124135),(#124136,#124137,#124138,#124139,#124140,#124141,#124142)),
 .UNSPECIFIED.,.F.,.F.,.F.)
B_SPLINE_SURFACE_WITH_KNOTS((2,2),(3,2,2,3),(0.,0.289681084359922),(0.2113983000937,
0.214285714285714,0.228883374894809,0.22905822564282),.UNSPECIFIED.)
GEOMETRIC_REPRESENTATION_ITEM()
RATIONAL_B_SPLINE_SURFACE(((0.998054921708738,0.998986490969345,1.,0.994876086397764,
0.991846493044689,0.991846493044689,0.991846493044689),(0.998054921708738,
0.998986490969345,1.,0.994876086397764,0.991846493044689,0.991846493044689,
0.991846493044689)))
REPRESENTATION_ITEM('')
SURFACE()
);
#1776=(
BOUNDED_SURFACE()
B_SPLINE_SURFACE(1,2,((#124159,#124160,#124161,#124162,#124163),(#124164,
#124165,#124166,#124167,#124168)),.UNSPECIFIED.,.F.,.F.,.F.)
B_SPLINE_SURFACE_WITH_KNOTS((2,2),(3,2,3),(0.,0.289807040993979),(0.504546746573288,
0.504719756176206,0.522020716468041),.UNSPECIFIED.)
GEOMETRIC_REPRESENTATION_ITEM()
RATIONAL_B_SPLINE_SURFACE(((0.996905579294159,0.996905579294159,0.996905579294159,
0.991635321911186,0.989306890555884),(0.996905579294159,0.996905579294159,
0.996905579294159,0.991635321911186,0.989306890555884)))
REPRESENTATION_ITEM('')
SURFACE()
);
#1777=(
BOUNDED_SURFACE()
B_SPLINE_SURFACE(1,2,((#124170,#124171,#124172,#124173,#124174,#124175,
#124176),(#124177,#124178,#124179,#124180,#124181,#124182,#124183)),
 .UNSPECIFIED.,.F.,.F.,.F.)
B_SPLINE_SURFACE_WITH_KNOTS((2,2),(3,2,2,3),(0.,0.289681084359917),(0.2113983000937,
0.214285714285714,0.228883374894809,0.22905822564282),.UNSPECIFIED.)
GEOMETRIC_REPRESENTATION_ITEM()
RATIONAL_B_SPLINE_SURFACE(((0.998054921708738,0.998986490969345,1.,0.994876086397764,
0.991846493044689,0.991846493044689,0.991846493044689),(0.998054921708738,
0.998986490969345,1.,0.994876086397764,0.991846493044689,0.991846493044689,
0.991846493044689)))
REPRESENTATION_ITEM('')
SURFACE()
);
#1778=(
BOUNDED_SURFACE()
B_SPLINE_SURFACE(1,2,((#124200,#124201,#124202,#124203,#124204),(#124205,
#124206,#124207,#124208,#124209)),.UNSPECIFIED.,.F.,.F.,.F.)
B_SPLINE_SURFACE_WITH_KNOTS((2,2),(3,2,3),(0.,0.289807040994574),(0.504546746573288,
0.504719756176206,0.522020716468041),.UNSPECIFIED.)
GEOMETRIC_REPRESENTATION_ITEM()
RATIONAL_B_SPLINE_SURFACE(((0.996905579294158,0.996905579294158,0.996905579294158,
0.991635321911186,0.989306890555884),(0.996905579294158,0.996905579294158,
0.996905579294158,0.991635321911185,0.989306890555884)))
REPRESENTATION_ITEM('')
SURFACE()
);
#1779=(
BOUNDED_SURFACE()
B_SPLINE_SURFACE(1,2,((#124211,#124212,#124213,#124214,#124215,#124216,
#124217),(#124218,#124219,#124220,#124221,#124222,#124223,#124224)),
 .UNSPECIFIED.,.F.,.F.,.F.)
B_SPLINE_SURFACE_WITH_KNOTS((2,2),(3,2,2,3),(0.,0.289681084359919),(0.2113983000937,
0.214285714285714,0.228883374894809,0.22905822564282),.UNSPECIFIED.)
GEOMETRIC_REPRESENTATION_ITEM()
RATIONAL_B_SPLINE_SURFACE(((0.998054921708738,0.998986490969345,1.,0.994876086397764,
0.991846493044689,0.991846493044689,0.991846493044689),(0.998054921708738,
0.998986490969345,1.,0.994876086397764,0.991846493044689,0.991846493044689,
0.991846493044689)))
REPRESENTATION_ITEM('')
SURFACE()
);
#1780=(
BOUNDED_SURFACE()
B_SPLINE_SURFACE(1,2,((#124246,#124247,#124248,#124249,#124250),(#124251,
#124252,#124253,#124254,#124255)),.UNSPECIFIED.,.F.,.F.,.F.)
B_SPLINE_SURFACE_WITH_KNOTS((2,2),(3,2,3),(0.,0.289807040993985),(0.504546746573288,
0.504719756176206,0.522020716468041),.UNSPECIFIED.)
GEOMETRIC_REPRESENTATION_ITEM()
RATIONAL_B_SPLINE_SURFACE(((0.996905579294158,0.996905579294158,0.996905579294158,
0.991635321911186,0.989306890555884),(0.996905579294158,0.996905579294158,
0.996905579294158,0.991635321911186,0.989306890555884)))
REPRESENTATION_ITEM('')
SURFACE()
);
#1781=(
BOUNDED_SURFACE()
B_SPLINE_SURFACE(1,2,((#124257,#124258,#124259,#124260,#124261,#124262,
#124263),(#124264,#124265,#124266,#124267,#124268,#124269,#124270)),
 .UNSPECIFIED.,.F.,.F.,.F.)
B_SPLINE_SURFACE_WITH_KNOTS((2,2),(3,2,2,3),(0.,0.289681084359918),(0.2113983000937,
0.214285714285714,0.228883374894809,0.22905822564282),.UNSPECIFIED.)
GEOMETRIC_REPRESENTATION_ITEM()
RATIONAL_B_SPLINE_SURFACE(((0.998054921708738,0.998986490969345,1.,0.994876086397764,
0.991846493044689,0.991846493044689,0.991846493044689),(0.998054921708738,
0.998986490969345,1.,0.994876086397764,0.991846493044689,0.991846493044689,
0.991846493044689)))
REPRESENTATION_ITEM('')
SURFACE()
);
#1782=(
BOUNDED_SURFACE()
B_SPLINE_SURFACE(1,2,((#124287,#124288,#124289,#124290,#124291),(#124292,
#124293,#124294,#124295,#124296)),.UNSPECIFIED.,.F.,.F.,.F.)
B_SPLINE_SURFACE_WITH_KNOTS((2,2),(3,2,3),(0.,0.289807040994485),(0.504546746573288,
0.504719756176206,0.522020716468041),.UNSPECIFIED.)
GEOMETRIC_REPRESENTATION_ITEM()
RATIONAL_B_SPLINE_SURFACE(((0.996905579294158,0.996905579294158,0.996905579294158,
0.991635321911186,0.989306890555884),(0.996905579294158,0.996905579294158,
0.996905579294158,0.991635321911185,0.989306890555884)))
REPRESENTATION_ITEM('')
SURFACE()
);
#1783=(
BOUNDED_SURFACE()
B_SPLINE_SURFACE(1,2,((#124298,#124299,#124300,#124301,#124302,#124303,
#124304),(#124305,#124306,#124307,#124308,#124309,#124310,#124311)),
 .UNSPECIFIED.,.F.,.F.,.F.)
B_SPLINE_SURFACE_WITH_KNOTS((2,2),(3,2,2,3),(0.,0.289681084359917),(0.2113983000937,
0.214285714285714,0.228883374894809,0.22905822564282),.UNSPECIFIED.)
GEOMETRIC_REPRESENTATION_ITEM()
RATIONAL_B_SPLINE_SURFACE(((0.998054921708738,0.998986490969345,1.,0.994876086397764,
0.991846493044689,0.991846493044689,0.991846493044689),(0.998054921708738,
0.998986490969345,1.,0.994876086397764,0.991846493044689,0.991846493044689,
0.991846493044689)))
REPRESENTATION_ITEM('')
SURFACE()
);
#1784=(
BOUNDED_SURFACE()
B_SPLINE_SURFACE(1,2,((#124328,#124329,#124330,#124331,#124332),(#124333,
#124334,#124335,#124336,#124337)),.UNSPECIFIED.,.F.,.F.,.F.)
B_SPLINE_SURFACE_WITH_KNOTS((2,2),(3,2,3),(0.,0.289807040993984),(0.504546746573288,
0.504719756176206,0.522020716468041),.UNSPECIFIED.)
GEOMETRIC_REPRESENTATION_ITEM()
RATIONAL_B_SPLINE_SURFACE(((0.996905579294158,0.996905579294158,0.996905579294158,
0.991635321911185,0.989306890555884),(0.996905579294158,0.996905579294158,
0.996905579294158,0.991635321911186,0.989306890555884)))
REPRESENTATION_ITEM('')
SURFACE()
);
#1785=(
BOUNDED_SURFACE()
B_SPLINE_SURFACE(1,2,((#124339,#124340,#124341,#124342,#124343,#124344,
#124345),(#124346,#124347,#124348,#124349,#124350,#124351,#124352)),
 .UNSPECIFIED.,.F.,.F.,.F.)
B_SPLINE_SURFACE_WITH_KNOTS((2,2),(3,2,2,3),(0.,0.28968108435992),(0.2113983000937,
0.214285714285714,0.228883374894809,0.22905822564282),.UNSPECIFIED.)
GEOMETRIC_REPRESENTATION_ITEM()
RATIONAL_B_SPLINE_SURFACE(((0.998054921708738,0.998986490969345,1.,0.994876086397764,
0.991846493044689,0.991846493044689,0.991846493044689),(0.998054921708738,
0.998986490969345,1.,0.994876086397764,0.991846493044689,0.991846493044689,
0.991846493044689)))
REPRESENTATION_ITEM('')
SURFACE()
);
#1786=(
BOUNDED_SURFACE()
B_SPLINE_SURFACE(1,2,((#124369,#124370,#124371,#124372,#124373),(#124374,
#124375,#124376,#124377,#124378)),.UNSPECIFIED.,.F.,.F.,.F.)
B_SPLINE_SURFACE_WITH_KNOTS((2,2),(3,2,3),(0.,0.28980704099449),(0.504546746573288,
0.504719756176206,0.522020716468041),.UNSPECIFIED.)
GEOMETRIC_REPRESENTATION_ITEM()
RATIONAL_B_SPLINE_SURFACE(((0.996905579294158,0.996905579294158,0.996905579294158,
0.991635321911186,0.989306890555884),(0.996905579294158,0.996905579294158,
0.996905579294158,0.991635321911185,0.989306890555884)))
REPRESENTATION_ITEM('')
SURFACE()
);
#1787=(
BOUNDED_SURFACE()
B_SPLINE_SURFACE(1,2,((#124380,#124381,#124382,#124383,#124384,#124385,
#124386),(#124387,#124388,#124389,#124390,#124391,#124392,#124393)),
 .UNSPECIFIED.,.F.,.F.,.F.)
B_SPLINE_SURFACE_WITH_KNOTS((2,2),(3,2,2,3),(0.,0.289681084359921),(0.2113983000937,
0.214285714285714,0.228883374894809,0.22905822564282),.UNSPECIFIED.)
GEOMETRIC_REPRESENTATION_ITEM()
RATIONAL_B_SPLINE_SURFACE(((0.998054921708738,0.998986490969345,1.,0.994876086397764,
0.991846493044689,0.991846493044689,0.991846493044689),(0.998054921708738,
0.998986490969345,1.,0.994876086397764,0.991846493044689,0.991846493044689,
0.991846493044689)))
REPRESENTATION_ITEM('')
SURFACE()
);
#1788=(
BOUNDED_SURFACE()
B_SPLINE_SURFACE(1,2,((#124419,#124420,#124421,#124422,#124423),(#124424,
#124425,#124426,#124427,#124428)),.UNSPECIFIED.,.F.,.F.,.F.)
B_SPLINE_SURFACE_WITH_KNOTS((2,2),(3,2,3),(0.,0.289807040994261),(0.504546746573288,
0.504719756176206,0.522020716468041),.UNSPECIFIED.)
GEOMETRIC_REPRESENTATION_ITEM()
RATIONAL_B_SPLINE_SURFACE(((0.996905579294158,0.996905579294158,0.996905579294158,
0.991635321911186,0.989306890555884),(0.996905579294159,0.996905579294159,
0.996905579294159,0.991635321911186,0.989306890555884)))
REPRESENTATION_ITEM('')
SURFACE()
);
#1789=(
BOUNDED_SURFACE()
B_SPLINE_SURFACE(1,2,((#124430,#124431,#124432,#124433,#124434,#124435,
#124436),(#124437,#124438,#124439,#124440,#124441,#124442,#124443)),
 .UNSPECIFIED.,.F.,.F.,.F.)
B_SPLINE_SURFACE_WITH_KNOTS((2,2),(3,2,2,3),(0.,0.28968108435992),(0.2113983000937,
0.214285714285714,0.228883374894809,0.22905822564282),.UNSPECIFIED.)
GEOMETRIC_REPRESENTATION_ITEM()
RATIONAL_B_SPLINE_SURFACE(((0.998054921708738,0.998986490969345,1.,0.994876086397764,
0.991846493044689,0.991846493044689,0.991846493044689),(0.998054921708738,
0.998986490969345,1.,0.994876086397764,0.991846493044689,0.991846493044689,
0.991846493044689)))
REPRESENTATION_ITEM('')
SURFACE()
);
#1790=(
BOUNDED_SURFACE()
B_SPLINE_SURFACE(1,2,((#124469,#124470,#124471,#124472,#124473),(#124474,
#124475,#124476,#124477,#124478)),.UNSPECIFIED.,.F.,.F.,.F.)
B_SPLINE_SURFACE_WITH_KNOTS((2,2),(3,2,3),(0.,0.289807040995303),(0.504546746573288,
0.504719756176206,0.522020716468041),.UNSPECIFIED.)
GEOMETRIC_REPRESENTATION_ITEM()
RATIONAL_B_SPLINE_SURFACE(((0.996905579294158,0.996905579294158,0.996905579294158,
0.991635321911185,0.989306890555884),(0.996905579294158,0.996905579294158,
0.996905579294158,0.991635321911186,0.989306890555884)))
REPRESENTATION_ITEM('')
SURFACE()
);
#1791=(
BOUNDED_SURFACE()
B_SPLINE_SURFACE(1,2,((#124480,#124481,#124482,#124483,#124484,#124485,
#124486),(#124487,#124488,#124489,#124490,#124491,#124492,#124493)),
 .UNSPECIFIED.,.F.,.F.,.F.)
B_SPLINE_SURFACE_WITH_KNOTS((2,2),(3,2,2,3),(0.,0.289681084359921),(0.2113983000937,
0.214285714285714,0.228883374894811,0.229058225642822),.UNSPECIFIED.)
GEOMETRIC_REPRESENTATION_ITEM()
RATIONAL_B_SPLINE_SURFACE(((0.998054921708738,0.998986490969345,1.,0.994876086397763,
0.991846493044688,0.991846493044688,0.991846493044688),(0.998054921708738,
0.998986490969345,1.,0.994876086397763,0.991846493044688,0.991846493044688,
0.991846493044688)))
REPRESENTATION_ITEM('')
SURFACE()
);
#1792=(
BOUNDED_SURFACE()
B_SPLINE_SURFACE(1,2,((#124519,#124520,#124521,#124522,#124523),(#124524,
#124525,#124526,#124527,#124528)),.UNSPECIFIED.,.F.,.F.,.F.)
B_SPLINE_SURFACE_WITH_KNOTS((2,2),(3,2,3),(0.,0.28980704099402),(0.504546746573288,
0.504719756176206,0.522020716468041),.UNSPECIFIED.)
GEOMETRIC_REPRESENTATION_ITEM()
RATIONAL_B_SPLINE_SURFACE(((0.996905579294158,0.996905579294158,0.996905579294158,
0.991635321911185,0.989306890555884),(0.996905579294158,0.996905579294158,
0.996905579294158,0.991635321911185,0.989306890555884)))
REPRESENTATION_ITEM('')
SURFACE()
);
#1793=(
BOUNDED_SURFACE()
B_SPLINE_SURFACE(1,2,((#124530,#124531,#124532,#124533,#124534,#124535,
#124536),(#124537,#124538,#124539,#124540,#124541,#124542,#124543)),
 .UNSPECIFIED.,.F.,.F.,.F.)
B_SPLINE_SURFACE_WITH_KNOTS((2,2),(3,2,2,3),(0.,0.289681084359926),(0.211398300093698,
0.214285714285714,0.228883374894809,0.22905822564282),.UNSPECIFIED.)
GEOMETRIC_REPRESENTATION_ITEM()
RATIONAL_B_SPLINE_SURFACE(((0.998054921708736,0.998986490969344,1.,0.994876086397764,
0.991846493044689,0.991846493044689,0.991846493044689),(0.998054921708736,
0.998986490969344,1.,0.994876086397764,0.991846493044689,0.991846493044689,
0.991846493044689)))
REPRESENTATION_ITEM('')
SURFACE()
);
#1794=(
BOUNDED_SURFACE()
B_SPLINE_SURFACE(1,2,((#124560,#124561,#124562,#124563,#124564),(#124565,
#124566,#124567,#124568,#124569)),.UNSPECIFIED.,.F.,.F.,.F.)
B_SPLINE_SURFACE_WITH_KNOTS((2,2),(3,2,3),(0.,0.28980704099391),(0.504546746573288,
0.504719756176206,0.522020716468041),.UNSPECIFIED.)
GEOMETRIC_REPRESENTATION_ITEM()
RATIONAL_B_SPLINE_SURFACE(((0.996905579294158,0.996905579294158,0.996905579294158,
0.991635321911186,0.989306890555884),(0.996905579294158,0.996905579294158,
0.996905579294158,0.991635321911186,0.989306890555884)))
REPRESENTATION_ITEM('')
SURFACE()
);
#1795=(
BOUNDED_SURFACE()
B_SPLINE_SURFACE(1,2,((#124571,#124572,#124573,#124574,#124575,#124576,
#124577),(#124578,#124579,#124580,#124581,#124582,#124583,#124584)),
 .UNSPECIFIED.,.F.,.F.,.F.)
B_SPLINE_SURFACE_WITH_KNOTS((2,2),(3,2,2,3),(0.,0.289681084360126),(0.2113983000937,
0.214285714285714,0.228883374894809,0.22905822564282),.UNSPECIFIED.)
GEOMETRIC_REPRESENTATION_ITEM()
RATIONAL_B_SPLINE_SURFACE(((0.998054921708738,0.998986490969345,1.,0.994876086397764,
0.991846493044689,0.991846493044689,0.991846493044689),(0.998054921708738,
0.998986490969345,1.,0.994876086397764,0.991846493044689,0.991846493044689,
0.991846493044689)))
REPRESENTATION_ITEM('')
SURFACE()
);
#1796=(
BOUNDED_SURFACE()
B_SPLINE_SURFACE(1,2,((#124601,#124602,#124603,#124604,#124605),(#124606,
#124607,#124608,#124609,#124610)),.UNSPECIFIED.,.F.,.F.,.F.)
B_SPLINE_SURFACE_WITH_KNOTS((2,2),(3,2,3),(0.,0.289807040994542),(0.504546746573034,
0.504719756175955,0.522020716468043),.UNSPECIFIED.)
GEOMETRIC_REPRESENTATION_ITEM()
RATIONAL_B_SPLINE_SURFACE(((0.996905579294312,0.996905579294312,0.996905579294312,
0.991635321911219,0.989306890555884),(0.996905579294312,0.996905579294312,
0.996905579294312,0.991635321911219,0.989306890555884)))
REPRESENTATION_ITEM('')
SURFACE()
);
#1797=(
BOUNDED_SURFACE()
B_SPLINE_SURFACE(1,2,((#124612,#124613,#124614,#124615,#124616,#124617,
#124618),(#124619,#124620,#124621,#124622,#124623,#124624,#124625)),
 .UNSPECIFIED.,.F.,.F.,.F.)
B_SPLINE_SURFACE_WITH_KNOTS((2,2),(3,2,2,3),(0.,0.289681084359927),(0.2113983000937,
0.214285714285714,0.228883374894809,0.22905822564282),.UNSPECIFIED.)
GEOMETRIC_REPRESENTATION_ITEM()
RATIONAL_B_SPLINE_SURFACE(((0.998054921708738,0.998986490969345,1.,0.994876086397764,
0.991846493044689,0.991846493044689,0.991846493044689),(0.998054921708738,
0.998986490969345,1.,0.994876086397764,0.991846493044689,0.991846493044689,
0.991846493044689)))
REPRESENTATION_ITEM('')
SURFACE()
);
#1798=(
BOUNDED_SURFACE()
B_SPLINE_SURFACE(1,2,((#124647,#124648,#124649,#124650,#124651),(#124652,
#124653,#124654,#124655,#124656)),.UNSPECIFIED.,.F.,.F.,.F.)
B_SPLINE_SURFACE_WITH_KNOTS((2,2),(3,2,3),(0.,0.289807040993132),(0.504546746573153,
0.504719756176073,0.522020716468042),.UNSPECIFIED.)
GEOMETRIC_REPRESENTATION_ITEM()
RATIONAL_B_SPLINE_SURFACE(((0.99690557929424,0.99690557929424,0.99690557929424,
0.991635321911203,0.989306890555884),(0.99690557929424,0.99690557929424,
0.99690557929424,0.991635321911203,0.989306890555884)))
REPRESENTATION_ITEM('')
SURFACE()
);
#1799=(
BOUNDED_SURFACE()
B_SPLINE_SURFACE(1,2,((#124658,#124659,#124660,#124661,#124662,#124663,
#124664),(#124665,#124666,#124667,#124668,#124669,#124670,#124671)),
 .UNSPECIFIED.,.F.,.F.,.F.)
B_SPLINE_SURFACE_WITH_KNOTS((2,2),(3,2,2,3),(0.,0.289681084360278),(0.211398300093698,
0.214285714285714,0.228883374894809,0.22905822564282),.UNSPECIFIED.)
GEOMETRIC_REPRESENTATION_ITEM()
RATIONAL_B_SPLINE_SURFACE(((0.998054921708737,0.998986490969345,1.,0.994876086397764,
0.991846493044689,0.991846493044689,0.991846493044689),(0.998054921708737,
0.998986490969345,1.,0.994876086397764,0.991846493044689,0.991846493044689,
0.991846493044689)))
REPRESENTATION_ITEM('')
SURFACE()
);
#1800=(
BOUNDED_SURFACE()
B_SPLINE_SURFACE(1,2,((#124688,#124689,#124690,#124691,#124692),(#124693,
#124694,#124695,#124696,#124697)),.UNSPECIFIED.,.F.,.F.,.F.)
B_SPLINE_SURFACE_WITH_KNOTS((2,2),(3,2,3),(0.,0.289807040994288),(0.504546746573288,
0.504719756176206,0.522020716468042),.UNSPECIFIED.)
GEOMETRIC_REPRESENTATION_ITEM()
RATIONAL_B_SPLINE_SURFACE(((0.996905579294158,0.996905579294158,0.996905579294158,
0.991635321911185,0.989306890555884),(0.996905579294158,0.996905579294158,
0.996905579294158,0.991635321911185,0.989306890555884)))
REPRESENTATION_ITEM('')
SURFACE()
);
#1801=(
BOUNDED_SURFACE()
B_SPLINE_SURFACE(1,2,((#124699,#124700,#124701,#124702,#124703,#124704,
#124705),(#124706,#124707,#124708,#124709,#124710,#124711,#124712)),
 .UNSPECIFIED.,.F.,.F.,.F.)
B_SPLINE_SURFACE_WITH_KNOTS((2,2),(3,2,2,3),(0.,0.289681084361153),(0.211398300093696,
0.214285714285714,0.228883374894809,0.22905822564282),.UNSPECIFIED.)
GEOMETRIC_REPRESENTATION_ITEM()
RATIONAL_B_SPLINE_SURFACE(((0.998054921708735,0.998986490969344,1.,0.994876086397764,
0.991846493044689,0.991846493044689,0.991846493044689),(0.998054921708735,
0.998986490969344,1.,0.994876086397764,0.991846493044689,0.991846493044689,
0.991846493044689)))
REPRESENTATION_ITEM('')
SURFACE()
);
#1802=(
BOUNDED_SURFACE()
B_SPLINE_SURFACE(1,2,((#124729,#124730,#124731,#124732,#124733),(#124734,
#124735,#124736,#124737,#124738)),.UNSPECIFIED.,.F.,.F.,.F.)
B_SPLINE_SURFACE_WITH_KNOTS((2,2),(3,2,3),(0.,0.289807040994107),(0.504546746573004,
0.504719756175925,0.522020716468042),.UNSPECIFIED.)
GEOMETRIC_REPRESENTATION_ITEM()
RATIONAL_B_SPLINE_SURFACE(((0.99690557929433,0.99690557929433,0.99690557929433,
0.991635321911223,0.989306890555884),(0.99690557929433,0.99690557929433,
0.99690557929433,0.991635321911223,0.989306890555884)))
REPRESENTATION_ITEM('')
SURFACE()
);
#1803=(
BOUNDED_SURFACE()
B_SPLINE_SURFACE(1,2,((#124740,#124741,#124742,#124743,#124744,#124745,
#124746),(#124747,#124748,#124749,#124750,#124751,#124752,#124753)),
 .UNSPECIFIED.,.F.,.F.,.F.)
B_SPLINE_SURFACE_WITH_KNOTS((2,2),(3,2,2,3),(0.,0.289681084359926),(0.2113983000937,
0.214285714285714,0.22888337489481,0.229058225642821),.UNSPECIFIED.)
GEOMETRIC_REPRESENTATION_ITEM()
RATIONAL_B_SPLINE_SURFACE(((0.998054921708738,0.998986490969345,1.,0.994876086397764,
0.991846493044689,0.991846493044689,0.991846493044689),(0.998054921708738,
0.998986490969345,1.,0.994876086397763,0.991846493044689,0.991846493044689,
0.991846493044689)))
REPRESENTATION_ITEM('')
SURFACE()
);
#1804=(
BOUNDED_SURFACE()
B_SPLINE_SURFACE(1,2,((#124775,#124776,#124777,#124778,#124779),(#124780,
#124781,#124782,#124783,#124784)),.UNSPECIFIED.,.F.,.F.,.F.)
B_SPLINE_SURFACE_WITH_KNOTS((2,2),(3,2,3),(0.,0.289807040994811),(0.504546746573147,
0.504719756176067,0.522020716468042),.UNSPECIFIED.)
GEOMETRIC_REPRESENTATION_ITEM()
RATIONAL_B_SPLINE_SURFACE(((0.996905579294243,0.996905579294243,0.996905579294243,
0.991635321911204,0.989306890555884),(0.996905579294243,0.996905579294243,
0.996905579294243,0.991635321911204,0.989306890555884)))
REPRESENTATION_ITEM('')
SURFACE()
);
#1805=(
BOUNDED_SURFACE()
B_SPLINE_SURFACE(1,2,((#124786,#124787,#124788,#124789,#124790,#124791,
#124792),(#124793,#124794,#124795,#124796,#124797,#124798,#124799)),
 .UNSPECIFIED.,.F.,.F.,.F.)
B_SPLINE_SURFACE_WITH_KNOTS((2,2),(3,2,2,3),(0.,0.28968108435992),(0.2113983000937,
0.214285714285714,0.228883374894809,0.22905822564282),.UNSPECIFIED.)
GEOMETRIC_REPRESENTATION_ITEM()
RATIONAL_B_SPLINE_SURFACE(((0.998054921708738,0.998986490969345,1.,0.994876086397764,
0.991846493044689,0.991846493044689,0.991846493044689),(0.998054921708738,
0.998986490969345,1.,0.994876086397764,0.991846493044689,0.991846493044689,
0.991846493044689)))
REPRESENTATION_ITEM('')
SURFACE()
);
#1806=(
BOUNDED_SURFACE()
B_SPLINE_SURFACE(1,2,((#124825,#124826,#124827,#124828,#124829),(#124830,
#124831,#124832,#124833,#124834)),.UNSPECIFIED.,.F.,.F.,.F.)
B_SPLINE_SURFACE_WITH_KNOTS((2,2),(3,2,3),(0.,0.289807040993315),(0.5045467465732,
0.504719756176119,0.522020716468042),.UNSPECIFIED.)
GEOMETRIC_REPRESENTATION_ITEM()
RATIONAL_B_SPLINE_SURFACE(((0.996905579294211,0.996905579294211,0.996905579294211,
0.991635321911197,0.989306890555884),(0.996905579294211,0.996905579294211,
0.996905579294211,0.991635321911197,0.989306890555884)))
REPRESENTATION_ITEM('')
SURFACE()
);
#1807=(
BOUNDED_SURFACE()
B_SPLINE_SURFACE(1,2,((#124836,#124837,#124838,#124839,#124840,#124841,
#124842),(#124843,#124844,#124845,#124846,#124847,#124848,#124849)),
 .UNSPECIFIED.,.F.,.F.,.F.)
B_SPLINE_SURFACE_WITH_KNOTS((2,2),(3,2,2,3),(0.,0.289681084359922),(0.211398300093699,
0.214285714285714,0.22888337489485,0.229058225642861),.UNSPECIFIED.)
GEOMETRIC_REPRESENTATION_ITEM()
RATIONAL_B_SPLINE_SURFACE(((0.998054921708738,0.998986490969345,1.,0.994876086397749,
0.991846493044672,0.991846493044672,0.991846493044672),(0.998054921708738,
0.998986490969345,1.,0.994876086397749,0.991846493044672,0.991846493044672,
0.991846493044672)))
REPRESENTATION_ITEM('')
SURFACE()
);
#1808=(
BOUNDED_SURFACE()
B_SPLINE_SURFACE(1,2,((#124866,#124867,#124868,#124869,#124870),(#124871,
#124872,#124873,#124874,#124875)),.UNSPECIFIED.,.F.,.F.,.F.)
B_SPLINE_SURFACE_WITH_KNOTS((2,2),(3,2,3),(0.,0.289807040994463),(0.504546746573278,
0.504719756176196,0.522020716468041),.UNSPECIFIED.)
GEOMETRIC_REPRESENTATION_ITEM()
RATIONAL_B_SPLINE_SURFACE(((0.996905579294165,0.996905579294165,0.996905579294165,
0.991635321911187,0.989306890555884),(0.996905579294165,0.996905579294165,
0.996905579294165,0.991635321911187,0.989306890555884)))
REPRESENTATION_ITEM('')
SURFACE()
);
#1809=(
BOUNDED_SURFACE()
B_SPLINE_SURFACE(1,2,((#124877,#124878,#124879,#124880,#124881,#124882,
#124883),(#124884,#124885,#124886,#124887,#124888,#124889,#124890)),
 .UNSPECIFIED.,.F.,.F.,.F.)
B_SPLINE_SURFACE_WITH_KNOTS((2,2),(3,2,2,3),(0.,0.289681084360176),(0.2113983000937,
0.214285714285714,0.228883374894816,0.229058225642827),.UNSPECIFIED.)
GEOMETRIC_REPRESENTATION_ITEM()
RATIONAL_B_SPLINE_SURFACE(((0.998054921708738,0.998986490969345,1.,0.994876086397761,
0.991846493044686,0.991846493044686,0.991846493044686),(0.998054921708738,
0.998986490969345,1.,0.994876086397761,0.991846493044686,0.991846493044686,
0.991846493044686)))
REPRESENTATION_ITEM('')
SURFACE()
);
#1810=(
BOUNDED_SURFACE()
B_SPLINE_SURFACE(1,2,((#124907,#124908,#124909,#124910,#124911),(#124912,
#124913,#124914,#124915,#124916)),.UNSPECIFIED.,.F.,.F.,.F.)
B_SPLINE_SURFACE_WITH_KNOTS((2,2),(3,2,3),(0.,0.289807040994211),(0.504546746573288,
0.504719756176206,0.522020716468041),.UNSPECIFIED.)
GEOMETRIC_REPRESENTATION_ITEM()
RATIONAL_B_SPLINE_SURFACE(((0.996905579294158,0.996905579294158,0.996905579294158,
0.991635321911186,0.989306890555885),(0.996905579294158,0.996905579294158,
0.996905579294158,0.991635321911186,0.989306890555884)))
REPRESENTATION_ITEM('')
SURFACE()
);
#1811=(
BOUNDED_SURFACE()
B_SPLINE_SURFACE(1,2,((#124918,#124919,#124920,#124921,#124922,#124923,
#124924),(#124925,#124926,#124927,#124928,#124929,#124930,#124931)),
 .UNSPECIFIED.,.F.,.F.,.F.)
B_SPLINE_SURFACE_WITH_KNOTS((2,2),(3,2,2,3),(0.,0.289681084359936),(0.2113983000937,
0.214285714285714,0.228883374894809,0.22905822564282),.UNSPECIFIED.)
GEOMETRIC_REPRESENTATION_ITEM()
RATIONAL_B_SPLINE_SURFACE(((0.998054921708738,0.998986490969345,1.,0.994876086397764,
0.991846493044689,0.991846493044689,0.991846493044689),(0.998054921708738,
0.998986490969345,1.,0.994876086397764,0.991846493044689,0.991846493044689,
0.991846493044689)))
REPRESENTATION_ITEM('')
SURFACE()
);
#1812=(
BOUNDED_SURFACE()
B_SPLINE_SURFACE(1,2,((#124948,#124949,#124950,#124951,#124952),(#124953,
#124954,#124955,#124956,#124957)),.UNSPECIFIED.,.F.,.F.,.F.)
B_SPLINE_SURFACE_WITH_KNOTS((2,2),(3,2,3),(0.,0.289807040993962),(0.504546746573288,
0.504719756176206,0.522020716468041),.UNSPECIFIED.)
GEOMETRIC_REPRESENTATION_ITEM()
RATIONAL_B_SPLINE_SURFACE(((0.996905579294158,0.996905579294158,0.996905579294158,
0.991635321911186,0.989306890555884),(0.996905579294158,0.996905579294158,
0.996905579294158,0.991635321911186,0.989306890555884)))
REPRESENTATION_ITEM('')
SURFACE()
);
#1813=(
BOUNDED_SURFACE()
B_SPLINE_SURFACE(1,2,((#124959,#124960,#124961,#124962,#124963,#124964,
#124965),(#124966,#124967,#124968,#124969,#124970,#124971,#124972)),
 .UNSPECIFIED.,.F.,.F.,.F.)
B_SPLINE_SURFACE_WITH_KNOTS((2,2),(3,2,2,3),(0.,0.289681084359929),(0.211398300093699,
0.214285714285714,0.228883374894879,0.229058225642891),.UNSPECIFIED.)
GEOMETRIC_REPRESENTATION_ITEM()
RATIONAL_B_SPLINE_SURFACE(((0.998054921708738,0.998986490969345,1.,0.994876086397739,
0.99184649304466,0.99184649304466,0.99184649304466),(0.998054921708738,
0.998986490969345,1.,0.994876086397739,0.99184649304466,0.99184649304466,
0.99184649304466)))
REPRESENTATION_ITEM('')
SURFACE()
);
#1814=(
BOUNDED_SURFACE()
B_SPLINE_SURFACE(1,2,((#124994,#124995,#124996,#124997,#124998),(#124999,
#125000,#125001,#125002,#125003)),.UNSPECIFIED.,.F.,.F.,.F.)
B_SPLINE_SURFACE_WITH_KNOTS((2,2),(3,2,3),(0.,0.289807040993889),(0.504546746573288,
0.504719756176206,0.522020716468041),.UNSPECIFIED.)
GEOMETRIC_REPRESENTATION_ITEM()
RATIONAL_B_SPLINE_SURFACE(((0.996905579294158,0.996905579294158,0.996905579294158,
0.991635321911186,0.989306890555884),(0.996905579294158,0.996905579294158,
0.996905579294158,0.991635321911186,0.989306890555884)))
REPRESENTATION_ITEM('')
SURFACE()
);
#1815=(
BOUNDED_SURFACE()
B_SPLINE_SURFACE(1,2,((#125005,#125006,#125007,#125008,#125009,#125010,
#125011),(#125012,#125013,#125014,#125015,#125016,#125017,#125018)),
 .UNSPECIFIED.,.F.,.F.,.F.)
B_SPLINE_SURFACE_WITH_KNOTS((2,2),(3,2,2,3),(0.,0.289681084359923),(0.211398300093701,
0.214285714285714,0.228883374894809,0.22905822564282),.UNSPECIFIED.)
GEOMETRIC_REPRESENTATION_ITEM()
RATIONAL_B_SPLINE_SURFACE(((0.998054921708739,0.998986490969345,1.,0.994876086397764,
0.991846493044689,0.991846493044689,0.991846493044689),(0.998054921708739,
0.998986490969345,1.,0.994876086397764,0.991846493044689,0.991846493044689,
0.991846493044689)))
REPRESENTATION_ITEM('')
SURFACE()
);
#1816=(
BOUNDED_SURFACE()
B_SPLINE_SURFACE(1,2,((#125040,#125041,#125042,#125043,#125044),(#125045,
#125046,#125047,#125048,#125049)),.UNSPECIFIED.,.F.,.F.,.F.)
B_SPLINE_SURFACE_WITH_KNOTS((2,2),(3,2,3),(0.,0.28980704099297),(0.504546746573287,
0.504719756176205,0.52202071646804),.UNSPECIFIED.)
GEOMETRIC_REPRESENTATION_ITEM()
RATIONAL_B_SPLINE_SURFACE(((0.996905579294159,0.996905579294159,0.996905579294159,
0.991635321911186,0.989306890555885),(0.996905579294159,0.996905579294159,
0.996905579294159,0.991635321911186,0.989306890555885)))
REPRESENTATION_ITEM('')
SURFACE()
);
#1817=(
BOUNDED_SURFACE()
B_SPLINE_SURFACE(1,2,((#125051,#125052,#125053,#125054,#125055,#125056,
#125057),(#125058,#125059,#125060,#125061,#125062,#125063,#125064)),
 .UNSPECIFIED.,.F.,.F.,.F.)
B_SPLINE_SURFACE_WITH_KNOTS((2,2),(3,2,2,3),(0.,0.289681084359914),(0.211398300093701,
0.214285714285714,0.22888337489481,0.229058225642821),.UNSPECIFIED.)
GEOMETRIC_REPRESENTATION_ITEM()
RATIONAL_B_SPLINE_SURFACE(((0.998054921708739,0.998986490969346,1.,0.994876086397763,
0.991846493044689,0.991846493044689,0.991846493044689),(0.998054921708739,
0.998986490969346,1.,0.994876086397763,0.991846493044689,0.991846493044689,
0.991846493044689)))
REPRESENTATION_ITEM('')
SURFACE()
);
#1818=(
BOUNDED_SURFACE()
B_SPLINE_SURFACE(1,2,((#125079,#125080,#125081,#125082,#125083),(#125084,
#125085,#125086,#125087,#125088)),.UNSPECIFIED.,.F.,.F.,.F.)
B_SPLINE_SURFACE_WITH_KNOTS((2,2),(3,2,3),(0.,0.290406869879303),(0.262499170173511,
0.263098999273794,0.280537087669266),.UNSPECIFIED.)
GEOMETRIC_REPRESENTATION_ITEM()
RATIONAL_B_SPLINE_SURFACE(((0.989150325841652,0.989150325841652,0.989150325841652,
0.991395311444461,0.996628941948308),(0.989150325841652,0.989150325841652,
0.989150325841652,0.991395311444461,0.996628941948308)))
REPRESENTATION_ITEM('')
SURFACE()
);
#1819=(
BOUNDED_SURFACE()
B_SPLINE_SURFACE(1,2,((#125105,#125106,#125107),(#125108,#125109,#125110)),
 .UNSPECIFIED.,.F.,.F.,.F.)
B_SPLINE_SURFACE_WITH_KNOTS((2,2),(3,3),(0.,0.289681084359935),(0.452822299828566,
0.470019760166367),.UNSPECIFIED.)
GEOMETRIC_REPRESENTATION_ITEM()
RATIONAL_B_SPLINE_SURFACE(((0.98875548626282,0.986817927519786,0.987787102172814),
(0.98875548626282,0.986817927519786,0.987787102172814)))
REPRESENTATION_ITEM('')
SURFACE()
);
#1820=(
BOUNDED_SURFACE()
B_SPLINE_SURFACE(1,2,((#125112,#125113,#125114,#125115,#125116),(#125117,
#125118,#125119,#125120,#125121)),.UNSPECIFIED.,.F.,.F.,.F.)
B_SPLINE_SURFACE_WITH_KNOTS((2,2),(3,2,3),(0.,0.290406869885275),(0.262499170167527,
0.263098999273794,0.280537087669266),.UNSPECIFIED.)
GEOMETRIC_REPRESENTATION_ITEM()
RATIONAL_B_SPLINE_SURFACE(((0.989150325841652,0.989150325841652,0.989150325841652,
0.991395311444461,0.996628941948308),(0.989150325841652,0.989150325841652,
0.989150325841652,0.991395311444461,0.996628941948308)))
REPRESENTATION_ITEM('')
SURFACE()
);
#1821=(
BOUNDED_SURFACE()
B_SPLINE_SURFACE(1,2,((#125138,#125139,#125140),(#125141,#125142,#125143)),
 .UNSPECIFIED.,.F.,.F.,.F.)
B_SPLINE_SURFACE_WITH_KNOTS((2,2),(3,3),(0.,0.289681084359924),(0.452822299828566,
0.470019760166367),.UNSPECIFIED.)
GEOMETRIC_REPRESENTATION_ITEM()
RATIONAL_B_SPLINE_SURFACE(((0.98875548626282,0.986817927519786,0.987787102172814),
(0.98875548626282,0.986817927519786,0.987787102172814)))
REPRESENTATION_ITEM('')
SURFACE()
);
#1822=(
BOUNDED_SURFACE()
B_SPLINE_SURFACE(1,2,((#125145,#125146,#125147,#125148,#125149),(#125150,
#125151,#125152,#125153,#125154)),.UNSPECIFIED.,.F.,.F.,.F.)
B_SPLINE_SURFACE_WITH_KNOTS((2,2),(3,2,3),(0.,0.290406869890717),(0.262499170162089,
0.263098999273794,0.280537087669266),.UNSPECIFIED.)
GEOMETRIC_REPRESENTATION_ITEM()
RATIONAL_B_SPLINE_SURFACE(((0.989150325841652,0.989150325841652,0.989150325841652,
0.991395311444461,0.996628941948308),(0.989150325841652,0.989150325841652,
0.989150325841652,0.991395311444461,0.996628941948308)))
REPRESENTATION_ITEM('')
SURFACE()
);
#1823=(
BOUNDED_SURFACE()
B_SPLINE_SURFACE(1,2,((#125171,#125172,#125173),(#125174,#125175,#125176)),
 .UNSPECIFIED.,.F.,.F.,.F.)
B_SPLINE_SURFACE_WITH_KNOTS((2,2),(3,3),(0.,0.289681084359928),(0.452822299828566,
0.470019760166367),.UNSPECIFIED.)
GEOMETRIC_REPRESENTATION_ITEM()
RATIONAL_B_SPLINE_SURFACE(((0.98875548626282,0.986817927519786,0.987787102172814),
(0.98875548626282,0.986817927519786,0.987787102172814)))
REPRESENTATION_ITEM('')
SURFACE()
);
#1824=(
BOUNDED_SURFACE()
B_SPLINE_SURFACE(1,2,((#125178,#125179,#125180,#125181,#125182),(#125183,
#125184,#125185,#125186,#125187)),.UNSPECIFIED.,.F.,.F.,.F.)
B_SPLINE_SURFACE_WITH_KNOTS((2,2),(3,2,3),(0.,0.290406869901633),(0.262499170151171,
0.263098999273794,0.280537087669266),.UNSPECIFIED.)
GEOMETRIC_REPRESENTATION_ITEM()
RATIONAL_B_SPLINE_SURFACE(((0.989150325841652,0.989150325841652,0.989150325841652,
0.991395311444461,0.996628941948308),(0.989150325841652,0.989150325841652,
0.989150325841652,0.991395311444461,0.996628941948308)))
REPRESENTATION_ITEM('')
SURFACE()
);
#1825=(
BOUNDED_SURFACE()
B_SPLINE_SURFACE(1,2,((#125204,#125205,#125206),(#125207,#125208,#125209)),
 .UNSPECIFIED.,.F.,.F.,.F.)
B_SPLINE_SURFACE_WITH_KNOTS((2,2),(3,3),(0.,0.289681084359924),(0.452822299828566,
0.470019760166366),.UNSPECIFIED.)
GEOMETRIC_REPRESENTATION_ITEM()
RATIONAL_B_SPLINE_SURFACE(((0.98875548626282,0.986817927519786,0.987787102172814),
(0.98875548626282,0.986817927519786,0.987787102172814)))
REPRESENTATION_ITEM('')
SURFACE()
);
#1826=(
BOUNDED_SURFACE()
B_SPLINE_SURFACE(1,2,((#125211,#125212,#125213,#125214,#125215),(#125216,
#125217,#125218,#125219,#125220)),.UNSPECIFIED.,.F.,.F.,.F.)
B_SPLINE_SURFACE_WITH_KNOTS((2,2),(3,2,3),(0.,0.290406869898682),(0.262499170154123,
0.263098999273794,0.280537087669266),.UNSPECIFIED.)
GEOMETRIC_REPRESENTATION_ITEM()
RATIONAL_B_SPLINE_SURFACE(((0.989150325841652,0.989150325841652,0.989150325841652,
0.991395311444461,0.996628941948308),(0.989150325841652,0.989150325841652,
0.989150325841652,0.991395311444461,0.996628941948308)))
REPRESENTATION_ITEM('')
SURFACE()
);
#1827=(
BOUNDED_SURFACE()
B_SPLINE_SURFACE(1,2,((#125237,#125238,#125239),(#125240,#125241,#125242)),
 .UNSPECIFIED.,.F.,.F.,.F.)
B_SPLINE_SURFACE_WITH_KNOTS((2,2),(3,3),(0.,0.289681084359916),(0.452822299828566,
0.470019760166367),.UNSPECIFIED.)
GEOMETRIC_REPRESENTATION_ITEM()
RATIONAL_B_SPLINE_SURFACE(((0.98875548626282,0.986817927519786,0.987787102172814),
(0.98875548626282,0.986817927519786,0.987787102172814)))
REPRESENTATION_ITEM('')
SURFACE()
);
#1828=(
BOUNDED_SURFACE()
B_SPLINE_SURFACE(1,2,((#125244,#125245,#125246,#125247,#125248),(#125249,
#125250,#125251,#125252,#125253)),.UNSPECIFIED.,.F.,.F.,.F.)
B_SPLINE_SURFACE_WITH_KNOTS((2,2),(3,2,3),(0.,0.290406869896393),(0.262499170156412,
0.263098999273794,0.280537087669266),.UNSPECIFIED.)
GEOMETRIC_REPRESENTATION_ITEM()
RATIONAL_B_SPLINE_SURFACE(((0.989150325841652,0.989150325841652,0.989150325841652,
0.991395311444461,0.996628941948308),(0.989150325841652,0.989150325841652,
0.989150325841652,0.991395311444461,0.996628941948308)))
REPRESENTATION_ITEM('')
SURFACE()
);
#1829=(
BOUNDED_SURFACE()
B_SPLINE_SURFACE(1,2,((#125270,#125271,#125272),(#125273,#125274,#125275)),
 .UNSPECIFIED.,.F.,.F.,.F.)
B_SPLINE_SURFACE_WITH_KNOTS((2,2),(3,3),(0.,0.289681084359921),(0.452822299828566,
0.470019760166367),.UNSPECIFIED.)
GEOMETRIC_REPRESENTATION_ITEM()
RATIONAL_B_SPLINE_SURFACE(((0.98875548626282,0.986817927519786,0.987787102172814),
(0.98875548626282,0.986817927519786,0.987787102172814)))
REPRESENTATION_ITEM('')
SURFACE()
);
#1830=(
BOUNDED_SURFACE()
B_SPLINE_SURFACE(1,2,((#125277,#125278,#125279,#125280,#125281),(#125282,
#125283,#125284,#125285,#125286)),.UNSPECIFIED.,.F.,.F.,.F.)
B_SPLINE_SURFACE_WITH_KNOTS((2,2),(3,2,3),(0.,0.290406869895255),(0.262499170157545,
0.263098999273794,0.280537087669266),.UNSPECIFIED.)
GEOMETRIC_REPRESENTATION_ITEM()
RATIONAL_B_SPLINE_SURFACE(((0.989150325841652,0.989150325841652,0.989150325841652,
0.991395311444461,0.996628941948308),(0.989150325841652,0.989150325841652,
0.989150325841652,0.991395311444461,0.996628941948308)))
REPRESENTATION_ITEM('')
SURFACE()
);
#1831=(
BOUNDED_SURFACE()
B_SPLINE_SURFACE(1,2,((#125303,#125304,#125305),(#125306,#125307,#125308)),
 .UNSPECIFIED.,.F.,.F.,.F.)
B_SPLINE_SURFACE_WITH_KNOTS((2,2),(3,3),(0.,0.289681084359914),(0.452822299828566,
0.470019760166366),.UNSPECIFIED.)
GEOMETRIC_REPRESENTATION_ITEM()
RATIONAL_B_SPLINE_SURFACE(((0.98875548626282,0.986817927519786,0.987787102172814),
(0.98875548626282,0.986817927519786,0.987787102172814)))
REPRESENTATION_ITEM('')
SURFACE()
);
#1832=(
BOUNDED_SURFACE()
B_SPLINE_SURFACE(1,2,((#125310,#125311,#125312,#125313,#125314),(#125315,
#125316,#125317,#125318,#125319)),.UNSPECIFIED.,.F.,.F.,.F.)
B_SPLINE_SURFACE_WITH_KNOTS((2,2),(3,2,3),(0.,0.290406869893768),(0.262499170159038,
0.263098999273794,0.280537087669266),.UNSPECIFIED.)
GEOMETRIC_REPRESENTATION_ITEM()
RATIONAL_B_SPLINE_SURFACE(((0.989150325841652,0.989150325841652,0.989150325841652,
0.991395311444461,0.996628941948308),(0.989150325841652,0.989150325841652,
0.989150325841652,0.991395311444461,0.996628941948308)))
REPRESENTATION_ITEM('')
SURFACE()
);
#1833=(
BOUNDED_SURFACE()
B_SPLINE_SURFACE(1,2,((#125336,#125337,#125338),(#125339,#125340,#125341)),
 .UNSPECIFIED.,.F.,.F.,.F.)
B_SPLINE_SURFACE_WITH_KNOTS((2,2),(3,3),(0.,0.289681084359924),(0.452822299828566,
0.470019760166367),.UNSPECIFIED.)
GEOMETRIC_REPRESENTATION_ITEM()
RATIONAL_B_SPLINE_SURFACE(((0.98875548626282,0.986817927519786,0.987787102172814),
(0.98875548626282,0.986817927519786,0.987787102172814)))
REPRESENTATION_ITEM('')
SURFACE()
);
#1834=(
BOUNDED_SURFACE()
B_SPLINE_SURFACE(1,2,((#125343,#125344,#125345,#125346,#125347),(#125348,
#125349,#125350,#125351,#125352)),.UNSPECIFIED.,.F.,.F.,.F.)
B_SPLINE_SURFACE_WITH_KNOTS((2,2),(3,2,3),(0.,0.290406869888898),(0.262499170163906,
0.263098999273794,0.280537087669266),.UNSPECIFIED.)
GEOMETRIC_REPRESENTATION_ITEM()
RATIONAL_B_SPLINE_SURFACE(((0.989150325841652,0.989150325841652,0.989150325841652,
0.991395311444461,0.996628941948308),(0.989150325841652,0.989150325841652,
0.989150325841652,0.991395311444461,0.996628941948308)))
REPRESENTATION_ITEM('')
SURFACE()
);
#1835=(
BOUNDED_SURFACE()
B_SPLINE_SURFACE(1,2,((#125369,#125370,#125371),(#125372,#125373,#125374)),
 .UNSPECIFIED.,.F.,.F.,.F.)
B_SPLINE_SURFACE_WITH_KNOTS((2,2),(3,3),(0.,0.289681084359924),(0.452822299828566,
0.470019760166367),.UNSPECIFIED.)
GEOMETRIC_REPRESENTATION_ITEM()
RATIONAL_B_SPLINE_SURFACE(((0.98875548626282,0.986817927519786,0.987787102172814),
(0.98875548626282,0.986817927519786,0.987787102172814)))
REPRESENTATION_ITEM('')
SURFACE()
);
#1836=(
BOUNDED_SURFACE()
B_SPLINE_SURFACE(1,2,((#125376,#125377,#125378,#125379,#125380),(#125381,
#125382,#125383,#125384,#125385)),.UNSPECIFIED.,.F.,.F.,.F.)
B_SPLINE_SURFACE_WITH_KNOTS((2,2),(3,2,3),(0.,0.290406869893245),(0.262499170159558,
0.263098999273794,0.280537087669266),.UNSPECIFIED.)
GEOMETRIC_REPRESENTATION_ITEM()
RATIONAL_B_SPLINE_SURFACE(((0.989150325841652,0.989150325841652,0.989150325841652,
0.991395311444461,0.996628941948308),(0.989150325841652,0.989150325841652,
0.989150325841652,0.991395311444461,0.996628941948308)))
REPRESENTATION_ITEM('')
SURFACE()
);
#1837=(
BOUNDED_SURFACE()
B_SPLINE_SURFACE(1,2,((#125402,#125403,#125404),(#125405,#125406,#125407)),
 .UNSPECIFIED.,.F.,.F.,.F.)
B_SPLINE_SURFACE_WITH_KNOTS((2,2),(3,3),(0.,0.289681084359924),(0.452822299828566,
0.470019760166501),.UNSPECIFIED.)
GEOMETRIC_REPRESENTATION_ITEM()
RATIONAL_B_SPLINE_SURFACE(((0.988755486262821,0.986817927519771,0.987787102172829),
(0.988755486262821,0.986817927519771,0.987787102172829)))
REPRESENTATION_ITEM('')
SURFACE()
);
#1838=(
BOUNDED_SURFACE()
B_SPLINE_SURFACE(1,2,((#125409,#125410,#125411,#125412,#125413),(#125414,
#125415,#125416,#125417,#125418)),.UNSPECIFIED.,.F.,.F.,.F.)
B_SPLINE_SURFACE_WITH_KNOTS((2,2),(3,2,3),(0.,0.290406869899846),(0.262499170152963,
0.263098999273796,0.280537087669266),.UNSPECIFIED.)
GEOMETRIC_REPRESENTATION_ITEM()
RATIONAL_B_SPLINE_SURFACE(((0.989150325841653,0.989150325841653,0.989150325841653,
0.991395311444461,0.996628941948308),(0.989150325841653,0.989150325841653,
0.989150325841653,0.991395311444461,0.996628941948308)))
REPRESENTATION_ITEM('')
SURFACE()
);
#1839=(
BOUNDED_SURFACE()
B_SPLINE_SURFACE(1,2,((#125435,#125436,#125437),(#125438,#125439,#125440)),
 .UNSPECIFIED.,.F.,.F.,.F.)
B_SPLINE_SURFACE_WITH_KNOTS((2,2),(3,3),(0.,0.289681084359926),(0.452822299828566,
0.470019760166501),.UNSPECIFIED.)
GEOMETRIC_REPRESENTATION_ITEM()
RATIONAL_B_SPLINE_SURFACE(((0.988755486262821,0.986817927519771,0.987787102172829),
(0.988755486262821,0.986817927519771,0.987787102172829)))
REPRESENTATION_ITEM('')
SURFACE()
);
#1840=(
BOUNDED_SURFACE()
B_SPLINE_SURFACE(1,2,((#125442,#125443,#125444,#125445,#125446),(#125447,
#125448,#125449,#125450,#125451)),.UNSPECIFIED.,.F.,.F.,.F.)
B_SPLINE_SURFACE_WITH_KNOTS((2,2),(3,2,3),(0.,0.29040686990032),(0.262499170152489,
0.263098999273796,0.280537087669266),.UNSPECIFIED.)
GEOMETRIC_REPRESENTATION_ITEM()
RATIONAL_B_SPLINE_SURFACE(((0.989150325841653,0.989150325841653,0.989150325841653,
0.991395311444461,0.996628941948308),(0.989150325841653,0.989150325841653,
0.989150325841653,0.991395311444461,0.996628941948308)))
REPRESENTATION_ITEM('')
SURFACE()
);
#1841=(
BOUNDED_SURFACE()
B_SPLINE_SURFACE(1,2,((#125468,#125469,#125470),(#125471,#125472,#125473)),
 .UNSPECIFIED.,.F.,.F.,.F.)
B_SPLINE_SURFACE_WITH_KNOTS((2,2),(3,3),(0.,0.289681084359922),(0.452822299828566,
0.470019760166501),.UNSPECIFIED.)
GEOMETRIC_REPRESENTATION_ITEM()
RATIONAL_B_SPLINE_SURFACE(((0.988755486262821,0.986817927519771,0.987787102172829),
(0.988755486262821,0.986817927519771,0.987787102172829)))
REPRESENTATION_ITEM('')
SURFACE()
);
#1842=(
BOUNDED_SURFACE()
B_SPLINE_SURFACE(1,2,((#125475,#125476,#125477,#125478,#125479),(#125480,
#125481,#125482,#125483,#125484)),.UNSPECIFIED.,.F.,.F.,.F.)
B_SPLINE_SURFACE_WITH_KNOTS((2,2),(3,2,3),(0.,0.290406869901643),(0.262499170151161,
0.263098999273794,0.280537087669266),.UNSPECIFIED.)
GEOMETRIC_REPRESENTATION_ITEM()
RATIONAL_B_SPLINE_SURFACE(((0.989150325841652,0.989150325841652,0.989150325841652,
0.991395311444461,0.996628941948308),(0.989150325841653,0.989150325841653,
0.989150325841653,0.991395311444461,0.996628941948308)))
REPRESENTATION_ITEM('')
SURFACE()
);
#1843=(
BOUNDED_SURFACE()
B_SPLINE_SURFACE(1,2,((#125501,#125502,#125503),(#125504,#125505,#125506)),
 .UNSPECIFIED.,.F.,.F.,.F.)
B_SPLINE_SURFACE_WITH_KNOTS((2,2),(3,3),(0.,0.289681084359917),(0.452822299828566,
0.470019760166501),.UNSPECIFIED.)
GEOMETRIC_REPRESENTATION_ITEM()
RATIONAL_B_SPLINE_SURFACE(((0.988755486262821,0.986817927519771,0.987787102172829),
(0.988755486262821,0.986817927519771,0.987787102172829)))
REPRESENTATION_ITEM('')
SURFACE()
);
#1844=(
BOUNDED_SURFACE()
B_SPLINE_SURFACE(1,2,((#125508,#125509,#125510,#125511,#125512),(#125513,
#125514,#125515,#125516,#125517)),.UNSPECIFIED.,.F.,.F.,.F.)
B_SPLINE_SURFACE_WITH_KNOTS((2,2),(3,2,3),(0.,0.290406869900499),(0.262499170152311,
0.263098999273794,0.280537087669266),.UNSPECIFIED.)
GEOMETRIC_REPRESENTATION_ITEM()
RATIONAL_B_SPLINE_SURFACE(((0.989150325841652,0.989150325841652,0.989150325841652,
0.991395311444461,0.996628941948308),(0.989150325841652,0.989150325841652,
0.989150325841652,0.991395311444461,0.996628941948308)))
REPRESENTATION_ITEM('')
SURFACE()
);
#1845=(
BOUNDED_SURFACE()
B_SPLINE_SURFACE(1,2,((#125534,#125535,#125536),(#125537,#125538,#125539)),
 .UNSPECIFIED.,.F.,.F.,.F.)
B_SPLINE_SURFACE_WITH_KNOTS((2,2),(3,3),(0.,0.289681084359924),(0.452822299828566,
0.470019760166501),.UNSPECIFIED.)
GEOMETRIC_REPRESENTATION_ITEM()
RATIONAL_B_SPLINE_SURFACE(((0.988755486262821,0.986817927519771,0.987787102172829),
(0.98875548626282,0.986817927519771,0.987787102172829)))
REPRESENTATION_ITEM('')
SURFACE()
);
#1846=(
BOUNDED_SURFACE()
B_SPLINE_SURFACE(1,2,((#125541,#125542,#125543,#125544,#125545),(#125546,
#125547,#125548,#125549,#125550)),.UNSPECIFIED.,.F.,.F.,.F.)
B_SPLINE_SURFACE_WITH_KNOTS((2,2),(3,2,3),(0.,0.290038654277662),(0.262867385775147,
0.263098999273794,0.280537087669266),.UNSPECIFIED.)
GEOMETRIC_REPRESENTATION_ITEM()
RATIONAL_B_SPLINE_SURFACE(((0.989150325841652,0.989150325841652,0.989150325841652,
0.991395311444461,0.996628941948308),(0.989150325841652,0.989150325841652,
0.989150325841652,0.991395311444461,0.996628941948308)))
REPRESENTATION_ITEM('')
SURFACE()
);
#1847=(
BOUNDED_SURFACE()
B_SPLINE_SURFACE(1,2,((#125558,#125559,#125560),(#125561,#125562,#125563)),
 .UNSPECIFIED.,.F.,.F.,.F.)
B_SPLINE_SURFACE_WITH_KNOTS((2,2),(3,3),(0.,0.289681084359922),(0.452822299828566,
0.470019760166501),.UNSPECIFIED.)
GEOMETRIC_REPRESENTATION_ITEM()
RATIONAL_B_SPLINE_SURFACE(((0.988755486262821,0.986817927519771,0.987787102172829),
(0.988755486262821,0.986817927519771,0.987787102172829)))
REPRESENTATION_ITEM('')
SURFACE()
);
#1848=(
BOUNDED_SURFACE()
B_SPLINE_SURFACE(1,2,((#125565,#125566,#125567,#125568,#125569),(#125570,
#125571,#125572,#125573,#125574)),.UNSPECIFIED.,.F.,.F.,.F.)
B_SPLINE_SURFACE_WITH_KNOTS((2,2),(3,2,3),(0.,0.290406869901189),(0.262499170151615,
0.263098999273794,0.280537087669266),.UNSPECIFIED.)
GEOMETRIC_REPRESENTATION_ITEM()
RATIONAL_B_SPLINE_SURFACE(((0.989150325841652,0.989150325841652,0.989150325841652,
0.991395311444461,0.996628941948308),(0.989150325841652,0.989150325841652,
0.989150325841652,0.991395311444461,0.996628941948308)))
REPRESENTATION_ITEM('')
SURFACE()
);
#1849=(
BOUNDED_SURFACE()
B_SPLINE_SURFACE(1,2,((#125591,#125592,#125593),(#125594,#125595,#125596)),
 .UNSPECIFIED.,.F.,.F.,.F.)
B_SPLINE_SURFACE_WITH_KNOTS((2,2),(3,3),(0.,0.289681084359921),(0.452822299828566,
0.470019760166501),.UNSPECIFIED.)
GEOMETRIC_REPRESENTATION_ITEM()
RATIONAL_B_SPLINE_SURFACE(((0.98875548626282,0.986817927519771,0.987787102172829),
(0.98875548626282,0.986817927519771,0.987787102172829)))
REPRESENTATION_ITEM('')
SURFACE()
);
#1850=(
BOUNDED_SURFACE()
B_SPLINE_SURFACE(1,2,((#125598,#125599,#125600,#125601,#125602),(#125603,
#125604,#125605,#125606,#125607)),.UNSPECIFIED.,.F.,.F.,.F.)
B_SPLINE_SURFACE_WITH_KNOTS((2,2),(3,2,3),(0.,0.290406869898487),(0.26249917015432,
0.263098999273794,0.280537087669266),.UNSPECIFIED.)
GEOMETRIC_REPRESENTATION_ITEM()
RATIONAL_B_SPLINE_SURFACE(((0.989150325841652,0.989150325841652,0.989150325841652,
0.991395311444461,0.996628941948308),(0.989150325841652,0.989150325841652,
0.989150325841652,0.991395311444461,0.996628941948308)))
REPRESENTATION_ITEM('')
SURFACE()
);
#1851=(
BOUNDED_SURFACE()
B_SPLINE_SURFACE(1,2,((#125624,#125625,#125626),(#125627,#125628,#125629)),
 .UNSPECIFIED.,.F.,.F.,.F.)
B_SPLINE_SURFACE_WITH_KNOTS((2,2),(3,3),(0.,0.289681084359928),(0.452822299828566,
0.470019760166367),.UNSPECIFIED.)
GEOMETRIC_REPRESENTATION_ITEM()
RATIONAL_B_SPLINE_SURFACE(((0.98875548626282,0.986817927519786,0.987787102172814),
(0.98875548626282,0.986817927519786,0.987787102172814)))
REPRESENTATION_ITEM('')
SURFACE()
);
#1852=(
BOUNDED_SURFACE()
B_SPLINE_SURFACE(1,2,((#125631,#125632,#125633,#125634,#125635),(#125636,
#125637,#125638,#125639,#125640)),.UNSPECIFIED.,.F.,.F.,.F.)
B_SPLINE_SURFACE_WITH_KNOTS((2,2),(3,2,3),(0.,0.290406869899282),(0.262499170153521,
0.263098999273794,0.280537087669266),.UNSPECIFIED.)
GEOMETRIC_REPRESENTATION_ITEM()
RATIONAL_B_SPLINE_SURFACE(((0.989150325841652,0.989150325841652,0.989150325841652,
0.991395311444461,0.996628941948308),(0.989150325841652,0.989150325841652,
0.989150325841652,0.991395311444461,0.996628941948308)))
REPRESENTATION_ITEM('')
SURFACE()
);
#1853=(
BOUNDED_SURFACE()
B_SPLINE_SURFACE(1,2,((#125657,#125658,#125659),(#125660,#125661,#125662)),
 .UNSPECIFIED.,.F.,.F.,.F.)
B_SPLINE_SURFACE_WITH_KNOTS((2,2),(3,3),(0.,0.289681084359918),(0.452822299828566,
0.470019760166367),.UNSPECIFIED.)
GEOMETRIC_REPRESENTATION_ITEM()
RATIONAL_B_SPLINE_SURFACE(((0.98875548626282,0.986817927519786,0.987787102172814),
(0.98875548626282,0.986817927519786,0.987787102172814)))
REPRESENTATION_ITEM('')
SURFACE()
);
#1854=(
BOUNDED_SURFACE()
B_SPLINE_SURFACE(1,2,((#125664,#125665,#125666,#125667,#125668),(#125669,
#125670,#125671,#125672,#125673)),.UNSPECIFIED.,.F.,.F.,.F.)
B_SPLINE_SURFACE_WITH_KNOTS((2,2),(3,2,3),(0.,0.290406869910884),(0.262499170141919,
0.263098999273794,0.280537087669266),.UNSPECIFIED.)
GEOMETRIC_REPRESENTATION_ITEM()
RATIONAL_B_SPLINE_SURFACE(((0.989150325841652,0.989150325841652,0.989150325841652,
0.991395311444461,0.996628941948308),(0.989150325841652,0.989150325841652,
0.989150325841652,0.991395311444461,0.996628941948308)))
REPRESENTATION_ITEM('')
SURFACE()
);
#1855=(
BOUNDED_SURFACE()
B_SPLINE_SURFACE(1,2,((#125690,#125691,#125692),(#125693,#125694,#125695)),
 .UNSPECIFIED.,.F.,.F.,.F.)
B_SPLINE_SURFACE_WITH_KNOTS((2,2),(3,3),(0.,0.289681084359921),(0.452822299828567,
0.470019760166367),.UNSPECIFIED.)
GEOMETRIC_REPRESENTATION_ITEM()
RATIONAL_B_SPLINE_SURFACE(((0.98875548626282,0.986817927519786,0.987787102172814),
(0.98875548626282,0.986817927519786,0.987787102172814)))
REPRESENTATION_ITEM('')
SURFACE()
);
#1856=(
BOUNDED_SURFACE()
B_SPLINE_SURFACE(1,2,((#125697,#125698,#125699,#125700,#125701),(#125702,
#125703,#125704,#125705,#125706)),.UNSPECIFIED.,.F.,.F.,.F.)
B_SPLINE_SURFACE_WITH_KNOTS((2,2),(3,2,3),(0.,0.290406869918552),(0.262499170134253,
0.263098999273794,0.280537087669266),.UNSPECIFIED.)
GEOMETRIC_REPRESENTATION_ITEM()
RATIONAL_B_SPLINE_SURFACE(((0.989150325841652,0.989150325841652,0.989150325841652,
0.991395311444461,0.996628941948308),(0.989150325841652,0.989150325841652,
0.989150325841652,0.991395311444461,0.996628941948308)))
REPRESENTATION_ITEM('')
SURFACE()
);
#1857=(
BOUNDED_SURFACE()
B_SPLINE_SURFACE(1,2,((#125723,#125724,#125725),(#125726,#125727,#125728)),
 .UNSPECIFIED.,.F.,.F.,.F.)
B_SPLINE_SURFACE_WITH_KNOTS((2,2),(3,3),(0.,0.28968108435992),(0.452822299828566,
0.470019760166367),.UNSPECIFIED.)
GEOMETRIC_REPRESENTATION_ITEM()
RATIONAL_B_SPLINE_SURFACE(((0.98875548626282,0.986817927519786,0.987787102172814),
(0.98875548626282,0.986817927519786,0.987787102172814)))
REPRESENTATION_ITEM('')
SURFACE()
);
#1858=(
BOUNDED_SURFACE()
B_SPLINE_SURFACE(1,2,((#125730,#125731,#125732,#125733,#125734),(#125735,
#125736,#125737,#125738,#125739)),.UNSPECIFIED.,.F.,.F.,.F.)
B_SPLINE_SURFACE_WITH_KNOTS((2,2),(3,2,3),(0.,0.290406869903407),(0.262499170150806,
0.263098999273794,0.280537087669266),.UNSPECIFIED.)
GEOMETRIC_REPRESENTATION_ITEM()
RATIONAL_B_SPLINE_SURFACE(((0.989150325841652,0.989150325841652,0.989150325841652,
0.991395311444461,0.996628941948308),(0.989150325841652,0.989150325841652,
0.989150325841652,0.991395311444461,0.996628941948308)))
REPRESENTATION_ITEM('')
SURFACE()
);
#1859=(
BOUNDED_SURFACE()
B_SPLINE_SURFACE(1,2,((#125756,#125757,#125758),(#125759,#125760,#125761)),
 .UNSPECIFIED.,.F.,.F.,.F.)
B_SPLINE_SURFACE_WITH_KNOTS((2,2),(3,3),(0.,0.289681084359922),(0.452822299828566,
0.470019760166367),.UNSPECIFIED.)
GEOMETRIC_REPRESENTATION_ITEM()
RATIONAL_B_SPLINE_SURFACE(((0.98875548626282,0.986817927519786,0.987787102172814),
(0.98875548626282,0.986817927519786,0.987787102172814)))
REPRESENTATION_ITEM('')
SURFACE()
);
#1860=(
BOUNDED_SURFACE()
B_SPLINE_SURFACE(1,2,((#125763,#125764,#125765,#125766,#125767),(#125768,
#125769,#125770,#125771,#125772)),.UNSPECIFIED.,.F.,.F.,.F.)
B_SPLINE_SURFACE_WITH_KNOTS((2,2),(3,2,3),(0.,0.290406869880632),(0.26249917017217,
0.263098999273794,0.280537087669266),.UNSPECIFIED.)
GEOMETRIC_REPRESENTATION_ITEM()
RATIONAL_B_SPLINE_SURFACE(((0.989150325841652,0.989150325841652,0.989150325841652,
0.991395311444461,0.996628941948308),(0.989150325841652,0.989150325841652,
0.989150325841652,0.991395311444461,0.996628941948308)))
REPRESENTATION_ITEM('')
SURFACE()
);
#1861=(
BOUNDED_SURFACE()
B_SPLINE_SURFACE(1,2,((#125783,#125784,#125785),(#125786,#125787,#125788)),
 .UNSPECIFIED.,.F.,.F.,.F.)
B_SPLINE_SURFACE_WITH_KNOTS((2,2),(3,3),(0.,0.289681084359921),(0.452822299828567,
0.470019760166369),.UNSPECIFIED.)
GEOMETRIC_REPRESENTATION_ITEM()
RATIONAL_B_SPLINE_SURFACE(((0.98875548626282,0.986817927519786,0.987787102172814),
(0.98875548626282,0.986817927519786,0.987787102172814)))
REPRESENTATION_ITEM('')
SURFACE()
);
#1862=(
BOUNDED_SURFACE()
B_SPLINE_SURFACE(1,2,((#125796,#125797,#125798,#125799,#125800),(#125801,
#125802,#125803,#125804,#125805)),.UNSPECIFIED.,.F.,.F.,.F.)
B_SPLINE_SURFACE_WITH_KNOTS((2,2),(3,2,3),(0.,0.290406869877571),(0.262499170175233,
0.263098999273796,0.280537087669266),.UNSPECIFIED.)
GEOMETRIC_REPRESENTATION_ITEM()
RATIONAL_B_SPLINE_SURFACE(((0.989150325841653,0.989150325841653,0.989150325841653,
0.991395311444461,0.996628941948308),(0.989150325841653,0.989150325841653,
0.989150325841653,0.991395311444461,0.996628941948308)))
REPRESENTATION_ITEM('')
SURFACE()
);
#1863=(
BOUNDED_SURFACE()
B_SPLINE_SURFACE(1,2,((#125822,#125823,#125824),(#125825,#125826,#125827)),
 .UNSPECIFIED.,.F.,.F.,.F.)
B_SPLINE_SURFACE_WITH_KNOTS((2,2),(3,3),(0.,0.289681084359925),(0.452822299828567,
0.470019760166366),.UNSPECIFIED.)
GEOMETRIC_REPRESENTATION_ITEM()
RATIONAL_B_SPLINE_SURFACE(((0.98875548626282,0.986817927519786,0.987787102172814),
(0.98875548626282,0.986817927519787,0.987787102172814)))
REPRESENTATION_ITEM('')
SURFACE()
);
#1864=(
BOUNDED_SURFACE()
B_SPLINE_SURFACE(1,2,((#125829,#125830,#125831,#125832,#125833),(#125834,
#125835,#125836,#125837,#125838)),.UNSPECIFIED.,.F.,.F.,.F.)
B_SPLINE_SURFACE_WITH_KNOTS((2,2),(3,2,3),(0.,0.290406869909595),(0.262499170143283,
0.263098999273795,0.280537087669267),.UNSPECIFIED.)
GEOMETRIC_REPRESENTATION_ITEM()
RATIONAL_B_SPLINE_SURFACE(((0.989150325841653,0.989150325841653,0.989150325841653,
0.991395311444461,0.996628941948308),(0.989150325841653,0.989150325841653,
0.989150325841653,0.991395311444461,0.996628941948308)))
REPRESENTATION_ITEM('')
SURFACE()
);
#1865=(
BOUNDED_SURFACE()
B_SPLINE_SURFACE(1,2,((#125855,#125856,#125857),(#125858,#125859,#125860)),
 .UNSPECIFIED.,.F.,.F.,.F.)
B_SPLINE_SURFACE_WITH_KNOTS((2,2),(3,3),(0.,0.289681084359917),(0.452822299828565,
0.470019760166369),.UNSPECIFIED.)
GEOMETRIC_REPRESENTATION_ITEM()
RATIONAL_B_SPLINE_SURFACE(((0.988755486262821,0.986817927519786,0.987787102172814),
(0.988755486262821,0.986817927519786,0.987787102172814)))
REPRESENTATION_ITEM('')
SURFACE()
);
#1866=(
BOUNDED_SURFACE()
B_SPLINE_SURFACE(1,2,((#125862,#125863,#125864,#125865,#125866),(#125867,
#125868,#125869,#125870,#125871)),.UNSPECIFIED.,.F.,.F.,.F.)
B_SPLINE_SURFACE_WITH_KNOTS((2,2),(3,2,3),(0.,0.290406869891073),(0.262499170161812,
0.263098999273795,0.280537087669267),.UNSPECIFIED.)
GEOMETRIC_REPRESENTATION_ITEM()
RATIONAL_B_SPLINE_SURFACE(((0.989150325841653,0.989150325841653,0.989150325841653,
0.991395311444461,0.996628941948308),(0.989150325841653,0.989150325841653,
0.989150325841653,0.991395311444461,0.996628941948308)))
REPRESENTATION_ITEM('')
SURFACE()
);
#1867=(
BOUNDED_SURFACE()
B_SPLINE_SURFACE(1,2,((#125888,#125889,#125890),(#125891,#125892,#125893)),
 .UNSPECIFIED.,.F.,.F.,.F.)
B_SPLINE_SURFACE_WITH_KNOTS((2,2),(3,3),(0.,0.289681084359919),(0.452822299828565,
0.470019760166396),.UNSPECIFIED.)
GEOMETRIC_REPRESENTATION_ITEM()
RATIONAL_B_SPLINE_SURFACE(((0.988755486262821,0.986817927519783,0.987787102172817),
(0.988755486262821,0.986817927519783,0.987787102172817)))
REPRESENTATION_ITEM('')
SURFACE()
);
#1868=(
BOUNDED_SURFACE()
B_SPLINE_SURFACE(1,2,((#125895,#125896,#125897,#125898,#125899),(#125900,
#125901,#125902,#125903,#125904)),.UNSPECIFIED.,.F.,.F.,.F.)
B_SPLINE_SURFACE_WITH_KNOTS((2,2),(3,2,3),(0.,0.290406869911321),(0.262499170142164,
0.263098999273795,0.280537087669267),.UNSPECIFIED.)
GEOMETRIC_REPRESENTATION_ITEM()
RATIONAL_B_SPLINE_SURFACE(((0.989150325841653,0.989150325841653,0.989150325841653,
0.991395311444461,0.996628941948308),(0.989150325841653,0.989150325841653,
0.989150325841653,0.991395311444461,0.996628941948308)))
REPRESENTATION_ITEM('')
SURFACE()
);
#1869=(
BOUNDED_SURFACE()
B_SPLINE_SURFACE(1,2,((#125921,#125922,#125923),(#125924,#125925,#125926)),
 .UNSPECIFIED.,.F.,.F.,.F.)
B_SPLINE_SURFACE_WITH_KNOTS((2,2),(3,3),(0.,0.289681084359927),(0.452822299828565,
0.470019760166366),.UNSPECIFIED.)
GEOMETRIC_REPRESENTATION_ITEM()
RATIONAL_B_SPLINE_SURFACE(((0.988755486262821,0.986817927519786,0.987787102172814),
(0.988755486262821,0.986817927519787,0.987787102172814)))
REPRESENTATION_ITEM('')
SURFACE()
);
#1870=(
BOUNDED_SURFACE()
B_SPLINE_SURFACE(1,2,((#125928,#125929,#125930,#125931,#125932),(#125933,
#125934,#125935,#125936,#125937)),.UNSPECIFIED.,.F.,.F.,.F.)
B_SPLINE_SURFACE_WITH_KNOTS((2,2),(3,2,3),(0.,0.29040686991619),(0.262499170136658,
0.263098999273795,0.280537087669267),.UNSPECIFIED.)
GEOMETRIC_REPRESENTATION_ITEM()
RATIONAL_B_SPLINE_SURFACE(((0.989150325841653,0.989150325841653,0.989150325841653,
0.991395311444461,0.996628941948308),(0.989150325841653,0.989150325841653,
0.989150325841653,0.991395311444461,0.996628941948308)))
REPRESENTATION_ITEM('')
SURFACE()
);
#1871=(
BOUNDED_SURFACE()
B_SPLINE_SURFACE(1,2,((#125954,#125955,#125956),(#125957,#125958,#125959)),
 .UNSPECIFIED.,.F.,.F.,.F.)
B_SPLINE_SURFACE_WITH_KNOTS((2,2),(3,3),(0.,0.289681084359918),(0.452822299828565,
0.470019760166365),.UNSPECIFIED.)
GEOMETRIC_REPRESENTATION_ITEM()
RATIONAL_B_SPLINE_SURFACE(((0.988755486262821,0.986817927519786,0.987787102172814),
(0.988755486262821,0.986817927519787,0.987787102172814)))
REPRESENTATION_ITEM('')
SURFACE()
);
#1872=(
BOUNDED_SURFACE()
B_SPLINE_SURFACE(1,2,((#125961,#125962,#125963,#125964,#125965),(#125966,
#125967,#125968,#125969,#125970)),.UNSPECIFIED.,.F.,.F.,.F.)
B_SPLINE_SURFACE_WITH_KNOTS((2,2),(3,2,3),(0.,0.290406869902415),(0.262499170150461,
0.263098999273795,0.280537087669267),.UNSPECIFIED.)
GEOMETRIC_REPRESENTATION_ITEM()
RATIONAL_B_SPLINE_SURFACE(((0.989150325841653,0.989150325841653,0.989150325841653,
0.991395311444461,0.996628941948308),(0.989150325841653,0.989150325841653,
0.989150325841653,0.991395311444461,0.996628941948308)))
REPRESENTATION_ITEM('')
SURFACE()
);
#1873=(
BOUNDED_SURFACE()
B_SPLINE_SURFACE(1,2,((#125987,#125988,#125989),(#125990,#125991,#125992)),
 .UNSPECIFIED.,.F.,.F.,.F.)
B_SPLINE_SURFACE_WITH_KNOTS((2,2),(3,3),(0.,0.289681084359927),(0.452822299828565,
0.470019760166365),.UNSPECIFIED.)
GEOMETRIC_REPRESENTATION_ITEM()
RATIONAL_B_SPLINE_SURFACE(((0.988755486262821,0.986817927519786,0.987787102172814),
(0.988755486262821,0.986817927519787,0.987787102172814)))
REPRESENTATION_ITEM('')
SURFACE()
);
#1874=(
BOUNDED_SURFACE()
B_SPLINE_SURFACE(1,2,((#125994,#125995,#125996,#125997,#125998),(#125999,
#126000,#126001,#126002,#126003)),.UNSPECIFIED.,.F.,.F.,.F.)
B_SPLINE_SURFACE_WITH_KNOTS((2,2),(3,2,3),(0.,0.290406869886822),(0.262499170166043,
0.263098999273795,0.280537087669266),.UNSPECIFIED.)
GEOMETRIC_REPRESENTATION_ITEM()
RATIONAL_B_SPLINE_SURFACE(((0.989150325841653,0.989150325841653,0.989150325841653,
0.991395311444461,0.996628941948308),(0.989150325841653,0.989150325841653,
0.989150325841653,0.991395311444461,0.996628941948308)))
REPRESENTATION_ITEM('')
SURFACE()
);
#1875=(
BOUNDED_SURFACE()
B_SPLINE_SURFACE(1,2,((#126020,#126021,#126022),(#126023,#126024,#126025)),
 .UNSPECIFIED.,.F.,.F.,.F.)
B_SPLINE_SURFACE_WITH_KNOTS((2,2),(3,3),(0.,0.289681084359919),(0.452822299828566,
0.470019760166367),.UNSPECIFIED.)
GEOMETRIC_REPRESENTATION_ITEM()
RATIONAL_B_SPLINE_SURFACE(((0.98875548626282,0.986817927519786,0.987787102172814),
(0.98875548626282,0.986817927519786,0.987787102172814)))
REPRESENTATION_ITEM('')
SURFACE()
);
#1876=(
BOUNDED_SURFACE()
B_SPLINE_SURFACE(1,2,((#126027,#126028,#126029,#126030,#126031),(#126032,
#126033,#126034,#126035,#126036)),.UNSPECIFIED.,.F.,.F.,.F.)
B_SPLINE_SURFACE_WITH_KNOTS((2,2),(3,2,3),(0.710318915640084,1.),(0.504616569534327,
0.52191752982614,0.522090539429058),.UNSPECIFIED.)
GEOMETRIC_REPRESENTATION_ITEM()
RATIONAL_B_SPLINE_SURFACE(((0.996968549833597,0.991680746768561,0.989334769731189,
0.989334769731189,0.989334769731189),(0.996968549833597,0.991680746768561,
0.989334769731189,0.989334769731189,0.989334769731189)))
REPRESENTATION_ITEM('')
SURFACE()
);
#1877=(
BOUNDED_SURFACE()
B_SPLINE_SURFACE(1,2,((#126047,#126048,#126049,#126050,#126051),(#126052,
#126053,#126054,#126055,#126056)),.UNSPECIFIED.,.F.,.F.,.F.)
B_SPLINE_SURFACE_WITH_KNOTS((2,2),(3,2,3),(0.710192959008446,1.),(0.211502584834065,
0.214285714285714,0.228987659635175),.UNSPECIFIED.)
GEOMETRIC_REPRESENTATION_ITEM()
RATIONAL_B_SPLINE_SURFACE(((0.998122319569323,0.999023095875705,1.,0.994839481491404,
0.99180331349328),(0.998122319569323,0.999023095875705,1.,0.994839481491404,
0.99180331349328)))
REPRESENTATION_ITEM('')
SURFACE()
);
#1878=(
BOUNDED_SURFACE()
B_SPLINE_SURFACE(1,2,((#126070,#126071,#126072,#126073,#126074),(#126075,
#126076,#126077,#126078,#126079)),.UNSPECIFIED.,.F.,.F.,.F.)
B_SPLINE_SURFACE_WITH_KNOTS((2,2),(3,2,3),(0.709731017409647,1.),(0.504616569534327,
0.52191752982614,0.522505428214631),.UNSPECIFIED.)
GEOMETRIC_REPRESENTATION_ITEM()
RATIONAL_B_SPLINE_SURFACE(((0.996968549833597,0.991680746768561,0.989334769731189,
0.989334769731189,0.989334769731189),(0.996968549833597,0.991680746768561,
0.989334769731189,0.989334769731189,0.989334769731189)))
REPRESENTATION_ITEM('')
SURFACE()
);
#1879=(
BOUNDED_SURFACE()
B_SPLINE_SURFACE(1,2,((#126090,#126091,#126092,#126093,#126094),(#126095,
#126096,#126097,#126098,#126099)),.UNSPECIFIED.,.F.,.F.,.F.)
B_SPLINE_SURFACE_WITH_KNOTS((2,2),(3,2,3),(0.710192959007514,1.),(0.211502584834065,
0.214285714285714,0.228987659635175),.UNSPECIFIED.)
GEOMETRIC_REPRESENTATION_ITEM()
RATIONAL_B_SPLINE_SURFACE(((0.998122319569323,0.999023095875705,1.,0.994839481491404,
0.99180331349328),(0.998122319569323,0.999023095875705,1.,0.994839481491404,
0.99180331349328)))
REPRESENTATION_ITEM('')
SURFACE()
);
#1880=(
BOUNDED_SURFACE()
B_SPLINE_SURFACE(1,2,((#126113,#126114,#126115,#126116,#126117),(#126118,
#126119,#126120,#126121,#126122)),.UNSPECIFIED.,.F.,.F.,.F.)
B_SPLINE_SURFACE_WITH_KNOTS((2,2),(3,2,3),(0.709731017450111,1.),(0.504616569534327,
0.52191752982614,0.522505428174168),.UNSPECIFIED.)
GEOMETRIC_REPRESENTATION_ITEM()
RATIONAL_B_SPLINE_SURFACE(((0.996968549833597,0.991680746768561,0.989334769731189,
0.989334769731189,0.989334769731189),(0.996968549833597,0.991680746768561,
0.989334769731189,0.989334769731189,0.989334769731189)))
REPRESENTATION_ITEM('')
SURFACE()
);
#1881=(
BOUNDED_SURFACE()
B_SPLINE_SURFACE(1,2,((#126133,#126134,#126135,#126136,#126137),(#126138,
#126139,#126140,#126141,#126142)),.UNSPECIFIED.,.F.,.F.,.F.)
B_SPLINE_SURFACE_WITH_KNOTS((2,2),(3,2,3),(0.710192959007509,1.),(0.211502584834065,
0.214285714285714,0.228987659635175),.UNSPECIFIED.)
GEOMETRIC_REPRESENTATION_ITEM()
RATIONAL_B_SPLINE_SURFACE(((0.998122319569323,0.999023095875705,1.,0.994839481491404,
0.99180331349328),(0.998122319569323,0.999023095875705,1.,0.994839481491404,
0.99180331349328)))
REPRESENTATION_ITEM('')
SURFACE()
);
#1882=(
BOUNDED_SURFACE()
B_SPLINE_SURFACE(1,2,((#126156,#126157,#126158,#126159,#126160),(#126161,
#126162,#126163,#126164,#126165)),.UNSPECIFIED.,.F.,.F.,.F.)
B_SPLINE_SURFACE_WITH_KNOTS((2,2),(3,2,3),(0.709731017378141,1.),(0.504616569534327,
0.52191752982614,0.522505428246138),.UNSPECIFIED.)
GEOMETRIC_REPRESENTATION_ITEM()
RATIONAL_B_SPLINE_SURFACE(((0.996968549833598,0.991680746768561,0.989334769731189,
0.989334769731189,0.989334769731189),(0.996968549833598,0.991680746768561,
0.989334769731189,0.989334769731189,0.989334769731189)))
REPRESENTATION_ITEM('')
SURFACE()
);
#1883=(
BOUNDED_SURFACE()
B_SPLINE_SURFACE(1,2,((#126176,#126177,#126178,#126179,#126180),(#126181,
#126182,#126183,#126184,#126185)),.UNSPECIFIED.,.F.,.F.,.F.)
B_SPLINE_SURFACE_WITH_KNOTS((2,2),(3,2,3),(0.710192959007511,1.),(0.211502584834065,
0.214285714285714,0.228987659635175),.UNSPECIFIED.)
GEOMETRIC_REPRESENTATION_ITEM()
RATIONAL_B_SPLINE_SURFACE(((0.998122319569323,0.999023095875705,1.,0.994839481491404,
0.99180331349328),(0.998122319569323,0.999023095875705,1.,0.994839481491404,
0.99180331349328)))
REPRESENTATION_ITEM('')
SURFACE()
);
#1884=(
BOUNDED_SURFACE()
B_SPLINE_SURFACE(1,2,((#126199,#126200,#126201,#126202,#126203),(#126204,
#126205,#126206,#126207,#126208)),.UNSPECIFIED.,.F.,.F.,.F.)
B_SPLINE_SURFACE_WITH_KNOTS((2,2),(3,2,3),(0.709731017387927,1.),(0.504616569534327,
0.52191752982614,0.522505428181681),.UNSPECIFIED.)
GEOMETRIC_REPRESENTATION_ITEM()
RATIONAL_B_SPLINE_SURFACE(((0.996968549833597,0.991680746768561,0.989334769731189,
0.989334769731189,0.989334769731189),(0.996968549833597,0.991680746768561,
0.989334769731189,0.989334769731189,0.989334769731189)))
REPRESENTATION_ITEM('')
SURFACE()
);
#1885=(
BOUNDED_SURFACE()
B_SPLINE_SURFACE(1,2,((#126219,#126220,#126221,#126222,#126223),(#126224,
#126225,#126226,#126227,#126228)),.UNSPECIFIED.,.F.,.F.,.F.)
B_SPLINE_SURFACE_WITH_KNOTS((2,2),(3,2,3),(0.710192959006926,1.),(0.211502584834065,
0.214285714285714,0.228987659635175),.UNSPECIFIED.)
GEOMETRIC_REPRESENTATION_ITEM()
RATIONAL_B_SPLINE_SURFACE(((0.998122319569323,0.999023095875705,1.,0.994839481491404,
0.991803313493279),(0.998122319569323,0.999023095875705,1.,0.994839481491404,
0.991803313493279)))
REPRESENTATION_ITEM('')
SURFACE()
);
#1886=(
BOUNDED_SURFACE()
B_SPLINE_SURFACE(1,2,((#126242,#126243,#126244,#126245,#126246),(#126247,
#126248,#126249,#126250,#126251)),.UNSPECIFIED.,.F.,.F.,.F.)
B_SPLINE_SURFACE_WITH_KNOTS((2,2),(3,2,3),(0.710318915639154,1.),(0.504616569534327,
0.52191752982614,0.522090539429058),.UNSPECIFIED.)
GEOMETRIC_REPRESENTATION_ITEM()
RATIONAL_B_SPLINE_SURFACE(((0.996968549833597,0.991680746768561,0.989334769731189,
0.989334769731189,0.989334769731189),(0.996968549833597,0.991680746768561,
0.989334769731189,0.989334769731189,0.989334769731189)))
REPRESENTATION_ITEM('')
SURFACE()
);
#1887=(
BOUNDED_SURFACE()
B_SPLINE_SURFACE(1,2,((#126262,#126263,#126264,#126265,#126266),(#126267,
#126268,#126269,#126270,#126271)),.UNSPECIFIED.,.F.,.F.,.F.)
B_SPLINE_SURFACE_WITH_KNOTS((2,2),(3,2,3),(0.710192959007513,1.),(0.211502584834065,
0.214285714285714,0.228987659635175),.UNSPECIFIED.)
GEOMETRIC_REPRESENTATION_ITEM()
RATIONAL_B_SPLINE_SURFACE(((0.998122319569323,0.999023095875705,1.,0.994839481491404,
0.991803313493279),(0.998122319569323,0.999023095875705,1.,0.994839481491404,
0.991803313493279)))
REPRESENTATION_ITEM('')
SURFACE()
);
#1888=(
BOUNDED_SURFACE()
B_SPLINE_SURFACE(1,2,((#126285,#126286,#126287,#126288,#126289),(#126290,
#126291,#126292,#126293,#126294)),.UNSPECIFIED.,.F.,.F.,.F.)
B_SPLINE_SURFACE_WITH_KNOTS((2,2),(3,2,3),(0.709731017354647,1.),(0.504616569534327,
0.52191752982614,0.522505428214449),.UNSPECIFIED.)
GEOMETRIC_REPRESENTATION_ITEM()
RATIONAL_B_SPLINE_SURFACE(((0.996968549833597,0.991680746768561,0.989334769731189,
0.989334769731189,0.989334769731189),(0.996968549833597,0.991680746768561,
0.989334769731189,0.989334769731189,0.989334769731189)))
REPRESENTATION_ITEM('')
SURFACE()
);
#1889=(
BOUNDED_SURFACE()
B_SPLINE_SURFACE(1,2,((#126305,#126306,#126307,#126308,#126309),(#126310,
#126311,#126312,#126313,#126314)),.UNSPECIFIED.,.F.,.F.,.F.)
B_SPLINE_SURFACE_WITH_KNOTS((2,2),(3,2,3),(0.710192959006931,1.),(0.211502584834065,
0.214285714285714,0.228987659635175),.UNSPECIFIED.)
GEOMETRIC_REPRESENTATION_ITEM()
RATIONAL_B_SPLINE_SURFACE(((0.998122319569323,0.999023095875705,1.,0.994839481491404,
0.99180331349328),(0.998122319569323,0.999023095875705,1.,0.994839481491404,
0.99180331349328)))
REPRESENTATION_ITEM('')
SURFACE()
);
#1890=(
BOUNDED_SURFACE()
B_SPLINE_SURFACE(1,2,((#126328,#126329,#126330,#126331,#126332),(#126333,
#126334,#126335,#126336,#126337)),.UNSPECIFIED.,.F.,.F.,.F.)
B_SPLINE_SURFACE_WITH_KNOTS((2,2),(3,2,3),(0.710318915639071,1.),(0.504616569534328,
0.52191752982614,0.522090539429058),.UNSPECIFIED.)
GEOMETRIC_REPRESENTATION_ITEM()
RATIONAL_B_SPLINE_SURFACE(((0.996968549833597,0.991680746768561,0.989334769731189,
0.989334769731189,0.989334769731189),(0.996968549833597,0.991680746768561,
0.989334769731189,0.989334769731189,0.989334769731189)))
REPRESENTATION_ITEM('')
SURFACE()
);
#1891=(
BOUNDED_SURFACE()
B_SPLINE_SURFACE(1,2,((#126348,#126349,#126350,#126351,#126352),(#126353,
#126354,#126355,#126356,#126357)),.UNSPECIFIED.,.F.,.F.,.F.)
B_SPLINE_SURFACE_WITH_KNOTS((2,2),(3,2,3),(0.710192959007428,1.),(0.211502584834064,
0.214285714285714,0.228987659635174),.UNSPECIFIED.)
GEOMETRIC_REPRESENTATION_ITEM()
RATIONAL_B_SPLINE_SURFACE(((0.998122319569322,0.999023095875704,1.,0.994839481491404,
0.99180331349328),(0.998122319569322,0.999023095875704,1.,0.994839481491405,
0.99180331349328)))
REPRESENTATION_ITEM('')
SURFACE()
);
#1892=(
BOUNDED_SURFACE()
B_SPLINE_SURFACE(1,2,((#126371,#126372,#126373,#126374,#126375),(#126376,
#126377,#126378,#126379,#126380)),.UNSPECIFIED.,.F.,.F.,.F.)
B_SPLINE_SURFACE_WITH_KNOTS((2,2),(3,2,3),(0.709731017404435,1.),(0.504616569534328,
0.521917529826141,0.522505428219767),.UNSPECIFIED.)
GEOMETRIC_REPRESENTATION_ITEM()
RATIONAL_B_SPLINE_SURFACE(((0.996968549833597,0.991680746768561,0.989334769731189,
0.989334769731189,0.989334769731189),(0.996968549833597,0.991680746768561,
0.989334769731189,0.989334769731189,0.989334769731189)))
REPRESENTATION_ITEM('')
SURFACE()
);
#1893=(
BOUNDED_SURFACE()
B_SPLINE_SURFACE(1,2,((#126391,#126392,#126393,#126394,#126395),(#126396,
#126397,#126398,#126399,#126400)),.UNSPECIFIED.,.F.,.F.,.F.)
B_SPLINE_SURFACE_WITH_KNOTS((2,2),(3,2,3),(0.710192959007438,1.),(0.211502584834064,
0.214285714285714,0.228987659635174),.UNSPECIFIED.)
GEOMETRIC_REPRESENTATION_ITEM()
RATIONAL_B_SPLINE_SURFACE(((0.998122319569322,0.999023095875704,1.,0.994839481491405,
0.99180331349328),(0.998122319569322,0.999023095875704,1.,0.994839481491405,
0.99180331349328)))
REPRESENTATION_ITEM('')
SURFACE()
);
#1894=(
BOUNDED_SURFACE()
B_SPLINE_SURFACE(1,2,((#126414,#126415,#126416,#126417,#126418),(#126419,
#126420,#126421,#126422,#126423)),.UNSPECIFIED.,.F.,.F.,.F.)
B_SPLINE_SURFACE_WITH_KNOTS((2,2),(3,2,3),(0.709731017441998,1.),(0.504616569534328,
0.521917529826141,0.522505428181611),.UNSPECIFIED.)
GEOMETRIC_REPRESENTATION_ITEM()
RATIONAL_B_SPLINE_SURFACE(((0.996968549833597,0.99168074676856,0.989334769731189,
0.989334769731189,0.989334769731189),(0.996968549833597,0.99168074676856,
0.989334769731189,0.989334769731189,0.989334769731189)))
REPRESENTATION_ITEM('')
SURFACE()
);
#1895=(
BOUNDED_SURFACE()
B_SPLINE_SURFACE(1,2,((#126434,#126435,#126436,#126437,#126438),(#126439,
#126440,#126441,#126442,#126443)),.UNSPECIFIED.,.F.,.F.,.F.)
B_SPLINE_SURFACE_WITH_KNOTS((2,2),(3,2,3),(0.710192959006837,1.),(0.211502584834064,
0.214285714285714,0.228987659635174),.UNSPECIFIED.)
GEOMETRIC_REPRESENTATION_ITEM()
RATIONAL_B_SPLINE_SURFACE(((0.998122319569322,0.999023095875704,1.,0.994839481491405,
0.99180331349328),(0.998122319569322,0.999023095875704,1.,0.994839481491405,
0.99180331349328)))
REPRESENTATION_ITEM('')
SURFACE()
);
#1896=(
BOUNDED_SURFACE()
B_SPLINE_SURFACE(1,2,((#126457,#126458,#126459,#126460,#126461),(#126462,
#126463,#126464,#126465,#126466)),.UNSPECIFIED.,.F.,.F.,.F.)
B_SPLINE_SURFACE_WITH_KNOTS((2,2),(3,2,3),(0.709731017396997,1.),(0.504616569534328,
0.521917529826141,0.522505428227195),.UNSPECIFIED.)
GEOMETRIC_REPRESENTATION_ITEM()
RATIONAL_B_SPLINE_SURFACE(((0.996968549833597,0.991680746768561,0.989334769731189,
0.989334769731189,0.989334769731189),(0.996968549833597,0.991680746768561,
0.989334769731189,0.989334769731189,0.989334769731189)))
REPRESENTATION_ITEM('')
SURFACE()
);
#1897=(
BOUNDED_SURFACE()
B_SPLINE_SURFACE(1,2,((#126477,#126478,#126479,#126480,#126481),(#126482,
#126483,#126484,#126485,#126486)),.UNSPECIFIED.,.F.,.F.,.F.)
B_SPLINE_SURFACE_WITH_KNOTS((2,2),(3,2,3),(0.710192959007424,1.),(0.211502584834064,
0.214285714285714,0.228987659635174),.UNSPECIFIED.)
GEOMETRIC_REPRESENTATION_ITEM()
RATIONAL_B_SPLINE_SURFACE(((0.998122319569322,0.999023095875704,1.,0.994839481491405,
0.99180331349328),(0.998122319569322,0.999023095875704,1.,0.994839481491405,
0.99180331349328)))
REPRESENTATION_ITEM('')
SURFACE()
);
#1898=(
BOUNDED_SURFACE()
B_SPLINE_SURFACE(1,2,((#126500,#126501,#126502,#126503,#126504),(#126505,
#126506,#126507,#126508,#126509)),.UNSPECIFIED.,.F.,.F.,.F.)
B_SPLINE_SURFACE_WITH_KNOTS((2,2),(3,2,3),(0.709731017376469,1.),(0.504616569534328,
0.521917529826141,0.522505428193485),.UNSPECIFIED.)
GEOMETRIC_REPRESENTATION_ITEM()
RATIONAL_B_SPLINE_SURFACE(((0.996968549833597,0.99168074676856,0.989334769731189,
0.989334769731189,0.989334769731189),(0.996968549833597,0.99168074676856,
0.989334769731189,0.989334769731189,0.989334769731189)))
REPRESENTATION_ITEM('')
SURFACE()
);
#1899=(
BOUNDED_SURFACE()
B_SPLINE_SURFACE(1,2,((#126520,#126521,#126522,#126523,#126524),(#126525,
#126526,#126527,#126528,#126529)),.UNSPECIFIED.,.F.,.F.,.F.)
B_SPLINE_SURFACE_WITH_KNOTS((2,2),(3,2,3),(0.710192959006924,1.),(0.211502584834064,
0.214285714285714,0.228987659635174),.UNSPECIFIED.)
GEOMETRIC_REPRESENTATION_ITEM()
RATIONAL_B_SPLINE_SURFACE(((0.998122319569322,0.999023095875704,1.,0.994839481491405,
0.99180331349328),(0.998122319569322,0.999023095875704,1.,0.994839481491405,
0.99180331349328)))
REPRESENTATION_ITEM('')
SURFACE()
);
#1900=(
BOUNDED_SURFACE()
B_SPLINE_SURFACE(1,2,((#126543,#126544,#126545,#126546,#126547),(#126548,
#126549,#126550,#126551,#126552)),.UNSPECIFIED.,.F.,.F.,.F.)
B_SPLINE_SURFACE_WITH_KNOTS((2,2),(3,2,3),(0.709731017436248,1.),(0.504616569534328,
0.521917529826141,0.522505428187947),.UNSPECIFIED.)
GEOMETRIC_REPRESENTATION_ITEM()
RATIONAL_B_SPLINE_SURFACE(((0.996968549833597,0.99168074676856,0.989334769731189,
0.989334769731189,0.989334769731189),(0.996968549833597,0.99168074676856,
0.989334769731189,0.989334769731189,0.989334769731189)))
REPRESENTATION_ITEM('')
SURFACE()
);
#1901=(
BOUNDED_SURFACE()
B_SPLINE_SURFACE(1,2,((#126563,#126564,#126565,#126566,#126567),(#126568,
#126569,#126570,#126571,#126572)),.UNSPECIFIED.,.F.,.F.,.F.)
B_SPLINE_SURFACE_WITH_KNOTS((2,2),(3,2,3),(0.710192959007417,1.),(0.211502584834064,
0.214285714285714,0.228987659635174),.UNSPECIFIED.)
GEOMETRIC_REPRESENTATION_ITEM()
RATIONAL_B_SPLINE_SURFACE(((0.998122319569322,0.999023095875704,1.,0.994839481491405,
0.99180331349328),(0.998122319569322,0.999023095875704,1.,0.994839481491405,
0.99180331349328)))
REPRESENTATION_ITEM('')
SURFACE()
);
#1902=(
BOUNDED_SURFACE()
B_SPLINE_SURFACE(1,2,((#126586,#126587,#126588,#126589,#126590),(#126591,
#126592,#126593,#126594,#126595)),.UNSPECIFIED.,.F.,.F.,.F.)
B_SPLINE_SURFACE_WITH_KNOTS((2,2),(3,2,3),(0.710318915638563,1.),(0.504616569534328,
0.521917529826141,0.522090539429059),.UNSPECIFIED.)
GEOMETRIC_REPRESENTATION_ITEM()
RATIONAL_B_SPLINE_SURFACE(((0.996968549833597,0.991680746768561,0.989334769731189,
0.989334769731189,0.989334769731189),(0.996968549833597,0.991680746768561,
0.989334769731189,0.989334769731189,0.989334769731189)))
REPRESENTATION_ITEM('')
SURFACE()
);
#1903=(
BOUNDED_SURFACE()
B_SPLINE_SURFACE(1,2,((#126606,#126607,#126608,#126609,#126610),(#126611,
#126612,#126613,#126614,#126615)),.UNSPECIFIED.,.F.,.F.,.F.)
B_SPLINE_SURFACE_WITH_KNOTS((2,2),(3,2,3),(0.710192959006919,1.),(0.211502584834064,
0.214285714285714,0.228987659635174),.UNSPECIFIED.)
GEOMETRIC_REPRESENTATION_ITEM()
RATIONAL_B_SPLINE_SURFACE(((0.998122319569322,0.999023095875704,1.,0.994839481491405,
0.99180331349328),(0.998122319569322,0.999023095875704,1.,0.994839481491405,
0.99180331349328)))
REPRESENTATION_ITEM('')
SURFACE()
);
#1904=(
BOUNDED_SURFACE()
B_SPLINE_SURFACE(1,2,((#126629,#126630,#126631,#126632,#126633),(#126634,
#126635,#126636,#126637,#126638)),.UNSPECIFIED.,.F.,.F.,.F.)
B_SPLINE_SURFACE_WITH_KNOTS((2,2),(3,2,3),(0.710318915638789,1.),(0.504616569534328,
0.521917529826141,0.522090539429059),.UNSPECIFIED.)
GEOMETRIC_REPRESENTATION_ITEM()
RATIONAL_B_SPLINE_SURFACE(((0.996968549833597,0.991680746768561,0.989334769731189,
0.989334769731189,0.989334769731189),(0.996968549833597,0.991680746768561,
0.989334769731189,0.989334769731189,0.989334769731189)))
REPRESENTATION_ITEM('')
SURFACE()
);
#1905=(
BOUNDED_SURFACE()
B_SPLINE_SURFACE(1,2,((#126649,#126650,#126651,#126652,#126653),(#126654,
#126655,#126656,#126657,#126658)),.UNSPECIFIED.,.F.,.F.,.F.)
B_SPLINE_SURFACE_WITH_KNOTS((2,2),(3,2,3),(0.710192959007146,1.),(0.211502584834064,
0.214285714285714,0.228987659635174),.UNSPECIFIED.)
GEOMETRIC_REPRESENTATION_ITEM()
RATIONAL_B_SPLINE_SURFACE(((0.998122319569322,0.999023095875704,1.,0.994839481491405,
0.99180331349328),(0.998122319569322,0.999023095875704,1.,0.994839481491405,
0.99180331349328)))
REPRESENTATION_ITEM('')
SURFACE()
);
#1906=(
BOUNDED_SURFACE()
B_SPLINE_SURFACE(1,2,((#126672,#126673,#126674,#126675,#126676),(#126677,
#126678,#126679,#126680,#126681)),.UNSPECIFIED.,.F.,.F.,.F.)
B_SPLINE_SURFACE_WITH_KNOTS((2,2),(3,2,3),(0.709731017416746,1.),(0.504616569534328,
0.521917529826141,0.522505428206132),.UNSPECIFIED.)
GEOMETRIC_REPRESENTATION_ITEM()
RATIONAL_B_SPLINE_SURFACE(((0.996968549833597,0.99168074676856,0.989334769731189,
0.989334769731189,0.989334769731189),(0.996968549833597,0.99168074676856,
0.989334769731189,0.989334769731189,0.989334769731189)))
REPRESENTATION_ITEM('')
SURFACE()
);
#1907=(
BOUNDED_SURFACE()
B_SPLINE_SURFACE(1,2,((#126692,#126693,#126694,#126695,#126696),(#126697,
#126698,#126699,#126700,#126701)),.UNSPECIFIED.,.F.,.F.,.F.)
B_SPLINE_SURFACE_WITH_KNOTS((2,2),(3,2,3),(0.710192959006101,1.),(0.211502584834064,
0.214285714285714,0.228987659635174),.UNSPECIFIED.)
GEOMETRIC_REPRESENTATION_ITEM()
RATIONAL_B_SPLINE_SURFACE(((0.998122319569322,0.999023095875704,1.,0.994839481491405,
0.99180331349328),(0.998122319569322,0.999023095875704,1.,0.994839481491405,
0.99180331349328)))
REPRESENTATION_ITEM('')
SURFACE()
);
#1908=(
BOUNDED_SURFACE()
B_SPLINE_SURFACE(1,2,((#126715,#126716,#126717,#126718,#126719),(#126720,
#126721,#126722,#126723,#126724)),.UNSPECIFIED.,.F.,.F.,.F.)
B_SPLINE_SURFACE_WITH_KNOTS((2,2),(3,2,3),(0.709731017422478,1.),(0.504616569534328,
0.521917529826141,0.522505428201685),.UNSPECIFIED.)
GEOMETRIC_REPRESENTATION_ITEM()
RATIONAL_B_SPLINE_SURFACE(((0.996968549833597,0.991680746768561,0.989334769731189,
0.989334769731189,0.989334769731189),(0.996968549833597,0.99168074676856,
0.989334769731189,0.989334769731189,0.989334769731189)))
REPRESENTATION_ITEM('')
SURFACE()
);
#1909=(
BOUNDED_SURFACE()
B_SPLINE_SURFACE(1,2,((#126735,#126736,#126737,#126738,#126739),(#126740,
#126741,#126742,#126743,#126744)),.UNSPECIFIED.,.F.,.F.,.F.)
B_SPLINE_SURFACE_WITH_KNOTS((2,2),(3,2,3),(0.710192959007388,1.),(0.211502584834062,
0.214285714285714,0.228987659635174),.UNSPECIFIED.)
GEOMETRIC_REPRESENTATION_ITEM()
RATIONAL_B_SPLINE_SURFACE(((0.998122319569321,0.999023095875703,1.,0.994839481491405,
0.99180331349328),(0.998122319569321,0.999023095875703,1.,0.994839481491405,
0.99180331349328)))
REPRESENTATION_ITEM('')
SURFACE()
);
#1910=(
BOUNDED_SURFACE()
B_SPLINE_SURFACE(1,2,((#126758,#126759,#126760,#126761,#126762),(#126763,
#126764,#126765,#126766,#126767)),.UNSPECIFIED.,.F.,.F.,.F.)
B_SPLINE_SURFACE_WITH_KNOTS((2,2),(3,2,3),(0.709731017390974,1.),(0.504616569534328,
0.521917529826141,0.522505428233296),.UNSPECIFIED.)
GEOMETRIC_REPRESENTATION_ITEM()
RATIONAL_B_SPLINE_SURFACE(((0.996968549833597,0.991680746768561,0.989334769731189,
0.989334769731189,0.989334769731189),(0.996968549833597,0.991680746768561,
0.989334769731189,0.989334769731189,0.989334769731189)))
REPRESENTATION_ITEM('')
SURFACE()
);
#1911=(
BOUNDED_SURFACE()
B_SPLINE_SURFACE(1,2,((#126778,#126779,#126780,#126781,#126782),(#126783,
#126784,#126785,#126786,#126787)),.UNSPECIFIED.,.F.,.F.,.F.)
B_SPLINE_SURFACE_WITH_KNOTS((2,2),(3,2,3),(0.710192959007501,1.),(0.211502584834064,
0.214285714285714,0.228987659635174),.UNSPECIFIED.)
GEOMETRIC_REPRESENTATION_ITEM()
RATIONAL_B_SPLINE_SURFACE(((0.998122319569322,0.999023095875704,1.,0.994839481491405,
0.99180331349328),(0.998122319569322,0.999023095875704,1.,0.994839481491405,
0.99180331349328)))
REPRESENTATION_ITEM('')
SURFACE()
);
#1912=(
BOUNDED_SURFACE()
B_SPLINE_SURFACE(1,2,((#126801,#126802,#126803,#126804,#126805),(#126806,
#126807,#126808,#126809,#126810)),.UNSPECIFIED.,.F.,.F.,.F.)
B_SPLINE_SURFACE_WITH_KNOTS((2,2),(3,2,3),(0.710318915638503,1.),(0.504616569534054,
0.521917529826142,0.522090539429063),.UNSPECIFIED.)
GEOMETRIC_REPRESENTATION_ITEM()
RATIONAL_B_SPLINE_SURFACE(((0.996968549833764,0.991680746768598,0.989334769731189,
0.989334769731189,0.989334769731189),(0.996968549833764,0.991680746768598,
0.989334769731189,0.989334769731189,0.989334769731189)))
REPRESENTATION_ITEM('')
SURFACE()
);
#1913=(
BOUNDED_SURFACE()
B_SPLINE_SURFACE(1,2,((#126821,#126822,#126823,#126824,#126825),(#126826,
#126827,#126828,#126829,#126830)),.UNSPECIFIED.,.F.,.F.,.F.)
B_SPLINE_SURFACE_WITH_KNOTS((2,2),(3,2,3),(0.710192959006864,1.),(0.211502584834064,
0.214285714285714,0.228987659635173),.UNSPECIFIED.)
GEOMETRIC_REPRESENTATION_ITEM()
RATIONAL_B_SPLINE_SURFACE(((0.998122319569322,0.999023095875704,1.,0.994839481491405,
0.99180331349328),(0.998122319569322,0.999023095875704,1.,0.994839481491405,
0.99180331349328)))
REPRESENTATION_ITEM('')
SURFACE()
);
#1914=(
BOUNDED_SURFACE()
B_SPLINE_SURFACE(1,2,((#126844,#126845,#126846,#126847,#126848),(#126849,
#126850,#126851,#126852,#126853)),.UNSPECIFIED.,.F.,.F.,.F.)
B_SPLINE_SURFACE_WITH_KNOTS((2,2),(3,2,3),(0.709731017406796,1.),(0.504616569534173,
0.521917529826141,0.522505428218247),.UNSPECIFIED.)
GEOMETRIC_REPRESENTATION_ITEM()
RATIONAL_B_SPLINE_SURFACE(((0.996968549833692,0.991680746768582,0.989334769731189,
0.989334769731189,0.989334769731189),(0.996968549833692,0.991680746768582,
0.989334769731189,0.989334769731189,0.989334769731189)))
REPRESENTATION_ITEM('')
SURFACE()
);
#1915=(
BOUNDED_SURFACE()
B_SPLINE_SURFACE(1,2,((#126864,#126865,#126866,#126867,#126868),(#126869,
#126870,#126871,#126872,#126873)),.UNSPECIFIED.,.F.,.F.,.F.)
B_SPLINE_SURFACE_WITH_KNOTS((2,2),(3,2,3),(0.710192959008269,1.),(0.211502584834063,
0.214285714285714,0.228987659635173),.UNSPECIFIED.)
GEOMETRIC_REPRESENTATION_ITEM()
RATIONAL_B_SPLINE_SURFACE(((0.998122319569321,0.999023095875704,1.,0.994839481491405,
0.99180331349328),(0.998122319569321,0.999023095875704,1.,0.994839481491405,
0.99180331349328)))
REPRESENTATION_ITEM('')
SURFACE()
);
#1916=(
BOUNDED_SURFACE()
B_SPLINE_SURFACE(1,2,((#126887,#126888,#126889,#126890,#126891),(#126892,
#126893,#126894,#126895,#126896)),.UNSPECIFIED.,.F.,.F.,.F.)
B_SPLINE_SURFACE_WITH_KNOTS((2,2),(3,2,3),(0.710318915638758,1.),(0.504616569533916,
0.521917529826141,0.522090539429063),.UNSPECIFIED.)
GEOMETRIC_REPRESENTATION_ITEM()
RATIONAL_B_SPLINE_SURFACE(((0.996968549833849,0.991680746768616,0.989334769731189,
0.989334769731189,0.989334769731189),(0.996968549833849,0.991680746768616,
0.989334769731189,0.989334769731189,0.989334769731189)))
REPRESENTATION_ITEM('')
SURFACE()
);
#1917=(
BOUNDED_SURFACE()
B_SPLINE_SURFACE(1,2,((#126907,#126908,#126909,#126910,#126911),(#126912,
#126913,#126914,#126915,#126916)),.UNSPECIFIED.,.F.,.F.,.F.)
B_SPLINE_SURFACE_WITH_KNOTS((2,2),(3,2,3),(0.710192959007119,1.),(0.21150258483406,
0.214285714285714,0.228987659635174),.UNSPECIFIED.)
GEOMETRIC_REPRESENTATION_ITEM()
RATIONAL_B_SPLINE_SURFACE(((0.998122319569319,0.999023095875703,1.,0.994839481491405,
0.99180331349328),(0.998122319569319,0.999023095875703,1.,0.994839481491405,
0.99180331349328)))
REPRESENTATION_ITEM('')
SURFACE()
);
#1918=(
BOUNDED_SURFACE()
B_SPLINE_SURFACE(1,2,((#126930,#126931,#126932,#126933,#126934),(#126935,
#126936,#126937,#126938,#126939)),.UNSPECIFIED.,.F.,.F.,.F.)
B_SPLINE_SURFACE_WITH_KNOTS((2,2),(3,2,3),(0.710053410952874,1.),(0.504616569534023,
0.521917529826142,0.522183034673918),.UNSPECIFIED.)
GEOMETRIC_REPRESENTATION_ITEM()
RATIONAL_B_SPLINE_SURFACE(((0.996968549833783,0.991680746768602,0.989334769731188,
0.989334769731188,0.989334769731188),(0.996968549833783,0.991680746768602,
0.989334769731188,0.989334769731188,0.989334769731188)))
REPRESENTATION_ITEM('')
SURFACE()
);
#1919=(
BOUNDED_SURFACE()
B_SPLINE_SURFACE(1,2,((#126947,#126948,#126949,#126950,#126951),(#126952,
#126953,#126954,#126955,#126956)),.UNSPECIFIED.,.F.,.F.,.F.)
B_SPLINE_SURFACE_WITH_KNOTS((2,2),(3,2,3),(0.710192959007306,1.),(0.211502584834064,
0.214285714285714,0.228987659635173),.UNSPECIFIED.)
GEOMETRIC_REPRESENTATION_ITEM()
RATIONAL_B_SPLINE_SURFACE(((0.998122319569322,0.999023095875704,1.,0.994839481491405,
0.99180331349328),(0.998122319569322,0.999023095875704,1.,0.994839481491405,
0.99180331349328)))
REPRESENTATION_ITEM('')
SURFACE()
);
#1920=(
BOUNDED_SURFACE()
B_SPLINE_SURFACE(1,2,((#126958,#126959,#126960,#126961,#126962),(#126963,
#126964,#126965,#126966,#126967)),.UNSPECIFIED.,.F.,.F.,.F.)
B_SPLINE_SURFACE_WITH_KNOTS((2,2),(3,2,3),(0.709731017417456,1.),(0.504616569533889,
0.521917529826142,0.522505428205581),.UNSPECIFIED.)
GEOMETRIC_REPRESENTATION_ITEM()
RATIONAL_B_SPLINE_SURFACE(((0.996968549833865,0.99168074676862,0.989334769731189,
0.989334769731189,0.989334769731189),(0.996968549833865,0.99168074676862,
0.989334769731189,0.989334769731189,0.989334769731189)))
REPRESENTATION_ITEM('')
SURFACE()
);
#1921=(
BOUNDED_SURFACE()
B_SPLINE_SURFACE(1,2,((#126978,#126979,#126980,#126981,#126982),(#126983,
#126984,#126985,#126986,#126987)),.UNSPECIFIED.,.F.,.F.,.F.)
B_SPLINE_SURFACE_WITH_KNOTS((2,2),(3,2,3),(0.710192959006265,1.),(0.211502584834064,
0.214285714285714,0.228987659635021),.UNSPECIFIED.)
GEOMETRIC_REPRESENTATION_ITEM()
RATIONAL_B_SPLINE_SURFACE(((0.998122319569322,0.999023095875704,1.,0.994839481491458,
0.991803313493343),(0.998122319569322,0.999023095875704,1.,0.994839481491458,
0.991803313493343)))
REPRESENTATION_ITEM('')
SURFACE()
);
#1922=(
BOUNDED_SURFACE()
B_SPLINE_SURFACE(1,2,((#127001,#127002,#127003,#127004,#127005),(#127006,
#127007,#127008,#127009,#127010)),.UNSPECIFIED.,.F.,.F.,.F.)
B_SPLINE_SURFACE_WITH_KNOTS((2,2),(3,2,3),(0.709731017421646,1.),(0.504616569534085,
0.521917529826141,0.522505428203218),.UNSPECIFIED.)
GEOMETRIC_REPRESENTATION_ITEM()
RATIONAL_B_SPLINE_SURFACE(((0.996968549833745,0.991680746768594,0.989334769731189,
0.989334769731189,0.989334769731189),(0.996968549833745,0.991680746768594,
0.989334769731189,0.989334769731189,0.989334769731189)))
REPRESENTATION_ITEM('')
SURFACE()
);
#1923=(
BOUNDED_SURFACE()
B_SPLINE_SURFACE(1,2,((#127021,#127022,#127023,#127024,#127025),(#127026,
#127027,#127028,#127029,#127030)),.UNSPECIFIED.,.F.,.F.,.F.)
B_SPLINE_SURFACE_WITH_KNOTS((2,2),(3,2,3),(0.710192959008099,1.),(0.211502584834064,
0.214285714285714,0.228987659635071),.UNSPECIFIED.)
GEOMETRIC_REPRESENTATION_ITEM()
RATIONAL_B_SPLINE_SURFACE(((0.998122319569322,0.999023095875704,1.,0.994839481491441,
0.991803313493322),(0.998122319569322,0.999023095875704,1.,0.994839481491441,
0.991803313493322)))
REPRESENTATION_ITEM('')
SURFACE()
);
#1924=(
BOUNDED_SURFACE()
B_SPLINE_SURFACE(1,2,((#127044,#127045,#127046,#127047,#127048),(#127049,
#127050,#127051,#127052,#127053)),.UNSPECIFIED.,.F.,.F.,.F.)
B_SPLINE_SURFACE_WITH_KNOTS((2,2),(3,2,3),(0.709731017417918,1.),(0.504616569534229,
0.521917529826141,0.522505428205796),.UNSPECIFIED.)
GEOMETRIC_REPRESENTATION_ITEM()
RATIONAL_B_SPLINE_SURFACE(((0.996968549833657,0.991680746768574,0.989334769731189,
0.989334769731189,0.989334769731189),(0.996968549833657,0.991680746768574,
0.989334769731189,0.989334769731189,0.989334769731189)))
REPRESENTATION_ITEM('')
SURFACE()
);
#1925=(
BOUNDED_SURFACE()
B_SPLINE_SURFACE(1,2,((#127064,#127065,#127066,#127067,#127068),(#127069,
#127070,#127071,#127072,#127073)),.UNSPECIFIED.,.F.,.F.,.F.)
B_SPLINE_SURFACE_WITH_KNOTS((2,2),(3,2,3),(0.710192959006948,1.),(0.211502584834064,
0.214285714285714,0.228987659635144),.UNSPECIFIED.)
GEOMETRIC_REPRESENTATION_ITEM()
RATIONAL_B_SPLINE_SURFACE(((0.998122319569322,0.999023095875704,1.,0.994839481491415,
0.991803313493292),(0.998122319569322,0.999023095875704,1.,0.994839481491415,
0.991803313493292)))
REPRESENTATION_ITEM('')
SURFACE()
);
#1926=(
BOUNDED_SURFACE()
B_SPLINE_SURFACE(1,2,((#127087,#127088,#127089,#127090,#127091),(#127092,
#127093,#127094,#127095,#127096)),.UNSPECIFIED.,.F.,.F.,.F.)
B_SPLINE_SURFACE_WITH_KNOTS((2,2),(3,2,3),(0.709731017397925,1.),(0.504616569534201,
0.521917529826141,0.522505428226044),.UNSPECIFIED.)
GEOMETRIC_REPRESENTATION_ITEM()
RATIONAL_B_SPLINE_SURFACE(((0.996968549833674,0.991680746768578,0.989334769731189,
0.989334769731189,0.989334769731189),(0.996968549833674,0.991680746768578,
0.989334769731189,0.989334769731189,0.989334769731189)))
REPRESENTATION_ITEM('')
SURFACE()
);
#1927=(
BOUNDED_SURFACE()
B_SPLINE_SURFACE(1,2,((#127107,#127108,#127109,#127110,#127111),(#127112,
#127113,#127114,#127115,#127116)),.UNSPECIFIED.,.F.,.F.,.F.)
B_SPLINE_SURFACE_WITH_KNOTS((2,2),(3,2,3),(0.710192959007196,1.),(0.211502584834064,
0.214285714285714,0.228987659635168),.UNSPECIFIED.)
GEOMETRIC_REPRESENTATION_ITEM()
RATIONAL_B_SPLINE_SURFACE(((0.998122319569322,0.999023095875704,1.,0.994839481491406,
0.991803313493282),(0.998122319569322,0.999023095875704,1.,0.994839481491406,
0.991803313493282)))
REPRESENTATION_ITEM('')
SURFACE()
);
#1928=(
BOUNDED_SURFACE()
B_SPLINE_SURFACE(1,2,((#127130,#127131,#127132,#127133,#127134),(#127135,
#127136,#127137,#127138,#127139)),.UNSPECIFIED.,.F.,.F.,.F.)
B_SPLINE_SURFACE_WITH_KNOTS((2,2),(3,2,3),(0.709731017432417,1.),(0.504616569534328,
0.521917529826141,0.522505428191805),.UNSPECIFIED.)
GEOMETRIC_REPRESENTATION_ITEM()
RATIONAL_B_SPLINE_SURFACE(((0.996968549833597,0.99168074676856,0.989334769731189,
0.989334769731189,0.989334769731189),(0.996968549833597,0.99168074676856,
0.989334769731189,0.989334769731189,0.989334769731189)))
REPRESENTATION_ITEM('')
SURFACE()
);
#1929=(
BOUNDED_SURFACE()
B_SPLINE_SURFACE(1,2,((#127150,#127151,#127152,#127153,#127154),(#127155,
#127156,#127157,#127158,#127159)),.UNSPECIFIED.,.F.,.F.,.F.)
B_SPLINE_SURFACE_WITH_KNOTS((2,2),(3,2,3),(0.710192959006417,1.),(0.211502584834052,
0.214285714285714,0.228987659635174),.UNSPECIFIED.)
GEOMETRIC_REPRESENTATION_ITEM()
RATIONAL_B_SPLINE_SURFACE(((0.998122319569314,0.9990230958757,1.,0.994839481491405,
0.99180331349328),(0.998122319569314,0.9990230958757,1.,0.994839481491405,
0.99180331349328)))
REPRESENTATION_ITEM('')
SURFACE()
);
#1930=(
BOUNDED_SURFACE()
B_SPLINE_SURFACE(1,2,((#127173,#127174,#127175,#127176,#127177),(#127178,
#127179,#127180,#127181,#127182)),.UNSPECIFIED.,.F.,.F.,.F.)
B_SPLINE_SURFACE_WITH_KNOTS((2,2),(3,2,3),(0.710318915639158,1.),(0.504616569534302,
0.521917529826141,0.52209053942906),.UNSPECIFIED.)
GEOMETRIC_REPRESENTATION_ITEM()
RATIONAL_B_SPLINE_SURFACE(((0.996968549833613,0.991680746768564,0.989334769731189,
0.989334769731189,0.989334769731189),(0.996968549833613,0.991680746768564,
0.989334769731189,0.989334769731189,0.989334769731189)))
REPRESENTATION_ITEM('')
SURFACE()
);
#1931=(
BOUNDED_SURFACE()
B_SPLINE_SURFACE(1,2,((#127193,#127194,#127195,#127196,#127197),(#127198,
#127199,#127200,#127201,#127202)),.UNSPECIFIED.,.F.,.F.,.F.)
B_SPLINE_SURFACE_WITH_KNOTS((2,2),(3,2,3),(0.710192959007516,1.),(0.211502584834065,
0.214285714285714,0.228987659635173),.UNSPECIFIED.)
GEOMETRIC_REPRESENTATION_ITEM()
RATIONAL_B_SPLINE_SURFACE(((0.998122319569323,0.999023095875705,1.,0.994839481491405,
0.99180331349328),(0.998122319569323,0.999023095875705,1.,0.994839481491405,
0.99180331349328)))
REPRESENTATION_ITEM('')
SURFACE()
);
#1932=(
BOUNDED_SURFACE()
B_SPLINE_SURFACE(1,2,((#127216,#127217,#127218,#127219,#127220),(#127221,
#127222,#127223,#127224,#127225)),.UNSPECIFIED.,.F.,.F.,.F.)
B_SPLINE_SURFACE_WITH_KNOTS((2,2),(3,2,3),(0.710318915640079,1.),(0.504616569534327,
0.52191752982614,0.522090539429058),.UNSPECIFIED.)
GEOMETRIC_REPRESENTATION_ITEM()
RATIONAL_B_SPLINE_SURFACE(((0.996968549833597,0.991680746768561,0.989334769731189,
0.989334769731189,0.989334769731189),(0.996968549833597,0.991680746768561,
0.989334769731189,0.989334769731189,0.989334769731189)))
REPRESENTATION_ITEM('')
SURFACE()
);
#1933=(
BOUNDED_SURFACE()
B_SPLINE_SURFACE(1,2,((#127236,#127237,#127238,#127239,#127240),(#127241,
#127242,#127243,#127244,#127245)),.UNSPECIFIED.,.F.,.F.,.F.)
B_SPLINE_SURFACE_WITH_KNOTS((2,2),(3,2,3),(0.710192959008445,1.),(0.211502584834065,
0.214285714285714,0.228987659635175),.UNSPECIFIED.)
GEOMETRIC_REPRESENTATION_ITEM()
RATIONAL_B_SPLINE_SURFACE(((0.998122319569323,0.999023095875705,1.,0.994839481491404,
0.99180331349328),(0.998122319569323,0.999023095875705,1.,0.994839481491404,
0.99180331349328)))
REPRESENTATION_ITEM('')
SURFACE()
);
#1934=(
BOUNDED_SURFACE()
B_SPLINE_SURFACE(1,2,((#127259,#127260,#127261,#127262,#127263),(#127264,
#127265,#127266,#127267,#127268)),.UNSPECIFIED.,.F.,.F.,.F.)
B_SPLINE_SURFACE_WITH_KNOTS((2,2),(3,2,3),(0.709595573560721,1.),(0.469422374511333,
0.470019760166364,0.48736334072649),.UNSPECIFIED.)
GEOMETRIC_REPRESENTATION_ITEM()
RATIONAL_B_SPLINE_SURFACE(((0.987787102172814,0.987787102172814,0.987787102172814,
0.988764511531023,0.992698258926488),(0.987787102172814,0.987787102172814,
0.987787102172814,0.988764511531023,0.992698258926488)))
REPRESENTATION_ITEM('')
SURFACE()
);
#1935=(
BOUNDED_SURFACE()
B_SPLINE_SURFACE(1,2,((#127277,#127278,#127279),(#127280,#127281,#127282)),
 .UNSPECIFIED.,.F.,.F.,.F.)
B_SPLINE_SURFACE_WITH_KNOTS((2,2),(3,3),(0.710318915640071,1.),(0.24585118339369,
0.263098999273796),.UNSPECIFIED.)
GEOMETRIC_REPRESENTATION_ITEM()
RATIONAL_B_SPLINE_SURFACE(((0.987633126750594,0.986929835989062,0.989150325841653),
(0.987633126750594,0.986929835989062,0.989150325841653)))
REPRESENTATION_ITEM('')
SURFACE()
);
#1936=(
BOUNDED_SURFACE()
B_SPLINE_SURFACE(1,2,((#127284,#127285,#127286,#127287,#127288),(#127289,
#127290,#127291,#127292,#127293)),.UNSPECIFIED.,.F.,.F.,.F.)
B_SPLINE_SURFACE_WITH_KNOTS((2,2),(3,2,3),(0.709595573563224,1.),(0.469422374513835,
0.470019760166364,0.48736334072649),.UNSPECIFIED.)
GEOMETRIC_REPRESENTATION_ITEM()
RATIONAL_B_SPLINE_SURFACE(((0.987787102172814,0.987787102172814,0.987787102172814,
0.988764511531023,0.992698258926488),(0.987787102172814,0.987787102172814,
0.987787102172814,0.988764511531023,0.992698258926488)))
REPRESENTATION_ITEM('')
SURFACE()
);
#1937=(
BOUNDED_SURFACE()
B_SPLINE_SURFACE(1,2,((#127302,#127303,#127304),(#127305,#127306,#127307)),
 .UNSPECIFIED.,.F.,.F.,.F.)
B_SPLINE_SURFACE_WITH_KNOTS((2,2),(3,3),(0.710318915640084,1.),(0.24585118339369,
0.263098999273796),.UNSPECIFIED.)
GEOMETRIC_REPRESENTATION_ITEM()
RATIONAL_B_SPLINE_SURFACE(((0.987633126750594,0.986929835989062,0.989150325841653),
(0.987633126750594,0.986929835989062,0.989150325841653)))
REPRESENTATION_ITEM('')
SURFACE()
);
#1938=(
BOUNDED_SURFACE()
B_SPLINE_SURFACE(1,2,((#127309,#127310,#127311,#127312,#127313),(#127314,
#127315,#127316,#127317,#127318)),.UNSPECIFIED.,.F.,.F.,.F.)
B_SPLINE_SURFACE_WITH_KNOTS((2,2),(3,2,3),(0.709595573570259,1.),(0.46942237452087,
0.470019760166364,0.48736334072649),.UNSPECIFIED.)
GEOMETRIC_REPRESENTATION_ITEM()
RATIONAL_B_SPLINE_SURFACE(((0.987787102172814,0.987787102172814,0.987787102172814,
0.988764511531023,0.992698258926488),(0.987787102172814,0.987787102172814,
0.987787102172814,0.988764511531023,0.992698258926488)))
REPRESENTATION_ITEM('')
SURFACE()
);
#1939=(
BOUNDED_SURFACE()
B_SPLINE_SURFACE(1,2,((#127327,#127328,#127329),(#127330,#127331,#127332)),
 .UNSPECIFIED.,.F.,.F.,.F.)
B_SPLINE_SURFACE_WITH_KNOTS((2,2),(3,3),(0.710318915640074,1.),(0.24585118339369,
0.263098999273796),.UNSPECIFIED.)
GEOMETRIC_REPRESENTATION_ITEM()
RATIONAL_B_SPLINE_SURFACE(((0.987633126750594,0.986929835989062,0.989150325841653),
(0.987633126750594,0.986929835989062,0.989150325841653)))
REPRESENTATION_ITEM('')
SURFACE()
);
#1940=(
BOUNDED_SURFACE()
B_SPLINE_SURFACE(1,2,((#127334,#127335,#127336,#127337,#127338),(#127339,
#127340,#127341,#127342,#127343)),.UNSPECIFIED.,.F.,.F.,.F.)
B_SPLINE_SURFACE_WITH_KNOTS((2,2),(3,2,3),(0.709595573576442,1.),(0.469422374527051,
0.470019760166364,0.48736334072649),.UNSPECIFIED.)
GEOMETRIC_REPRESENTATION_ITEM()
RATIONAL_B_SPLINE_SURFACE(((0.987787102172814,0.987787102172814,0.987787102172814,
0.988764511531023,0.992698258926488),(0.987787102172814,0.987787102172814,
0.987787102172814,0.988764511531023,0.992698258926488)))
REPRESENTATION_ITEM('')
SURFACE()
);
#1941=(
BOUNDED_SURFACE()
B_SPLINE_SURFACE(1,2,((#127352,#127353,#127354),(#127355,#127356,#127357)),
 .UNSPECIFIED.,.F.,.F.,.F.)
B_SPLINE_SURFACE_WITH_KNOTS((2,2),(3,3),(0.710318915640077,1.),(0.24585118339369,
0.263098999273796),.UNSPECIFIED.)
GEOMETRIC_REPRESENTATION_ITEM()
RATIONAL_B_SPLINE_SURFACE(((0.987633126750594,0.986929835989062,0.989150325841653),
(0.987633126750594,0.986929835989062,0.989150325841653)))
REPRESENTATION_ITEM('')
SURFACE()
);
#1942=(
BOUNDED_SURFACE()
B_SPLINE_SURFACE(1,2,((#127359,#127360,#127361,#127362,#127363),(#127364,
#127365,#127366,#127367,#127368)),.UNSPECIFIED.,.F.,.F.,.F.)
B_SPLINE_SURFACE_WITH_KNOTS((2,2),(3,2,3),(0.709595573604623,1.),(0.469422374555238,
0.470019760166364,0.48736334072649),.UNSPECIFIED.)
GEOMETRIC_REPRESENTATION_ITEM()
RATIONAL_B_SPLINE_SURFACE(((0.987787102172814,0.987787102172814,0.987787102172814,
0.988764511531023,0.992698258926488),(0.987787102172814,0.987787102172814,
0.987787102172814,0.988764511531023,0.992698258926488)))
REPRESENTATION_ITEM('')
SURFACE()
);
#1943=(
BOUNDED_SURFACE()
B_SPLINE_SURFACE(1,2,((#127377,#127378,#127379),(#127380,#127381,#127382)),
 .UNSPECIFIED.,.F.,.F.,.F.)
B_SPLINE_SURFACE_WITH_KNOTS((2,2),(3,3),(0.710318915640083,1.),(0.24585118339369,
0.263098999273796),.UNSPECIFIED.)
GEOMETRIC_REPRESENTATION_ITEM()
RATIONAL_B_SPLINE_SURFACE(((0.987633126750594,0.986929835989062,0.989150325841653),
(0.987633126750594,0.986929835989062,0.989150325841653)))
REPRESENTATION_ITEM('')
SURFACE()
);
#1944=(
BOUNDED_SURFACE()
B_SPLINE_SURFACE(1,2,((#127384,#127385,#127386,#127387,#127388),(#127389,
#127390,#127391,#127392,#127393)),.UNSPECIFIED.,.F.,.F.,.F.)
B_SPLINE_SURFACE_WITH_KNOTS((2,2),(3,2,3),(0.709595573593217,1.),(0.469422374543823,
0.470019760166364,0.48736334072649),.UNSPECIFIED.)
GEOMETRIC_REPRESENTATION_ITEM()
RATIONAL_B_SPLINE_SURFACE(((0.987787102172814,0.987787102172814,0.987787102172814,
0.988764511531023,0.992698258926488),(0.987787102172814,0.987787102172814,
0.987787102172814,0.988764511531023,0.992698258926488)))
REPRESENTATION_ITEM('')
SURFACE()
);
#1945=(
BOUNDED_SURFACE()
B_SPLINE_SURFACE(1,2,((#127402,#127403,#127404),(#127405,#127406,#127407)),
 .UNSPECIFIED.,.F.,.F.,.F.)
B_SPLINE_SURFACE_WITH_KNOTS((2,2),(3,3),(0.710318915640078,1.),(0.24585118339369,
0.263098999273796),.UNSPECIFIED.)
GEOMETRIC_REPRESENTATION_ITEM()
RATIONAL_B_SPLINE_SURFACE(((0.987633126750594,0.986929835989062,0.989150325841653),
(0.987633126750594,0.986929835989062,0.989150325841653)))
REPRESENTATION_ITEM('')
SURFACE()
);
#1946=(
BOUNDED_SURFACE()
B_SPLINE_SURFACE(1,2,((#127409,#127410,#127411,#127412,#127413),(#127414,
#127415,#127416,#127417,#127418)),.UNSPECIFIED.,.F.,.F.,.F.)
B_SPLINE_SURFACE_WITH_KNOTS((2,2),(3,2,3),(0.70959557358438,1.),(0.469422374534986,
0.470019760166364,0.48736334072649),.UNSPECIFIED.)
GEOMETRIC_REPRESENTATION_ITEM()
RATIONAL_B_SPLINE_SURFACE(((0.987787102172814,0.987787102172814,0.987787102172814,
0.988764511531023,0.992698258926488),(0.987787102172814,0.987787102172814,
0.987787102172814,0.988764511531023,0.992698258926488)))
REPRESENTATION_ITEM('')
SURFACE()
);
#1947=(
BOUNDED_SURFACE()
B_SPLINE_SURFACE(1,2,((#127427,#127428,#127429),(#127430,#127431,#127432)),
 .UNSPECIFIED.,.F.,.F.,.F.)
B_SPLINE_SURFACE_WITH_KNOTS((2,2),(3,3),(0.710318915640084,1.),(0.24585118339369,
0.263098999273796),.UNSPECIFIED.)
GEOMETRIC_REPRESENTATION_ITEM()
RATIONAL_B_SPLINE_SURFACE(((0.987633126750594,0.986929835989062,0.989150325841653),
(0.987633126750594,0.986929835989062,0.989150325841653)))
REPRESENTATION_ITEM('')
SURFACE()
);
#1948=(
BOUNDED_SURFACE()
B_SPLINE_SURFACE(1,2,((#127434,#127435,#127436,#127437,#127438),(#127439,
#127440,#127441,#127442,#127443)),.UNSPECIFIED.,.F.,.F.,.F.)
B_SPLINE_SURFACE_WITH_KNOTS((2,2),(3,2,3),(0.709595573589852,1.),(0.469422374540461,
0.470019760166364,0.48736334072649),.UNSPECIFIED.)
GEOMETRIC_REPRESENTATION_ITEM()
RATIONAL_B_SPLINE_SURFACE(((0.987787102172814,0.987787102172814,0.987787102172814,
0.988764511531023,0.992698258926488),(0.987787102172814,0.987787102172814,
0.987787102172814,0.988764511531023,0.992698258926488)))
REPRESENTATION_ITEM('')
SURFACE()
);
#1949=(
BOUNDED_SURFACE()
B_SPLINE_SURFACE(1,2,((#127452,#127453,#127454),(#127455,#127456,#127457)),
 .UNSPECIFIED.,.F.,.F.,.F.)
B_SPLINE_SURFACE_WITH_KNOTS((2,2),(3,3),(0.710318915640076,1.),(0.24585118339369,
0.263098999273796),.UNSPECIFIED.)
GEOMETRIC_REPRESENTATION_ITEM()
RATIONAL_B_SPLINE_SURFACE(((0.987633126750594,0.986929835989062,0.989150325841653),
(0.987633126750594,0.986929835989062,0.989150325841653)))
REPRESENTATION_ITEM('')
SURFACE()
);
#1950=(
BOUNDED_SURFACE()
B_SPLINE_SURFACE(1,2,((#127459,#127460,#127461,#127462,#127463),(#127464,
#127465,#127466,#127467,#127468)),.UNSPECIFIED.,.F.,.F.,.F.)
B_SPLINE_SURFACE_WITH_KNOTS((2,2),(3,2,3),(0.709595573559204,1.),(0.469422374509813,
0.470019760166364,0.48736334072649),.UNSPECIFIED.)
GEOMETRIC_REPRESENTATION_ITEM()
RATIONAL_B_SPLINE_SURFACE(((0.987787102172814,0.987787102172814,0.987787102172814,
0.988764511531023,0.992698258926488),(0.987787102172814,0.987787102172814,
0.987787102172814,0.988764511531023,0.992698258926488)))
REPRESENTATION_ITEM('')
SURFACE()
);
#1951=(
BOUNDED_SURFACE()
B_SPLINE_SURFACE(1,2,((#127477,#127478,#127479),(#127480,#127481,#127482)),
 .UNSPECIFIED.,.F.,.F.,.F.)
B_SPLINE_SURFACE_WITH_KNOTS((2,2),(3,3),(0.710318915640081,1.),(0.24585118339369,
0.263098999273796),.UNSPECIFIED.)
GEOMETRIC_REPRESENTATION_ITEM()
RATIONAL_B_SPLINE_SURFACE(((0.987633126750594,0.986929835989062,0.989150325841653),
(0.987633126750594,0.986929835989062,0.989150325841653)))
REPRESENTATION_ITEM('')
SURFACE()
);
#1952=(
BOUNDED_SURFACE()
B_SPLINE_SURFACE(1,2,((#127484,#127485,#127486,#127487,#127488),(#127489,
#127490,#127491,#127492,#127493)),.UNSPECIFIED.,.F.,.F.,.F.)
B_SPLINE_SURFACE_WITH_KNOTS((2,2),(3,2,3),(0.709595573594376,1.),(0.469422374544989,
0.470019760166364,0.48736334072649),.UNSPECIFIED.)
GEOMETRIC_REPRESENTATION_ITEM()
RATIONAL_B_SPLINE_SURFACE(((0.987787102172814,0.987787102172814,0.987787102172814,
0.988764511531023,0.992698258926488),(0.987787102172814,0.987787102172814,
0.987787102172814,0.988764511531023,0.992698258926488)))
REPRESENTATION_ITEM('')
SURFACE()
);
#1953=(
BOUNDED_SURFACE()
B_SPLINE_SURFACE(1,2,((#127502,#127503,#127504),(#127505,#127506,#127507)),
 .UNSPECIFIED.,.F.,.F.,.F.)
B_SPLINE_SURFACE_WITH_KNOTS((2,2),(3,3),(0.710318915640075,1.),(0.24585118339369,
0.263098999273938),.UNSPECIFIED.)
GEOMETRIC_REPRESENTATION_ITEM()
RATIONAL_B_SPLINE_SURFACE(((0.987633126750594,0.986929835989056,0.989150325841689),
(0.987633126750594,0.986929835989056,0.989150325841689)))
REPRESENTATION_ITEM('')
SURFACE()
);
#1954=(
BOUNDED_SURFACE()
B_SPLINE_SURFACE(1,2,((#127509,#127510,#127511,#127512,#127513),(#127514,
#127515,#127516,#127517,#127518)),.UNSPECIFIED.,.F.,.F.,.F.)
B_SPLINE_SURFACE_WITH_KNOTS((2,2),(3,2,3),(0.709595573559938,1.),(0.469422374510549,
0.470019760166367,0.48736334072649),.UNSPECIFIED.)
GEOMETRIC_REPRESENTATION_ITEM()
RATIONAL_B_SPLINE_SURFACE(((0.987787102172814,0.987787102172814,0.987787102172814,
0.988764511531024,0.992698258926488),(0.987787102172814,0.987787102172814,
0.987787102172814,0.988764511531024,0.992698258926488)))
REPRESENTATION_ITEM('')
SURFACE()
);
#1955=(
BOUNDED_SURFACE()
B_SPLINE_SURFACE(1,2,((#127527,#127528,#127529),(#127530,#127531,#127532)),
 .UNSPECIFIED.,.F.,.F.,.F.)
B_SPLINE_SURFACE_WITH_KNOTS((2,2),(3,3),(0.710318915640069,1.),(0.24585118339369,
0.263098999273938),.UNSPECIFIED.)
GEOMETRIC_REPRESENTATION_ITEM()
RATIONAL_B_SPLINE_SURFACE(((0.987633126750594,0.986929835989056,0.98915032584169),
(0.987633126750594,0.986929835989056,0.98915032584169)))
REPRESENTATION_ITEM('')
SURFACE()
);
#1956=(
BOUNDED_SURFACE()
B_SPLINE_SURFACE(1,2,((#127534,#127535,#127536,#127537,#127538),(#127539,
#127540,#127541,#127542,#127543)),.UNSPECIFIED.,.F.,.F.,.F.)
B_SPLINE_SURFACE_WITH_KNOTS((2,2),(3,2,3),(0.70959557357981,1.),(0.469422374530418,
0.470019760166367,0.48736334072649),.UNSPECIFIED.)
GEOMETRIC_REPRESENTATION_ITEM()
RATIONAL_B_SPLINE_SURFACE(((0.987787102172814,0.987787102172814,0.987787102172814,
0.988764511531024,0.992698258926488),(0.987787102172814,0.987787102172814,
0.987787102172814,0.988764511531024,0.992698258926488)))
REPRESENTATION_ITEM('')
SURFACE()
);
#1957=(
BOUNDED_SURFACE()
B_SPLINE_SURFACE(1,2,((#127552,#127553,#127554),(#127555,#127556,#127557)),
 .UNSPECIFIED.,.F.,.F.,.F.)
B_SPLINE_SURFACE_WITH_KNOTS((2,2),(3,3),(0.710318915640074,1.),(0.24585118339369,
0.263098999273937),.UNSPECIFIED.)
GEOMETRIC_REPRESENTATION_ITEM()
RATIONAL_B_SPLINE_SURFACE(((0.987633126750594,0.986929835989056,0.989150325841689),
(0.987633126750594,0.986929835989056,0.989150325841689)))
REPRESENTATION_ITEM('')
SURFACE()
);
#1958=(
BOUNDED_SURFACE()
B_SPLINE_SURFACE(1,2,((#127559,#127560,#127561,#127562,#127563),(#127564,
#127565,#127566,#127567,#127568)),.UNSPECIFIED.,.F.,.F.,.F.)
B_SPLINE_SURFACE_WITH_KNOTS((2,2),(3,2,3),(0.709595573595216,1.),(0.469422374545822,
0.470019760166364,0.48736334072649),.UNSPECIFIED.)
GEOMETRIC_REPRESENTATION_ITEM()
RATIONAL_B_SPLINE_SURFACE(((0.987787102172814,0.987787102172814,0.987787102172814,
0.988764511531023,0.992698258926488),(0.987787102172814,0.987787102172814,
0.987787102172814,0.988764511531023,0.992698258926488)))
REPRESENTATION_ITEM('')
SURFACE()
);
#1959=(
BOUNDED_SURFACE()
B_SPLINE_SURFACE(1,2,((#127577,#127578,#127579),(#127580,#127581,#127582)),
 .UNSPECIFIED.,.F.,.F.,.F.)
B_SPLINE_SURFACE_WITH_KNOTS((2,2),(3,3),(0.710318915640078,1.),(0.24585118339369,
0.263098999273938),.UNSPECIFIED.)
GEOMETRIC_REPRESENTATION_ITEM()
RATIONAL_B_SPLINE_SURFACE(((0.987633126750594,0.986929835989056,0.98915032584169),
(0.987633126750594,0.986929835989056,0.98915032584169)))
REPRESENTATION_ITEM('')
SURFACE()
);
#1960=(
BOUNDED_SURFACE()
B_SPLINE_SURFACE(1,2,((#127584,#127585,#127586,#127587,#127588),(#127589,
#127590,#127591,#127592,#127593)),.UNSPECIFIED.,.F.,.F.,.F.)
B_SPLINE_SURFACE_WITH_KNOTS((2,2),(3,2,3),(0.709595573583186,1.),(0.469422374533795,
0.470019760166364,0.48736334072649),.UNSPECIFIED.)
GEOMETRIC_REPRESENTATION_ITEM()
RATIONAL_B_SPLINE_SURFACE(((0.987787102172814,0.987787102172814,0.987787102172814,
0.988764511531023,0.992698258926488),(0.987787102172814,0.987787102172814,
0.987787102172814,0.988764511531023,0.992698258926488)))
REPRESENTATION_ITEM('')
SURFACE()
);
#1961=(
BOUNDED_SURFACE()
B_SPLINE_SURFACE(1,2,((#127602,#127603,#127604),(#127605,#127606,#127607)),
 .UNSPECIFIED.,.F.,.F.,.F.)
B_SPLINE_SURFACE_WITH_KNOTS((2,2),(3,3),(0.710318915640077,1.),(0.24585118339369,
0.263098999273938),.UNSPECIFIED.)
GEOMETRIC_REPRESENTATION_ITEM()
RATIONAL_B_SPLINE_SURFACE(((0.987633126750594,0.986929835989056,0.989150325841689),
(0.987633126750594,0.986929835989056,0.989150325841689)))
REPRESENTATION_ITEM('')
SURFACE()
);
#1962=(
BOUNDED_SURFACE()
B_SPLINE_SURFACE(1,2,((#127609,#127610,#127611,#127612,#127613),(#127614,
#127615,#127616,#127617,#127618)),.UNSPECIFIED.,.F.,.F.,.F.)
B_SPLINE_SURFACE_WITH_KNOTS((2,2),(3,2,3),(0.709961051579736,1.),(0.469787852530351,
0.470019760166364,0.48736334072649),.UNSPECIFIED.)
GEOMETRIC_REPRESENTATION_ITEM()
RATIONAL_B_SPLINE_SURFACE(((0.987787102172814,0.987787102172814,0.987787102172814,
0.988764511531023,0.992698258926488),(0.987787102172814,0.987787102172814,
0.987787102172814,0.988764511531023,0.992698258926488)))
REPRESENTATION_ITEM('')
SURFACE()
);
#1963=(
BOUNDED_SURFACE()
B_SPLINE_SURFACE(1,2,((#127627,#127628,#127629),(#127630,#127631,#127632)),
 .UNSPECIFIED.,.F.,.F.,.F.)
B_SPLINE_SURFACE_WITH_KNOTS((2,2),(3,3),(0.710318915640071,1.),(0.24585118339369,
0.263098999273938),.UNSPECIFIED.)
GEOMETRIC_REPRESENTATION_ITEM()
RATIONAL_B_SPLINE_SURFACE(((0.987633126750594,0.986929835989056,0.98915032584169),
(0.987633126750594,0.986929835989056,0.98915032584169)))
REPRESENTATION_ITEM('')
SURFACE()
);
#1964=(
BOUNDED_SURFACE()
B_SPLINE_SURFACE(1,2,((#127634,#127635,#127636,#127637,#127638),(#127639,
#127640,#127641,#127642,#127643)),.UNSPECIFIED.,.F.,.F.,.F.)
B_SPLINE_SURFACE_WITH_KNOTS((2,2),(3,2,3),(0.709595573585733,1.),(0.469422374536338,
0.470019760166364,0.48736334072649),.UNSPECIFIED.)
GEOMETRIC_REPRESENTATION_ITEM()
RATIONAL_B_SPLINE_SURFACE(((0.987787102172814,0.987787102172814,0.987787102172814,
0.988764511531023,0.992698258926488),(0.987787102172814,0.987787102172814,
0.987787102172814,0.988764511531023,0.992698258926488)))
REPRESENTATION_ITEM('')
SURFACE()
);
#1965=(
BOUNDED_SURFACE()
B_SPLINE_SURFACE(1,2,((#127652,#127653,#127654),(#127655,#127656,#127657)),
 .UNSPECIFIED.,.F.,.F.,.F.)
B_SPLINE_SURFACE_WITH_KNOTS((2,2),(3,3),(0.710318915640081,1.),(0.245851183393689,
0.263098999273938),.UNSPECIFIED.)
GEOMETRIC_REPRESENTATION_ITEM()
RATIONAL_B_SPLINE_SURFACE(((0.987633126750594,0.986929835989056,0.989150325841689),
(0.987633126750594,0.986929835989056,0.989150325841689)))
REPRESENTATION_ITEM('')
SURFACE()
);
#1966=(
BOUNDED_SURFACE()
B_SPLINE_SURFACE(1,2,((#127659,#127660,#127661,#127662,#127663),(#127664,
#127665,#127666,#127667,#127668)),.UNSPECIFIED.,.F.,.F.,.F.)
B_SPLINE_SURFACE_WITH_KNOTS((2,2),(3,2,3),(0.709595573571102,1.),(0.469422374521711,
0.470019760166364,0.48736334072649),.UNSPECIFIED.)
GEOMETRIC_REPRESENTATION_ITEM()
RATIONAL_B_SPLINE_SURFACE(((0.987787102172814,0.987787102172814,0.987787102172814,
0.988764511531023,0.992698258926488),(0.987787102172814,0.987787102172814,
0.987787102172814,0.988764511531023,0.992698258926488)))
REPRESENTATION_ITEM('')
SURFACE()
);
#1967=(
BOUNDED_SURFACE()
B_SPLINE_SURFACE(1,2,((#127677,#127678,#127679),(#127680,#127681,#127682)),
 .UNSPECIFIED.,.F.,.F.,.F.)
B_SPLINE_SURFACE_WITH_KNOTS((2,2),(3,3),(0.710318915640074,1.),(0.24585118339369,
0.263098999273796),.UNSPECIFIED.)
GEOMETRIC_REPRESENTATION_ITEM()
RATIONAL_B_SPLINE_SURFACE(((0.987633126750594,0.986929835989062,0.989150325841653),
(0.987633126750594,0.986929835989062,0.989150325841653)))
REPRESENTATION_ITEM('')
SURFACE()
);
#1968=(
BOUNDED_SURFACE()
B_SPLINE_SURFACE(1,2,((#127684,#127685,#127686,#127687,#127688),(#127689,
#127690,#127691,#127692,#127693)),.UNSPECIFIED.,.F.,.F.,.F.)
B_SPLINE_SURFACE_WITH_KNOTS((2,2),(3,2,3),(0.709595573536973,1.),(0.469422374487583,
0.470019760166364,0.48736334072649),.UNSPECIFIED.)
GEOMETRIC_REPRESENTATION_ITEM()
RATIONAL_B_SPLINE_SURFACE(((0.987787102172814,0.987787102172814,0.987787102172814,
0.988764511531023,0.992698258926488),(0.987787102172814,0.987787102172814,
0.987787102172814,0.988764511531023,0.992698258926488)))
REPRESENTATION_ITEM('')
SURFACE()
);
#1969=(
BOUNDED_SURFACE()
B_SPLINE_SURFACE(1,2,((#127702,#127703,#127704),(#127705,#127706,#127707)),
 .UNSPECIFIED.,.F.,.F.,.F.)
B_SPLINE_SURFACE_WITH_KNOTS((2,2),(3,3),(0.71031891564008,1.),(0.24585118339369,
0.263098999273796),.UNSPECIFIED.)
GEOMETRIC_REPRESENTATION_ITEM()
RATIONAL_B_SPLINE_SURFACE(((0.987633126750594,0.986929835989062,0.989150325841653),
(0.987633126750594,0.986929835989062,0.989150325841653)))
REPRESENTATION_ITEM('')
SURFACE()
);
#1970=(
BOUNDED_SURFACE()
B_SPLINE_SURFACE(1,2,((#127709,#127710,#127711,#127712,#127713),(#127714,
#127715,#127716,#127717,#127718)),.UNSPECIFIED.,.F.,.F.,.F.)
B_SPLINE_SURFACE_WITH_KNOTS((2,2),(3,2,3),(0.709595573578629,1.),(0.469422374529239,
0.470019760166364,0.48736334072649),.UNSPECIFIED.)
GEOMETRIC_REPRESENTATION_ITEM()
RATIONAL_B_SPLINE_SURFACE(((0.987787102172814,0.987787102172814,0.987787102172814,
0.988764511531023,0.992698258926488),(0.987787102172814,0.987787102172814,
0.987787102172814,0.988764511531023,0.992698258926488)))
REPRESENTATION_ITEM('')
SURFACE()
);
#1971=(
BOUNDED_SURFACE()
B_SPLINE_SURFACE(1,2,((#127727,#127728,#127729),(#127730,#127731,#127732)),
 .UNSPECIFIED.,.F.,.F.,.F.)
B_SPLINE_SURFACE_WITH_KNOTS((2,2),(3,3),(0.710318915640078,1.),(0.24585118339369,
0.263098999273796),.UNSPECIFIED.)
GEOMETRIC_REPRESENTATION_ITEM()
RATIONAL_B_SPLINE_SURFACE(((0.987633126750594,0.986929835989062,0.989150325841653),
(0.987633126750594,0.986929835989062,0.989150325841653)))
REPRESENTATION_ITEM('')
SURFACE()
);
#1972=(
BOUNDED_SURFACE()
B_SPLINE_SURFACE(1,2,((#127734,#127735,#127736,#127737,#127738),(#127739,
#127740,#127741,#127742,#127743)),.UNSPECIFIED.,.F.,.F.,.F.)
B_SPLINE_SURFACE_WITH_KNOTS((2,2),(3,2,3),(0.709595573584959,1.),(0.469422374535573,
0.470019760166364,0.48736334072649),.UNSPECIFIED.)
GEOMETRIC_REPRESENTATION_ITEM()
RATIONAL_B_SPLINE_SURFACE(((0.987787102172814,0.987787102172814,0.987787102172814,
0.988764511531023,0.992698258926488),(0.987787102172814,0.987787102172814,
0.987787102172814,0.988764511531023,0.992698258926488)))
REPRESENTATION_ITEM('')
SURFACE()
);
#1973=(
BOUNDED_SURFACE()
B_SPLINE_SURFACE(1,2,((#127752,#127753,#127754),(#127755,#127756,#127757)),
 .UNSPECIFIED.,.F.,.F.,.F.)
B_SPLINE_SURFACE_WITH_KNOTS((2,2),(3,3),(0.71031891564008,1.),(0.24585118339369,
0.263098999273796),.UNSPECIFIED.)
GEOMETRIC_REPRESENTATION_ITEM()
RATIONAL_B_SPLINE_SURFACE(((0.987633126750594,0.986929835989062,0.989150325841653),
(0.987633126750594,0.986929835989062,0.989150325841653)))
REPRESENTATION_ITEM('')
SURFACE()
);
#1974=(
BOUNDED_SURFACE()
B_SPLINE_SURFACE(1,2,((#127759,#127760,#127761,#127762,#127763),(#127764,
#127765,#127766,#127767,#127768)),.UNSPECIFIED.,.F.,.F.,.F.)
B_SPLINE_SURFACE_WITH_KNOTS((2,2),(3,2,3),(0.709595573563293,1.),(0.469422374515312,
0.470019760166364,0.48736334072649),.UNSPECIFIED.)
GEOMETRIC_REPRESENTATION_ITEM()
RATIONAL_B_SPLINE_SURFACE(((0.987787102172814,0.987787102172814,0.987787102172814,
0.988764511531023,0.992698258926488),(0.987787102172814,0.987787102172814,
0.987787102172814,0.988764511531023,0.992698258926488)))
REPRESENTATION_ITEM('')
SURFACE()
);
#1975=(
BOUNDED_SURFACE()
B_SPLINE_SURFACE(1,2,((#127777,#127778,#127779),(#127780,#127781,#127782)),
 .UNSPECIFIED.,.F.,.F.,.F.)
B_SPLINE_SURFACE_WITH_KNOTS((2,2),(3,3),(0.710318915638679,1.),(0.24585118339369,
0.263098999273796),.UNSPECIFIED.)
GEOMETRIC_REPRESENTATION_ITEM()
RATIONAL_B_SPLINE_SURFACE(((0.987633126750594,0.986929835989062,0.989150325841653),
(0.987633126750594,0.986929835989062,0.989150325841653)))
REPRESENTATION_ITEM('')
SURFACE()
);
#1976=(
BOUNDED_SURFACE()
B_SPLINE_SURFACE(1,2,((#127784,#127785,#127786,#127787,#127788),(#127789,
#127790,#127791,#127792,#127793)),.UNSPECIFIED.,.F.,.F.,.F.)
B_SPLINE_SURFACE_WITH_KNOTS((2,2),(3,2,3),(0.709595573585933,1.),(0.469422374536543,
0.470019760166364,0.48736334072649),.UNSPECIFIED.)
GEOMETRIC_REPRESENTATION_ITEM()
RATIONAL_B_SPLINE_SURFACE(((0.987787102172814,0.987787102172814,0.987787102172814,
0.988764511531023,0.992698258926488),(0.987787102172814,0.987787102172814,
0.987787102172814,0.988764511531023,0.992698258926488)))
REPRESENTATION_ITEM('')
SURFACE()
);
#1977=(
BOUNDED_SURFACE()
B_SPLINE_SURFACE(1,2,((#127802,#127803,#127804),(#127805,#127806,#127807)),
 .UNSPECIFIED.,.F.,.F.,.F.)
B_SPLINE_SURFACE_WITH_KNOTS((2,2),(3,3),(0.710318915640079,1.),(0.24585118339369,
0.263098999273799),.UNSPECIFIED.)
GEOMETRIC_REPRESENTATION_ITEM()
RATIONAL_B_SPLINE_SURFACE(((0.987633126750594,0.986929835989062,0.989150325841654),
(0.987633126750594,0.986929835989062,0.989150325841654)))
REPRESENTATION_ITEM('')
SURFACE()
);
#1978=(
BOUNDED_SURFACE()
B_SPLINE_SURFACE(1,2,((#127809,#127810,#127811,#127812,#127813),(#127814,
#127815,#127816,#127817,#127818)),.UNSPECIFIED.,.F.,.F.,.F.)
B_SPLINE_SURFACE_WITH_KNOTS((2,2),(3,2,3),(0.709595573588909,1.),(0.469422374539605,
0.470019760166367,0.487363340726489),.UNSPECIFIED.)
GEOMETRIC_REPRESENTATION_ITEM()
RATIONAL_B_SPLINE_SURFACE(((0.987787102172814,0.987787102172814,0.987787102172814,
0.988764511531024,0.992698258926487),(0.987787102172814,0.987787102172814,
0.987787102172814,0.988764511531024,0.992698258926487)))
REPRESENTATION_ITEM('')
SURFACE()
);
#1979=(
BOUNDED_SURFACE()
B_SPLINE_SURFACE(1,2,((#127827,#127828,#127829),(#127830,#127831,#127832)),
 .UNSPECIFIED.,.F.,.F.,.F.)
B_SPLINE_SURFACE_WITH_KNOTS((2,2),(3,3),(0.710318915640001,1.),(0.245851183393691,
0.263098999273797),.UNSPECIFIED.)
GEOMETRIC_REPRESENTATION_ITEM()
RATIONAL_B_SPLINE_SURFACE(((0.987633126750594,0.986929835989062,0.989150325841653),
(0.987633126750594,0.986929835989062,0.989150325841653)))
REPRESENTATION_ITEM('')
SURFACE()
);
#1980=(
BOUNDED_SURFACE()
B_SPLINE_SURFACE(1,2,((#127834,#127835,#127836,#127837,#127838),(#127839,
#127840,#127841,#127842,#127843)),.UNSPECIFIED.,.F.,.F.,.F.)
B_SPLINE_SURFACE_WITH_KNOTS((2,2),(3,2,3),(0.709595573560027,1.),(0.469422374510715,
0.470019760166363,0.487363340726489),.UNSPECIFIED.)
GEOMETRIC_REPRESENTATION_ITEM()
RATIONAL_B_SPLINE_SURFACE(((0.987787102172813,0.987787102172813,0.987787102172813,
0.988764511531023,0.992698258926487),(0.987787102172814,0.987787102172814,
0.987787102172814,0.988764511531023,0.992698258926487)))
REPRESENTATION_ITEM('')
SURFACE()
);
#1981=(
BOUNDED_SURFACE()
B_SPLINE_SURFACE(1,2,((#127852,#127853,#127854),(#127855,#127856,#127857)),
 .UNSPECIFIED.,.F.,.F.,.F.)
B_SPLINE_SURFACE_WITH_KNOTS((2,2),(3,3),(0.71031891564,1.),(0.245851183393691,
0.2630989992738),.UNSPECIFIED.)
GEOMETRIC_REPRESENTATION_ITEM()
RATIONAL_B_SPLINE_SURFACE(((0.987633126750594,0.986929835989062,0.989150325841654),
(0.987633126750594,0.986929835989062,0.989150325841654)))
REPRESENTATION_ITEM('')
SURFACE()
);
#1982=(
BOUNDED_SURFACE()
B_SPLINE_SURFACE(1,2,((#127859,#127860,#127861,#127862,#127863),(#127864,
#127865,#127866,#127867,#127868)),.UNSPECIFIED.,.F.,.F.,.F.)
B_SPLINE_SURFACE_WITH_KNOTS((2,2),(3,2,3),(0.70959557356092,1.),(0.469422374511607,
0.470019760166363,0.487363340726489),.UNSPECIFIED.)
GEOMETRIC_REPRESENTATION_ITEM()
RATIONAL_B_SPLINE_SURFACE(((0.987787102172813,0.987787102172813,0.987787102172813,
0.988764511531023,0.992698258926487),(0.987787102172813,0.987787102172813,
0.987787102172813,0.988764511531023,0.992698258926487)))
REPRESENTATION_ITEM('')
SURFACE()
);
#1983=(
BOUNDED_SURFACE()
B_SPLINE_SURFACE(1,2,((#127877,#127878,#127879),(#127880,#127881,#127882)),
 .UNSPECIFIED.,.F.,.F.,.F.)
B_SPLINE_SURFACE_WITH_KNOTS((2,2),(3,3),(0.710318915640003,1.),(0.245851183393691,
0.26309899927383),.UNSPECIFIED.)
GEOMETRIC_REPRESENTATION_ITEM()
RATIONAL_B_SPLINE_SURFACE(((0.987633126750594,0.98692983598906,0.989150325841661),
(0.987633126750594,0.98692983598906,0.989150325841662)))
REPRESENTATION_ITEM('')
SURFACE()
);
#1984=(
BOUNDED_SURFACE()
B_SPLINE_SURFACE(1,2,((#127884,#127885,#127886,#127887,#127888),(#127889,
#127890,#127891,#127892,#127893)),.UNSPECIFIED.,.F.,.F.,.F.)
B_SPLINE_SURFACE_WITH_KNOTS((2,2),(3,2,3),(0.709595573558224,1.),(0.469422374509515,
0.470019760166363,0.487363340726489),.UNSPECIFIED.)
GEOMETRIC_REPRESENTATION_ITEM()
RATIONAL_B_SPLINE_SURFACE(((0.987787102172813,0.987787102172813,0.987787102172813,
0.988764511531023,0.992698258926487),(0.987787102172813,0.987787102172813,
0.987787102172813,0.988764511531023,0.992698258926487)))
REPRESENTATION_ITEM('')
SURFACE()
);
#1985=(
BOUNDED_SURFACE()
B_SPLINE_SURFACE(1,2,((#127902,#127903,#127904),(#127905,#127906,#127907)),
 .UNSPECIFIED.,.F.,.F.,.F.)
B_SPLINE_SURFACE_WITH_KNOTS((2,2),(3,3),(0.7103189156394,1.),(0.245851183393691,
0.263098999273797),.UNSPECIFIED.)
GEOMETRIC_REPRESENTATION_ITEM()
RATIONAL_B_SPLINE_SURFACE(((0.987633126750594,0.986929835989062,0.989150325841653),
(0.987633126750594,0.986929835989062,0.989150325841653)))
REPRESENTATION_ITEM('')
SURFACE()
);
#1986=(
BOUNDED_SURFACE()
B_SPLINE_SURFACE(1,2,((#127909,#127910,#127911,#127912,#127913),(#127914,
#127915,#127916,#127917,#127918)),.UNSPECIFIED.,.F.,.F.,.F.)
B_SPLINE_SURFACE_WITH_KNOTS((2,2),(3,2,3),(0.709595573582174,1.),(0.46942237453283,
0.470019760166363,0.487363340726489),.UNSPECIFIED.)
GEOMETRIC_REPRESENTATION_ITEM()
RATIONAL_B_SPLINE_SURFACE(((0.987787102172814,0.987787102172814,0.987787102172814,
0.988764511531023,0.992698258926487),(0.987787102172814,0.987787102172814,
0.987787102172814,0.988764511531023,0.992698258926487)))
REPRESENTATION_ITEM('')
SURFACE()
);
#1987=(
BOUNDED_SURFACE()
B_SPLINE_SURFACE(1,2,((#127927,#127928,#127929),(#127930,#127931,#127932)),
 .UNSPECIFIED.,.F.,.F.,.F.)
B_SPLINE_SURFACE_WITH_KNOTS((2,2),(3,3),(0.710318915640033,1.),(0.245851183393691,
0.263098999273797),.UNSPECIFIED.)
GEOMETRIC_REPRESENTATION_ITEM()
RATIONAL_B_SPLINE_SURFACE(((0.987633126750594,0.986929835989062,0.989150325841653),
(0.987633126750594,0.986929835989062,0.989150325841653)))
REPRESENTATION_ITEM('')
SURFACE()
);
#1988=(
BOUNDED_SURFACE()
B_SPLINE_SURFACE(1,2,((#127934,#127935,#127936,#127937,#127938),(#127939,
#127940,#127941,#127942,#127943)),.UNSPECIFIED.,.F.,.F.,.F.)
B_SPLINE_SURFACE_WITH_KNOTS((2,2),(3,2,3),(0.709595573563331,1.),(0.469422374514008,
0.470019760166363,0.487363340726489),.UNSPECIFIED.)
GEOMETRIC_REPRESENTATION_ITEM()
RATIONAL_B_SPLINE_SURFACE(((0.987787102172813,0.987787102172813,0.987787102172813,
0.988764511531023,0.992698258926487),(0.987787102172813,0.987787102172813,
0.987787102172813,0.988764511531023,0.992698258926487)))
REPRESENTATION_ITEM('')
SURFACE()
);
#1989=(
BOUNDED_SURFACE()
B_SPLINE_SURFACE(1,2,((#127952,#127953,#127954),(#127955,#127956,#127957)),
 .UNSPECIFIED.,.F.,.F.,.F.)
B_SPLINE_SURFACE_WITH_KNOTS((2,2),(3,3),(0.710318915640017,1.),(0.245851183393691,
0.263098999273797),.UNSPECIFIED.)
GEOMETRIC_REPRESENTATION_ITEM()
RATIONAL_B_SPLINE_SURFACE(((0.987633126750594,0.986929835989062,0.989150325841653),
(0.987633126750594,0.986929835989062,0.989150325841653)))
REPRESENTATION_ITEM('')
SURFACE()
);
#1990=(
BOUNDED_SURFACE()
B_SPLINE_SURFACE(1,2,((#127959,#127960,#127961,#127962,#127963),(#127964,
#127965,#127966,#127967,#127968)),.UNSPECIFIED.,.F.,.F.,.F.)
B_SPLINE_SURFACE_WITH_KNOTS((2,2),(3,2,3),(0.709595573612439,1.),(0.46942237456311,
0.470019760166363,0.487363340726489),.UNSPECIFIED.)
GEOMETRIC_REPRESENTATION_ITEM()
RATIONAL_B_SPLINE_SURFACE(((0.987787102172814,0.987787102172814,0.987787102172814,
0.988764511531023,0.992698258926487),(0.987787102172813,0.987787102172813,
0.987787102172813,0.988764511531023,0.992698258926487)))
REPRESENTATION_ITEM('')
SURFACE()
);
#1991=(
BOUNDED_SURFACE()
B_SPLINE_SURFACE(1,2,((#127977,#127978,#127979),(#127980,#127981,#127982)),
 .UNSPECIFIED.,.F.,.F.,.F.)
B_SPLINE_SURFACE_WITH_KNOTS((2,2),(3,3),(0.710318915640028,1.),(0.245851183393691,
0.263098999273796),.UNSPECIFIED.)
GEOMETRIC_REPRESENTATION_ITEM()
RATIONAL_B_SPLINE_SURFACE(((0.987633126750594,0.986929835989062,0.989150325841653),
(0.987633126750594,0.986929835989062,0.989150325841653)))
REPRESENTATION_ITEM('')
SURFACE()
);
#1992=(
BOUNDED_SURFACE()
B_SPLINE_SURFACE(1,2,((#127984,#127985,#127986,#127987,#127988),(#127989,
#127990,#127991,#127992,#127993)),.UNSPECIFIED.,.F.,.F.,.F.)
B_SPLINE_SURFACE_WITH_KNOTS((2,2),(3,2,3),(0.,0.290289290029958),(0.194028469417326,
0.211502584834065,0.212110790666945),.UNSPECIFIED.)
GEOMETRIC_REPRESENTATION_ITEM()
RATIONAL_B_SPLINE_SURFACE(((0.989812124691679,0.992466718773227,0.998122319569323,
0.998122319569323,0.998122319569323),(0.989812124691679,0.992466718773227,
0.998122319569323,0.998122319569323,0.998122319569323)))
REPRESENTATION_ITEM('')
SURFACE()
);
#1993=(
BOUNDED_SURFACE()
B_SPLINE_SURFACE(1,2,((#128002,#128003,#128004),(#128005,#128006,#128007)),
 .UNSPECIFIED.,.F.,.F.,.F.)
B_SPLINE_SURFACE_WITH_KNOTS((2,2),(3,3),(0.,0.289807040991561),(0.52191752982614,
0.539102123117534),.UNSPECIFIED.)
GEOMETRIC_REPRESENTATION_ITEM()
RATIONAL_B_SPLINE_SURFACE(((0.989334769731189,0.987004571835916,0.987576759359605),
(0.989334769731189,0.987004571835916,0.987576759359605)))
REPRESENTATION_ITEM('')
SURFACE()
);
#1994=(
BOUNDED_SURFACE()
B_SPLINE_SURFACE(1,2,((#128009,#128010,#128011,#128012,#128013),(#128014,
#128015,#128016,#128017,#128018)),.UNSPECIFIED.,.F.,.F.,.F.)
B_SPLINE_SURFACE_WITH_KNOTS((2,2),(3,2,3),(0.,0.290289290020155),(0.194028469417326,
0.211502584834065,0.212110790657142),.UNSPECIFIED.)
GEOMETRIC_REPRESENTATION_ITEM()
RATIONAL_B_SPLINE_SURFACE(((0.989812124691679,0.992466718773227,0.998122319569323,
0.998122319569323,0.998122319569323),(0.989812124691679,0.992466718773227,
0.998122319569323,0.998122319569323,0.998122319569323)))
REPRESENTATION_ITEM('')
SURFACE()
);
#1995=(
BOUNDED_SURFACE()
B_SPLINE_SURFACE(1,2,((#128027,#128028,#128029),(#128030,#128031,#128032)),
 .UNSPECIFIED.,.F.,.F.,.F.)
B_SPLINE_SURFACE_WITH_KNOTS((2,2),(3,3),(0.,0.289807040992492),(0.52191752982614,
0.539102123117534),.UNSPECIFIED.)
GEOMETRIC_REPRESENTATION_ITEM()
RATIONAL_B_SPLINE_SURFACE(((0.989334769731189,0.987004571835916,0.987576759359605),
(0.989334769731189,0.987004571835916,0.987576759359605)))
REPRESENTATION_ITEM('')
SURFACE()
);
#1996=(
BOUNDED_SURFACE()
B_SPLINE_SURFACE(1,2,((#128034,#128035,#128036,#128037,#128038),(#128039,
#128040,#128041,#128042,#128043)),.UNSPECIFIED.,.F.,.F.,.F.)
B_SPLINE_SURFACE_WITH_KNOTS((2,2),(3,2,3),(0.,0.290289290029112),(0.194028469417326,
0.211502584834065,0.212110790666098),.UNSPECIFIED.)
GEOMETRIC_REPRESENTATION_ITEM()
RATIONAL_B_SPLINE_SURFACE(((0.989812124691679,0.992466718773227,0.998122319569323,
0.998122319569323,0.998122319569323),(0.989812124691679,0.992466718773227,
0.998122319569323,0.998122319569323,0.998122319569323)))
REPRESENTATION_ITEM('')
SURFACE()
);
#1997=(
BOUNDED_SURFACE()
B_SPLINE_SURFACE(1,2,((#128052,#128053,#128054),(#128055,#128056,#128057)),
 .UNSPECIFIED.,.F.,.F.,.F.)
B_SPLINE_SURFACE_WITH_KNOTS((2,2),(3,3),(0.,0.289807040992486),(0.52191752982614,
0.539102123117534),.UNSPECIFIED.)
GEOMETRIC_REPRESENTATION_ITEM()
RATIONAL_B_SPLINE_SURFACE(((0.989334769731189,0.987004571835916,0.987576759359605),
(0.989334769731189,0.987004571835916,0.987576759359605)))
REPRESENTATION_ITEM('')
SURFACE()
);
#1998=(
BOUNDED_SURFACE()
B_SPLINE_SURFACE(1,2,((#128059,#128060,#128061,#128062,#128063),(#128064,
#128065,#128066,#128067,#128068)),.UNSPECIFIED.,.F.,.F.,.F.)
B_SPLINE_SURFACE_WITH_KNOTS((2,2),(3,2,3),(0.,0.290289290026752),(0.194028469417326,
0.211502584834065,0.212110790663731),.UNSPECIFIED.)
GEOMETRIC_REPRESENTATION_ITEM()
RATIONAL_B_SPLINE_SURFACE(((0.989812124691679,0.992466718773227,0.998122319569323,
0.998122319569323,0.998122319569323),(0.989812124691679,0.992466718773227,
0.998122319569323,0.998122319569323,0.998122319569323)))
REPRESENTATION_ITEM('')
SURFACE()
);
#1999=(
BOUNDED_SURFACE()
B_SPLINE_SURFACE(1,2,((#128077,#128078,#128079),(#128080,#128081,#128082)),
 .UNSPECIFIED.,.F.,.F.,.F.)
B_SPLINE_SURFACE_WITH_KNOTS((2,2),(3,3),(0.,0.289807040992493),(0.52191752982614,
0.539102123117534),.UNSPECIFIED.)
GEOMETRIC_REPRESENTATION_ITEM()
RATIONAL_B_SPLINE_SURFACE(((0.989334769731189,0.987004571835916,0.987576759359605),
(0.989334769731189,0.987004571835916,0.987576759359604)))
REPRESENTATION_ITEM('')
SURFACE()
);
#2000=(
BOUNDED_SURFACE()
B_SPLINE_SURFACE(1,2,((#128084,#128085,#128086,#128087,#128088),(#128089,
#128090,#128091,#128092,#128093)),.UNSPECIFIED.,.F.,.F.,.F.)
B_SPLINE_SURFACE_WITH_KNOTS((2,2),(3,2,3),(0.,0.290289290015737),(0.194028469417326,
0.211502584834065,0.21211079065272),.UNSPECIFIED.)
GEOMETRIC_REPRESENTATION_ITEM()
RATIONAL_B_SPLINE_SURFACE(((0.989812124691679,0.992466718773227,0.998122319569323,
0.998122319569323,0.998122319569323),(0.989812124691679,0.992466718773227,
0.998122319569323,0.998122319569323,0.998122319569323)))
REPRESENTATION_ITEM('')
SURFACE()
);
#2001=(
BOUNDED_SURFACE()
B_SPLINE_SURFACE(1,2,((#128102,#128103,#128104),(#128105,#128106,#128107)),
 .UNSPECIFIED.,.F.,.F.,.F.)
B_SPLINE_SURFACE_WITH_KNOTS((2,2),(3,3),(0.,0.289807040993074),(0.52191752982614,
0.539102123117534),.UNSPECIFIED.)
GEOMETRIC_REPRESENTATION_ITEM()
RATIONAL_B_SPLINE_SURFACE(((0.989334769731189,0.987004571835916,0.987576759359605),
(0.989334769731189,0.987004571835916,0.987576759359605)))
REPRESENTATION_ITEM('')
SURFACE()
);
#2002=(
BOUNDED_SURFACE()
B_SPLINE_SURFACE(1,2,((#128109,#128110,#128111,#128112,#128113),(#128114,
#128115,#128116,#128117,#128118)),.UNSPECIFIED.,.F.,.F.,.F.)
B_SPLINE_SURFACE_WITH_KNOTS((2,2),(3,2,3),(0.,0.290289290022082),(0.194028469417326,
0.211502584834065,0.212110790659061),.UNSPECIFIED.)
GEOMETRIC_REPRESENTATION_ITEM()
RATIONAL_B_SPLINE_SURFACE(((0.989812124691679,0.992466718773227,0.998122319569323,
0.998122319569323,0.998122319569323),(0.989812124691679,0.992466718773227,
0.998122319569323,0.998122319569323,0.998122319569323)))
REPRESENTATION_ITEM('')
SURFACE()
);
#2003=(
BOUNDED_SURFACE()
B_SPLINE_SURFACE(1,2,((#128127,#128128,#128129),(#128130,#128131,#128132)),
 .UNSPECIFIED.,.F.,.F.,.F.)
B_SPLINE_SURFACE_WITH_KNOTS((2,2),(3,3),(0.,0.289807040992486),(0.52191752982614,
0.539102123117534),.UNSPECIFIED.)
GEOMETRIC_REPRESENTATION_ITEM()
RATIONAL_B_SPLINE_SURFACE(((0.989334769731189,0.987004571835916,0.987576759359605),
(0.989334769731189,0.987004571835916,0.987576759359605)))
REPRESENTATION_ITEM('')
SURFACE()
);
#2004=(
BOUNDED_SURFACE()
B_SPLINE_SURFACE(1,2,((#128134,#128135,#128136,#128137,#128138),(#128139,
#128140,#128141,#128142,#128143)),.UNSPECIFIED.,.F.,.F.,.F.)
B_SPLINE_SURFACE_WITH_KNOTS((2,2),(3,2,3),(0.,0.290289290016757),(0.194028469417326,
0.211502584834065,0.212110790653736),.UNSPECIFIED.)
GEOMETRIC_REPRESENTATION_ITEM()
RATIONAL_B_SPLINE_SURFACE(((0.989812124691679,0.992466718773227,0.998122319569323,
0.998122319569323,0.998122319569323),(0.989812124691679,0.992466718773227,
0.998122319569323,0.998122319569323,0.998122319569323)))
REPRESENTATION_ITEM('')
SURFACE()
);
#2005=(
BOUNDED_SURFACE()
B_SPLINE_SURFACE(1,2,((#128152,#128153,#128154),(#128155,#128156,#128157)),
 .UNSPECIFIED.,.F.,.F.,.F.)
B_SPLINE_SURFACE_WITH_KNOTS((2,2),(3,3),(0.,0.289807040993074),(0.52191752982614,
0.539102123117534),.UNSPECIFIED.)
GEOMETRIC_REPRESENTATION_ITEM()
RATIONAL_B_SPLINE_SURFACE(((0.989334769731189,0.987004571835916,0.987576759359605),
(0.989334769731189,0.987004571835916,0.987576759359605)))
REPRESENTATION_ITEM('')
SURFACE()
);
#2006=(
BOUNDED_SURFACE()
B_SPLINE_SURFACE(1,2,((#128159,#128160,#128161,#128162,#128163),(#128164,
#128165,#128166,#128167,#128168)),.UNSPECIFIED.,.F.,.F.,.F.)
B_SPLINE_SURFACE_WITH_KNOTS((2,2),(3,2,3),(0.,0.290289290019312),(0.194028469417326,
0.211502584834065,0.212110790656298),.UNSPECIFIED.)
GEOMETRIC_REPRESENTATION_ITEM()
RATIONAL_B_SPLINE_SURFACE(((0.989812124691679,0.992466718773227,0.998122319569323,
0.998122319569323,0.998122319569323),(0.989812124691679,0.992466718773227,
0.998122319569323,0.998122319569323,0.998122319569323)))
REPRESENTATION_ITEM('')
SURFACE()
);
#2007=(
BOUNDED_SURFACE()
B_SPLINE_SURFACE(1,2,((#128177,#128178,#128179),(#128180,#128181,#128182)),
 .UNSPECIFIED.,.F.,.F.,.F.)
B_SPLINE_SURFACE_WITH_KNOTS((2,2),(3,3),(0.,0.289807040992569),(0.521917529826141,
0.539102123117534),.UNSPECIFIED.)
GEOMETRIC_REPRESENTATION_ITEM()
RATIONAL_B_SPLINE_SURFACE(((0.989334769731189,0.987004571835916,0.987576759359605),
(0.989334769731189,0.987004571835916,0.987576759359605)))
REPRESENTATION_ITEM('')
SURFACE()
);
#2008=(
BOUNDED_SURFACE()
B_SPLINE_SURFACE(1,2,((#128184,#128185,#128186,#128187,#128188),(#128189,
#128190,#128191,#128192,#128193)),.UNSPECIFIED.,.F.,.F.,.F.)
B_SPLINE_SURFACE_WITH_KNOTS((2,2),(3,2,3),(0.,0.290289290020932),(0.194028469417325,
0.211502584834064,0.212110790657912),.UNSPECIFIED.)
GEOMETRIC_REPRESENTATION_ITEM()
RATIONAL_B_SPLINE_SURFACE(((0.989812124691679,0.992466718773227,0.998122319569322,
0.998122319569322,0.998122319569322),(0.989812124691679,0.992466718773227,
0.998122319569322,0.998122319569323,0.998122319569323)))
REPRESENTATION_ITEM('')
SURFACE()
);
#2009=(
BOUNDED_SURFACE()
B_SPLINE_SURFACE(1,2,((#128202,#128203,#128204),(#128205,#128206,#128207)),
 .UNSPECIFIED.,.F.,.F.,.F.)
B_SPLINE_SURFACE_WITH_KNOTS((2,2),(3,3),(0.,0.289807040992568),(0.521917529826141,
0.539102123117535),.UNSPECIFIED.)
GEOMETRIC_REPRESENTATION_ITEM()
RATIONAL_B_SPLINE_SURFACE(((0.989334769731189,0.987004571835916,0.987576759359605),
(0.989334769731189,0.987004571835916,0.987576759359605)))
REPRESENTATION_ITEM('')
SURFACE()
);
#2010=(
BOUNDED_SURFACE()
B_SPLINE_SURFACE(1,2,((#128209,#128210,#128211,#128212,#128213),(#128214,
#128215,#128216,#128217,#128218)),.UNSPECIFIED.,.F.,.F.,.F.)
B_SPLINE_SURFACE_WITH_KNOTS((2,2),(3,2,3),(0.,0.290289290013028),(0.194028469417325,
0.211502584834064,0.21211079065001),.UNSPECIFIED.)
GEOMETRIC_REPRESENTATION_ITEM()
RATIONAL_B_SPLINE_SURFACE(((0.989812124691679,0.992466718773227,0.998122319569322,
0.998122319569322,0.998122319569322),(0.989812124691679,0.992466718773227,
0.998122319569322,0.998122319569322,0.998122319569322)))
REPRESENTATION_ITEM('')
SURFACE()
);
#2011=(
BOUNDED_SURFACE()
B_SPLINE_SURFACE(1,2,((#128227,#128228,#128229),(#128230,#128231,#128232)),
 .UNSPECIFIED.,.F.,.F.,.F.)
B_SPLINE_SURFACE_WITH_KNOTS((2,2),(3,3),(0.,0.289807040993163),(0.521917529826141,
0.539102123117535),.UNSPECIFIED.)
GEOMETRIC_REPRESENTATION_ITEM()
RATIONAL_B_SPLINE_SURFACE(((0.989334769731189,0.987004571835916,0.987576759359605),
(0.989334769731189,0.987004571835916,0.987576759359605)))
REPRESENTATION_ITEM('')
SURFACE()
);
#2012=(
BOUNDED_SURFACE()
B_SPLINE_SURFACE(1,2,((#128234,#128235,#128236,#128237,#128238),(#128239,
#128240,#128241,#128242,#128243)),.UNSPECIFIED.,.F.,.F.,.F.)
B_SPLINE_SURFACE_WITH_KNOTS((2,2),(3,2,3),(0.,0.290289290016891),(0.194028469417325,
0.211502584834064,0.212110790653872),.UNSPECIFIED.)
GEOMETRIC_REPRESENTATION_ITEM()
RATIONAL_B_SPLINE_SURFACE(((0.989812124691679,0.992466718773227,0.998122319569322,
0.998122319569322,0.998122319569322),(0.989812124691679,0.992466718773227,
0.998122319569322,0.998122319569322,0.998122319569322)))
REPRESENTATION_ITEM('')
SURFACE()
);
#2013=(
BOUNDED_SURFACE()
B_SPLINE_SURFACE(1,2,((#128252,#128253,#128254),(#128255,#128256,#128257)),
 .UNSPECIFIED.,.F.,.F.,.F.)
B_SPLINE_SURFACE_WITH_KNOTS((2,2),(3,3),(0.,0.289807040992575),(0.521917529826141,
0.539102123117535),.UNSPECIFIED.)
GEOMETRIC_REPRESENTATION_ITEM()
RATIONAL_B_SPLINE_SURFACE(((0.989334769731189,0.987004571835916,0.987576759359605),
(0.989334769731189,0.987004571835916,0.987576759359605)))
REPRESENTATION_ITEM('')
SURFACE()
);
#2014=(
BOUNDED_SURFACE()
B_SPLINE_SURFACE(1,2,((#128259,#128260,#128261,#128262,#128263),(#128264,
#128265,#128266,#128267,#128268)),.UNSPECIFIED.,.F.,.F.,.F.)
B_SPLINE_SURFACE_WITH_KNOTS((2,2),(3,2,3),(0.,0.290289290007279),(0.194028469417325,
0.211502584834064,0.21211079064426),.UNSPECIFIED.)
GEOMETRIC_REPRESENTATION_ITEM()
RATIONAL_B_SPLINE_SURFACE(((0.989812124691679,0.992466718773227,0.998122319569322,
0.998122319569322,0.998122319569322),(0.989812124691679,0.992466718773227,
0.998122319569322,0.998122319569322,0.998122319569322)))
REPRESENTATION_ITEM('')
SURFACE()
);
#2015=(
BOUNDED_SURFACE()
B_SPLINE_SURFACE(1,2,((#128277,#128278,#128279),(#128280,#128281,#128282)),
 .UNSPECIFIED.,.F.,.F.,.F.)
B_SPLINE_SURFACE_WITH_KNOTS((2,2),(3,3),(0.,0.289807040993073),(0.521917529826141,
0.539102123117535),.UNSPECIFIED.)
GEOMETRIC_REPRESENTATION_ITEM()
RATIONAL_B_SPLINE_SURFACE(((0.989334769731189,0.987004571835916,0.987576759359605),
(0.989334769731189,0.987004571835916,0.987576759359605)))
REPRESENTATION_ITEM('')
SURFACE()
);
#2016=(
BOUNDED_SURFACE()
B_SPLINE_SURFACE(1,2,((#128284,#128285,#128286,#128287,#128288),(#128289,
#128290,#128291,#128292,#128293)),.UNSPECIFIED.,.F.,.F.,.F.)
B_SPLINE_SURFACE_WITH_KNOTS((2,2),(3,2,3),(0.,0.290289290012074),(0.194028469417325,
0.211502584834064,0.212110790649057),.UNSPECIFIED.)
GEOMETRIC_REPRESENTATION_ITEM()
RATIONAL_B_SPLINE_SURFACE(((0.989812124691679,0.992466718773227,0.998122319569322,
0.998122319569322,0.998122319569322),(0.989812124691679,0.992466718773227,
0.998122319569322,0.998122319569322,0.998122319569322)))
REPRESENTATION_ITEM('')
SURFACE()
);
#2017=(
BOUNDED_SURFACE()
B_SPLINE_SURFACE(1,2,((#128302,#128303,#128304),(#128305,#128306,#128307)),
 .UNSPECIFIED.,.F.,.F.,.F.)
B_SPLINE_SURFACE_WITH_KNOTS((2,2),(3,3),(0.,0.289807040992579),(0.521917529826141,
0.539102123117535),.UNSPECIFIED.)
GEOMETRIC_REPRESENTATION_ITEM()
RATIONAL_B_SPLINE_SURFACE(((0.989334769731189,0.987004571835916,0.987576759359605),
(0.989334769731189,0.987004571835916,0.987576759359605)))
REPRESENTATION_ITEM('')
SURFACE()
);
#2018=(
BOUNDED_SURFACE()
B_SPLINE_SURFACE(1,2,((#128309,#128310,#128311,#128312,#128313),(#128314,
#128315,#128316,#128317,#128318)),.UNSPECIFIED.,.F.,.F.,.F.)
B_SPLINE_SURFACE_WITH_KNOTS((2,2),(3,2,3),(0.,0.290289290013357),(0.194028469417325,
0.211502584834064,0.212110790650338),.UNSPECIFIED.)
GEOMETRIC_REPRESENTATION_ITEM()
RATIONAL_B_SPLINE_SURFACE(((0.989812124691679,0.992466718773227,0.998122319569322,
0.998122319569322,0.998122319569322),(0.989812124691679,0.992466718773227,
0.998122319569322,0.998122319569322,0.998122319569322)))
REPRESENTATION_ITEM('')
SURFACE()
);
#2019=(
BOUNDED_SURFACE()
B_SPLINE_SURFACE(1,2,((#128327,#128328,#128329),(#128330,#128331,#128332)),
 .UNSPECIFIED.,.F.,.F.,.F.)
B_SPLINE_SURFACE_WITH_KNOTS((2,2),(3,3),(0.,0.289807040993077),(0.521917529826141,
0.539102123117535),.UNSPECIFIED.)
GEOMETRIC_REPRESENTATION_ITEM()
RATIONAL_B_SPLINE_SURFACE(((0.989334769731189,0.987004571835916,0.987576759359605),
(0.989334769731189,0.987004571835916,0.987576759359605)))
REPRESENTATION_ITEM('')
SURFACE()
);
#2020=(
BOUNDED_SURFACE()
B_SPLINE_SURFACE(1,2,((#128334,#128335,#128336,#128337,#128338),(#128339,
#128340,#128341,#128342,#128343)),.UNSPECIFIED.,.F.,.F.,.F.)
B_SPLINE_SURFACE_WITH_KNOTS((2,2),(3,2,3),(0.,0.290289290017703),(0.194028469417325,
0.211502584834064,0.212110790654683),.UNSPECIFIED.)
GEOMETRIC_REPRESENTATION_ITEM()
RATIONAL_B_SPLINE_SURFACE(((0.989812124691679,0.992466718773227,0.998122319569322,
0.998122319569322,0.998122319569322),(0.989812124691679,0.992466718773227,
0.998122319569322,0.998122319569322,0.998122319569322)))
REPRESENTATION_ITEM('')
SURFACE()
);
#2021=(
BOUNDED_SURFACE()
B_SPLINE_SURFACE(1,2,((#128352,#128353,#128354),(#128355,#128356,#128357)),
 .UNSPECIFIED.,.F.,.F.,.F.)
B_SPLINE_SURFACE_WITH_KNOTS((2,2),(3,3),(0.,0.289807040992847),(0.521917529826141,
0.539102123117535),.UNSPECIFIED.)
GEOMETRIC_REPRESENTATION_ITEM()
RATIONAL_B_SPLINE_SURFACE(((0.989334769731189,0.987004571835916,0.987576759359605),
(0.989334769731189,0.987004571835916,0.987576759359605)))
REPRESENTATION_ITEM('')
SURFACE()
);
#2022=(
BOUNDED_SURFACE()
B_SPLINE_SURFACE(1,2,((#128359,#128360,#128361,#128362,#128363),(#128364,
#128365,#128366,#128367,#128368)),.UNSPECIFIED.,.F.,.F.,.F.)
B_SPLINE_SURFACE_WITH_KNOTS((2,2),(3,2,3),(0.,0.290289290035709),(0.194028469417325,
0.211502584834064,0.212110790672689),.UNSPECIFIED.)
GEOMETRIC_REPRESENTATION_ITEM()
RATIONAL_B_SPLINE_SURFACE(((0.989812124691679,0.992466718773227,0.998122319569322,
0.998122319569322,0.998122319569322),(0.989812124691679,0.992466718773227,
0.998122319569322,0.998122319569322,0.998122319569322)))
REPRESENTATION_ITEM('')
SURFACE()
);
#2023=(
BOUNDED_SURFACE()
B_SPLINE_SURFACE(1,2,((#128377,#128378,#128379),(#128380,#128381,#128382)),
 .UNSPECIFIED.,.F.,.F.,.F.)
B_SPLINE_SURFACE_WITH_KNOTS((2,2),(3,3),(0.,0.289807040993896),(0.521917529826141,
0.539102123117535),.UNSPECIFIED.)
GEOMETRIC_REPRESENTATION_ITEM()
RATIONAL_B_SPLINE_SURFACE(((0.989334769731189,0.987004571835916,0.987576759359605),
(0.989334769731189,0.987004571835916,0.987576759359605)))
REPRESENTATION_ITEM('')
SURFACE()
);
#2024=(
BOUNDED_SURFACE()
B_SPLINE_SURFACE(1,2,((#128384,#128385,#128386,#128387,#128388),(#128389,
#128390,#128391,#128392,#128393)),.UNSPECIFIED.,.F.,.F.,.F.)
B_SPLINE_SURFACE_WITH_KNOTS((2,2),(3,2,3),(0.,0.290289290042823),(0.194028469417325,
0.211502584834064,0.212110790679806),.UNSPECIFIED.)
GEOMETRIC_REPRESENTATION_ITEM()
RATIONAL_B_SPLINE_SURFACE(((0.989812124691679,0.992466718773227,0.998122319569322,
0.998122319569322,0.998122319569322),(0.989812124691679,0.992466718773227,
0.998122319569322,0.998122319569322,0.998122319569322)))
REPRESENTATION_ITEM('')
SURFACE()
);
#2025=(
BOUNDED_SURFACE()
B_SPLINE_SURFACE(1,2,((#128402,#128403,#128404),(#128405,#128406,#128407)),
 .UNSPECIFIED.,.F.,.F.,.F.)
B_SPLINE_SURFACE_WITH_KNOTS((2,2),(3,3),(0.,0.289807040992612),(0.521917529826139,
0.539102123117535),.UNSPECIFIED.)
GEOMETRIC_REPRESENTATION_ITEM()
RATIONAL_B_SPLINE_SURFACE(((0.989334769731189,0.987004571835916,0.987576759359605),
(0.989334769731189,0.987004571835916,0.987576759359605)))
REPRESENTATION_ITEM('')
SURFACE()
);
#2026=(
BOUNDED_SURFACE()
B_SPLINE_SURFACE(1,2,((#128409,#128410,#128411,#128412,#128413),(#128414,
#128415,#128416,#128417,#128418)),.UNSPECIFIED.,.F.,.F.,.F.)
B_SPLINE_SURFACE_WITH_KNOTS((2,2),(3,2,3),(0.,0.290289290028364),(0.194028469417325,
0.211502584834064,0.212110790665341),.UNSPECIFIED.)
GEOMETRIC_REPRESENTATION_ITEM()
RATIONAL_B_SPLINE_SURFACE(((0.989812124691679,0.992466718773227,0.998122319569322,
0.998122319569322,0.998122319569322),(0.989812124691679,0.992466718773227,
0.998122319569322,0.998122319569322,0.998122319569322)))
REPRESENTATION_ITEM('')
SURFACE()
);
#2027=(
BOUNDED_SURFACE()
B_SPLINE_SURFACE(1,2,((#128427,#128428,#128429),(#128430,#128431,#128432)),
 .UNSPECIFIED.,.F.,.F.,.F.)
B_SPLINE_SURFACE_WITH_KNOTS((2,2),(3,3),(0.,0.289807040992501),(0.521917529826141,
0.539102123117535),.UNSPECIFIED.)
GEOMETRIC_REPRESENTATION_ITEM()
RATIONAL_B_SPLINE_SURFACE(((0.989334769731189,0.987004571835916,0.987576759359605),
(0.989334769731189,0.987004571835916,0.987576759359605)))
REPRESENTATION_ITEM('')
SURFACE()
);
#2028=(
BOUNDED_SURFACE()
B_SPLINE_SURFACE(1,2,((#128434,#128435,#128436,#128437,#128438),(#128439,
#128440,#128441,#128442,#128443)),.UNSPECIFIED.,.F.,.F.,.F.)
B_SPLINE_SURFACE_WITH_KNOTS((2,2),(3,2,3),(0.,0.290289290031972),(0.194028469417325,
0.211502584834065,0.212110790668951),.UNSPECIFIED.)
GEOMETRIC_REPRESENTATION_ITEM()
RATIONAL_B_SPLINE_SURFACE(((0.989812124691679,0.992466718773227,0.998122319569322,
0.998122319569322,0.998122319569322),(0.989812124691679,0.992466718773227,
0.998122319569322,0.998122319569322,0.998122319569322)))
REPRESENTATION_ITEM('')
SURFACE()
);
#2029=(
BOUNDED_SURFACE()
B_SPLINE_SURFACE(1,2,((#128452,#128453,#128454),(#128455,#128456,#128457)),
 .UNSPECIFIED.,.F.,.F.,.F.)
B_SPLINE_SURFACE_WITH_KNOTS((2,2),(3,3),(0.,0.289807040993131),(0.521917529826141,
0.539102123117535),.UNSPECIFIED.)
GEOMETRIC_REPRESENTATION_ITEM()
RATIONAL_B_SPLINE_SURFACE(((0.989334769731189,0.987004571835916,0.987576759359605),
(0.989334769731189,0.987004571835916,0.987576759359605)))
REPRESENTATION_ITEM('')
SURFACE()
);
#2030=(
BOUNDED_SURFACE()
B_SPLINE_SURFACE(1,2,((#128459,#128460,#128461,#128462,#128463),(#128464,
#128465,#128466,#128467,#128468)),.UNSPECIFIED.,.F.,.F.,.F.)
B_SPLINE_SURFACE_WITH_KNOTS((2,2),(3,2,3),(0.,0.290289290001602),(0.194028469417325,
0.211502584834064,0.212110790638577),.UNSPECIFIED.)
GEOMETRIC_REPRESENTATION_ITEM()
RATIONAL_B_SPLINE_SURFACE(((0.989812124691679,0.992466718773227,0.998122319569322,
0.998122319569322,0.998122319569322),(0.989812124691679,0.992466718773227,
0.998122319569322,0.998122319569322,0.998122319569322)))
REPRESENTATION_ITEM('')
SURFACE()
);
#2031=(
BOUNDED_SURFACE()
B_SPLINE_SURFACE(1,2,((#128477,#128478,#128479),(#128480,#128481,#128482)),
 .UNSPECIFIED.,.F.,.F.,.F.)
B_SPLINE_SURFACE_WITH_KNOTS((2,2),(3,3),(0.,0.289807040991728),(0.52191752982614,
0.539102123117535),.UNSPECIFIED.)
GEOMETRIC_REPRESENTATION_ITEM()
RATIONAL_B_SPLINE_SURFACE(((0.989334769731189,0.987004571835916,0.987576759359605),
(0.989334769731189,0.987004571835916,0.987576759359605)))
REPRESENTATION_ITEM('')
SURFACE()
);
#2032=(
BOUNDED_SURFACE()
B_SPLINE_SURFACE(1,2,((#128484,#128485,#128486,#128487,#128488),(#128489,
#128490,#128491,#128492,#128493)),.UNSPECIFIED.,.F.,.F.,.F.)
B_SPLINE_SURFACE_WITH_KNOTS((2,2),(3,2,3),(0.,0.290289290017461),(0.194028469417325,
0.211502584834064,0.212110790654441),.UNSPECIFIED.)
GEOMETRIC_REPRESENTATION_ITEM()
RATIONAL_B_SPLINE_SURFACE(((0.989812124691679,0.992466718773227,0.998122319569322,
0.998122319569322,0.998122319569322),(0.989812124691679,0.992466718773227,
0.998122319569322,0.998122319569323,0.998122319569323)))
REPRESENTATION_ITEM('')
SURFACE()
);
#2033=(
BOUNDED_SURFACE()
B_SPLINE_SURFACE(1,2,((#128502,#128503,#128504),(#128505,#128506,#128507)),
 .UNSPECIFIED.,.F.,.F.,.F.)
B_SPLINE_SURFACE_WITH_KNOTS((2,2),(3,3),(0.,0.289807040992881),(0.521917529826137,
0.539102123117536),.UNSPECIFIED.)
GEOMETRIC_REPRESENTATION_ITEM()
RATIONAL_B_SPLINE_SURFACE(((0.98933476973119,0.987004571835915,0.987576759359605),
(0.98933476973119,0.987004571835915,0.987576759359605)))
REPRESENTATION_ITEM('')
SURFACE()
);
#2034=(
BOUNDED_SURFACE()
B_SPLINE_SURFACE(1,2,((#128509,#128510,#128511,#128512,#128513),(#128514,
#128515,#128516,#128517,#128518)),.UNSPECIFIED.,.F.,.F.,.F.)
B_SPLINE_SURFACE_WITH_KNOTS((2,2),(3,2,3),(0.,0.289948761105454),(0.194028469417325,
0.211502584834065,0.211770261742427),.UNSPECIFIED.)
GEOMETRIC_REPRESENTATION_ITEM()
RATIONAL_B_SPLINE_SURFACE(((0.989812124691679,0.992466718773227,0.998122319569323,
0.998122319569323,0.998122319569323),(0.989812124691679,0.992466718773227,
0.998122319569323,0.998122319569323,0.998122319569323)))
REPRESENTATION_ITEM('')
SURFACE()
);
#2035=(
BOUNDED_SURFACE()
B_SPLINE_SURFACE(1,2,((#128527,#128528,#128529),(#128530,#128531,#128532)),
 .UNSPECIFIED.,.F.,.F.,.F.)
B_SPLINE_SURFACE_WITH_KNOTS((2,2),(3,3),(0.,0.289807040992693),(0.521917529826141,
0.539102123117535),.UNSPECIFIED.)
GEOMETRIC_REPRESENTATION_ITEM()
RATIONAL_B_SPLINE_SURFACE(((0.989334769731189,0.987004571835916,0.987576759359605),
(0.989334769731189,0.987004571835916,0.987576759359605)))
REPRESENTATION_ITEM('')
SURFACE()
);
#2036=(
BOUNDED_SURFACE()
B_SPLINE_SURFACE(1,2,((#128534,#128535,#128536,#128537,#128538),(#128539,
#128540,#128541,#128542,#128543)),.UNSPECIFIED.,.F.,.F.,.F.)
B_SPLINE_SURFACE_WITH_KNOTS((2,2),(3,2,3),(0.,0.290289290033966),(0.194028469417325,
0.211502584834065,0.212110790670942),.UNSPECIFIED.)
GEOMETRIC_REPRESENTATION_ITEM()
RATIONAL_B_SPLINE_SURFACE(((0.989812124691679,0.992466718773227,0.998122319569322,
0.998122319569322,0.998122319569322),(0.989812124691679,0.992466718773227,
0.998122319569322,0.998122319569322,0.998122319569322)))
REPRESENTATION_ITEM('')
SURFACE()
);
#2037=(
BOUNDED_SURFACE()
B_SPLINE_SURFACE(1,2,((#128552,#128553,#128554),(#128555,#128556,#128557)),
 .UNSPECIFIED.,.F.,.F.,.F.)
B_SPLINE_SURFACE_WITH_KNOTS((2,2),(3,3),(0.,0.289807040993739),(0.521917529826141,
0.539102123117535),.UNSPECIFIED.)
GEOMETRIC_REPRESENTATION_ITEM()
RATIONAL_B_SPLINE_SURFACE(((0.989334769731189,0.987004571835916,0.987576759359605),
(0.989334769731189,0.987004571835916,0.987576759359605)))
REPRESENTATION_ITEM('')
SURFACE()
);
#2038=(
BOUNDED_SURFACE()
B_SPLINE_SURFACE(1,2,((#128559,#128560,#128561,#128562,#128563),(#128564,
#128565,#128566,#128567,#128568)),.UNSPECIFIED.,.F.,.F.,.F.)
B_SPLINE_SURFACE_WITH_KNOTS((2,2),(3,2,3),(0.,0.290289290019958),(0.194028469417325,
0.211502584834064,0.212110790656939),.UNSPECIFIED.)
GEOMETRIC_REPRESENTATION_ITEM()
RATIONAL_B_SPLINE_SURFACE(((0.989812124691679,0.992466718773227,0.998122319569322,
0.998122319569322,0.998122319569322),(0.989812124691679,0.992466718773227,
0.998122319569322,0.998122319569323,0.998122319569323)))
REPRESENTATION_ITEM('')
SURFACE()
);
#2039=(
BOUNDED_SURFACE()
B_SPLINE_SURFACE(1,2,((#128577,#128578,#128579),(#128580,#128581,#128582)),
 .UNSPECIFIED.,.F.,.F.,.F.)
B_SPLINE_SURFACE_WITH_KNOTS((2,2),(3,3),(0.,0.289807040991906),(0.521917529826141,
0.539102123117535),.UNSPECIFIED.)
GEOMETRIC_REPRESENTATION_ITEM()
RATIONAL_B_SPLINE_SURFACE(((0.989334769731189,0.987004571835916,0.987576759359605),
(0.989334769731189,0.987004571835916,0.987576759359605)))
REPRESENTATION_ITEM('')
SURFACE()
);
#2040=(
BOUNDED_SURFACE()
B_SPLINE_SURFACE(1,2,((#128584,#128585,#128586,#128587,#128588),(#128589,
#128590,#128591,#128592,#128593)),.UNSPECIFIED.,.F.,.F.,.F.)
B_SPLINE_SURFACE_WITH_KNOTS((2,2),(3,2,3),(0.,0.290289290009697),(0.194028469417325,
0.211502584834064,0.212110790646677),.UNSPECIFIED.)
GEOMETRIC_REPRESENTATION_ITEM()
RATIONAL_B_SPLINE_SURFACE(((0.989812124691679,0.992466718773227,0.998122319569322,
0.998122319569322,0.998122319569322),(0.989812124691679,0.992466718773227,
0.998122319569322,0.998122319569322,0.998122319569322)))
REPRESENTATION_ITEM('')
SURFACE()
);
#2041=(
BOUNDED_SURFACE()
B_SPLINE_SURFACE(1,2,((#128602,#128603,#128604),(#128605,#128606,#128607)),
 .UNSPECIFIED.,.F.,.F.,.F.)
B_SPLINE_SURFACE_WITH_KNOTS((2,2),(3,3),(0.,0.289807040993054),(0.521917529826141,
0.539102123117535),.UNSPECIFIED.)
GEOMETRIC_REPRESENTATION_ITEM()
RATIONAL_B_SPLINE_SURFACE(((0.989334769731189,0.987004571835916,0.987576759359605),
(0.989334769731189,0.987004571835916,0.987576759359605)))
REPRESENTATION_ITEM('')
SURFACE()
);
#2042=(
BOUNDED_SURFACE()
B_SPLINE_SURFACE(1,2,((#128609,#128610,#128611,#128612,#128613),(#128614,
#128615,#128616,#128617,#128618)),.UNSPECIFIED.,.F.,.F.,.F.)
B_SPLINE_SURFACE_WITH_KNOTS((2,2),(3,2,3),(0.,0.29028929002793),(0.194028469417325,
0.211502584834064,0.212110790664903),.UNSPECIFIED.)
GEOMETRIC_REPRESENTATION_ITEM()
RATIONAL_B_SPLINE_SURFACE(((0.989812124691679,0.992466718773227,0.998122319569322,
0.998122319569322,0.998122319569322),(0.989812124691679,0.992466718773227,
0.998122319569322,0.998122319569323,0.998122319569323)))
REPRESENTATION_ITEM('')
SURFACE()
);
#2043=(
BOUNDED_SURFACE()
B_SPLINE_SURFACE(1,2,((#128627,#128628,#128629),(#128630,#128631,#128632)),
 .UNSPECIFIED.,.F.,.F.,.F.)
B_SPLINE_SURFACE_WITH_KNOTS((2,2),(3,3),(0.,0.289807040992803),(0.521917529826141,
0.539102123117535),.UNSPECIFIED.)
GEOMETRIC_REPRESENTATION_ITEM()
RATIONAL_B_SPLINE_SURFACE(((0.989334769731189,0.987004571835916,0.987576759359605),
(0.989334769731189,0.987004571835916,0.987576759359605)))
REPRESENTATION_ITEM('')
SURFACE()
);
#2044=(
BOUNDED_SURFACE()
B_SPLINE_SURFACE(1,2,((#128634,#128635,#128636,#128637,#128638),(#128639,
#128640,#128641,#128642,#128643)),.UNSPECIFIED.,.F.,.F.,.F.)
B_SPLINE_SURFACE_WITH_KNOTS((2,2),(3,2,3),(0.,0.290289290034783),(0.194028469417325,
0.211502584834064,0.212110790671746),.UNSPECIFIED.)
GEOMETRIC_REPRESENTATION_ITEM()
RATIONAL_B_SPLINE_SURFACE(((0.989812124691679,0.992466718773227,0.998122319569322,
0.998122319569322,0.998122319569322),(0.989812124691679,0.992466718773227,
0.998122319569322,0.998122319569322,0.998122319569322)))
REPRESENTATION_ITEM('')
SURFACE()
);
#2045=(
BOUNDED_SURFACE()
B_SPLINE_SURFACE(1,2,((#128652,#128653,#128654),(#128655,#128656,#128657)),
 .UNSPECIFIED.,.F.,.F.,.F.)
B_SPLINE_SURFACE_WITH_KNOTS((2,2),(3,3),(0.,0.289807040993645),(0.521917529826128,
0.539102123117535),.UNSPECIFIED.)
GEOMETRIC_REPRESENTATION_ITEM()
RATIONAL_B_SPLINE_SURFACE(((0.989334769731192,0.987004571835915,0.987576759359605),
(0.989334769731192,0.987004571835915,0.987576759359605)))
REPRESENTATION_ITEM('')
SURFACE()
);
#2046=(
BOUNDED_SURFACE()
B_SPLINE_SURFACE(1,2,((#128659,#128660,#128661,#128662,#128663),(#128664,
#128665,#128666,#128667,#128668)),.UNSPECIFIED.,.F.,.F.,.F.)
B_SPLINE_SURFACE_WITH_KNOTS((2,2),(3,2,3),(0.,0.290289290037585),(0.194028469417326,
0.211502584834064,0.212110790674559),.UNSPECIFIED.)
GEOMETRIC_REPRESENTATION_ITEM()
RATIONAL_B_SPLINE_SURFACE(((0.989812124691679,0.992466718773227,0.998122319569322,
0.998122319569322,0.998122319569322),(0.989812124691679,0.992466718773227,
0.998122319569322,0.998122319569322,0.998122319569322)))
REPRESENTATION_ITEM('')
SURFACE()
);
#2047=(
BOUNDED_SURFACE()
B_SPLINE_SURFACE(1,2,((#128677,#128678,#128679),(#128680,#128681,#128682)),
 .UNSPECIFIED.,.F.,.F.,.F.)
B_SPLINE_SURFACE_WITH_KNOTS((2,2),(3,3),(0.,0.28980704099156),(0.52191752982614,
0.539102123117534),.UNSPECIFIED.)
GEOMETRIC_REPRESENTATION_ITEM()
RATIONAL_B_SPLINE_SURFACE(((0.989334769731189,0.987004571835916,0.987576759359605),
(0.989334769731189,0.987004571835916,0.987576759359605)))
REPRESENTATION_ITEM('')
SURFACE()
);
#2048=(
BOUNDED_SURFACE()
B_SPLINE_SURFACE(1,2,((#128684,#128685,#128686,#128687,#128688),(#128689,
#128690,#128691,#128692,#128693)),.UNSPECIFIED.,.F.,.F.,.F.)
B_SPLINE_SURFACE_WITH_KNOTS((2,2),(3,2,3),(0.,0.290289290026043),(0.194028469417326,
0.211502584834066,0.21211079066303),.UNSPECIFIED.)
GEOMETRIC_REPRESENTATION_ITEM()
RATIONAL_B_SPLINE_SURFACE(((0.989812124691679,0.992466718773227,0.998122319569323,
0.998122319569323,0.998122319569323),(0.989812124691679,0.992466718773227,
0.998122319569323,0.998122319569323,0.998122319569323)))
REPRESENTATION_ITEM('')
SURFACE()
);
#2049=(
BOUNDED_SURFACE()
B_SPLINE_SURFACE(1,2,((#128702,#128703,#128704),(#128705,#128706,#128707)),
 .UNSPECIFIED.,.F.,.F.,.F.)
B_SPLINE_SURFACE_WITH_KNOTS((2,2),(3,3),(0.,0.289807040991556),(0.52191752982614,
0.539102123117534),.UNSPECIFIED.)
GEOMETRIC_REPRESENTATION_ITEM()
RATIONAL_B_SPLINE_SURFACE(((0.989334769731189,0.987004571835916,0.987576759359605),
(0.989334769731189,0.987004571835916,0.987576759359605)))
REPRESENTATION_ITEM('')
SURFACE()
);
#2050=(
BOUNDED_SURFACE()
B_SPLINE_SURFACE(1,2,((#128709,#128710,#128711,#128712,#128713),(#128714,
#128715,#128716,#128717,#128718)),.UNSPECIFIED.,.F.,.F.,.F.)
B_SPLINE_SURFACE_WITH_KNOTS((2,2),(3,2,3),(0.,0.289681084359917),(0.469916319328034,
0.487259899888159,0.48743333569376),.UNSPECIFIED.)
GEOMETRIC_REPRESENTATION_ITEM()
RATIONAL_B_SPLINE_SURFACE(((0.987775548376701,0.988735325500096,0.992651440660746,
0.992651440660746,0.992651440660746),(0.987775548376701,0.988735325500096,
0.992651440660745,0.992651440660745,0.992651440660745)))
REPRESENTATION_ITEM('')
SURFACE()
);
#2051=(
BOUNDED_SURFACE()
B_SPLINE_SURFACE(1,2,((#128729,#128730,#128731,#128732,#128733),(#128734,
#128735,#128736,#128737,#128738)),.UNSPECIFIED.,.F.,.F.,.F.)
B_SPLINE_SURFACE_WITH_KNOTS((2,2),(3,2,3),(0.,0.290401167136834),(0.245359924934102,
0.245954053070908,0.263201868951011),.UNSPECIFIED.)
GEOMETRIC_REPRESENTATION_ITEM()
RATIONAL_B_SPLINE_SURFACE(((0.987624841600687,0.987624841600687,0.987624841600687,
0.986938988894508,0.989176916802451),(0.987624841600687,0.987624841600687,
0.987624841600687,0.986938988894508,0.989176916802451)))
REPRESENTATION_ITEM('')
SURFACE()
);
#2052=(
BOUNDED_SURFACE()
B_SPLINE_SURFACE(1,2,((#128755,#128756,#128757,#128758,#128759),(#128760,
#128761,#128762,#128763,#128764)),.UNSPECIFIED.,.F.,.F.,.F.)
B_SPLINE_SURFACE_WITH_KNOTS((2,2),(3,2,3),(0.,0.289681084359941),(0.469916319328034,
0.487259899888159,0.48743333569376),.UNSPECIFIED.)
GEOMETRIC_REPRESENTATION_ITEM()
RATIONAL_B_SPLINE_SURFACE(((0.987775548376701,0.988735325500096,0.992651440660746,
0.992651440660746,0.992651440660746),(0.987775548376701,0.988735325500096,
0.992651440660746,0.992651440660746,0.992651440660746)))
REPRESENTATION_ITEM('')
SURFACE()
);
#2053=(
BOUNDED_SURFACE()
B_SPLINE_SURFACE(1,2,((#128766,#128767,#128768,#128769,#128770),(#128771,
#128772,#128773,#128774,#128775)),.UNSPECIFIED.,.F.,.F.,.F.)
B_SPLINE_SURFACE_WITH_KNOTS((2,2),(3,2,3),(0.,0.290401167093823),(0.245359924977154,
0.245954053070908,0.263201868951011),.UNSPECIFIED.)
GEOMETRIC_REPRESENTATION_ITEM()
RATIONAL_B_SPLINE_SURFACE(((0.987624841600687,0.987624841600687,0.987624841600687,
0.986938988894508,0.989176916802451),(0.987624841600687,0.987624841600687,
0.987624841600687,0.986938988894508,0.989176916802451)))
REPRESENTATION_ITEM('')
SURFACE()
);
#2054=(
BOUNDED_SURFACE()
B_SPLINE_SURFACE(1,2,((#128792,#128793,#128794,#128795,#128796),(#128797,
#128798,#128799,#128800,#128801)),.UNSPECIFIED.,.F.,.F.,.F.)
B_SPLINE_SURFACE_WITH_KNOTS((2,2),(3,2,3),(0.,0.289681084359923),(0.469916319328034,
0.487259899888159,0.48743333569376),.UNSPECIFIED.)
GEOMETRIC_REPRESENTATION_ITEM()
RATIONAL_B_SPLINE_SURFACE(((0.987775548376701,0.988735325500096,0.992651440660746,
0.992651440660746,0.992651440660746),(0.987775548376701,0.988735325500096,
0.992651440660746,0.992651440660746,0.992651440660746)))
REPRESENTATION_ITEM('')
SURFACE()
);
#2055=(
BOUNDED_SURFACE()
B_SPLINE_SURFACE(1,2,((#128803,#128804,#128805,#128806,#128807),(#128808,
#128809,#128810,#128811,#128812)),.UNSPECIFIED.,.F.,.F.,.F.)
B_SPLINE_SURFACE_WITH_KNOTS((2,2),(3,2,3),(0.,0.290401167129692),(0.245359924941374,
0.245954053070908,0.263201868951011),.UNSPECIFIED.)
GEOMETRIC_REPRESENTATION_ITEM()
RATIONAL_B_SPLINE_SURFACE(((0.987624841600687,0.987624841600687,0.987624841600687,
0.986938988894508,0.989176916802451),(0.987624841600687,0.987624841600687,
0.987624841600687,0.986938988894508,0.989176916802451)))
REPRESENTATION_ITEM('')
SURFACE()
);
#2056=(
BOUNDED_SURFACE()
B_SPLINE_SURFACE(1,2,((#128829,#128830,#128831,#128832,#128833),(#128834,
#128835,#128836,#128837,#128838)),.UNSPECIFIED.,.F.,.F.,.F.)
B_SPLINE_SURFACE_WITH_KNOTS((2,2),(3,2,3),(0.,0.289681084359927),(0.469916319328034,
0.487259899888159,0.48743333569376),.UNSPECIFIED.)
GEOMETRIC_REPRESENTATION_ITEM()
RATIONAL_B_SPLINE_SURFACE(((0.987775548376701,0.988735325500096,0.992651440660745,
0.992651440660745,0.992651440660745),(0.987775548376701,0.988735325500096,
0.992651440660745,0.992651440660745,0.992651440660745)))
REPRESENTATION_ITEM('')
SURFACE()
);
#2057=(
BOUNDED_SURFACE()
B_SPLINE_SURFACE(1,2,((#128840,#128841,#128842,#128843,#128844),(#128845,
#128846,#128847,#128848,#128849)),.UNSPECIFIED.,.F.,.F.,.F.)
B_SPLINE_SURFACE_WITH_KNOTS((2,2),(3,2,3),(0.,0.290401167115997),(0.245359924955159,
0.245954053070908,0.263201868951011),.UNSPECIFIED.)
GEOMETRIC_REPRESENTATION_ITEM()
RATIONAL_B_SPLINE_SURFACE(((0.987624841600687,0.987624841600687,0.987624841600687,
0.986938988894508,0.989176916802451),(0.987624841600687,0.987624841600687,
0.987624841600687,0.986938988894507,0.989176916802451)))
REPRESENTATION_ITEM('')
SURFACE()
);
#2058=(
BOUNDED_SURFACE()
B_SPLINE_SURFACE(1,2,((#128866,#128867,#128868,#128869,#128870),(#128871,
#128872,#128873,#128874,#128875)),.UNSPECIFIED.,.F.,.F.,.F.)
B_SPLINE_SURFACE_WITH_KNOTS((2,2),(3,2,3),(0.,0.289681084359927),(0.469916319328034,
0.487259899888159,0.48743333569376),.UNSPECIFIED.)
GEOMETRIC_REPRESENTATION_ITEM()
RATIONAL_B_SPLINE_SURFACE(((0.987775548376701,0.988735325500096,0.992651440660746,
0.992651440660746,0.992651440660746),(0.987775548376701,0.988735325500096,
0.992651440660746,0.992651440660746,0.992651440660746)))
REPRESENTATION_ITEM('')
SURFACE()
);
#2059=(
BOUNDED_SURFACE()
B_SPLINE_SURFACE(1,2,((#128877,#128878,#128879,#128880,#128881),(#128882,
#128883,#128884,#128885,#128886)),.UNSPECIFIED.,.F.,.F.,.F.)
B_SPLINE_SURFACE_WITH_KNOTS((2,2),(3,2,3),(0.,0.290401167122636),(0.245359924948379,
0.245954053070908,0.263201868951011),.UNSPECIFIED.)
GEOMETRIC_REPRESENTATION_ITEM()
RATIONAL_B_SPLINE_SURFACE(((0.987624841600687,0.987624841600687,0.987624841600687,
0.986938988894508,0.989176916802451),(0.987624841600687,0.987624841600687,
0.987624841600687,0.986938988894508,0.989176916802451)))
REPRESENTATION_ITEM('')
SURFACE()
);
#2060=(
BOUNDED_SURFACE()
B_SPLINE_SURFACE(1,2,((#128903,#128904,#128905,#128906,#128907),(#128908,
#128909,#128910,#128911,#128912)),.UNSPECIFIED.,.F.,.F.,.F.)
B_SPLINE_SURFACE_WITH_KNOTS((2,2),(3,2,3),(0.,0.289681084359917),(0.469916319328034,
0.487259899888159,0.48743333569376),.UNSPECIFIED.)
GEOMETRIC_REPRESENTATION_ITEM()
RATIONAL_B_SPLINE_SURFACE(((0.987775548376701,0.988735325500096,0.992651440660746,
0.992651440660746,0.992651440660746),(0.987775548376701,0.988735325500096,
0.992651440660746,0.992651440660746,0.992651440660746)))
REPRESENTATION_ITEM('')
SURFACE()
);
#2061=(
BOUNDED_SURFACE()
B_SPLINE_SURFACE(1,2,((#128914,#128915,#128916,#128917,#128918),(#128919,
#128920,#128921,#128922,#128923)),.UNSPECIFIED.,.F.,.F.,.F.)
B_SPLINE_SURFACE_WITH_KNOTS((2,2),(3,2,3),(0.,0.290401167100094),(0.245359924970891,
0.245954053070908,0.263201868951011),.UNSPECIFIED.)
GEOMETRIC_REPRESENTATION_ITEM()
RATIONAL_B_SPLINE_SURFACE(((0.987624841600687,0.987624841600687,0.987624841600687,
0.986938988894508,0.989176916802451),(0.987624841600687,0.987624841600687,
0.987624841600687,0.986938988894508,0.989176916802451)))
REPRESENTATION_ITEM('')
SURFACE()
);
#2062=(
BOUNDED_SURFACE()
B_SPLINE_SURFACE(1,2,((#128940,#128941,#128942,#128943,#128944),(#128945,
#128946,#128947,#128948,#128949)),.UNSPECIFIED.,.F.,.F.,.F.)
B_SPLINE_SURFACE_WITH_KNOTS((2,2),(3,2,3),(0.,0.289681084359919),(0.469916319328034,
0.487259899888159,0.48743333569376),.UNSPECIFIED.)
GEOMETRIC_REPRESENTATION_ITEM()
RATIONAL_B_SPLINE_SURFACE(((0.987775548376701,0.988735325500096,0.992651440660746,
0.992651440660746,0.992651440660746),(0.987775548376701,0.988735325500096,
0.992651440660746,0.992651440660746,0.992651440660746)))
REPRESENTATION_ITEM('')
SURFACE()
);
#2063=(
BOUNDED_SURFACE()
B_SPLINE_SURFACE(1,2,((#128951,#128952,#128953,#128954,#128955),(#128956,
#128957,#128958,#128959,#128960)),.UNSPECIFIED.,.F.,.F.,.F.)
B_SPLINE_SURFACE_WITH_KNOTS((2,2),(3,2,3),(0.,0.290401167107786),(0.245359924963182,
0.245954053070908,0.263201868951011),.UNSPECIFIED.)
GEOMETRIC_REPRESENTATION_ITEM()
RATIONAL_B_SPLINE_SURFACE(((0.987624841600687,0.987624841600687,0.987624841600687,
0.986938988894508,0.989176916802451),(0.987624841600687,0.987624841600687,
0.987624841600687,0.986938988894508,0.989176916802451)))
REPRESENTATION_ITEM('')
SURFACE()
);
#2064=(
BOUNDED_SURFACE()
B_SPLINE_SURFACE(1,2,((#128968,#128969,#128970,#128971,#128972),(#128973,
#128974,#128975,#128976,#128977)),.UNSPECIFIED.,.F.,.F.,.F.)
B_SPLINE_SURFACE_WITH_KNOTS((2,2),(3,2,3),(0.,0.289681084359914),(0.469916319328034,
0.487259899888159,0.48743333569376),.UNSPECIFIED.)
GEOMETRIC_REPRESENTATION_ITEM()
RATIONAL_B_SPLINE_SURFACE(((0.987775548376701,0.988735325500096,0.992651440660746,
0.992651440660746,0.992651440660746),(0.987775548376701,0.988735325500096,
0.992651440660745,0.992651440660745,0.992651440660745)))
REPRESENTATION_ITEM('')
SURFACE()
);
#2065=(
BOUNDED_SURFACE()
B_SPLINE_SURFACE(1,2,((#128979,#128980,#128981,#128982,#128983),(#128984,
#128985,#128986,#128987,#128988)),.UNSPECIFIED.,.F.,.F.,.F.)
B_SPLINE_SURFACE_WITH_KNOTS((2,2),(3,2,3),(0.,0.290401167130326),(0.245359924940621,
0.245954053070908,0.263201868951011),.UNSPECIFIED.)
GEOMETRIC_REPRESENTATION_ITEM()
RATIONAL_B_SPLINE_SURFACE(((0.987624841600687,0.987624841600687,0.987624841600687,
0.986938988894507,0.989176916802451),(0.987624841600687,0.987624841600687,
0.987624841600687,0.986938988894507,0.989176916802451)))
REPRESENTATION_ITEM('')
SURFACE()
);
#2066=(
BOUNDED_SURFACE()
B_SPLINE_SURFACE(1,2,((#129005,#129006,#129007,#129008,#129009),(#129010,
#129011,#129012,#129013,#129014)),.UNSPECIFIED.,.F.,.F.,.F.)
B_SPLINE_SURFACE_WITH_KNOTS((2,2),(3,2,3),(0.,0.289681084359921),(0.469916319328034,
0.487259899888159,0.48743333569376),.UNSPECIFIED.)
GEOMETRIC_REPRESENTATION_ITEM()
RATIONAL_B_SPLINE_SURFACE(((0.987775548376701,0.988735325500096,0.992651440660746,
0.992651440660746,0.992651440660746),(0.987775548376701,0.988735325500096,
0.992651440660746,0.992651440660746,0.992651440660746)))
REPRESENTATION_ITEM('')
SURFACE()
);
#2067=(
BOUNDED_SURFACE()
B_SPLINE_SURFACE(1,2,((#129016,#129017,#129018,#129019,#129020),(#129021,
#129022,#129023,#129024,#129025)),.UNSPECIFIED.,.F.,.F.,.F.)
B_SPLINE_SURFACE_WITH_KNOTS((2,2),(3,2,3),(0.,0.290401167111664),(0.245359924959248,
0.245954053070908,0.263201868951011),.UNSPECIFIED.)
GEOMETRIC_REPRESENTATION_ITEM()
RATIONAL_B_SPLINE_SURFACE(((0.987624841600687,0.987624841600687,0.987624841600687,
0.986938988894507,0.989176916802451),(0.987624841600687,0.987624841600687,
0.987624841600687,0.986938988894508,0.989176916802451)))
REPRESENTATION_ITEM('')
SURFACE()
);
#2068=(
BOUNDED_SURFACE()
B_SPLINE_SURFACE(1,2,((#129042,#129043,#129044,#129045,#129046),(#129047,
#129048,#129049,#129050,#129051)),.UNSPECIFIED.,.F.,.F.,.F.)
B_SPLINE_SURFACE_WITH_KNOTS((2,2),(3,2,3),(0.,0.289681084359923),(0.469916319328034,
0.487259899888159,0.48743333569376),.UNSPECIFIED.)
GEOMETRIC_REPRESENTATION_ITEM()
RATIONAL_B_SPLINE_SURFACE(((0.987775548376701,0.988735325500096,0.992651440660746,
0.992651440660746,0.992651440660746),(0.987775548376701,0.988735325500096,
0.992651440660746,0.992651440660746,0.992651440660746)))
REPRESENTATION_ITEM('')
SURFACE()
);
#2069=(
BOUNDED_SURFACE()
B_SPLINE_SURFACE(1,2,((#129053,#129054,#129055,#129056,#129057),(#129058,
#129059,#129060,#129061,#129062)),.UNSPECIFIED.,.F.,.F.,.F.)
B_SPLINE_SURFACE_WITH_KNOTS((2,2),(3,2,3),(0.,0.290401167139708),(0.245359924931369,
0.245954053070908,0.263201868951016),.UNSPECIFIED.)
GEOMETRIC_REPRESENTATION_ITEM()
RATIONAL_B_SPLINE_SURFACE(((0.987624841600687,0.987624841600687,0.987624841600687,
0.986938988894507,0.989176916802452),(0.987624841600687,0.987624841600687,
0.987624841600687,0.986938988894507,0.989176916802452)))
REPRESENTATION_ITEM('')
SURFACE()
);
#2070=(
BOUNDED_SURFACE()
B_SPLINE_SURFACE(1,2,((#129079,#129080,#129081,#129082,#129083),(#129084,
#129085,#129086,#129087,#129088)),.UNSPECIFIED.,.F.,.F.,.F.)
B_SPLINE_SURFACE_WITH_KNOTS((2,2),(3,2,3),(0.,0.289681084359925),(0.469916319328038,
0.487259899888159,0.48743333569376),.UNSPECIFIED.)
GEOMETRIC_REPRESENTATION_ITEM()
RATIONAL_B_SPLINE_SURFACE(((0.987775548376701,0.988735325500097,0.992651440660745,
0.992651440660745,0.992651440660745),(0.987775548376701,0.988735325500097,
0.992651440660745,0.992651440660745,0.992651440660745)))
REPRESENTATION_ITEM('')
SURFACE()
);
#2071=(
BOUNDED_SURFACE()
B_SPLINE_SURFACE(1,2,((#129090,#129091,#129092,#129093,#129094),(#129095,
#129096,#129097,#129098,#129099)),.UNSPECIFIED.,.F.,.F.,.F.)
B_SPLINE_SURFACE_WITH_KNOTS((2,2),(3,2,3),(0.,0.290401167093765),(0.245359924977085,
0.245954053070908,0.263201868951013),.UNSPECIFIED.)
GEOMETRIC_REPRESENTATION_ITEM()
RATIONAL_B_SPLINE_SURFACE(((0.987624841600687,0.987624841600687,0.987624841600687,
0.986938988894508,0.989176916802451),(0.987624841600687,0.987624841600687,
0.987624841600687,0.986938988894508,0.989176916802451)))
REPRESENTATION_ITEM('')
SURFACE()
);
#2072=(
BOUNDED_SURFACE()
B_SPLINE_SURFACE(1,2,((#129116,#129117,#129118,#129119,#129120),(#129121,
#129122,#129123,#129124,#129125)),.UNSPECIFIED.,.F.,.F.,.F.)
B_SPLINE_SURFACE_WITH_KNOTS((2,2),(3,2,3),(0.,0.289681084359923),(0.469916319328036,
0.487259899888159,0.48743333569376),.UNSPECIFIED.)
GEOMETRIC_REPRESENTATION_ITEM()
RATIONAL_B_SPLINE_SURFACE(((0.987775548376701,0.988735325500096,0.992651440660745,
0.992651440660745,0.992651440660745),(0.987775548376701,0.988735325500096,
0.992651440660745,0.992651440660745,0.992651440660745)))
REPRESENTATION_ITEM('')
SURFACE()
);
#2073=(
BOUNDED_SURFACE()
B_SPLINE_SURFACE(1,2,((#129127,#129128,#129129,#129130,#129131),(#129132,
#129133,#129134,#129135,#129136)),.UNSPECIFIED.,.F.,.F.,.F.)
B_SPLINE_SURFACE_WITH_KNOTS((2,2),(3,2,3),(0.,0.290401167125862),(0.245359924945024,
0.245954053070908,0.263201868951011),.UNSPECIFIED.)
GEOMETRIC_REPRESENTATION_ITEM()
RATIONAL_B_SPLINE_SURFACE(((0.987624841600687,0.987624841600687,0.987624841600687,
0.986938988894508,0.989176916802451),(0.987624841600687,0.987624841600687,
0.987624841600687,0.986938988894508,0.989176916802451)))
REPRESENTATION_ITEM('')
SURFACE()
);
#2074=(
BOUNDED_SURFACE()
B_SPLINE_SURFACE(1,2,((#129153,#129154,#129155,#129156,#129157),(#129158,
#129159,#129160,#129161,#129162)),.UNSPECIFIED.,.F.,.F.,.F.)
B_SPLINE_SURFACE_WITH_KNOTS((2,2),(3,2,3),(0.,0.289681084359923),(0.469916319328034,
0.48725989988816,0.487433335693761),.UNSPECIFIED.)
GEOMETRIC_REPRESENTATION_ITEM()
RATIONAL_B_SPLINE_SURFACE(((0.987775548376701,0.988735325500096,0.992651440660746,
0.992651440660746,0.992651440660746),(0.987775548376701,0.988735325500096,
0.992651440660746,0.992651440660746,0.992651440660746)))
REPRESENTATION_ITEM('')
SURFACE()
);
#2075=(
BOUNDED_SURFACE()
B_SPLINE_SURFACE(1,2,((#129164,#129165,#129166,#129167,#129168),(#129169,
#129170,#129171,#129172,#129173)),.UNSPECIFIED.,.F.,.F.,.F.)
B_SPLINE_SURFACE_WITH_KNOTS((2,2),(3,2,3),(0.,0.290401167139431),(0.245359924931563,
0.245954053070908,0.263201868951011),.UNSPECIFIED.)
GEOMETRIC_REPRESENTATION_ITEM()
RATIONAL_B_SPLINE_SURFACE(((0.987624841600687,0.987624841600687,0.987624841600687,
0.986938988894508,0.989176916802451),(0.987624841600687,0.987624841600687,
0.987624841600687,0.986938988894508,0.989176916802451)))
REPRESENTATION_ITEM('')
SURFACE()
);
#2076=(
BOUNDED_SURFACE()
B_SPLINE_SURFACE(1,2,((#129190,#129191,#129192,#129193,#129194),(#129195,
#129196,#129197,#129198,#129199)),.UNSPECIFIED.,.F.,.F.,.F.)
B_SPLINE_SURFACE_WITH_KNOTS((2,2),(3,2,3),(0.,0.289681084359921),(0.469916319328034,
0.487259899888159,0.48743333569376),.UNSPECIFIED.)
GEOMETRIC_REPRESENTATION_ITEM()
RATIONAL_B_SPLINE_SURFACE(((0.987775548376701,0.988735325500096,0.992651440660745,
0.992651440660745,0.992651440660745),(0.987775548376701,0.988735325500096,
0.992651440660745,0.992651440660745,0.992651440660745)))
REPRESENTATION_ITEM('')
SURFACE()
);
#2077=(
BOUNDED_SURFACE()
B_SPLINE_SURFACE(1,2,((#129201,#129202,#129203,#129204,#129205),(#129206,
#129207,#129208,#129209,#129210)),.UNSPECIFIED.,.F.,.F.,.F.)
B_SPLINE_SURFACE_WITH_KNOTS((2,2),(3,2,3),(0.,0.290401167098445),(0.245359924972439,
0.245954053070908,0.263201868951011),.UNSPECIFIED.)
GEOMETRIC_REPRESENTATION_ITEM()
RATIONAL_B_SPLINE_SURFACE(((0.987624841600687,0.987624841600687,0.987624841600687,
0.986938988894508,0.989176916802451),(0.987624841600687,0.987624841600687,
0.987624841600687,0.986938988894508,0.989176916802451)))
REPRESENTATION_ITEM('')
SURFACE()
);
#2078=(
BOUNDED_SURFACE()
B_SPLINE_SURFACE(1,2,((#129227,#129228,#129229,#129230,#129231),(#129232,
#129233,#129234,#129235,#129236)),.UNSPECIFIED.,.F.,.F.,.F.)
B_SPLINE_SURFACE_WITH_KNOTS((2,2),(3,2,3),(0.,0.289681084359924),(0.469916319328034,
0.487259899888159,0.48743333569376),.UNSPECIFIED.)
GEOMETRIC_REPRESENTATION_ITEM()
RATIONAL_B_SPLINE_SURFACE(((0.987775548376701,0.988735325500096,0.992651440660746,
0.992651440660746,0.992651440660746),(0.987775548376701,0.988735325500096,
0.992651440660746,0.992651440660746,0.992651440660746)))
REPRESENTATION_ITEM('')
SURFACE()
);
#2079=(
BOUNDED_SURFACE()
B_SPLINE_SURFACE(1,2,((#129238,#129239,#129240,#129241,#129242),(#129243,
#129244,#129245,#129246,#129247)),.UNSPECIFIED.,.F.,.F.,.F.)
B_SPLINE_SURFACE_WITH_KNOTS((2,2),(3,2,3),(0.,0.290401167125722),(0.245359924945411,
0.245954053070908,0.263201868951011),.UNSPECIFIED.)
GEOMETRIC_REPRESENTATION_ITEM()
RATIONAL_B_SPLINE_SURFACE(((0.987624841600687,0.987624841600687,0.987624841600687,
0.986938988894508,0.989176916802451),(0.987624841600687,0.987624841600687,
0.987624841600687,0.986938988894508,0.989176916802451)))
REPRESENTATION_ITEM('')
SURFACE()
);
#2080=(
BOUNDED_SURFACE()
B_SPLINE_SURFACE(1,2,((#129264,#129265,#129266,#129267,#129268),(#129269,
#129270,#129271,#129272,#129273)),.UNSPECIFIED.,.F.,.F.,.F.)
B_SPLINE_SURFACE_WITH_KNOTS((2,2),(3,2,3),(0.,0.289681084359924),(0.469916319328034,
0.48725989988816,0.487433335693761),.UNSPECIFIED.)
GEOMETRIC_REPRESENTATION_ITEM()
RATIONAL_B_SPLINE_SURFACE(((0.987775548376701,0.988735325500096,0.992651440660746,
0.992651440660746,0.992651440660746),(0.987775548376701,0.988735325500096,
0.992651440660746,0.992651440660746,0.992651440660746)))
REPRESENTATION_ITEM('')
SURFACE()
);
#2081=(
BOUNDED_SURFACE()
B_SPLINE_SURFACE(1,2,((#129275,#129276,#129277,#129278,#129279),(#129280,
#129281,#129282,#129283,#129284)),.UNSPECIFIED.,.F.,.F.,.F.)
B_SPLINE_SURFACE_WITH_KNOTS((2,2),(3,2,3),(0.,0.290401167113126),(0.24535992495785,
0.245954053070908,0.263201868951011),.UNSPECIFIED.)
GEOMETRIC_REPRESENTATION_ITEM()
RATIONAL_B_SPLINE_SURFACE(((0.987624841600687,0.987624841600687,0.987624841600687,
0.986938988894508,0.989176916802451),(0.987624841600687,0.987624841600687,
0.987624841600687,0.986938988894508,0.989176916802451)))
REPRESENTATION_ITEM('')
SURFACE()
);
#2082=(
BOUNDED_SURFACE()
B_SPLINE_SURFACE(1,2,((#129301,#129302,#129303,#129304,#129305),(#129306,
#129307,#129308,#129309,#129310)),.UNSPECIFIED.,.F.,.F.,.F.)
B_SPLINE_SURFACE_WITH_KNOTS((2,2),(3,2,3),(0.,0.289681084359923),(0.469916319328034,
0.487259899888159,0.48743333569376),.UNSPECIFIED.)
GEOMETRIC_REPRESENTATION_ITEM()
RATIONAL_B_SPLINE_SURFACE(((0.987775548376701,0.988735325500096,0.992651440660746,
0.992651440660746,0.992651440660746),(0.987775548376701,0.988735325500096,
0.992651440660746,0.992651440660746,0.992651440660746)))
REPRESENTATION_ITEM('')
SURFACE()
);
#2083=(
BOUNDED_SURFACE()
B_SPLINE_SURFACE(1,2,((#129312,#129313,#129314,#129315,#129316),(#129317,
#129318,#129319,#129320,#129321)),.UNSPECIFIED.,.F.,.F.,.F.)
B_SPLINE_SURFACE_WITH_KNOTS((2,2),(3,2,3),(0.,0.290401167145354),(0.245359924925784,
0.245954053070908,0.263201868951011),.UNSPECIFIED.)
GEOMETRIC_REPRESENTATION_ITEM()
RATIONAL_B_SPLINE_SURFACE(((0.987624841600687,0.987624841600687,0.987624841600687,
0.986938988894508,0.989176916802451),(0.987624841600687,0.987624841600687,
0.987624841600687,0.986938988894508,0.989176916802451)))
REPRESENTATION_ITEM('')
SURFACE()
);
#2084=(
BOUNDED_SURFACE()
B_SPLINE_SURFACE(1,2,((#129338,#129339,#129340,#129341,#129342),(#129343,
#129344,#129345,#129346,#129347)),.UNSPECIFIED.,.F.,.F.,.F.)
B_SPLINE_SURFACE_WITH_KNOTS((2,2),(3,2,3),(0.,0.289681084359931),(0.469916319328034,
0.487259899888159,0.48743333569376),.UNSPECIFIED.)
GEOMETRIC_REPRESENTATION_ITEM()
RATIONAL_B_SPLINE_SURFACE(((0.987775548376701,0.988735325500096,0.992651440660746,
0.992651440660746,0.992651440660746),(0.987775548376701,0.988735325500096,
0.992651440660746,0.992651440660746,0.992651440660746)))
REPRESENTATION_ITEM('')
SURFACE()
);
#2085=(
BOUNDED_SURFACE()
B_SPLINE_SURFACE(1,2,((#129349,#129350,#129351,#129352,#129353),(#129354,
#129355,#129356,#129357,#129358)),.UNSPECIFIED.,.F.,.F.,.F.)
B_SPLINE_SURFACE_WITH_KNOTS((2,2),(3,2,3),(0.,0.290401167104879),(0.245359924965993,
0.245954053070908,0.263201868951011),.UNSPECIFIED.)
GEOMETRIC_REPRESENTATION_ITEM()
RATIONAL_B_SPLINE_SURFACE(((0.987624841600687,0.987624841600687,0.987624841600687,
0.986938988894508,0.989176916802451),(0.987624841600687,0.987624841600687,
0.987624841600687,0.986938988894508,0.989176916802451)))
REPRESENTATION_ITEM('')
SURFACE()
);
#2086=(
BOUNDED_SURFACE()
B_SPLINE_SURFACE(1,2,((#129375,#129376,#129377,#129378,#129379),(#129380,
#129381,#129382,#129383,#129384)),.UNSPECIFIED.,.F.,.F.,.F.)
B_SPLINE_SURFACE_WITH_KNOTS((2,2),(3,2,3),(0.,0.289681084359923),(0.469916319328034,
0.487259899888159,0.48743333569376),.UNSPECIFIED.)
GEOMETRIC_REPRESENTATION_ITEM()
RATIONAL_B_SPLINE_SURFACE(((0.987775548376701,0.988735325500096,0.992651440660746,
0.992651440660746,0.992651440660746),(0.987775548376701,0.988735325500096,
0.992651440660746,0.992651440660746,0.992651440660746)))
REPRESENTATION_ITEM('')
SURFACE()
);
#2087=(
BOUNDED_SURFACE()
B_SPLINE_SURFACE(1,2,((#129386,#129387,#129388,#129389,#129390),(#129391,
#129392,#129393,#129394,#129395)),.UNSPECIFIED.,.F.,.F.,.F.)
B_SPLINE_SURFACE_WITH_KNOTS((2,2),(3,2,3),(0.,0.290401167103061),(0.245359924967892,
0.245954053070908,0.263201868951011),.UNSPECIFIED.)
GEOMETRIC_REPRESENTATION_ITEM()
RATIONAL_B_SPLINE_SURFACE(((0.987624841600687,0.987624841600687,0.987624841600687,
0.986938988894507,0.989176916802451),(0.987624841600687,0.987624841600687,
0.987624841600687,0.986938988894508,0.989176916802451)))
REPRESENTATION_ITEM('')
SURFACE()
);
#2088=(
BOUNDED_SURFACE()
B_SPLINE_SURFACE(1,2,((#129412,#129413,#129414,#129415,#129416),(#129417,
#129418,#129419,#129420,#129421)),.UNSPECIFIED.,.F.,.F.,.F.)
B_SPLINE_SURFACE_WITH_KNOTS((2,2),(3,2,3),(0.,0.28968108435992),(0.469916319328034,
0.487259899888159,0.48743333569376),.UNSPECIFIED.)
GEOMETRIC_REPRESENTATION_ITEM()
RATIONAL_B_SPLINE_SURFACE(((0.987775548376701,0.988735325500096,0.992651440660746,
0.992651440660746,0.992651440660746),(0.987775548376701,0.988735325500096,
0.992651440660746,0.992651440660746,0.992651440660746)))
REPRESENTATION_ITEM('')
SURFACE()
);
#2089=(
BOUNDED_SURFACE()
B_SPLINE_SURFACE(1,2,((#129423,#129424,#129425,#129426,#129427),(#129428,
#129429,#129430,#129431,#129432)),.UNSPECIFIED.,.F.,.F.,.F.)
B_SPLINE_SURFACE_WITH_KNOTS((2,2),(3,2,3),(0.,0.290401167141549),(0.245359924929602,
0.245954053070908,0.263201868951011),.UNSPECIFIED.)
GEOMETRIC_REPRESENTATION_ITEM()
RATIONAL_B_SPLINE_SURFACE(((0.987624841600687,0.987624841600687,0.987624841600687,
0.986938988894508,0.989176916802451),(0.987624841600687,0.987624841600687,
0.987624841600687,0.986938988894508,0.989176916802451)))
REPRESENTATION_ITEM('')
SURFACE()
);
#2090=(
BOUNDED_SURFACE()
B_SPLINE_SURFACE(1,2,((#129449,#129450,#129451,#129452,#129453),(#129454,
#129455,#129456,#129457,#129458)),.UNSPECIFIED.,.F.,.F.,.F.)
B_SPLINE_SURFACE_WITH_KNOTS((2,2),(3,2,3),(0.,0.289681084359919),(0.469916319328034,
0.487259899888159,0.48743333569376),.UNSPECIFIED.)
GEOMETRIC_REPRESENTATION_ITEM()
RATIONAL_B_SPLINE_SURFACE(((0.987775548376701,0.988735325500096,0.992651440660746,
0.992651440660746,0.992651440660746),(0.987775548376701,0.988735325500096,
0.992651440660746,0.992651440660746,0.992651440660746)))
REPRESENTATION_ITEM('')
SURFACE()
);
#2091=(
BOUNDED_SURFACE()
B_SPLINE_SURFACE(1,2,((#129460,#129461,#129462,#129463,#129464),(#129465,
#129466,#129467,#129468,#129469)),.UNSPECIFIED.,.F.,.F.,.F.)
B_SPLINE_SURFACE_WITH_KNOTS((2,2),(3,2,3),(0.,0.290401167496561),(0.245359925137882,
0.245954053070908,0.263201868951011),.UNSPECIFIED.)
GEOMETRIC_REPRESENTATION_ITEM()
RATIONAL_B_SPLINE_SURFACE(((0.987624841600687,0.987624841600687,0.987624841600687,
0.986938988894508,0.989176916802451),(0.987624841600687,0.987624841600687,
0.987624841600687,0.986938988894508,0.989176916802451)))
REPRESENTATION_ITEM('')
SURFACE()
);
#2092=(
BOUNDED_SURFACE()
B_SPLINE_SURFACE(1,2,((#129480,#129481,#129482,#129483,#129484),(#129485,
#129486,#129487,#129488,#129489)),.UNSPECIFIED.,.F.,.F.,.F.)
B_SPLINE_SURFACE_WITH_KNOTS((2,2),(3,2,3),(0.,0.289681084359921),(0.469916319328034,
0.487259899888159,0.48743333569376),.UNSPECIFIED.)
GEOMETRIC_REPRESENTATION_ITEM()
RATIONAL_B_SPLINE_SURFACE(((0.987775548376701,0.988735325500096,0.992651440660746,
0.992651440660746,0.992651440660746),(0.987775548376701,0.988735325500096,
0.992651440660746,0.992651440660746,0.992651440660746)))
REPRESENTATION_ITEM('')
SURFACE()
);
#2093=(
BOUNDED_SURFACE()
B_SPLINE_SURFACE(1,2,((#129497,#129498,#129499,#129500,#129501),(#129502,
#129503,#129504,#129505,#129506)),.UNSPECIFIED.,.F.,.F.,.F.)
B_SPLINE_SURFACE_WITH_KNOTS((2,2),(3,2,3),(0.,0.290401167141741),(0.245359924929359,
0.245954053070908,0.263201868951016),.UNSPECIFIED.)
GEOMETRIC_REPRESENTATION_ITEM()
RATIONAL_B_SPLINE_SURFACE(((0.987624841600687,0.987624841600687,0.987624841600687,
0.986938988894508,0.989176916802452),(0.987624841600687,0.987624841600687,
0.987624841600687,0.986938988894508,0.989176916802452)))
REPRESENTATION_ITEM('')
SURFACE()
);
#2094=(
BOUNDED_SURFACE()
B_SPLINE_SURFACE(1,2,((#129523,#129524,#129525,#129526,#129527),(#129528,
#129529,#129530,#129531,#129532)),.UNSPECIFIED.,.F.,.F.,.F.)
B_SPLINE_SURFACE_WITH_KNOTS((2,2),(3,2,3),(0.,0.289681084359923),(0.469916319328038,
0.487259899888158,0.487433335693759),.UNSPECIFIED.)
GEOMETRIC_REPRESENTATION_ITEM()
RATIONAL_B_SPLINE_SURFACE(((0.987775548376701,0.988735325500097,0.992651440660745,
0.992651440660745,0.992651440660745),(0.987775548376701,0.988735325500097,
0.992651440660745,0.992651440660745,0.992651440660745)))
REPRESENTATION_ITEM('')
SURFACE()
);
#2095=(
BOUNDED_SURFACE()
B_SPLINE_SURFACE(1,2,((#129534,#129535,#129536,#129537,#129538),(#129539,
#129540,#129541,#129542,#129543)),.UNSPECIFIED.,.F.,.F.,.F.)
B_SPLINE_SURFACE_WITH_KNOTS((2,2),(3,2,3),(0.,0.290401167126936),(0.245359924944069,
0.245954053070909,0.263201868951012),.UNSPECIFIED.)
GEOMETRIC_REPRESENTATION_ITEM()
RATIONAL_B_SPLINE_SURFACE(((0.987624841600687,0.987624841600687,0.987624841600687,
0.986938988894508,0.989176916802451),(0.987624841600687,0.987624841600687,
0.987624841600687,0.986938988894508,0.989176916802451)))
REPRESENTATION_ITEM('')
SURFACE()
);
#2096=(
BOUNDED_SURFACE()
B_SPLINE_SURFACE(1,2,((#129560,#129561,#129562,#129563,#129564),(#129565,
#129566,#129567,#129568,#129569)),.UNSPECIFIED.,.F.,.F.,.F.)
B_SPLINE_SURFACE_WITH_KNOTS((2,2),(3,2,3),(0.,0.289681084359924),(0.469916319328033,
0.487259899888158,0.487433335693759),.UNSPECIFIED.)
GEOMETRIC_REPRESENTATION_ITEM()
RATIONAL_B_SPLINE_SURFACE(((0.9877755483767,0.988735325500095,0.992651440660745,
0.992651440660745,0.992651440660745),(0.9877755483767,0.988735325500095,
0.992651440660745,0.992651440660745,0.992651440660745)))
REPRESENTATION_ITEM('')
SURFACE()
);
#2097=(
BOUNDED_SURFACE()
B_SPLINE_SURFACE(1,2,((#129571,#129572,#129573,#129574,#129575),(#129576,
#129577,#129578,#129579,#129580)),.UNSPECIFIED.,.F.,.F.,.F.)
B_SPLINE_SURFACE_WITH_KNOTS((2,2),(3,2,3),(0.,0.290401167114357),(0.245359924956648,
0.245954053070909,0.263201868951012),.UNSPECIFIED.)
GEOMETRIC_REPRESENTATION_ITEM()
RATIONAL_B_SPLINE_SURFACE(((0.987624841600687,0.987624841600687,0.987624841600687,
0.986938988894508,0.989176916802451),(0.987624841600687,0.987624841600687,
0.987624841600687,0.986938988894508,0.989176916802451)))
REPRESENTATION_ITEM('')
SURFACE()
);
#2098=(
BOUNDED_SURFACE()
B_SPLINE_SURFACE(1,2,((#129597,#129598,#129599,#129600,#129601),(#129602,
#129603,#129604,#129605,#129606)),.UNSPECIFIED.,.F.,.F.,.F.)
B_SPLINE_SURFACE_WITH_KNOTS((2,2),(3,2,3),(0.,0.289681084359919),(0.469916319328033,
0.487259899888158,0.487433335693759),.UNSPECIFIED.)
GEOMETRIC_REPRESENTATION_ITEM()
RATIONAL_B_SPLINE_SURFACE(((0.9877755483767,0.988735325500095,0.992651440660745,
0.992651440660745,0.992651440660745),(0.9877755483767,0.988735325500095,
0.992651440660745,0.992651440660745,0.992651440660745)))
REPRESENTATION_ITEM('')
SURFACE()
);
#2099=(
BOUNDED_SURFACE()
B_SPLINE_SURFACE(1,2,((#129608,#129609,#129610,#129611,#129612),(#129613,
#129614,#129615,#129616,#129617)),.UNSPECIFIED.,.F.,.F.,.F.)
B_SPLINE_SURFACE_WITH_KNOTS((2,2),(3,2,3),(0.,0.290401167111398),(0.245359924959528,
0.245954053070909,0.263201868951012),.UNSPECIFIED.)
GEOMETRIC_REPRESENTATION_ITEM()
RATIONAL_B_SPLINE_SURFACE(((0.987624841600687,0.987624841600687,0.987624841600687,
0.986938988894508,0.989176916802451),(0.987624841600687,0.987624841600687,
0.987624841600687,0.986938988894508,0.989176916802451)))
REPRESENTATION_ITEM('')
SURFACE()
);
#2100=(
BOUNDED_SURFACE()
B_SPLINE_SURFACE(1,2,((#129634,#129635,#129636,#129637,#129638),(#129639,
#129640,#129641,#129642,#129643)),.UNSPECIFIED.,.F.,.F.,.F.)
B_SPLINE_SURFACE_WITH_KNOTS((2,2),(3,2,3),(0.,0.289681084359919),(0.469916319328033,
0.487259899888158,0.487433335693759),.UNSPECIFIED.)
GEOMETRIC_REPRESENTATION_ITEM()
RATIONAL_B_SPLINE_SURFACE(((0.9877755483767,0.988735325500095,0.992651440660745,
0.992651440660745,0.992651440660745),(0.9877755483767,0.988735325500095,
0.992651440660745,0.992651440660745,0.992651440660745)))
REPRESENTATION_ITEM('')
SURFACE()
);
#2101=(
BOUNDED_SURFACE()
B_SPLINE_SURFACE(1,2,((#129645,#129646,#129647,#129648,#129649),(#129650,
#129651,#129652,#129653,#129654)),.UNSPECIFIED.,.F.,.F.,.F.)
B_SPLINE_SURFACE_WITH_KNOTS((2,2),(3,2,3),(0.,0.290401167112765),(0.24535992495884,
0.245954053070909,0.263201868951012),.UNSPECIFIED.)
GEOMETRIC_REPRESENTATION_ITEM()
RATIONAL_B_SPLINE_SURFACE(((0.987624841600687,0.987624841600687,0.987624841600687,
0.986938988894508,0.989176916802451),(0.987624841600687,0.987624841600687,
0.987624841600687,0.986938988894508,0.989176916802451)))
REPRESENTATION_ITEM('')
SURFACE()
);
#2102=(
BOUNDED_SURFACE()
B_SPLINE_SURFACE(1,2,((#129671,#129672,#129673,#129674,#129675),(#129676,
#129677,#129678,#129679,#129680)),.UNSPECIFIED.,.F.,.F.,.F.)
B_SPLINE_SURFACE_WITH_KNOTS((2,2),(3,2,3),(0.,0.289681084359927),(0.469916319328033,
0.487259899888158,0.487433335693759),.UNSPECIFIED.)
GEOMETRIC_REPRESENTATION_ITEM()
RATIONAL_B_SPLINE_SURFACE(((0.9877755483767,0.988735325500095,0.992651440660745,
0.992651440660745,0.992651440660745),(0.9877755483767,0.988735325500095,
0.992651440660745,0.992651440660745,0.992651440660745)))
REPRESENTATION_ITEM('')
SURFACE()
);
#2103=(
BOUNDED_SURFACE()
B_SPLINE_SURFACE(1,2,((#129682,#129683,#129684,#129685,#129686),(#129687,
#129688,#129689,#129690,#129691)),.UNSPECIFIED.,.F.,.F.,.F.)
B_SPLINE_SURFACE_WITH_KNOTS((2,2),(3,2,3),(0.,0.290401167150003),(0.245359924921204,
0.245954053070909,0.263201868951012),.UNSPECIFIED.)
GEOMETRIC_REPRESENTATION_ITEM()
RATIONAL_B_SPLINE_SURFACE(((0.987624841600687,0.987624841600687,0.987624841600687,
0.986938988894508,0.989176916802451),(0.987624841600687,0.987624841600687,
0.987624841600687,0.986938988894508,0.989176916802451)))
REPRESENTATION_ITEM('')
SURFACE()
);
#2104=(
BOUNDED_SURFACE()
B_SPLINE_SURFACE(1,2,((#129708,#129709,#129710,#129711,#129712),(#129713,
#129714,#129715,#129716,#129717)),.UNSPECIFIED.,.F.,.F.,.F.)
B_SPLINE_SURFACE_WITH_KNOTS((2,2),(3,2,3),(0.,0.289681084359916),(0.469916319328029,
0.487259899888781,0.487433335694389),.UNSPECIFIED.)
GEOMETRIC_REPRESENTATION_ITEM()
RATIONAL_B_SPLINE_SURFACE(((0.9877755483767,0.988735325500129,0.992651440661026,
0.992651440661026,0.992651440661026),(0.9877755483767,0.988735325500129,
0.992651440661026,0.992651440661026,0.992651440661026)))
REPRESENTATION_ITEM('')
SURFACE()
);
#2105=(
BOUNDED_SURFACE()
B_SPLINE_SURFACE(1,2,((#129719,#129720,#129721,#129722,#129723),(#129724,
#129725,#129726,#129727,#129728)),.UNSPECIFIED.,.F.,.F.,.F.)
B_SPLINE_SURFACE_WITH_KNOTS((2,2),(3,2,3),(0.,0.290401167096493),(0.245359924974528,
0.245954053070909,0.263201868951012),.UNSPECIFIED.)
GEOMETRIC_REPRESENTATION_ITEM()
RATIONAL_B_SPLINE_SURFACE(((0.987624841600687,0.987624841600687,0.987624841600687,
0.986938988894508,0.989176916802451),(0.987624841600687,0.987624841600687,
0.987624841600687,0.986938988894508,0.989176916802451)))
REPRESENTATION_ITEM('')
SURFACE()
);
#2106=(
BOUNDED_SURFACE()
B_SPLINE_SURFACE(1,2,((#129745,#129746,#129747,#129748,#129749),(#129750,
#129751,#129752,#129753,#129754)),.UNSPECIFIED.,.F.,.F.,.F.)
B_SPLINE_SURFACE_WITH_KNOTS((2,2),(3,2,3),(0.,0.289681084359929),(0.469916319328032,
0.487259899888158,0.487433335693759),.UNSPECIFIED.)
GEOMETRIC_REPRESENTATION_ITEM()
RATIONAL_B_SPLINE_SURFACE(((0.9877755483767,0.988735325500095,0.992651440660745,
0.992651440660745,0.992651440660745),(0.9877755483767,0.988735325500095,
0.992651440660745,0.992651440660745,0.992651440660745)))
REPRESENTATION_ITEM('')
SURFACE()
);
#2107=(
BOUNDED_SURFACE()
B_SPLINE_SURFACE(1,2,((#129762,#129763,#129764,#129765,#129766),(#129767,
#129768,#129769,#129770,#129771)),.UNSPECIFIED.,.F.,.F.,.F.)
B_SPLINE_SURFACE_WITH_KNOTS((2,2),(3,2,3),(0.,0.290401167109339),(0.245359924961707,
0.245954053070909,0.263201868951011),.UNSPECIFIED.)
GEOMETRIC_REPRESENTATION_ITEM()
RATIONAL_B_SPLINE_SURFACE(((0.987624841600687,0.987624841600687,0.987624841600687,
0.986938988894508,0.989176916802451),(0.987624841600687,0.987624841600687,
0.987624841600687,0.986938988894508,0.989176916802451)))
REPRESENTATION_ITEM('')
SURFACE()
);
#2108=(
BOUNDED_SURFACE()
B_SPLINE_SURFACE(1,2,((#129773,#129774,#129775),(#129776,#129777,#129778)),
 .UNSPECIFIED.,.F.,.F.,.F.)
B_SPLINE_SURFACE_WITH_KNOTS((2,2),(3,3),(0.710192959008444,1.),(0.194132688793569,
0.211606804210308),.UNSPECIFIED.)
GEOMETRIC_REPRESENTATION_ITEM()
RATIONAL_B_SPLINE_SURFACE(((0.989843896581211,0.992516389311156,0.998189888755648),
(0.989843896581211,0.992516389311156,0.998189888755648)))
REPRESENTATION_ITEM('')
SURFACE()
);
#2109=(
BOUNDED_SURFACE()
B_SPLINE_SURFACE(1,2,((#129789,#129790,#129791,#129792,#129793),(#129794,
#129795,#129796,#129797,#129798)),.UNSPECIFIED.,.F.,.F.,.F.)
B_SPLINE_SURFACE_WITH_KNOTS((2,2),(3,2,3),(0.709727264421552,1.),(0.521815037222016,
0.53899963051341,0.539591283949508),.UNSPECIFIED.)
GEOMETRIC_REPRESENTATION_ITEM()
RATIONAL_B_SPLINE_SURFACE(((0.989362668575565,0.987015160230477,0.987570037304351,
0.987570037304351,0.987570037304351),(0.989362668575565,0.987015160230477,
0.987570037304351,0.987570037304351,0.987570037304351)))
REPRESENTATION_ITEM('')
SURFACE()
);
#2110=(
BOUNDED_SURFACE()
B_SPLINE_SURFACE(1,2,((#129809,#129810,#129811),(#129812,#129813,#129814)),
 .UNSPECIFIED.,.F.,.F.,.F.)
B_SPLINE_SURFACE_WITH_KNOTS((2,2),(3,3),(0.710192959008445,1.),(0.194132688793569,
0.211606804210308),.UNSPECIFIED.)
GEOMETRIC_REPRESENTATION_ITEM()
RATIONAL_B_SPLINE_SURFACE(((0.989843896581211,0.992516389311156,0.998189888755648),
(0.989843896581211,0.992516389311156,0.998189888755648)))
REPRESENTATION_ITEM('')
SURFACE()
);
#2111=(
BOUNDED_SURFACE()
B_SPLINE_SURFACE(1,2,((#129822,#129823,#129824,#129825,#129826),(#129827,
#129828,#129829,#129830,#129831)),.UNSPECIFIED.,.F.,.F.,.F.)
B_SPLINE_SURFACE_WITH_KNOTS((2,2),(3,2,3),(0.709727264434569,1.),(0.521815037222016,
0.53899963051341,0.539591283935433),.UNSPECIFIED.)
GEOMETRIC_REPRESENTATION_ITEM()
RATIONAL_B_SPLINE_SURFACE(((0.989362668575565,0.987015160230477,0.987570037304351,
0.987570037304351,0.987570037304351),(0.989362668575565,0.987015160230477,
0.987570037304351,0.987570037304351,0.987570037304351)))
REPRESENTATION_ITEM('')
SURFACE()
);
#2112=(
BOUNDED_SURFACE()
B_SPLINE_SURFACE(1,2,((#129842,#129843,#129844),(#129845,#129846,#129847)),
 .UNSPECIFIED.,.F.,.F.,.F.)
B_SPLINE_SURFACE_WITH_KNOTS((2,2),(3,3),(0.71019295900751,1.),(0.194132688793569,
0.211606804210308),.UNSPECIFIED.)
GEOMETRIC_REPRESENTATION_ITEM()
RATIONAL_B_SPLINE_SURFACE(((0.989843896581211,0.992516389311156,0.998189888755648),
(0.989843896581211,0.992516389311156,0.998189888755648)))
REPRESENTATION_ITEM('')
SURFACE()
);
#2113=(
BOUNDED_SURFACE()
B_SPLINE_SURFACE(1,2,((#129855,#129856,#129857,#129858,#129859),(#129860,
#129861,#129862,#129863,#129864)),.UNSPECIFIED.,.F.,.F.,.F.)
B_SPLINE_SURFACE_WITH_KNOTS((2,2),(3,2,3),(0.709727264435488,1.),(0.521815037222016,
0.53899963051341,0.539591283934722),.UNSPECIFIED.)
GEOMETRIC_REPRESENTATION_ITEM()
RATIONAL_B_SPLINE_SURFACE(((0.989362668575565,0.987015160230477,0.987570037304351,
0.987570037304351,0.987570037304351),(0.989362668575565,0.987015160230477,
0.987570037304351,0.987570037304351,0.987570037304351)))
REPRESENTATION_ITEM('')
SURFACE()
);
#2114=(
BOUNDED_SURFACE()
B_SPLINE_SURFACE(1,2,((#129875,#129876,#129877),(#129878,#129879,#129880)),
 .UNSPECIFIED.,.F.,.F.,.F.)
B_SPLINE_SURFACE_WITH_KNOTS((2,2),(3,3),(0.710192959007511,1.),(0.194132688793569,
0.211606804210308),.UNSPECIFIED.)
GEOMETRIC_REPRESENTATION_ITEM()
RATIONAL_B_SPLINE_SURFACE(((0.989843896581211,0.992516389311156,0.998189888755648),
(0.989843896581211,0.992516389311156,0.998189888755648)))
REPRESENTATION_ITEM('')
SURFACE()
);
#2115=(
BOUNDED_SURFACE()
B_SPLINE_SURFACE(1,2,((#129888,#129889,#129890,#129891,#129892),(#129893,
#129894,#129895,#129896,#129897)),.UNSPECIFIED.,.F.,.F.,.F.)
B_SPLINE_SURFACE_WITH_KNOTS((2,2),(3,2,3),(0.709727264431373,1.),(0.521815037222016,
0.53899963051341,0.539591283938545),.UNSPECIFIED.)
GEOMETRIC_REPRESENTATION_ITEM()
RATIONAL_B_SPLINE_SURFACE(((0.989362668575565,0.987015160230477,0.987570037304351,
0.987570037304351,0.987570037304351),(0.989362668575565,0.987015160230477,
0.987570037304351,0.987570037304351,0.987570037304351)))
REPRESENTATION_ITEM('')
SURFACE()
);
#2116=(
BOUNDED_SURFACE()
B_SPLINE_SURFACE(1,2,((#129908,#129909,#129910),(#129911,#129912,#129913)),
 .UNSPECIFIED.,.F.,.F.,.F.)
B_SPLINE_SURFACE_WITH_KNOTS((2,2),(3,3),(0.710192959007508,1.),(0.194132688793569,
0.211606804210308),.UNSPECIFIED.)
GEOMETRIC_REPRESENTATION_ITEM()
RATIONAL_B_SPLINE_SURFACE(((0.989843896581211,0.992516389311156,0.998189888755648),
(0.989843896581211,0.992516389311156,0.998189888755648)))
REPRESENTATION_ITEM('')
SURFACE()
);
#2117=(
BOUNDED_SURFACE()
B_SPLINE_SURFACE(1,2,((#129921,#129922,#129923,#129924,#129925),(#129926,
#129927,#129928,#129929,#129930)),.UNSPECIFIED.,.F.,.F.,.F.)
B_SPLINE_SURFACE_WITH_KNOTS((2,2),(3,2,3),(0.709727264444556,1.),(0.521815037222016,
0.53899963051341,0.53959128392486),.UNSPECIFIED.)
GEOMETRIC_REPRESENTATION_ITEM()
RATIONAL_B_SPLINE_SURFACE(((0.989362668575565,0.987015160230477,0.987570037304351,
0.987570037304351,0.987570037304351),(0.989362668575565,0.987015160230477,
0.987570037304351,0.987570037304351,0.987570037304351)))
REPRESENTATION_ITEM('')
SURFACE()
);
#2118=(
BOUNDED_SURFACE()
B_SPLINE_SURFACE(1,2,((#129941,#129942,#129943),(#129944,#129945,#129946)),
 .UNSPECIFIED.,.F.,.F.,.F.)
B_SPLINE_SURFACE_WITH_KNOTS((2,2),(3,3),(0.710192959006928,1.),(0.194132688793569,
0.211606804210308),.UNSPECIFIED.)
GEOMETRIC_REPRESENTATION_ITEM()
RATIONAL_B_SPLINE_SURFACE(((0.989843896581211,0.992516389311156,0.998189888755648),
(0.989843896581211,0.992516389311156,0.998189888755648)))
REPRESENTATION_ITEM('')
SURFACE()
);
#2119=(
BOUNDED_SURFACE()
B_SPLINE_SURFACE(1,2,((#129954,#129955,#129956,#129957,#129958),(#129959,
#129960,#129961,#129962,#129963)),.UNSPECIFIED.,.F.,.F.,.F.)
B_SPLINE_SURFACE_WITH_KNOTS((2,2),(3,2,3),(0.709727264376017,1.),(0.521815037222016,
0.53899963051341,0.539591283993824),.UNSPECIFIED.)
GEOMETRIC_REPRESENTATION_ITEM()
RATIONAL_B_SPLINE_SURFACE(((0.989362668575565,0.987015160230477,0.987570037304351,
0.987570037304351,0.987570037304351),(0.989362668575565,0.987015160230477,
0.987570037304351,0.987570037304351,0.987570037304351)))
REPRESENTATION_ITEM('')
SURFACE()
);
#2120=(
BOUNDED_SURFACE()
B_SPLINE_SURFACE(1,2,((#129974,#129975,#129976),(#129977,#129978,#129979)),
 .UNSPECIFIED.,.F.,.F.,.F.)
B_SPLINE_SURFACE_WITH_KNOTS((2,2),(3,3),(0.710192959007512,1.),(0.194132688793569,
0.211606804210308),.UNSPECIFIED.)
GEOMETRIC_REPRESENTATION_ITEM()
RATIONAL_B_SPLINE_SURFACE(((0.989843896581211,0.992516389311156,0.998189888755648),
(0.989843896581211,0.992516389311156,0.998189888755648)))
REPRESENTATION_ITEM('')
SURFACE()
);
#2121=(
BOUNDED_SURFACE()
B_SPLINE_SURFACE(1,2,((#129987,#129988,#129989,#129990,#129991),(#129992,
#129993,#129994,#129995,#129996)),.UNSPECIFIED.,.F.,.F.,.F.)
B_SPLINE_SURFACE_WITH_KNOTS((2,2),(3,2,3),(0.709727264422407,1.),(0.521815037222016,
0.53899963051341,0.539591283947025),.UNSPECIFIED.)
GEOMETRIC_REPRESENTATION_ITEM()
RATIONAL_B_SPLINE_SURFACE(((0.989362668575565,0.987015160230477,0.987570037304351,
0.987570037304351,0.987570037304351),(0.989362668575565,0.987015160230477,
0.987570037304351,0.987570037304351,0.987570037304351)))
REPRESENTATION_ITEM('')
SURFACE()
);
#2122=(
BOUNDED_SURFACE()
B_SPLINE_SURFACE(1,2,((#130007,#130008,#130009),(#130010,#130011,#130012)),
 .UNSPECIFIED.,.F.,.F.,.F.)
B_SPLINE_SURFACE_WITH_KNOTS((2,2),(3,3),(0.710192959006932,1.),(0.194132688793569,
0.211606804210308),.UNSPECIFIED.)
GEOMETRIC_REPRESENTATION_ITEM()
RATIONAL_B_SPLINE_SURFACE(((0.989843896581211,0.992516389311156,0.998189888755648),
(0.989843896581211,0.992516389311156,0.998189888755648)))
REPRESENTATION_ITEM('')
SURFACE()
);
#2123=(
BOUNDED_SURFACE()
B_SPLINE_SURFACE(1,2,((#130020,#130021,#130022,#130023,#130024),(#130025,
#130026,#130027,#130028,#130029)),.UNSPECIFIED.,.F.,.F.,.F.)
B_SPLINE_SURFACE_WITH_KNOTS((2,2),(3,2,3),(0.709727264379074,1.),(0.521815037222017,
0.53899963051341,0.539591283990695),.UNSPECIFIED.)
GEOMETRIC_REPRESENTATION_ITEM()
RATIONAL_B_SPLINE_SURFACE(((0.989362668575565,0.987015160230477,0.987570037304351,
0.987570037304351,0.987570037304351),(0.989362668575565,0.987015160230477,
0.987570037304351,0.987570037304351,0.987570037304351)))
REPRESENTATION_ITEM('')
SURFACE()
);
#2124=(
BOUNDED_SURFACE()
B_SPLINE_SURFACE(1,2,((#130040,#130041,#130042),(#130043,#130044,#130045)),
 .UNSPECIFIED.,.F.,.F.,.F.)
B_SPLINE_SURFACE_WITH_KNOTS((2,2),(3,3),(0.710192959007428,1.),(0.194132688793568,
0.211606804210307),.UNSPECIFIED.)
GEOMETRIC_REPRESENTATION_ITEM()
RATIONAL_B_SPLINE_SURFACE(((0.989843896581211,0.992516389311155,0.998189888755648),
(0.989843896581211,0.992516389311155,0.998189888755648)))
REPRESENTATION_ITEM('')
SURFACE()
);
#2125=(
BOUNDED_SURFACE()
B_SPLINE_SURFACE(1,2,((#130053,#130054,#130055,#130056,#130057),(#130058,
#130059,#130060,#130061,#130062)),.UNSPECIFIED.,.F.,.F.,.F.)
B_SPLINE_SURFACE_WITH_KNOTS((2,2),(3,2,3),(0.709727264425964,1.),(0.521815037222018,
0.538999630513411,0.539591283943759),.UNSPECIFIED.)
GEOMETRIC_REPRESENTATION_ITEM()
RATIONAL_B_SPLINE_SURFACE(((0.989362668575565,0.987015160230477,0.987570037304351,
0.987570037304351,0.987570037304351),(0.989362668575565,0.987015160230477,
0.987570037304351,0.987570037304351,0.987570037304351)))
REPRESENTATION_ITEM('')
SURFACE()
);
#2126=(
BOUNDED_SURFACE()
B_SPLINE_SURFACE(1,2,((#130073,#130074,#130075),(#130076,#130077,#130078)),
 .UNSPECIFIED.,.F.,.F.,.F.)
B_SPLINE_SURFACE_WITH_KNOTS((2,2),(3,3),(0.710192959007435,1.),(0.194132688793568,
0.211606804210307),.UNSPECIFIED.)
GEOMETRIC_REPRESENTATION_ITEM()
RATIONAL_B_SPLINE_SURFACE(((0.989843896581211,0.992516389311156,0.998189888755648),
(0.989843896581211,0.992516389311156,0.998189888755648)))
REPRESENTATION_ITEM('')
SURFACE()
);
#2127=(
BOUNDED_SURFACE()
B_SPLINE_SURFACE(1,2,((#130086,#130087,#130088,#130089,#130090),(#130091,
#130092,#130093,#130094,#130095)),.UNSPECIFIED.,.F.,.F.,.F.)
B_SPLINE_SURFACE_WITH_KNOTS((2,2),(3,2,3),(0.709727264418055,1.),(0.521815037222017,
0.538999630513411,0.539591283951268),.UNSPECIFIED.)
GEOMETRIC_REPRESENTATION_ITEM()
RATIONAL_B_SPLINE_SURFACE(((0.989362668575565,0.987015160230477,0.987570037304351,
0.987570037304351,0.987570037304351),(0.989362668575565,0.987015160230477,
0.987570037304351,0.987570037304351,0.987570037304351)))
REPRESENTATION_ITEM('')
SURFACE()
);
#2128=(
BOUNDED_SURFACE()
B_SPLINE_SURFACE(1,2,((#130106,#130107,#130108),(#130109,#130110,#130111)),
 .UNSPECIFIED.,.F.,.F.,.F.)
B_SPLINE_SURFACE_WITH_KNOTS((2,2),(3,3),(0.710192959006835,1.),(0.194132688793568,
0.211606804210307),.UNSPECIFIED.)
GEOMETRIC_REPRESENTATION_ITEM()
RATIONAL_B_SPLINE_SURFACE(((0.989843896581211,0.992516389311155,0.998189888755648),
(0.989843896581211,0.992516389311155,0.998189888755648)))
REPRESENTATION_ITEM('')
SURFACE()
);
#2129=(
BOUNDED_SURFACE()
B_SPLINE_SURFACE(1,2,((#130119,#130120,#130121,#130122,#130123),(#130124,
#130125,#130126,#130127,#130128)),.UNSPECIFIED.,.F.,.F.,.F.)
B_SPLINE_SURFACE_WITH_KNOTS((2,2),(3,2,3),(0.709727264402715,1.),(0.521815037222018,
0.538999630513411,0.539591283967167),.UNSPECIFIED.)
GEOMETRIC_REPRESENTATION_ITEM()
RATIONAL_B_SPLINE_SURFACE(((0.989362668575565,0.987015160230477,0.987570037304351,
0.987570037304351,0.987570037304351),(0.989362668575565,0.987015160230477,
0.987570037304351,0.987570037304351,0.987570037304351)))
REPRESENTATION_ITEM('')
SURFACE()
);
#2130=(
BOUNDED_SURFACE()
B_SPLINE_SURFACE(1,2,((#130139,#130140,#130141),(#130142,#130143,#130144)),
 .UNSPECIFIED.,.F.,.F.,.F.)
B_SPLINE_SURFACE_WITH_KNOTS((2,2),(3,3),(0.710192959007424,1.),(0.194132688793568,
0.211606804210307),.UNSPECIFIED.)
GEOMETRIC_REPRESENTATION_ITEM()
RATIONAL_B_SPLINE_SURFACE(((0.989843896581211,0.992516389311155,0.998189888755648),
(0.989843896581211,0.992516389311155,0.998189888755648)))
REPRESENTATION_ITEM('')
SURFACE()
);
#2131=(
BOUNDED_SURFACE()
B_SPLINE_SURFACE(1,2,((#130152,#130153,#130154,#130155,#130156),(#130157,
#130158,#130159,#130160,#130161)),.UNSPECIFIED.,.F.,.F.,.F.)
B_SPLINE_SURFACE_WITH_KNOTS((2,2),(3,2,3),(0.709727264418693,1.),(0.521815037222018,
0.538999630513411,0.539591283950436),.UNSPECIFIED.)
GEOMETRIC_REPRESENTATION_ITEM()
RATIONAL_B_SPLINE_SURFACE(((0.989362668575565,0.987015160230477,0.987570037304351,
0.987570037304351,0.987570037304351),(0.989362668575565,0.987015160230477,
0.987570037304351,0.987570037304351,0.987570037304351)))
REPRESENTATION_ITEM('')
SURFACE()
);
#2132=(
BOUNDED_SURFACE()
B_SPLINE_SURFACE(1,2,((#130172,#130173,#130174),(#130175,#130176,#130177)),
 .UNSPECIFIED.,.F.,.F.,.F.)
B_SPLINE_SURFACE_WITH_KNOTS((2,2),(3,3),(0.710192959006924,1.),(0.194132688793568,
0.211606804210307),.UNSPECIFIED.)
GEOMETRIC_REPRESENTATION_ITEM()
RATIONAL_B_SPLINE_SURFACE(((0.989843896581211,0.992516389311155,0.998189888755648),
(0.989843896581211,0.992516389311155,0.998189888755648)))
REPRESENTATION_ITEM('')
SURFACE()
);
#2133=(
BOUNDED_SURFACE()
B_SPLINE_SURFACE(1,2,((#130185,#130186,#130187,#130188,#130189),(#130190,
#130191,#130192,#130193,#130194)),.UNSPECIFIED.,.F.,.F.,.F.)
B_SPLINE_SURFACE_WITH_KNOTS((2,2),(3,2,3),(0.709727264417126,1.),(0.521815037222017,
0.538999630513412,0.53959128395279),.UNSPECIFIED.)
GEOMETRIC_REPRESENTATION_ITEM()
RATIONAL_B_SPLINE_SURFACE(((0.989362668575565,0.987015160230477,0.987570037304351,
0.987570037304351,0.987570037304351),(0.989362668575565,0.987015160230477,
0.987570037304351,0.987570037304351,0.987570037304351)))
REPRESENTATION_ITEM('')
SURFACE()
);
#2134=(
BOUNDED_SURFACE()
B_SPLINE_SURFACE(1,2,((#130205,#130206,#130207),(#130208,#130209,#130210)),
 .UNSPECIFIED.,.F.,.F.,.F.)
B_SPLINE_SURFACE_WITH_KNOTS((2,2),(3,3),(0.710192959007418,1.),(0.194132688793568,
0.211606804210307),.UNSPECIFIED.)
GEOMETRIC_REPRESENTATION_ITEM()
RATIONAL_B_SPLINE_SURFACE(((0.989843896581211,0.992516389311156,0.998189888755648),
(0.989843896581211,0.992516389311156,0.998189888755648)))
REPRESENTATION_ITEM('')
SURFACE()
);
#2135=(
BOUNDED_SURFACE()
B_SPLINE_SURFACE(1,2,((#130218,#130219,#130220,#130221,#130222),(#130223,
#130224,#130225,#130226,#130227)),.UNSPECIFIED.,.F.,.F.,.F.)
B_SPLINE_SURFACE_WITH_KNOTS((2,2),(3,2,3),(0.709727265139864,1.),(0.521815037222017,
0.538999630513411,0.539591284245209),.UNSPECIFIED.)
GEOMETRIC_REPRESENTATION_ITEM()
RATIONAL_B_SPLINE_SURFACE(((0.989362668575565,0.987015160230477,0.987570037304351,
0.987570037304351,0.987570037304351),(0.989362668575565,0.987015160230477,
0.987570037304351,0.987570037304351,0.987570037304351)))
REPRESENTATION_ITEM('')
SURFACE()
);
#2136=(
BOUNDED_SURFACE()
B_SPLINE_SURFACE(1,2,((#130235,#130236,#130237),(#130238,#130239,#130240)),
 .UNSPECIFIED.,.F.,.F.,.F.)
B_SPLINE_SURFACE_WITH_KNOTS((2,2),(3,3),(0.710192959006919,1.),(0.194132688793568,
0.211606804210307),.UNSPECIFIED.)
GEOMETRIC_REPRESENTATION_ITEM()
RATIONAL_B_SPLINE_SURFACE(((0.989843896581211,0.992516389311155,0.998189888755648),
(0.989843896581211,0.992516389311155,0.998189888755648)))
REPRESENTATION_ITEM('')
SURFACE()
);
#2137=(
BOUNDED_SURFACE()
B_SPLINE_SURFACE(1,2,((#130242,#130243,#130244,#130245,#130246),(#130247,
#130248,#130249,#130250,#130251)),.UNSPECIFIED.,.F.,.F.,.F.)
B_SPLINE_SURFACE_WITH_KNOTS((2,2),(3,2,3),(0.709727264430238,1.),(0.521815037222018,
0.538999630513411,0.539591283939394),.UNSPECIFIED.)
GEOMETRIC_REPRESENTATION_ITEM()
RATIONAL_B_SPLINE_SURFACE(((0.989362668575565,0.987015160230477,0.987570037304351,
0.987570037304351,0.987570037304351),(0.989362668575565,0.987015160230477,
0.987570037304351,0.987570037304351,0.987570037304351)))
REPRESENTATION_ITEM('')
SURFACE()
);
#2138=(
BOUNDED_SURFACE()
B_SPLINE_SURFACE(1,2,((#130262,#130263,#130264),(#130265,#130266,#130267)),
 .UNSPECIFIED.,.F.,.F.,.F.)
B_SPLINE_SURFACE_WITH_KNOTS((2,2),(3,3),(0.710192959007147,1.),(0.194132688793568,
0.211606804210307),.UNSPECIFIED.)
GEOMETRIC_REPRESENTATION_ITEM()
RATIONAL_B_SPLINE_SURFACE(((0.989843896581211,0.992516389311156,0.998189888755648),
(0.989843896581211,0.992516389311156,0.998189888755648)))
REPRESENTATION_ITEM('')
SURFACE()
);
#2139=(
BOUNDED_SURFACE()
B_SPLINE_SURFACE(1,2,((#130275,#130276,#130277,#130278,#130279),(#130280,
#130281,#130282,#130283,#130284)),.UNSPECIFIED.,.F.,.F.,.F.)
B_SPLINE_SURFACE_WITH_KNOTS((2,2),(3,2,3),(0.709727264407736,1.),(0.521815037222018,
0.538999630513411,0.539591283960815),.UNSPECIFIED.)
GEOMETRIC_REPRESENTATION_ITEM()
RATIONAL_B_SPLINE_SURFACE(((0.989362668575565,0.987015160230477,0.987570037304351,
0.987570037304351,0.987570037304351),(0.989362668575565,0.987015160230477,
0.987570037304351,0.987570037304351,0.987570037304351)))
REPRESENTATION_ITEM('')
SURFACE()
);
#2140=(
BOUNDED_SURFACE()
B_SPLINE_SURFACE(1,2,((#130295,#130296,#130297),(#130298,#130299,#130300)),
 .UNSPECIFIED.,.F.,.F.,.F.)
B_SPLINE_SURFACE_WITH_KNOTS((2,2),(3,3),(0.710192959006099,1.),(0.194132688793568,
0.211606804210307),.UNSPECIFIED.)
GEOMETRIC_REPRESENTATION_ITEM()
RATIONAL_B_SPLINE_SURFACE(((0.989843896581211,0.992516389311156,0.998189888755648),
(0.989843896581211,0.992516389311156,0.998189888755648)))
REPRESENTATION_ITEM('')
SURFACE()
);
#2141=(
BOUNDED_SURFACE()
B_SPLINE_SURFACE(1,2,((#130308,#130309,#130310,#130311,#130312),(#130313,
#130314,#130315,#130316,#130317)),.UNSPECIFIED.,.F.,.F.,.F.)
B_SPLINE_SURFACE_WITH_KNOTS((2,2),(3,2,3),(0.709727264416509,1.),(0.521815037222015,
0.538999630513412,0.539591283953501),.UNSPECIFIED.)
GEOMETRIC_REPRESENTATION_ITEM()
RATIONAL_B_SPLINE_SURFACE(((0.989362668575565,0.987015160230477,0.987570037304351,
0.987570037304351,0.987570037304351),(0.989362668575565,0.987015160230477,
0.987570037304351,0.987570037304351,0.987570037304351)))
REPRESENTATION_ITEM('')
SURFACE()
);
#2142=(
BOUNDED_SURFACE()
B_SPLINE_SURFACE(1,2,((#130328,#130329,#130330),(#130331,#130332,#130333)),
 .UNSPECIFIED.,.F.,.F.,.F.)
B_SPLINE_SURFACE_WITH_KNOTS((2,2),(3,3),(0.710192959007386,1.),(0.194132688793568,
0.211606804210307),.UNSPECIFIED.)
GEOMETRIC_REPRESENTATION_ITEM()
RATIONAL_B_SPLINE_SURFACE(((0.989843896581211,0.992516389311155,0.998189888755647),
(0.989843896581211,0.992516389311155,0.998189888755647)))
REPRESENTATION_ITEM('')
SURFACE()
);
#2143=(
BOUNDED_SURFACE()
B_SPLINE_SURFACE(1,2,((#130341,#130342,#130343,#130344,#130345),(#130346,
#130347,#130348,#130349,#130350)),.UNSPECIFIED.,.F.,.F.,.F.)
B_SPLINE_SURFACE_WITH_KNOTS((2,2),(3,2,3),(0.709727264462459,1.),(0.521815037222018,
0.538999630513411,0.539591283907463),.UNSPECIFIED.)
GEOMETRIC_REPRESENTATION_ITEM()
RATIONAL_B_SPLINE_SURFACE(((0.989362668575565,0.987015160230477,0.987570037304351,
0.987570037304351,0.987570037304351),(0.989362668575565,0.987015160230477,
0.987570037304351,0.987570037304351,0.987570037304351)))
REPRESENTATION_ITEM('')
SURFACE()
);
#2144=(
BOUNDED_SURFACE()
B_SPLINE_SURFACE(1,2,((#130361,#130362,#130363),(#130364,#130365,#130366)),
 .UNSPECIFIED.,.F.,.F.,.F.)
B_SPLINE_SURFACE_WITH_KNOTS((2,2),(3,3),(0.710192959007503,1.),(0.194132688793568,
0.211606804210308),.UNSPECIFIED.)
GEOMETRIC_REPRESENTATION_ITEM()
RATIONAL_B_SPLINE_SURFACE(((0.98984389658121,0.992516389311155,0.998189888755648),
(0.989843896581211,0.992516389311156,0.998189888755648)))
REPRESENTATION_ITEM('')
SURFACE()
);
#2145=(
BOUNDED_SURFACE()
B_SPLINE_SURFACE(1,2,((#130374,#130375,#130376,#130377,#130378),(#130379,
#130380,#130381,#130382,#130383)),.UNSPECIFIED.,.F.,.F.,.F.)
B_SPLINE_SURFACE_WITH_KNOTS((2,2),(3,2,3),(0.709727264412533,1.),(0.521815037222017,
0.538999630513411,0.539591283956678),.UNSPECIFIED.)
GEOMETRIC_REPRESENTATION_ITEM()
RATIONAL_B_SPLINE_SURFACE(((0.989362668575565,0.987015160230477,0.987570037304351,
0.987570037304351,0.987570037304351),(0.989362668575565,0.987015160230477,
0.987570037304351,0.987570037304351,0.987570037304351)))
REPRESENTATION_ITEM('')
SURFACE()
);
#2146=(
BOUNDED_SURFACE()
B_SPLINE_SURFACE(1,2,((#130394,#130395,#130396),(#130397,#130398,#130399)),
 .UNSPECIFIED.,.F.,.F.,.F.)
B_SPLINE_SURFACE_WITH_KNOTS((2,2),(3,3),(0.710192959006866,1.),(0.194132688793568,
0.211606804210307),.UNSPECIFIED.)
GEOMETRIC_REPRESENTATION_ITEM()
RATIONAL_B_SPLINE_SURFACE(((0.989843896581211,0.992516389311155,0.998189888755648),
(0.989843896581211,0.992516389311155,0.998189888755648)))
REPRESENTATION_ITEM('')
SURFACE()
);
#2147=(
BOUNDED_SURFACE()
B_SPLINE_SURFACE(1,2,((#130407,#130408,#130409,#130410,#130411),(#130412,
#130413,#130414,#130415,#130416)),.UNSPECIFIED.,.F.,.F.,.F.)
B_SPLINE_SURFACE_WITH_KNOTS((2,2),(3,2,3),(0.709727264424186,1.),(0.521815037222016,
0.538999630513411,0.539591283946352),.UNSPECIFIED.)
GEOMETRIC_REPRESENTATION_ITEM()
RATIONAL_B_SPLINE_SURFACE(((0.989362668575565,0.987015160230477,0.987570037304351,
0.987570037304351,0.987570037304351),(0.989362668575565,0.987015160230477,
0.987570037304351,0.987570037304351,0.987570037304351)))
REPRESENTATION_ITEM('')
SURFACE()
);
#2148=(
BOUNDED_SURFACE()
B_SPLINE_SURFACE(1,2,((#130427,#130428,#130429),(#130430,#130431,#130432)),
 .UNSPECIFIED.,.F.,.F.,.F.)
B_SPLINE_SURFACE_WITH_KNOTS((2,2),(3,3),(0.710192959008264,1.),(0.194132688793568,
0.211606804210306),.UNSPECIFIED.)
GEOMETRIC_REPRESENTATION_ITEM()
RATIONAL_B_SPLINE_SURFACE(((0.989843896581211,0.992516389311155,0.998189888755647),
(0.989843896581211,0.992516389311155,0.998189888755647)))
REPRESENTATION_ITEM('')
SURFACE()
);
#2149=(
BOUNDED_SURFACE()
B_SPLINE_SURFACE(1,2,((#130440,#130441,#130442,#130443,#130444),(#130445,
#130446,#130447,#130448,#130449)),.UNSPECIFIED.,.F.,.F.,.F.)
B_SPLINE_SURFACE_WITH_KNOTS((2,2),(3,2,3),(0.709727264436057,1.),(0.521815037222013,
0.538999630513413,0.539591283933454),.UNSPECIFIED.)
GEOMETRIC_REPRESENTATION_ITEM()
RATIONAL_B_SPLINE_SURFACE(((0.989362668575566,0.987015160230477,0.987570037304351,
0.987570037304351,0.987570037304351),(0.989362668575566,0.987015160230477,
0.987570037304351,0.987570037304351,0.987570037304351)))
REPRESENTATION_ITEM('')
SURFACE()
);
#2150=(
BOUNDED_SURFACE()
B_SPLINE_SURFACE(1,2,((#130460,#130461,#130462),(#130463,#130464,#130465)),
 .UNSPECIFIED.,.F.,.F.,.F.)
B_SPLINE_SURFACE_WITH_KNOTS((2,2),(3,3),(0.710192959007117,1.),(0.194132688793568,
0.211606804210307),.UNSPECIFIED.)
GEOMETRIC_REPRESENTATION_ITEM()
RATIONAL_B_SPLINE_SURFACE(((0.98984389658121,0.992516389311155,0.998189888755647),
(0.989843896581211,0.992516389311155,0.998189888755647)))
REPRESENTATION_ITEM('')
SURFACE()
);
#2151=(
BOUNDED_SURFACE()
B_SPLINE_SURFACE(1,2,((#130473,#130474,#130475,#130476,#130477),(#130478,
#130479,#130480,#130481,#130482)),.UNSPECIFIED.,.F.,.F.,.F.)
B_SPLINE_SURFACE_WITH_KNOTS((2,2),(3,2,3),(0.709727264437685,1.),(0.521815037222018,
0.538999630513411,0.539591283931768),.UNSPECIFIED.)
GEOMETRIC_REPRESENTATION_ITEM()
RATIONAL_B_SPLINE_SURFACE(((0.989362668575564,0.987015160230477,0.987570037304351,
0.987570037304351,0.987570037304351),(0.989362668575564,0.987015160230477,
0.987570037304351,0.987570037304351,0.987570037304351)))
REPRESENTATION_ITEM('')
SURFACE()
);
#2152=(
BOUNDED_SURFACE()
B_SPLINE_SURFACE(1,2,((#130493,#130494,#130495),(#130496,#130497,#130498)),
 .UNSPECIFIED.,.F.,.F.,.F.)
B_SPLINE_SURFACE_WITH_KNOTS((2,2),(3,3),(0.710192959007304,1.),(0.194132688793568,
0.211606804210308),.UNSPECIFIED.)
GEOMETRIC_REPRESENTATION_ITEM()
RATIONAL_B_SPLINE_SURFACE(((0.989843896581211,0.992516389311156,0.998189888755648),
(0.989843896581211,0.992516389311156,0.998189888755648)))
REPRESENTATION_ITEM('')
SURFACE()
);
#2153=(
BOUNDED_SURFACE()
B_SPLINE_SURFACE(1,2,((#130506,#130507,#130508,#130509,#130510),(#130511,
#130512,#130513,#130514,#130515)),.UNSPECIFIED.,.F.,.F.,.F.)
B_SPLINE_SURFACE_WITH_KNOTS((2,2),(3,2,3),(0.709727264371731,1.),(0.521815037222015,
0.538999630513411,0.539591283996905),.UNSPECIFIED.)
GEOMETRIC_REPRESENTATION_ITEM()
RATIONAL_B_SPLINE_SURFACE(((0.989362668575565,0.987015160230477,0.987570037304351,
0.987570037304351,0.987570037304351),(0.989362668575565,0.987015160230477,
0.987570037304351,0.987570037304351,0.987570037304351)))
REPRESENTATION_ITEM('')
SURFACE()
);
#2154=(
BOUNDED_SURFACE()
B_SPLINE_SURFACE(1,2,((#130526,#130527,#130528),(#130529,#130530,#130531)),
 .UNSPECIFIED.,.F.,.F.,.F.)
B_SPLINE_SURFACE_WITH_KNOTS((2,2),(3,3),(0.710192959006264,1.),(0.194132688793568,
0.211606804210307),.UNSPECIFIED.)
GEOMETRIC_REPRESENTATION_ITEM()
RATIONAL_B_SPLINE_SURFACE(((0.989843896581211,0.992516389311155,0.998189888755648),
(0.989843896581211,0.992516389311155,0.998189888755648)))
REPRESENTATION_ITEM('')
SURFACE()
);
#2155=(
BOUNDED_SURFACE()
B_SPLINE_SURFACE(1,2,((#130539,#130540,#130541,#130542,#130543),(#130544,
#130545,#130546,#130547,#130548)),.UNSPECIFIED.,.F.,.F.,.F.)
B_SPLINE_SURFACE_WITH_KNOTS((2,2),(3,2,3),(0.709727264448413,1.),(0.521815037222016,
0.538999630513412,0.539591283922137),.UNSPECIFIED.)
GEOMETRIC_REPRESENTATION_ITEM()
RATIONAL_B_SPLINE_SURFACE(((0.989362668575565,0.987015160230477,0.987570037304351,
0.987570037304351,0.987570037304351),(0.989362668575565,0.987015160230477,
0.987570037304351,0.987570037304351,0.987570037304351)))
REPRESENTATION_ITEM('')
SURFACE()
);
#2156=(
BOUNDED_SURFACE()
B_SPLINE_SURFACE(1,2,((#130559,#130560,#130561),(#130562,#130563,#130564)),
 .UNSPECIFIED.,.F.,.F.,.F.)
B_SPLINE_SURFACE_WITH_KNOTS((2,2),(3,3),(0.710192959008098,1.),(0.194132688793568,
0.211606804210307),.UNSPECIFIED.)
GEOMETRIC_REPRESENTATION_ITEM()
RATIONAL_B_SPLINE_SURFACE(((0.989843896581211,0.992516389311156,0.998189888755648),
(0.989843896581211,0.992516389311156,0.998189888755648)))
REPRESENTATION_ITEM('')
SURFACE()
);
#2157=(
BOUNDED_SURFACE()
B_SPLINE_SURFACE(1,2,((#130572,#130573,#130574,#130575,#130576),(#130577,
#130578,#130579,#130580,#130581)),.UNSPECIFIED.,.F.,.F.,.F.)
B_SPLINE_SURFACE_WITH_KNOTS((2,2),(3,2,3),(0.709727264440069,1.),(0.521815037222017,
0.538999630513412,0.539591283929231),.UNSPECIFIED.)
GEOMETRIC_REPRESENTATION_ITEM()
RATIONAL_B_SPLINE_SURFACE(((0.989362668575565,0.987015160230477,0.987570037304351,
0.987570037304351,0.987570037304351),(0.989362668575565,0.987015160230477,
0.987570037304351,0.987570037304351,0.987570037304351)))
REPRESENTATION_ITEM('')
SURFACE()
);
#2158=(
BOUNDED_SURFACE()
B_SPLINE_SURFACE(1,2,((#130592,#130593,#130594),(#130595,#130596,#130597)),
 .UNSPECIFIED.,.F.,.F.,.F.)
B_SPLINE_SURFACE_WITH_KNOTS((2,2),(3,3),(0.710192959006946,1.),(0.194132688793568,
0.211606804210307),.UNSPECIFIED.)
GEOMETRIC_REPRESENTATION_ITEM()
RATIONAL_B_SPLINE_SURFACE(((0.989843896581211,0.992516389311155,0.998189888755648),
(0.989843896581211,0.992516389311155,0.998189888755648)))
REPRESENTATION_ITEM('')
SURFACE()
);
#2159=(
BOUNDED_SURFACE()
B_SPLINE_SURFACE(1,2,((#130605,#130606,#130607,#130608,#130609),(#130610,
#130611,#130612,#130613,#130614)),.UNSPECIFIED.,.F.,.F.,.F.)
B_SPLINE_SURFACE_WITH_KNOTS((2,2),(3,2,3),(0.709727264416401,1.),(0.521815037222017,
0.538999630513411,0.539591283953233),.UNSPECIFIED.)
GEOMETRIC_REPRESENTATION_ITEM()
RATIONAL_B_SPLINE_SURFACE(((0.989362668575565,0.987015160230477,0.987570037304351,
0.987570037304351,0.987570037304351),(0.989362668575565,0.987015160230477,
0.987570037304351,0.987570037304351,0.987570037304351)))
REPRESENTATION_ITEM('')
SURFACE()
);
#2160=(
BOUNDED_SURFACE()
B_SPLINE_SURFACE(1,2,((#130625,#130626,#130627),(#130628,#130629,#130630)),
 .UNSPECIFIED.,.F.,.F.,.F.)
B_SPLINE_SURFACE_WITH_KNOTS((2,2),(3,3),(0.710192959007193,1.),(0.194132688793568,
0.211606804210307),.UNSPECIFIED.)
GEOMETRIC_REPRESENTATION_ITEM()
RATIONAL_B_SPLINE_SURFACE(((0.989843896581211,0.992516389311155,0.998189888755648),
(0.989843896581211,0.992516389311155,0.998189888755648)))
REPRESENTATION_ITEM('')
SURFACE()
);
#2161=(
BOUNDED_SURFACE()
B_SPLINE_SURFACE(1,2,((#130638,#130639,#130640,#130641,#130642),(#130643,
#130644,#130645,#130646,#130647)),.UNSPECIFIED.,.F.,.F.,.F.)
B_SPLINE_SURFACE_WITH_KNOTS((2,2),(3,2,3),(0.709727264443144,1.),(0.521815037222018,
0.538999630513411,0.539591283926624),.UNSPECIFIED.)
GEOMETRIC_REPRESENTATION_ITEM()
RATIONAL_B_SPLINE_SURFACE(((0.989362668575565,0.987015160230477,0.987570037304351,
0.987570037304351,0.987570037304351),(0.989362668575565,0.987015160230477,
0.987570037304351,0.987570037304351,0.987570037304351)))
REPRESENTATION_ITEM('')
SURFACE()
);
#2162=(
BOUNDED_SURFACE()
B_SPLINE_SURFACE(1,2,((#130658,#130659,#130660),(#130661,#130662,#130663)),
 .UNSPECIFIED.,.F.,.F.,.F.)
B_SPLINE_SURFACE_WITH_KNOTS((2,2),(3,3),(0.71019295900745,1.),(0.194132688793569,
0.211606804210307),.UNSPECIFIED.)
GEOMETRIC_REPRESENTATION_ITEM()
RATIONAL_B_SPLINE_SURFACE(((0.989843896581211,0.992516389311156,0.998189888755648),
(0.989843896581211,0.992516389311156,0.998189888755648)))
REPRESENTATION_ITEM('')
SURFACE()
);
#2163=(
BOUNDED_SURFACE()
B_SPLINE_SURFACE(1,2,((#130671,#130672,#130673,#130674,#130675),(#130676,
#130677,#130678,#130679,#130680)),.UNSPECIFIED.,.F.,.F.,.F.)
B_SPLINE_SURFACE_WITH_KNOTS((2,2),(3,2,3),(0.709727264402816,1.),(0.521815037222017,
0.53899963051341,0.539591283968033),.UNSPECIFIED.)
GEOMETRIC_REPRESENTATION_ITEM()
RATIONAL_B_SPLINE_SURFACE(((0.989362668575565,0.987015160230477,0.987570037304351,
0.987570037304351,0.987570037304351),(0.989362668575565,0.987015160230477,
0.987570037304351,0.987570037304351,0.987570037304351)))
REPRESENTATION_ITEM('')
SURFACE()
);
#2164=(
BOUNDED_SURFACE()
B_SPLINE_SURFACE(1,2,((#130691,#130692,#130693),(#130694,#130695,#130696)),
 .UNSPECIFIED.,.F.,.F.,.F.)
B_SPLINE_SURFACE_WITH_KNOTS((2,2),(3,3),(0.710192959008445,1.),(0.194132688793569,
0.211606804210309),.UNSPECIFIED.)
GEOMETRIC_REPRESENTATION_ITEM()
RATIONAL_B_SPLINE_SURFACE(((0.989843896581211,0.992516389311156,0.998189888755648),
(0.989843896581211,0.992516389311156,0.998189888755648)))
REPRESENTATION_ITEM('')
SURFACE()
);
#2165=(
BOUNDED_SURFACE()
B_SPLINE_SURFACE(1,2,((#130710,#130711,#130712,#130713,#130714),(#130715,
#130716,#130717,#130718,#130719)),.UNSPECIFIED.,.F.,.F.,.F.)
B_SPLINE_SURFACE_WITH_KNOTS((2,2),(3,2,3),(0.709727265150677,1.),(0.521815037222016,
0.53899963051341,0.539591284235917),.UNSPECIFIED.)
GEOMETRIC_REPRESENTATION_ITEM()
RATIONAL_B_SPLINE_SURFACE(((0.989362668575565,0.987015160230477,0.987570037304351,
0.987570037304351,0.987570037304351),(0.989362668575565,0.987015160230477,
0.987570037304351,0.987570037304351,0.987570037304351)))
REPRESENTATION_ITEM('')
SURFACE()
);
#2166=(
BOUNDED_SURFACE()
B_SPLINE_SURFACE(1,2,((#130721,#130722,#130723),(#130724,#130725,#130726)),
 .UNSPECIFIED.,.F.,.F.,.F.)
B_SPLINE_SURFACE_WITH_KNOTS((2,2),(3,3),(0.710318915638064,1.),(0.228780950825331,
0.245954053070933),.UNSPECIFIED.)
GEOMETRIC_REPRESENTATION_ITEM()
RATIONAL_B_SPLINE_SURFACE(((0.991889110260675,0.988307723348173,0.987624841600685),
(0.991889110260675,0.988307723348173,0.987624841600685)))
REPRESENTATION_ITEM('')
SURFACE()
);
#2167=(
BOUNDED_SURFACE()
B_SPLINE_SURFACE(1,2,((#130739,#130740,#130741,#130742,#130743),(#130744,
#130745,#130746,#130747,#130748)),.UNSPECIFIED.,.F.,.F.,.F.)
B_SPLINE_SURFACE_WITH_KNOTS((2,2),(3,2,3),(0.710192959008441,1.),(0.487259899888159,
0.5,0.504824515313956),.UNSPECIFIED.)
GEOMETRIC_REPRESENTATION_ITEM()
RATIONAL_B_SPLINE_SURFACE(((0.992651440660745,0.99552810727657,1.,0.998306550597157,
0.996841863226482),(0.992651440660745,0.99552810727657,1.,0.998306550597157,
0.996841863226482)))
REPRESENTATION_ITEM('')
SURFACE()
);
#2168=(
BOUNDED_SURFACE()
B_SPLINE_SURFACE(1,2,((#130770,#130771,#130772),(#130773,#130774,#130775)),
 .UNSPECIFIED.,.F.,.F.,.F.)
B_SPLINE_SURFACE_WITH_KNOTS((2,2),(3,3),(0.710318915638051,1.),(0.228780950825644,
0.245954053070933),.UNSPECIFIED.)
GEOMETRIC_REPRESENTATION_ITEM()
RATIONAL_B_SPLINE_SURFACE(((0.991889110260545,0.988307723348161,0.987624841600685),
(0.991889110260545,0.988307723348161,0.987624841600685)))
REPRESENTATION_ITEM('')
SURFACE()
);
#2169=(
BOUNDED_SURFACE()
B_SPLINE_SURFACE(1,2,((#130777,#130778,#130779,#130780,#130781),(#130782,
#130783,#130784,#130785,#130786)),.UNSPECIFIED.,.F.,.F.,.F.)
B_SPLINE_SURFACE_WITH_KNOTS((2,2),(3,2,3),(0.710192959008439,1.),(0.487259899888159,
0.5,0.504824515313956),.UNSPECIFIED.)
GEOMETRIC_REPRESENTATION_ITEM()
RATIONAL_B_SPLINE_SURFACE(((0.992651440660745,0.99552810727657,1.,0.998306550597157,
0.996841863226482),(0.992651440660745,0.99552810727657,1.,0.998306550597157,
0.996841863226482)))
REPRESENTATION_ITEM('')
SURFACE()
);
#2170=(
BOUNDED_SURFACE()
B_SPLINE_SURFACE(1,2,((#130808,#130809,#130810),(#130811,#130812,#130813)),
 .UNSPECIFIED.,.F.,.F.,.F.)
B_SPLINE_SURFACE_WITH_KNOTS((2,2),(3,3),(0.710318915638056,1.),(0.228780950825752,
0.245954053070933),.UNSPECIFIED.)
GEOMETRIC_REPRESENTATION_ITEM()
RATIONAL_B_SPLINE_SURFACE(((0.9918891102605,0.988307723348156,0.987624841600685),
(0.9918891102605,0.988307723348156,0.987624841600685)))
REPRESENTATION_ITEM('')
SURFACE()
);
#2171=(
BOUNDED_SURFACE()
B_SPLINE_SURFACE(1,2,((#130815,#130816,#130817,#130818,#130819),(#130820,
#130821,#130822,#130823,#130824)),.UNSPECIFIED.,.F.,.F.,.F.)
B_SPLINE_SURFACE_WITH_KNOTS((2,2),(3,2,3),(0.71019295900844,1.),(0.487259899888159,
0.5,0.504824515313956),.UNSPECIFIED.)
GEOMETRIC_REPRESENTATION_ITEM()
RATIONAL_B_SPLINE_SURFACE(((0.992651440660745,0.99552810727657,1.,0.998306550597157,
0.996841863226482),(0.992651440660745,0.99552810727657,1.,0.998306550597157,
0.996841863226482)))
REPRESENTATION_ITEM('')
SURFACE()
);
#2172=(
BOUNDED_SURFACE()
B_SPLINE_SURFACE(1,2,((#130846,#130847,#130848),(#130849,#130850,#130851)),
 .UNSPECIFIED.,.F.,.F.,.F.)
B_SPLINE_SURFACE_WITH_KNOTS((2,2),(3,3),(0.710318915638053,1.),(0.228780950825752,
0.245954053070933),.UNSPECIFIED.)
GEOMETRIC_REPRESENTATION_ITEM()
RATIONAL_B_SPLINE_SURFACE(((0.9918891102605,0.988307723348156,0.987624841600685),
(0.9918891102605,0.988307723348156,0.987624841600685)))
REPRESENTATION_ITEM('')
SURFACE()
);
#2173=(
BOUNDED_SURFACE()
B_SPLINE_SURFACE(1,2,((#130853,#130854,#130855,#130856,#130857),(#130858,
#130859,#130860,#130861,#130862)),.UNSPECIFIED.,.F.,.F.,.F.)
B_SPLINE_SURFACE_WITH_KNOTS((2,2),(3,2,3),(0.710192959008442,1.),(0.487259899888159,
0.5,0.504824515313956),.UNSPECIFIED.)
GEOMETRIC_REPRESENTATION_ITEM()
RATIONAL_B_SPLINE_SURFACE(((0.992651440660745,0.99552810727657,1.,0.998306550597157,
0.996841863226482),(0.992651440660745,0.99552810727657,1.,0.998306550597157,
0.996841863226482)))
REPRESENTATION_ITEM('')
SURFACE()
);
#2174=(
BOUNDED_SURFACE()
B_SPLINE_SURFACE(1,2,((#130884,#130885,#130886),(#130887,#130888,#130889)),
 .UNSPECIFIED.,.F.,.F.,.F.)
B_SPLINE_SURFACE_WITH_KNOTS((2,2),(3,3),(0.71031891563806,1.),(0.228780950825244,
0.245954053070933),.UNSPECIFIED.)
GEOMETRIC_REPRESENTATION_ITEM()
RATIONAL_B_SPLINE_SURFACE(((0.991889110260711,0.988307723348176,0.987624841600685),
(0.991889110260711,0.988307723348176,0.987624841600685)))
REPRESENTATION_ITEM('')
SURFACE()
);
#2175=(
BOUNDED_SURFACE()
B_SPLINE_SURFACE(1,2,((#130891,#130892,#130893,#130894,#130895),(#130896,
#130897,#130898,#130899,#130900)),.UNSPECIFIED.,.F.,.F.,.F.)
B_SPLINE_SURFACE_WITH_KNOTS((2,2),(3,2,3),(0.71019295900844,1.),(0.487259899888159,
0.5,0.504824515313956),.UNSPECIFIED.)
GEOMETRIC_REPRESENTATION_ITEM()
RATIONAL_B_SPLINE_SURFACE(((0.992651440660745,0.99552810727657,1.,0.998306550597157,
0.996841863226482),(0.992651440660745,0.99552810727657,1.,0.998306550597157,
0.996841863226482)))
REPRESENTATION_ITEM('')
SURFACE()
);
#2176=(
BOUNDED_SURFACE()
B_SPLINE_SURFACE(1,2,((#130922,#130923,#130924),(#130925,#130926,#130927)),
 .UNSPECIFIED.,.F.,.F.,.F.)
B_SPLINE_SURFACE_WITH_KNOTS((2,2),(3,3),(0.710318915638065,1.),(0.228780950825394,
0.245954053070933),.UNSPECIFIED.)
GEOMETRIC_REPRESENTATION_ITEM()
RATIONAL_B_SPLINE_SURFACE(((0.991889110260649,0.988307723348171,0.987624841600685),
(0.991889110260649,0.988307723348171,0.987624841600685)))
REPRESENTATION_ITEM('')
SURFACE()
);
#2177=(
BOUNDED_SURFACE()
B_SPLINE_SURFACE(1,2,((#130929,#130930,#130931,#130932,#130933),(#130934,
#130935,#130936,#130937,#130938)),.UNSPECIFIED.,.F.,.F.,.F.)
B_SPLINE_SURFACE_WITH_KNOTS((2,2),(3,2,3),(0.710192959008443,1.),(0.487259899888159,
0.5,0.504824515313788),.UNSPECIFIED.)
GEOMETRIC_REPRESENTATION_ITEM()
RATIONAL_B_SPLINE_SURFACE(((0.992651440660745,0.99552810727657,1.,0.998306550597216,
0.996841863226584),(0.992651440660745,0.99552810727657,1.,0.998306550597216,
0.996841863226584)))
REPRESENTATION_ITEM('')
SURFACE()
);
#2178=(
BOUNDED_SURFACE()
B_SPLINE_SURFACE(1,2,((#130960,#130961,#130962),(#130963,#130964,#130965)),
 .UNSPECIFIED.,.F.,.F.,.F.)
B_SPLINE_SURFACE_WITH_KNOTS((2,2),(3,3),(0.71031891563806,1.),(0.228780950825462,
0.245954053070933),.UNSPECIFIED.)
GEOMETRIC_REPRESENTATION_ITEM()
RATIONAL_B_SPLINE_SURFACE(((0.99188911026062,0.988307723348168,0.987624841600685),
(0.99188911026062,0.988307723348168,0.987624841600685)))
REPRESENTATION_ITEM('')
SURFACE()
);
#2179=(
BOUNDED_SURFACE()
B_SPLINE_SURFACE(1,2,((#130967,#130968,#130969,#130970,#130971),(#130972,
#130973,#130974,#130975,#130976)),.UNSPECIFIED.,.F.,.F.,.F.)
B_SPLINE_SURFACE_WITH_KNOTS((2,2),(3,2,3),(0.710192959008441,1.),(0.487259899888159,
0.5,0.504824515313956),.UNSPECIFIED.)
GEOMETRIC_REPRESENTATION_ITEM()
RATIONAL_B_SPLINE_SURFACE(((0.992651440660745,0.99552810727657,1.,0.998306550597157,
0.996841863226482),(0.992651440660745,0.99552810727657,1.,0.998306550597157,
0.996841863226482)))
REPRESENTATION_ITEM('')
SURFACE()
);
#2180=(
BOUNDED_SURFACE()
B_SPLINE_SURFACE(1,2,((#130998,#130999,#131000),(#131001,#131002,#131003)),
 .UNSPECIFIED.,.F.,.F.,.F.)
B_SPLINE_SURFACE_WITH_KNOTS((2,2),(3,3),(0.710318915638069,1.),(0.228780950825752,
0.245954053070933),.UNSPECIFIED.)
GEOMETRIC_REPRESENTATION_ITEM()
RATIONAL_B_SPLINE_SURFACE(((0.991889110260499,0.988307723348156,0.987624841600685),
(0.9918891102605,0.988307723348156,0.987624841600685)))
REPRESENTATION_ITEM('')
SURFACE()
);
#2181=(
BOUNDED_SURFACE()
B_SPLINE_SURFACE(1,2,((#131005,#131006,#131007,#131008,#131009),(#131010,
#131011,#131012,#131013,#131014)),.UNSPECIFIED.,.F.,.F.,.F.)
B_SPLINE_SURFACE_WITH_KNOTS((2,2),(3,2,3),(0.710192959008442,1.),(0.487259899888159,
0.5,0.504824515313956),.UNSPECIFIED.)
GEOMETRIC_REPRESENTATION_ITEM()
RATIONAL_B_SPLINE_SURFACE(((0.992651440660745,0.99552810727657,1.,0.998306550597157,
0.996841863226482),(0.992651440660745,0.99552810727657,1.,0.998306550597157,
0.996841863226482)))
REPRESENTATION_ITEM('')
SURFACE()
);
#2182=(
BOUNDED_SURFACE()
B_SPLINE_SURFACE(1,2,((#131036,#131037,#131038),(#131039,#131040,#131041)),
 .UNSPECIFIED.,.F.,.F.,.F.)
B_SPLINE_SURFACE_WITH_KNOTS((2,2),(3,3),(0.710318915638061,1.),(0.228780950825752,
0.245954053070933),.UNSPECIFIED.)
GEOMETRIC_REPRESENTATION_ITEM()
RATIONAL_B_SPLINE_SURFACE(((0.9918891102605,0.988307723348156,0.987624841600685),
(0.9918891102605,0.988307723348156,0.987624841600685)))
REPRESENTATION_ITEM('')
SURFACE()
);
#2183=(
BOUNDED_SURFACE()
B_SPLINE_SURFACE(1,2,((#131043,#131044,#131045,#131046,#131047),(#131048,
#131049,#131050,#131051,#131052)),.UNSPECIFIED.,.F.,.F.,.F.)
B_SPLINE_SURFACE_WITH_KNOTS((2,2),(3,2,3),(0.710192959008441,1.),(0.487259899888159,
0.5,0.504824515313956),.UNSPECIFIED.)
GEOMETRIC_REPRESENTATION_ITEM()
RATIONAL_B_SPLINE_SURFACE(((0.992651440660745,0.99552810727657,1.,0.998306550597157,
0.996841863226482),(0.992651440660745,0.99552810727657,1.,0.998306550597157,
0.996841863226482)))
REPRESENTATION_ITEM('')
SURFACE()
);
#2184=(
BOUNDED_SURFACE()
B_SPLINE_SURFACE(1,2,((#131074,#131075,#131076),(#131077,#131078,#131079)),
 .UNSPECIFIED.,.F.,.F.,.F.)
B_SPLINE_SURFACE_WITH_KNOTS((2,2),(3,3),(0.710318915638057,1.),(0.228780950825722,
0.245954053070933),.UNSPECIFIED.)
GEOMETRIC_REPRESENTATION_ITEM()
RATIONAL_B_SPLINE_SURFACE(((0.991889110260512,0.988307723348158,0.987624841600685),
(0.991889110260512,0.988307723348158,0.987624841600685)))
REPRESENTATION_ITEM('')
SURFACE()
);
#2185=(
BOUNDED_SURFACE()
B_SPLINE_SURFACE(1,2,((#131081,#131082,#131083,#131084,#131085),(#131086,
#131087,#131088,#131089,#131090)),.UNSPECIFIED.,.F.,.F.,.F.)
B_SPLINE_SURFACE_WITH_KNOTS((2,2),(3,2,3),(0.71019295900844,1.),(0.487259899888159,
0.5,0.504824515313956),.UNSPECIFIED.)
GEOMETRIC_REPRESENTATION_ITEM()
RATIONAL_B_SPLINE_SURFACE(((0.992651440660745,0.99552810727657,1.,0.998306550597157,
0.996841863226482),(0.992651440660745,0.99552810727657,1.,0.998306550597157,
0.996841863226482)))
REPRESENTATION_ITEM('')
SURFACE()
);
#2186=(
BOUNDED_SURFACE()
B_SPLINE_SURFACE(1,2,((#131112,#131113,#131114),(#131115,#131116,#131117)),
 .UNSPECIFIED.,.F.,.F.,.F.)
B_SPLINE_SURFACE_WITH_KNOTS((2,2),(3,3),(0.710318915638055,1.),(0.228780950825752,
0.245954053070933),.UNSPECIFIED.)
GEOMETRIC_REPRESENTATION_ITEM()
RATIONAL_B_SPLINE_SURFACE(((0.991889110260499,0.988307723348156,0.987624841600685),
(0.991889110260499,0.988307723348156,0.987624841600685)))
REPRESENTATION_ITEM('')
SURFACE()
);
#2187=(
BOUNDED_SURFACE()
B_SPLINE_SURFACE(1,2,((#131119,#131120,#131121,#131122,#131123),(#131124,
#131125,#131126,#131127,#131128)),.UNSPECIFIED.,.F.,.F.,.F.)
B_SPLINE_SURFACE_WITH_KNOTS((2,2),(3,2,3),(0.710192959008438,1.),(0.487259899888159,
0.5,0.504824515313956),.UNSPECIFIED.)
GEOMETRIC_REPRESENTATION_ITEM()
RATIONAL_B_SPLINE_SURFACE(((0.992651440660745,0.99552810727657,1.,0.998306550597157,
0.996841863226482),(0.992651440660745,0.99552810727657,1.,0.998306550597157,
0.996841863226482)))
REPRESENTATION_ITEM('')
SURFACE()
);
#2188=(
BOUNDED_SURFACE()
B_SPLINE_SURFACE(1,2,((#131150,#131151,#131152),(#131153,#131154,#131155)),
 .UNSPECIFIED.,.F.,.F.,.F.)
B_SPLINE_SURFACE_WITH_KNOTS((2,2),(3,3),(0.710318915638057,1.),(0.228780950825752,
0.245954053070933),.UNSPECIFIED.)
GEOMETRIC_REPRESENTATION_ITEM()
RATIONAL_B_SPLINE_SURFACE(((0.9918891102605,0.988307723348156,0.987624841600685),
(0.9918891102605,0.988307723348156,0.987624841600685)))
REPRESENTATION_ITEM('')
SURFACE()
);
#2189=(
BOUNDED_SURFACE()
B_SPLINE_SURFACE(1,2,((#131157,#131158,#131159,#131160,#131161),(#131162,
#131163,#131164,#131165,#131166)),.UNSPECIFIED.,.F.,.F.,.F.)
B_SPLINE_SURFACE_WITH_KNOTS((2,2),(3,2,3),(0.710192959008445,1.),(0.487259899888159,
0.5,0.504824515313956),.UNSPECIFIED.)
GEOMETRIC_REPRESENTATION_ITEM()
RATIONAL_B_SPLINE_SURFACE(((0.992651440660745,0.99552810727657,1.,0.998306550597157,
0.996841863226482),(0.992651440660745,0.99552810727657,1.,0.998306550597157,
0.996841863226482)))
REPRESENTATION_ITEM('')
SURFACE()
);
#2190=(
BOUNDED_SURFACE()
B_SPLINE_SURFACE(1,2,((#131188,#131189,#131190),(#131191,#131192,#131193)),
 .UNSPECIFIED.,.F.,.F.,.F.)
B_SPLINE_SURFACE_WITH_KNOTS((2,2),(3,3),(0.710318915638057,1.),(0.228780950825522,
0.245954053070933),.UNSPECIFIED.)
GEOMETRIC_REPRESENTATION_ITEM()
RATIONAL_B_SPLINE_SURFACE(((0.991889110260596,0.988307723348166,0.987624841600685),
(0.991889110260596,0.988307723348166,0.987624841600685)))
REPRESENTATION_ITEM('')
SURFACE()
);
#2191=(
BOUNDED_SURFACE()
B_SPLINE_SURFACE(1,2,((#131195,#131196,#131197,#131198,#131199),(#131200,
#131201,#131202,#131203,#131204)),.UNSPECIFIED.,.F.,.F.,.F.)
B_SPLINE_SURFACE_WITH_KNOTS((2,2),(3,2,3),(0.710192959008444,1.),(0.487259899888159,
0.5,0.504824515313956),.UNSPECIFIED.)
GEOMETRIC_REPRESENTATION_ITEM()
RATIONAL_B_SPLINE_SURFACE(((0.992651440660745,0.99552810727657,1.,0.998306550597157,
0.996841863226482),(0.992651440660745,0.99552810727657,1.,0.998306550597157,
0.996841863226482)))
REPRESENTATION_ITEM('')
SURFACE()
);
#2192=(
BOUNDED_SURFACE()
B_SPLINE_SURFACE(1,2,((#131226,#131227,#131228),(#131229,#131230,#131231)),
 .UNSPECIFIED.,.F.,.F.,.F.)
B_SPLINE_SURFACE_WITH_KNOTS((2,2),(3,3),(0.71031891563806,1.),(0.22878095082566,
0.245954053070933),.UNSPECIFIED.)
GEOMETRIC_REPRESENTATION_ITEM()
RATIONAL_B_SPLINE_SURFACE(((0.991889110260538,0.98830772334816,0.987624841600685),
(0.991889110260538,0.98830772334816,0.987624841600685)))
REPRESENTATION_ITEM('')
SURFACE()
);
#2193=(
BOUNDED_SURFACE()
B_SPLINE_SURFACE(1,2,((#131233,#131234,#131235,#131236,#131237),(#131238,
#131239,#131240,#131241,#131242)),.UNSPECIFIED.,.F.,.F.,.F.)
B_SPLINE_SURFACE_WITH_KNOTS((2,2),(3,2,3),(0.710192959008441,1.),(0.487259899888159,
0.5,0.504824515313956),.UNSPECIFIED.)
GEOMETRIC_REPRESENTATION_ITEM()
RATIONAL_B_SPLINE_SURFACE(((0.992651440660745,0.99552810727657,1.,0.998306550597157,
0.996841863226482),(0.992651440660745,0.99552810727657,1.,0.998306550597157,
0.996841863226482)))
REPRESENTATION_ITEM('')
SURFACE()
);
#2194=(
BOUNDED_SURFACE()
B_SPLINE_SURFACE(1,2,((#131264,#131265,#131266),(#131267,#131268,#131269)),
 .UNSPECIFIED.,.F.,.F.,.F.)
B_SPLINE_SURFACE_WITH_KNOTS((2,2),(3,3),(0.710318915638052,1.),(0.228780950825752,
0.245954053070933),.UNSPECIFIED.)
GEOMETRIC_REPRESENTATION_ITEM()
RATIONAL_B_SPLINE_SURFACE(((0.991889110260499,0.988307723348156,0.987624841600685),
(0.991889110260499,0.988307723348156,0.987624841600685)))
REPRESENTATION_ITEM('')
SURFACE()
);
#2195=(
BOUNDED_SURFACE()
B_SPLINE_SURFACE(1,2,((#131271,#131272,#131273,#131274,#131275),(#131276,
#131277,#131278,#131279,#131280)),.UNSPECIFIED.,.F.,.F.,.F.)
B_SPLINE_SURFACE_WITH_KNOTS((2,2),(3,2,3),(0.710192959008436,1.),(0.487259899888159,
0.5,0.504824515313956),.UNSPECIFIED.)
GEOMETRIC_REPRESENTATION_ITEM()
RATIONAL_B_SPLINE_SURFACE(((0.992651440660745,0.99552810727657,1.,0.998306550597157,
0.996841863226482),(0.992651440660745,0.99552810727657,1.,0.998306550597157,
0.996841863226482)))
REPRESENTATION_ITEM('')
SURFACE()
);
#2196=(
BOUNDED_SURFACE()
B_SPLINE_SURFACE(1,2,((#131302,#131303,#131304),(#131305,#131306,#131307)),
 .UNSPECIFIED.,.F.,.F.,.F.)
B_SPLINE_SURFACE_WITH_KNOTS((2,2),(3,3),(0.710318915638056,1.),(0.228780950825752,
0.245954053070933),.UNSPECIFIED.)
GEOMETRIC_REPRESENTATION_ITEM()
RATIONAL_B_SPLINE_SURFACE(((0.991889110260499,0.988307723348156,0.987624841600685),
(0.991889110260499,0.988307723348156,0.987624841600685)))
REPRESENTATION_ITEM('')
SURFACE()
);
#2197=(
BOUNDED_SURFACE()
B_SPLINE_SURFACE(1,2,((#131309,#131310,#131311,#131312,#131313),(#131314,
#131315,#131316,#131317,#131318)),.UNSPECIFIED.,.F.,.F.,.F.)
B_SPLINE_SURFACE_WITH_KNOTS((2,2),(3,2,3),(0.710192959008442,1.),(0.487259899888159,
0.5,0.504824515313956),.UNSPECIFIED.)
GEOMETRIC_REPRESENTATION_ITEM()
RATIONAL_B_SPLINE_SURFACE(((0.992651440660745,0.99552810727657,1.,0.998306550597157,
0.996841863226482),(0.992651440660745,0.99552810727657,1.,0.998306550597157,
0.996841863226482)))
REPRESENTATION_ITEM('')
SURFACE()
);
#2198=(
BOUNDED_SURFACE()
B_SPLINE_SURFACE(1,2,((#131340,#131341,#131342),(#131343,#131344,#131345)),
 .UNSPECIFIED.,.F.,.F.,.F.)
B_SPLINE_SURFACE_WITH_KNOTS((2,2),(3,3),(0.710318915638057,1.),(0.228780950825752,
0.245954053070933),.UNSPECIFIED.)
GEOMETRIC_REPRESENTATION_ITEM()
RATIONAL_B_SPLINE_SURFACE(((0.991889110260499,0.988307723348156,0.987624841600685),
(0.991889110260499,0.988307723348156,0.987624841600685)))
REPRESENTATION_ITEM('')
SURFACE()
);
#2199=(
BOUNDED_SURFACE()
B_SPLINE_SURFACE(1,2,((#131347,#131348,#131349,#131350,#131351),(#131352,
#131353,#131354,#131355,#131356)),.UNSPECIFIED.,.F.,.F.,.F.)
B_SPLINE_SURFACE_WITH_KNOTS((2,2),(3,2,3),(0.710192959008438,1.),(0.487259899888159,
0.5,0.504824515313956),.UNSPECIFIED.)
GEOMETRIC_REPRESENTATION_ITEM()
RATIONAL_B_SPLINE_SURFACE(((0.992651440660745,0.99552810727657,1.,0.998306550597157,
0.996841863226482),(0.992651440660745,0.99552810727657,1.,0.998306550597157,
0.996841863226482)))
REPRESENTATION_ITEM('')
SURFACE()
);
#2200=(
BOUNDED_SURFACE()
B_SPLINE_SURFACE(1,2,((#131378,#131379,#131380),(#131381,#131382,#131383)),
 .UNSPECIFIED.,.F.,.F.,.F.)
B_SPLINE_SURFACE_WITH_KNOTS((2,2),(3,3),(0.710318915638058,1.),(0.228780950825752,
0.245954053070933),.UNSPECIFIED.)
GEOMETRIC_REPRESENTATION_ITEM()
RATIONAL_B_SPLINE_SURFACE(((0.9918891102605,0.988307723348156,0.987624841600685),
(0.9918891102605,0.988307723348156,0.987624841600685)))
REPRESENTATION_ITEM('')
SURFACE()
);
#2201=(
BOUNDED_SURFACE()
B_SPLINE_SURFACE(1,2,((#131385,#131386,#131387,#131388,#131389),(#131390,
#131391,#131392,#131393,#131394)),.UNSPECIFIED.,.F.,.F.,.F.)
B_SPLINE_SURFACE_WITH_KNOTS((2,2),(3,2,3),(0.710192959008441,1.),(0.487259899888159,
0.5,0.504824515313956),.UNSPECIFIED.)
GEOMETRIC_REPRESENTATION_ITEM()
RATIONAL_B_SPLINE_SURFACE(((0.992651440660745,0.99552810727657,1.,0.998306550597157,
0.996841863226482),(0.992651440660745,0.99552810727657,1.,0.998306550597157,
0.996841863226482)))
REPRESENTATION_ITEM('')
SURFACE()
);
#2202=(
BOUNDED_SURFACE()
B_SPLINE_SURFACE(1,2,((#131416,#131417,#131418),(#131419,#131420,#131421)),
 .UNSPECIFIED.,.F.,.F.,.F.)
B_SPLINE_SURFACE_WITH_KNOTS((2,2),(3,3),(0.710318915638058,1.),(0.228780950825752,
0.245954053070933),.UNSPECIFIED.)
GEOMETRIC_REPRESENTATION_ITEM()
RATIONAL_B_SPLINE_SURFACE(((0.9918891102605,0.988307723348156,0.987624841600685),
(0.9918891102605,0.988307723348156,0.987624841600685)))
REPRESENTATION_ITEM('')
SURFACE()
);
#2203=(
BOUNDED_SURFACE()
B_SPLINE_SURFACE(1,2,((#131423,#131424,#131425,#131426,#131427),(#131428,
#131429,#131430,#131431,#131432)),.UNSPECIFIED.,.F.,.F.,.F.)
B_SPLINE_SURFACE_WITH_KNOTS((2,2),(3,2,3),(0.710192959008441,1.),(0.487259899888159,
0.5,0.504824515313956),.UNSPECIFIED.)
GEOMETRIC_REPRESENTATION_ITEM()
RATIONAL_B_SPLINE_SURFACE(((0.992651440660745,0.99552810727657,1.,0.998306550597157,
0.996841863226482),(0.992651440660745,0.99552810727657,1.,0.998306550597157,
0.996841863226482)))
REPRESENTATION_ITEM('')
SURFACE()
);
#2204=(
BOUNDED_SURFACE()
B_SPLINE_SURFACE(1,2,((#131454,#131455,#131456),(#131457,#131458,#131459)),
 .UNSPECIFIED.,.F.,.F.,.F.)
B_SPLINE_SURFACE_WITH_KNOTS((2,2),(3,3),(0.710318915638061,1.),(0.228780950825752,
0.245954053070933),.UNSPECIFIED.)
GEOMETRIC_REPRESENTATION_ITEM()
RATIONAL_B_SPLINE_SURFACE(((0.991889110260499,0.988307723348156,0.987624841600685),
(0.991889110260499,0.988307723348156,0.987624841600685)))
REPRESENTATION_ITEM('')
SURFACE()
);
#2205=(
BOUNDED_SURFACE()
B_SPLINE_SURFACE(1,2,((#131461,#131462,#131463,#131464,#131465),(#131466,
#131467,#131468,#131469,#131470)),.UNSPECIFIED.,.F.,.F.,.F.)
B_SPLINE_SURFACE_WITH_KNOTS((2,2),(3,2,3),(0.710192959008439,1.),(0.487259899888159,
0.5,0.504824515313956),.UNSPECIFIED.)
GEOMETRIC_REPRESENTATION_ITEM()
RATIONAL_B_SPLINE_SURFACE(((0.992651440660745,0.99552810727657,1.,0.998306550597157,
0.996841863226482),(0.992651440660745,0.99552810727657,1.,0.998306550597157,
0.996841863226482)))
REPRESENTATION_ITEM('')
SURFACE()
);
#2206=(
BOUNDED_SURFACE()
B_SPLINE_SURFACE(1,2,((#131492,#131493,#131494),(#131495,#131496,#131497)),
 .UNSPECIFIED.,.F.,.F.,.F.)
B_SPLINE_SURFACE_WITH_KNOTS((2,2),(3,3),(0.710318915638065,1.),(0.228780950825752,
0.245954053070933),.UNSPECIFIED.)
GEOMETRIC_REPRESENTATION_ITEM()
RATIONAL_B_SPLINE_SURFACE(((0.9918891102605,0.988307723348156,0.987624841600685),
(0.9918891102605,0.988307723348156,0.987624841600685)))
REPRESENTATION_ITEM('')
SURFACE()
);
#2207=(
BOUNDED_SURFACE()
B_SPLINE_SURFACE(1,2,((#131499,#131500,#131501,#131502,#131503),(#131504,
#131505,#131506,#131507,#131508)),.UNSPECIFIED.,.F.,.F.,.F.)
B_SPLINE_SURFACE_WITH_KNOTS((2,2),(3,2,3),(0.710192959007031,1.),(0.487259899888159,
0.5,0.504824515313956),.UNSPECIFIED.)
GEOMETRIC_REPRESENTATION_ITEM()
RATIONAL_B_SPLINE_SURFACE(((0.992651440660745,0.99552810727657,1.,0.998306550597157,
0.996841863226482),(0.992651440660745,0.99552810727657,1.,0.998306550597157,
0.996841863226482)))
REPRESENTATION_ITEM('')
SURFACE()
);
#2208=(
BOUNDED_SURFACE()
B_SPLINE_SURFACE(1,2,((#131530,#131531,#131532),(#131533,#131534,#131535)),
 .UNSPECIFIED.,.F.,.F.,.F.)
B_SPLINE_SURFACE_WITH_KNOTS((2,2),(3,3),(0.710318915640078,1.),(0.228780950825752,
0.245954053070908),.UNSPECIFIED.)
GEOMETRIC_REPRESENTATION_ITEM()
RATIONAL_B_SPLINE_SURFACE(((0.991889110260499,0.988307723348161,0.987624841600687),
(0.991889110260499,0.988307723348161,0.987624841600687)))
REPRESENTATION_ITEM('')
SURFACE()
);
#2209=(
BOUNDED_SURFACE()
B_SPLINE_SURFACE(1,2,((#131537,#131538,#131539,#131540,#131541),(#131542,
#131543,#131544,#131545,#131546)),.UNSPECIFIED.,.F.,.F.,.F.)
B_SPLINE_SURFACE_WITH_KNOTS((2,2),(3,2,3),(0.710192959007785,1.),(0.487259899888159,
0.5,0.504824515313955),.UNSPECIFIED.)
GEOMETRIC_REPRESENTATION_ITEM()
RATIONAL_B_SPLINE_SURFACE(((0.992651440660745,0.99552810727657,1.,0.998306550597157,
0.996841863226483),(0.992651440660745,0.99552810727657,1.,0.998306550597157,
0.996841863226483)))
REPRESENTATION_ITEM('')
SURFACE()
);
#2210=(
BOUNDED_SURFACE()
B_SPLINE_SURFACE(1,2,((#131568,#131569,#131570),(#131571,#131572,#131573)),
 .UNSPECIFIED.,.F.,.F.,.F.)
B_SPLINE_SURFACE_WITH_KNOTS((2,2),(3,3),(0.710318915638065,1.),(0.228780950825753,
0.245954053070934),.UNSPECIFIED.)
GEOMETRIC_REPRESENTATION_ITEM()
RATIONAL_B_SPLINE_SURFACE(((0.991889110260499,0.988307723348156,0.987624841600685),
(0.991889110260499,0.988307723348156,0.987624841600685)))
REPRESENTATION_ITEM('')
SURFACE()
);
#2211=(
BOUNDED_SURFACE()
B_SPLINE_SURFACE(1,2,((#131575,#131576,#131577,#131578,#131579),(#131580,
#131581,#131582,#131583,#131584)),.UNSPECIFIED.,.F.,.F.,.F.)
B_SPLINE_SURFACE_WITH_KNOTS((2,2),(3,2,3),(0.710192959008349,1.),(0.487259899888158,
0.5,0.504824515313955),.UNSPECIFIED.)
GEOMETRIC_REPRESENTATION_ITEM()
RATIONAL_B_SPLINE_SURFACE(((0.992651440660745,0.995528107276569,1.,0.998306550597157,
0.996841863226483),(0.992651440660745,0.995528107276569,1.,0.998306550597157,
0.996841863226483)))
REPRESENTATION_ITEM('')
SURFACE()
);
#2212=(
BOUNDED_SURFACE()
B_SPLINE_SURFACE(1,2,((#131606,#131607,#131608),(#131609,#131610,#131611)),
 .UNSPECIFIED.,.F.,.F.,.F.)
B_SPLINE_SURFACE_WITH_KNOTS((2,2),(3,3),(0.710318915638056,1.),(0.228780950825753,
0.245954053070934),.UNSPECIFIED.)
GEOMETRIC_REPRESENTATION_ITEM()
RATIONAL_B_SPLINE_SURFACE(((0.991889110260499,0.988307723348156,0.987624841600685),
(0.991889110260499,0.988307723348156,0.987624841600685)))
REPRESENTATION_ITEM('')
SURFACE()
);
#2213=(
BOUNDED_SURFACE()
B_SPLINE_SURFACE(1,2,((#131613,#131614,#131615,#131616,#131617),(#131618,
#131619,#131620,#131621,#131622)),.UNSPECIFIED.,.F.,.F.,.F.)
B_SPLINE_SURFACE_WITH_KNOTS((2,2),(3,2,3),(0.710192959008359,1.),(0.487259899888158,
0.5,0.504824515313955),.UNSPECIFIED.)
GEOMETRIC_REPRESENTATION_ITEM()
RATIONAL_B_SPLINE_SURFACE(((0.992651440660745,0.995528107276569,1.,0.998306550597157,
0.996841863226483),(0.992651440660745,0.995528107276569,1.,0.998306550597157,
0.996841863226483)))
REPRESENTATION_ITEM('')
SURFACE()
);
#2214=(
BOUNDED_SURFACE()
B_SPLINE_SURFACE(1,2,((#131644,#131645,#131646),(#131647,#131648,#131649)),
 .UNSPECIFIED.,.F.,.F.,.F.)
B_SPLINE_SURFACE_WITH_KNOTS((2,2),(3,3),(0.710318915638063,1.),(0.228780950825753,
0.245954053070934),.UNSPECIFIED.)
GEOMETRIC_REPRESENTATION_ITEM()
RATIONAL_B_SPLINE_SURFACE(((0.991889110260499,0.988307723348156,0.987624841600685),
(0.991889110260499,0.988307723348156,0.987624841600685)))
REPRESENTATION_ITEM('')
SURFACE()
);
#2215=(
BOUNDED_SURFACE()
B_SPLINE_SURFACE(1,2,((#131651,#131652,#131653,#131654,#131655),(#131656,
#131657,#131658,#131659,#131660)),.UNSPECIFIED.,.F.,.F.,.F.)
B_SPLINE_SURFACE_WITH_KNOTS((2,2),(3,2,3),(0.710192959008363,1.),(0.487259899888158,
0.5,0.504824515313955),.UNSPECIFIED.)
GEOMETRIC_REPRESENTATION_ITEM()
RATIONAL_B_SPLINE_SURFACE(((0.992651440660745,0.995528107276569,1.,0.998306550597157,
0.996841863226482),(0.992651440660745,0.995528107276569,1.,0.998306550597157,
0.996841863226482)))
REPRESENTATION_ITEM('')
SURFACE()
);
#2216=(
BOUNDED_SURFACE()
B_SPLINE_SURFACE(1,2,((#131682,#131683,#131684),(#131685,#131686,#131687)),
 .UNSPECIFIED.,.F.,.F.,.F.)
B_SPLINE_SURFACE_WITH_KNOTS((2,2),(3,3),(0.710318915638062,1.),(0.228780950825753,
0.245954053070934),.UNSPECIFIED.)
GEOMETRIC_REPRESENTATION_ITEM()
RATIONAL_B_SPLINE_SURFACE(((0.991889110260499,0.988307723348156,0.987624841600685),
(0.991889110260499,0.988307723348156,0.987624841600685)))
REPRESENTATION_ITEM('')
SURFACE()
);
#2217=(
BOUNDED_SURFACE()
B_SPLINE_SURFACE(1,2,((#131689,#131690,#131691,#131692,#131693),(#131694,
#131695,#131696,#131697,#131698)),.UNSPECIFIED.,.F.,.F.,.F.)
B_SPLINE_SURFACE_WITH_KNOTS((2,2),(3,2,3),(0.710192959007758,1.),(0.487259899888158,
0.5,0.504824515313955),.UNSPECIFIED.)
GEOMETRIC_REPRESENTATION_ITEM()
RATIONAL_B_SPLINE_SURFACE(((0.992651440660745,0.995528107276569,1.,0.998306550597157,
0.996841863226483),(0.992651440660745,0.995528107276569,1.,0.998306550597157,
0.996841863226483)))
REPRESENTATION_ITEM('')
SURFACE()
);
#2218=(
BOUNDED_SURFACE()
B_SPLINE_SURFACE(1,2,((#131720,#131721,#131722),(#131723,#131724,#131725)),
 .UNSPECIFIED.,.F.,.F.,.F.)
B_SPLINE_SURFACE_WITH_KNOTS((2,2),(3,3),(0.710318915638052,1.),(0.228780950825681,
0.245954053070934),.UNSPECIFIED.)
GEOMETRIC_REPRESENTATION_ITEM()
RATIONAL_B_SPLINE_SURFACE(((0.991889110260529,0.988307723348159,0.987624841600685),
(0.991889110260529,0.988307723348159,0.987624841600685)))
REPRESENTATION_ITEM('')
SURFACE()
);
#2219=(
BOUNDED_SURFACE()
B_SPLINE_SURFACE(1,2,((#131727,#131728,#131729,#131730,#131731),(#131732,
#131733,#131734,#131735,#131736)),.UNSPECIFIED.,.F.,.F.,.F.)
B_SPLINE_SURFACE_WITH_KNOTS((2,2),(3,2,3),(0.710192959008391,1.),(0.487259899888158,
0.5,0.504824515313955),.UNSPECIFIED.)
GEOMETRIC_REPRESENTATION_ITEM()
RATIONAL_B_SPLINE_SURFACE(((0.992651440660745,0.99552810727657,1.,0.998306550597158,
0.996841863226483),(0.992651440660745,0.99552810727657,1.,0.998306550597158,
0.996841863226483)))
REPRESENTATION_ITEM('')
SURFACE()
);
#2220=(
BOUNDED_SURFACE()
B_SPLINE_SURFACE(1,2,((#131758,#131759,#131760),(#131761,#131762,#131763)),
 .UNSPECIFIED.,.F.,.F.,.F.)
B_SPLINE_SURFACE_WITH_KNOTS((2,2),(3,3),(0.710318915638062,1.),(0.22878095082552,
0.245954053071561),.UNSPECIFIED.)
GEOMETRIC_REPRESENTATION_ITEM()
RATIONAL_B_SPLINE_SURFACE(((0.991889110260596,0.988307723348035,0.987624841600635),
(0.991889110260596,0.988307723348035,0.987624841600635)))
REPRESENTATION_ITEM('')
SURFACE()
);
#2221=(
BOUNDED_SURFACE()
B_SPLINE_SURFACE(1,2,((#131765,#131766,#131767,#131768,#131769),(#131770,
#131771,#131772,#131773,#131774)),.UNSPECIFIED.,.F.,.F.,.F.)
B_SPLINE_SURFACE_WITH_KNOTS((2,2),(3,2,3),(0.710192959008374,1.),(0.487259899888158,
0.5,0.504824515313955),.UNSPECIFIED.)
GEOMETRIC_REPRESENTATION_ITEM()
RATIONAL_B_SPLINE_SURFACE(((0.992651440660745,0.995528107276569,1.,0.998306550597157,
0.996841863226483),(0.992651440660745,0.995528107276569,1.,0.998306550597157,
0.996841863226483)))
REPRESENTATION_ITEM('')
SURFACE()
);
#2222=(
BOUNDED_SURFACE()
B_SPLINE_SURFACE(1,2,((#131796,#131797,#131798),(#131799,#131800,#131801)),
 .UNSPECIFIED.,.F.,.F.,.F.)
B_SPLINE_SURFACE_WITH_KNOTS((2,2),(3,3),(0.710318915638058,1.),(0.228780950825311,
0.245954053070934),.UNSPECIFIED.)
GEOMETRIC_REPRESENTATION_ITEM()
RATIONAL_B_SPLINE_SURFACE(((0.991889110260684,0.988307723348174,0.987624841600685),
(0.991889110260683,0.988307723348174,0.987624841600685)))
REPRESENTATION_ITEM('')
SURFACE()
);
#2223=(
BOUNDED_SURFACE()
B_SPLINE_SURFACE(1,2,((#131803,#131804,#131805,#131806,#131807),(#131808,
#131809,#131810,#131811,#131812)),.UNSPECIFIED.,.F.,.F.,.F.)
B_SPLINE_SURFACE_WITH_KNOTS((2,2),(3,2,3),(0.710192959008376,1.),(0.487259899888158,
0.5,0.504824515313552),.UNSPECIFIED.)
GEOMETRIC_REPRESENTATION_ITEM()
RATIONAL_B_SPLINE_SURFACE(((0.992651440660745,0.995528107276569,1.,0.998306550597299,
0.996841863226727),(0.992651440660745,0.995528107276569,1.,0.998306550597299,
0.996841863226727)))
REPRESENTATION_ITEM('')
SURFACE()
);
#2224=(
BOUNDED_SURFACE()
B_SPLINE_SURFACE(1,2,((#131823,#131824,#131825),(#131826,#131827,#131828)),
 .UNSPECIFIED.,.F.,.F.,.F.)
B_SPLINE_SURFACE_WITH_KNOTS((2,2),(3,3),(0.,0.289807040991559),(0.53899963051341,
0.556316102183953),.UNSPECIFIED.)
GEOMETRIC_REPRESENTATION_ITEM()
RATIONAL_B_SPLINE_SURFACE(((0.987570037304351,0.988129172627919,0.99163541140107),
(0.987570037304351,0.988129172627919,0.99163541140107)))
REPRESENTATION_ITEM('')
SURFACE()
);
#2225=(
BOUNDED_SURFACE()
B_SPLINE_SURFACE(1,2,((#131837,#131838,#131839,#131840,#131841),(#131842,
#131843,#131844,#131845,#131846)),.UNSPECIFIED.,.F.,.F.,.F.)
B_SPLINE_SURFACE_WITH_KNOTS((2,2),(3,2,3),(0.,0.290279631762495),(0.176864064841898,
0.194132688793569,0.194731236520879),.UNSPECIFIED.)
GEOMETRIC_REPRESENTATION_ITEM()
RATIONAL_B_SPLINE_SURFACE(((0.987492606357657,0.987202831733786,0.989843896581211,
0.989843896581211,0.989843896581211),(0.987492606357657,0.987202831733786,
0.989843896581211,0.989843896581211,0.989843896581211)))
REPRESENTATION_ITEM('')
SURFACE()
);
#2226=(
BOUNDED_SURFACE()
B_SPLINE_SURFACE(1,2,((#131855,#131856,#131857),(#131858,#131859,#131860),
(#131861,#131862,#131863)),.UNSPECIFIED.,.F.,.F.,.F.)
B_SPLINE_SURFACE_WITH_KNOTS((2,1,2),(3,3),(-0.0028980704099156,0.,0.28980704099156),
(0.53899963051341,0.556316102183953),.UNSPECIFIED.)
GEOMETRIC_REPRESENTATION_ITEM()
RATIONAL_B_SPLINE_SURFACE(((0.987570037304351,0.988129172627919,0.99163541140107),
(0.987570037304351,0.988129172627919,0.99163541140107),(0.987570037304351,
0.988129172627919,0.99163541140107)))
REPRESENTATION_ITEM('')
SURFACE()
);
#2227=(
BOUNDED_SURFACE()
B_SPLINE_SURFACE(1,2,((#131865,#131866,#131867,#131868,#131869),(#131870,
#131871,#131872,#131873,#131874)),.UNSPECIFIED.,.F.,.F.,.F.)
B_SPLINE_SURFACE_WITH_KNOTS((2,2),(3,2,3),(0.,0.290279631761532),(0.176864064841898,
0.194132688793569,0.194731236519916),.UNSPECIFIED.)
GEOMETRIC_REPRESENTATION_ITEM()
RATIONAL_B_SPLINE_SURFACE(((0.987492606357657,0.987202831733786,0.989843896581211,
0.989843896581211,0.989843896581211),(0.987492606357657,0.987202831733786,
0.989843896581211,0.989843896581211,0.989843896581211)))
REPRESENTATION_ITEM('')
SURFACE()
);
#2228=(
BOUNDED_SURFACE()
B_SPLINE_SURFACE(1,2,((#131883,#131884,#131885),(#131886,#131887,#131888),
(#131889,#131890,#131891)),.UNSPECIFIED.,.F.,.F.,.F.)
B_SPLINE_SURFACE_WITH_KNOTS((2,1,2),(3,3),(-0.00289807040992491,0.,0.289807040992491),
(0.53899963051341,0.556316102183953),.UNSPECIFIED.)
GEOMETRIC_REPRESENTATION_ITEM()
RATIONAL_B_SPLINE_SURFACE(((0.987570037304351,0.988129172627919,0.99163541140107),
(0.987570037304351,0.988129172627919,0.99163541140107),(0.987570037304351,
0.988129172627919,0.99163541140107)))
REPRESENTATION_ITEM('')
SURFACE()
);
#2229=(
BOUNDED_SURFACE()
B_SPLINE_SURFACE(1,2,((#131893,#131894,#131895,#131896,#131897),(#131898,
#131899,#131900,#131901,#131902)),.UNSPECIFIED.,.F.,.F.,.F.)
B_SPLINE_SURFACE_WITH_KNOTS((2,2),(3,2,3),(0.,0.290279631742111),(0.176864064841898,
0.194132688793569,0.194731236500496),.UNSPECIFIED.)
GEOMETRIC_REPRESENTATION_ITEM()
RATIONAL_B_SPLINE_SURFACE(((0.987492606357657,0.987202831733786,0.989843896581211,
0.989843896581211,0.989843896581211),(0.987492606357657,0.987202831733785,
0.989843896581211,0.989843896581211,0.989843896581211)))
REPRESENTATION_ITEM('')
SURFACE()
);
#2230=(
BOUNDED_SURFACE()
B_SPLINE_SURFACE(1,2,((#131911,#131912,#131913),(#131914,#131915,#131916),
(#131917,#131918,#131919)),.UNSPECIFIED.,.F.,.F.,.F.)
B_SPLINE_SURFACE_WITH_KNOTS((2,1,2),(3,3),(-0.00289807040992489,0.,0.289807040992489),
(0.53899963051341,0.556316102183953),.UNSPECIFIED.)
GEOMETRIC_REPRESENTATION_ITEM()
RATIONAL_B_SPLINE_SURFACE(((0.987570037304351,0.988129172627919,0.99163541140107),
(0.987570037304351,0.988129172627919,0.99163541140107),(0.987570037304351,
0.988129172627919,0.99163541140107)))
REPRESENTATION_ITEM('')
SURFACE()
);
#2231=(
BOUNDED_SURFACE()
B_SPLINE_SURFACE(1,2,((#131921,#131922,#131923,#131924,#131925),(#131926,
#131927,#131928,#131929,#131930)),.UNSPECIFIED.,.F.,.F.,.F.)
B_SPLINE_SURFACE_WITH_KNOTS((2,2),(3,2,3),(0.,0.290279631766158),(0.176864064841898,
0.194132688793569,0.194731236524534),.UNSPECIFIED.)
GEOMETRIC_REPRESENTATION_ITEM()
RATIONAL_B_SPLINE_SURFACE(((0.987492606357657,0.987202831733786,0.989843896581211,
0.989843896581211,0.989843896581211),(0.987492606357657,0.987202831733786,
0.989843896581211,0.989843896581211,0.989843896581211)))
REPRESENTATION_ITEM('')
SURFACE()
);
#2232=(
BOUNDED_SURFACE()
B_SPLINE_SURFACE(1,2,((#131939,#131940,#131941),(#131942,#131943,#131944),
(#131945,#131946,#131947)),.UNSPECIFIED.,.F.,.F.,.F.)
B_SPLINE_SURFACE_WITH_KNOTS((2,1,2),(3,3),(-0.00289807040992489,0.,0.289807040992489),
(0.53899963051341,0.556316102183953),.UNSPECIFIED.)
GEOMETRIC_REPRESENTATION_ITEM()
RATIONAL_B_SPLINE_SURFACE(((0.987570037304351,0.988129172627919,0.99163541140107),
(0.987570037304351,0.988129172627919,0.99163541140107),(0.987570037304351,
0.988129172627919,0.99163541140107)))
REPRESENTATION_ITEM('')
SURFACE()
);
#2233=(
BOUNDED_SURFACE()
B_SPLINE_SURFACE(1,2,((#131949,#131950,#131951,#131952,#131953),(#131954,
#131955,#131956,#131957,#131958)),.UNSPECIFIED.,.F.,.F.,.F.)
B_SPLINE_SURFACE_WITH_KNOTS((2,2),(3,2,3),(0.,0.290279631775689),(0.176864064841898,
0.194132688793569,0.194731236534068),.UNSPECIFIED.)
GEOMETRIC_REPRESENTATION_ITEM()
RATIONAL_B_SPLINE_SURFACE(((0.987492606357657,0.987202831733786,0.989843896581211,
0.989843896581211,0.989843896581211),(0.987492606357657,0.987202831733786,
0.989843896581211,0.989843896581211,0.989843896581211)))
REPRESENTATION_ITEM('')
SURFACE()
);
#2234=(
BOUNDED_SURFACE()
B_SPLINE_SURFACE(1,2,((#131967,#131968,#131969),(#131970,#131971,#131972),
(#131973,#131974,#131975)),.UNSPECIFIED.,.F.,.F.,.F.)
B_SPLINE_SURFACE_WITH_KNOTS((2,1,2),(3,3),(-0.0028980704099307,0.,0.28980704099307),
(0.53899963051341,0.556316102183953),.UNSPECIFIED.)
GEOMETRIC_REPRESENTATION_ITEM()
RATIONAL_B_SPLINE_SURFACE(((0.987570037304351,0.988129172627919,0.99163541140107),
(0.987570037304351,0.988129172627919,0.99163541140107),(0.987570037304351,
0.988129172627919,0.99163541140107)))
REPRESENTATION_ITEM('')
SURFACE()
);
#2235=(
BOUNDED_SURFACE()
B_SPLINE_SURFACE(1,2,((#131977,#131978,#131979,#131980,#131981),(#131982,
#131983,#131984,#131985,#131986)),.UNSPECIFIED.,.F.,.F.,.F.)
B_SPLINE_SURFACE_WITH_KNOTS((2,2),(3,2,3),(0.,0.290279631757529),(0.176864064841898,
0.194132688793569,0.194731236515912),.UNSPECIFIED.)
GEOMETRIC_REPRESENTATION_ITEM()
RATIONAL_B_SPLINE_SURFACE(((0.987492606357657,0.987202831733786,0.989843896581211,
0.989843896581211,0.989843896581211),(0.987492606357657,0.987202831733786,
0.989843896581211,0.989843896581211,0.989843896581211)))
REPRESENTATION_ITEM('')
SURFACE()
);
#2236=(
BOUNDED_SURFACE()
B_SPLINE_SURFACE(1,2,((#131995,#131996,#131997),(#131998,#131999,#132000),
(#132001,#132002,#132003)),.UNSPECIFIED.,.F.,.F.,.F.)
B_SPLINE_SURFACE_WITH_KNOTS((2,1,2),(3,3),(-0.00289807040992488,0.,0.289807040992488),
(0.53899963051341,0.556316102183954),.UNSPECIFIED.)
GEOMETRIC_REPRESENTATION_ITEM()
RATIONAL_B_SPLINE_SURFACE(((0.987570037304351,0.988129172627919,0.99163541140107),
(0.987570037304351,0.988129172627919,0.99163541140107),(0.987570037304351,
0.988129172627919,0.99163541140107)))
REPRESENTATION_ITEM('')
SURFACE()
);
#2237=(
BOUNDED_SURFACE()
B_SPLINE_SURFACE(1,2,((#132005,#132006,#132007,#132008,#132009),(#132010,
#132011,#132012,#132013,#132014)),.UNSPECIFIED.,.F.,.F.,.F.)
B_SPLINE_SURFACE_WITH_KNOTS((2,2),(3,2,3),(0.,0.290279631749781),(0.176864064841898,
0.194132688793569,0.19473123650816),.UNSPECIFIED.)
GEOMETRIC_REPRESENTATION_ITEM()
RATIONAL_B_SPLINE_SURFACE(((0.987492606357657,0.987202831733786,0.989843896581211,
0.989843896581211,0.989843896581211),(0.987492606357657,0.987202831733786,
0.989843896581211,0.989843896581211,0.989843896581211)))
REPRESENTATION_ITEM('')
SURFACE()
);
#2238=(
BOUNDED_SURFACE()
B_SPLINE_SURFACE(1,2,((#132023,#132024,#132025),(#132026,#132027,#132028),
(#132029,#132030,#132031)),.UNSPECIFIED.,.F.,.F.,.F.)
B_SPLINE_SURFACE_WITH_KNOTS((2,1,2),(3,3),(-0.0028980704099307,0.,0.28980704099307),
(0.53899963051341,0.556316102183953),.UNSPECIFIED.)
GEOMETRIC_REPRESENTATION_ITEM()
RATIONAL_B_SPLINE_SURFACE(((0.987570037304351,0.988129172627919,0.99163541140107),
(0.987570037304351,0.988129172627919,0.99163541140107),(0.987570037304351,
0.988129172627919,0.99163541140107)))
REPRESENTATION_ITEM('')
SURFACE()
);
#2239=(
BOUNDED_SURFACE()
B_SPLINE_SURFACE(1,2,((#132033,#132034,#132035,#132036,#132037),(#132038,
#132039,#132040,#132041,#132042)),.UNSPECIFIED.,.F.,.F.,.F.)
B_SPLINE_SURFACE_WITH_KNOTS((2,2),(3,2,3),(0.,0.29027963174592),(0.176864064841898,
0.194132688793569,0.194731236504307),.UNSPECIFIED.)
GEOMETRIC_REPRESENTATION_ITEM()
RATIONAL_B_SPLINE_SURFACE(((0.987492606357657,0.987202831733786,0.989843896581211,
0.989843896581211,0.989843896581211),(0.987492606357657,0.987202831733786,
0.989843896581211,0.989843896581211,0.989843896581211)))
REPRESENTATION_ITEM('')
SURFACE()
);
#2240=(
BOUNDED_SURFACE()
B_SPLINE_SURFACE(1,2,((#132051,#132052,#132053),(#132054,#132055,#132056),
(#132057,#132058,#132059)),.UNSPECIFIED.,.F.,.F.,.F.)
B_SPLINE_SURFACE_WITH_KNOTS((2,1,2),(3,3),(-0.00289807040992572,0.,0.289807040992572),
(0.538999630513411,0.556316102183953),.UNSPECIFIED.)
GEOMETRIC_REPRESENTATION_ITEM()
RATIONAL_B_SPLINE_SURFACE(((0.987570037304351,0.988129172627919,0.99163541140107),
(0.987570037304351,0.988129172627919,0.99163541140107),(0.987570037304351,
0.988129172627919,0.99163541140107)))
REPRESENTATION_ITEM('')
SURFACE()
);
#2241=(
BOUNDED_SURFACE()
B_SPLINE_SURFACE(1,2,((#132061,#132062,#132063,#132064,#132065),(#132066,
#132067,#132068,#132069,#132070)),.UNSPECIFIED.,.F.,.F.,.F.)
B_SPLINE_SURFACE_WITH_KNOTS((2,2),(3,2,3),(0.,0.290279631772035),(0.176864064841897,
0.194132688793568,0.194731236530414),.UNSPECIFIED.)
GEOMETRIC_REPRESENTATION_ITEM()
RATIONAL_B_SPLINE_SURFACE(((0.987492606357657,0.987202831733786,0.989843896581211,
0.989843896581211,0.989843896581211),(0.987492606357657,0.987202831733786,
0.989843896581211,0.989843896581211,0.989843896581211)))
REPRESENTATION_ITEM('')
SURFACE()
);
#2242=(
BOUNDED_SURFACE()
B_SPLINE_SURFACE(1,2,((#132079,#132080,#132081),(#132082,#132083,#132084),
(#132085,#132086,#132087)),.UNSPECIFIED.,.F.,.F.,.F.)
B_SPLINE_SURFACE_WITH_KNOTS((2,1,2),(3,3),(-0.00289807040992567,0.,0.289807040992567),
(0.538999630513411,0.556316102183955),.UNSPECIFIED.)
GEOMETRIC_REPRESENTATION_ITEM()
RATIONAL_B_SPLINE_SURFACE(((0.987570037304351,0.988129172627919,0.99163541140107),
(0.987570037304351,0.988129172627919,0.99163541140107),(0.987570037304351,
0.988129172627919,0.99163541140107)))
REPRESENTATION_ITEM('')
SURFACE()
);
#2243=(
BOUNDED_SURFACE()
B_SPLINE_SURFACE(1,2,((#132089,#132090,#132091,#132092,#132093),(#132094,
#132095,#132096,#132097,#132098)),.UNSPECIFIED.,.F.,.F.,.F.)
B_SPLINE_SURFACE_WITH_KNOTS((2,2),(3,2,3),(0.,0.290279631748006),(0.176864064841897,
0.194132688793568,0.194731236506389),.UNSPECIFIED.)
GEOMETRIC_REPRESENTATION_ITEM()
RATIONAL_B_SPLINE_SURFACE(((0.987492606357657,0.987202831733786,0.989843896581211,
0.989843896581211,0.989843896581211),(0.987492606357657,0.987202831733786,
0.989843896581211,0.989843896581211,0.989843896581211)))
REPRESENTATION_ITEM('')
SURFACE()
);
#2244=(
BOUNDED_SURFACE()
B_SPLINE_SURFACE(1,2,((#132107,#132108,#132109),(#132110,#132111,#132112),
(#132113,#132114,#132115)),.UNSPECIFIED.,.F.,.F.,.F.)
B_SPLINE_SURFACE_WITH_KNOTS((2,1,2),(3,3),(-0.00289807040993166,0.,0.289807040993166),
(0.538999630513411,0.556316102183954),.UNSPECIFIED.)
GEOMETRIC_REPRESENTATION_ITEM()
RATIONAL_B_SPLINE_SURFACE(((0.987570037304351,0.988129172627919,0.99163541140107),
(0.987570037304351,0.988129172627919,0.99163541140107),(0.987570037304351,
0.988129172627919,0.99163541140107)))
REPRESENTATION_ITEM('')
SURFACE()
);
#2245=(
BOUNDED_SURFACE()
B_SPLINE_SURFACE(1,2,((#132117,#132118,#132119,#132120,#132121),(#132122,
#132123,#132124,#132125,#132126)),.UNSPECIFIED.,.F.,.F.,.F.)
B_SPLINE_SURFACE_WITH_KNOTS((2,2),(3,2,3),(0.,0.290279631752551),(0.176864064841897,
0.194132688793568,0.194731236510931),.UNSPECIFIED.)
GEOMETRIC_REPRESENTATION_ITEM()
RATIONAL_B_SPLINE_SURFACE(((0.987492606357657,0.987202831733785,0.98984389658121,
0.98984389658121,0.98984389658121),(0.987492606357657,0.987202831733785,
0.98984389658121,0.98984389658121,0.98984389658121)))
REPRESENTATION_ITEM('')
SURFACE()
);
#2246=(
BOUNDED_SURFACE()
B_SPLINE_SURFACE(1,2,((#132135,#132136,#132137),(#132138,#132139,#132140),
(#132141,#132142,#132143)),.UNSPECIFIED.,.F.,.F.,.F.)
B_SPLINE_SURFACE_WITH_KNOTS((2,1,2),(3,3),(-0.00289807040992572,0.,0.289807040992572),
(0.538999630513411,0.556316102183955),.UNSPECIFIED.)
GEOMETRIC_REPRESENTATION_ITEM()
RATIONAL_B_SPLINE_SURFACE(((0.987570037304351,0.988129172627919,0.99163541140107),
(0.987570037304351,0.988129172627919,0.99163541140107),(0.987570037304351,
0.988129172627919,0.99163541140107)))
REPRESENTATION_ITEM('')
SURFACE()
);
#2247=(
BOUNDED_SURFACE()
B_SPLINE_SURFACE(1,2,((#132145,#132146,#132147,#132148,#132149),(#132150,
#132151,#132152,#132153,#132154)),.UNSPECIFIED.,.F.,.F.,.F.)
B_SPLINE_SURFACE_WITH_KNOTS((2,2),(3,2,3),(0.,0.290279631773371),(0.176864064841897,
0.194132688793568,0.194731236531752),.UNSPECIFIED.)
GEOMETRIC_REPRESENTATION_ITEM()
RATIONAL_B_SPLINE_SURFACE(((0.987492606357657,0.987202831733786,0.989843896581211,
0.989843896581211,0.989843896581211),(0.987492606357657,0.987202831733786,
0.989843896581211,0.989843896581211,0.989843896581211)))
REPRESENTATION_ITEM('')
SURFACE()
);
#2248=(
BOUNDED_SURFACE()
B_SPLINE_SURFACE(1,2,((#132163,#132164,#132165),(#132166,#132167,#132168),
(#132169,#132170,#132171)),.UNSPECIFIED.,.F.,.F.,.F.)
B_SPLINE_SURFACE_WITH_KNOTS((2,1,2),(3,3),(-0.00289807040993075,0.,0.289807040993075),
(0.538999630513411,0.556316102183955),.UNSPECIFIED.)
GEOMETRIC_REPRESENTATION_ITEM()
RATIONAL_B_SPLINE_SURFACE(((0.987570037304351,0.988129172627919,0.99163541140107),
(0.987570037304351,0.988129172627919,0.99163541140107),(0.987570037304351,
0.988129172627919,0.99163541140107)))
REPRESENTATION_ITEM('')
SURFACE()
);
#2249=(
BOUNDED_SURFACE()
B_SPLINE_SURFACE(1,2,((#132173,#132174,#132175,#132176,#132177),(#132178,
#132179,#132180,#132181,#132182)),.UNSPECIFIED.,.F.,.F.,.F.)
B_SPLINE_SURFACE_WITH_KNOTS((2,2),(3,2,3),(0.,0.2902796317778),(0.176864064841897,
0.194132688793568,0.194731236536179),.UNSPECIFIED.)
GEOMETRIC_REPRESENTATION_ITEM()
RATIONAL_B_SPLINE_SURFACE(((0.987492606357657,0.987202831733786,0.989843896581211,
0.989843896581211,0.989843896581211),(0.987492606357657,0.987202831733786,
0.989843896581211,0.989843896581211,0.989843896581211)))
REPRESENTATION_ITEM('')
SURFACE()
);
#2250=(
BOUNDED_SURFACE()
B_SPLINE_SURFACE(1,2,((#132191,#132192,#132193),(#132194,#132195,#132196),
(#132197,#132198,#132199)),.UNSPECIFIED.,.F.,.F.,.F.)
B_SPLINE_SURFACE_WITH_KNOTS((2,1,2),(3,3),(-0.00289807040992579,0.,0.289807040992579),
(0.538999630513411,0.556316102183955),.UNSPECIFIED.)
GEOMETRIC_REPRESENTATION_ITEM()
RATIONAL_B_SPLINE_SURFACE(((0.987570037304351,0.988129172627919,0.99163541140107),
(0.987570037304351,0.988129172627919,0.99163541140107),(0.987570037304351,
0.988129172627919,0.99163541140107)))
REPRESENTATION_ITEM('')
SURFACE()
);
#2251=(
BOUNDED_SURFACE()
B_SPLINE_SURFACE(1,2,((#132201,#132202,#132203,#132204,#132205),(#132206,
#132207,#132208,#132209,#132210)),.UNSPECIFIED.,.F.,.F.,.F.)
B_SPLINE_SURFACE_WITH_KNOTS((2,2),(3,2,3),(0.,0.290279631762204),(0.176864064841897,
0.194132688793568,0.194731236520584),.UNSPECIFIED.)
GEOMETRIC_REPRESENTATION_ITEM()
RATIONAL_B_SPLINE_SURFACE(((0.987492606357657,0.987202831733786,0.989843896581211,
0.989843896581211,0.989843896581211),(0.987492606357657,0.987202831733786,
0.989843896581211,0.989843896581211,0.989843896581211)))
REPRESENTATION_ITEM('')
SURFACE()
);
#2252=(
BOUNDED_SURFACE()
B_SPLINE_SURFACE(1,2,((#132219,#132220,#132221),(#132222,#132223,#132224),
(#132225,#132226,#132227)),.UNSPECIFIED.,.F.,.F.,.F.)
B_SPLINE_SURFACE_WITH_KNOTS((2,1,2),(3,3),(-0.00289807040993075,0.,0.289807040993075),
(0.538999630513411,0.556316102183955),.UNSPECIFIED.)
GEOMETRIC_REPRESENTATION_ITEM()
RATIONAL_B_SPLINE_SURFACE(((0.987570037304351,0.988129172627919,0.99163541140107),
(0.987570037304351,0.988129172627919,0.99163541140107),(0.987570037304351,
0.988129172627919,0.99163541140107)))
REPRESENTATION_ITEM('')
SURFACE()
);
#2253=(
BOUNDED_SURFACE()
B_SPLINE_SURFACE(1,2,((#132229,#132230,#132231,#132232,#132233),(#132234,
#132235,#132236,#132237,#132238)),.UNSPECIFIED.,.F.,.F.,.F.)
B_SPLINE_SURFACE_WITH_KNOTS((2,2),(3,2,3),(0.,0.290279631773358),(0.176864064841897,
0.194132688793568,0.194731236531739),.UNSPECIFIED.)
GEOMETRIC_REPRESENTATION_ITEM()
RATIONAL_B_SPLINE_SURFACE(((0.987492606357657,0.987202831733786,0.989843896581211,
0.989843896581211,0.989843896581211),(0.987492606357657,0.987202831733786,
0.989843896581211,0.989843896581211,0.989843896581211)))
REPRESENTATION_ITEM('')
SURFACE()
);
#2254=(
BOUNDED_SURFACE()
B_SPLINE_SURFACE(1,2,((#132247,#132248,#132249),(#132250,#132251,#132252),
(#132253,#132254,#132255)),.UNSPECIFIED.,.F.,.F.,.F.)
B_SPLINE_SURFACE_WITH_KNOTS((2,1,2),(3,3),(-0.00289807040992848,0.,0.289807040992848),
(0.538999630513411,0.556316102183955),.UNSPECIFIED.)
GEOMETRIC_REPRESENTATION_ITEM()
RATIONAL_B_SPLINE_SURFACE(((0.987570037304351,0.988129172627919,0.99163541140107),
(0.987570037304351,0.988129172627919,0.99163541140107),(0.987570037304351,
0.988129172627919,0.99163541140107)))
REPRESENTATION_ITEM('')
SURFACE()
);
#2255=(
BOUNDED_SURFACE()
B_SPLINE_SURFACE(1,2,((#132257,#132258,#132259,#132260,#132261),(#132262,
#132263,#132264,#132265,#132266)),.UNSPECIFIED.,.F.,.F.,.F.)
B_SPLINE_SURFACE_WITH_KNOTS((2,2),(3,2,3),(0.,0.290279631764032),(0.176864064841897,
0.194132688793568,0.194731236522411),.UNSPECIFIED.)
GEOMETRIC_REPRESENTATION_ITEM()
RATIONAL_B_SPLINE_SURFACE(((0.987492606357657,0.987202831733786,0.989843896581211,
0.989843896581211,0.989843896581211),(0.987492606357657,0.987202831733786,
0.989843896581211,0.989843896581211,0.989843896581211)))
REPRESENTATION_ITEM('')
SURFACE()
);
#2256=(
BOUNDED_SURFACE()
B_SPLINE_SURFACE(1,2,((#132275,#132276,#132277),(#132278,#132279,#132280),
(#132281,#132282,#132283)),.UNSPECIFIED.,.F.,.F.,.F.)
B_SPLINE_SURFACE_WITH_KNOTS((2,1,2),(3,3),(-0.00289807040993903,0.,0.289807040993903),
(0.538999630513411,0.556316102183955),.UNSPECIFIED.)
GEOMETRIC_REPRESENTATION_ITEM()
RATIONAL_B_SPLINE_SURFACE(((0.987570037304351,0.988129172627919,0.99163541140107),
(0.987570037304351,0.988129172627919,0.99163541140107),(0.987570037304351,
0.988129172627919,0.99163541140107)))
REPRESENTATION_ITEM('')
SURFACE()
);
#2257=(
BOUNDED_SURFACE()
B_SPLINE_SURFACE(1,2,((#132285,#132286,#132287,#132288,#132289),(#132290,
#132291,#132292,#132293,#132294)),.UNSPECIFIED.,.F.,.F.,.F.)
B_SPLINE_SURFACE_WITH_KNOTS((2,2),(3,2,3),(0.,0.290279631752155),(0.176864064841897,
0.194132688793568,0.194731236510534),.UNSPECIFIED.)
GEOMETRIC_REPRESENTATION_ITEM()
RATIONAL_B_SPLINE_SURFACE(((0.987492606357657,0.987202831733786,0.98984389658121,
0.98984389658121,0.98984389658121),(0.987492606357657,0.987202831733786,
0.989843896581211,0.989843896581211,0.989843896581211)))
REPRESENTATION_ITEM('')
SURFACE()
);
#2258=(
BOUNDED_SURFACE()
B_SPLINE_SURFACE(1,2,((#132303,#132304,#132305),(#132306,#132307,#132308),
(#132309,#132310,#132311)),.UNSPECIFIED.,.F.,.F.,.F.)
B_SPLINE_SURFACE_WITH_KNOTS((2,1,2),(3,3),(-0.00289807040992612,0.,0.289807040992612),
(0.538999630513411,0.556316102183954),.UNSPECIFIED.)
GEOMETRIC_REPRESENTATION_ITEM()
RATIONAL_B_SPLINE_SURFACE(((0.987570037304351,0.988129172627919,0.99163541140107),
(0.987570037304351,0.988129172627919,0.99163541140107),(0.987570037304351,
0.988129172627919,0.99163541140107)))
REPRESENTATION_ITEM('')
SURFACE()
);
#2259=(
BOUNDED_SURFACE()
B_SPLINE_SURFACE(1,2,((#132313,#132314,#132315,#132316,#132317),(#132318,
#132319,#132320,#132321,#132322)),.UNSPECIFIED.,.F.,.F.,.F.)
B_SPLINE_SURFACE_WITH_KNOTS((2,2),(3,2,3),(0.,0.290279631748086),(0.176864064841897,
0.194132688793568,0.194731236506461),.UNSPECIFIED.)
GEOMETRIC_REPRESENTATION_ITEM()
RATIONAL_B_SPLINE_SURFACE(((0.987492606357657,0.987202831733786,0.98984389658121,
0.98984389658121,0.98984389658121),(0.987492606357657,0.987202831733786,
0.989843896581211,0.989843896581211,0.989843896581211)))
REPRESENTATION_ITEM('')
SURFACE()
);
#2260=(
BOUNDED_SURFACE()
B_SPLINE_SURFACE(1,2,((#132331,#132332,#132333),(#132334,#132335,#132336),
(#132337,#132338,#132339)),.UNSPECIFIED.,.F.,.F.,.F.)
B_SPLINE_SURFACE_WITH_KNOTS((2,1,2),(3,3),(-0.00289807040992496,0.,0.289807040992496),
(0.538999630513411,0.556316102183955),.UNSPECIFIED.)
GEOMETRIC_REPRESENTATION_ITEM()
RATIONAL_B_SPLINE_SURFACE(((0.987570037304351,0.988129172627919,0.99163541140107),
(0.987570037304351,0.988129172627919,0.99163541140107),(0.987570037304351,
0.988129172627919,0.99163541140107)))
REPRESENTATION_ITEM('')
SURFACE()
);
#2261=(
BOUNDED_SURFACE()
B_SPLINE_SURFACE(1,2,((#132341,#132342,#132343,#132344,#132345),(#132346,
#132347,#132348,#132349,#132350)),.UNSPECIFIED.,.F.,.F.,.F.)
B_SPLINE_SURFACE_WITH_KNOTS((2,2),(3,2,3),(0.,0.290279631782441),(0.176864064841897,
0.194132688793568,0.194731236540818),.UNSPECIFIED.)
GEOMETRIC_REPRESENTATION_ITEM()
RATIONAL_B_SPLINE_SURFACE(((0.987492606357657,0.987202831733786,0.989843896581211,
0.989843896581211,0.989843896581211),(0.987492606357657,0.987202831733786,
0.989843896581211,0.989843896581211,0.989843896581211)))
REPRESENTATION_ITEM('')
SURFACE()
);
#2262=(
BOUNDED_SURFACE()
B_SPLINE_SURFACE(1,2,((#132359,#132360,#132361),(#132362,#132363,#132364),
(#132365,#132366,#132367)),.UNSPECIFIED.,.F.,.F.,.F.)
B_SPLINE_SURFACE_WITH_KNOTS((2,1,2),(3,3),(-0.00289807040993131,0.,0.289807040993131),
(0.538999630513411,0.556316102183955),.UNSPECIFIED.)
GEOMETRIC_REPRESENTATION_ITEM()
RATIONAL_B_SPLINE_SURFACE(((0.987570037304351,0.988129172627919,0.99163541140107),
(0.987570037304351,0.988129172627919,0.99163541140107),(0.987570037304351,
0.988129172627919,0.99163541140107)))
REPRESENTATION_ITEM('')
SURFACE()
);
#2263=(
BOUNDED_SURFACE()
B_SPLINE_SURFACE(1,2,((#132369,#132370,#132371,#132372,#132373),(#132374,
#132375,#132376,#132377,#132378)),.UNSPECIFIED.,.F.,.F.,.F.)
B_SPLINE_SURFACE_WITH_KNOTS((2,2),(3,2,3),(0.,0.290279631760911),(0.176864064841897,
0.194132688793568,0.194731236519285),.UNSPECIFIED.)
GEOMETRIC_REPRESENTATION_ITEM()
RATIONAL_B_SPLINE_SURFACE(((0.987492606357657,0.987202831733786,0.989843896581211,
0.989843896581211,0.989843896581211),(0.987492606357657,0.987202831733786,
0.989843896581211,0.989843896581211,0.989843896581211)))
REPRESENTATION_ITEM('')
SURFACE()
);
#2264=(
BOUNDED_SURFACE()
B_SPLINE_SURFACE(1,2,((#132387,#132388,#132389),(#132390,#132391,#132392),
(#132393,#132394,#132395)),.UNSPECIFIED.,.F.,.F.,.F.)
B_SPLINE_SURFACE_WITH_KNOTS((2,1,2),(3,3),(-0.00289807040991731,0.,0.289807040991731),
(0.538999630513411,0.556316102183955),.UNSPECIFIED.)
GEOMETRIC_REPRESENTATION_ITEM()
RATIONAL_B_SPLINE_SURFACE(((0.987570037304351,0.988129172627919,0.99163541140107),
(0.987570037304351,0.988129172627919,0.99163541140107),(0.987570037304351,
0.988129172627919,0.99163541140107)))
REPRESENTATION_ITEM('')
SURFACE()
);
#2265=(
BOUNDED_SURFACE()
B_SPLINE_SURFACE(1,2,((#132397,#132398,#132399,#132400,#132401),(#132402,
#132403,#132404,#132405,#132406)),.UNSPECIFIED.,.F.,.F.,.F.)
B_SPLINE_SURFACE_WITH_KNOTS((2,2),(3,2,3),(0.,0.290279631775496),(0.176864064841897,
0.194132688793569,0.194731236533875),.UNSPECIFIED.)
GEOMETRIC_REPRESENTATION_ITEM()
RATIONAL_B_SPLINE_SURFACE(((0.987492606357657,0.987202831733786,0.989843896581211,
0.989843896581211,0.989843896581211),(0.987492606357657,0.987202831733786,
0.989843896581211,0.989843896581211,0.989843896581211)))
REPRESENTATION_ITEM('')
SURFACE()
);
#2266=(
BOUNDED_SURFACE()
B_SPLINE_SURFACE(1,2,((#132415,#132416,#132417),(#132418,#132419,#132420),
(#132421,#132422,#132423)),.UNSPECIFIED.,.F.,.F.,.F.)
B_SPLINE_SURFACE_WITH_KNOTS((2,1,2),(3,3),(-0.00289807040992881,0.,0.289807040992881),
(0.538999630513411,0.556316102183955),.UNSPECIFIED.)
GEOMETRIC_REPRESENTATION_ITEM()
RATIONAL_B_SPLINE_SURFACE(((0.987570037304351,0.988129172627919,0.99163541140107),
(0.987570037304351,0.988129172627919,0.99163541140107),(0.987570037304351,
0.988129172627919,0.99163541140107)))
REPRESENTATION_ITEM('')
SURFACE()
);
#2267=(
BOUNDED_SURFACE()
B_SPLINE_SURFACE(1,2,((#132425,#132426,#132427,#132428,#132429),(#132430,
#132431,#132432,#132433,#132434)),.UNSPECIFIED.,.F.,.F.,.F.)
B_SPLINE_SURFACE_WITH_KNOTS((2,2),(3,2,3),(0.,0.290279631758543),(0.176864064841897,
0.194132688793568,0.194731236516916),.UNSPECIFIED.)
GEOMETRIC_REPRESENTATION_ITEM()
RATIONAL_B_SPLINE_SURFACE(((0.987492606357657,0.987202831733786,0.989843896581211,
0.989843896581211,0.989843896581211),(0.987492606357657,0.987202831733786,
0.989843896581211,0.989843896581211,0.989843896581211)))
REPRESENTATION_ITEM('')
SURFACE()
);
#2268=(
BOUNDED_SURFACE()
B_SPLINE_SURFACE(1,2,((#132443,#132444,#132445),(#132446,#132447,#132448),
(#132449,#132450,#132451)),.UNSPECIFIED.,.F.,.F.,.F.)
B_SPLINE_SURFACE_WITH_KNOTS((2,1,2),(3,3),(-0.00289807040992695,0.,0.289807040992695),
(0.538999630513411,0.556316102183954),.UNSPECIFIED.)
GEOMETRIC_REPRESENTATION_ITEM()
RATIONAL_B_SPLINE_SURFACE(((0.987570037304351,0.988129172627919,0.99163541140107),
(0.987570037304351,0.988129172627919,0.99163541140107),(0.987570037304351,
0.988129172627919,0.99163541140107)))
REPRESENTATION_ITEM('')
SURFACE()
);
#2269=(
BOUNDED_SURFACE()
B_SPLINE_SURFACE(1,2,((#132453,#132454,#132455,#132456,#132457),(#132458,
#132459,#132460,#132461,#132462)),.UNSPECIFIED.,.F.,.F.,.F.)
B_SPLINE_SURFACE_WITH_KNOTS((2,2),(3,2,3),(0.,0.290279631770573),(0.176864064841897,
0.194132688793568,0.194731236528949),.UNSPECIFIED.)
GEOMETRIC_REPRESENTATION_ITEM()
RATIONAL_B_SPLINE_SURFACE(((0.987492606357657,0.987202831733786,0.989843896581211,
0.989843896581211,0.989843896581211),(0.987492606357657,0.987202831733786,
0.989843896581211,0.989843896581211,0.989843896581211)))
REPRESENTATION_ITEM('')
SURFACE()
);
#2270=(
BOUNDED_SURFACE()
B_SPLINE_SURFACE(1,2,((#132471,#132472,#132473),(#132474,#132475,#132476),
(#132477,#132478,#132479)),.UNSPECIFIED.,.F.,.F.,.F.)
B_SPLINE_SURFACE_WITH_KNOTS((2,1,2),(3,3),(-0.00289807040993738,0.,0.289807040993738),
(0.538999630513411,0.556316102183954),.UNSPECIFIED.)
GEOMETRIC_REPRESENTATION_ITEM()
RATIONAL_B_SPLINE_SURFACE(((0.987570037304351,0.988129172627919,0.99163541140107),
(0.987570037304351,0.988129172627919,0.99163541140107),(0.987570037304351,
0.988129172627919,0.99163541140107)))
REPRESENTATION_ITEM('')
SURFACE()
);
#2271=(
BOUNDED_SURFACE()
B_SPLINE_SURFACE(1,2,((#132481,#132482,#132483,#132484,#132485),(#132486,
#132487,#132488,#132489,#132490)),.UNSPECIFIED.,.F.,.F.,.F.)
B_SPLINE_SURFACE_WITH_KNOTS((2,2),(3,2,3),(0.,0.290279631757276),(0.176864064841897,
0.194132688793568,0.194731236515657),.UNSPECIFIED.)
GEOMETRIC_REPRESENTATION_ITEM()
RATIONAL_B_SPLINE_SURFACE(((0.987492606357657,0.987202831733786,0.98984389658121,
0.98984389658121,0.98984389658121),(0.987492606357657,0.987202831733786,
0.98984389658121,0.98984389658121,0.98984389658121)))
REPRESENTATION_ITEM('')
SURFACE()
);
#2272=(
BOUNDED_SURFACE()
B_SPLINE_SURFACE(1,2,((#132499,#132500,#132501),(#132502,#132503,#132504),
(#132505,#132506,#132507)),.UNSPECIFIED.,.F.,.F.,.F.)
B_SPLINE_SURFACE_WITH_KNOTS((2,1,2),(3,3),(-0.00289807040991906,0.,0.289807040991906),
(0.538999630513411,0.556316102183956),.UNSPECIFIED.)
GEOMETRIC_REPRESENTATION_ITEM()
RATIONAL_B_SPLINE_SURFACE(((0.987570037304351,0.988129172627919,0.99163541140107),
(0.987570037304351,0.988129172627919,0.99163541140107),(0.987570037304351,
0.988129172627919,0.99163541140107)))
REPRESENTATION_ITEM('')
SURFACE()
);
#2273=(
BOUNDED_SURFACE()
B_SPLINE_SURFACE(1,2,((#132509,#132510,#132511,#132512,#132513),(#132514,
#132515,#132516,#132517,#132518)),.UNSPECIFIED.,.F.,.F.,.F.)
B_SPLINE_SURFACE_WITH_KNOTS((2,2),(3,2,3),(0.,0.290279631753777),(0.176864064841897,
0.194132688793568,0.194731236512156),.UNSPECIFIED.)
GEOMETRIC_REPRESENTATION_ITEM()
RATIONAL_B_SPLINE_SURFACE(((0.987492606357657,0.987202831733786,0.989843896581211,
0.989843896581211,0.989843896581211),(0.987492606357657,0.987202831733786,
0.989843896581211,0.989843896581211,0.989843896581211)))
REPRESENTATION_ITEM('')
SURFACE()
);
#2274=(
BOUNDED_SURFACE()
B_SPLINE_SURFACE(1,2,((#132527,#132528,#132529),(#132530,#132531,#132532),
(#132533,#132534,#132535)),.UNSPECIFIED.,.F.,.F.,.F.)
B_SPLINE_SURFACE_WITH_KNOTS((2,1,2),(3,3),(-0.00289807040993058,0.,0.289807040993058),
(0.538999630513411,0.556316102183954),.UNSPECIFIED.)
GEOMETRIC_REPRESENTATION_ITEM()
RATIONAL_B_SPLINE_SURFACE(((0.987570037304351,0.988129172627919,0.99163541140107),
(0.987570037304351,0.988129172627919,0.99163541140107),(0.987570037304351,
0.988129172627919,0.99163541140107)))
REPRESENTATION_ITEM('')
SURFACE()
);
#2275=(
BOUNDED_SURFACE()
B_SPLINE_SURFACE(1,2,((#132537,#132538,#132539,#132540,#132541),(#132542,
#132543,#132544,#132545,#132546)),.UNSPECIFIED.,.F.,.F.,.F.)
B_SPLINE_SURFACE_WITH_KNOTS((2,2),(3,2,3),(0.,0.290279631751751),(0.176864064841897,
0.194132688793568,0.194731236510121),.UNSPECIFIED.)
GEOMETRIC_REPRESENTATION_ITEM()
RATIONAL_B_SPLINE_SURFACE(((0.987492606357657,0.987202831733785,0.98984389658121,
0.98984389658121,0.98984389658121),(0.987492606357657,0.987202831733785,
0.98984389658121,0.98984389658121,0.98984389658121)))
REPRESENTATION_ITEM('')
SURFACE()
);
#2276=(
BOUNDED_SURFACE()
B_SPLINE_SURFACE(1,2,((#132555,#132556,#132557),(#132558,#132559,#132560),
(#132561,#132562,#132563)),.UNSPECIFIED.,.F.,.F.,.F.)
B_SPLINE_SURFACE_WITH_KNOTS((2,1,2),(3,3),(-0.00289807040992803,0.,0.289807040992803),
(0.538999630513411,0.556316102183955),.UNSPECIFIED.)
GEOMETRIC_REPRESENTATION_ITEM()
RATIONAL_B_SPLINE_SURFACE(((0.987570037304351,0.988129172627919,0.99163541140107),
(0.987570037304351,0.988129172627919,0.99163541140107),(0.987570037304351,
0.988129172627919,0.99163541140107)))
REPRESENTATION_ITEM('')
SURFACE()
);
#2277=(
BOUNDED_SURFACE()
B_SPLINE_SURFACE(1,2,((#132565,#132566,#132567,#132568,#132569),(#132570,
#132571,#132572,#132573,#132574)),.UNSPECIFIED.,.F.,.F.,.F.)
B_SPLINE_SURFACE_WITH_KNOTS((2,2),(3,2,3),(0.,0.290279631762918),(0.176864064841898,
0.194132688793568,0.194731236521282),.UNSPECIFIED.)
GEOMETRIC_REPRESENTATION_ITEM()
RATIONAL_B_SPLINE_SURFACE(((0.987492606357657,0.987202831733786,0.98984389658121,
0.98984389658121,0.98984389658121),(0.987492606357657,0.987202831733786,
0.98984389658121,0.98984389658121,0.98984389658121)))
REPRESENTATION_ITEM('')
SURFACE()
);
#2278=(
BOUNDED_SURFACE()
B_SPLINE_SURFACE(1,2,((#132583,#132584,#132585),(#132586,#132587,#132588),
(#132589,#132590,#132591)),.UNSPECIFIED.,.F.,.F.,.F.)
B_SPLINE_SURFACE_WITH_KNOTS((2,1,2),(3,3),(-0.0028980704099156,0.,0.28980704099156),
(0.53899963051341,0.556316102183953),.UNSPECIFIED.)
GEOMETRIC_REPRESENTATION_ITEM()
RATIONAL_B_SPLINE_SURFACE(((0.987570037304351,0.988129172627919,0.99163541140107),
(0.987570037304351,0.988129172627919,0.99163541140107),(0.987570037304351,
0.988129172627919,0.99163541140107)))
REPRESENTATION_ITEM('')
SURFACE()
);
#2279=(
BOUNDED_SURFACE()
B_SPLINE_SURFACE(1,2,((#132593,#132594,#132595,#132596,#132597),(#132598,
#132599,#132600,#132601,#132602)),.UNSPECIFIED.,.F.,.F.,.F.)
B_SPLINE_SURFACE_WITH_KNOTS((2,2),(3,2,3),(0.,0.290279631766922),(0.176864064841898,
0.194132688793569,0.194731236525302),.UNSPECIFIED.)
GEOMETRIC_REPRESENTATION_ITEM()
RATIONAL_B_SPLINE_SURFACE(((0.987492606357657,0.987202831733786,0.989843896581211,
0.989843896581211,0.989843896581211),(0.987492606357657,0.987202831733786,
0.989843896581211,0.989843896581211,0.989843896581211)))
REPRESENTATION_ITEM('')
SURFACE()
);
#2280=(
BOUNDED_SURFACE()
B_SPLINE_SURFACE(1,2,((#132611,#132612,#132613),(#132614,#132615,#132616),
(#132617,#132618,#132619)),.UNSPECIFIED.,.F.,.F.,.F.)
B_SPLINE_SURFACE_WITH_KNOTS((2,1,2),(3,3),(-0.00289807040991558,0.,0.289807040991558),
(0.53899963051341,0.556316102183954),.UNSPECIFIED.)
GEOMETRIC_REPRESENTATION_ITEM()
RATIONAL_B_SPLINE_SURFACE(((0.987570037304351,0.988129172627919,0.99163541140107),
(0.987570037304351,0.988129172627919,0.99163541140107),(0.987570037304351,
0.988129172627919,0.99163541140107)))
REPRESENTATION_ITEM('')
SURFACE()
);
#2281=(
BOUNDED_SURFACE()
B_SPLINE_SURFACE(1,2,((#132621,#132622,#132623,#132624,#132625),(#132626,
#132627,#132628,#132629,#132630),(#132631,#132632,#132633,#132634,#132635)),
 .UNSPECIFIED.,.F.,.F.,.F.)
B_SPLINE_SURFACE_WITH_KNOTS((2,1,2),(3,2,3),(-0.00289681084359915,0.,0.290279631760325),
(0.176864064841898,0.194132688793569,0.194731236518711),.UNSPECIFIED.)
GEOMETRIC_REPRESENTATION_ITEM()
RATIONAL_B_SPLINE_SURFACE(((0.987492606357657,0.987202831733786,0.989843896581211,
0.989843896581211,0.989843896581211),(0.987492606357657,0.987202831733786,
0.989843896581211,0.989843896581211,0.989843896581211),(0.987492606357657,
0.987202831733786,0.989843896581211,0.989843896581211,0.989843896581211)))
REPRESENTATION_ITEM('')
SURFACE()
);
#2282=(
BOUNDED_SURFACE()
B_SPLINE_SURFACE(1,2,((#132637,#132638,#132639),(#132640,#132641,#132642)),
 .UNSPECIFIED.,.F.,.F.,.F.)
B_SPLINE_SURFACE_WITH_KNOTS((2,2),(3,3),(0.,0.289807040991619),(0.22888337489439,
0.246056477139967),.UNSPECIFIED.)
GEOMETRIC_REPRESENTATION_ITEM()
RATIONAL_B_SPLINE_SURFACE(((0.991846493044863,0.988282393439513,0.987616798999169),
(0.991846493044863,0.988282393439513,0.987616798999169)))
REPRESENTATION_ITEM('')
SURFACE()
);
#2283=(
BOUNDED_SURFACE()
B_SPLINE_SURFACE(1,2,((#132665,#132666,#132667,#132668,#132669),(#132670,
#132671,#132672,#132673,#132674)),.UNSPECIFIED.,.F.,.F.,.F.)
B_SPLINE_SURFACE_WITH_KNOTS((2,2),(3,2,3),(0.,0.289681084359922),(0.487155140750431,
0.5,0.504719756176227),.UNSPECIFIED.)
GEOMETRIC_REPRESENTATION_ITEM()
RATIONAL_B_SPLINE_SURFACE(((0.992604240083356,0.995491335852357,1.,0.998343322021369,
0.996905579294145),(0.992604240083356,0.995491335852357,1.,0.998343322021369,
0.996905579294145)))
REPRESENTATION_ITEM('')
SURFACE()
);
#2284=(
BOUNDED_SURFACE()
B_SPLINE_SURFACE(1,2,((#132676,#132677,#132678),(#132679,#132680,#132681)),
 .UNSPECIFIED.,.F.,.F.,.F.)
B_SPLINE_SURFACE_WITH_KNOTS((2,2),(3,3),(0.,0.289807040991568),(0.228883374894701,
0.246056477139965),.UNSPECIFIED.)
GEOMETRIC_REPRESENTATION_ITEM()
RATIONAL_B_SPLINE_SURFACE(((0.991846493044734,0.988282393439502,0.987616798999169),
(0.991846493044734,0.988282393439502,0.987616798999169)))
REPRESENTATION_ITEM('')
SURFACE()
);
#2285=(
BOUNDED_SURFACE()
B_SPLINE_SURFACE(1,2,((#132704,#132705,#132706,#132707,#132708),(#132709,
#132710,#132711,#132712,#132713)),.UNSPECIFIED.,.F.,.F.,.F.)
B_SPLINE_SURFACE_WITH_KNOTS((2,2),(3,2,3),(0.,0.289681084359935),(0.487155140750431,
0.5,0.504719756176228),.UNSPECIFIED.)
GEOMETRIC_REPRESENTATION_ITEM()
RATIONAL_B_SPLINE_SURFACE(((0.992604240083356,0.995491335852357,1.,0.998343322021369,
0.996905579294145),(0.992604240083356,0.995491335852357,1.,0.998343322021369,
0.996905579294145)))
REPRESENTATION_ITEM('')
SURFACE()
);
#2286=(
BOUNDED_SURFACE()
B_SPLINE_SURFACE(1,2,((#132715,#132716,#132717),(#132718,#132719,#132720)),
 .UNSPECIFIED.,.F.,.F.,.F.)
B_SPLINE_SURFACE_WITH_KNOTS((2,2),(3,3),(0.,0.289807040991561),(0.228883374894809,
0.246056477139964),.UNSPECIFIED.)
GEOMETRIC_REPRESENTATION_ITEM()
RATIONAL_B_SPLINE_SURFACE(((0.991846493044689,0.988282393439498,0.987616798999169),
(0.991846493044689,0.988282393439498,0.987616798999169)))
REPRESENTATION_ITEM('')
SURFACE()
);
#2287=(
BOUNDED_SURFACE()
B_SPLINE_SURFACE(1,2,((#132743,#132744,#132745,#132746,#132747),(#132748,
#132749,#132750,#132751,#132752)),.UNSPECIFIED.,.F.,.F.,.F.)
B_SPLINE_SURFACE_WITH_KNOTS((2,2),(3,2,3),(0.,0.289681084360113),(0.48715514075043,
0.5,0.504719756176228),.UNSPECIFIED.)
GEOMETRIC_REPRESENTATION_ITEM()
RATIONAL_B_SPLINE_SURFACE(((0.992604240083356,0.995491335852357,1.,0.998343322021369,
0.996905579294145),(0.992604240083356,0.995491335852357,1.,0.998343322021369,
0.996905579294145)))
REPRESENTATION_ITEM('')
SURFACE()
);
#2288=(
BOUNDED_SURFACE()
B_SPLINE_SURFACE(1,2,((#132754,#132755,#132756),(#132757,#132758,#132759)),
 .UNSPECIFIED.,.F.,.F.,.F.)
B_SPLINE_SURFACE_WITH_KNOTS((2,2),(3,3),(0.,0.289807040991569),(0.228883374894809,
0.246056477139964),.UNSPECIFIED.)
GEOMETRIC_REPRESENTATION_ITEM()
RATIONAL_B_SPLINE_SURFACE(((0.991846493044689,0.988282393439498,0.987616798999169),
(0.991846493044689,0.988282393439498,0.987616798999169)))
REPRESENTATION_ITEM('')
SURFACE()
);
#2289=(
BOUNDED_SURFACE()
B_SPLINE_SURFACE(1,2,((#132782,#132783,#132784,#132785,#132786),(#132787,
#132788,#132789,#132790,#132791)),.UNSPECIFIED.,.F.,.F.,.F.)
B_SPLINE_SURFACE_WITH_KNOTS((2,2),(3,2,3),(0.,0.289681084359931),(0.48715514075043,
0.5,0.504719756176228),.UNSPECIFIED.)
GEOMETRIC_REPRESENTATION_ITEM()
RATIONAL_B_SPLINE_SURFACE(((0.992604240083356,0.995491335852357,1.,0.998343322021369,
0.996905579294145),(0.992604240083356,0.995491335852357,1.,0.998343322021369,
0.996905579294145)))
REPRESENTATION_ITEM('')
SURFACE()
);
#2290=(
BOUNDED_SURFACE()
B_SPLINE_SURFACE(1,2,((#132793,#132794,#132795),(#132796,#132797,#132798)),
 .UNSPECIFIED.,.F.,.F.,.F.)
B_SPLINE_SURFACE_WITH_KNOTS((2,2),(3,3),(0.,0.289807040991559),(0.228883374894304,
0.246056477139967),.UNSPECIFIED.)
GEOMETRIC_REPRESENTATION_ITEM()
RATIONAL_B_SPLINE_SURFACE(((0.991846493044899,0.988282393439517,0.987616798999169),
(0.991846493044899,0.988282393439516,0.987616798999169)))
REPRESENTATION_ITEM('')
SURFACE()
);
#2291=(
BOUNDED_SURFACE()
B_SPLINE_SURFACE(1,2,((#132821,#132822,#132823,#132824,#132825),(#132826,
#132827,#132828,#132829,#132830)),.UNSPECIFIED.,.F.,.F.,.F.)
B_SPLINE_SURFACE_WITH_KNOTS((2,2),(3,2,3),(0.,0.289681084360006),(0.487155140750431,
0.5,0.504719756176228),.UNSPECIFIED.)
GEOMETRIC_REPRESENTATION_ITEM()
RATIONAL_B_SPLINE_SURFACE(((0.992604240083356,0.995491335852357,1.,0.998343322021369,
0.996905579294145),(0.992604240083356,0.995491335852357,1.,0.998343322021369,
0.996905579294145)))
REPRESENTATION_ITEM('')
SURFACE()
);
#2292=(
BOUNDED_SURFACE()
B_SPLINE_SURFACE(1,2,((#132832,#132833,#132834),(#132835,#132836,#132837)),
 .UNSPECIFIED.,.F.,.F.,.F.)
B_SPLINE_SURFACE_WITH_KNOTS((2,2),(3,3),(0.,0.289807040991556),(0.228883374894453,
0.246056477139966),.UNSPECIFIED.)
GEOMETRIC_REPRESENTATION_ITEM()
RATIONAL_B_SPLINE_SURFACE(((0.991846493044837,0.988282393439511,0.987616798999169),
(0.991846493044837,0.988282393439511,0.987616798999169)))
REPRESENTATION_ITEM('')
SURFACE()
);
#2293=(
BOUNDED_SURFACE()
B_SPLINE_SURFACE(1,2,((#132860,#132861,#132862,#132863,#132864),(#132865,
#132866,#132867,#132868,#132869)),.UNSPECIFIED.,.F.,.F.,.F.)
B_SPLINE_SURFACE_WITH_KNOTS((2,2),(3,2,3),(0.,0.289681084359969),(0.48715514075043,
0.5,0.504719756176227),.UNSPECIFIED.)
GEOMETRIC_REPRESENTATION_ITEM()
RATIONAL_B_SPLINE_SURFACE(((0.992604240083356,0.995491335852357,1.,0.99834332202137,
0.996905579294146),(0.992604240083356,0.995491335852357,1.,0.99834332202137,
0.996905579294146)))
REPRESENTATION_ITEM('')
SURFACE()
);
#2294=(
BOUNDED_SURFACE()
B_SPLINE_SURFACE(1,2,((#132871,#132872,#132873),(#132874,#132875,#132876)),
 .UNSPECIFIED.,.F.,.F.,.F.)
B_SPLINE_SURFACE_WITH_KNOTS((2,2),(3,3),(0.,0.289807040991562),(0.228883374894634,
0.246056477139965),.UNSPECIFIED.)
GEOMETRIC_REPRESENTATION_ITEM()
RATIONAL_B_SPLINE_SURFACE(((0.991846493044762,0.988282393439504,0.987616798999169),
(0.991846493044762,0.988282393439504,0.987616798999169)))
REPRESENTATION_ITEM('')
SURFACE()
);
#2295=(
BOUNDED_SURFACE()
B_SPLINE_SURFACE(1,2,((#132899,#132900,#132901,#132902,#132903),(#132904,
#132905,#132906,#132907,#132908)),.UNSPECIFIED.,.F.,.F.,.F.)
B_SPLINE_SURFACE_WITH_KNOTS((2,2),(3,2,3),(0.,0.289681084360211),(0.487155140750431,
0.5,0.504719756176228),.UNSPECIFIED.)
GEOMETRIC_REPRESENTATION_ITEM()
RATIONAL_B_SPLINE_SURFACE(((0.992604240083356,0.995491335852357,1.,0.998343322021369,
0.996905579294145),(0.992604240083356,0.995491335852358,1.,0.998343322021369,
0.996905579294145)))
REPRESENTATION_ITEM('')
SURFACE()
);
#2296=(
BOUNDED_SURFACE()
B_SPLINE_SURFACE(1,2,((#132910,#132911,#132912),(#132913,#132914,#132915)),
 .UNSPECIFIED.,.F.,.F.,.F.)
B_SPLINE_SURFACE_WITH_KNOTS((2,2),(3,3),(0.,0.289807040991558),(0.228883374894809,
0.246056477139964),.UNSPECIFIED.)
GEOMETRIC_REPRESENTATION_ITEM()
RATIONAL_B_SPLINE_SURFACE(((0.991846493044689,0.988282393439498,0.987616798999169),
(0.991846493044689,0.988282393439498,0.987616798999169)))
REPRESENTATION_ITEM('')
SURFACE()
);
#2297=(
BOUNDED_SURFACE()
B_SPLINE_SURFACE(1,2,((#132938,#132939,#132940,#132941,#132942),(#132943,
#132944,#132945,#132946,#132947)),.UNSPECIFIED.,.F.,.F.,.F.)
B_SPLINE_SURFACE_WITH_KNOTS((2,2),(3,2,3),(0.,0.289681084360285),(0.487155140750431,
0.5,0.504719756176228),.UNSPECIFIED.)
GEOMETRIC_REPRESENTATION_ITEM()
RATIONAL_B_SPLINE_SURFACE(((0.992604240083356,0.995491335852358,1.,0.998343322021369,
0.996905579294145),(0.992604240083356,0.995491335852357,1.,0.998343322021369,
0.996905579294145)))
REPRESENTATION_ITEM('')
SURFACE()
);
#2298=(
BOUNDED_SURFACE()
B_SPLINE_SURFACE(1,2,((#132949,#132950,#132951),(#132952,#132953,#132954)),
 .UNSPECIFIED.,.F.,.F.,.F.)
B_SPLINE_SURFACE_WITH_KNOTS((2,2),(3,3),(0.,0.289807040991562),(0.228883374894809,
0.246056477139964),.UNSPECIFIED.)
GEOMETRIC_REPRESENTATION_ITEM()
RATIONAL_B_SPLINE_SURFACE(((0.991846493044689,0.988282393439498,0.987616798999169),
(0.991846493044689,0.988282393439498,0.987616798999169)))
REPRESENTATION_ITEM('')
SURFACE()
);
#2299=(
BOUNDED_SURFACE()
B_SPLINE_SURFACE(1,2,((#132975,#132976,#132977,#132978,#132979),(#132980,
#132981,#132982,#132983,#132984)),.UNSPECIFIED.,.F.,.F.,.F.)
B_SPLINE_SURFACE_WITH_KNOTS((2,2),(3,2,3),(0.,0.289681084359921),(0.487155140750431,
0.5,0.504719756176228),.UNSPECIFIED.)
GEOMETRIC_REPRESENTATION_ITEM()
RATIONAL_B_SPLINE_SURFACE(((0.992604240083356,0.995491335852357,1.,0.998343322021369,
0.996905579294145),(0.992604240083356,0.995491335852357,1.,0.998343322021369,
0.996905579294145)))
REPRESENTATION_ITEM('')
SURFACE()
);
#2300=(
BOUNDED_SURFACE()
B_SPLINE_SURFACE(1,2,((#132986,#132987,#132988),(#132989,#132990,#132991)),
 .UNSPECIFIED.,.F.,.F.,.F.)
B_SPLINE_SURFACE_WITH_KNOTS((2,2),(3,3),(0.,0.289807040991563),(0.228883374894809,
0.246056477139964),.UNSPECIFIED.)
GEOMETRIC_REPRESENTATION_ITEM()
RATIONAL_B_SPLINE_SURFACE(((0.991846493044689,0.988282393439498,0.987616798999169),
(0.991846493044689,0.988282393439498,0.987616798999169)))
REPRESENTATION_ITEM('')
SURFACE()
);
#2301=(
BOUNDED_SURFACE()
B_SPLINE_SURFACE(1,2,((#133014,#133015,#133016,#133017,#133018),(#133019,
#133020,#133021,#133022,#133023)),.UNSPECIFIED.,.F.,.F.,.F.)
B_SPLINE_SURFACE_WITH_KNOTS((2,2),(3,2,3),(0.,0.289681084359926),(0.487155140750431,
0.5,0.504719756176228),.UNSPECIFIED.)
GEOMETRIC_REPRESENTATION_ITEM()
RATIONAL_B_SPLINE_SURFACE(((0.992604240083356,0.995491335852357,1.,0.998343322021369,
0.996905579294145),(0.992604240083356,0.995491335852357,1.,0.998343322021369,
0.996905579294145)))
REPRESENTATION_ITEM('')
SURFACE()
);
#2302=(
BOUNDED_SURFACE()
B_SPLINE_SURFACE(1,2,((#133025,#133026,#133027),(#133028,#133029,#133030)),
 .UNSPECIFIED.,.F.,.F.,.F.)
B_SPLINE_SURFACE_WITH_KNOTS((2,2),(3,3),(0.,0.289807040991564),(0.228883374894809,
0.246056477139964),.UNSPECIFIED.)
GEOMETRIC_REPRESENTATION_ITEM()
RATIONAL_B_SPLINE_SURFACE(((0.991846493044689,0.988282393439498,0.987616798999169),
(0.991846493044689,0.988282393439498,0.987616798999169)))
REPRESENTATION_ITEM('')
SURFACE()
);
#2303=(
BOUNDED_SURFACE()
B_SPLINE_SURFACE(1,2,((#133053,#133054,#133055,#133056,#133057),(#133058,
#133059,#133060,#133061,#133062)),.UNSPECIFIED.,.F.,.F.,.F.)
B_SPLINE_SURFACE_WITH_KNOTS((2,2),(3,2,3),(0.,0.289681084359927),(0.487155140750431,
0.5,0.504719756176228),.UNSPECIFIED.)
GEOMETRIC_REPRESENTATION_ITEM()
RATIONAL_B_SPLINE_SURFACE(((0.992604240083356,0.995491335852357,1.,0.998343322021369,
0.996905579294145),(0.992604240083356,0.995491335852357,1.,0.998343322021369,
0.996905579294145)))
REPRESENTATION_ITEM('')
SURFACE()
);
#2304=(
BOUNDED_SURFACE()
B_SPLINE_SURFACE(1,2,((#133064,#133065,#133066),(#133067,#133068,#133069)),
 .UNSPECIFIED.,.F.,.F.,.F.)
B_SPLINE_SURFACE_WITH_KNOTS((2,2),(3,3),(0.,0.289807040991562),(0.228883374894809,
0.246056477139964),.UNSPECIFIED.)
GEOMETRIC_REPRESENTATION_ITEM()
RATIONAL_B_SPLINE_SURFACE(((0.991846493044689,0.988282393439498,0.987616798999169),
(0.991846493044689,0.988282393439498,0.987616798999169)))
REPRESENTATION_ITEM('')
SURFACE()
);
#2305=(
BOUNDED_SURFACE()
B_SPLINE_SURFACE(1,2,((#133092,#133093,#133094,#133095,#133096),(#133097,
#133098,#133099,#133100,#133101)),.UNSPECIFIED.,.F.,.F.,.F.)
B_SPLINE_SURFACE_WITH_KNOTS((2,2),(3,2,3),(0.,0.289681084359921),(0.487155140750431,
0.5,0.504719756176228),.UNSPECIFIED.)
GEOMETRIC_REPRESENTATION_ITEM()
RATIONAL_B_SPLINE_SURFACE(((0.992604240083356,0.995491335852357,1.,0.998343322021369,
0.996905579294145),(0.992604240083356,0.995491335852357,1.,0.998343322021369,
0.996905579294145)))
REPRESENTATION_ITEM('')
SURFACE()
);
#2306=(
BOUNDED_SURFACE()
B_SPLINE_SURFACE(1,2,((#133103,#133104,#133105),(#133106,#133107,#133108)),
 .UNSPECIFIED.,.F.,.F.,.F.)
B_SPLINE_SURFACE_WITH_KNOTS((2,2),(3,3),(0.,0.289807040991567),(0.228883374894809,
0.246056477139964),.UNSPECIFIED.)
GEOMETRIC_REPRESENTATION_ITEM()
RATIONAL_B_SPLINE_SURFACE(((0.991846493044689,0.988282393439498,0.987616798999169),
(0.991846493044689,0.988282393439498,0.987616798999169)))
REPRESENTATION_ITEM('')
SURFACE()
);
#2307=(
BOUNDED_SURFACE()
B_SPLINE_SURFACE(1,2,((#133131,#133132,#133133,#133134,#133135),(#133136,
#133137,#133138,#133139,#133140)),.UNSPECIFIED.,.F.,.F.,.F.)
B_SPLINE_SURFACE_WITH_KNOTS((2,2),(3,2,3),(0.,0.289681084359922),(0.487155140750431,
0.5,0.504719756176228),.UNSPECIFIED.)
GEOMETRIC_REPRESENTATION_ITEM()
RATIONAL_B_SPLINE_SURFACE(((0.992604240083356,0.995491335852357,1.,0.998343322021369,
0.996905579294145),(0.992604240083356,0.995491335852357,1.,0.998343322021369,
0.996905579294145)))
REPRESENTATION_ITEM('')
SURFACE()
);
#2308=(
BOUNDED_SURFACE()
B_SPLINE_SURFACE(1,2,((#133142,#133143,#133144),(#133145,#133146,#133147)),
 .UNSPECIFIED.,.F.,.F.,.F.)
B_SPLINE_SURFACE_WITH_KNOTS((2,2),(3,3),(0.,0.289807040991561),(0.228883374894809,
0.246056477139964),.UNSPECIFIED.)
GEOMETRIC_REPRESENTATION_ITEM()
RATIONAL_B_SPLINE_SURFACE(((0.991846493044689,0.988282393439498,0.987616798999169),
(0.991846493044689,0.988282393439498,0.987616798999169)))
REPRESENTATION_ITEM('')
SURFACE()
);
#2309=(
BOUNDED_SURFACE()
B_SPLINE_SURFACE(1,2,((#133170,#133171,#133172,#133173,#133174),(#133175,
#133176,#133177,#133178,#133179)),.UNSPECIFIED.,.F.,.F.,.F.)
B_SPLINE_SURFACE_WITH_KNOTS((2,2),(3,2,3),(0.,0.289681084359917),(0.487155140750431,
0.5,0.504719756176228),.UNSPECIFIED.)
GEOMETRIC_REPRESENTATION_ITEM()
RATIONAL_B_SPLINE_SURFACE(((0.992604240083356,0.995491335852357,1.,0.998343322021369,
0.996905579294145),(0.992604240083356,0.995491335852357,1.,0.998343322021369,
0.996905579294145)))
REPRESENTATION_ITEM('')
SURFACE()
);
#2310=(
BOUNDED_SURFACE()
B_SPLINE_SURFACE(1,2,((#133181,#133182,#133183),(#133184,#133185,#133186)),
 .UNSPECIFIED.,.F.,.F.,.F.)
B_SPLINE_SURFACE_WITH_KNOTS((2,2),(3,3),(0.,0.289807040991563),(0.228883374894809,
0.246056477139964),.UNSPECIFIED.)
GEOMETRIC_REPRESENTATION_ITEM()
RATIONAL_B_SPLINE_SURFACE(((0.991846493044689,0.988282393439498,0.987616798999169),
(0.991846493044689,0.988282393439497,0.987616798999169)))
REPRESENTATION_ITEM('')
SURFACE()
);
#2311=(
BOUNDED_SURFACE()
B_SPLINE_SURFACE(1,2,((#133194,#133195,#133196,#133197,#133198),(#133199,
#133200,#133201,#133202,#133203)),.UNSPECIFIED.,.F.,.F.,.F.)
B_SPLINE_SURFACE_WITH_KNOTS((2,2),(3,2,3),(0.,0.28968108435992),(0.487155140750431,
0.5,0.504719756176228),.UNSPECIFIED.)
GEOMETRIC_REPRESENTATION_ITEM()
RATIONAL_B_SPLINE_SURFACE(((0.992604240083356,0.995491335852357,1.,0.998343322021369,
0.996905579294145),(0.992604240083356,0.995491335852357,1.,0.998343322021369,
0.996905579294145)))
REPRESENTATION_ITEM('')
SURFACE()
);
#2312=(
BOUNDED_SURFACE()
B_SPLINE_SURFACE(1,2,((#133205,#133206,#133207),(#133208,#133209,#133210)),
 .UNSPECIFIED.,.F.,.F.,.F.)
B_SPLINE_SURFACE_WITH_KNOTS((2,2),(3,3),(0.,0.289807040991567),(0.228883374894809,
0.246056477139964),.UNSPECIFIED.)
GEOMETRIC_REPRESENTATION_ITEM()
RATIONAL_B_SPLINE_SURFACE(((0.991846493044689,0.988282393439498,0.987616798999169),
(0.991846493044689,0.988282393439498,0.987616798999169)))
REPRESENTATION_ITEM('')
SURFACE()
);
#2313=(
BOUNDED_SURFACE()
B_SPLINE_SURFACE(1,2,((#133233,#133234,#133235,#133236,#133237),(#133238,
#133239,#133240,#133241,#133242)),.UNSPECIFIED.,.F.,.F.,.F.)
B_SPLINE_SURFACE_WITH_KNOTS((2,2),(3,2,3),(0.,0.289681084359922),(0.487155140750431,
0.5,0.504719756176228),.UNSPECIFIED.)
GEOMETRIC_REPRESENTATION_ITEM()
RATIONAL_B_SPLINE_SURFACE(((0.992604240083356,0.995491335852357,1.,0.998343322021369,
0.996905579294145),(0.992604240083356,0.995491335852357,1.,0.998343322021369,
0.996905579294145)))
REPRESENTATION_ITEM('')
SURFACE()
);
#2314=(
BOUNDED_SURFACE()
B_SPLINE_SURFACE(1,2,((#133244,#133245,#133246),(#133247,#133248,#133249)),
 .UNSPECIFIED.,.F.,.F.,.F.)
B_SPLINE_SURFACE_WITH_KNOTS((2,2),(3,3),(0.,0.28980704099156),(0.228883374894809,
0.246056477139964),.UNSPECIFIED.)
GEOMETRIC_REPRESENTATION_ITEM()
RATIONAL_B_SPLINE_SURFACE(((0.991846493044689,0.988282393439498,0.987616798999169),
(0.991846493044689,0.988282393439498,0.987616798999169)))
REPRESENTATION_ITEM('')
SURFACE()
);
#2315=(
BOUNDED_SURFACE()
B_SPLINE_SURFACE(1,2,((#133272,#133273,#133274,#133275,#133276),(#133277,
#133278,#133279,#133280,#133281)),.UNSPECIFIED.,.F.,.F.,.F.)
B_SPLINE_SURFACE_WITH_KNOTS((2,2),(3,2,3),(0.,0.289681084359922),(0.487155140750431,
0.5,0.504719756176228),.UNSPECIFIED.)
GEOMETRIC_REPRESENTATION_ITEM()
RATIONAL_B_SPLINE_SURFACE(((0.992604240083356,0.995491335852357,1.,0.998343322021369,
0.996905579294145),(0.992604240083356,0.995491335852357,1.,0.998343322021369,
0.996905579294145)))
REPRESENTATION_ITEM('')
SURFACE()
);
#2316=(
BOUNDED_SURFACE()
B_SPLINE_SURFACE(1,2,((#133283,#133284,#133285),(#133286,#133287,#133288)),
 .UNSPECIFIED.,.F.,.F.,.F.)
B_SPLINE_SURFACE_WITH_KNOTS((2,2),(3,3),(0.,0.289807040991562),(0.228883374894809,
0.246056477139964),.UNSPECIFIED.)
GEOMETRIC_REPRESENTATION_ITEM()
RATIONAL_B_SPLINE_SURFACE(((0.991846493044689,0.988282393439498,0.987616798999169),
(0.991846493044689,0.988282393439498,0.987616798999169)))
REPRESENTATION_ITEM('')
SURFACE()
);
#2317=(
BOUNDED_SURFACE()
B_SPLINE_SURFACE(1,2,((#133311,#133312,#133313,#133314,#133315),(#133316,
#133317,#133318,#133319,#133320)),.UNSPECIFIED.,.F.,.F.,.F.)
B_SPLINE_SURFACE_WITH_KNOTS((2,2),(3,2,3),(0.,0.289681084359926),(0.487155140750431,
0.5,0.504719756176228),.UNSPECIFIED.)
GEOMETRIC_REPRESENTATION_ITEM()
RATIONAL_B_SPLINE_SURFACE(((0.992604240083356,0.995491335852357,1.,0.998343322021369,
0.996905579294145),(0.992604240083356,0.995491335852357,1.,0.998343322021369,
0.996905579294145)))
REPRESENTATION_ITEM('')
SURFACE()
);
#2318=(
BOUNDED_SURFACE()
B_SPLINE_SURFACE(1,2,((#133322,#133323,#133324),(#133325,#133326,#133327)),
 .UNSPECIFIED.,.F.,.F.,.F.)
B_SPLINE_SURFACE_WITH_KNOTS((2,2),(3,3),(0.,0.289807040991563),(0.228883374894809,
0.246056477139964),.UNSPECIFIED.)
GEOMETRIC_REPRESENTATION_ITEM()
RATIONAL_B_SPLINE_SURFACE(((0.991846493044689,0.988282393439498,0.987616798999169),
(0.991846493044689,0.988282393439498,0.987616798999169)))
REPRESENTATION_ITEM('')
SURFACE()
);
#2319=(
BOUNDED_SURFACE()
B_SPLINE_SURFACE(1,2,((#133350,#133351,#133352,#133353,#133354),(#133355,
#133356,#133357,#133358,#133359)),.UNSPECIFIED.,.F.,.F.,.F.)
B_SPLINE_SURFACE_WITH_KNOTS((2,2),(3,2,3),(0.,0.289681084359923),(0.487155140750431,
0.5,0.504719756176228),.UNSPECIFIED.)
GEOMETRIC_REPRESENTATION_ITEM()
RATIONAL_B_SPLINE_SURFACE(((0.992604240083356,0.995491335852357,1.,0.998343322021369,
0.996905579294145),(0.992604240083356,0.995491335852358,1.,0.998343322021369,
0.996905579294145)))
REPRESENTATION_ITEM('')
SURFACE()
);
#2320=(
BOUNDED_SURFACE()
B_SPLINE_SURFACE(1,2,((#133361,#133362,#133363),(#133364,#133365,#133366)),
 .UNSPECIFIED.,.F.,.F.,.F.)
B_SPLINE_SURFACE_WITH_KNOTS((2,2),(3,3),(0.,0.289807040991562),(0.228883374894809,
0.246056477139964),.UNSPECIFIED.)
GEOMETRIC_REPRESENTATION_ITEM()
RATIONAL_B_SPLINE_SURFACE(((0.991846493044689,0.988282393439498,0.987616798999169),
(0.991846493044689,0.988282393439498,0.987616798999169)))
REPRESENTATION_ITEM('')
SURFACE()
);
#2321=(
BOUNDED_SURFACE()
B_SPLINE_SURFACE(1,2,((#133389,#133390,#133391,#133392,#133393),(#133394,
#133395,#133396,#133397,#133398)),.UNSPECIFIED.,.F.,.F.,.F.)
B_SPLINE_SURFACE_WITH_KNOTS((2,2),(3,2,3),(0.,0.289681084359926),(0.487155140750431,
0.5,0.504719756176228),.UNSPECIFIED.)
GEOMETRIC_REPRESENTATION_ITEM()
RATIONAL_B_SPLINE_SURFACE(((0.992604240083356,0.995491335852358,1.,0.998343322021369,
0.996905579294145),(0.992604240083356,0.995491335852357,1.,0.998343322021369,
0.996905579294145)))
REPRESENTATION_ITEM('')
SURFACE()
);
#2322=(
BOUNDED_SURFACE()
B_SPLINE_SURFACE(1,2,((#133400,#133401,#133402),(#133403,#133404,#133405)),
 .UNSPECIFIED.,.F.,.F.,.F.)
B_SPLINE_SURFACE_WITH_KNOTS((2,2),(3,3),(0.,0.289807040991556),(0.228883374894809,
0.246056477139964),.UNSPECIFIED.)
GEOMETRIC_REPRESENTATION_ITEM()
RATIONAL_B_SPLINE_SURFACE(((0.991846493044689,0.988282393439498,0.987616798999169),
(0.991846493044689,0.988282393439498,0.987616798999169)))
REPRESENTATION_ITEM('')
SURFACE()
);
#2323=(
BOUNDED_SURFACE()
B_SPLINE_SURFACE(1,2,((#133416,#133417,#133418,#133419,#133420),(#133421,
#133422,#133423,#133424,#133425)),.UNSPECIFIED.,.F.,.F.,.F.)
B_SPLINE_SURFACE_WITH_KNOTS((2,2),(3,2,3),(0.,0.289681084360264),(0.487155140750431,
0.5,0.504719756176228),.UNSPECIFIED.)
GEOMETRIC_REPRESENTATION_ITEM()
RATIONAL_B_SPLINE_SURFACE(((0.992604240083356,0.995491335852357,1.,0.998343322021369,
0.996905579294145),(0.992604240083356,0.995491335852357,1.,0.998343322021369,
0.996905579294145)))
REPRESENTATION_ITEM('')
SURFACE()
);
#2324=(
BOUNDED_SURFACE()
B_SPLINE_SURFACE(1,2,((#133439,#133440,#133441),(#133442,#133443,#133444)),
 .UNSPECIFIED.,.F.,.F.,.F.)
B_SPLINE_SURFACE_WITH_KNOTS((2,2),(3,3),(0.,0.289807040991758),(0.228883374894809,
0.246056477139964),.UNSPECIFIED.)
GEOMETRIC_REPRESENTATION_ITEM()
RATIONAL_B_SPLINE_SURFACE(((0.991846493044689,0.988282393439498,0.987616798999169),
(0.991846493044689,0.988282393439498,0.987616798999169)))
REPRESENTATION_ITEM('')
SURFACE()
);
#2325=(
BOUNDED_SURFACE()
B_SPLINE_SURFACE(1,2,((#133467,#133468,#133469,#133470,#133471),(#133472,
#133473,#133474,#133475,#133476)),.UNSPECIFIED.,.F.,.F.,.F.)
B_SPLINE_SURFACE_WITH_KNOTS((2,2),(3,2,3),(0.,0.289681084360126),(0.487155140750322,
0.5,0.504719756194363),.UNSPECIFIED.)
GEOMETRIC_REPRESENTATION_ITEM()
RATIONAL_B_SPLINE_SURFACE(((0.992604240083307,0.995491335852319,1.,0.998343322015004,
0.996905579283096),(0.992604240083307,0.995491335852319,1.,0.998343322015004,
0.996905579283096)))
REPRESENTATION_ITEM('')
SURFACE()
);
#2326=(
BOUNDED_SURFACE()
B_SPLINE_SURFACE(1,2,((#133478,#133479,#133480),(#133481,#133482,#133483)),
 .UNSPECIFIED.,.F.,.F.,.F.)
B_SPLINE_SURFACE_WITH_KNOTS((2,2),(3,3),(0.,0.289807040992207),(0.22888337489481,
0.246056477139965),.UNSPECIFIED.)
GEOMETRIC_REPRESENTATION_ITEM()
RATIONAL_B_SPLINE_SURFACE(((0.991846493044689,0.988282393439497,0.987616798999169),
(0.991846493044689,0.988282393439497,0.987616798999169)))
REPRESENTATION_ITEM('')
SURFACE()
);
#2327=(
BOUNDED_SURFACE()
B_SPLINE_SURFACE(1,2,((#133506,#133507,#133508,#133509,#133510),(#133511,
#133512,#133513,#133514,#133515)),.UNSPECIFIED.,.F.,.F.,.F.)
B_SPLINE_SURFACE_WITH_KNOTS((2,2),(3,2,3),(0.,0.289681084359926),(0.48715514075043,
0.5,0.504719756176227),.UNSPECIFIED.)
GEOMETRIC_REPRESENTATION_ITEM()
RATIONAL_B_SPLINE_SURFACE(((0.992604240083356,0.995491335852357,1.,0.99834332202137,
0.996905579294146),(0.992604240083356,0.995491335852357,1.,0.99834332202137,
0.996905579294146)))
REPRESENTATION_ITEM('')
SURFACE()
);
#2328=(
BOUNDED_SURFACE()
B_SPLINE_SURFACE(1,2,((#133517,#133518,#133519),(#133520,#133521,#133522)),
 .UNSPECIFIED.,.F.,.F.,.F.)
B_SPLINE_SURFACE_WITH_KNOTS((2,2),(3,3),(0.,0.289807040991645),(0.22888337489481,
0.246056477139965),.UNSPECIFIED.)
GEOMETRIC_REPRESENTATION_ITEM()
RATIONAL_B_SPLINE_SURFACE(((0.991846493044689,0.988282393439497,0.987616798999169),
(0.991846493044689,0.988282393439497,0.987616798999169)))
REPRESENTATION_ITEM('')
SURFACE()
);
#2329=(
BOUNDED_SURFACE()
B_SPLINE_SURFACE(1,2,((#133545,#133546,#133547,#133548,#133549),(#133550,
#133551,#133552,#133553,#133554)),.UNSPECIFIED.,.F.,.F.,.F.)
B_SPLINE_SURFACE_WITH_KNOTS((2,2),(3,2,3),(0.,0.289681084359923),(0.487155140750429,
0.5,0.504719756176227),.UNSPECIFIED.)
GEOMETRIC_REPRESENTATION_ITEM()
RATIONAL_B_SPLINE_SURFACE(((0.992604240083356,0.995491335852357,1.,0.99834332202137,
0.996905579294146),(0.992604240083356,0.995491335852357,1.,0.99834332202137,
0.996905579294146)))
REPRESENTATION_ITEM('')
SURFACE()
);
#2330=(
BOUNDED_SURFACE()
B_SPLINE_SURFACE(1,2,((#133556,#133557,#133558),(#133559,#133560,#133561)),
 .UNSPECIFIED.,.F.,.F.,.F.)
B_SPLINE_SURFACE_WITH_KNOTS((2,2),(3,3),(0.,0.289807040991643),(0.22888337489481,
0.246056477139965),.UNSPECIFIED.)
GEOMETRIC_REPRESENTATION_ITEM()
RATIONAL_B_SPLINE_SURFACE(((0.991846493044689,0.988282393439497,0.987616798999169),
(0.991846493044689,0.988282393439497,0.987616798999169)))
REPRESENTATION_ITEM('')
SURFACE()
);
#2331=(
BOUNDED_SURFACE()
B_SPLINE_SURFACE(1,2,((#133584,#133585,#133586,#133587,#133588),(#133589,
#133590,#133591,#133592,#133593)),.UNSPECIFIED.,.F.,.F.,.F.)
B_SPLINE_SURFACE_WITH_KNOTS((2,2),(3,2,3),(0.,0.289681084359917),(0.487155140750429,
0.5,0.504719756176227),.UNSPECIFIED.)
GEOMETRIC_REPRESENTATION_ITEM()
RATIONAL_B_SPLINE_SURFACE(((0.992604240083356,0.995491335852357,1.,0.99834332202137,
0.996905579294146),(0.992604240083356,0.995491335852357,1.,0.99834332202137,
0.996905579294146)))
REPRESENTATION_ITEM('')
SURFACE()
);
#2332=(
BOUNDED_SURFACE()
B_SPLINE_SURFACE(1,2,((#133595,#133596,#133597),(#133598,#133599,#133600)),
 .UNSPECIFIED.,.F.,.F.,.F.)
B_SPLINE_SURFACE_WITH_KNOTS((2,2),(3,3),(0.,0.289807040991633),(0.22888337489481,
0.246056477139965),.UNSPECIFIED.)
GEOMETRIC_REPRESENTATION_ITEM()
RATIONAL_B_SPLINE_SURFACE(((0.991846493044689,0.988282393439497,0.987616798999169),
(0.991846493044689,0.988282393439497,0.987616798999169)))
REPRESENTATION_ITEM('')
SURFACE()
);
#2333=(
BOUNDED_SURFACE()
B_SPLINE_SURFACE(1,2,((#133623,#133624,#133625,#133626,#133627),(#133628,
#133629,#133630,#133631,#133632)),.UNSPECIFIED.,.F.,.F.,.F.)
B_SPLINE_SURFACE_WITH_KNOTS((2,2),(3,2,3),(0.,0.289681084359922),(0.487155140750429,
0.5,0.504719756176227),.UNSPECIFIED.)
GEOMETRIC_REPRESENTATION_ITEM()
RATIONAL_B_SPLINE_SURFACE(((0.992604240083356,0.995491335852357,1.,0.99834332202137,
0.996905579294146),(0.992604240083356,0.995491335852357,1.,0.99834332202137,
0.996905579294146)))
REPRESENTATION_ITEM('')
SURFACE()
);
#2334=(
BOUNDED_SURFACE()
B_SPLINE_SURFACE(1,2,((#133634,#133635,#133636),(#133637,#133638,#133639)),
 .UNSPECIFIED.,.F.,.F.,.F.)
B_SPLINE_SURFACE_WITH_KNOTS((2,2),(3,3),(0.,0.289807040992241),(0.228883374894738,
0.246056477139966),.UNSPECIFIED.)
GEOMETRIC_REPRESENTATION_ITEM()
RATIONAL_B_SPLINE_SURFACE(((0.991846493044719,0.9882823934395,0.987616798999169),
(0.991846493044719,0.9882823934395,0.987616798999169)))
REPRESENTATION_ITEM('')
SURFACE()
);
#2335=(
BOUNDED_SURFACE()
B_SPLINE_SURFACE(1,2,((#133662,#133663,#133664,#133665,#133666),(#133667,
#133668,#133669,#133670,#133671)),.UNSPECIFIED.,.F.,.F.,.F.)
B_SPLINE_SURFACE_WITH_KNOTS((2,2),(3,2,3),(0.,0.289681084360918),(0.48715514075043,
0.5,0.504719756176227),.UNSPECIFIED.)
GEOMETRIC_REPRESENTATION_ITEM()
RATIONAL_B_SPLINE_SURFACE(((0.992604240083356,0.995491335852357,1.,0.99834332202137,
0.996905579294146),(0.992604240083356,0.995491335852357,1.,0.99834332202137,
0.996905579294146)))
REPRESENTATION_ITEM('')
SURFACE()
);
#2336=(
BOUNDED_SURFACE()
B_SPLINE_SURFACE(1,2,((#133673,#133674,#133675),(#133676,#133677,#133678)),
 .UNSPECIFIED.,.F.,.F.,.F.)
B_SPLINE_SURFACE_WITH_KNOTS((2,2),(3,3),(0.,0.289807040991604),(0.228883374894582,
0.246056477139967),.UNSPECIFIED.)
GEOMETRIC_REPRESENTATION_ITEM()
RATIONAL_B_SPLINE_SURFACE(((0.991846493044783,0.988282393439506,0.987616798999169),
(0.991846493044784,0.988282393439506,0.987616798999169)))
REPRESENTATION_ITEM('')
SURFACE()
);
#2337=(
BOUNDED_SURFACE()
B_SPLINE_SURFACE(1,2,((#133701,#133702,#133703,#133704,#133705),(#133706,
#133707,#133708,#133709,#133710)),.UNSPECIFIED.,.F.,.F.,.F.)
B_SPLINE_SURFACE_WITH_KNOTS((2,2),(3,2,3),(0.,0.289681084359918),(0.487155140750429,
0.5,0.504719756176226),.UNSPECIFIED.)
GEOMETRIC_REPRESENTATION_ITEM()
RATIONAL_B_SPLINE_SURFACE(((0.992604240083356,0.995491335852357,1.,0.99834332202137,
0.996905579294146),(0.992604240083356,0.995491335852357,1.,0.99834332202137,
0.996905579294146)))
REPRESENTATION_ITEM('')
SURFACE()
);
#2338=(
BOUNDED_SURFACE()
B_SPLINE_SURFACE(1,2,((#133712,#133713,#133714),(#133715,#133716,#133717)),
 .UNSPECIFIED.,.F.,.F.,.F.)
B_SPLINE_SURFACE_WITH_KNOTS((2,2),(3,3),(0.,0.289807040991624),(0.22888337489437,
0.246056477139968),.UNSPECIFIED.)
GEOMETRIC_REPRESENTATION_ITEM()
RATIONAL_B_SPLINE_SURFACE(((0.991846493044871,0.988282393439514,0.987616798999169),
(0.991846493044871,0.988282393439514,0.987616798999169)))
REPRESENTATION_ITEM('')
SURFACE()
);
#2339=(
BOUNDED_SURFACE()
B_SPLINE_SURFACE(1,2,((#133740,#133741,#133742,#133743,#133744),(#133745,
#133746,#133747,#133748,#133749)),.UNSPECIFIED.,.F.,.F.,.F.)
B_SPLINE_SURFACE_WITH_KNOTS((2,2),(3,2,3),(0.,0.289681084359928),(0.487155140750429,
0.5,0.504719756176226),.UNSPECIFIED.)
GEOMETRIC_REPRESENTATION_ITEM()
RATIONAL_B_SPLINE_SURFACE(((0.992604240083356,0.995491335852357,1.,0.99834332202137,
0.996905579294146),(0.992604240083356,0.995491335852357,1.,0.99834332202137,
0.996905579294146)))
REPRESENTATION_ITEM('')
SURFACE()
);
#2340=(
BOUNDED_SURFACE()
B_SPLINE_SURFACE(1,2,((#133751,#133752,#133753),(#133754,#133755,#133756)),
 .UNSPECIFIED.,.F.,.F.,.F.)
B_SPLINE_SURFACE_WITH_KNOTS((2,2),(3,3),(0.71031891564008,1.),(0.538896351358318,
0.556212823028861),.UNSPECIFIED.)
GEOMETRIC_REPRESENTATION_ITEM()
RATIONAL_B_SPLINE_SURFACE(((0.987563472532048,0.988105030697865,0.991593692313265),
(0.987563472532048,0.988105030697865,0.991593692313265)))
REPRESENTATION_ITEM('')
SURFACE()
);
#2341=(
BOUNDED_SURFACE()
B_SPLINE_SURFACE(1,2,((#133767,#133768,#133769),(#133770,#133771,#133772)),
 .UNSPECIFIED.,.F.,.F.,.F.)
B_SPLINE_SURFACE_WITH_KNOTS((2,2),(3,3),(0.710192959008443,1.),(0.176967058622922,
0.194235682574593),.UNSPECIFIED.)
GEOMETRIC_REPRESENTATION_ITEM()
RATIONAL_B_SPLINE_SURFACE(((0.98748925405691,0.987216959588932,0.989875504592249),
(0.98748925405691,0.987216959588932,0.989875504592249)))
REPRESENTATION_ITEM('')
SURFACE()
);
#2342=(
BOUNDED_SURFACE()
B_SPLINE_SURFACE(1,2,((#133780,#133781,#133782),(#133783,#133784,#133785)),
 .UNSPECIFIED.,.F.,.F.,.F.)
B_SPLINE_SURFACE_WITH_KNOTS((2,2),(3,3),(0.71031891564008,1.),(0.538896351358318,
0.556212823028861),.UNSPECIFIED.)
GEOMETRIC_REPRESENTATION_ITEM()
RATIONAL_B_SPLINE_SURFACE(((0.987563472532048,0.988105030697865,0.991593692313265),
(0.987563472532048,0.988105030697865,0.991593692313265)))
REPRESENTATION_ITEM('')
SURFACE()
);
#2343=(
BOUNDED_SURFACE()
B_SPLINE_SURFACE(1,2,((#133796,#133797,#133798),(#133799,#133800,#133801)),
 .UNSPECIFIED.,.F.,.F.,.F.)
B_SPLINE_SURFACE_WITH_KNOTS((2,2),(3,3),(0.710192959008445,1.),(0.176967058622922,
0.194235682574593),.UNSPECIFIED.)
GEOMETRIC_REPRESENTATION_ITEM()
RATIONAL_B_SPLINE_SURFACE(((0.98748925405691,0.987216959588932,0.989875504592249),
(0.98748925405691,0.987216959588932,0.989875504592249)))
REPRESENTATION_ITEM('')
SURFACE()
);
#2344=(
BOUNDED_SURFACE()
B_SPLINE_SURFACE(1,2,((#133809,#133810,#133811),(#133812,#133813,#133814)),
 .UNSPECIFIED.,.F.,.F.,.F.)
B_SPLINE_SURFACE_WITH_KNOTS((2,2),(3,3),(0.710318915639147,1.),(0.538896351358318,
0.556212823028861),.UNSPECIFIED.)
GEOMETRIC_REPRESENTATION_ITEM()
RATIONAL_B_SPLINE_SURFACE(((0.987563472532048,0.988105030697866,0.991593692313265),
(0.987563472532048,0.988105030697865,0.991593692313265)))
REPRESENTATION_ITEM('')
SURFACE()
);
#2345=(
BOUNDED_SURFACE()
B_SPLINE_SURFACE(1,2,((#133825,#133826,#133827),(#133828,#133829,#133830)),
 .UNSPECIFIED.,.F.,.F.,.F.)
B_SPLINE_SURFACE_WITH_KNOTS((2,2),(3,3),(0.71019295900751,1.),(0.176967058622922,
0.194235682574593),.UNSPECIFIED.)
GEOMETRIC_REPRESENTATION_ITEM()
RATIONAL_B_SPLINE_SURFACE(((0.98748925405691,0.987216959588932,0.989875504592249),
(0.98748925405691,0.987216959588932,0.989875504592249)))
REPRESENTATION_ITEM('')
SURFACE()
);
#2346=(
BOUNDED_SURFACE()
B_SPLINE_SURFACE(1,2,((#133838,#133839,#133840),(#133841,#133842,#133843)),
 .UNSPECIFIED.,.F.,.F.,.F.)
B_SPLINE_SURFACE_WITH_KNOTS((2,2),(3,3),(0.710318915639151,1.),(0.538896351358318,
0.556212823028861),.UNSPECIFIED.)
GEOMETRIC_REPRESENTATION_ITEM()
RATIONAL_B_SPLINE_SURFACE(((0.987563472532048,0.988105030697865,0.991593692313265),
(0.987563472532048,0.988105030697865,0.991593692313265)))
REPRESENTATION_ITEM('')
SURFACE()
);
#2347=(
BOUNDED_SURFACE()
B_SPLINE_SURFACE(1,2,((#133854,#133855,#133856),(#133857,#133858,#133859)),
 .UNSPECIFIED.,.F.,.F.,.F.)
B_SPLINE_SURFACE_WITH_KNOTS((2,2),(3,3),(0.71019295900751,1.),(0.176967058622922,
0.194235682574593),.UNSPECIFIED.)
GEOMETRIC_REPRESENTATION_ITEM()
RATIONAL_B_SPLINE_SURFACE(((0.98748925405691,0.987216959588932,0.989875504592249),
(0.98748925405691,0.987216959588932,0.989875504592249)))
REPRESENTATION_ITEM('')
SURFACE()
);
#2348=(
BOUNDED_SURFACE()
B_SPLINE_SURFACE(1,2,((#133867,#133868,#133869),(#133870,#133871,#133872)),
 .UNSPECIFIED.,.F.,.F.,.F.)
B_SPLINE_SURFACE_WITH_KNOTS((2,2),(3,3),(0.710318915639144,1.),(0.538896351358318,
0.556212823028861),.UNSPECIFIED.)
GEOMETRIC_REPRESENTATION_ITEM()
RATIONAL_B_SPLINE_SURFACE(((0.987563472532048,0.988105030697865,0.991593692313265),
(0.987563472532048,0.988105030697865,0.991593692313265)))
REPRESENTATION_ITEM('')
SURFACE()
);
#2349=(
BOUNDED_SURFACE()
B_SPLINE_SURFACE(1,2,((#133883,#133884,#133885),(#133886,#133887,#133888)),
 .UNSPECIFIED.,.F.,.F.,.F.)
B_SPLINE_SURFACE_WITH_KNOTS((2,2),(3,3),(0.710192959007507,1.),(0.176967058622922,
0.194235682574593),.UNSPECIFIED.)
GEOMETRIC_REPRESENTATION_ITEM()
RATIONAL_B_SPLINE_SURFACE(((0.98748925405691,0.987216959588931,0.989875504592249),
(0.98748925405691,0.987216959588932,0.989875504592249)))
REPRESENTATION_ITEM('')
SURFACE()
);
#2350=(
BOUNDED_SURFACE()
B_SPLINE_SURFACE(1,2,((#133896,#133897,#133898),(#133899,#133900,#133901)),
 .UNSPECIFIED.,.F.,.F.,.F.)
B_SPLINE_SURFACE_WITH_KNOTS((2,2),(3,3),(0.710318915638568,1.),(0.538896351358318,
0.556212823028861),.UNSPECIFIED.)
GEOMETRIC_REPRESENTATION_ITEM()
RATIONAL_B_SPLINE_SURFACE(((0.987563472532048,0.988105030697866,0.991593692313265),
(0.987563472532048,0.988105030697865,0.991593692313265)))
REPRESENTATION_ITEM('')
SURFACE()
);
#2351=(
BOUNDED_SURFACE()
B_SPLINE_SURFACE(1,2,((#133912,#133913,#133914),(#133915,#133916,#133917)),
 .UNSPECIFIED.,.F.,.F.,.F.)
B_SPLINE_SURFACE_WITH_KNOTS((2,2),(3,3),(0.710192959006925,1.),(0.176967058622922,
0.194235682574593),.UNSPECIFIED.)
GEOMETRIC_REPRESENTATION_ITEM()
RATIONAL_B_SPLINE_SURFACE(((0.98748925405691,0.987216959588932,0.989875504592249),
(0.98748925405691,0.987216959588932,0.989875504592249)))
REPRESENTATION_ITEM('')
SURFACE()
);
#2352=(
BOUNDED_SURFACE()
B_SPLINE_SURFACE(1,2,((#133925,#133926,#133927),(#133928,#133929,#133930)),
 .UNSPECIFIED.,.F.,.F.,.F.)
B_SPLINE_SURFACE_WITH_KNOTS((2,2),(3,3),(0.710318915639155,1.),(0.538896351358318,
0.556212823028861),.UNSPECIFIED.)
GEOMETRIC_REPRESENTATION_ITEM()
RATIONAL_B_SPLINE_SURFACE(((0.987563472532048,0.988105030697865,0.991593692313265),
(0.987563472532048,0.988105030697865,0.991593692313265)))
REPRESENTATION_ITEM('')
SURFACE()
);
#2353=(
BOUNDED_SURFACE()
B_SPLINE_SURFACE(1,2,((#133941,#133942,#133943),(#133944,#133945,#133946)),
 .UNSPECIFIED.,.F.,.F.,.F.)
B_SPLINE_SURFACE_WITH_KNOTS((2,2),(3,3),(0.710192959007512,1.),(0.176967058622922,
0.194235682574593),.UNSPECIFIED.)
GEOMETRIC_REPRESENTATION_ITEM()
RATIONAL_B_SPLINE_SURFACE(((0.98748925405691,0.987216959588931,0.989875504592249),
(0.98748925405691,0.987216959588931,0.989875504592249)))
REPRESENTATION_ITEM('')
SURFACE()
);
#2354=(
BOUNDED_SURFACE()
B_SPLINE_SURFACE(1,2,((#133954,#133955,#133956),(#133957,#133958,#133959)),
 .UNSPECIFIED.,.F.,.F.,.F.)
B_SPLINE_SURFACE_WITH_KNOTS((2,2),(3,3),(0.710318915638571,1.),(0.538896351358318,
0.556212823028861),.UNSPECIFIED.)
GEOMETRIC_REPRESENTATION_ITEM()
RATIONAL_B_SPLINE_SURFACE(((0.987563472532048,0.988105030697865,0.991593692313265),
(0.987563472532048,0.988105030697865,0.991593692313265)))
REPRESENTATION_ITEM('')
SURFACE()
);
#2355=(
BOUNDED_SURFACE()
B_SPLINE_SURFACE(1,2,((#133970,#133971,#133972),(#133973,#133974,#133975)),
 .UNSPECIFIED.,.F.,.F.,.F.)
B_SPLINE_SURFACE_WITH_KNOTS((2,2),(3,3),(0.710192959006933,1.),(0.176967058622922,
0.194235682574593),.UNSPECIFIED.)
GEOMETRIC_REPRESENTATION_ITEM()
RATIONAL_B_SPLINE_SURFACE(((0.98748925405691,0.987216959588931,0.989875504592249),
(0.98748925405691,0.987216959588931,0.989875504592249)))
REPRESENTATION_ITEM('')
SURFACE()
);
#2356=(
BOUNDED_SURFACE()
B_SPLINE_SURFACE(1,2,((#133983,#133984,#133985),(#133986,#133987,#133988)),
 .UNSPECIFIED.,.F.,.F.,.F.)
B_SPLINE_SURFACE_WITH_KNOTS((2,2),(3,3),(0.71031891563907,1.),(0.538896351358319,
0.556212823028861),.UNSPECIFIED.)
GEOMETRIC_REPRESENTATION_ITEM()
RATIONAL_B_SPLINE_SURFACE(((0.987563472532048,0.988105030697866,0.991593692313265),
(0.987563472532048,0.988105030697866,0.991593692313265)))
REPRESENTATION_ITEM('')
SURFACE()
);
#2357=(
BOUNDED_SURFACE()
B_SPLINE_SURFACE(1,2,((#133999,#134000,#134001),(#134002,#134003,#134004)),
 .UNSPECIFIED.,.F.,.F.,.F.)
B_SPLINE_SURFACE_WITH_KNOTS((2,2),(3,3),(0.710192959007426,1.),(0.176967058622921,
0.194235682574592),.UNSPECIFIED.)
GEOMETRIC_REPRESENTATION_ITEM()
RATIONAL_B_SPLINE_SURFACE(((0.98748925405691,0.987216959588932,0.989875504592249),
(0.98748925405691,0.987216959588932,0.989875504592249)))
REPRESENTATION_ITEM('')
SURFACE()
);
#2358=(
BOUNDED_SURFACE()
B_SPLINE_SURFACE(1,2,((#134012,#134013,#134014),(#134015,#134016,#134017)),
 .UNSPECIFIED.,.F.,.F.,.F.)
B_SPLINE_SURFACE_WITH_KNOTS((2,2),(3,3),(0.710318915639068,1.),(0.538896351358319,
0.556212823028862),.UNSPECIFIED.)
GEOMETRIC_REPRESENTATION_ITEM()
RATIONAL_B_SPLINE_SURFACE(((0.987563472532048,0.988105030697866,0.991593692313266),
(0.987563472532048,0.988105030697866,0.991593692313266)))
REPRESENTATION_ITEM('')
SURFACE()
);
#2359=(
BOUNDED_SURFACE()
B_SPLINE_SURFACE(1,2,((#134028,#134029,#134030),(#134031,#134032,#134033)),
 .UNSPECIFIED.,.F.,.F.,.F.)
B_SPLINE_SURFACE_WITH_KNOTS((2,2),(3,3),(0.710192959007431,1.),(0.176967058622921,
0.194235682574592),.UNSPECIFIED.)
GEOMETRIC_REPRESENTATION_ITEM()
RATIONAL_B_SPLINE_SURFACE(((0.98748925405691,0.987216959588931,0.989875504592249),
(0.98748925405691,0.987216959588931,0.989875504592249)))
REPRESENTATION_ITEM('')
SURFACE()
);
#2360=(
BOUNDED_SURFACE()
B_SPLINE_SURFACE(1,2,((#134041,#134042,#134043),(#134044,#134045,#134046)),
 .UNSPECIFIED.,.F.,.F.,.F.)
B_SPLINE_SURFACE_WITH_KNOTS((2,2),(3,3),(0.710318915638475,1.),(0.538896351358319,
0.556212823028862),.UNSPECIFIED.)
GEOMETRIC_REPRESENTATION_ITEM()
RATIONAL_B_SPLINE_SURFACE(((0.987563472532048,0.988105030697866,0.991593692313266),
(0.987563472532048,0.988105030697866,0.991593692313266)))
REPRESENTATION_ITEM('')
SURFACE()
);
#2361=(
BOUNDED_SURFACE()
B_SPLINE_SURFACE(1,2,((#134057,#134058,#134059),(#134060,#134061,#134062)),
 .UNSPECIFIED.,.F.,.F.,.F.)
B_SPLINE_SURFACE_WITH_KNOTS((2,2),(3,3),(0.710192959006835,1.),(0.176967058622921,
0.194235682574592),.UNSPECIFIED.)
GEOMETRIC_REPRESENTATION_ITEM()
RATIONAL_B_SPLINE_SURFACE(((0.98748925405691,0.987216959588931,0.989875504592249),
(0.98748925405691,0.987216959588931,0.989875504592249)))
REPRESENTATION_ITEM('')
SURFACE()
);
#2362=(
BOUNDED_SURFACE()
B_SPLINE_SURFACE(1,2,((#134070,#134071,#134072),(#134073,#134074,#134075)),
 .UNSPECIFIED.,.F.,.F.,.F.)
B_SPLINE_SURFACE_WITH_KNOTS((2,2),(3,3),(0.710318915639071,1.),(0.538896351358319,
0.556212823028862),.UNSPECIFIED.)
GEOMETRIC_REPRESENTATION_ITEM()
RATIONAL_B_SPLINE_SURFACE(((0.987563472532048,0.988105030697866,0.991593692313266),
(0.987563472532048,0.988105030697866,0.991593692313266)))
REPRESENTATION_ITEM('')
SURFACE()
);
#2363=(
BOUNDED_SURFACE()
B_SPLINE_SURFACE(1,2,((#134086,#134087,#134088),(#134089,#134090,#134091)),
 .UNSPECIFIED.,.F.,.F.,.F.)
B_SPLINE_SURFACE_WITH_KNOTS((2,2),(3,3),(0.710192959007428,1.),(0.176967058622921,
0.194235682574592),.UNSPECIFIED.)
GEOMETRIC_REPRESENTATION_ITEM()
RATIONAL_B_SPLINE_SURFACE(((0.98748925405691,0.987216959588932,0.989875504592249),
(0.98748925405691,0.987216959588932,0.989875504592249)))
REPRESENTATION_ITEM('')
SURFACE()
);
#2364=(
BOUNDED_SURFACE()
B_SPLINE_SURFACE(1,2,((#134099,#134100,#134101),(#134102,#134103,#134104)),
 .UNSPECIFIED.,.F.,.F.,.F.)
B_SPLINE_SURFACE_WITH_KNOTS((2,2),(3,3),(0.71031891563857,1.),(0.538896351358319,
0.556212823028862),.UNSPECIFIED.)
GEOMETRIC_REPRESENTATION_ITEM()
RATIONAL_B_SPLINE_SURFACE(((0.987563472532048,0.988105030697866,0.991593692313266),
(0.987563472532048,0.988105030697866,0.991593692313266)))
REPRESENTATION_ITEM('')
SURFACE()
);
#2365=(
BOUNDED_SURFACE()
B_SPLINE_SURFACE(1,2,((#134115,#134116,#134117),(#134118,#134119,#134120)),
 .UNSPECIFIED.,.F.,.F.,.F.)
B_SPLINE_SURFACE_WITH_KNOTS((2,2),(3,3),(0.710192959006926,1.),(0.176967058622921,
0.194235682574592),.UNSPECIFIED.)
GEOMETRIC_REPRESENTATION_ITEM()
RATIONAL_B_SPLINE_SURFACE(((0.98748925405691,0.987216959588932,0.989875504592249),
(0.98748925405691,0.987216959588932,0.989875504592249)))
REPRESENTATION_ITEM('')
SURFACE()
);
#2366=(
BOUNDED_SURFACE()
B_SPLINE_SURFACE(1,2,((#134128,#134129,#134130),(#134131,#134132,#134133)),
 .UNSPECIFIED.,.F.,.F.,.F.)
B_SPLINE_SURFACE_WITH_KNOTS((2,2),(3,3),(0.710318915639063,1.),(0.538896351358319,
0.556212823028862),.UNSPECIFIED.)
GEOMETRIC_REPRESENTATION_ITEM()
RATIONAL_B_SPLINE_SURFACE(((0.987563472532048,0.988105030697866,0.991593692313266),
(0.987563472532048,0.988105030697866,0.991593692313266)))
REPRESENTATION_ITEM('')
SURFACE()
);
#2367=(
BOUNDED_SURFACE()
B_SPLINE_SURFACE(1,2,((#134144,#134145,#134146),(#134147,#134148,#134149)),
 .UNSPECIFIED.,.F.,.F.,.F.)
B_SPLINE_SURFACE_WITH_KNOTS((2,2),(3,3),(0.710192959007417,1.),(0.176967058622921,
0.194235682574592),.UNSPECIFIED.)
GEOMETRIC_REPRESENTATION_ITEM()
RATIONAL_B_SPLINE_SURFACE(((0.98748925405691,0.987216959588931,0.989875504592249),
(0.98748925405691,0.987216959588931,0.989875504592249)))
REPRESENTATION_ITEM('')
SURFACE()
);
#2368=(
BOUNDED_SURFACE()
B_SPLINE_SURFACE(1,2,((#134157,#134158,#134159),(#134160,#134161,#134162)),
 .UNSPECIFIED.,.F.,.F.,.F.)
B_SPLINE_SURFACE_WITH_KNOTS((2,2),(3,3),(0.710318915638562,1.),(0.538896351358319,
0.556212823028862),.UNSPECIFIED.)
GEOMETRIC_REPRESENTATION_ITEM()
RATIONAL_B_SPLINE_SURFACE(((0.987563472532048,0.988105030697866,0.991593692313266),
(0.987563472532048,0.988105030697866,0.991593692313266)))
REPRESENTATION_ITEM('')
SURFACE()
);
#2369=(
BOUNDED_SURFACE()
B_SPLINE_SURFACE(1,2,((#134173,#134174,#134175),(#134176,#134177,#134178)),
 .UNSPECIFIED.,.F.,.F.,.F.)
B_SPLINE_SURFACE_WITH_KNOTS((2,2),(3,3),(0.710192959006918,1.),(0.176967058622921,
0.194235682574592),.UNSPECIFIED.)
GEOMETRIC_REPRESENTATION_ITEM()
RATIONAL_B_SPLINE_SURFACE(((0.98748925405691,0.987216959588931,0.989875504592249),
(0.98748925405691,0.987216959588931,0.989875504592249)))
REPRESENTATION_ITEM('')
SURFACE()
);
#2370=(
BOUNDED_SURFACE()
B_SPLINE_SURFACE(1,2,((#134186,#134187,#134188),(#134189,#134190,#134191)),
 .UNSPECIFIED.,.F.,.F.,.F.)
B_SPLINE_SURFACE_WITH_KNOTS((2,2),(3,3),(0.71031891563879,1.),(0.538896351358319,
0.556212823028862),.UNSPECIFIED.)
GEOMETRIC_REPRESENTATION_ITEM()
RATIONAL_B_SPLINE_SURFACE(((0.987563472532048,0.988105030697866,0.991593692313266),
(0.987563472532048,0.988105030697866,0.991593692313266)))
REPRESENTATION_ITEM('')
SURFACE()
);
#2371=(
BOUNDED_SURFACE()
B_SPLINE_SURFACE(1,2,((#134202,#134203,#134204),(#134205,#134206,#134207)),
 .UNSPECIFIED.,.F.,.F.,.F.)
B_SPLINE_SURFACE_WITH_KNOTS((2,2),(3,3),(0.710192959007143,1.),(0.176967058622921,
0.194235682574592),.UNSPECIFIED.)
GEOMETRIC_REPRESENTATION_ITEM()
RATIONAL_B_SPLINE_SURFACE(((0.98748925405691,0.987216959588932,0.989875504592249),
(0.98748925405691,0.987216959588932,0.989875504592249)))
REPRESENTATION_ITEM('')
SURFACE()
);
#2372=(
BOUNDED_SURFACE()
B_SPLINE_SURFACE(1,2,((#134215,#134216,#134217),(#134218,#134219,#134220)),
 .UNSPECIFIED.,.F.,.F.,.F.)
B_SPLINE_SURFACE_WITH_KNOTS((2,2),(3,3),(0.71031891563774,1.),(0.538896351358319,
0.556212823028862),.UNSPECIFIED.)
GEOMETRIC_REPRESENTATION_ITEM()
RATIONAL_B_SPLINE_SURFACE(((0.987563472532048,0.988105030697866,0.991593692313266),
(0.987563472532048,0.988105030697866,0.991593692313266)))
REPRESENTATION_ITEM('')
SURFACE()
);
#2373=(
BOUNDED_SURFACE()
B_SPLINE_SURFACE(1,2,((#134231,#134232,#134233),(#134234,#134235,#134236)),
 .UNSPECIFIED.,.F.,.F.,.F.)
B_SPLINE_SURFACE_WITH_KNOTS((2,2),(3,3),(0.710192959006099,1.),(0.176967058622921,
0.194235682574592),.UNSPECIFIED.)
GEOMETRIC_REPRESENTATION_ITEM()
RATIONAL_B_SPLINE_SURFACE(((0.98748925405691,0.987216959588931,0.989875504592249),
(0.98748925405691,0.987216959588932,0.989875504592249)))
REPRESENTATION_ITEM('')
SURFACE()
);
#2374=(
BOUNDED_SURFACE()
B_SPLINE_SURFACE(1,2,((#134244,#134245,#134246),(#134247,#134248,#134249)),
 .UNSPECIFIED.,.F.,.F.,.F.)
B_SPLINE_SURFACE_WITH_KNOTS((2,2),(3,3),(0.710318915639028,1.),(0.538896351358319,
0.556212823028862),.UNSPECIFIED.)
GEOMETRIC_REPRESENTATION_ITEM()
RATIONAL_B_SPLINE_SURFACE(((0.987563472532048,0.988105030697866,0.991593692313266),
(0.987563472532048,0.988105030697866,0.991593692313266)))
REPRESENTATION_ITEM('')
SURFACE()
);
#2375=(
BOUNDED_SURFACE()
B_SPLINE_SURFACE(1,2,((#134260,#134261,#134262),(#134263,#134264,#134265)),
 .UNSPECIFIED.,.F.,.F.,.F.)
B_SPLINE_SURFACE_WITH_KNOTS((2,2),(3,3),(0.710192959007385,1.),(0.176967058622921,
0.194235682574592),.UNSPECIFIED.)
GEOMETRIC_REPRESENTATION_ITEM()
RATIONAL_B_SPLINE_SURFACE(((0.98748925405691,0.987216959588932,0.989875504592249),
(0.98748925405691,0.987216959588932,0.989875504592249)))
REPRESENTATION_ITEM('')
SURFACE()
);
#2376=(
BOUNDED_SURFACE()
B_SPLINE_SURFACE(1,2,((#134273,#134274,#134275),(#134276,#134277,#134278)),
 .UNSPECIFIED.,.F.,.F.,.F.)
B_SPLINE_SURFACE_WITH_KNOTS((2,2),(3,3),(0.710318915639144,1.),(0.538896351358319,
0.556212823028862),.UNSPECIFIED.)
GEOMETRIC_REPRESENTATION_ITEM()
RATIONAL_B_SPLINE_SURFACE(((0.987563472532048,0.988105030697866,0.991593692313266),
(0.987563472532048,0.988105030697866,0.991593692313266)))
REPRESENTATION_ITEM('')
SURFACE()
);
#2377=(
BOUNDED_SURFACE()
B_SPLINE_SURFACE(1,2,((#134289,#134290,#134291),(#134292,#134293,#134294)),
 .UNSPECIFIED.,.F.,.F.,.F.)
B_SPLINE_SURFACE_WITH_KNOTS((2,2),(3,3),(0.710192959007499,1.),(0.176967058622921,
0.194235682574596),.UNSPECIFIED.)
GEOMETRIC_REPRESENTATION_ITEM()
RATIONAL_B_SPLINE_SURFACE(((0.98748925405691,0.987216959588931,0.98987550459225),
(0.98748925405691,0.987216959588931,0.98987550459225)))
REPRESENTATION_ITEM('')
SURFACE()
);
#2378=(
BOUNDED_SURFACE()
B_SPLINE_SURFACE(1,2,((#134302,#134303,#134304),(#134305,#134306,#134307)),
 .UNSPECIFIED.,.F.,.F.,.F.)
B_SPLINE_SURFACE_WITH_KNOTS((2,2),(3,3),(0.710318915638508,1.),(0.538896351358319,
0.556212823028862),.UNSPECIFIED.)
GEOMETRIC_REPRESENTATION_ITEM()
RATIONAL_B_SPLINE_SURFACE(((0.987563472532048,0.988105030697866,0.991593692313266),
(0.987563472532048,0.988105030697866,0.991593692313266)))
REPRESENTATION_ITEM('')
SURFACE()
);
#2379=(
BOUNDED_SURFACE()
B_SPLINE_SURFACE(1,2,((#134318,#134319,#134320),(#134321,#134322,#134323)),
 .UNSPECIFIED.,.F.,.F.,.F.)
B_SPLINE_SURFACE_WITH_KNOTS((2,2),(3,3),(0.710192959006863,1.),(0.176967058622921,
0.194235682574592),.UNSPECIFIED.)
GEOMETRIC_REPRESENTATION_ITEM()
RATIONAL_B_SPLINE_SURFACE(((0.98748925405691,0.987216959588931,0.989875504592249),
(0.98748925405691,0.987216959588931,0.989875504592249)))
REPRESENTATION_ITEM('')
SURFACE()
);
#2380=(
BOUNDED_SURFACE()
B_SPLINE_SURFACE(1,2,((#134331,#134332,#134333),(#134334,#134335,#134336)),
 .UNSPECIFIED.,.F.,.F.,.F.)
B_SPLINE_SURFACE_WITH_KNOTS((2,2),(3,3),(0.71031891563991,1.),(0.538896351358319,
0.556212823028862),.UNSPECIFIED.)
GEOMETRIC_REPRESENTATION_ITEM()
RATIONAL_B_SPLINE_SURFACE(((0.987563472532048,0.988105030697866,0.991593692313266),
(0.987563472532048,0.988105030697866,0.991593692313266)))
REPRESENTATION_ITEM('')
SURFACE()
);
#2381=(
BOUNDED_SURFACE()
B_SPLINE_SURFACE(1,2,((#134347,#134348,#134349),(#134350,#134351,#134352)),
 .UNSPECIFIED.,.F.,.F.,.F.)
B_SPLINE_SURFACE_WITH_KNOTS((2,2),(3,3),(0.710192959008264,1.),(0.176967058622921,
0.194235682574593),.UNSPECIFIED.)
GEOMETRIC_REPRESENTATION_ITEM()
RATIONAL_B_SPLINE_SURFACE(((0.98748925405691,0.987216959588931,0.989875504592249),
(0.98748925405691,0.987216959588932,0.989875504592249)))
REPRESENTATION_ITEM('')
SURFACE()
);
#2382=(
BOUNDED_SURFACE()
B_SPLINE_SURFACE(1,2,((#134360,#134361,#134362),(#134363,#134364,#134365)),
 .UNSPECIFIED.,.F.,.F.,.F.)
B_SPLINE_SURFACE_WITH_KNOTS((2,2),(3,3),(0.710318915638761,1.),(0.538896351358319,
0.556212823028862),.UNSPECIFIED.)
GEOMETRIC_REPRESENTATION_ITEM()
RATIONAL_B_SPLINE_SURFACE(((0.987563472532048,0.988105030697866,0.991593692313266),
(0.987563472532048,0.988105030697866,0.991593692313266)))
REPRESENTATION_ITEM('')
SURFACE()
);
#2383=(
BOUNDED_SURFACE()
B_SPLINE_SURFACE(1,2,((#134376,#134377,#134378),(#134379,#134380,#134381)),
 .UNSPECIFIED.,.F.,.F.,.F.)
B_SPLINE_SURFACE_WITH_KNOTS((2,2),(3,3),(0.710192959007121,1.),(0.176967058622921,
0.194235682574592),.UNSPECIFIED.)
GEOMETRIC_REPRESENTATION_ITEM()
RATIONAL_B_SPLINE_SURFACE(((0.98748925405691,0.987216959588932,0.989875504592249),
(0.98748925405691,0.987216959588932,0.989875504592249)))
REPRESENTATION_ITEM('')
SURFACE()
);
#2384=(
BOUNDED_SURFACE()
B_SPLINE_SURFACE(1,2,((#134389,#134390,#134391),(#134392,#134393,#134394)),
 .UNSPECIFIED.,.F.,.F.,.F.)
B_SPLINE_SURFACE_WITH_KNOTS((2,2),(3,3),(0.710318915638945,1.),(0.538896351358319,
0.556212823028862),.UNSPECIFIED.)
GEOMETRIC_REPRESENTATION_ITEM()
RATIONAL_B_SPLINE_SURFACE(((0.987563472532048,0.988105030697866,0.991593692313266),
(0.987563472532048,0.988105030697866,0.991593692313266)))
REPRESENTATION_ITEM('')
SURFACE()
);
#2385=(
BOUNDED_SURFACE()
B_SPLINE_SURFACE(1,2,((#134405,#134406,#134407),(#134408,#134409,#134410)),
 .UNSPECIFIED.,.F.,.F.,.F.)
B_SPLINE_SURFACE_WITH_KNOTS((2,2),(3,3),(0.710192959007306,1.),(0.176967058622921,
0.194235682574592),.UNSPECIFIED.)
GEOMETRIC_REPRESENTATION_ITEM()
RATIONAL_B_SPLINE_SURFACE(((0.98748925405691,0.987216959588932,0.989875504592249),
(0.98748925405691,0.987216959588932,0.989875504592249)))
REPRESENTATION_ITEM('')
SURFACE()
);
#2386=(
BOUNDED_SURFACE()
B_SPLINE_SURFACE(1,2,((#134418,#134419,#134420),(#134421,#134422,#134423)),
 .UNSPECIFIED.,.F.,.F.,.F.)
B_SPLINE_SURFACE_WITH_KNOTS((2,2),(3,3),(0.710318915637902,1.),(0.538896351358319,
0.556212823028862),.UNSPECIFIED.)
GEOMETRIC_REPRESENTATION_ITEM()
RATIONAL_B_SPLINE_SURFACE(((0.987563472532048,0.988105030697866,0.991593692313266),
(0.987563472532048,0.988105030697866,0.991593692313266)))
REPRESENTATION_ITEM('')
SURFACE()
);
#2387=(
BOUNDED_SURFACE()
B_SPLINE_SURFACE(1,2,((#134434,#134435,#134436),(#134437,#134438,#134439)),
 .UNSPECIFIED.,.F.,.F.,.F.)
B_SPLINE_SURFACE_WITH_KNOTS((2,2),(3,3),(0.710192959006265,1.),(0.176967058622921,
0.194235682574592),.UNSPECIFIED.)
GEOMETRIC_REPRESENTATION_ITEM()
RATIONAL_B_SPLINE_SURFACE(((0.98748925405691,0.987216959588932,0.989875504592249),
(0.98748925405691,0.987216959588932,0.989875504592249)))
REPRESENTATION_ITEM('')
SURFACE()
);
#2388=(
BOUNDED_SURFACE()
B_SPLINE_SURFACE(1,2,((#134447,#134448,#134449),(#134450,#134451,#134452)),
 .UNSPECIFIED.,.F.,.F.,.F.)
B_SPLINE_SURFACE_WITH_KNOTS((2,2),(3,3),(0.710318915639735,1.),(0.538896351358319,
0.556212823028863),.UNSPECIFIED.)
GEOMETRIC_REPRESENTATION_ITEM()
RATIONAL_B_SPLINE_SURFACE(((0.987563472532048,0.988105030697866,0.991593692313266),
(0.987563472532048,0.988105030697866,0.991593692313266)))
REPRESENTATION_ITEM('')
SURFACE()
);
#2389=(
BOUNDED_SURFACE()
B_SPLINE_SURFACE(1,2,((#134463,#134464,#134465),(#134466,#134467,#134468)),
 .UNSPECIFIED.,.F.,.F.,.F.)
B_SPLINE_SURFACE_WITH_KNOTS((2,2),(3,3),(0.710192959008098,1.),(0.176967058622921,
0.194235682574592),.UNSPECIFIED.)
GEOMETRIC_REPRESENTATION_ITEM()
RATIONAL_B_SPLINE_SURFACE(((0.98748925405691,0.987216959588931,0.989875504592249),
(0.98748925405691,0.987216959588931,0.989875504592249)))
REPRESENTATION_ITEM('')
SURFACE()
);
#2390=(
BOUNDED_SURFACE()
B_SPLINE_SURFACE(1,2,((#134476,#134477,#134478),(#134479,#134480,#134481)),
 .UNSPECIFIED.,.F.,.F.,.F.)
B_SPLINE_SURFACE_WITH_KNOTS((2,2),(3,3),(0.710318915638586,1.),(0.538896351358319,
0.556212823028862),.UNSPECIFIED.)
GEOMETRIC_REPRESENTATION_ITEM()
RATIONAL_B_SPLINE_SURFACE(((0.987563472532048,0.988105030697866,0.991593692313266),
(0.987563472532048,0.988105030697866,0.991593692313266)))
REPRESENTATION_ITEM('')
SURFACE()
);
#2391=(
BOUNDED_SURFACE()
B_SPLINE_SURFACE(1,2,((#134492,#134493,#134494),(#134495,#134496,#134497)),
 .UNSPECIFIED.,.F.,.F.,.F.)
B_SPLINE_SURFACE_WITH_KNOTS((2,2),(3,3),(0.710192959006949,1.),(0.176967058622921,
0.194235682574592),.UNSPECIFIED.)
GEOMETRIC_REPRESENTATION_ITEM()
RATIONAL_B_SPLINE_SURFACE(((0.98748925405691,0.987216959588931,0.989875504592249),
(0.98748925405691,0.987216959588931,0.989875504592249)))
REPRESENTATION_ITEM('')
SURFACE()
);
#2392=(
BOUNDED_SURFACE()
B_SPLINE_SURFACE(1,2,((#134505,#134506,#134507),(#134508,#134509,#134510)),
 .UNSPECIFIED.,.F.,.F.,.F.)
B_SPLINE_SURFACE_WITH_KNOTS((2,2),(3,3),(0.710318915638841,1.),(0.538896351358319,
0.556212823028862),.UNSPECIFIED.)
GEOMETRIC_REPRESENTATION_ITEM()
RATIONAL_B_SPLINE_SURFACE(((0.987563472532048,0.988105030697866,0.991593692313266),
(0.987563472532048,0.988105030697866,0.991593692313266)))
REPRESENTATION_ITEM('')
SURFACE()
);
#2393=(
BOUNDED_SURFACE()
B_SPLINE_SURFACE(1,2,((#134521,#134522,#134523),(#134524,#134525,#134526)),
 .UNSPECIFIED.,.F.,.F.,.F.)
B_SPLINE_SURFACE_WITH_KNOTS((2,2),(3,3),(0.710192959007194,1.),(0.176967058622922,
0.194235682574592),.UNSPECIFIED.)
GEOMETRIC_REPRESENTATION_ITEM()
RATIONAL_B_SPLINE_SURFACE(((0.98748925405691,0.987216959588932,0.989875504592249),
(0.98748925405691,0.987216959588932,0.989875504592249)))
REPRESENTATION_ITEM('')
SURFACE()
);
#2394=(
BOUNDED_SURFACE()
B_SPLINE_SURFACE(1,2,((#134534,#134535,#134536),(#134537,#134538,#134539)),
 .UNSPECIFIED.,.F.,.F.,.F.)
B_SPLINE_SURFACE_WITH_KNOTS((2,2),(3,3),(0.710318915640079,1.),(0.538896351358318,
0.556212823028861),.UNSPECIFIED.)
GEOMETRIC_REPRESENTATION_ITEM()
RATIONAL_B_SPLINE_SURFACE(((0.987563472532048,0.988105030697865,0.991593692313265),
(0.987563472532048,0.988105030697865,0.991593692313265)))
REPRESENTATION_ITEM('')
SURFACE()
);
#2395=(
BOUNDED_SURFACE()
B_SPLINE_SURFACE(1,2,((#134550,#134551,#134552),(#134553,#134554,#134555)),
 .UNSPECIFIED.,.F.,.F.,.F.)
B_SPLINE_SURFACE_WITH_KNOTS((2,2),(3,3),(0.71019295900844,1.),(0.176967058622922,
0.194235682574593),.UNSPECIFIED.)
GEOMETRIC_REPRESENTATION_ITEM()
RATIONAL_B_SPLINE_SURFACE(((0.98748925405691,0.987216959588932,0.989875504592249),
(0.98748925405691,0.987216959588932,0.989875504592249)))
REPRESENTATION_ITEM('')
SURFACE()
);
#2396=(
BOUNDED_SURFACE()
B_SPLINE_SURFACE(1,2,((#134563,#134564,#134565),(#134566,#134567,#134568)),
 .UNSPECIFIED.,.F.,.F.,.F.)
B_SPLINE_SURFACE_WITH_KNOTS((2,2),(3,3),(0.710318915640083,1.),(0.538896351358318,
0.556212823028861),.UNSPECIFIED.)
GEOMETRIC_REPRESENTATION_ITEM()
RATIONAL_B_SPLINE_SURFACE(((0.987563472532048,0.988105030697865,0.991593692313265),
(0.987563472532048,0.988105030697865,0.991593692313265)))
REPRESENTATION_ITEM('')
SURFACE()
);
#2397=(
BOUNDED_SURFACE()
B_SPLINE_SURFACE(1,2,((#134579,#134580,#134581),(#134582,#134583,#134584)),
 .UNSPECIFIED.,.F.,.F.,.F.)
B_SPLINE_SURFACE_WITH_KNOTS((2,2),(3,3),(0.710192959008441,1.),(0.176967058622922,
0.194235682574593),.UNSPECIFIED.)
GEOMETRIC_REPRESENTATION_ITEM()
RATIONAL_B_SPLINE_SURFACE(((0.98748925405691,0.987216959588932,0.989875504592249),
(0.98748925405691,0.987216959588932,0.989875504592249)))
REPRESENTATION_ITEM('')
SURFACE()
);
#2398=(
BOUNDED_SURFACE()
B_SPLINE_SURFACE(1,2,((#134592,#134593,#134594,#134595,#134596),(#134597,
#134598,#134599,#134600,#134601)),.UNSPECIFIED.,.F.,.F.,.F.)
B_SPLINE_SURFACE_WITH_KNOTS((2,2),(3,2,3),(0.710192959006966,1.),(0.504546746572904,
0.504719756175826,0.522020716468042),.UNSPECIFIED.)
GEOMETRIC_REPRESENTATION_ITEM()
RATIONAL_B_SPLINE_SURFACE(((0.99690557929439,0.99690557929439,0.99690557929439,
0.991635321911236,0.989306890555884),(0.99690557929439,0.99690557929439,
0.99690557929439,0.991635321911236,0.989306890555884)))
REPRESENTATION_ITEM('')
SURFACE()
);
#2399=(
BOUNDED_SURFACE()
B_SPLINE_SURFACE(1,2,((#134614,#134615,#134616,#134617,#134618,#134619,
#134620),(#134621,#134622,#134623,#134624,#134625,#134626,#134627)),
 .UNSPECIFIED.,.F.,.F.,.F.)
B_SPLINE_SURFACE_WITH_KNOTS((2,2),(3,2,2,3),(0.710318915640022,1.),(0.211398300093701,
0.214285714285714,0.228883374894809,0.22905822564282),.UNSPECIFIED.)
GEOMETRIC_REPRESENTATION_ITEM()
RATIONAL_B_SPLINE_SURFACE(((0.998054921708739,0.998986490969345,1.,0.994876086397764,
0.991846493044689,0.991846493044689,0.991846493044689),(0.998054921708739,
0.998986490969345,1.,0.994876086397764,0.991846493044689,0.991846493044689,
0.991846493044689)))
REPRESENTATION_ITEM('')
SURFACE()
);
#2400=(
BOUNDED_SURFACE()
B_SPLINE_SURFACE(1,2,((#134638,#134639,#134640,#134641,#134642),(#134643,
#134644,#134645,#134646,#134647)),.UNSPECIFIED.,.F.,.F.,.F.)
B_SPLINE_SURFACE_WITH_KNOTS((2,2),(3,2,3),(0.710192959007032,1.),(0.504546746573206,
0.504719756176125,0.522020716468041),.UNSPECIFIED.)
GEOMETRIC_REPRESENTATION_ITEM()
RATIONAL_B_SPLINE_SURFACE(((0.996905579294208,0.996905579294208,0.996905579294208,
0.991635321911196,0.989306890555884),(0.996905579294208,0.996905579294208,
0.996905579294208,0.991635321911196,0.989306890555884)))
REPRESENTATION_ITEM('')
SURFACE()
);
#2401=(
BOUNDED_SURFACE()
B_SPLINE_SURFACE(1,2,((#134660,#134661,#134662,#134663,#134664,#134665,
#134666),(#134667,#134668,#134669,#134670,#134671,#134672,#134673)),
 .UNSPECIFIED.,.F.,.F.,.F.)
B_SPLINE_SURFACE_WITH_KNOTS((2,2),(3,2,2,3),(0.710318915640066,1.),(0.2113983000937,
0.214285714285714,0.228883374894809,0.22905822564282),.UNSPECIFIED.)
GEOMETRIC_REPRESENTATION_ITEM()
RATIONAL_B_SPLINE_SURFACE(((0.998054921708738,0.998986490969345,1.,0.994876086397764,
0.991846493044689,0.991846493044689,0.991846493044689),(0.998054921708738,
0.998986490969345,1.,0.994876086397764,0.991846493044689,0.991846493044689,
0.991846493044689)))
REPRESENTATION_ITEM('')
SURFACE()
);
#2402=(
BOUNDED_SURFACE()
B_SPLINE_SURFACE(1,2,((#134684,#134685,#134686,#134687,#134688),(#134689,
#134690,#134691,#134692,#134693)),.UNSPECIFIED.,.F.,.F.,.F.)
B_SPLINE_SURFACE_WITH_KNOTS((2,2),(3,2,3),(0.710192959007032,1.),(0.504546746573288,
0.504719756176206,0.522020716468041),.UNSPECIFIED.)
GEOMETRIC_REPRESENTATION_ITEM()
RATIONAL_B_SPLINE_SURFACE(((0.996905579294158,0.996905579294158,0.996905579294158,
0.991635321911186,0.989306890555884),(0.996905579294158,0.996905579294158,
0.996905579294158,0.991635321911186,0.989306890555884)))
REPRESENTATION_ITEM('')
SURFACE()
);
#2403=(
BOUNDED_SURFACE()
B_SPLINE_SURFACE(1,2,((#134706,#134707,#134708,#134709,#134710,#134711,
#134712),(#134713,#134714,#134715,#134716,#134717,#134718,#134719)),
 .UNSPECIFIED.,.F.,.F.,.F.)
B_SPLINE_SURFACE_WITH_KNOTS((2,2),(3,2,2,3),(0.710318915639876,1.),(0.2113983000937,
0.214285714285714,0.228883374894809,0.22905822564282),.UNSPECIFIED.)
GEOMETRIC_REPRESENTATION_ITEM()
RATIONAL_B_SPLINE_SURFACE(((0.998054921708738,0.998986490969345,1.,0.994876086397764,
0.991846493044689,0.991846493044689,0.991846493044689),(0.998054921708738,
0.998986490969345,1.,0.994876086397764,0.991846493044689,0.991846493044689,
0.991846493044689)))
REPRESENTATION_ITEM('')
SURFACE()
);
#2404=(
BOUNDED_SURFACE()
B_SPLINE_SURFACE(1,2,((#134730,#134731,#134732,#134733,#134734),(#134735,
#134736,#134737,#134738,#134739)),.UNSPECIFIED.,.F.,.F.,.F.)
B_SPLINE_SURFACE_WITH_KNOTS((2,2),(3,2,3),(0.710192959007029,1.),(0.504546746573288,
0.504719756176206,0.522020716468041),.UNSPECIFIED.)
GEOMETRIC_REPRESENTATION_ITEM()
RATIONAL_B_SPLINE_SURFACE(((0.996905579294158,0.996905579294158,0.996905579294158,
0.991635321911186,0.989306890555884),(0.996905579294158,0.996905579294158,
0.996905579294158,0.991635321911186,0.989306890555885)))
REPRESENTATION_ITEM('')
SURFACE()
);
#2405=(
BOUNDED_SURFACE()
B_SPLINE_SURFACE(1,2,((#134752,#134753,#134754,#134755,#134756,#134757,
#134758),(#134759,#134760,#134761,#134762,#134763,#134764,#134765)),
 .UNSPECIFIED.,.F.,.F.,.F.)
B_SPLINE_SURFACE_WITH_KNOTS((2,2),(3,2,2,3),(0.71031891564008,1.),(0.2113983000937,
0.214285714285714,0.228883374894809,0.22905822564282),.UNSPECIFIED.)
GEOMETRIC_REPRESENTATION_ITEM()
RATIONAL_B_SPLINE_SURFACE(((0.998054921708738,0.998986490969345,1.,0.994876086397764,
0.991846493044689,0.991846493044689,0.991846493044689),(0.998054921708738,
0.998986490969345,1.,0.994876086397764,0.991846493044689,0.991846493044689,
0.991846493044689)))
REPRESENTATION_ITEM('')
SURFACE()
);
#2406=(
BOUNDED_SURFACE()
B_SPLINE_SURFACE(1,2,((#134776,#134777,#134778,#134779,#134780),(#134781,
#134782,#134783,#134784,#134785)),.UNSPECIFIED.,.F.,.F.,.F.)
B_SPLINE_SURFACE_WITH_KNOTS((2,2),(3,2,3),(0.710192959007034,1.),(0.504546746572823,
0.504719756175746,0.522020716468043),.UNSPECIFIED.)
GEOMETRIC_REPRESENTATION_ITEM()
RATIONAL_B_SPLINE_SURFACE(((0.996905579294439,0.996905579294439,0.996905579294439,
0.991635321911247,0.989306890555884),(0.996905579294439,0.996905579294439,
0.996905579294439,0.991635321911247,0.989306890555884)))
REPRESENTATION_ITEM('')
SURFACE()
);
#2407=(
BOUNDED_SURFACE()
B_SPLINE_SURFACE(1,2,((#134798,#134799,#134800,#134801,#134802,#134803,
#134804),(#134805,#134806,#134807,#134808,#134809,#134810,#134811)),
 .UNSPECIFIED.,.F.,.F.,.F.)
B_SPLINE_SURFACE_WITH_KNOTS((2,2),(3,2,2,3),(0.710318915639999,1.),(0.211398300093699,
0.214285714285714,0.228883374894809,0.22905822564282),.UNSPECIFIED.)
GEOMETRIC_REPRESENTATION_ITEM()
RATIONAL_B_SPLINE_SURFACE(((0.998054921708737,0.998986490969345,1.,0.994876086397764,
0.991846493044689,0.991846493044689,0.991846493044689),(0.998054921708737,
0.998986490969345,1.,0.994876086397764,0.991846493044689,0.991846493044689,
0.991846493044689)))
REPRESENTATION_ITEM('')
SURFACE()
);
#2408=(
BOUNDED_SURFACE()
B_SPLINE_SURFACE(1,2,((#134822,#134823,#134824,#134825,#134826),(#134827,
#134828,#134829,#134830,#134831)),.UNSPECIFIED.,.F.,.F.,.F.)
B_SPLINE_SURFACE_WITH_KNOTS((2,2),(3,2,3),(0.71019295900703,1.),(0.504546746572967,
0.504719756175888,0.522020716468043),.UNSPECIFIED.)
GEOMETRIC_REPRESENTATION_ITEM()
RATIONAL_B_SPLINE_SURFACE(((0.996905579294352,0.996905579294352,0.996905579294352,
0.991635321911228,0.989306890555884),(0.996905579294352,0.996905579294352,
0.996905579294352,0.991635321911228,0.989306890555884)))
REPRESENTATION_ITEM('')
SURFACE()
);
#2409=(
BOUNDED_SURFACE()
B_SPLINE_SURFACE(1,2,((#134844,#134845,#134846,#134847,#134848,#134849,
#134850),(#134851,#134852,#134853,#134854,#134855,#134856,#134857)),
 .UNSPECIFIED.,.F.,.F.,.F.)
B_SPLINE_SURFACE_WITH_KNOTS((2,2),(3,2,2,3),(0.710318915640028,1.),(0.2113983000937,
0.214285714285714,0.228883374894809,0.22905822564282),.UNSPECIFIED.)
GEOMETRIC_REPRESENTATION_ITEM()
RATIONAL_B_SPLINE_SURFACE(((0.998054921708738,0.998986490969345,1.,0.994876086397764,
0.991846493044689,0.991846493044689,0.991846493044689),(0.998054921708738,
0.998986490969345,1.,0.994876086397764,0.991846493044689,0.991846493044689,
0.991846493044689)))
REPRESENTATION_ITEM('')
SURFACE()
);
#2410=(
BOUNDED_SURFACE()
B_SPLINE_SURFACE(1,2,((#134872,#134873,#134874,#134875,#134876),(#134877,
#134878,#134879,#134880,#134881)),.UNSPECIFIED.,.F.,.F.,.F.)
B_SPLINE_SURFACE_WITH_KNOTS((2,2),(3,2,3),(0.710192959007035,1.),(0.504546746573141,
0.504719756176061,0.522020716468042),.UNSPECIFIED.)
GEOMETRIC_REPRESENTATION_ITEM()
RATIONAL_B_SPLINE_SURFACE(((0.996905579294247,0.996905579294247,0.996905579294247,
0.991635321911205,0.989306890555884),(0.996905579294247,0.996905579294247,
0.996905579294247,0.991635321911205,0.989306890555884)))
REPRESENTATION_ITEM('')
SURFACE()
);
#2411=(
BOUNDED_SURFACE()
B_SPLINE_SURFACE(1,2,((#134894,#134895,#134896,#134897,#134898,#134899,
#134900),(#134901,#134902,#134903,#134904,#134905,#134906,#134907)),
 .UNSPECIFIED.,.F.,.F.,.F.)
B_SPLINE_SURFACE_WITH_KNOTS((2,2),(3,2,2,3),(0.710318915639771,1.),(0.2113983000937,
0.214285714285714,0.228883374894809,0.22905822564282),.UNSPECIFIED.)
GEOMETRIC_REPRESENTATION_ITEM()
RATIONAL_B_SPLINE_SURFACE(((0.998054921708738,0.998986490969345,1.,0.994876086397764,
0.991846493044689,0.991846493044689,0.991846493044689),(0.998054921708738,
0.998986490969345,1.,0.994876086397764,0.991846493044689,0.991846493044689,
0.991846493044689)))
REPRESENTATION_ITEM('')
SURFACE()
);
#2412=(
BOUNDED_SURFACE()
B_SPLINE_SURFACE(1,2,((#134918,#134919,#134920,#134921,#134922),(#134923,
#134924,#134925,#134926,#134927)),.UNSPECIFIED.,.F.,.F.,.F.)
B_SPLINE_SURFACE_WITH_KNOTS((2,2),(3,2,3),(0.710192959007034,1.),(0.504546746573288,
0.504719756176206,0.522020716468041),.UNSPECIFIED.)
GEOMETRIC_REPRESENTATION_ITEM()
RATIONAL_B_SPLINE_SURFACE(((0.996905579294158,0.996905579294158,0.996905579294158,
0.991635321911186,0.989306890555884),(0.996905579294158,0.996905579294158,
0.996905579294158,0.991635321911186,0.989306890555884)))
REPRESENTATION_ITEM('')
SURFACE()
);
#2413=(
BOUNDED_SURFACE()
B_SPLINE_SURFACE(1,2,((#134940,#134941,#134942,#134943,#134944,#134945,
#134946),(#134947,#134948,#134949,#134950,#134951,#134952,#134953)),
 .UNSPECIFIED.,.F.,.F.,.F.)
B_SPLINE_SURFACE_WITH_KNOTS((2,2),(3,2,2,3),(0.710318915639696,1.),(0.2113983000937,
0.214285714285714,0.228883374894809,0.22905822564282),.UNSPECIFIED.)
GEOMETRIC_REPRESENTATION_ITEM()
RATIONAL_B_SPLINE_SURFACE(((0.998054921708738,0.998986490969345,1.,0.994876086397764,
0.991846493044689,0.991846493044689,0.991846493044689),(0.998054921708738,
0.998986490969345,1.,0.994876086397764,0.991846493044689,0.991846493044689,
0.991846493044689)))
REPRESENTATION_ITEM('')
SURFACE()
);
#2414=(
BOUNDED_SURFACE()
B_SPLINE_SURFACE(1,2,((#134964,#134965,#134966,#134967,#134968),(#134969,
#134970,#134971,#134972,#134973)),.UNSPECIFIED.,.F.,.F.,.F.)
B_SPLINE_SURFACE_WITH_KNOTS((2,2),(3,2,3),(0.710192959007031,1.),(0.504546746573288,
0.504719756176206,0.522020716468041),.UNSPECIFIED.)
GEOMETRIC_REPRESENTATION_ITEM()
RATIONAL_B_SPLINE_SURFACE(((0.996905579294158,0.996905579294158,0.996905579294158,
0.991635321911186,0.989306890555884),(0.996905579294158,0.996905579294158,
0.996905579294158,0.991635321911186,0.989306890555884)))
REPRESENTATION_ITEM('')
SURFACE()
);
#2415=(
BOUNDED_SURFACE()
B_SPLINE_SURFACE(1,2,((#134986,#134987,#134988,#134989,#134990,#134991,
#134992),(#134993,#134994,#134995,#134996,#134997,#134998,#134999)),
 .UNSPECIFIED.,.F.,.F.,.F.)
B_SPLINE_SURFACE_WITH_KNOTS((2,2),(3,2,2,3),(0.710318915640075,1.),(0.211398300093699,
0.214285714285714,0.228883374894809,0.22905822564282),.UNSPECIFIED.)
GEOMETRIC_REPRESENTATION_ITEM()
RATIONAL_B_SPLINE_SURFACE(((0.998054921708738,0.998986490969345,1.,0.994876086397764,
0.991846493044689,0.991846493044689,0.991846493044689),(0.998054921708738,
0.998986490969345,1.,0.994876086397764,0.991846493044689,0.991846493044689,
0.991846493044689)))
REPRESENTATION_ITEM('')
SURFACE()
);
#2416=(
BOUNDED_SURFACE()
B_SPLINE_SURFACE(1,2,((#135010,#135011,#135012,#135013,#135014),(#135015,
#135016,#135017,#135018,#135019)),.UNSPECIFIED.,.F.,.F.,.F.)
B_SPLINE_SURFACE_WITH_KNOTS((2,2),(3,2,3),(0.710192959007033,1.),(0.504546746573288,
0.504719756176206,0.522020716468041),.UNSPECIFIED.)
GEOMETRIC_REPRESENTATION_ITEM()
RATIONAL_B_SPLINE_SURFACE(((0.996905579294158,0.996905579294158,0.996905579294158,
0.991635321911186,0.989306890555884),(0.996905579294158,0.996905579294158,
0.996905579294158,0.991635321911186,0.989306890555884)))
REPRESENTATION_ITEM('')
SURFACE()
);
#2417=(
BOUNDED_SURFACE()
B_SPLINE_SURFACE(1,2,((#135032,#135033,#135034,#135035,#135036,#135037,
#135038),(#135039,#135040,#135041,#135042,#135043,#135044,#135045)),
 .UNSPECIFIED.,.F.,.F.,.F.)
B_SPLINE_SURFACE_WITH_KNOTS((2,2),(3,2,2,3),(0.710318915640075,1.),(0.211398300093695,
0.214285714285714,0.228883374894809,0.22905822564282),.UNSPECIFIED.)
GEOMETRIC_REPRESENTATION_ITEM()
RATIONAL_B_SPLINE_SURFACE(((0.998054921708735,0.998986490969344,1.,0.994876086397764,
0.991846493044689,0.991846493044689,0.991846493044689),(0.998054921708735,
0.998986490969344,1.,0.994876086397764,0.991846493044689,0.991846493044689,
0.991846493044689)))
REPRESENTATION_ITEM('')
SURFACE()
);
#2418=(
BOUNDED_SURFACE()
B_SPLINE_SURFACE(1,2,((#135056,#135057,#135058,#135059,#135060),(#135061,
#135062,#135063,#135064,#135065)),.UNSPECIFIED.,.F.,.F.,.F.)
B_SPLINE_SURFACE_WITH_KNOTS((2,2),(3,2,3),(0.71019295900703,1.),(0.504546746573288,
0.504719756176206,0.522020716468041),.UNSPECIFIED.)
GEOMETRIC_REPRESENTATION_ITEM()
RATIONAL_B_SPLINE_SURFACE(((0.996905579294158,0.996905579294158,0.996905579294158,
0.991635321911186,0.989306890555885),(0.996905579294158,0.996905579294158,
0.996905579294158,0.991635321911186,0.989306890555885)))
REPRESENTATION_ITEM('')
SURFACE()
);
#2419=(
BOUNDED_SURFACE()
B_SPLINE_SURFACE(1,2,((#135078,#135079,#135080,#135081,#135082,#135083,
#135084),(#135085,#135086,#135087,#135088,#135089,#135090,#135091)),
 .UNSPECIFIED.,.F.,.F.,.F.)
B_SPLINE_SURFACE_WITH_KNOTS((2,2),(3,2,2,3),(0.710318915640078,1.),(0.2113983000937,
0.214285714285714,0.228883374894809,0.22905822564282),.UNSPECIFIED.)
GEOMETRIC_REPRESENTATION_ITEM()
RATIONAL_B_SPLINE_SURFACE(((0.998054921708738,0.998986490969345,1.,0.994876086397764,
0.991846493044689,0.991846493044689,0.991846493044689),(0.998054921708738,
0.998986490969345,1.,0.994876086397764,0.991846493044689,0.991846493044689,
0.991846493044689)))
REPRESENTATION_ITEM('')
SURFACE()
);
#2420=(
BOUNDED_SURFACE()
B_SPLINE_SURFACE(1,2,((#135102,#135103,#135104,#135105,#135106),(#135107,
#135108,#135109,#135110,#135111)),.UNSPECIFIED.,.F.,.F.,.F.)
B_SPLINE_SURFACE_WITH_KNOTS((2,2),(3,2,3),(0.71019295900703,1.),(0.504546746573288,
0.504719756176206,0.522020716468041),.UNSPECIFIED.)
GEOMETRIC_REPRESENTATION_ITEM()
RATIONAL_B_SPLINE_SURFACE(((0.996905579294158,0.996905579294158,0.996905579294158,
0.991635321911186,0.989306890555884),(0.996905579294158,0.996905579294158,
0.996905579294158,0.991635321911186,0.989306890555884)))
REPRESENTATION_ITEM('')
SURFACE()
);
#2421=(
BOUNDED_SURFACE()
B_SPLINE_SURFACE(1,2,((#135124,#135125,#135126,#135127,#135128,#135129,
#135130),(#135131,#135132,#135133,#135134,#135135,#135136,#135137)),
 .UNSPECIFIED.,.F.,.F.,.F.)
B_SPLINE_SURFACE_WITH_KNOTS((2,2),(3,2,2,3),(0.710318915640077,1.),(0.2113983000937,
0.214285714285714,0.228883374894809,0.22905822564282),.UNSPECIFIED.)
GEOMETRIC_REPRESENTATION_ITEM()
RATIONAL_B_SPLINE_SURFACE(((0.998054921708738,0.998986490969345,1.,0.994876086397764,
0.991846493044689,0.991846493044689,0.991846493044689),(0.998054921708738,
0.998986490969345,1.,0.994876086397764,0.991846493044689,0.991846493044689,
0.991846493044689)))
REPRESENTATION_ITEM('')
SURFACE()
);
#2422=(
BOUNDED_SURFACE()
B_SPLINE_SURFACE(1,2,((#135148,#135149,#135150,#135151,#135152),(#135153,
#135154,#135155,#135156,#135157)),.UNSPECIFIED.,.F.,.F.,.F.)
B_SPLINE_SURFACE_WITH_KNOTS((2,2),(3,2,3),(0.710192959007036,1.),(0.504546746573288,
0.504719756176206,0.522020716468041),.UNSPECIFIED.)
GEOMETRIC_REPRESENTATION_ITEM()
RATIONAL_B_SPLINE_SURFACE(((0.996905579294158,0.996905579294158,0.996905579294158,
0.991635321911186,0.989306890555884),(0.996905579294158,0.996905579294158,
0.996905579294158,0.991635321911186,0.989306890555884)))
REPRESENTATION_ITEM('')
SURFACE()
);
#2423=(
BOUNDED_SURFACE()
B_SPLINE_SURFACE(1,2,((#135170,#135171,#135172,#135173,#135174,#135175,
#135176),(#135177,#135178,#135179,#135180,#135181,#135182,#135183)),
 .UNSPECIFIED.,.F.,.F.,.F.)
B_SPLINE_SURFACE_WITH_KNOTS((2,2),(3,2,2,3),(0.710318915640077,1.),(0.2113983000937,
0.214285714285714,0.228883374894809,0.22905822564282),.UNSPECIFIED.)
GEOMETRIC_REPRESENTATION_ITEM()
RATIONAL_B_SPLINE_SURFACE(((0.998054921708738,0.998986490969345,1.,0.994876086397764,
0.991846493044689,0.991846493044689,0.991846493044689),(0.998054921708738,
0.998986490969345,1.,0.994876086397764,0.991846493044689,0.991846493044689,
0.991846493044689)))
REPRESENTATION_ITEM('')
SURFACE()
);
#2424=(
BOUNDED_SURFACE()
B_SPLINE_SURFACE(1,2,((#135198,#135199,#135200,#135201,#135202),(#135203,
#135204,#135205,#135206,#135207)),.UNSPECIFIED.,.F.,.F.,.F.)
B_SPLINE_SURFACE_WITH_KNOTS((2,2),(3,2,3),(0.710192959007037,1.),(0.504546746573288,
0.504719756176206,0.522020716468041),.UNSPECIFIED.)
GEOMETRIC_REPRESENTATION_ITEM()
RATIONAL_B_SPLINE_SURFACE(((0.996905579294158,0.996905579294158,0.996905579294158,
0.991635321911186,0.989306890555884),(0.996905579294158,0.996905579294158,
0.996905579294158,0.991635321911186,0.989306890555884)))
REPRESENTATION_ITEM('')
SURFACE()
);
#2425=(
BOUNDED_SURFACE()
B_SPLINE_SURFACE(1,2,((#135220,#135221,#135222,#135223,#135224,#135225,
#135226),(#135227,#135228,#135229,#135230,#135231,#135232,#135233)),
 .UNSPECIFIED.,.F.,.F.,.F.)
B_SPLINE_SURFACE_WITH_KNOTS((2,2),(3,2,2,3),(0.710318915640079,1.),(0.2113983000937,
0.214285714285714,0.228883374894809,0.22905822564282),.UNSPECIFIED.)
GEOMETRIC_REPRESENTATION_ITEM()
RATIONAL_B_SPLINE_SURFACE(((0.998054921708738,0.998986490969345,1.,0.994876086397764,
0.991846493044689,0.991846493044689,0.991846493044689),(0.998054921708738,
0.998986490969345,1.,0.994876086397764,0.991846493044689,0.991846493044689,
0.991846493044689)))
REPRESENTATION_ITEM('')
SURFACE()
);
#2426=(
BOUNDED_SURFACE()
B_SPLINE_SURFACE(1,2,((#135248,#135249,#135250,#135251,#135252),(#135253,
#135254,#135255,#135256,#135257)),.UNSPECIFIED.,.F.,.F.,.F.)
B_SPLINE_SURFACE_WITH_KNOTS((2,2),(3,2,3),(0.71019295900703,1.),(0.504546746573288,
0.504719756176206,0.522020716468041),.UNSPECIFIED.)
GEOMETRIC_REPRESENTATION_ITEM()
RATIONAL_B_SPLINE_SURFACE(((0.996905579294158,0.996905579294158,0.996905579294158,
0.991635321911186,0.989306890555884),(0.996905579294158,0.996905579294158,
0.996905579294158,0.991635321911186,0.989306890555884)))
REPRESENTATION_ITEM('')
SURFACE()
);
#2427=(
BOUNDED_SURFACE()
B_SPLINE_SURFACE(1,2,((#135270,#135271,#135272,#135273,#135274,#135275,
#135276),(#135277,#135278,#135279,#135280,#135281,#135282,#135283)),
 .UNSPECIFIED.,.F.,.F.,.F.)
B_SPLINE_SURFACE_WITH_KNOTS((2,2),(3,2,2,3),(0.710318915640075,1.),(0.2113983000936,
0.214285714285714,0.228883374894809,0.229058225642821),.UNSPECIFIED.)
GEOMETRIC_REPRESENTATION_ITEM()
RATIONAL_B_SPLINE_SURFACE(((0.998054921708674,0.99898649096931,1.,0.994876086397764,
0.991846493044689,0.991846493044689,0.991846493044689),(0.998054921708674,
0.99898649096931,1.,0.994876086397764,0.991846493044689,0.991846493044689,
0.991846493044689)))
REPRESENTATION_ITEM('')
SURFACE()
);
#2428=(
BOUNDED_SURFACE()
B_SPLINE_SURFACE(1,2,((#135298,#135299,#135300,#135301,#135302),(#135303,
#135304,#135305,#135306,#135307)),.UNSPECIFIED.,.F.,.F.,.F.)
B_SPLINE_SURFACE_WITH_KNOTS((2,2),(3,2,3),(0.710192959007027,1.),(0.504546746573288,
0.504719756176206,0.522020716468041),.UNSPECIFIED.)
GEOMETRIC_REPRESENTATION_ITEM()
RATIONAL_B_SPLINE_SURFACE(((0.996905579294158,0.996905579294158,0.996905579294158,
0.991635321911186,0.989306890555884),(0.996905579294158,0.996905579294158,
0.996905579294158,0.991635321911186,0.989306890555884)))
REPRESENTATION_ITEM('')
SURFACE()
);
#2429=(
BOUNDED_SURFACE()
B_SPLINE_SURFACE(1,2,((#135320,#135321,#135322,#135323,#135324,#135325,
#135326),(#135327,#135328,#135329,#135330,#135331,#135332,#135333)),
 .UNSPECIFIED.,.F.,.F.,.F.)
B_SPLINE_SURFACE_WITH_KNOTS((2,2),(3,2,2,3),(0.710318915640073,1.),(0.2113983000937,
0.214285714285714,0.228883374894809,0.22905822564282),.UNSPECIFIED.)
GEOMETRIC_REPRESENTATION_ITEM()
RATIONAL_B_SPLINE_SURFACE(((0.998054921708738,0.998986490969345,1.,0.994876086397764,
0.991846493044689,0.991846493044689,0.991846493044689),(0.998054921708738,
0.998986490969345,1.,0.994876086397764,0.991846493044689,0.991846493044689,
0.991846493044689)))
REPRESENTATION_ITEM('')
SURFACE()
);
#2430=(
BOUNDED_SURFACE()
B_SPLINE_SURFACE(1,2,((#135344,#135345,#135346,#135347,#135348),(#135349,
#135350,#135351,#135352,#135353)),.UNSPECIFIED.,.F.,.F.,.F.)
B_SPLINE_SURFACE_WITH_KNOTS((2,2),(3,2,3),(0.710192959007035,1.),(0.504546746573288,
0.504719756176206,0.522020716468041),.UNSPECIFIED.)
GEOMETRIC_REPRESENTATION_ITEM()
RATIONAL_B_SPLINE_SURFACE(((0.996905579294158,0.996905579294158,0.996905579294158,
0.991635321911186,0.989306890555884),(0.996905579294158,0.996905579294158,
0.996905579294158,0.991635321911186,0.989306890555884)))
REPRESENTATION_ITEM('')
SURFACE()
);
#2431=(
BOUNDED_SURFACE()
B_SPLINE_SURFACE(1,2,((#135366,#135367,#135368,#135369,#135370,#135371,
#135372),(#135373,#135374,#135375,#135376,#135377,#135378,#135379)),
 .UNSPECIFIED.,.F.,.F.,.F.)
B_SPLINE_SURFACE_WITH_KNOTS((2,2),(3,2,2,3),(0.71031891564008,1.),(0.2113983000937,
0.214285714285714,0.228883374894809,0.22905822564282),.UNSPECIFIED.)
GEOMETRIC_REPRESENTATION_ITEM()
RATIONAL_B_SPLINE_SURFACE(((0.998054921708738,0.998986490969345,1.,0.994876086397764,
0.991846493044689,0.991846493044689,0.991846493044689),(0.998054921708738,
0.998986490969345,1.,0.994876086397764,0.991846493044689,0.991846493044689,
0.991846493044689)))
REPRESENTATION_ITEM('')
SURFACE()
);
#2432=(
BOUNDED_SURFACE()
B_SPLINE_SURFACE(1,2,((#135390,#135391,#135392,#135393,#135394),(#135395,
#135396,#135397,#135398,#135399)),.UNSPECIFIED.,.F.,.F.,.F.)
B_SPLINE_SURFACE_WITH_KNOTS((2,2),(3,2,3),(0.710192959007028,1.),(0.504546746573288,
0.504719756176206,0.522020716468041),.UNSPECIFIED.)
GEOMETRIC_REPRESENTATION_ITEM()
RATIONAL_B_SPLINE_SURFACE(((0.996905579294158,0.996905579294158,0.996905579294158,
0.991635321911186,0.989306890555884),(0.996905579294158,0.996905579294158,
0.996905579294158,0.991635321911186,0.989306890555884)))
REPRESENTATION_ITEM('')
SURFACE()
);
#2433=(
BOUNDED_SURFACE()
B_SPLINE_SURFACE(1,2,((#135412,#135413,#135414,#135415,#135416,#135417,
#135418),(#135419,#135420,#135421,#135422,#135423,#135424,#135425)),
 .UNSPECIFIED.,.F.,.F.,.F.)
B_SPLINE_SURFACE_WITH_KNOTS((2,2),(3,2,2,3),(0.710318915640078,1.),(0.2113983000937,
0.214285714285714,0.228883374894809,0.22905822564282),.UNSPECIFIED.)
GEOMETRIC_REPRESENTATION_ITEM()
RATIONAL_B_SPLINE_SURFACE(((0.998054921708738,0.998986490969345,1.,0.994876086397764,
0.991846493044689,0.991846493044689,0.991846493044689),(0.998054921708738,
0.998986490969345,1.,0.994876086397764,0.991846493044689,0.991846493044689,
0.991846493044689)))
REPRESENTATION_ITEM('')
SURFACE()
);
#2434=(
BOUNDED_SURFACE()
B_SPLINE_SURFACE(1,2,((#135436,#135437,#135438,#135439,#135440),(#135441,
#135442,#135443,#135444,#135445)),.UNSPECIFIED.,.F.,.F.,.F.)
B_SPLINE_SURFACE_WITH_KNOTS((2,2),(3,2,3),(0.710192959007034,1.),(0.504546746573288,
0.504719756176206,0.522020716468041),.UNSPECIFIED.)
GEOMETRIC_REPRESENTATION_ITEM()
RATIONAL_B_SPLINE_SURFACE(((0.996905579294158,0.996905579294158,0.996905579294158,
0.991635321911186,0.989306890555884),(0.996905579294158,0.996905579294158,
0.996905579294158,0.991635321911186,0.989306890555884)))
REPRESENTATION_ITEM('')
SURFACE()
);
#2435=(
BOUNDED_SURFACE()
B_SPLINE_SURFACE(1,2,((#135458,#135459,#135460,#135461,#135462,#135463,
#135464),(#135465,#135466,#135467,#135468,#135469,#135470,#135471)),
 .UNSPECIFIED.,.F.,.F.,.F.)
B_SPLINE_SURFACE_WITH_KNOTS((2,2),(3,2,2,3),(0.71031891564008,1.),(0.2113983000937,
0.214285714285714,0.228883374894809,0.22905822564282),.UNSPECIFIED.)
GEOMETRIC_REPRESENTATION_ITEM()
RATIONAL_B_SPLINE_SURFACE(((0.998054921708738,0.998986490969345,1.,0.994876086397764,
0.991846493044689,0.991846493044689,0.991846493044689),(0.998054921708738,
0.998986490969345,1.,0.994876086397764,0.991846493044689,0.991846493044689,
0.991846493044689)))
REPRESENTATION_ITEM('')
SURFACE()
);
#2436=(
BOUNDED_SURFACE()
B_SPLINE_SURFACE(1,2,((#135482,#135483,#135484,#135485,#135486),(#135487,
#135488,#135489,#135490,#135491)),.UNSPECIFIED.,.F.,.F.,.F.)
B_SPLINE_SURFACE_WITH_KNOTS((2,2),(3,2,3),(0.710192959007032,1.),(0.504546746573288,
0.504719756176206,0.522020716468041),.UNSPECIFIED.)
GEOMETRIC_REPRESENTATION_ITEM()
RATIONAL_B_SPLINE_SURFACE(((0.996905579294159,0.996905579294159,0.996905579294159,
0.991635321911186,0.989306890555885),(0.996905579294158,0.996905579294158,
0.996905579294158,0.991635321911186,0.989306890555885)))
REPRESENTATION_ITEM('')
SURFACE()
);
#2437=(
BOUNDED_SURFACE()
B_SPLINE_SURFACE(1,2,((#135504,#135505,#135506,#135507,#135508,#135509,
#135510),(#135511,#135512,#135513,#135514,#135515,#135516,#135517)),
 .UNSPECIFIED.,.F.,.F.,.F.)
B_SPLINE_SURFACE_WITH_KNOTS((2,2),(3,2,2,3),(0.710318915640082,1.),(0.2113983000937,
0.214285714285714,0.228883374894809,0.22905822564282),.UNSPECIFIED.)
GEOMETRIC_REPRESENTATION_ITEM()
RATIONAL_B_SPLINE_SURFACE(((0.998054921708738,0.998986490969345,1.,0.994876086397764,
0.991846493044689,0.991846493044689,0.991846493044689),(0.998054921708738,
0.998986490969345,1.,0.994876086397764,0.991846493044689,0.991846493044689,
0.991846493044689)))
REPRESENTATION_ITEM('')
SURFACE()
);
#2438=(
BOUNDED_SURFACE()
B_SPLINE_SURFACE(1,2,((#135528,#135529,#135530,#135531,#135532),(#135533,
#135534,#135535,#135536,#135537)),.UNSPECIFIED.,.F.,.F.,.F.)
B_SPLINE_SURFACE_WITH_KNOTS((2,2),(3,2,3),(0.710192959007032,1.),(0.504546746573288,
0.504719756176206,0.522020716468041),.UNSPECIFIED.)
GEOMETRIC_REPRESENTATION_ITEM()
RATIONAL_B_SPLINE_SURFACE(((0.996905579294159,0.996905579294159,0.996905579294159,
0.991635321911186,0.989306890555885),(0.996905579294158,0.996905579294158,
0.996905579294158,0.991635321911186,0.989306890555885)))
REPRESENTATION_ITEM('')
SURFACE()
);
#2439=(
BOUNDED_SURFACE()
B_SPLINE_SURFACE(1,2,((#135550,#135551,#135552,#135553,#135554,#135555,
#135556),(#135557,#135558,#135559,#135560,#135561,#135562,#135563)),
 .UNSPECIFIED.,.F.,.F.,.F.)
B_SPLINE_SURFACE_WITH_KNOTS((2,2),(3,2,2,3),(0.710318915639715,1.),(0.2113983000937,
0.214285714285714,0.228883374894809,0.22905822564282),.UNSPECIFIED.)
GEOMETRIC_REPRESENTATION_ITEM()
RATIONAL_B_SPLINE_SURFACE(((0.998054921708738,0.998986490969345,1.,0.994876086397764,
0.991846493044689,0.991846493044689,0.991846493044689),(0.998054921708738,
0.998986490969345,1.,0.994876086397764,0.991846493044689,0.991846493044689,
0.991846493044689)))
REPRESENTATION_ITEM('')
SURFACE()
);
#2440=(
BOUNDED_SURFACE()
B_SPLINE_SURFACE(1,2,((#135574,#135575,#135576,#135577,#135578),(#135579,
#135580,#135581,#135582,#135583)),.UNSPECIFIED.,.F.,.F.,.F.)
B_SPLINE_SURFACE_WITH_KNOTS((2,2),(3,2,3),(0.710192959006589,1.),(0.504546746573288,
0.504719756176206,0.522020716468041),.UNSPECIFIED.)
GEOMETRIC_REPRESENTATION_ITEM()
RATIONAL_B_SPLINE_SURFACE(((0.996905579294158,0.996905579294158,0.996905579294158,
0.991635321911186,0.989306890555884),(0.996905579294158,0.996905579294158,
0.996905579294158,0.991635321911186,0.989306890555884)))
REPRESENTATION_ITEM('')
SURFACE()
);
#2441=(
BOUNDED_SURFACE()
B_SPLINE_SURFACE(1,2,((#135596,#135597,#135598,#135599,#135600,#135601,
#135602),(#135603,#135604,#135605,#135606,#135607,#135608,#135609)),
 .UNSPECIFIED.,.F.,.F.,.F.)
B_SPLINE_SURFACE_WITH_KNOTS((2,2),(3,2,2,3),(0.710318915638234,1.),(0.211398300093588,
0.214285714285714,0.228883374913777,0.229058225661979),.UNSPECIFIED.)
GEOMETRIC_REPRESENTATION_ITEM()
RATIONAL_B_SPLINE_SURFACE(((0.998054921708666,0.998986490969306,1.,0.994876086391106,
0.991846493036816,0.991846493036816,0.991846493036816),(0.998054921708666,
0.998986490969306,1.,0.994876086391106,0.991846493036816,0.991846493036816,
0.991846493036816)))
REPRESENTATION_ITEM('')
SURFACE()
);
#2442=(
BOUNDED_SURFACE()
B_SPLINE_SURFACE(1,2,((#135620,#135621,#135622,#135623,#135624),(#135625,
#135626,#135627,#135628,#135629)),.UNSPECIFIED.,.F.,.F.,.F.)
B_SPLINE_SURFACE_WITH_KNOTS((2,2),(3,2,3),(0.710192959006379,1.),(0.504546746573287,
0.504719756176205,0.52202071646804),.UNSPECIFIED.)
GEOMETRIC_REPRESENTATION_ITEM()
RATIONAL_B_SPLINE_SURFACE(((0.996905579294159,0.996905579294159,0.996905579294159,
0.991635321911186,0.989306890555885),(0.996905579294159,0.996905579294159,
0.996905579294159,0.991635321911186,0.989306890555885)))
REPRESENTATION_ITEM('')
SURFACE()
);
#2443=(
BOUNDED_SURFACE()
B_SPLINE_SURFACE(1,2,((#135642,#135643,#135644,#135645,#135646,#135647,
#135648),(#135649,#135650,#135651,#135652,#135653,#135654,#135655)),
 .UNSPECIFIED.,.F.,.F.,.F.)
B_SPLINE_SURFACE_WITH_KNOTS((2,2),(3,2,2,3),(0.710318915639423,1.),(0.211398300093701,
0.214285714285714,0.228883374894811,0.229058225642822),.UNSPECIFIED.)
GEOMETRIC_REPRESENTATION_ITEM()
RATIONAL_B_SPLINE_SURFACE(((0.998054921708739,0.998986490969345,1.,0.994876086397763,
0.991846493044688,0.991846493044688,0.991846493044688),(0.998054921708739,
0.998986490969345,1.,0.994876086397763,0.991846493044688,0.991846493044688,
0.991846493044688)))
REPRESENTATION_ITEM('')
SURFACE()
);
#2444=(
BOUNDED_SURFACE()
B_SPLINE_SURFACE(1,2,((#135666,#135667,#135668,#135669,#135670),(#135671,
#135672,#135673,#135674,#135675)),.UNSPECIFIED.,.F.,.F.,.F.)
B_SPLINE_SURFACE_WITH_KNOTS((2,2),(3,2,3),(0.710192959006944,1.),(0.504546746573287,
0.504719756176205,0.52202071646804),.UNSPECIFIED.)
GEOMETRIC_REPRESENTATION_ITEM()
RATIONAL_B_SPLINE_SURFACE(((0.996905579294159,0.996905579294159,0.996905579294159,
0.991635321911186,0.989306890555885),(0.996905579294159,0.996905579294159,
0.996905579294159,0.991635321911186,0.989306890555885)))
REPRESENTATION_ITEM('')
SURFACE()
);
#2445=(
BOUNDED_SURFACE()
B_SPLINE_SURFACE(1,2,((#135688,#135689,#135690,#135691,#135692,#135693,
#135694),(#135695,#135696,#135697,#135698,#135699,#135700,#135701)),
 .UNSPECIFIED.,.F.,.F.,.F.)
B_SPLINE_SURFACE_WITH_KNOTS((2,2),(3,2,2,3),(0.710318915639994,1.),(0.211398300093701,
0.214285714285714,0.22888337489481,0.229058225642821),.UNSPECIFIED.)
GEOMETRIC_REPRESENTATION_ITEM()
RATIONAL_B_SPLINE_SURFACE(((0.998054921708739,0.998986490969345,1.,0.994876086397763,
0.991846493044689,0.991846493044689,0.991846493044689),(0.998054921708739,
0.998986490969345,1.,0.994876086397763,0.991846493044689,0.991846493044689,
0.991846493044689)))
REPRESENTATION_ITEM('')
SURFACE()
);
#2446=(
BOUNDED_SURFACE()
B_SPLINE_SURFACE(1,2,((#135712,#135713,#135714,#135715,#135716),(#135717,
#135718,#135719,#135720,#135721)),.UNSPECIFIED.,.F.,.F.,.F.)
B_SPLINE_SURFACE_WITH_KNOTS((2,2),(3,2,3),(0.710192959006949,1.),(0.504546746573287,
0.504719756176205,0.52202071646804),.UNSPECIFIED.)
GEOMETRIC_REPRESENTATION_ITEM()
RATIONAL_B_SPLINE_SURFACE(((0.996905579294159,0.996905579294159,0.996905579294159,
0.991635321911186,0.989306890555885),(0.996905579294159,0.996905579294159,
0.996905579294159,0.991635321911186,0.989306890555885)))
REPRESENTATION_ITEM('')
SURFACE()
);
#2447=(
BOUNDED_SURFACE()
B_SPLINE_SURFACE(1,2,((#135734,#135735,#135736,#135737,#135738,#135739,
#135740),(#135741,#135742,#135743,#135744,#135745,#135746,#135747)),
 .UNSPECIFIED.,.F.,.F.,.F.)
B_SPLINE_SURFACE_WITH_KNOTS((2,2),(3,2,2,3),(0.710318915640003,1.),(0.211398300093701,
0.214285714285714,0.228883374894811,0.229058225642822),.UNSPECIFIED.)
GEOMETRIC_REPRESENTATION_ITEM()
RATIONAL_B_SPLINE_SURFACE(((0.998054921708739,0.998986490969345,1.,0.994876086397763,
0.991846493044688,0.991846493044688,0.991846493044688),(0.998054921708739,
0.998986490969345,1.,0.994876086397763,0.991846493044688,0.991846493044688,
0.991846493044688)))
REPRESENTATION_ITEM('')
SURFACE()
);
#2448=(
BOUNDED_SURFACE()
B_SPLINE_SURFACE(1,2,((#135758,#135759,#135760,#135761,#135762),(#135763,
#135764,#135765,#135766,#135767)),.UNSPECIFIED.,.F.,.F.,.F.)
B_SPLINE_SURFACE_WITH_KNOTS((2,2),(3,2,3),(0.710192959006957,1.),(0.504546746573287,
0.504719756176205,0.52202071646804),.UNSPECIFIED.)
GEOMETRIC_REPRESENTATION_ITEM()
RATIONAL_B_SPLINE_SURFACE(((0.996905579294159,0.996905579294159,0.996905579294159,
0.991635321911186,0.989306890555885),(0.996905579294159,0.996905579294159,
0.996905579294159,0.991635321911186,0.989306890555885)))
REPRESENTATION_ITEM('')
SURFACE()
);
#2449=(
BOUNDED_SURFACE()
B_SPLINE_SURFACE(1,2,((#135780,#135781,#135782,#135783,#135784,#135785,
#135786),(#135787,#135788,#135789,#135790,#135791,#135792,#135793)),
 .UNSPECIFIED.,.F.,.F.,.F.)
B_SPLINE_SURFACE_WITH_KNOTS((2,2),(3,2,2,3),(0.710318915640001,1.),(0.211398300093701,
0.214285714285714,0.22888337489481,0.229058225642821),.UNSPECIFIED.)
GEOMETRIC_REPRESENTATION_ITEM()
RATIONAL_B_SPLINE_SURFACE(((0.998054921708739,0.998986490969345,1.,0.994876086397763,
0.991846493044689,0.991846493044689,0.991846493044689),(0.998054921708739,
0.998986490969345,1.,0.994876086397763,0.991846493044689,0.991846493044689,
0.991846493044689)))
REPRESENTATION_ITEM('')
SURFACE()
);
#2450=(
BOUNDED_SURFACE()
B_SPLINE_SURFACE(1,2,((#135804,#135805,#135806,#135807,#135808),(#135809,
#135810,#135811,#135812,#135813)),.UNSPECIFIED.,.F.,.F.,.F.)
B_SPLINE_SURFACE_WITH_KNOTS((2,2),(3,2,3),(0.710192959006349,1.),(0.504546746573239,
0.504719756176158,0.52202071646804),.UNSPECIFIED.)
GEOMETRIC_REPRESENTATION_ITEM()
RATIONAL_B_SPLINE_SURFACE(((0.996905579294188,0.996905579294188,0.996905579294188,
0.991635321911192,0.989306890555885),(0.996905579294188,0.996905579294188,
0.996905579294188,0.991635321911192,0.989306890555885)))
REPRESENTATION_ITEM('')
SURFACE()
);
#2451=(
BOUNDED_SURFACE()
B_SPLINE_SURFACE(1,2,((#135826,#135827,#135828,#135829,#135830,#135831,
#135832),(#135833,#135834,#135835,#135836,#135837,#135838,#135839)),
 .UNSPECIFIED.,.F.,.F.,.F.)
B_SPLINE_SURFACE_WITH_KNOTS((2,2),(3,2,2,3),(0.710318915639035,1.),(0.211398300093701,
0.214285714285714,0.22888337489481,0.229058225642821),.UNSPECIFIED.)
GEOMETRIC_REPRESENTATION_ITEM()
RATIONAL_B_SPLINE_SURFACE(((0.998054921708739,0.998986490969345,1.,0.994876086397763,
0.991846493044688,0.991846493044688,0.991846493044688),(0.998054921708739,
0.998986490969345,1.,0.994876086397763,0.991846493044688,0.991846493044688,
0.991846493044688)))
REPRESENTATION_ITEM('')
SURFACE()
);
#2452=(
BOUNDED_SURFACE()
B_SPLINE_SURFACE(1,2,((#135850,#135851,#135852,#135853,#135854),(#135855,
#135856,#135857,#135858,#135859)),.UNSPECIFIED.,.F.,.F.,.F.)
B_SPLINE_SURFACE_WITH_KNOTS((2,2),(3,2,3),(0.710192959006982,1.),(0.504546746573089,
0.504719756176009,0.522020716468041),.UNSPECIFIED.)
GEOMETRIC_REPRESENTATION_ITEM()
RATIONAL_B_SPLINE_SURFACE(((0.996905579294279,0.996905579294279,0.996905579294279,
0.991635321911212,0.989306890555884),(0.996905579294279,0.996905579294279,
0.996905579294279,0.991635321911212,0.989306890555884)))
REPRESENTATION_ITEM('')
SURFACE()
);
#2453=(
BOUNDED_SURFACE()
B_SPLINE_SURFACE(1,2,((#135872,#135873,#135874,#135875,#135876,#135877,
#135878),(#135879,#135880,#135881,#135882,#135883,#135884,#135885)),
 .UNSPECIFIED.,.F.,.F.,.F.)
B_SPLINE_SURFACE_WITH_KNOTS((2,2),(3,2,2,3),(0.710318915640038,1.),(0.211398300093701,
0.214285714285714,0.22888337489481,0.229058225642821),.UNSPECIFIED.)
GEOMETRIC_REPRESENTATION_ITEM()
RATIONAL_B_SPLINE_SURFACE(((0.998054921708739,0.998986490969345,1.,0.994876086397764,
0.991846493044689,0.991846493044689,0.991846493044689),(0.998054921708739,
0.998986490969345,1.,0.994876086397764,0.991846493044689,0.991846493044689,
0.991846493044689)))
REPRESENTATION_ITEM('')
SURFACE()
);
#2454=(
BOUNDED_SURFACE()
B_SPLINE_SURFACE(1,2,((#135896,#135897,#135898,#135899,#135900),(#135901,
#135902,#135903,#135904,#135905)),.UNSPECIFIED.,.F.,.F.,.F.)
B_SPLINE_SURFACE_WITH_KNOTS((2,2),(3,2,3),(0.710192959006966,1.),(0.504546746572885,
0.504719756175807,0.522020716468042),.UNSPECIFIED.)
GEOMETRIC_REPRESENTATION_ITEM()
RATIONAL_B_SPLINE_SURFACE(((0.996905579294401,0.996905579294401,0.996905579294401,
0.991635321911239,0.989306890555884),(0.996905579294401,0.996905579294401,
0.996905579294401,0.991635321911239,0.989306890555884)))
REPRESENTATION_ITEM('')
SURFACE()
);
#2455=(
BOUNDED_SURFACE()
B_SPLINE_SURFACE(1,2,((#135918,#135919,#135920,#135921,#135922,#135923,
#135924),(#135925,#135926,#135927,#135928,#135929,#135930,#135931)),
 .UNSPECIFIED.,.F.,.F.,.F.)
B_SPLINE_SURFACE_WITH_KNOTS((2,2),(3,2,2,3),(0.710318915640017,1.),(0.211398300093701,
0.214285714285714,0.22888337489481,0.229058225642821),.UNSPECIFIED.)
GEOMETRIC_REPRESENTATION_ITEM()
RATIONAL_B_SPLINE_SURFACE(((0.998054921708739,0.998986490969345,1.,0.994876086397764,
0.991846493044689,0.991846493044689,0.991846493044689),(0.998054921708739,
0.998986490969345,1.,0.994876086397764,0.991846493044689,0.991846493044689,
0.991846493044689)))
REPRESENTATION_ITEM('')
SURFACE()
);
#2456=(
BOUNDED_SURFACE()
B_SPLINE_SURFACE(1,2,((#135946,#135947,#135948,#135949,#135950),(#135951,
#135952,#135953,#135954,#135955)),.UNSPECIFIED.,.F.,.F.,.F.)
B_SPLINE_SURFACE_WITH_KNOTS((2,2),(3,2,3),(0.,0.290270016613605),(0.159799014184082,
0.176967058622922,0.177555991080089),.UNSPECIFIED.)
GEOMETRIC_REPRESENTATION_ITEM()
RATIONAL_B_SPLINE_SURFACE(((0.990927469170791,0.98775996257079,0.98748925405691,
0.98748925405691,0.98748925405691),(0.990927469170791,0.98775996257079,
0.98748925405691,0.98748925405691,0.98748925405691)))
REPRESENTATION_ITEM('')
SURFACE()
);
#2457=(
BOUNDED_SURFACE()
B_SPLINE_SURFACE(1,2,((#135968,#135969,#135970,#135971,#135972,#135973,
#135974),(#135975,#135976,#135977,#135978,#135979,#135980,#135981)),
 .UNSPECIFIED.,.F.,.F.,.F.)
B_SPLINE_SURFACE_WITH_KNOTS((2,2),(3,2,2,3),(0.,0.28980704099156),(0.556037361265318,
0.55621282302886,0.571428571428571,0.573758999383056),.UNSPECIFIED.)
GEOMETRIC_REPRESENTATION_ITEM()
RATIONAL_B_SPLINE_SURFACE(((0.991593692313265,0.991593692313265,0.991593692313265,
0.994659131878644,1.,0.999181998279397,0.998417372792936),(0.991593692313265,
0.991593692313265,0.991593692313265,0.994659131878644,1.,0.999181998279397,
0.998417372792936)))
REPRESENTATION_ITEM('')
SURFACE()
);
#2458=(
BOUNDED_SURFACE()
B_SPLINE_SURFACE(1,2,((#135996,#135997,#135998,#135999,#136000),(#136001,
#136002,#136003,#136004,#136005)),.UNSPECIFIED.,.F.,.F.,.F.)
B_SPLINE_SURFACE_WITH_KNOTS((2,2),(3,2,3),(0.,0.290270016636536),(0.159799014184195,
0.176967058622922,0.177555991102387),.UNSPECIFIED.)
GEOMETRIC_REPRESENTATION_ITEM()
RATIONAL_B_SPLINE_SURFACE(((0.990927469170749,0.987759962570789,0.987489254056911,
0.987489254056911,0.987489254056911),(0.990927469170749,0.987759962570789,
0.987489254056911,0.987489254056911,0.987489254056911)))
REPRESENTATION_ITEM('')
SURFACE()
);
#2459=(
BOUNDED_SURFACE()
B_SPLINE_SURFACE(1,2,((#136018,#136019,#136020,#136021,#136022,#136023,
#136024),(#136025,#136026,#136027,#136028,#136029,#136030,#136031)),
 .UNSPECIFIED.,.F.,.F.,.F.)
B_SPLINE_SURFACE_WITH_KNOTS((2,2),(3,2,2,3),(0.,0.289807040991559),(0.556037361265318,
0.55621282302886,0.571428571428571,0.573758999383056),.UNSPECIFIED.)
GEOMETRIC_REPRESENTATION_ITEM()
RATIONAL_B_SPLINE_SURFACE(((0.991593692313265,0.991593692313265,0.991593692313265,
0.994659131878644,1.,0.999181998279397,0.998417372792936),(0.991593692313265,
0.991593692313265,0.991593692313265,0.994659131878644,1.,0.999181998279397,
0.998417372792936)))
REPRESENTATION_ITEM('')
SURFACE()
);
#2460=(
BOUNDED_SURFACE()
B_SPLINE_SURFACE(1,2,((#136042,#136043,#136044,#136045,#136046),(#136047,
#136048,#136049,#136050,#136051)),.UNSPECIFIED.,.F.,.F.,.F.)
B_SPLINE_SURFACE_WITH_KNOTS((2,2),(3,2,3),(0.,0.290270016612959),(0.15979901418427,
0.176967058622922,0.177555991079012),.UNSPECIFIED.)
GEOMETRIC_REPRESENTATION_ITEM()
RATIONAL_B_SPLINE_SURFACE(((0.990927469170721,0.987759962570787,0.98748925405691,
0.98748925405691,0.98748925405691),(0.990927469170722,0.987759962570787,
0.98748925405691,0.98748925405691,0.98748925405691)))
REPRESENTATION_ITEM('')
SURFACE()
);
#2461=(
BOUNDED_SURFACE()
B_SPLINE_SURFACE(1,2,((#136064,#136065,#136066,#136067,#136068,#136069,
#136070),(#136071,#136072,#136073,#136074,#136075,#136076,#136077)),
 .UNSPECIFIED.,.F.,.F.,.F.)
B_SPLINE_SURFACE_WITH_KNOTS((2,2),(3,2,2,3),(0.,0.289807040992493),(0.556037361265318,
0.55621282302886,0.571428571428571,0.573758999383056),.UNSPECIFIED.)
GEOMETRIC_REPRESENTATION_ITEM()
RATIONAL_B_SPLINE_SURFACE(((0.991593692313265,0.991593692313265,0.991593692313265,
0.994659131878644,1.,0.999181998279397,0.998417372792936),(0.991593692313265,
0.991593692313265,0.991593692313265,0.994659131878644,1.,0.999181998279397,
0.998417372792936)))
REPRESENTATION_ITEM('')
SURFACE()
);
#2462=(
BOUNDED_SURFACE()
B_SPLINE_SURFACE(1,2,((#136092,#136093,#136094,#136095,#136096),(#136097,
#136098,#136099,#136100,#136101)),.UNSPECIFIED.,.F.,.F.,.F.)
B_SPLINE_SURFACE_WITH_KNOTS((2,2),(3,2,3),(0.,0.290270016625899),(0.159799014184081,
0.176967058622922,0.177555991091513),.UNSPECIFIED.)
GEOMETRIC_REPRESENTATION_ITEM()
RATIONAL_B_SPLINE_SURFACE(((0.990927469170791,0.98775996257079,0.98748925405691,
0.98748925405691,0.98748925405691),(0.990927469170791,0.98775996257079,
0.98748925405691,0.98748925405691,0.98748925405691)))
REPRESENTATION_ITEM('')
SURFACE()
);
#2463=(
BOUNDED_SURFACE()
B_SPLINE_SURFACE(1,2,((#136117,#136118,#136119,#136120,#136121,#136122,
#136123),(#136124,#136125,#136126,#136127,#136128,#136129,#136130)),
 .UNSPECIFIED.,.F.,.F.,.F.)
B_SPLINE_SURFACE_WITH_KNOTS((2,2),(3,2,2,3),(0.,0.289807040992489),(0.556037361265319,
0.55621282302886,0.571428571428571,0.573758999382975),.UNSPECIFIED.)
GEOMETRIC_REPRESENTATION_ITEM()
RATIONAL_B_SPLINE_SURFACE(((0.991593692313265,0.991593692313265,0.991593692313265,
0.994659131878644,1.,0.999181998279426,0.99841737279299),(0.991593692313265,
0.991593692313265,0.991593692313265,0.994659131878644,1.,0.999181998279426,
0.99841737279299)))
REPRESENTATION_ITEM('')
SURFACE()
);
#2464=(
BOUNDED_SURFACE()
B_SPLINE_SURFACE(1,2,((#136141,#136142,#136143,#136144,#136145),(#136146,
#136147,#136148,#136149,#136150)),.UNSPECIFIED.,.F.,.F.,.F.)
B_SPLINE_SURFACE_WITH_KNOTS((2,2),(3,2,3),(0.,0.290270016605119),(0.159799014184081,
0.176967058622922,0.177555991071273),.UNSPECIFIED.)
GEOMETRIC_REPRESENTATION_ITEM()
RATIONAL_B_SPLINE_SURFACE(((0.990927469170791,0.98775996257079,0.98748925405691,
0.98748925405691,0.98748925405691),(0.990927469170791,0.98775996257079,
0.98748925405691,0.98748925405691,0.98748925405691)))
REPRESENTATION_ITEM('')
SURFACE()
);
#2465=(
BOUNDED_SURFACE()
B_SPLINE_SURFACE(1,2,((#136163,#136164,#136165,#136166,#136167,#136168,
#136169),(#136170,#136171,#136172,#136173,#136174,#136175,#136176)),
 .UNSPECIFIED.,.F.,.F.,.F.)
B_SPLINE_SURFACE_WITH_KNOTS((2,2),(3,2,2,3),(0.,0.289807040992493),(0.556037361265319,
0.55621282302886,0.571428571428571,0.573758999382975),.UNSPECIFIED.)
GEOMETRIC_REPRESENTATION_ITEM()
RATIONAL_B_SPLINE_SURFACE(((0.991593692313265,0.991593692313265,0.991593692313265,
0.994659131878644,1.,0.999181998279426,0.99841737279299),(0.991593692313265,
0.991593692313265,0.991593692313265,0.994659131878644,1.,0.999181998279426,
0.99841737279299)))
REPRESENTATION_ITEM('')
SURFACE()
);
#2466=(
BOUNDED_SURFACE()
B_SPLINE_SURFACE(1,2,((#136191,#136192,#136193,#136194,#136195),(#136196,
#136197,#136198,#136199,#136200)),.UNSPECIFIED.,.F.,.F.,.F.)
B_SPLINE_SURFACE_WITH_KNOTS((2,2),(3,2,3),(0.,0.290270016611538),(0.15979901418427,
0.176967058622922,0.177555991077158),.UNSPECIFIED.)
GEOMETRIC_REPRESENTATION_ITEM()
RATIONAL_B_SPLINE_SURFACE(((0.990927469170722,0.987759962570787,0.98748925405691,
0.98748925405691,0.98748925405691),(0.990927469170722,0.987759962570787,
0.98748925405691,0.98748925405691,0.98748925405691)))
REPRESENTATION_ITEM('')
SURFACE()
);
#2467=(
BOUNDED_SURFACE()
B_SPLINE_SURFACE(1,2,((#136213,#136214,#136215,#136216,#136217,#136218,
#136219),(#136220,#136221,#136222,#136223,#136224,#136225,#136226)),
 .UNSPECIFIED.,.F.,.F.,.F.)
B_SPLINE_SURFACE_WITH_KNOTS((2,2),(3,2,2,3),(0.,0.289807040993075),(0.556037361265318,
0.55621282302886,0.571428571428571,0.573758999383056),.UNSPECIFIED.)
GEOMETRIC_REPRESENTATION_ITEM()
RATIONAL_B_SPLINE_SURFACE(((0.991593692313265,0.991593692313265,0.991593692313265,
0.994659131878644,1.,0.999181998279397,0.998417372792936),(0.991593692313265,
0.991593692313265,0.991593692313265,0.994659131878644,1.,0.999181998279397,
0.998417372792936)))
REPRESENTATION_ITEM('')
SURFACE()
);
#2468=(
BOUNDED_SURFACE()
B_SPLINE_SURFACE(1,2,((#136237,#136238,#136239,#136240,#136241),(#136242,
#136243,#136244,#136245,#136246)),.UNSPECIFIED.,.F.,.F.,.F.)
B_SPLINE_SURFACE_WITH_KNOTS((2,2),(3,2,3),(0.,0.29027001661619),(0.159799014184193,
0.176967058622922,0.177555991082371),.UNSPECIFIED.)
GEOMETRIC_REPRESENTATION_ITEM()
RATIONAL_B_SPLINE_SURFACE(((0.99092746917075,0.987759962570788,0.98748925405691,
0.98748925405691,0.98748925405691),(0.99092746917075,0.987759962570788,
0.98748925405691,0.98748925405691,0.98748925405691)))
REPRESENTATION_ITEM('')
SURFACE()
);
#2469=(
BOUNDED_SURFACE()
B_SPLINE_SURFACE(1,2,((#136259,#136260,#136261,#136262,#136263,#136264,
#136265),(#136266,#136267,#136268,#136269,#136270,#136271,#136272)),
 .UNSPECIFIED.,.F.,.F.,.F.)
B_SPLINE_SURFACE_WITH_KNOTS((2,2),(3,2,2,3),(0.,0.289807040992488),(0.556037361265318,
0.55621282302886,0.571428571428571,0.573758999383057),.UNSPECIFIED.)
GEOMETRIC_REPRESENTATION_ITEM()
RATIONAL_B_SPLINE_SURFACE(((0.991593692313265,0.991593692313265,0.991593692313265,
0.994659131878644,1.,0.999181998279397,0.998417372792936),(0.991593692313265,
0.991593692313265,0.991593692313265,0.994659131878644,1.,0.999181998279397,
0.998417372792936)))
REPRESENTATION_ITEM('')
SURFACE()
);
#2470=(
BOUNDED_SURFACE()
B_SPLINE_SURFACE(1,2,((#136287,#136288,#136289,#136290,#136291),(#136292,
#136293,#136294,#136295,#136296)),.UNSPECIFIED.,.F.,.F.,.F.)
B_SPLINE_SURFACE_WITH_KNOTS((2,2),(3,2,3),(0.,0.290270016643447),(0.159799014184081,
0.176967058622922,0.177555991109407),.UNSPECIFIED.)
GEOMETRIC_REPRESENTATION_ITEM()
RATIONAL_B_SPLINE_SURFACE(((0.990927469170791,0.98775996257079,0.98748925405691,
0.98748925405691,0.98748925405691),(0.990927469170791,0.98775996257079,
0.98748925405691,0.98748925405691,0.98748925405691)))
REPRESENTATION_ITEM('')
SURFACE()
);
#2471=(
BOUNDED_SURFACE()
B_SPLINE_SURFACE(1,2,((#136309,#136310,#136311,#136312,#136313,#136314,
#136315),(#136316,#136317,#136318,#136319,#136320,#136321,#136322)),
 .UNSPECIFIED.,.F.,.F.,.F.)
B_SPLINE_SURFACE_WITH_KNOTS((2,2),(3,2,2,3),(0.,0.289807040993064),(0.556037361265318,
0.55621282302886,0.571428571428571,0.573758999383056),.UNSPECIFIED.)
GEOMETRIC_REPRESENTATION_ITEM()
RATIONAL_B_SPLINE_SURFACE(((0.991593692313265,0.991593692313265,0.991593692313265,
0.994659131878644,1.,0.999181998279397,0.998417372792936),(0.991593692313265,
0.991593692313265,0.991593692313265,0.994659131878644,1.,0.999181998279397,
0.998417372792936)))
REPRESENTATION_ITEM('')
SURFACE()
);
#2472=(
BOUNDED_SURFACE()
B_SPLINE_SURFACE(1,2,((#136333,#136334,#136335,#136336,#136337),(#136338,
#136339,#136340,#136341,#136342)),.UNSPECIFIED.,.F.,.F.,.F.)
B_SPLINE_SURFACE_WITH_KNOTS((2,2),(3,2,3),(0.,0.290270016648069),(0.159799014184083,
0.176967058622922,0.177555991114313),.UNSPECIFIED.)
GEOMETRIC_REPRESENTATION_ITEM()
RATIONAL_B_SPLINE_SURFACE(((0.99092746917079,0.98775996257079,0.98748925405691,
0.98748925405691,0.98748925405691),(0.99092746917079,0.98775996257079,0.98748925405691,
0.98748925405691,0.98748925405691)))
REPRESENTATION_ITEM('')
SURFACE()
);
#2473=(
BOUNDED_SURFACE()
B_SPLINE_SURFACE(1,2,((#136355,#136356,#136357,#136358,#136359,#136360,
#136361),(#136362,#136363,#136364,#136365,#136366,#136367,#136368)),
 .UNSPECIFIED.,.F.,.F.,.F.)
B_SPLINE_SURFACE_WITH_KNOTS((2,2),(3,2,2,3),(0.,0.289807040992575),(0.556037361265319,
0.556212823028861,0.571428571428571,0.573758999383056),.UNSPECIFIED.)
GEOMETRIC_REPRESENTATION_ITEM()
RATIONAL_B_SPLINE_SURFACE(((0.991593692313265,0.991593692313265,0.991593692313265,
0.994659131878645,1.,0.999181998279397,0.998417372792936),(0.991593692313265,
0.991593692313265,0.991593692313265,0.994659131878645,1.,0.999181998279397,
0.998417372792936)))
REPRESENTATION_ITEM('')
SURFACE()
);
#2474=(
BOUNDED_SURFACE()
B_SPLINE_SURFACE(1,2,((#136379,#136380,#136381,#136382,#136383),(#136384,
#136385,#136386,#136387,#136388)),.UNSPECIFIED.,.F.,.F.,.F.)
B_SPLINE_SURFACE_WITH_KNOTS((2,2),(3,2,3),(0.,0.290270016630719),(0.159799014184082,
0.176967058622921,0.177555991097006),.UNSPECIFIED.)
GEOMETRIC_REPRESENTATION_ITEM()
RATIONAL_B_SPLINE_SURFACE(((0.990927469170791,0.98775996257079,0.98748925405691,
0.98748925405691,0.98748925405691),(0.990927469170791,0.98775996257079,
0.98748925405691,0.98748925405691,0.98748925405691)))
REPRESENTATION_ITEM('')
SURFACE()
);
#2475=(
BOUNDED_SURFACE()
B_SPLINE_SURFACE(1,2,((#136401,#136402,#136403,#136404,#136405,#136406,
#136407),(#136408,#136409,#136410,#136411,#136412,#136413,#136414)),
 .UNSPECIFIED.,.F.,.F.,.F.)
B_SPLINE_SURFACE_WITH_KNOTS((2,2),(3,2,2,3),(0.,0.28980704099257),(0.55603736126532,
0.556212823028861,0.571428571428571,0.573758999382978),.UNSPECIFIED.)
GEOMETRIC_REPRESENTATION_ITEM()
RATIONAL_B_SPLINE_SURFACE(((0.991593692313265,0.991593692313265,0.991593692313265,
0.994659131878645,1.,0.999181998279424,0.998417372792988),(0.991593692313266,
0.991593692313266,0.991593692313266,0.994659131878645,1.,0.999181998279424,
0.998417372792988)))
REPRESENTATION_ITEM('')
SURFACE()
);
#2476=(
BOUNDED_SURFACE()
B_SPLINE_SURFACE(1,2,((#136429,#136430,#136431,#136432,#136433),(#136434,
#136435,#136436,#136437,#136438)),.UNSPECIFIED.,.F.,.F.,.F.)
B_SPLINE_SURFACE_WITH_KNOTS((2,2),(3,2,3),(0.,0.290270016637826),(0.15979901418408,
0.176967058622921,0.17755599110352),.UNSPECIFIED.)
GEOMETRIC_REPRESENTATION_ITEM()
RATIONAL_B_SPLINE_SURFACE(((0.990927469170791,0.98775996257079,0.98748925405691,
0.98748925405691,0.98748925405691),(0.990927469170791,0.98775996257079,
0.98748925405691,0.98748925405691,0.98748925405691)))
REPRESENTATION_ITEM('')
SURFACE()
);
#2477=(
BOUNDED_SURFACE()
B_SPLINE_SURFACE(1,2,((#136451,#136452,#136453,#136454,#136455,#136456,
#136457),(#136458,#136459,#136460,#136461,#136462,#136463,#136464)),
 .UNSPECIFIED.,.F.,.F.,.F.)
B_SPLINE_SURFACE_WITH_KNOTS((2,2),(3,2,2,3),(0.,0.28980704099316),(0.556037361265319,
0.556212823028861,0.571428571428571,0.573758999383057),.UNSPECIFIED.)
GEOMETRIC_REPRESENTATION_ITEM()
RATIONAL_B_SPLINE_SURFACE(((0.991593692313265,0.991593692313265,0.991593692313265,
0.994659131878645,1.,0.999181998279397,0.998417372792936),(0.991593692313265,
0.991593692313265,0.991593692313265,0.994659131878645,1.,0.999181998279397,
0.998417372792936)))
REPRESENTATION_ITEM('')
SURFACE()
);
#2478=(
BOUNDED_SURFACE()
B_SPLINE_SURFACE(1,2,((#136470,#136471,#136472,#136473,#136474),(#136475,
#136476,#136477,#136478,#136479)),.UNSPECIFIED.,.F.,.F.,.F.)
B_SPLINE_SURFACE_WITH_KNOTS((2,2),(3,2,3),(0.,0.290270016637931),(0.15979901418408,
0.176967058622921,0.177555991104342),.UNSPECIFIED.)
GEOMETRIC_REPRESENTATION_ITEM()
RATIONAL_B_SPLINE_SURFACE(((0.990927469170792,0.98775996257079,0.98748925405691,
0.98748925405691,0.98748925405691),(0.990927469170792,0.98775996257079,
0.98748925405691,0.98748925405691,0.98748925405691)))
REPRESENTATION_ITEM('')
SURFACE()
);
#2479=(
BOUNDED_SURFACE()
B_SPLINE_SURFACE(1,2,((#136492,#136493,#136494,#136495,#136496,#136497,
#136498),(#136499,#136500,#136501,#136502,#136503,#136504,#136505)),
 .UNSPECIFIED.,.F.,.F.,.F.)
B_SPLINE_SURFACE_WITH_KNOTS((2,2),(3,2,2,3),(0.,0.289807040992571),(0.556037361265319,
0.556212823028861,0.571428571428571,0.573758999383057),.UNSPECIFIED.)
GEOMETRIC_REPRESENTATION_ITEM()
RATIONAL_B_SPLINE_SURFACE(((0.991593692313266,0.991593692313266,0.991593692313266,
0.994659131878645,1.,0.999181998279397,0.998417372792936),(0.991593692313266,
0.991593692313266,0.991593692313266,0.994659131878645,1.,0.999181998279397,
0.998417372792936)))
REPRESENTATION_ITEM('')
SURFACE()
);
#2480=(
BOUNDED_SURFACE()
B_SPLINE_SURFACE(1,2,((#136511,#136512,#136513,#136514,#136515),(#136516,
#136517,#136518,#136519,#136520)),.UNSPECIFIED.,.F.,.F.,.F.)
B_SPLINE_SURFACE_WITH_KNOTS((2,2),(3,2,3),(0.,0.290270016625139),(0.159799014184192,
0.176967058622921,0.177555991091401),.UNSPECIFIED.)
GEOMETRIC_REPRESENTATION_ITEM()
RATIONAL_B_SPLINE_SURFACE(((0.99092746917075,0.987759962570789,0.98748925405691,
0.98748925405691,0.98748925405691),(0.99092746917075,0.987759962570789,
0.98748925405691,0.98748925405691,0.98748925405691)))
REPRESENTATION_ITEM('')
SURFACE()
);
#2481=(
BOUNDED_SURFACE()
B_SPLINE_SURFACE(1,2,((#136533,#136534,#136535,#136536,#136537,#136538,
#136539),(#136540,#136541,#136542,#136543,#136544,#136545,#136546)),
 .UNSPECIFIED.,.F.,.F.,.F.)
B_SPLINE_SURFACE_WITH_KNOTS((2,2),(3,2,2,3),(0.,0.289807040993071),(0.556037361265319,
0.556212823028861,0.571428571428571,0.573758999383058),.UNSPECIFIED.)
GEOMETRIC_REPRESENTATION_ITEM()
RATIONAL_B_SPLINE_SURFACE(((0.991593692313265,0.991593692313265,0.991593692313265,
0.994659131878645,1.,0.999181998279397,0.998417372792936),(0.991593692313265,
0.991593692313265,0.991593692313265,0.994659131878645,1.,0.999181998279397,
0.998417372792936)))
REPRESENTATION_ITEM('')
SURFACE()
);
#2482=(
BOUNDED_SURFACE()
B_SPLINE_SURFACE(1,2,((#136557,#136558,#136559,#136560,#136561),(#136562,
#136563,#136564,#136565,#136566)),.UNSPECIFIED.,.F.,.F.,.F.)
B_SPLINE_SURFACE_WITH_KNOTS((2,2),(3,2,3),(0.,0.29027001664356),(0.15979901418408,
0.176967058622921,0.177555991109305),.UNSPECIFIED.)
GEOMETRIC_REPRESENTATION_ITEM()
RATIONAL_B_SPLINE_SURFACE(((0.990927469170792,0.98775996257079,0.98748925405691,
0.98748925405691,0.98748925405691),(0.990927469170792,0.98775996257079,
0.98748925405691,0.98748925405691,0.98748925405691)))
REPRESENTATION_ITEM('')
SURFACE()
);
#2483=(
BOUNDED_SURFACE()
B_SPLINE_SURFACE(1,2,((#136579,#136580,#136581,#136582,#136583,#136584,
#136585),(#136586,#136587,#136588,#136589,#136590,#136591,#136592)),
 .UNSPECIFIED.,.F.,.F.,.F.)
B_SPLINE_SURFACE_WITH_KNOTS((2,2),(3,2,2,3),(0.,0.289807040992579),(0.556037361265319,
0.556212823028861,0.571428571428571,0.573758999383058),.UNSPECIFIED.)
GEOMETRIC_REPRESENTATION_ITEM()
RATIONAL_B_SPLINE_SURFACE(((0.991593692313266,0.991593692313266,0.991593692313266,
0.994659131878645,1.,0.999181998279397,0.998417372792936),(0.991593692313266,
0.991593692313266,0.991593692313266,0.994659131878645,1.,0.999181998279397,
0.998417372792936)))
REPRESENTATION_ITEM('')
SURFACE()
);
#2484=(
BOUNDED_SURFACE()
B_SPLINE_SURFACE(1,2,((#136607,#136608,#136609,#136610,#136611),(#136612,
#136613,#136614,#136615,#136616)),.UNSPECIFIED.,.F.,.F.,.F.)
B_SPLINE_SURFACE_WITH_KNOTS((2,2),(3,2,3),(0.,0.290270016658068),(0.15979901418408,
0.176967058622921,0.177555991124176),.UNSPECIFIED.)
GEOMETRIC_REPRESENTATION_ITEM()
RATIONAL_B_SPLINE_SURFACE(((0.990927469170792,0.98775996257079,0.98748925405691,
0.98748925405691,0.98748925405691),(0.990927469170792,0.98775996257079,
0.98748925405691,0.98748925405691,0.98748925405691)))
REPRESENTATION_ITEM('')
SURFACE()
);
#2485=(
BOUNDED_SURFACE()
B_SPLINE_SURFACE(1,2,((#136629,#136630,#136631,#136632,#136633,#136634,
#136635),(#136636,#136637,#136638,#136639,#136640,#136641,#136642)),
 .UNSPECIFIED.,.F.,.F.,.F.)
B_SPLINE_SURFACE_WITH_KNOTS((2,2),(3,2,2,3),(0.,0.289807040993077),(0.55603736126532,
0.556212823028861,0.571428571428571,0.573758999382976),.UNSPECIFIED.)
GEOMETRIC_REPRESENTATION_ITEM()
RATIONAL_B_SPLINE_SURFACE(((0.991593692313265,0.991593692313265,0.991593692313265,
0.994659131878645,1.,0.999181998279425,0.998417372792989),(0.991593692313265,
0.991593692313265,0.991593692313265,0.994659131878645,1.,0.999181998279425,
0.998417372792989)))
REPRESENTATION_ITEM('')
SURFACE()
);
#2486=(
BOUNDED_SURFACE()
B_SPLINE_SURFACE(1,2,((#136653,#136654,#136655,#136656,#136657),(#136658,
#136659,#136660,#136661,#136662)),.UNSPECIFIED.,.F.,.F.,.F.)
B_SPLINE_SURFACE_WITH_KNOTS((2,2),(3,2,3),(0.,0.29027001664428),(0.159799014184081,
0.176967058622921,0.177555991110565),.UNSPECIFIED.)
GEOMETRIC_REPRESENTATION_ITEM()
RATIONAL_B_SPLINE_SURFACE(((0.990927469170791,0.98775996257079,0.98748925405691,
0.98748925405691,0.98748925405691),(0.990927469170791,0.98775996257079,
0.98748925405691,0.98748925405691,0.98748925405691)))
REPRESENTATION_ITEM('')
SURFACE()
);
#2487=(
BOUNDED_SURFACE()
B_SPLINE_SURFACE(1,2,((#136678,#136679,#136680,#136681,#136682,#136683,
#136684),(#136685,#136686,#136687,#136688,#136689,#136690,#136691)),
 .UNSPECIFIED.,.F.,.F.,.F.)
B_SPLINE_SURFACE_WITH_KNOTS((2,2),(3,2,2,3),(0.,0.289807040992854),(0.556037361265321,
0.556212823028862,0.571428571428571,0.573758999382978),.UNSPECIFIED.)
GEOMETRIC_REPRESENTATION_ITEM()
RATIONAL_B_SPLINE_SURFACE(((0.991593692313266,0.991593692313266,0.991593692313266,
0.994659131878645,1.,0.999181998279425,0.998417372792988),(0.991593692313266,
0.991593692313266,0.991593692313266,0.994659131878645,1.,0.999181998279425,
0.998417372792988)))
REPRESENTATION_ITEM('')
SURFACE()
);
#2488=(
BOUNDED_SURFACE()
B_SPLINE_SURFACE(1,2,((#136697,#136698,#136699,#136700,#136701),(#136702,
#136703,#136704,#136705,#136706)),.UNSPECIFIED.,.F.,.F.,.F.)
B_SPLINE_SURFACE_WITH_KNOTS((2,2),(3,2,3),(0.,0.290270016616668),(0.159799014184082,
0.176967058622921,0.177555991082798),.UNSPECIFIED.)
GEOMETRIC_REPRESENTATION_ITEM()
RATIONAL_B_SPLINE_SURFACE(((0.990927469170791,0.98775996257079,0.98748925405691,
0.98748925405691,0.98748925405691),(0.990927469170791,0.98775996257079,
0.98748925405691,0.98748925405691,0.98748925405691)))
REPRESENTATION_ITEM('')
SURFACE()
);
#2489=(
BOUNDED_SURFACE()
B_SPLINE_SURFACE(1,2,((#136719,#136720,#136721,#136722,#136723,#136724,
#136725),(#136726,#136727,#136728,#136729,#136730,#136731,#136732)),
 .UNSPECIFIED.,.F.,.F.,.F.)
B_SPLINE_SURFACE_WITH_KNOTS((2,2),(3,2,2,3),(0.,0.289807040993902),(0.55603736126532,
0.556212823028861,0.571428571428571,0.573758999382978),.UNSPECIFIED.)
GEOMETRIC_REPRESENTATION_ITEM()
RATIONAL_B_SPLINE_SURFACE(((0.991593692313265,0.991593692313265,0.991593692313265,
0.994659131878645,1.,0.999181998279424,0.998417372792988),(0.991593692313266,
0.991593692313266,0.991593692313266,0.994659131878645,1.,0.999181998279424,
0.998417372792988)))
REPRESENTATION_ITEM('')
SURFACE()
);
#2490=(
BOUNDED_SURFACE()
B_SPLINE_SURFACE(1,2,((#136747,#136748,#136749,#136750,#136751),(#136752,
#136753,#136754,#136755,#136756)),.UNSPECIFIED.,.F.,.F.,.F.)
B_SPLINE_SURFACE_WITH_KNOTS((2,2),(3,2,3),(0.,0.290270016636515),(0.15979901418409,
0.176967058622921,0.177555991102485),.UNSPECIFIED.)
GEOMETRIC_REPRESENTATION_ITEM()
RATIONAL_B_SPLINE_SURFACE(((0.990927469170788,0.98775996257079,0.98748925405691,
0.98748925405691,0.98748925405691),(0.990927469170788,0.98775996257079,
0.98748925405691,0.98748925405691,0.98748925405691)))
REPRESENTATION_ITEM('')
SURFACE()
);
#2491=(
BOUNDED_SURFACE()
B_SPLINE_SURFACE(1,2,((#136769,#136770,#136771,#136772,#136773,#136774,
#136775),(#136776,#136777,#136778,#136779,#136780,#136781,#136782)),
 .UNSPECIFIED.,.F.,.F.,.F.)
B_SPLINE_SURFACE_WITH_KNOTS((2,2),(3,2,2,3),(0.,0.289807040992609),(0.556037361265319,
0.556212823028861,0.571428571428571,0.573758999383058),.UNSPECIFIED.)
GEOMETRIC_REPRESENTATION_ITEM()
RATIONAL_B_SPLINE_SURFACE(((0.991593692313265,0.991593692313265,0.991593692313265,
0.994659131878645,1.,0.999181998279397,0.998417372792936),(0.991593692313265,
0.991593692313265,0.991593692313265,0.994659131878645,1.,0.999181998279397,
0.998417372792936)))
REPRESENTATION_ITEM('')
SURFACE()
);
#2492=(
BOUNDED_SURFACE()
B_SPLINE_SURFACE(1,2,((#136788,#136789,#136790,#136791,#136792),(#136793,
#136794,#136795,#136796,#136797)),.UNSPECIFIED.,.F.,.F.,.F.)
B_SPLINE_SURFACE_WITH_KNOTS((2,2),(3,2,3),(0.,0.290270016618184),(0.15979901418402,
0.176967058622921,0.17755599108467),.UNSPECIFIED.)
GEOMETRIC_REPRESENTATION_ITEM()
RATIONAL_B_SPLINE_SURFACE(((0.990927469170814,0.987759962570791,0.98748925405691,
0.98748925405691,0.98748925405691),(0.990927469170814,0.987759962570791,
0.98748925405691,0.98748925405691,0.98748925405691)))
REPRESENTATION_ITEM('')
SURFACE()
);
#2493=(
BOUNDED_SURFACE()
B_SPLINE_SURFACE(1,2,((#136810,#136811,#136812,#136813,#136814,#136815,
#136816),(#136817,#136818,#136819,#136820,#136821,#136822,#136823)),
 .UNSPECIFIED.,.F.,.F.,.F.)
B_SPLINE_SURFACE_WITH_KNOTS((2,2),(3,2,2,3),(0.,0.289807040992497),(0.55603736126532,
0.556212823028861,0.571428571428571,0.573758999382969),.UNSPECIFIED.)
GEOMETRIC_REPRESENTATION_ITEM()
RATIONAL_B_SPLINE_SURFACE(((0.991593692313265,0.991593692313265,0.991593692313265,
0.994659131878645,1.,0.999181998279428,0.998417372792994),(0.991593692313265,
0.991593692313265,0.991593692313265,0.994659131878645,1.,0.999181998279428,
0.998417372792994)))
REPRESENTATION_ITEM('')
SURFACE()
);
#2494=(
BOUNDED_SURFACE()
B_SPLINE_SURFACE(1,2,((#136838,#136839,#136840,#136841,#136842),(#136843,
#136844,#136845,#136846,#136847)),.UNSPECIFIED.,.F.,.F.,.F.)
B_SPLINE_SURFACE_WITH_KNOTS((2,2),(3,2,3),(0.,0.2902700166395),(0.159799014184269,
0.176967058622921,0.177555991105355),.UNSPECIFIED.)
GEOMETRIC_REPRESENTATION_ITEM()
RATIONAL_B_SPLINE_SURFACE(((0.990927469170722,0.987759962570788,0.98748925405691,
0.98748925405691,0.98748925405691),(0.990927469170722,0.987759962570787,
0.98748925405691,0.98748925405691,0.98748925405691)))
REPRESENTATION_ITEM('')
SURFACE()
);
#2495=(
BOUNDED_SURFACE()
B_SPLINE_SURFACE(1,2,((#136863,#136864,#136865,#136866,#136867,#136868,
#136869),(#136870,#136871,#136872,#136873,#136874,#136875,#136876)),
 .UNSPECIFIED.,.F.,.F.,.F.)
B_SPLINE_SURFACE_WITH_KNOTS((2,2),(3,2,2,3),(0.,0.289807040993133),(0.55603736126532,
0.556212823028862,0.571428571428571,0.573758999383058),.UNSPECIFIED.)
GEOMETRIC_REPRESENTATION_ITEM()
RATIONAL_B_SPLINE_SURFACE(((0.991593692313266,0.991593692313266,0.991593692313266,
0.994659131878645,1.,0.999181998279396,0.998417372792935),(0.991593692313266,
0.991593692313266,0.991593692313266,0.994659131878645,1.,0.999181998279396,
0.998417372792935)))
REPRESENTATION_ITEM('')
SURFACE()
);
#2496=(
BOUNDED_SURFACE()
B_SPLINE_SURFACE(1,2,((#136887,#136888,#136889,#136890,#136891),(#136892,
#136893,#136894,#136895,#136896)),.UNSPECIFIED.,.F.,.F.,.F.)
B_SPLINE_SURFACE_WITH_KNOTS((2,2),(3,2,3),(0.,0.290270016635147),(0.159799014184073,
0.176967058622922,0.177555991100849),.UNSPECIFIED.)
GEOMETRIC_REPRESENTATION_ITEM()
RATIONAL_B_SPLINE_SURFACE(((0.990927469170794,0.98775996257079,0.98748925405691,
0.98748925405691,0.98748925405691),(0.990927469170794,0.98775996257079,
0.98748925405691,0.98748925405691,0.98748925405691)))
REPRESENTATION_ITEM('')
SURFACE()
);
#2497=(
BOUNDED_SURFACE()
B_SPLINE_SURFACE(1,2,((#136912,#136913,#136914,#136915,#136916,#136917,
#136918),(#136919,#136920,#136921,#136922,#136923,#136924,#136925)),
 .UNSPECIFIED.,.F.,.F.,.F.)
B_SPLINE_SURFACE_WITH_KNOTS((2,2),(3,2,2,3),(0.,0.289807040991732),(0.55603736126532,
0.556212823028861,0.571428571428571,0.573758999382983),.UNSPECIFIED.)
GEOMETRIC_REPRESENTATION_ITEM()
RATIONAL_B_SPLINE_SURFACE(((0.991593692313265,0.991593692313265,0.991593692313265,
0.994659131878645,1.,0.999181998279423,0.998417372792985),(0.991593692313265,
0.991593692313265,0.991593692313265,0.994659131878645,1.,0.999181998279423,
0.998417372792985)))
REPRESENTATION_ITEM('')
SURFACE()
);
#2498=(
BOUNDED_SURFACE()
B_SPLINE_SURFACE(1,2,((#136936,#136937,#136938,#136939,#136940),(#136941,
#136942,#136943,#136944,#136945)),.UNSPECIFIED.,.F.,.F.,.F.)
B_SPLINE_SURFACE_WITH_KNOTS((2,2),(3,2,3),(0.,0.290270016625215),(0.159799014184268,
0.176967058622921,0.177555991091437),.UNSPECIFIED.)
GEOMETRIC_REPRESENTATION_ITEM()
RATIONAL_B_SPLINE_SURFACE(((0.990927469170722,0.987759962570787,0.98748925405691,
0.98748925405691,0.98748925405691),(0.990927469170722,0.987759962570787,
0.98748925405691,0.98748925405691,0.98748925405691)))
REPRESENTATION_ITEM('')
SURFACE()
);
#2499=(
BOUNDED_SURFACE()
B_SPLINE_SURFACE(1,2,((#136958,#136959,#136960,#136961,#136962,#136963,
#136964),(#136965,#136966,#136967,#136968,#136969,#136970,#136971)),
 .UNSPECIFIED.,.F.,.F.,.F.)
B_SPLINE_SURFACE_WITH_KNOTS((2,2),(3,2,2,3),(0.,0.289807040992884),(0.556037361265319,
0.556212823028861,0.571428571428571,0.573758999383057),.UNSPECIFIED.)
GEOMETRIC_REPRESENTATION_ITEM()
RATIONAL_B_SPLINE_SURFACE(((0.991593692313265,0.991593692313265,0.991593692313265,
0.994659131878645,1.,0.999181998279397,0.998417372792936),(0.991593692313266,
0.991593692313266,0.991593692313266,0.994659131878645,1.,0.999181998279397,
0.998417372792936)))
REPRESENTATION_ITEM('')
SURFACE()
);
#2500=(
BOUNDED_SURFACE()
B_SPLINE_SURFACE(1,2,((#136986,#136987,#136988,#136989,#136990),(#136991,
#136992,#136993,#136994,#136995)),.UNSPECIFIED.,.F.,.F.,.F.)
B_SPLINE_SURFACE_WITH_KNOTS((2,2),(3,2,3),(0.,0.290270016640829),(0.159799014184241,
0.176967058622921,0.17755599110692),.UNSPECIFIED.)
GEOMETRIC_REPRESENTATION_ITEM()
RATIONAL_B_SPLINE_SURFACE(((0.990927469170732,0.987759962570788,0.98748925405691,
0.98748925405691,0.98748925405691),(0.990927469170732,0.987759962570788,
0.98748925405691,0.98748925405691,0.98748925405691)))
REPRESENTATION_ITEM('')
SURFACE()
);
#2501=(
BOUNDED_SURFACE()
B_SPLINE_SURFACE(1,2,((#137008,#137009,#137010,#137011,#137012,#137013,
#137014),(#137015,#137016,#137017,#137018,#137019,#137020,#137021)),
 .UNSPECIFIED.,.F.,.F.,.F.)
B_SPLINE_SURFACE_WITH_KNOTS((2,2),(3,2,2,3),(0.,0.289807040992694),(0.556037361265319,
0.556212823028861,0.571428571428571,0.573758999383043),.UNSPECIFIED.)
GEOMETRIC_REPRESENTATION_ITEM()
RATIONAL_B_SPLINE_SURFACE(((0.991593692313266,0.991593692313266,0.991593692313266,
0.994659131878645,1.,0.999181998279402,0.998417372792945),(0.991593692313266,
0.991593692313266,0.991593692313266,0.994659131878645,1.,0.999181998279402,
0.998417372792945)))
REPRESENTATION_ITEM('')
SURFACE()
);
#2502=(
BOUNDED_SURFACE()
B_SPLINE_SURFACE(1,2,((#137036,#137037,#137038,#137039,#137040),(#137041,
#137042,#137043,#137044,#137045)),.UNSPECIFIED.,.F.,.F.,.F.)
B_SPLINE_SURFACE_WITH_KNOTS((2,2),(3,2,3),(0.,0.29027001662598),(0.159799014184254,
0.176967058622921,0.177555991092038),.UNSPECIFIED.)
GEOMETRIC_REPRESENTATION_ITEM()
RATIONAL_B_SPLINE_SURFACE(((0.990927469170727,0.987759962570788,0.98748925405691,
0.98748925405691,0.98748925405691),(0.990927469170727,0.987759962570788,
0.98748925405691,0.98748925405691,0.98748925405691)))
REPRESENTATION_ITEM('')
SURFACE()
);
#2503=(
BOUNDED_SURFACE()
B_SPLINE_SURFACE(1,2,((#137058,#137059,#137060,#137061,#137062,#137063,
#137064),(#137065,#137066,#137067,#137068,#137069,#137070,#137071)),
 .UNSPECIFIED.,.F.,.F.,.F.)
B_SPLINE_SURFACE_WITH_KNOTS((2,2),(3,2,2,3),(0.,0.289807040993741),(0.55603736126532,
0.556212823028862,0.571428571428571,0.573758999383057),.UNSPECIFIED.)
GEOMETRIC_REPRESENTATION_ITEM()
RATIONAL_B_SPLINE_SURFACE(((0.991593692313266,0.991593692313266,0.991593692313266,
0.994659131878645,1.,0.999181998279397,0.998417372792936),(0.991593692313266,
0.991593692313266,0.991593692313266,0.994659131878645,1.,0.999181998279397,
0.998417372792936)))
REPRESENTATION_ITEM('')
SURFACE()
);
#2504=(
BOUNDED_SURFACE()
B_SPLINE_SURFACE(1,2,((#137077,#137078,#137079,#137080,#137081),(#137082,
#137083,#137084,#137085,#137086)),.UNSPECIFIED.,.F.,.F.,.F.)
B_SPLINE_SURFACE_WITH_KNOTS((2,2),(3,2,3),(0.,0.290270016597558),(0.159799014184244,
0.176967058622922,0.177555991064019),.UNSPECIFIED.)
GEOMETRIC_REPRESENTATION_ITEM()
RATIONAL_B_SPLINE_SURFACE(((0.990927469170731,0.987759962570788,0.98748925405691,
0.98748925405691,0.98748925405691),(0.990927469170731,0.987759962570788,
0.98748925405691,0.98748925405691,0.98748925405691)))
REPRESENTATION_ITEM('')
SURFACE()
);
#2505=(
BOUNDED_SURFACE()
B_SPLINE_SURFACE(1,2,((#137099,#137100,#137101,#137102,#137103,#137104,
#137105),(#137106,#137107,#137108,#137109,#137110,#137111,#137112)),
 .UNSPECIFIED.,.F.,.F.,.F.)
B_SPLINE_SURFACE_WITH_KNOTS((2,2),(3,2,2,3),(0.,0.289807040991906),(0.556037361265319,
0.556212823028861,0.571428571428571,0.573758999383057),.UNSPECIFIED.)
GEOMETRIC_REPRESENTATION_ITEM()
RATIONAL_B_SPLINE_SURFACE(((0.991593692313266,0.991593692313266,0.991593692313266,
0.994659131878645,1.,0.999181998279397,0.998417372792936),(0.991593692313266,
0.991593692313266,0.991593692313266,0.994659131878645,1.,0.999181998279397,
0.998417372792936)))
REPRESENTATION_ITEM('')
SURFACE()
);
#2506=(
BOUNDED_SURFACE()
B_SPLINE_SURFACE(1,2,((#137118,#137119,#137120,#137121,#137122),(#137123,
#137124,#137125,#137126,#137127)),.UNSPECIFIED.,.F.,.F.,.F.)
B_SPLINE_SURFACE_WITH_KNOTS((2,2),(3,2,3),(0.,0.290270016589869),(0.159799014184269,
0.176967058622921,0.177555991056242),.UNSPECIFIED.)
GEOMETRIC_REPRESENTATION_ITEM()
RATIONAL_B_SPLINE_SURFACE(((0.990927469170722,0.987759962570787,0.98748925405691,
0.98748925405691,0.98748925405691),(0.990927469170722,0.987759962570787,
0.98748925405691,0.98748925405691,0.98748925405691)))
REPRESENTATION_ITEM('')
SURFACE()
);
#2507=(
BOUNDED_SURFACE()
B_SPLINE_SURFACE(1,2,((#137140,#137141,#137142,#137143,#137144,#137145,
#137146),(#137147,#137148,#137149,#137150,#137151,#137152,#137153)),
 .UNSPECIFIED.,.F.,.F.,.F.)
B_SPLINE_SURFACE_WITH_KNOTS((2,2),(3,2,2,3),(0.,0.289807040993049),(0.556037361265319,
0.556212823028861,0.571428571428571,0.573758999383058),.UNSPECIFIED.)
GEOMETRIC_REPRESENTATION_ITEM()
RATIONAL_B_SPLINE_SURFACE(((0.991593692313265,0.991593692313265,0.991593692313265,
0.994659131878645,1.,0.999181998279397,0.998417372792936),(0.991593692313265,
0.991593692313265,0.991593692313265,0.994659131878645,1.,0.999181998279397,
0.998417372792936)))
REPRESENTATION_ITEM('')
SURFACE()
);
#2508=(
BOUNDED_SURFACE()
B_SPLINE_SURFACE(1,2,((#137168,#137169,#137170,#137171,#137172),(#137173,
#137174,#137175,#137176,#137177)),.UNSPECIFIED.,.F.,.F.,.F.)
B_SPLINE_SURFACE_WITH_KNOTS((2,2),(3,2,3),(0.,0.290270016612988),(0.15979901418427,
0.176967058622921,0.17755599107958),.UNSPECIFIED.)
GEOMETRIC_REPRESENTATION_ITEM()
RATIONAL_B_SPLINE_SURFACE(((0.990927469170722,0.987759962570788,0.98748925405691,
0.98748925405691,0.98748925405691),(0.990927469170721,0.987759962570787,
0.98748925405691,0.98748925405691,0.98748925405691)))
REPRESENTATION_ITEM('')
SURFACE()
);
#2509=(
BOUNDED_SURFACE()
B_SPLINE_SURFACE(1,2,((#137190,#137191,#137192,#137193,#137194,#137195,
#137196),(#137197,#137198,#137199,#137200,#137201,#137202,#137203)),
 .UNSPECIFIED.,.F.,.F.,.F.)
B_SPLINE_SURFACE_WITH_KNOTS((2,2),(3,2,2,3),(0.,0.28980704099156),(0.556037361265318,
0.55621282302886,0.571428571428571,0.573758999383056),.UNSPECIFIED.)
GEOMETRIC_REPRESENTATION_ITEM()
RATIONAL_B_SPLINE_SURFACE(((0.991593692313265,0.991593692313265,0.991593692313265,
0.994659131878644,1.,0.999181998279397,0.998417372792936),(0.991593692313265,
0.991593692313265,0.991593692313265,0.994659131878644,1.,0.999181998279397,
0.998417372792936)))
REPRESENTATION_ITEM('')
SURFACE()
);
#2510=(
BOUNDED_SURFACE()
B_SPLINE_SURFACE(1,2,((#137209,#137210,#137211,#137212,#137213),(#137214,
#137215,#137216,#137217,#137218)),.UNSPECIFIED.,.F.,.F.,.F.)
B_SPLINE_SURFACE_WITH_KNOTS((2,2),(3,2,3),(0.,0.290270016622051),(0.15979901418408,
0.176967058622922,0.177555991088182),.UNSPECIFIED.)
GEOMETRIC_REPRESENTATION_ITEM()
RATIONAL_B_SPLINE_SURFACE(((0.990927469170791,0.98775996257079,0.98748925405691,
0.98748925405691,0.98748925405691),(0.990927469170791,0.98775996257079,
0.98748925405691,0.98748925405691,0.98748925405691)))
REPRESENTATION_ITEM('')
SURFACE()
);
#2511=(
BOUNDED_SURFACE()
B_SPLINE_SURFACE(1,2,((#137231,#137232,#137233,#137234,#137235,#137236,
#137237),(#137238,#137239,#137240,#137241,#137242,#137243,#137244)),
 .UNSPECIFIED.,.F.,.F.,.F.)
B_SPLINE_SURFACE_WITH_KNOTS((2,2),(3,2,2,3),(0.,0.289807040991555),(0.556037361265319,
0.55621282302886,0.571428571428571,0.573758999382975),.UNSPECIFIED.)
GEOMETRIC_REPRESENTATION_ITEM()
RATIONAL_B_SPLINE_SURFACE(((0.991593692313265,0.991593692313265,0.991593692313265,
0.994659131878644,1.,0.999181998279426,0.99841737279299),(0.991593692313265,
0.991593692313265,0.991593692313265,0.994659131878644,1.,0.999181998279426,
0.99841737279299)))
REPRESENTATION_ITEM('')
SURFACE()
);
#2512=(
BOUNDED_SURFACE()
B_SPLINE_SURFACE(1,2,((#137255,#137256,#137257,#137258,#137259),(#137260,
#137261,#137262,#137263,#137264)),.UNSPECIFIED.,.F.,.F.,.F.)
B_SPLINE_SURFACE_WITH_KNOTS((2,2),(3,2,3),(0.,0.29027001662738),(0.159799014184193,
0.176967058622922,0.1775559910934),.UNSPECIFIED.)
GEOMETRIC_REPRESENTATION_ITEM()
RATIONAL_B_SPLINE_SURFACE(((0.99092746917075,0.987759962570788,0.98748925405691,
0.98748925405691,0.98748925405691),(0.99092746917075,0.987759962570788,
0.98748925405691,0.98748925405691,0.98748925405691)))
REPRESENTATION_ITEM('')
SURFACE()
);
#2513=(
BOUNDED_SURFACE()
B_SPLINE_SURFACE(1,2,((#137280,#137281,#137282,#137283,#137284,#137285,
#137286),(#137287,#137288,#137289,#137290,#137291,#137292,#137293)),
 .UNSPECIFIED.,.F.,.F.,.F.)
B_SPLINE_SURFACE_WITH_KNOTS((2,2),(3,2,2,3),(0.,0.289807040991561),(0.556037361265318,
0.55621282302886,0.571428571428571,0.573758999383057),.UNSPECIFIED.)
GEOMETRIC_REPRESENTATION_ITEM()
RATIONAL_B_SPLINE_SURFACE(((0.991593692313265,0.991593692313265,0.991593692313265,
0.994659131878644,1.,0.999181998279397,0.998417372792936),(0.991593692313265,
0.991593692313265,0.991593692313265,0.994659131878644,1.,0.999181998279397,
0.998417372792936)))
REPRESENTATION_ITEM('')
SURFACE()
);
#2514=(
BOUNDED_SURFACE()
B_SPLINE_SURFACE(1,2,((#137308,#137309,#137310,#137311,#137312),(#137313,
#137314,#137315,#137316,#137317)),.UNSPECIFIED.,.F.,.F.,.F.)
B_SPLINE_SURFACE_WITH_KNOTS((2,2),(3,2,3),(0.,0.290268982604117),(0.504616569533924,
0.52191752982614,0.522505428232031),.UNSPECIFIED.)
GEOMETRIC_REPRESENTATION_ITEM()
RATIONAL_B_SPLINE_SURFACE(((0.996968549833844,0.991680746768616,0.989334769731189,
0.989334769731189,0.989334769731189),(0.996968549833844,0.991680746768616,
0.989334769731189,0.989334769731189,0.989334769731189)))
REPRESENTATION_ITEM('')
SURFACE()
);
#2515=(
BOUNDED_SURFACE()
B_SPLINE_SURFACE(1,2,((#137328,#137329,#137330,#137331,#137332),(#137333,
#137334,#137335,#137336,#137337)),.UNSPECIFIED.,.F.,.F.,.F.)
B_SPLINE_SURFACE_WITH_KNOTS((2,2),(3,2,3),(0.,0.289807040991617),(0.211502584834065,
0.214285714285714,0.228987659635173),.UNSPECIFIED.)
GEOMETRIC_REPRESENTATION_ITEM()
RATIONAL_B_SPLINE_SURFACE(((0.998122319569323,0.999023095875705,1.,0.994839481491405,
0.99180331349328),(0.998122319569323,0.999023095875705,1.,0.994839481491405,
0.99180331349328)))
REPRESENTATION_ITEM('')
SURFACE()
);
#2516=(
BOUNDED_SURFACE()
B_SPLINE_SURFACE(1,2,((#137360,#137361,#137362,#137363,#137364),(#137365,
#137366,#137367,#137368,#137369)),.UNSPECIFIED.,.F.,.F.,.F.)
B_SPLINE_SURFACE_WITH_KNOTS((2,2),(3,2,3),(0.,0.290268982619199),(0.504616569534225,
0.521917529826141,0.522505428247126),.UNSPECIFIED.)
GEOMETRIC_REPRESENTATION_ITEM()
RATIONAL_B_SPLINE_SURFACE(((0.99696854983366,0.991680746768575,0.989334769731189,
0.989334769731189,0.989334769731189),(0.99696854983366,0.991680746768575,
0.989334769731189,0.989334769731189,0.989334769731189)))
REPRESENTATION_ITEM('')
SURFACE()
);
#2517=(
BOUNDED_SURFACE()
B_SPLINE_SURFACE(1,2,((#137371,#137372,#137373,#137374,#137375),(#137376,
#137377,#137378,#137379,#137380)),.UNSPECIFIED.,.F.,.F.,.F.)
B_SPLINE_SURFACE_WITH_KNOTS((2,2),(3,2,3),(0.,0.289807040991574),(0.211502584834048,
0.214285714285714,0.228987659635174),.UNSPECIFIED.)
GEOMETRIC_REPRESENTATION_ITEM()
RATIONAL_B_SPLINE_SURFACE(((0.998122319569312,0.999023095875699,1.,0.994839481491404,
0.99180331349328),(0.998122319569312,0.999023095875699,1.,0.994839481491404,
0.99180331349328)))
REPRESENTATION_ITEM('')
SURFACE()
);
#2518=(
BOUNDED_SURFACE()
B_SPLINE_SURFACE(1,2,((#137403,#137404,#137405,#137406,#137407),(#137408,
#137409,#137410,#137411,#137412)),.UNSPECIFIED.,.F.,.F.,.F.)
B_SPLINE_SURFACE_WITH_KNOTS((2,2),(3,2,3),(0.,0.290268982597261),(0.504616569534328,
0.521917529826141,0.522505428225168),.UNSPECIFIED.)
GEOMETRIC_REPRESENTATION_ITEM()
RATIONAL_B_SPLINE_SURFACE(((0.996968549833597,0.99168074676856,0.989334769731189,
0.989334769731189,0.989334769731189),(0.996968549833597,0.99168074676856,
0.989334769731189,0.989334769731189,0.989334769731189)))
REPRESENTATION_ITEM('')
SURFACE()
);
#2519=(
BOUNDED_SURFACE()
B_SPLINE_SURFACE(1,2,((#137414,#137415,#137416,#137417,#137418),(#137419,
#137420,#137421,#137422,#137423)),.UNSPECIFIED.,.F.,.F.,.F.)
B_SPLINE_SURFACE_WITH_KNOTS((2,2),(3,2,3),(0.,0.289807040991561),(0.21150258483404,
0.214285714285714,0.228987659635174),.UNSPECIFIED.)
GEOMETRIC_REPRESENTATION_ITEM()
RATIONAL_B_SPLINE_SURFACE(((0.998122319569306,0.999023095875696,1.,0.994839481491404,
0.99180331349328),(0.998122319569306,0.999023095875696,1.,0.994839481491404,
0.99180331349328)))
REPRESENTATION_ITEM('')
SURFACE()
);
#2520=(
BOUNDED_SURFACE()
B_SPLINE_SURFACE(1,2,((#137446,#137447,#137448,#137449,#137450),(#137451,
#137452,#137453,#137454,#137455)),.UNSPECIFIED.,.F.,.F.,.F.)
B_SPLINE_SURFACE_WITH_KNOTS((2,2),(3,2,3),(0.,0.290268982610398),(0.504616569534327,
0.521917529826141,0.52250542823832),.UNSPECIFIED.)
GEOMETRIC_REPRESENTATION_ITEM()
RATIONAL_B_SPLINE_SURFACE(((0.996968549833597,0.991680746768561,0.989334769731189,
0.989334769731189,0.989334769731189),(0.996968549833597,0.991680746768561,
0.989334769731189,0.989334769731189,0.989334769731189)))
REPRESENTATION_ITEM('')
SURFACE()
);
#2521=(
BOUNDED_SURFACE()
B_SPLINE_SURFACE(1,2,((#137457,#137458,#137459,#137460,#137461),(#137462,
#137463,#137464,#137465,#137466)),.UNSPECIFIED.,.F.,.F.,.F.)
B_SPLINE_SURFACE_WITH_KNOTS((2,2),(3,2,3),(0.,0.289807040991562),(0.211502584834064,
0.214285714285714,0.228987659635173),.UNSPECIFIED.)
GEOMETRIC_REPRESENTATION_ITEM()
RATIONAL_B_SPLINE_SURFACE(((0.998122319569322,0.999023095875704,1.,0.994839481491405,
0.99180331349328),(0.998122319569322,0.999023095875704,1.,0.994839481491405,
0.99180331349328)))
REPRESENTATION_ITEM('')
SURFACE()
);
#2522=(
BOUNDED_SURFACE()
B_SPLINE_SURFACE(1,2,((#137489,#137490,#137491,#137492,#137493),(#137494,
#137495,#137496,#137497,#137498)),.UNSPECIFIED.,.F.,.F.,.F.)
B_SPLINE_SURFACE_WITH_KNOTS((2,2),(3,2,3),(0.,0.29026898260331),(0.504616569533844,
0.521917529826141,0.522505428231226),.UNSPECIFIED.)
GEOMETRIC_REPRESENTATION_ITEM()
RATIONAL_B_SPLINE_SURFACE(((0.996968549833893,0.991680746768626,0.989334769731189,
0.989334769731189,0.989334769731189),(0.996968549833893,0.991680746768626,
0.989334769731189,0.989334769731189,0.989334769731189)))
REPRESENTATION_ITEM('')
SURFACE()
);
#2523=(
BOUNDED_SURFACE()
B_SPLINE_SURFACE(1,2,((#137500,#137501,#137502,#137503,#137504),(#137505,
#137506,#137507,#137508,#137509)),.UNSPECIFIED.,.F.,.F.,.F.)
B_SPLINE_SURFACE_WITH_KNOTS((2,2),(3,2,3),(0.,0.289807040991557),(0.211502584834063,
0.214285714285714,0.228987659635058),.UNSPECIFIED.)
GEOMETRIC_REPRESENTATION_ITEM()
RATIONAL_B_SPLINE_SURFACE(((0.998122319569322,0.999023095875704,1.,0.994839481491445,
0.991803313493328),(0.998122319569322,0.999023095875704,1.,0.994839481491445,
0.991803313493328)))
REPRESENTATION_ITEM('')
SURFACE()
);
#2524=(
BOUNDED_SURFACE()
B_SPLINE_SURFACE(1,2,((#137532,#137533,#137534,#137535,#137536),(#137537,
#137538,#137539,#137540,#137541)),.UNSPECIFIED.,.F.,.F.,.F.)
B_SPLINE_SURFACE_WITH_KNOTS((2,2),(3,2,3),(0.,0.290268982592995),(0.504616569533987,
0.521917529826141,0.522505428220914),.UNSPECIFIED.)
GEOMETRIC_REPRESENTATION_ITEM()
RATIONAL_B_SPLINE_SURFACE(((0.996968549833805,0.991680746768607,0.989334769731189,
0.989334769731189,0.989334769731189),(0.996968549833805,0.991680746768607,
0.989334769731189,0.989334769731189,0.989334769731189)))
REPRESENTATION_ITEM('')
SURFACE()
);
#2525=(
BOUNDED_SURFACE()
B_SPLINE_SURFACE(1,2,((#137543,#137544,#137545,#137546,#137547),(#137548,
#137549,#137550,#137551,#137552)),.UNSPECIFIED.,.F.,.F.,.F.)
B_SPLINE_SURFACE_WITH_KNOTS((2,2),(3,2,3),(0.,0.289807040991557),(0.211502584834064,
0.214285714285714,0.228987659635173),.UNSPECIFIED.)
GEOMETRIC_REPRESENTATION_ITEM()
RATIONAL_B_SPLINE_SURFACE(((0.998122319569322,0.999023095875704,1.,0.994839481491405,
0.99180331349328),(0.998122319569322,0.999023095875704,1.,0.994839481491405,
0.99180331349328)))
REPRESENTATION_ITEM('')
SURFACE()
);
#2526=(
BOUNDED_SURFACE()
B_SPLINE_SURFACE(1,2,((#137575,#137576,#137577,#137578,#137579),(#137580,
#137581,#137582,#137583,#137584)),.UNSPECIFIED.,.F.,.F.,.F.)
B_SPLINE_SURFACE_WITH_KNOTS((2,2),(3,2,3),(0.,0.290268982594292),(0.50461656953416,
0.521917529826141,0.522505428222218),.UNSPECIFIED.)
GEOMETRIC_REPRESENTATION_ITEM()
RATIONAL_B_SPLINE_SURFACE(((0.996968549833699,0.991680746768583,0.989334769731189,
0.989334769731189,0.989334769731189),(0.996968549833699,0.991680746768583,
0.989334769731189,0.989334769731189,0.989334769731189)))
REPRESENTATION_ITEM('')
SURFACE()
);
#2527=(
BOUNDED_SURFACE()
B_SPLINE_SURFACE(1,2,((#137586,#137587,#137588,#137589,#137590),(#137591,
#137592,#137593,#137594,#137595)),.UNSPECIFIED.,.F.,.F.,.F.)
B_SPLINE_SURFACE_WITH_KNOTS((2,2),(3,2,3),(0.,0.28980704099156),(0.211502584834035,
0.214285714285714,0.228987659635174),.UNSPECIFIED.)
GEOMETRIC_REPRESENTATION_ITEM()
RATIONAL_B_SPLINE_SURFACE(((0.998122319569303,0.999023095875694,1.,0.994839481491404,
0.99180331349328),(0.998122319569303,0.999023095875694,1.,0.994839481491404,
0.99180331349328)))
REPRESENTATION_ITEM('')
SURFACE()
);
#2528=(
BOUNDED_SURFACE()
B_SPLINE_SURFACE(1,2,((#137603,#137604,#137605,#137606,#137607),(#137608,
#137609,#137610,#137611,#137612)),.UNSPECIFIED.,.F.,.F.,.F.)
B_SPLINE_SURFACE_WITH_KNOTS((2,2),(3,2,3),(0.,0.289946589047145),(0.504616569534328,
0.521917529826141,0.522183034675071),.UNSPECIFIED.)
GEOMETRIC_REPRESENTATION_ITEM()
RATIONAL_B_SPLINE_SURFACE(((0.996968549833597,0.991680746768561,0.989334769731189,
0.989334769731189,0.989334769731189),(0.996968549833597,0.991680746768561,
0.989334769731189,0.989334769731189,0.989334769731189)))
REPRESENTATION_ITEM('')
SURFACE()
);
#2529=(
BOUNDED_SURFACE()
B_SPLINE_SURFACE(1,2,((#137614,#137615,#137616,#137617,#137618),(#137619,
#137620,#137621,#137622,#137623)),.UNSPECIFIED.,.F.,.F.,.F.)
B_SPLINE_SURFACE_WITH_KNOTS((2,2),(3,2,3),(0.,0.289807040991555),(0.211502584834064,
0.214285714285714,0.228987659635174),.UNSPECIFIED.)
GEOMETRIC_REPRESENTATION_ITEM()
RATIONAL_B_SPLINE_SURFACE(((0.998122319569322,0.999023095875704,1.,0.994839481491404,
0.99180331349328),(0.998122319569322,0.999023095875704,1.,0.994839481491404,
0.99180331349328)))
REPRESENTATION_ITEM('')
SURFACE()
);
#2530=(
BOUNDED_SURFACE()
B_SPLINE_SURFACE(1,2,((#137646,#137647,#137648,#137649,#137650),(#137651,
#137652,#137653,#137654,#137655)),.UNSPECIFIED.,.F.,.F.,.F.)
B_SPLINE_SURFACE_WITH_KNOTS((2,2),(3,2,3),(0.,0.290268982610033),(0.504616569534328,
0.521917529826141,0.522505428237962),.UNSPECIFIED.)
GEOMETRIC_REPRESENTATION_ITEM()
RATIONAL_B_SPLINE_SURFACE(((0.996968549833597,0.991680746768561,0.989334769731189,
0.989334769731189,0.989334769731189),(0.996968549833597,0.991680746768561,
0.989334769731189,0.989334769731189,0.989334769731189)))
REPRESENTATION_ITEM('')
SURFACE()
);
#2531=(
BOUNDED_SURFACE()
B_SPLINE_SURFACE(1,2,((#137657,#137658,#137659,#137660,#137661),(#137662,
#137663,#137664,#137665,#137666)),.UNSPECIFIED.,.F.,.F.,.F.)
B_SPLINE_SURFACE_WITH_KNOTS((2,2),(3,2,3),(0.,0.289807040991566),(0.211502584834064,
0.214285714285714,0.228987659635174),.UNSPECIFIED.)
GEOMETRIC_REPRESENTATION_ITEM()
RATIONAL_B_SPLINE_SURFACE(((0.998122319569322,0.999023095875704,1.,0.994839481491404,
0.99180331349328),(0.998122319569322,0.999023095875704,1.,0.994839481491404,
0.99180331349328)))
REPRESENTATION_ITEM('')
SURFACE()
);
#2532=(
BOUNDED_SURFACE()
B_SPLINE_SURFACE(1,2,((#137689,#137690,#137691,#137692,#137693),(#137694,
#137695,#137696,#137697,#137698)),.UNSPECIFIED.,.F.,.F.,.F.)
B_SPLINE_SURFACE_WITH_KNOTS((2,2),(3,2,3),(0.,0.290268982603647),(0.504616569534328,
0.521917529826141,0.522505428231568),.UNSPECIFIED.)
GEOMETRIC_REPRESENTATION_ITEM()
RATIONAL_B_SPLINE_SURFACE(((0.996968549833597,0.99168074676856,0.989334769731189,
0.989334769731189,0.989334769731189),(0.996968549833597,0.99168074676856,
0.989334769731189,0.989334769731189,0.989334769731189)))
REPRESENTATION_ITEM('')
SURFACE()
);
#2533=(
BOUNDED_SURFACE()
B_SPLINE_SURFACE(1,2,((#137700,#137701,#137702,#137703,#137704),(#137705,
#137706,#137707,#137708,#137709)),.UNSPECIFIED.,.F.,.F.,.F.)
B_SPLINE_SURFACE_WITH_KNOTS((2,2),(3,2,3),(0.,0.289807040991558),(0.21150258483406,
0.214285714285714,0.228987659635174),.UNSPECIFIED.)
GEOMETRIC_REPRESENTATION_ITEM()
RATIONAL_B_SPLINE_SURFACE(((0.998122319569319,0.999023095875703,1.,0.994839481491405,
0.99180331349328),(0.998122319569319,0.999023095875703,1.,0.994839481491405,
0.99180331349328)))
REPRESENTATION_ITEM('')
SURFACE()
);
#2534=(
BOUNDED_SURFACE()
B_SPLINE_SURFACE(1,2,((#137732,#137733,#137734,#137735,#137736),(#137737,
#137738,#137739,#137740,#137741)),.UNSPECIFIED.,.F.,.F.,.F.)
B_SPLINE_SURFACE_WITH_KNOTS((2,2),(3,2,3),(0.,0.290268982606492),(0.504616569534328,
0.521917529826141,0.522505428234414),.UNSPECIFIED.)
GEOMETRIC_REPRESENTATION_ITEM()
RATIONAL_B_SPLINE_SURFACE(((0.996968549833597,0.99168074676856,0.989334769731189,
0.989334769731189,0.989334769731189),(0.996968549833597,0.99168074676856,
0.989334769731189,0.989334769731189,0.989334769731189)))
REPRESENTATION_ITEM('')
SURFACE()
);
#2535=(
BOUNDED_SURFACE()
B_SPLINE_SURFACE(1,2,((#137743,#137744,#137745,#137746,#137747),(#137748,
#137749,#137750,#137751,#137752)),.UNSPECIFIED.,.F.,.F.,.F.)
B_SPLINE_SURFACE_WITH_KNOTS((2,2),(3,2,3),(0.,0.289807040991564),(0.211502584834064,
0.214285714285714,0.228987659635174),.UNSPECIFIED.)
GEOMETRIC_REPRESENTATION_ITEM()
RATIONAL_B_SPLINE_SURFACE(((0.998122319569322,0.999023095875704,1.,0.994839481491405,
0.99180331349328),(0.998122319569322,0.999023095875704,1.,0.994839481491405,
0.99180331349328)))
REPRESENTATION_ITEM('')
SURFACE()
);
#2536=(
BOUNDED_SURFACE()
B_SPLINE_SURFACE(1,2,((#137775,#137776,#137777,#137778,#137779),(#137780,
#137781,#137782,#137783,#137784)),.UNSPECIFIED.,.F.,.F.,.F.)
B_SPLINE_SURFACE_WITH_KNOTS((2,2),(3,2,3),(0.,0.290268982616428),(0.504616569534328,
0.521917529826141,0.522505428244344),.UNSPECIFIED.)
GEOMETRIC_REPRESENTATION_ITEM()
RATIONAL_B_SPLINE_SURFACE(((0.996968549833597,0.99168074676856,0.989334769731189,
0.989334769731189,0.989334769731189),(0.996968549833597,0.99168074676856,
0.989334769731189,0.989334769731189,0.989334769731189)))
REPRESENTATION_ITEM('')
SURFACE()
);
#2537=(
BOUNDED_SURFACE()
B_SPLINE_SURFACE(1,2,((#137786,#137787,#137788,#137789,#137790),(#137791,
#137792,#137793,#137794,#137795)),.UNSPECIFIED.,.F.,.F.,.F.)
B_SPLINE_SURFACE_WITH_KNOTS((2,2),(3,2,3),(0.,0.289807040991564),(0.211502584834024,
0.214285714285714,0.228987659635174),.UNSPECIFIED.)
GEOMETRIC_REPRESENTATION_ITEM()
RATIONAL_B_SPLINE_SURFACE(((0.998122319569296,0.99902309587569,1.,0.994839481491404,
0.99180331349328),(0.998122319569296,0.99902309587569,1.,0.994839481491404,
0.99180331349328)))
REPRESENTATION_ITEM('')
SURFACE()
);
#2538=(
BOUNDED_SURFACE()
B_SPLINE_SURFACE(1,2,((#137818,#137819,#137820,#137821,#137822),(#137823,
#137824,#137825,#137826,#137827)),.UNSPECIFIED.,.F.,.F.,.F.)
B_SPLINE_SURFACE_WITH_KNOTS((2,2),(3,2,3),(0.,0.29026898259843),(0.504616569534328,
0.521917529826141,0.522505428226351),.UNSPECIFIED.)
GEOMETRIC_REPRESENTATION_ITEM()
RATIONAL_B_SPLINE_SURFACE(((0.996968549833597,0.991680746768561,0.989334769731189,
0.989334769731189,0.989334769731189),(0.996968549833597,0.991680746768561,
0.989334769731189,0.989334769731189,0.989334769731189)))
REPRESENTATION_ITEM('')
SURFACE()
);
#2539=(
BOUNDED_SURFACE()
B_SPLINE_SURFACE(1,2,((#137829,#137830,#137831,#137832,#137833),(#137834,
#137835,#137836,#137837,#137838)),.UNSPECIFIED.,.F.,.F.,.F.)
B_SPLINE_SURFACE_WITH_KNOTS((2,2),(3,2,3),(0.,0.28980704099156),(0.211502584834064,
0.214285714285714,0.228987659635174),.UNSPECIFIED.)
GEOMETRIC_REPRESENTATION_ITEM()
RATIONAL_B_SPLINE_SURFACE(((0.998122319569322,0.999023095875704,1.,0.994839481491404,
0.99180331349328),(0.998122319569322,0.999023095875704,1.,0.994839481491404,
0.99180331349328)))
REPRESENTATION_ITEM('')
SURFACE()
);
#2540=(
BOUNDED_SURFACE()
B_SPLINE_SURFACE(1,2,((#137861,#137862,#137863,#137864,#137865),(#137866,
#137867,#137868,#137869,#137870)),.UNSPECIFIED.,.F.,.F.,.F.)
B_SPLINE_SURFACE_WITH_KNOTS((2,2),(3,2,3),(0.,0.290268982603716),(0.504616569534328,
0.521917529826141,0.52250542823164),.UNSPECIFIED.)
GEOMETRIC_REPRESENTATION_ITEM()
RATIONAL_B_SPLINE_SURFACE(((0.996968549833597,0.99168074676856,0.989334769731189,
0.989334769731189,0.989334769731189),(0.996968549833597,0.99168074676856,
0.989334769731189,0.989334769731189,0.989334769731189)))
REPRESENTATION_ITEM('')
SURFACE()
);
#2541=(
BOUNDED_SURFACE()
B_SPLINE_SURFACE(1,2,((#137872,#137873,#137874,#137875,#137876),(#137877,
#137878,#137879,#137880,#137881)),.UNSPECIFIED.,.F.,.F.,.F.)
B_SPLINE_SURFACE_WITH_KNOTS((2,2),(3,2,3),(0.,0.28980704099156),(0.211502584834064,
0.214285714285714,0.228987659635174),.UNSPECIFIED.)
GEOMETRIC_REPRESENTATION_ITEM()
RATIONAL_B_SPLINE_SURFACE(((0.998122319569322,0.999023095875704,1.,0.994839481491404,
0.99180331349328),(0.998122319569322,0.999023095875704,1.,0.994839481491404,
0.99180331349328)))
REPRESENTATION_ITEM('')
SURFACE()
);
#2542=(
BOUNDED_SURFACE()
B_SPLINE_SURFACE(1,2,((#137904,#137905,#137906,#137907,#137908),(#137909,
#137910,#137911,#137912,#137913)),.UNSPECIFIED.,.F.,.F.,.F.)
B_SPLINE_SURFACE_WITH_KNOTS((2,2),(3,2,3),(0.,0.290268982599203),(0.504616569534328,
0.521917529826141,0.52250542822713),.UNSPECIFIED.)
GEOMETRIC_REPRESENTATION_ITEM()
RATIONAL_B_SPLINE_SURFACE(((0.996968549833597,0.991680746768561,0.989334769731189,
0.989334769731189,0.989334769731189),(0.996968549833597,0.991680746768561,
0.989334769731189,0.989334769731189,0.989334769731189)))
REPRESENTATION_ITEM('')
SURFACE()
);
#2543=(
BOUNDED_SURFACE()
B_SPLINE_SURFACE(1,2,((#137915,#137916,#137917,#137918,#137919),(#137920,
#137921,#137922,#137923,#137924)),.UNSPECIFIED.,.F.,.F.,.F.)
B_SPLINE_SURFACE_WITH_KNOTS((2,2),(3,2,3),(0.,0.289807040991561),(0.211502584833965,
0.214285714285714,0.228987659635174),.UNSPECIFIED.)
GEOMETRIC_REPRESENTATION_ITEM()
RATIONAL_B_SPLINE_SURFACE(((0.998122319569258,0.99902309587567,1.,0.994839481491404,
0.99180331349328),(0.998122319569258,0.99902309587567,1.,0.994839481491404,
0.99180331349328)))
REPRESENTATION_ITEM('')
SURFACE()
);
#2544=(
BOUNDED_SURFACE()
B_SPLINE_SURFACE(1,2,((#137947,#137948,#137949,#137950,#137951),(#137952,
#137953,#137954,#137955,#137956)),.UNSPECIFIED.,.F.,.F.,.F.)
B_SPLINE_SURFACE_WITH_KNOTS((2,2),(3,2,3),(0.,0.290268982598464),(0.504616569534328,
0.521917529826141,0.522505428226386),.UNSPECIFIED.)
GEOMETRIC_REPRESENTATION_ITEM()
RATIONAL_B_SPLINE_SURFACE(((0.996968549833597,0.99168074676856,0.989334769731189,
0.989334769731189,0.989334769731189),(0.996968549833597,0.99168074676856,
0.989334769731189,0.989334769731189,0.989334769731189)))
REPRESENTATION_ITEM('')
SURFACE()
);
#2545=(
BOUNDED_SURFACE()
B_SPLINE_SURFACE(1,2,((#137958,#137959,#137960,#137961,#137962),(#137963,
#137964,#137965,#137966,#137967)),.UNSPECIFIED.,.F.,.F.,.F.)
B_SPLINE_SURFACE_WITH_KNOTS((2,2),(3,2,3),(0.,0.289807040991561),(0.211502584833903,
0.214285714285714,0.228987659635175),.UNSPECIFIED.)
GEOMETRIC_REPRESENTATION_ITEM()
RATIONAL_B_SPLINE_SURFACE(((0.998122319569217,0.999023095875648,1.,0.994839481491404,
0.991803313493279),(0.998122319569217,0.999023095875648,1.,0.994839481491404,
0.991803313493279)))
REPRESENTATION_ITEM('')
SURFACE()
);
#2546=(
BOUNDED_SURFACE()
B_SPLINE_SURFACE(1,2,((#137990,#137991,#137992,#137993,#137994),(#137995,
#137996,#137997,#137998,#137999)),.UNSPECIFIED.,.F.,.F.,.F.)
B_SPLINE_SURFACE_WITH_KNOTS((2,2),(3,2,3),(0.,0.290268982577918),(0.504616569534328,
0.521917529826141,0.522505428205845),.UNSPECIFIED.)
GEOMETRIC_REPRESENTATION_ITEM()
RATIONAL_B_SPLINE_SURFACE(((0.996968549833597,0.99168074676856,0.989334769731189,
0.989334769731189,0.989334769731189),(0.996968549833597,0.99168074676856,
0.989334769731189,0.989334769731189,0.989334769731189)))
REPRESENTATION_ITEM('')
SURFACE()
);
#2547=(
BOUNDED_SURFACE()
B_SPLINE_SURFACE(1,2,((#138001,#138002,#138003,#138004,#138005),(#138006,
#138007,#138008,#138009,#138010)),.UNSPECIFIED.,.F.,.F.,.F.)
B_SPLINE_SURFACE_WITH_KNOTS((2,2),(3,2,3),(0.,0.289807040991564),(0.211502584833963,
0.214285714285714,0.228987659635174),.UNSPECIFIED.)
GEOMETRIC_REPRESENTATION_ITEM()
RATIONAL_B_SPLINE_SURFACE(((0.998122319569257,0.999023095875669,1.,0.994839481491404,
0.99180331349328),(0.998122319569257,0.999023095875669,1.,0.994839481491404,
0.99180331349328)))
REPRESENTATION_ITEM('')
SURFACE()
);
#2548=(
BOUNDED_SURFACE()
B_SPLINE_SURFACE(1,2,((#138033,#138034,#138035,#138036,#138037),(#138038,
#138039,#138040,#138041,#138042)),.UNSPECIFIED.,.F.,.F.,.F.)
B_SPLINE_SURFACE_WITH_KNOTS((2,2),(3,2,3),(0.,0.290268982592395),(0.504616569534328,
0.521917529826141,0.522505428220313),.UNSPECIFIED.)
GEOMETRIC_REPRESENTATION_ITEM()
RATIONAL_B_SPLINE_SURFACE(((0.996968549833597,0.99168074676856,0.989334769731189,
0.989334769731189,0.989334769731189),(0.996968549833597,0.99168074676856,
0.989334769731189,0.989334769731189,0.989334769731189)))
REPRESENTATION_ITEM('')
SURFACE()
);
#2549=(
BOUNDED_SURFACE()
B_SPLINE_SURFACE(1,2,((#138044,#138045,#138046,#138047,#138048),(#138049,
#138050,#138051,#138052,#138053)),.UNSPECIFIED.,.F.,.F.,.F.)
B_SPLINE_SURFACE_WITH_KNOTS((2,2),(3,2,3),(0.,0.28980704099156),(0.211502584833935,
0.214285714285714,0.228987659635175),.UNSPECIFIED.)
GEOMETRIC_REPRESENTATION_ITEM()
RATIONAL_B_SPLINE_SURFACE(((0.998122319569238,0.999023095875659,1.,0.994839481491404,
0.991803313493279),(0.998122319569238,0.999023095875659,1.,0.994839481491404,
0.991803313493279)))
REPRESENTATION_ITEM('')
SURFACE()
);
#2550=(
BOUNDED_SURFACE()
B_SPLINE_SURFACE(1,2,((#138076,#138077,#138078,#138079,#138080),(#138081,
#138082,#138083,#138084,#138085)),.UNSPECIFIED.,.F.,.F.,.F.)
B_SPLINE_SURFACE_WITH_KNOTS((2,2),(3,2,3),(0.,0.290268982611678),(0.504616569534328,
0.521917529826141,0.522505428239596),.UNSPECIFIED.)
GEOMETRIC_REPRESENTATION_ITEM()
RATIONAL_B_SPLINE_SURFACE(((0.996968549833597,0.99168074676856,0.989334769731189,
0.989334769731189,0.989334769731189),(0.996968549833597,0.99168074676856,
0.989334769731189,0.989334769731189,0.989334769731189)))
REPRESENTATION_ITEM('')
SURFACE()
);
#2551=(
BOUNDED_SURFACE()
B_SPLINE_SURFACE(1,2,((#138087,#138088,#138089,#138090,#138091),(#138092,
#138093,#138094,#138095,#138096)),.UNSPECIFIED.,.F.,.F.,.F.)
B_SPLINE_SURFACE_WITH_KNOTS((2,2),(3,2,3),(0.,0.289807040991559),(0.211502584833671,
0.214285714285714,0.228987659635176),.UNSPECIFIED.)
GEOMETRIC_REPRESENTATION_ITEM()
RATIONAL_B_SPLINE_SURFACE(((0.998122319569068,0.999023095875566,1.,0.994839481491404,
0.991803313493279),(0.998122319569068,0.999023095875566,1.,0.994839481491404,
0.991803313493279)))
REPRESENTATION_ITEM('')
SURFACE()
);
#2552=(
BOUNDED_SURFACE()
B_SPLINE_SURFACE(1,2,((#138119,#138120,#138121,#138122,#138123),(#138124,
#138125,#138126,#138127,#138128)),.UNSPECIFIED.,.F.,.F.,.F.)
B_SPLINE_SURFACE_WITH_KNOTS((2,2),(3,2,3),(0.,0.290268982583992),(0.504616569534328,
0.521917529826141,0.522505428211919),.UNSPECIFIED.)
GEOMETRIC_REPRESENTATION_ITEM()
RATIONAL_B_SPLINE_SURFACE(((0.996968549833597,0.99168074676856,0.989334769731189,
0.989334769731189,0.989334769731189),(0.996968549833597,0.99168074676856,
0.989334769731189,0.989334769731189,0.989334769731189)))
REPRESENTATION_ITEM('')
SURFACE()
);
#2553=(
BOUNDED_SURFACE()
B_SPLINE_SURFACE(1,2,((#138130,#138131,#138132,#138133,#138134),(#138135,
#138136,#138137,#138138,#138139)),.UNSPECIFIED.,.F.,.F.,.F.)
B_SPLINE_SURFACE_WITH_KNOTS((2,2),(3,2,3),(0.,0.289807040991556),(0.211502584833923,
0.214285714285714,0.228987659635175),.UNSPECIFIED.)
GEOMETRIC_REPRESENTATION_ITEM()
RATIONAL_B_SPLINE_SURFACE(((0.99812231956923,0.999023095875655,1.,0.994839481491404,
0.99180331349328),(0.99812231956923,0.999023095875655,1.,0.994839481491404,
0.99180331349328)))
REPRESENTATION_ITEM('')
SURFACE()
);
#2554=(
BOUNDED_SURFACE()
B_SPLINE_SURFACE(1,2,((#138156,#138157,#138158,#138159,#138160),(#138161,
#138162,#138163,#138164,#138165)),.UNSPECIFIED.,.F.,.F.,.F.)
B_SPLINE_SURFACE_WITH_KNOTS((2,2),(3,2,3),(0.,0.290268982617608),(0.504616569534328,
0.521917529826141,0.522505428236512),.UNSPECIFIED.)
GEOMETRIC_REPRESENTATION_ITEM()
RATIONAL_B_SPLINE_SURFACE(((0.996968549833597,0.991680746768561,0.989334769731189,
0.989334769731189,0.989334769731189),(0.996968549833597,0.991680746768561,
0.989334769731189,0.989334769731189,0.989334769731189)))
REPRESENTATION_ITEM('')
SURFACE()
);
#2555=(
BOUNDED_SURFACE()
B_SPLINE_SURFACE(1,2,((#138173,#138174,#138175,#138176,#138177),(#138178,
#138179,#138180,#138181,#138182)),.UNSPECIFIED.,.F.,.F.,.F.)
B_SPLINE_SURFACE_WITH_KNOTS((2,2),(3,2,3),(0.,0.289807040991561),(0.21150258483406,
0.214285714285714,0.228987659635174),.UNSPECIFIED.)
GEOMETRIC_REPRESENTATION_ITEM()
RATIONAL_B_SPLINE_SURFACE(((0.998122319569319,0.999023095875703,1.,0.994839481491404,
0.99180331349328),(0.998122319569319,0.999023095875703,1.,0.994839481491404,
0.99180331349328)))
REPRESENTATION_ITEM('')
SURFACE()
);
#2556=(
BOUNDED_SURFACE()
B_SPLINE_SURFACE(1,2,((#138205,#138206,#138207,#138208,#138209),(#138210,
#138211,#138212,#138213,#138214)),.UNSPECIFIED.,.F.,.F.,.F.)
B_SPLINE_SURFACE_WITH_KNOTS((2,2),(3,2,3),(0.,0.290268982598661),(0.504616569534328,
0.521917529826141,0.522505428226585),.UNSPECIFIED.)
GEOMETRIC_REPRESENTATION_ITEM()
RATIONAL_B_SPLINE_SURFACE(((0.996968549833597,0.99168074676856,0.989334769731189,
0.989334769731189,0.989334769731189),(0.996968549833597,0.99168074676856,
0.989334769731189,0.989334769731189,0.989334769731189)))
REPRESENTATION_ITEM('')
SURFACE()
);
#2557=(
BOUNDED_SURFACE()
B_SPLINE_SURFACE(1,2,((#138216,#138217,#138218,#138219,#138220),(#138221,
#138222,#138223,#138224,#138225)),.UNSPECIFIED.,.F.,.F.,.F.)
B_SPLINE_SURFACE_WITH_KNOTS((2,2),(3,2,3),(0.,0.289807040993648),(0.211502584834061,
0.214285714285714,0.228987659635175),.UNSPECIFIED.)
GEOMETRIC_REPRESENTATION_ITEM()
RATIONAL_B_SPLINE_SURFACE(((0.99812231956932,0.999023095875703,1.,0.994839481491404,
0.99180331349328),(0.99812231956932,0.999023095875703,1.,0.994839481491404,
0.991803313493279)))
REPRESENTATION_ITEM('')
SURFACE()
);
#2558=(
BOUNDED_SURFACE()
B_SPLINE_SURFACE(1,2,((#138248,#138249,#138250,#138251,#138252),(#138253,
#138254,#138255,#138256,#138257)),.UNSPECIFIED.,.F.,.F.,.F.)
B_SPLINE_SURFACE_WITH_KNOTS((2,2),(3,2,3),(0.,0.290268982618429),(0.504616569534327,
0.521917529826142,0.522505428246144),.UNSPECIFIED.)
GEOMETRIC_REPRESENTATION_ITEM()
RATIONAL_B_SPLINE_SURFACE(((0.996968549833597,0.99168074676856,0.989334769731189,
0.989334769731189,0.989334769731189),(0.996968549833597,0.99168074676856,
0.989334769731189,0.989334769731189,0.989334769731189)))
REPRESENTATION_ITEM('')
SURFACE()
);
#2559=(
BOUNDED_SURFACE()
B_SPLINE_SURFACE(1,2,((#138259,#138260,#138261,#138262,#138263),(#138264,
#138265,#138266,#138267,#138268)),.UNSPECIFIED.,.F.,.F.,.F.)
B_SPLINE_SURFACE_WITH_KNOTS((2,2),(3,2,3),(0.,0.289807040992029),(0.211502584834065,
0.214285714285714,0.228987659635175),.UNSPECIFIED.)
GEOMETRIC_REPRESENTATION_ITEM()
RATIONAL_B_SPLINE_SURFACE(((0.998122319569323,0.999023095875705,1.,0.994839481491404,
0.991803313493279),(0.998122319569323,0.999023095875705,1.,0.994839481491404,
0.991803313493279)))
REPRESENTATION_ITEM('')
SURFACE()
);
#2560=(
BOUNDED_SURFACE()
B_SPLINE_SURFACE(1,2,((#138291,#138292,#138293,#138294,#138295),(#138296,
#138297,#138298,#138299,#138300)),.UNSPECIFIED.,.F.,.F.,.F.)
B_SPLINE_SURFACE_WITH_KNOTS((2,2),(3,2,3),(0.,0.290268982582821),(0.504616569534327,
0.52191752982614,0.522505428210736),.UNSPECIFIED.)
GEOMETRIC_REPRESENTATION_ITEM()
RATIONAL_B_SPLINE_SURFACE(((0.996968549833597,0.991680746768561,0.989334769731189,
0.989334769731189,0.989334769731189),(0.996968549833597,0.991680746768561,
0.989334769731189,0.989334769731189,0.989334769731189)))
REPRESENTATION_ITEM('')
SURFACE()
);
#2561=(
BOUNDED_SURFACE()
B_SPLINE_SURFACE(1,2,((#138302,#138303,#138304,#138305,#138306),(#138307,
#138308,#138309,#138310,#138311)),.UNSPECIFIED.,.F.,.F.,.F.)
B_SPLINE_SURFACE_WITH_KNOTS((2,2),(3,2,3),(0.,0.289807040991643),(0.211502584834065,
0.214285714285714,0.228987659635175),.UNSPECIFIED.)
GEOMETRIC_REPRESENTATION_ITEM()
RATIONAL_B_SPLINE_SURFACE(((0.998122319569323,0.999023095875705,1.,0.994839481491404,
0.991803313493279),(0.998122319569323,0.999023095875705,1.,0.994839481491404,
0.991803313493279)))
REPRESENTATION_ITEM('')
SURFACE()
);
#2562=(
BOUNDED_SURFACE()
B_SPLINE_SURFACE(1,2,((#138334,#138335,#138336,#138337,#138338),(#138339,
#138340,#138341,#138342,#138343)),.UNSPECIFIED.,.F.,.F.,.F.)
B_SPLINE_SURFACE_WITH_KNOTS((2,2),(3,2,3),(0.,0.290268982593328),(0.504616569534327,
0.521917529826142,0.522505428221249),.UNSPECIFIED.)
GEOMETRIC_REPRESENTATION_ITEM()
RATIONAL_B_SPLINE_SURFACE(((0.996968549833597,0.99168074676856,0.989334769731189,
0.989334769731189,0.989334769731189),(0.996968549833597,0.99168074676856,
0.989334769731189,0.989334769731189,0.989334769731189)))
REPRESENTATION_ITEM('')
SURFACE()
);
#2563=(
BOUNDED_SURFACE()
B_SPLINE_SURFACE(1,2,((#138345,#138346,#138347,#138348,#138349),(#138350,
#138351,#138352,#138353,#138354)),.UNSPECIFIED.,.F.,.F.,.F.)
B_SPLINE_SURFACE_WITH_KNOTS((2,2),(3,2,3),(0.,0.289807040991633),(0.211502584834064,
0.214285714285714,0.228987659635175),.UNSPECIFIED.)
GEOMETRIC_REPRESENTATION_ITEM()
RATIONAL_B_SPLINE_SURFACE(((0.998122319569322,0.999023095875704,1.,0.994839481491404,
0.991803313493279),(0.998122319569322,0.999023095875704,1.,0.994839481491404,
0.991803313493279)))
REPRESENTATION_ITEM('')
SURFACE()
);
#2564=(
BOUNDED_SURFACE()
B_SPLINE_SURFACE(1,2,((#138377,#138378,#138379,#138380,#138381),(#138382,
#138383,#138384,#138385,#138386)),.UNSPECIFIED.,.F.,.F.,.F.)
B_SPLINE_SURFACE_WITH_KNOTS((2,2),(3,2,3),(0.,0.290268982634772),(0.504616569534327,
0.521917529826142,0.522505428262693),.UNSPECIFIED.)
GEOMETRIC_REPRESENTATION_ITEM()
RATIONAL_B_SPLINE_SURFACE(((0.996968549833597,0.99168074676856,0.989334769731189,
0.989334769731189,0.989334769731189),(0.996968549833597,0.991680746768561,
0.989334769731189,0.989334769731189,0.989334769731189)))
REPRESENTATION_ITEM('')
SURFACE()
);
#2565=(
BOUNDED_SURFACE()
B_SPLINE_SURFACE(1,2,((#138388,#138389,#138390,#138391,#138392),(#138393,
#138394,#138395,#138396,#138397)),.UNSPECIFIED.,.F.,.F.,.F.)
B_SPLINE_SURFACE_WITH_KNOTS((2,2),(3,2,3),(0.,0.289807040991638),(0.211502584834065,
0.214285714285714,0.228987659635174),.UNSPECIFIED.)
GEOMETRIC_REPRESENTATION_ITEM()
RATIONAL_B_SPLINE_SURFACE(((0.998122319569323,0.999023095875705,1.,0.994839481491404,
0.99180331349328),(0.998122319569323,0.999023095875705,1.,0.994839481491404,
0.99180331349328)))
REPRESENTATION_ITEM('')
SURFACE()
);
#2566=(
BOUNDED_SURFACE()
B_SPLINE_SURFACE(1,2,((#138420,#138421,#138422,#138423,#138424),(#138425,
#138426,#138427,#138428,#138429)),.UNSPECIFIED.,.F.,.F.,.F.)
B_SPLINE_SURFACE_WITH_KNOTS((2,2),(3,2,3),(0.,0.290268982580509),(0.504616569534258,
0.521917529826143,0.522505428208433),.UNSPECIFIED.)
GEOMETRIC_REPRESENTATION_ITEM()
RATIONAL_B_SPLINE_SURFACE(((0.99696854983364,0.991680746768569,0.989334769731188,
0.989334769731188,0.989334769731188),(0.99696854983364,0.991680746768569,
0.989334769731188,0.989334769731188,0.989334769731188)))
REPRESENTATION_ITEM('')
SURFACE()
);
#2567=(
BOUNDED_SURFACE()
B_SPLINE_SURFACE(1,2,((#138431,#138432,#138433,#138434,#138435),(#138436,
#138437,#138438,#138439,#138440)),.UNSPECIFIED.,.F.,.F.,.F.)
B_SPLINE_SURFACE_WITH_KNOTS((2,2),(3,2,3),(0.,0.289807040991953),(0.211502584834065,
0.214285714285714,0.228987659634945),.UNSPECIFIED.)
GEOMETRIC_REPRESENTATION_ITEM()
RATIONAL_B_SPLINE_SURFACE(((0.998122319569323,0.999023095875705,1.,0.994839481491485,
0.991803313493374),(0.998122319569323,0.999023095875705,1.,0.994839481491485,
0.991803313493374)))
REPRESENTATION_ITEM('')
SURFACE()
);
#2568=(
BOUNDED_SURFACE()
B_SPLINE_SURFACE(1,2,((#138463,#138464,#138465,#138466,#138467),(#138468,
#138469,#138470,#138471,#138472)),.UNSPECIFIED.,.F.,.F.,.F.)
B_SPLINE_SURFACE_WITH_KNOTS((2,2),(3,2,3),(0.,0.290268982596918),(0.504616569534069,
0.52191752982614,0.522505428224833),.UNSPECIFIED.)
GEOMETRIC_REPRESENTATION_ITEM()
RATIONAL_B_SPLINE_SURFACE(((0.996968549833755,0.991680746768596,0.989334769731189,
0.989334769731189,0.989334769731189),(0.996968549833755,0.991680746768596,
0.989334769731189,0.989334769731189,0.989334769731189)))
REPRESENTATION_ITEM('')
SURFACE()
);
#2569=(
BOUNDED_SURFACE()
B_SPLINE_SURFACE(1,2,((#138474,#138475,#138476,#138477,#138478),(#138479,
#138480,#138481,#138482,#138483)),.UNSPECIFIED.,.F.,.F.,.F.)
B_SPLINE_SURFACE_WITH_KNOTS((2,2),(3,2,3),(0.,0.289807040991604),(0.211502584834065,
0.214285714285714,0.228987659635174),.UNSPECIFIED.)
GEOMETRIC_REPRESENTATION_ITEM()
RATIONAL_B_SPLINE_SURFACE(((0.998122319569323,0.999023095875705,1.,0.994839481491404,
0.99180331349328),(0.998122319569323,0.999023095875705,1.,0.994839481491404,
0.99180331349328)))
REPRESENTATION_ITEM('')
SURFACE()
);
#2570=(
BOUNDED_SURFACE()
B_SPLINE_SURFACE(1,2,((#138506,#138507,#138508,#138509,#138510),(#138511,
#138512,#138513,#138514,#138515)),.UNSPECIFIED.,.F.,.F.,.F.)
B_SPLINE_SURFACE_WITH_KNOTS((2,2),(3,2,3),(0.,0.290268982595245),(0.504616569533905,
0.52191752982614,0.52250542822317),.UNSPECIFIED.)
GEOMETRIC_REPRESENTATION_ITEM()
RATIONAL_B_SPLINE_SURFACE(((0.996968549833855,0.991680746768618,0.989334769731189,
0.989334769731189,0.989334769731189),(0.996968549833855,0.991680746768618,
0.989334769731189,0.989334769731189,0.989334769731189)))
REPRESENTATION_ITEM('')
SURFACE()
);
#2571=(
BOUNDED_SURFACE()
B_SPLINE_SURFACE(1,2,((#138529,#138530,#138531,#138532,#138533),(#138534,
#138535,#138536,#138537,#138538)),.UNSPECIFIED.,.F.,.F.,.F.)
B_SPLINE_SURFACE_WITH_KNOTS((2,2),(3,2,3),(0.,0.289807040991612),(0.211502584834063,
0.214285714285714,0.228987659635174),.UNSPECIFIED.)
GEOMETRIC_REPRESENTATION_ITEM()
RATIONAL_B_SPLINE_SURFACE(((0.998122319569321,0.999023095875704,1.,0.994839481491404,
0.99180331349328),(0.998122319569321,0.999023095875704,1.,0.994839481491404,
0.99180331349328)))
REPRESENTATION_ITEM('')
SURFACE()
);
#2572=(
BOUNDED_SURFACE()
B_SPLINE_SURFACE(1,2,((#138540,#138541,#138542,#138543,#138544),(#138545,
#138546,#138547,#138548,#138549)),.UNSPECIFIED.,.F.,.F.,.F.)
B_SPLINE_SURFACE_WITH_KNOTS((2,2),(3,2,3),(0.710192959008319,1.),(0.159729727643096,
0.159901408087482,0.177069452526135),.UNSPECIFIED.)
GEOMETRIC_REPRESENTATION_ITEM()
RATIONAL_B_SPLINE_SURFACE(((0.990889788836284,0.990889788836284,0.990889788836284,
0.987739559362111,0.987486127973996),(0.990889788836284,0.990889788836284,
0.990889788836284,0.987739559362111,0.987486127973996)))
REPRESENTATION_ITEM('')
SURFACE()
);
#2573=(
BOUNDED_SURFACE()
B_SPLINE_SURFACE(1,2,((#138560,#138561,#138562,#138563,#138564),(#138565,
#138566,#138567,#138568,#138569)),.UNSPECIFIED.,.F.,.F.,.F.)
B_SPLINE_SURFACE_WITH_KNOTS((2,2),(3,2,3),(0.710318915639718,1.),(0.556108173865714,
0.571428571428571,0.57365435021991),.UNSPECIFIED.)
GEOMETRIC_REPRESENTATION_ITEM()
RATIONAL_B_SPLINE_SURFACE(((0.991551633675927,0.994622399056525,1.,0.999218731101516,
0.99848615229188),(0.991551633675927,0.994622399056525,1.,0.999218731101516,
0.99848615229188)))
REPRESENTATION_ITEM('')
SURFACE()
);
#2574=(
BOUNDED_SURFACE()
B_SPLINE_SURFACE(1,2,((#138586,#138587,#138588,#138589,#138590),(#138591,
#138592,#138593,#138594,#138595)),.UNSPECIFIED.,.F.,.F.,.F.)
B_SPLINE_SURFACE_WITH_KNOTS((2,2),(3,2,3),(0.710192959008343,1.),(0.159729727643021,
0.159901408087408,0.177069452526135),.UNSPECIFIED.)
GEOMETRIC_REPRESENTATION_ITEM()
RATIONAL_B_SPLINE_SURFACE(((0.990889788836311,0.990889788836311,0.990889788836311,
0.987739559362112,0.987486127973996),(0.990889788836311,0.990889788836311,
0.990889788836311,0.987739559362112,0.987486127973996)))
REPRESENTATION_ITEM('')
SURFACE()
);
#2575=(
BOUNDED_SURFACE()
B_SPLINE_SURFACE(1,2,((#138603,#138604,#138605,#138606,#138607),(#138608,
#138609,#138610,#138611,#138612)),.UNSPECIFIED.,.F.,.F.,.F.)
B_SPLINE_SURFACE_WITH_KNOTS((2,2),(3,2,3),(0.710318915639972,1.),(0.556108173865714,
0.571428571428571,0.57365435021991),.UNSPECIFIED.)
GEOMETRIC_REPRESENTATION_ITEM()
RATIONAL_B_SPLINE_SURFACE(((0.991551633675927,0.994622399056525,1.,0.999218731101516,
0.99848615229188),(0.991551633675927,0.994622399056525,1.,0.999218731101516,
0.99848615229188)))
REPRESENTATION_ITEM('')
SURFACE()
);
#2576=(
BOUNDED_SURFACE()
B_SPLINE_SURFACE(1,2,((#138629,#138630,#138631,#138632,#138633),(#138634,
#138635,#138636,#138637,#138638)),.UNSPECIFIED.,.F.,.F.,.F.)
B_SPLINE_SURFACE_WITH_KNOTS((2,2),(3,2,3),(0.710192959008338,1.),(0.159729727643096,
0.159901408087482,0.177069452526135),.UNSPECIFIED.)
GEOMETRIC_REPRESENTATION_ITEM()
RATIONAL_B_SPLINE_SURFACE(((0.990889788836284,0.990889788836284,0.990889788836284,
0.987739559362111,0.987486127973996),(0.990889788836284,0.990889788836284,
0.990889788836284,0.987739559362111,0.987486127973996)))
REPRESENTATION_ITEM('')
SURFACE()
);
#2577=(
BOUNDED_SURFACE()
B_SPLINE_SURFACE(1,2,((#138646,#138647,#138648,#138649,#138650),(#138651,
#138652,#138653,#138654,#138655)),.UNSPECIFIED.,.F.,.F.,.F.)
B_SPLINE_SURFACE_WITH_KNOTS((2,2),(3,2,3),(0.710318915639015,1.),(0.556108173865714,
0.571428571428571,0.57365435021991),.UNSPECIFIED.)
GEOMETRIC_REPRESENTATION_ITEM()
RATIONAL_B_SPLINE_SURFACE(((0.991551633675927,0.994622399056525,1.,0.999218731101516,
0.99848615229188),(0.991551633675927,0.994622399056525,1.,0.999218731101516,
0.99848615229188)))
REPRESENTATION_ITEM('')
SURFACE()
);
#2578=(
BOUNDED_SURFACE()
B_SPLINE_SURFACE(1,2,((#138672,#138673,#138674,#138675,#138676),(#138677,
#138678,#138679,#138680,#138681)),.UNSPECIFIED.,.F.,.F.,.F.)
B_SPLINE_SURFACE_WITH_KNOTS((2,2),(3,2,3),(0.710192959007381,1.),(0.159729727643019,
0.159901408087406,0.177069452526135),.UNSPECIFIED.)
GEOMETRIC_REPRESENTATION_ITEM()
RATIONAL_B_SPLINE_SURFACE(((0.990889788836312,0.990889788836312,0.990889788836312,
0.987739559362112,0.987486127973996),(0.990889788836312,0.990889788836312,
0.990889788836312,0.987739559362112,0.987486127973996)))
REPRESENTATION_ITEM('')
SURFACE()
);
#2579=(
BOUNDED_SURFACE()
B_SPLINE_SURFACE(1,2,((#138689,#138690,#138691,#138692,#138693),(#138694,
#138695,#138696,#138697,#138698)),.UNSPECIFIED.,.F.,.F.,.F.)
B_SPLINE_SURFACE_WITH_KNOTS((2,2),(3,2,3),(0.710318915639014,1.),(0.556108173865714,
0.571428571428571,0.57365435021991),.UNSPECIFIED.)
GEOMETRIC_REPRESENTATION_ITEM()
RATIONAL_B_SPLINE_SURFACE(((0.991551633675927,0.994622399056525,1.,0.999218731101516,
0.99848615229188),(0.991551633675927,0.994622399056525,1.,0.999218731101516,
0.99848615229188)))
REPRESENTATION_ITEM('')
SURFACE()
);
#2580=(
BOUNDED_SURFACE()
B_SPLINE_SURFACE(1,2,((#138715,#138716,#138717,#138718,#138719),(#138720,
#138721,#138722,#138723,#138724)),.UNSPECIFIED.,.F.,.F.,.F.)
B_SPLINE_SURFACE_WITH_KNOTS((2,2),(3,2,3),(0.710192959007375,1.),(0.159729727643019,
0.159901408087406,0.177069452526135),.UNSPECIFIED.)
GEOMETRIC_REPRESENTATION_ITEM()
RATIONAL_B_SPLINE_SURFACE(((0.990889788836312,0.990889788836312,0.990889788836312,
0.987739559362112,0.987486127973996),(0.990889788836312,0.990889788836312,
0.990889788836312,0.987739559362112,0.987486127973996)))
REPRESENTATION_ITEM('')
SURFACE()
);
#2581=(
BOUNDED_SURFACE()
B_SPLINE_SURFACE(1,2,((#138732,#138733,#138734,#138735,#138736),(#138737,
#138738,#138739,#138740,#138741)),.UNSPECIFIED.,.F.,.F.,.F.)
B_SPLINE_SURFACE_WITH_KNOTS((2,2),(3,2,3),(0.710318915639014,1.),(0.556108173865714,
0.571428571428571,0.57365435021991),.UNSPECIFIED.)
GEOMETRIC_REPRESENTATION_ITEM()
RATIONAL_B_SPLINE_SURFACE(((0.991551633675927,0.994622399056525,1.,0.999218731101516,
0.99848615229188),(0.991551633675927,0.994622399056525,1.,0.999218731101516,
0.99848615229188)))
REPRESENTATION_ITEM('')
SURFACE()
);
#2582=(
BOUNDED_SURFACE()
B_SPLINE_SURFACE(1,2,((#138758,#138759,#138760,#138761,#138762),(#138763,
#138764,#138765,#138766,#138767)),.UNSPECIFIED.,.F.,.F.,.F.)
B_SPLINE_SURFACE_WITH_KNOTS((2,2),(3,2,3),(0.710192959007376,1.),(0.159729727643096,
0.159901408087482,0.177069452526135),.UNSPECIFIED.)
GEOMETRIC_REPRESENTATION_ITEM()
RATIONAL_B_SPLINE_SURFACE(((0.990889788836284,0.990889788836284,0.990889788836284,
0.987739559362111,0.987486127973996),(0.990889788836284,0.990889788836284,
0.990889788836284,0.987739559362111,0.987486127973996)))
REPRESENTATION_ITEM('')
SURFACE()
);
#2583=(
BOUNDED_SURFACE()
B_SPLINE_SURFACE(1,2,((#138775,#138776,#138777,#138778,#138779),(#138780,
#138781,#138782,#138783,#138784)),.UNSPECIFIED.,.F.,.F.,.F.)
B_SPLINE_SURFACE_WITH_KNOTS((2,2),(3,2,3),(0.710318915638436,1.),(0.556108173865714,
0.571428571428571,0.57365435021991),.UNSPECIFIED.)
GEOMETRIC_REPRESENTATION_ITEM()
RATIONAL_B_SPLINE_SURFACE(((0.991551633675927,0.994622399056525,1.,0.999218731101516,
0.99848615229188),(0.991551633675927,0.994622399056525,1.,0.999218731101516,
0.99848615229188)))
REPRESENTATION_ITEM('')
SURFACE()
);
#2584=(
BOUNDED_SURFACE()
B_SPLINE_SURFACE(1,2,((#138801,#138802,#138803,#138804,#138805),(#138806,
#138807,#138808,#138809,#138810)),.UNSPECIFIED.,.F.,.F.,.F.)
B_SPLINE_SURFACE_WITH_KNOTS((2,2),(3,2,3),(0.710192959006793,1.),(0.159729727643019,
0.159901408087406,0.177069452526135),.UNSPECIFIED.)
GEOMETRIC_REPRESENTATION_ITEM()
RATIONAL_B_SPLINE_SURFACE(((0.990889788836311,0.990889788836311,0.990889788836311,
0.987739559362112,0.987486127973996),(0.990889788836311,0.990889788836311,
0.990889788836311,0.987739559362112,0.987486127973996)))
REPRESENTATION_ITEM('')
SURFACE()
);
#2585=(
BOUNDED_SURFACE()
B_SPLINE_SURFACE(1,2,((#138818,#138819,#138820,#138821,#138822),(#138823,
#138824,#138825,#138826,#138827)),.UNSPECIFIED.,.F.,.F.,.F.)
B_SPLINE_SURFACE_WITH_KNOTS((2,2),(3,2,3),(0.710318915639023,1.),(0.556108173865714,
0.571428571428571,0.57365435021991),.UNSPECIFIED.)
GEOMETRIC_REPRESENTATION_ITEM()
RATIONAL_B_SPLINE_SURFACE(((0.991551633675927,0.994622399056525,1.,0.999218731101516,
0.99848615229188),(0.991551633675927,0.994622399056525,1.,0.999218731101516,
0.99848615229188)))
REPRESENTATION_ITEM('')
SURFACE()
);
#2586=(
BOUNDED_SURFACE()
B_SPLINE_SURFACE(1,2,((#138844,#138845,#138846,#138847,#138848),(#138849,
#138850,#138851,#138852,#138853)),.UNSPECIFIED.,.F.,.F.,.F.)
B_SPLINE_SURFACE_WITH_KNOTS((2,2),(3,2,3),(0.710192959007382,1.),(0.159729727643096,
0.159901408087482,0.177069452526135),.UNSPECIFIED.)
GEOMETRIC_REPRESENTATION_ITEM()
RATIONAL_B_SPLINE_SURFACE(((0.990889788836284,0.990889788836284,0.990889788836284,
0.987739559362111,0.987486127973996),(0.990889788836284,0.990889788836284,
0.990889788836284,0.987739559362111,0.987486127973996)))
REPRESENTATION_ITEM('')
SURFACE()
);
#2587=(
BOUNDED_SURFACE()
B_SPLINE_SURFACE(1,2,((#138861,#138862,#138863,#138864,#138865),(#138866,
#138867,#138868,#138869,#138870)),.UNSPECIFIED.,.F.,.F.,.F.)
B_SPLINE_SURFACE_WITH_KNOTS((2,2),(3,2,3),(0.710318915638469,1.),(0.556108173865714,
0.571428571428571,0.57365435021991),.UNSPECIFIED.)
GEOMETRIC_REPRESENTATION_ITEM()
RATIONAL_B_SPLINE_SURFACE(((0.991551633675927,0.994622399056525,1.,0.999218731101516,
0.99848615229188),(0.991551633675927,0.994622399056525,1.,0.999218731101516,
0.99848615229188)))
REPRESENTATION_ITEM('')
SURFACE()
);
#2588=(
BOUNDED_SURFACE()
B_SPLINE_SURFACE(1,2,((#138887,#138888,#138889,#138890,#138891),(#138892,
#138893,#138894,#138895,#138896)),.UNSPECIFIED.,.F.,.F.,.F.)
B_SPLINE_SURFACE_WITH_KNOTS((2,2),(3,2,3),(0.710192959006827,1.),(0.159729727643096,
0.159901408087482,0.177069452526135),.UNSPECIFIED.)
GEOMETRIC_REPRESENTATION_ITEM()
RATIONAL_B_SPLINE_SURFACE(((0.990889788836284,0.990889788836284,0.990889788836284,
0.987739559362111,0.987486127973996),(0.990889788836284,0.990889788836284,
0.990889788836284,0.987739559362111,0.987486127973996)))
REPRESENTATION_ITEM('')
SURFACE()
);
#2589=(
BOUNDED_SURFACE()
B_SPLINE_SURFACE(1,2,((#138904,#138905,#138906,#138907,#138908),(#138909,
#138910,#138911,#138912,#138913)),.UNSPECIFIED.,.F.,.F.,.F.)
B_SPLINE_SURFACE_WITH_KNOTS((2,2),(3,2,3),(0.710318915638963,1.),(0.556108173865715,
0.571428571428571,0.57365435021991),.UNSPECIFIED.)
GEOMETRIC_REPRESENTATION_ITEM()
RATIONAL_B_SPLINE_SURFACE(((0.991551633675927,0.994622399056526,1.,0.999218731101516,
0.99848615229188),(0.991551633675927,0.994622399056526,1.,0.999218731101516,
0.99848615229188)))
REPRESENTATION_ITEM('')
SURFACE()
);
#2590=(
BOUNDED_SURFACE()
B_SPLINE_SURFACE(1,2,((#138930,#138931,#138932,#138933,#138934),(#138935,
#138936,#138937,#138938,#138939)),.UNSPECIFIED.,.F.,.F.,.F.)
B_SPLINE_SURFACE_WITH_KNOTS((2,2),(3,2,3),(0.710192959007322,1.),(0.15972972764302,
0.159901408087407,0.177069452526134),.UNSPECIFIED.)
GEOMETRIC_REPRESENTATION_ITEM()
RATIONAL_B_SPLINE_SURFACE(((0.990889788836311,0.990889788836311,0.990889788836311,
0.987739559362112,0.987486127973996),(0.990889788836311,0.990889788836311,
0.990889788836311,0.987739559362112,0.987486127973996)))
REPRESENTATION_ITEM('')
SURFACE()
);
#2591=(
BOUNDED_SURFACE()
B_SPLINE_SURFACE(1,2,((#138947,#138948,#138949,#138950,#138951),(#138952,
#138953,#138954,#138955,#138956)),.UNSPECIFIED.,.F.,.F.,.F.)
B_SPLINE_SURFACE_WITH_KNOTS((2,2),(3,2,3),(0.710318915638946,1.),(0.556108173865715,
0.571428571428571,0.573654350219911),.UNSPECIFIED.)
GEOMETRIC_REPRESENTATION_ITEM()
RATIONAL_B_SPLINE_SURFACE(((0.991551633675927,0.994622399056526,1.,0.999218731101516,
0.99848615229188),(0.991551633675927,0.994622399056526,1.,0.999218731101516,
0.99848615229188)))
REPRESENTATION_ITEM('')
SURFACE()
);
#2592=(
BOUNDED_SURFACE()
B_SPLINE_SURFACE(1,2,((#138973,#138974,#138975,#138976,#138977),(#138978,
#138979,#138980,#138981,#138982)),.UNSPECIFIED.,.F.,.F.,.F.)
B_SPLINE_SURFACE_WITH_KNOTS((2,2),(3,2,3),(0.710192959007309,1.),(0.159729727643095,
0.159901408087481,0.177069452526134),.UNSPECIFIED.)
GEOMETRIC_REPRESENTATION_ITEM()
RATIONAL_B_SPLINE_SURFACE(((0.990889788836284,0.990889788836284,0.990889788836284,
0.987739559362111,0.987486127973996),(0.990889788836284,0.990889788836284,
0.990889788836284,0.987739559362111,0.987486127973996)))
REPRESENTATION_ITEM('')
SURFACE()
);
#2593=(
BOUNDED_SURFACE()
B_SPLINE_SURFACE(1,2,((#138990,#138991,#138992,#138993,#138994),(#138995,
#138996,#138997,#138998,#138999)),.UNSPECIFIED.,.F.,.F.,.F.)
B_SPLINE_SURFACE_WITH_KNOTS((2,2),(3,2,3),(0.710318915638348,1.),(0.556108173865715,
0.571428571428571,0.573654350219911),.UNSPECIFIED.)
GEOMETRIC_REPRESENTATION_ITEM()
RATIONAL_B_SPLINE_SURFACE(((0.991551633675927,0.994622399056526,1.,0.999218731101516,
0.99848615229188),(0.991551633675927,0.994622399056526,1.,0.999218731101516,
0.99848615229188)))
REPRESENTATION_ITEM('')
SURFACE()
);
#2594=(
BOUNDED_SURFACE()
B_SPLINE_SURFACE(1,2,((#139016,#139017,#139018,#139019,#139020),(#139021,
#139022,#139023,#139024,#139025)),.UNSPECIFIED.,.F.,.F.,.F.)
B_SPLINE_SURFACE_WITH_KNOTS((2,2),(3,2,3),(0.710192959006703,1.),(0.159729727643095,
0.159901408087481,0.177069452526134),.UNSPECIFIED.)
GEOMETRIC_REPRESENTATION_ITEM()
RATIONAL_B_SPLINE_SURFACE(((0.990889788836284,0.990889788836284,0.990889788836284,
0.987739559362111,0.987486127973996),(0.990889788836284,0.990889788836284,
0.990889788836284,0.987739559362111,0.987486127973996)))
REPRESENTATION_ITEM('')
SURFACE()
);
#2595=(
BOUNDED_SURFACE()
B_SPLINE_SURFACE(1,2,((#139033,#139034,#139035,#139036,#139037),(#139038,
#139039,#139040,#139041,#139042)),.UNSPECIFIED.,.F.,.F.,.F.)
B_SPLINE_SURFACE_WITH_KNOTS((2,2),(3,2,3),(0.710318915638935,1.),(0.556108173865715,
0.571428571428571,0.573654350219911),.UNSPECIFIED.)
GEOMETRIC_REPRESENTATION_ITEM()
RATIONAL_B_SPLINE_SURFACE(((0.991551633675927,0.994622399056526,1.,0.999218731101516,
0.99848615229188),(0.991551633675927,0.994622399056526,1.,0.999218731101516,
0.99848615229188)))
REPRESENTATION_ITEM('')
SURFACE()
);
#2596=(
BOUNDED_SURFACE()
B_SPLINE_SURFACE(1,2,((#139059,#139060,#139061,#139062,#139063),(#139064,
#139065,#139066,#139067,#139068)),.UNSPECIFIED.,.F.,.F.,.F.)
B_SPLINE_SURFACE_WITH_KNOTS((2,2),(3,2,3),(0.710192959007288,1.),(0.159729727643018,
0.159901408087405,0.177069452526134),.UNSPECIFIED.)
GEOMETRIC_REPRESENTATION_ITEM()
RATIONAL_B_SPLINE_SURFACE(((0.990889788836312,0.990889788836312,0.990889788836312,
0.987739559362112,0.987486127973996),(0.990889788836312,0.990889788836312,
0.990889788836312,0.987739559362112,0.987486127973996)))
REPRESENTATION_ITEM('')
SURFACE()
);
#2597=(
BOUNDED_SURFACE()
B_SPLINE_SURFACE(1,2,((#139076,#139077,#139078,#139079,#139080),(#139081,
#139082,#139083,#139084,#139085)),.UNSPECIFIED.,.F.,.F.,.F.)
B_SPLINE_SURFACE_WITH_KNOTS((2,2),(3,2,3),(0.710318915638428,1.),(0.556108173865715,
0.571428571428571,0.573654350219911),.UNSPECIFIED.)
GEOMETRIC_REPRESENTATION_ITEM()
RATIONAL_B_SPLINE_SURFACE(((0.991551633675927,0.994622399056526,1.,0.999218731101516,
0.99848615229188),(0.991551633675927,0.994622399056526,1.,0.999218731101516,
0.99848615229188)))
REPRESENTATION_ITEM('')
SURFACE()
);
#2598=(
BOUNDED_SURFACE()
B_SPLINE_SURFACE(1,2,((#139102,#139103,#139104,#139105,#139106),(#139107,
#139108,#139109,#139110,#139111)),.UNSPECIFIED.,.F.,.F.,.F.)
B_SPLINE_SURFACE_WITH_KNOTS((2,2),(3,2,3),(0.710192959006786,1.),(0.159729727643095,
0.159901408087481,0.177069452526134),.UNSPECIFIED.)
GEOMETRIC_REPRESENTATION_ITEM()
RATIONAL_B_SPLINE_SURFACE(((0.990889788836284,0.990889788836284,0.990889788836284,
0.987739559362111,0.987486127973996),(0.990889788836284,0.990889788836284,
0.990889788836284,0.987739559362111,0.987486127973996)))
REPRESENTATION_ITEM('')
SURFACE()
);
#2599=(
BOUNDED_SURFACE()
B_SPLINE_SURFACE(1,2,((#139119,#139120,#139121,#139122,#139123),(#139124,
#139125,#139126,#139127,#139128)),.UNSPECIFIED.,.F.,.F.,.F.)
B_SPLINE_SURFACE_WITH_KNOTS((2,2),(3,2,3),(0.710318915638931,1.),(0.556108173865715,
0.571428571428571,0.573654350219911),.UNSPECIFIED.)
GEOMETRIC_REPRESENTATION_ITEM()
RATIONAL_B_SPLINE_SURFACE(((0.991551633675927,0.994622399056526,1.,0.999218731101516,
0.99848615229188),(0.991551633675927,0.994622399056526,1.,0.999218731101516,
0.99848615229188)))
REPRESENTATION_ITEM('')
SURFACE()
);
#2600=(
BOUNDED_SURFACE()
B_SPLINE_SURFACE(1,2,((#139136,#139137,#139138,#139139,#139140),(#139141,
#139142,#139143,#139144,#139145)),.UNSPECIFIED.,.F.,.F.,.F.)
B_SPLINE_SURFACE_WITH_KNOTS((2,2),(3,2,3),(0.710192959007286,1.),(0.159729727643018,
0.159901408087405,0.177069452526134),.UNSPECIFIED.)
GEOMETRIC_REPRESENTATION_ITEM()
RATIONAL_B_SPLINE_SURFACE(((0.990889788836312,0.990889788836312,0.990889788836312,
0.987739559362112,0.987486127973996),(0.990889788836312,0.990889788836312,
0.990889788836312,0.987739559362112,0.987486127973996)))
REPRESENTATION_ITEM('')
SURFACE()
);
#2601=(
BOUNDED_SURFACE()
B_SPLINE_SURFACE(1,2,((#139147,#139148,#139149,#139150,#139151),(#139152,
#139153,#139154,#139155,#139156)),.UNSPECIFIED.,.F.,.F.,.F.)
B_SPLINE_SURFACE_WITH_KNOTS((2,2),(3,2,3),(0.710318915638446,1.),(0.556108173865715,
0.571428571428571,0.573654350219911),.UNSPECIFIED.)
GEOMETRIC_REPRESENTATION_ITEM()
RATIONAL_B_SPLINE_SURFACE(((0.991551633675927,0.994622399056526,1.,0.999218731101516,
0.99848615229188),(0.991551633675927,0.994622399056526,1.,0.999218731101516,
0.99848615229188)))
REPRESENTATION_ITEM('')
SURFACE()
);
#2602=(
BOUNDED_SURFACE()
B_SPLINE_SURFACE(1,2,((#139173,#139174,#139175,#139176,#139177),(#139178,
#139179,#139180,#139181,#139182)),.UNSPECIFIED.,.F.,.F.,.F.)
B_SPLINE_SURFACE_WITH_KNOTS((2,2),(3,2,3),(0.710192959006802,1.),(0.15972972764302,
0.159901408087407,0.177069452526134),.UNSPECIFIED.)
GEOMETRIC_REPRESENTATION_ITEM()
RATIONAL_B_SPLINE_SURFACE(((0.990889788836311,0.990889788836311,0.990889788836311,
0.987739559362112,0.987486127973996),(0.990889788836311,0.990889788836311,
0.990889788836311,0.987739559362112,0.987486127973996)))
REPRESENTATION_ITEM('')
SURFACE()
);
#2603=(
BOUNDED_SURFACE()
B_SPLINE_SURFACE(1,2,((#139190,#139191,#139192,#139193,#139194),(#139195,
#139196,#139197,#139198,#139199)),.UNSPECIFIED.,.F.,.F.,.F.)
B_SPLINE_SURFACE_WITH_KNOTS((2,2),(3,2,3),(0.710318915638684,1.),(0.556108173865715,
0.571428571428571,0.573654350219911),.UNSPECIFIED.)
GEOMETRIC_REPRESENTATION_ITEM()
RATIONAL_B_SPLINE_SURFACE(((0.991551633675927,0.994622399056526,1.,0.999218731101516,
0.99848615229188),(0.991551633675927,0.994622399056526,1.,0.999218731101516,
0.99848615229188)))
REPRESENTATION_ITEM('')
SURFACE()
);
#2604=(
BOUNDED_SURFACE()
B_SPLINE_SURFACE(1,2,((#139216,#139217,#139218,#139219,#139220),(#139221,
#139222,#139223,#139224,#139225)),.UNSPECIFIED.,.F.,.F.,.F.)
B_SPLINE_SURFACE_WITH_KNOTS((2,2),(3,2,3),(0.710192959007044,1.),(0.15972972764302,
0.159901408087407,0.177069452526134),.UNSPECIFIED.)
GEOMETRIC_REPRESENTATION_ITEM()
RATIONAL_B_SPLINE_SURFACE(((0.990889788836311,0.990889788836311,0.990889788836311,
0.987739559362112,0.987486127973996),(0.990889788836311,0.990889788836311,
0.990889788836311,0.987739559362112,0.987486127973996)))
REPRESENTATION_ITEM('')
SURFACE()
);
#2605=(
BOUNDED_SURFACE()
B_SPLINE_SURFACE(1,2,((#139233,#139234,#139235,#139236,#139237),(#139238,
#139239,#139240,#139241,#139242)),.UNSPECIFIED.,.F.,.F.,.F.)
B_SPLINE_SURFACE_WITH_KNOTS((2,2),(3,2,3),(0.710318915637618,1.),(0.556108173865715,
0.571428571428571,0.573654350219911),.UNSPECIFIED.)
GEOMETRIC_REPRESENTATION_ITEM()
RATIONAL_B_SPLINE_SURFACE(((0.991551633675927,0.994622399056526,1.,0.999218731101516,
0.99848615229188),(0.991551633675927,0.994622399056526,1.,0.999218731101516,
0.99848615229188)))
REPRESENTATION_ITEM('')
SURFACE()
);
#2606=(
BOUNDED_SURFACE()
B_SPLINE_SURFACE(1,2,((#139259,#139260,#139261,#139262,#139263),(#139264,
#139265,#139266,#139267,#139268)),.UNSPECIFIED.,.F.,.F.,.F.)
B_SPLINE_SURFACE_WITH_KNOTS((2,2),(3,2,3),(0.710192959005978,1.),(0.159729727643095,
0.159901408087481,0.177069452526134),.UNSPECIFIED.)
GEOMETRIC_REPRESENTATION_ITEM()
RATIONAL_B_SPLINE_SURFACE(((0.990889788836284,0.990889788836284,0.990889788836284,
0.987739559362111,0.987486127973996),(0.990889788836284,0.990889788836284,
0.990889788836284,0.987739559362111,0.987486127973996)))
REPRESENTATION_ITEM('')
SURFACE()
);
#2607=(
BOUNDED_SURFACE()
B_SPLINE_SURFACE(1,2,((#139276,#139277,#139278,#139279,#139280),(#139281,
#139282,#139283,#139284,#139285)),.UNSPECIFIED.,.F.,.F.,.F.)
B_SPLINE_SURFACE_WITH_KNOTS((2,2),(3,2,3),(0.710318915638879,1.),(0.556108173865715,
0.571428571428571,0.573654350219911),.UNSPECIFIED.)
GEOMETRIC_REPRESENTATION_ITEM()
RATIONAL_B_SPLINE_SURFACE(((0.991551633675927,0.994622399056526,1.,0.999218731101516,
0.99848615229188),(0.991551633675927,0.994622399056526,1.,0.999218731101516,
0.99848615229188)))
REPRESENTATION_ITEM('')
SURFACE()
);
#2608=(
BOUNDED_SURFACE()
B_SPLINE_SURFACE(1,2,((#139302,#139303,#139304,#139305,#139306),(#139307,
#139308,#139309,#139310,#139311)),.UNSPECIFIED.,.F.,.F.,.F.)
B_SPLINE_SURFACE_WITH_KNOTS((2,2),(3,2,3),(0.710192959007236,1.),(0.159729727642845,
0.159901408087234,0.177069452526135),.UNSPECIFIED.)
GEOMETRIC_REPRESENTATION_ITEM()
RATIONAL_B_SPLINE_SURFACE(((0.990889788836375,0.990889788836375,0.990889788836375,
0.987739559362115,0.987486127973996),(0.990889788836375,0.990889788836375,
0.990889788836375,0.987739559362115,0.987486127973996)))
REPRESENTATION_ITEM('')
SURFACE()
);
#2609=(
BOUNDED_SURFACE()
B_SPLINE_SURFACE(1,2,((#139319,#139320,#139321,#139322,#139323),(#139324,
#139325,#139326,#139327,#139328)),.UNSPECIFIED.,.F.,.F.,.F.)
B_SPLINE_SURFACE_WITH_KNOTS((2,2),(3,2,3),(0.710318915639,1.),(0.556108173865715,
0.571428571428571,0.573654350219911),.UNSPECIFIED.)
GEOMETRIC_REPRESENTATION_ITEM()
RATIONAL_B_SPLINE_SURFACE(((0.991551633675927,0.994622399056526,1.,0.999218731101516,
0.99848615229188),(0.991551633675927,0.994622399056526,1.,0.999218731101516,
0.99848615229188)))
REPRESENTATION_ITEM('')
SURFACE()
);
#2610=(
BOUNDED_SURFACE()
B_SPLINE_SURFACE(1,2,((#139345,#139346,#139347,#139348,#139349),(#139350,
#139351,#139352,#139353,#139354)),.UNSPECIFIED.,.F.,.F.,.F.)
B_SPLINE_SURFACE_WITH_KNOTS((2,2),(3,2,3),(0.710192959007357,1.),(0.159729727643095,
0.159901408087481,0.177069452526134),.UNSPECIFIED.)
GEOMETRIC_REPRESENTATION_ITEM()
RATIONAL_B_SPLINE_SURFACE(((0.990889788836284,0.990889788836284,0.990889788836284,
0.987739559362111,0.987486127973996),(0.990889788836284,0.990889788836284,
0.990889788836284,0.987739559362111,0.987486127973996)))
REPRESENTATION_ITEM('')
SURFACE()
);
#2611=(
BOUNDED_SURFACE()
B_SPLINE_SURFACE(1,2,((#139362,#139363,#139364,#139365,#139366),(#139367,
#139368,#139369,#139370,#139371)),.UNSPECIFIED.,.F.,.F.,.F.)
B_SPLINE_SURFACE_WITH_KNOTS((2,2),(3,2,3),(0.710318915638369,1.),(0.556108173865716,
0.571428571428571,0.573654350219912),.UNSPECIFIED.)
GEOMETRIC_REPRESENTATION_ITEM()
RATIONAL_B_SPLINE_SURFACE(((0.991551633675927,0.994622399056526,1.,0.999218731101515,
0.998486152291879),(0.991551633675927,0.994622399056526,1.,0.999218731101515,
0.998486152291879)))
REPRESENTATION_ITEM('')
SURFACE()
);
#2612=(
BOUNDED_SURFACE()
B_SPLINE_SURFACE(1,2,((#139388,#139389,#139390,#139391,#139392),(#139393,
#139394,#139395,#139396,#139397)),.UNSPECIFIED.,.F.,.F.,.F.)
B_SPLINE_SURFACE_WITH_KNOTS((2,2),(3,2,3),(0.710192959006723,1.),(0.159729727643025,
0.159901408087412,0.177069452526135),.UNSPECIFIED.)
GEOMETRIC_REPRESENTATION_ITEM()
RATIONAL_B_SPLINE_SURFACE(((0.99088978883631,0.99088978883631,0.99088978883631,
0.987739559362112,0.987486127973996),(0.99088978883631,0.99088978883631,
0.99088978883631,0.987739559362112,0.987486127973996)))
REPRESENTATION_ITEM('')
SURFACE()
);
#2613=(
BOUNDED_SURFACE()
B_SPLINE_SURFACE(1,2,((#139405,#139406,#139407,#139408,#139409),(#139410,
#139411,#139412,#139413,#139414)),.UNSPECIFIED.,.F.,.F.,.F.)
B_SPLINE_SURFACE_WITH_KNOTS((2,2),(3,2,3),(0.710318915639743,1.),(0.556108173865715,
0.571428571428571,0.573654350219911),.UNSPECIFIED.)
GEOMETRIC_REPRESENTATION_ITEM()
RATIONAL_B_SPLINE_SURFACE(((0.991551633675927,0.994622399056526,1.,0.999218731101516,
0.99848615229188),(0.991551633675927,0.994622399056526,1.,0.999218731101516,
0.99848615229188)))
REPRESENTATION_ITEM('')
SURFACE()
);
#2614=(
BOUNDED_SURFACE()
B_SPLINE_SURFACE(1,2,((#139431,#139432,#139433,#139434,#139435),(#139436,
#139437,#139438,#139439,#139440)),.UNSPECIFIED.,.F.,.F.,.F.)
B_SPLINE_SURFACE_WITH_KNOTS((2,2),(3,2,3),(0.710192959008268,1.),(0.159729727643095,
0.159901408087481,0.177069452526134),.UNSPECIFIED.)
GEOMETRIC_REPRESENTATION_ITEM()
RATIONAL_B_SPLINE_SURFACE(((0.990889788836284,0.990889788836284,0.990889788836284,
0.987739559362111,0.987486127973996),(0.990889788836284,0.990889788836284,
0.990889788836284,0.987739559362111,0.987486127973996)))
REPRESENTATION_ITEM('')
SURFACE()
);
#2615=(
BOUNDED_SURFACE()
B_SPLINE_SURFACE(1,2,((#139448,#139449,#139450,#139451,#139452),(#139453,
#139454,#139455,#139456,#139457)),.UNSPECIFIED.,.F.,.F.,.F.)
B_SPLINE_SURFACE_WITH_KNOTS((2,2),(3,2,3),(0.710318915638758,1.),(0.556108173865715,
0.571428571428571,0.573654350219911),.UNSPECIFIED.)
GEOMETRIC_REPRESENTATION_ITEM()
RATIONAL_B_SPLINE_SURFACE(((0.991551633675927,0.994622399056526,1.,0.999218731101516,
0.99848615229188),(0.991551633675927,0.994622399056526,1.,0.999218731101516,
0.99848615229188)))
REPRESENTATION_ITEM('')
SURFACE()
);
#2616=(
BOUNDED_SURFACE()
B_SPLINE_SURFACE(1,2,((#139474,#139475,#139476,#139477,#139478),(#139479,
#139480,#139481,#139482,#139483)),.UNSPECIFIED.,.F.,.F.,.F.)
B_SPLINE_SURFACE_WITH_KNOTS((2,2),(3,2,3),(0.710192959007121,1.),(0.159729727643082,
0.159901408087468,0.177069452526134),.UNSPECIFIED.)
GEOMETRIC_REPRESENTATION_ITEM()
RATIONAL_B_SPLINE_SURFACE(((0.990889788836289,0.990889788836289,0.990889788836289,
0.987739559362111,0.987486127973996),(0.990889788836289,0.990889788836289,
0.990889788836289,0.987739559362111,0.987486127973996)))
REPRESENTATION_ITEM('')
SURFACE()
);
#2617=(
BOUNDED_SURFACE()
B_SPLINE_SURFACE(1,2,((#139491,#139492,#139493,#139494,#139495),(#139496,
#139497,#139498,#139499,#139500)),.UNSPECIFIED.,.F.,.F.,.F.)
B_SPLINE_SURFACE_WITH_KNOTS((2,2),(3,2,3),(0.710318915638947,1.),(0.556108173865715,
0.571428571428571,0.573654350219911),.UNSPECIFIED.)
GEOMETRIC_REPRESENTATION_ITEM()
RATIONAL_B_SPLINE_SURFACE(((0.991551633675927,0.994622399056526,1.,0.999218731101516,
0.99848615229188),(0.991551633675927,0.994622399056526,1.,0.999218731101516,
0.99848615229188)))
REPRESENTATION_ITEM('')
SURFACE()
);
#2618=(
BOUNDED_SURFACE()
B_SPLINE_SURFACE(1,2,((#139517,#139518,#139519,#139520,#139521),(#139522,
#139523,#139524,#139525,#139526)),.UNSPECIFIED.,.F.,.F.,.F.)
B_SPLINE_SURFACE_WITH_KNOTS((2,2),(3,2,3),(0.710192959007308,1.),(0.159729727643095,
0.159901408087481,0.177069452526134),.UNSPECIFIED.)
GEOMETRIC_REPRESENTATION_ITEM()
RATIONAL_B_SPLINE_SURFACE(((0.990889788836284,0.990889788836284,0.990889788836284,
0.987739559362111,0.987486127973996),(0.990889788836284,0.990889788836284,
0.990889788836284,0.987739559362111,0.987486127973996)))
REPRESENTATION_ITEM('')
SURFACE()
);
#2619=(
BOUNDED_SURFACE()
B_SPLINE_SURFACE(1,2,((#139534,#139535,#139536,#139537,#139538),(#139539,
#139540,#139541,#139542,#139543)),.UNSPECIFIED.,.F.,.F.,.F.)
B_SPLINE_SURFACE_WITH_KNOTS((2,2),(3,2,3),(0.710318915637903,1.),(0.556108173865716,
0.571428571428571,0.573654350219911),.UNSPECIFIED.)
GEOMETRIC_REPRESENTATION_ITEM()
RATIONAL_B_SPLINE_SURFACE(((0.991551633675927,0.994622399056526,1.,0.999218731101516,
0.99848615229188),(0.991551633675927,0.994622399056526,1.,0.999218731101516,
0.99848615229188)))
REPRESENTATION_ITEM('')
SURFACE()
);
#2620=(
BOUNDED_SURFACE()
B_SPLINE_SURFACE(1,2,((#139560,#139561,#139562,#139563,#139564),(#139565,
#139566,#139567,#139568,#139569)),.UNSPECIFIED.,.F.,.F.,.F.)
B_SPLINE_SURFACE_WITH_KNOTS((2,2),(3,2,3),(0.710192959006264,1.),(0.15972972764307,
0.159901408087457,0.177069452526135),.UNSPECIFIED.)
GEOMETRIC_REPRESENTATION_ITEM()
RATIONAL_B_SPLINE_SURFACE(((0.990889788836293,0.990889788836293,0.990889788836293,
0.987739559362111,0.987486127973996),(0.990889788836293,0.990889788836293,
0.990889788836293,0.987739559362111,0.987486127973996)))
REPRESENTATION_ITEM('')
SURFACE()
);
#2621=(
BOUNDED_SURFACE()
B_SPLINE_SURFACE(1,2,((#139577,#139578,#139579,#139580,#139581),(#139582,
#139583,#139584,#139585,#139586)),.UNSPECIFIED.,.F.,.F.,.F.)
B_SPLINE_SURFACE_WITH_KNOTS((2,2),(3,2,3),(0.710318915639728,1.),(0.556108173865715,
0.571428571428571,0.573654350219911),.UNSPECIFIED.)
GEOMETRIC_REPRESENTATION_ITEM()
RATIONAL_B_SPLINE_SURFACE(((0.991551633675927,0.994622399056526,1.,0.999218731101516,
0.99848615229188),(0.991551633675927,0.994622399056526,1.,0.999218731101516,
0.99848615229188)))
REPRESENTATION_ITEM('')
SURFACE()
);
#2622=(
BOUNDED_SURFACE()
B_SPLINE_SURFACE(1,2,((#139603,#139604,#139605,#139606,#139607),(#139608,
#139609,#139610,#139611,#139612)),.UNSPECIFIED.,.F.,.F.,.F.)
B_SPLINE_SURFACE_WITH_KNOTS((2,2),(3,2,3),(0.710192959008098,1.),(0.159729727643095,
0.159901408087481,0.177069452526134),.UNSPECIFIED.)
GEOMETRIC_REPRESENTATION_ITEM()
RATIONAL_B_SPLINE_SURFACE(((0.990889788836284,0.990889788836284,0.990889788836284,
0.987739559362111,0.987486127973996),(0.990889788836284,0.990889788836284,
0.990889788836284,0.987739559362111,0.987486127973996)))
REPRESENTATION_ITEM('')
SURFACE()
);
#2623=(
BOUNDED_SURFACE()
B_SPLINE_SURFACE(1,2,((#139620,#139621,#139622,#139623,#139624),(#139625,
#139626,#139627,#139628,#139629)),.UNSPECIFIED.,.F.,.F.,.F.)
B_SPLINE_SURFACE_WITH_KNOTS((2,2),(3,2,3),(0.71031891563859,1.),(0.556108173865715,
0.571428571428571,0.573654350219927),.UNSPECIFIED.)
GEOMETRIC_REPRESENTATION_ITEM()
RATIONAL_B_SPLINE_SURFACE(((0.991551633675927,0.994622399056526,1.,0.99921873110151,
0.998486152291869),(0.991551633675927,0.994622399056526,1.,0.99921873110151,
0.998486152291869)))
REPRESENTATION_ITEM('')
SURFACE()
);
#2624=(
BOUNDED_SURFACE()
B_SPLINE_SURFACE(1,2,((#139646,#139647,#139648,#139649,#139650),(#139651,
#139652,#139653,#139654,#139655)),.UNSPECIFIED.,.F.,.F.,.F.)
B_SPLINE_SURFACE_WITH_KNOTS((2,2),(3,2,3),(0.710192959006948,1.),(0.159729727643096,
0.159901408087482,0.177069452526134),.UNSPECIFIED.)
GEOMETRIC_REPRESENTATION_ITEM()
RATIONAL_B_SPLINE_SURFACE(((0.990889788836284,0.990889788836284,0.990889788836284,
0.987739559362111,0.987486127973996),(0.990889788836284,0.990889788836284,
0.990889788836284,0.987739559362111,0.987486127973996)))
REPRESENTATION_ITEM('')
SURFACE()
);
#2625=(
BOUNDED_SURFACE()
B_SPLINE_SURFACE(1,2,((#139663,#139664,#139665,#139666,#139667),(#139668,
#139669,#139670,#139671,#139672)),.UNSPECIFIED.,.F.,.F.,.F.)
B_SPLINE_SURFACE_WITH_KNOTS((2,2),(3,2,3),(0.710318915639458,1.),(0.556108173865714,
0.571428571428571,0.57365435021991),.UNSPECIFIED.)
GEOMETRIC_REPRESENTATION_ITEM()
RATIONAL_B_SPLINE_SURFACE(((0.991551633675927,0.994622399056525,1.,0.999218731101516,
0.99848615229188),(0.991551633675927,0.994622399056525,1.,0.999218731101516,
0.99848615229188)))
REPRESENTATION_ITEM('')
SURFACE()
);
#2626=(
BOUNDED_SURFACE()
B_SPLINE_SURFACE(1,2,((#139689,#139690,#139691,#139692,#139693),(#139694,
#139695,#139696,#139697,#139698)),.UNSPECIFIED.,.F.,.F.,.F.)
B_SPLINE_SURFACE_WITH_KNOTS((2,2),(3,2,3),(0.710192959008439,1.),(0.159729727643019,
0.159901408087406,0.177069452526135),.UNSPECIFIED.)
GEOMETRIC_REPRESENTATION_ITEM()
RATIONAL_B_SPLINE_SURFACE(((0.990889788836312,0.990889788836312,0.990889788836312,
0.987739559362112,0.987486127973996),(0.990889788836312,0.990889788836312,
0.990889788836312,0.987739559362112,0.987486127973996)))
REPRESENTATION_ITEM('')
SURFACE()
);
#2627=(
BOUNDED_SURFACE()
B_SPLINE_SURFACE(1,2,((#139706,#139707,#139708,#139709,#139710),(#139711,
#139712,#139713,#139714,#139715)),.UNSPECIFIED.,.F.,.F.,.F.)
B_SPLINE_SURFACE_WITH_KNOTS((2,2),(3,2,3),(0.710318915639948,1.),(0.556108173865714,
0.571428571428571,0.57365435021991),.UNSPECIFIED.)
GEOMETRIC_REPRESENTATION_ITEM()
RATIONAL_B_SPLINE_SURFACE(((0.991551633675927,0.994622399056525,1.,0.999218731101516,
0.99848615229188),(0.991551633675927,0.994622399056525,1.,0.999218731101516,
0.99848615229188)))
REPRESENTATION_ITEM('')
SURFACE()
);
#2628=(
BOUNDED_SURFACE()
B_SPLINE_SURFACE(1,2,((#139732,#139733,#139734,#139735,#139736),(#139737,
#139738,#139739,#139740,#139741)),.UNSPECIFIED.,.F.,.F.,.F.)
B_SPLINE_SURFACE_WITH_KNOTS((2,2),(3,2,3),(0.710192959008305,1.),(0.159729727643019,
0.159901408087406,0.177069452526135),.UNSPECIFIED.)
GEOMETRIC_REPRESENTATION_ITEM()
RATIONAL_B_SPLINE_SURFACE(((0.990889788836311,0.990889788836311,0.990889788836311,
0.987739559362112,0.987486127973996),(0.990889788836311,0.990889788836311,
0.990889788836311,0.987739559362112,0.987486127973996)))
REPRESENTATION_ITEM('')
SURFACE()
);
#2629=(
BOUNDED_SURFACE()
B_SPLINE_SURFACE(1,2,((#139761,#139762,#139763,#139764,#139765),(#139766,
#139767,#139768,#139769,#139770)),.UNSPECIFIED.,.F.,.F.,.F.)
B_SPLINE_SURFACE_WITH_KNOTS((2,2),(3,2,3),(0.710318915639714,1.),(0.556108173865714,
0.571428571428571,0.57365435021991),.UNSPECIFIED.)
GEOMETRIC_REPRESENTATION_ITEM()
RATIONAL_B_SPLINE_SURFACE(((0.991551633675927,0.994622399056525,1.,0.999218731101516,
0.99848615229188),(0.991551633675927,0.994622399056525,1.,0.999218731101516,
0.99848615229188)))
REPRESENTATION_ITEM('')
SURFACE()
);
#2630=(
BOUNDED_SURFACE()
B_SPLINE_SURFACE(1,2,((#139772,#139773,#139774,#139775,#139776),(#139777,
#139778,#139779,#139780,#139781)),.UNSPECIFIED.,.F.,.F.,.F.)
B_SPLINE_SURFACE_WITH_KNOTS((2,2),(3,2,3),(0.70971070997379,1.),(0.194028469417326,
0.211502584834065,0.21211079066313),.UNSPECIFIED.)
GEOMETRIC_REPRESENTATION_ITEM()
RATIONAL_B_SPLINE_SURFACE(((0.989812124691679,0.992466718773227,0.998122319569323,
0.998122319569323,0.998122319569323),(0.989812124691679,0.992466718773227,
0.998122319569323,0.998122319569323,0.998122319569323)))
REPRESENTATION_ITEM('')
SURFACE()
);
#2631=(
BOUNDED_SURFACE()
B_SPLINE_SURFACE(1,2,((#139790,#139791,#139792),(#139793,#139794,#139795)),
 .UNSPECIFIED.,.F.,.F.,.F.)
B_SPLINE_SURFACE_WITH_KNOTS((2,2),(3,3),(0.710192959008376,1.),(0.52191752982614,
0.539102123117534),.UNSPECIFIED.)
GEOMETRIC_REPRESENTATION_ITEM()
RATIONAL_B_SPLINE_SURFACE(((0.989334769731189,0.987004571835916,0.987576759359605),
(0.989334769731189,0.987004571835916,0.987576759359605)))
REPRESENTATION_ITEM('')
SURFACE()
);
#2632=(
BOUNDED_SURFACE()
B_SPLINE_SURFACE(1,2,((#139804,#139805,#139806,#139807,#139808),(#139809,
#139810,#139811,#139812,#139813)),.UNSPECIFIED.,.F.,.F.,.F.)
B_SPLINE_SURFACE_WITH_KNOTS((2,2),(3,2,3),(0.709710709962227,1.),(0.194028469417326,
0.211502584834064,0.212110790674692),.UNSPECIFIED.)
GEOMETRIC_REPRESENTATION_ITEM()
RATIONAL_B_SPLINE_SURFACE(((0.989812124691679,0.992466718773227,0.998122319569322,
0.998122319569323,0.998122319569323),(0.989812124691679,0.992466718773227,
0.998122319569322,0.998122319569322,0.998122319569322)))
REPRESENTATION_ITEM('')
SURFACE()
);
#2633=(
BOUNDED_SURFACE()
B_SPLINE_SURFACE(1,2,((#139815,#139816,#139817),(#139818,#139819,#139820)),
 .UNSPECIFIED.,.F.,.F.,.F.)
B_SPLINE_SURFACE_WITH_KNOTS((2,2),(3,3),(0.710192959008442,1.),(0.521917529826125,
0.539102123117535),.UNSPECIFIED.)
GEOMETRIC_REPRESENTATION_ITEM()
RATIONAL_B_SPLINE_SURFACE(((0.989334769731193,0.987004571835915,0.987576759359605),
(0.989334769731193,0.987004571835915,0.987576759359605)))
REPRESENTATION_ITEM('')
SURFACE()
);
#2634=(
BOUNDED_SURFACE()
B_SPLINE_SURFACE(1,2,((#139829,#139830,#139831,#139832,#139833),(#139834,
#139835,#139836,#139837,#139838)),.UNSPECIFIED.,.F.,.F.,.F.)
B_SPLINE_SURFACE_WITH_KNOTS((2,2),(3,2,3),(0.709710709965086,1.),(0.194028469417325,
0.211502584834064,0.21211079067188),.UNSPECIFIED.)
GEOMETRIC_REPRESENTATION_ITEM()
RATIONAL_B_SPLINE_SURFACE(((0.989812124691679,0.992466718773227,0.998122319569322,
0.998122319569322,0.998122319569322),(0.989812124691679,0.992466718773227,
0.998122319569322,0.998122319569322,0.998122319569322)))
REPRESENTATION_ITEM('')
SURFACE()
);
#2635=(
BOUNDED_SURFACE()
B_SPLINE_SURFACE(1,2,((#139840,#139841,#139842),(#139843,#139844,#139845)),
 .UNSPECIFIED.,.F.,.F.,.F.)
B_SPLINE_SURFACE_WITH_KNOTS((2,2),(3,3),(0.71019295900844,1.),(0.521917529826117,
0.539102123117535),.UNSPECIFIED.)
GEOMETRIC_REPRESENTATION_ITEM()
RATIONAL_B_SPLINE_SURFACE(((0.989334769731195,0.987004571835915,0.987576759359605),
(0.989334769731195,0.987004571835915,0.987576759359605)))
REPRESENTATION_ITEM('')
SURFACE()
);
#2636=(
BOUNDED_SURFACE()
B_SPLINE_SURFACE(1,2,((#139854,#139855,#139856,#139857,#139858),(#139859,
#139860,#139861,#139862,#139863)),.UNSPECIFIED.,.F.,.F.,.F.)
B_SPLINE_SURFACE_WITH_KNOTS((2,2),(3,2,3),(0.70971070997195,1.),(0.194028469417325,
0.211502584834064,0.212110790665034),.UNSPECIFIED.)
GEOMETRIC_REPRESENTATION_ITEM()
RATIONAL_B_SPLINE_SURFACE(((0.989812124691679,0.992466718773227,0.998122319569322,
0.998122319569322,0.998122319569322),(0.989812124691679,0.992466718773227,
0.998122319569322,0.998122319569322,0.998122319569322)))
REPRESENTATION_ITEM('')
SURFACE()
);
#2637=(
BOUNDED_SURFACE()
B_SPLINE_SURFACE(1,2,((#139865,#139866,#139867),(#139868,#139869,#139870)),
 .UNSPECIFIED.,.F.,.F.,.F.)
B_SPLINE_SURFACE_WITH_KNOTS((2,2),(3,3),(0.710192959008441,1.),(0.521917529826141,
0.539102123117535),.UNSPECIFIED.)
GEOMETRIC_REPRESENTATION_ITEM()
RATIONAL_B_SPLINE_SURFACE(((0.989334769731189,0.987004571835916,0.987576759359605),
(0.989334769731189,0.987004571835916,0.987576759359605)))
REPRESENTATION_ITEM('')
SURFACE()
);
#2638=(
BOUNDED_SURFACE()
B_SPLINE_SURFACE(1,2,((#139879,#139880,#139881,#139882,#139883),(#139884,
#139885,#139886,#139887,#139888)),.UNSPECIFIED.,.F.,.F.,.F.)
B_SPLINE_SURFACE_WITH_KNOTS((2,2),(3,2,3),(0.709710709990175,1.),(0.194028469417325,
0.211502584834064,0.212110790646804),.UNSPECIFIED.)
GEOMETRIC_REPRESENTATION_ITEM()
RATIONAL_B_SPLINE_SURFACE(((0.989812124691679,0.992466718773227,0.998122319569322,
0.998122319569322,0.998122319569322),(0.989812124691679,0.992466718773227,
0.998122319569322,0.998122319569322,0.998122319569322)))
REPRESENTATION_ITEM('')
SURFACE()
);
#2639=(
BOUNDED_SURFACE()
B_SPLINE_SURFACE(1,2,((#139890,#139891,#139892),(#139893,#139894,#139895)),
 .UNSPECIFIED.,.F.,.F.,.F.)
B_SPLINE_SURFACE_WITH_KNOTS((2,2),(3,3),(0.710192959008441,1.),(0.52191752982614,
0.539102123117535),.UNSPECIFIED.)
GEOMETRIC_REPRESENTATION_ITEM()
RATIONAL_B_SPLINE_SURFACE(((0.989334769731189,0.987004571835916,0.987576759359605),
(0.989334769731189,0.987004571835916,0.987576759359605)))
REPRESENTATION_ITEM('')
SURFACE()
);
#2640=(
BOUNDED_SURFACE()
B_SPLINE_SURFACE(1,2,((#139904,#139905,#139906,#139907,#139908),(#139909,
#139910,#139911,#139912,#139913)),.UNSPECIFIED.,.F.,.F.,.F.)
B_SPLINE_SURFACE_WITH_KNOTS((2,2),(3,2,3),(0.709710709979902,1.),(0.194028469417325,
0.211502584834064,0.21211079065708),.UNSPECIFIED.)
GEOMETRIC_REPRESENTATION_ITEM()
RATIONAL_B_SPLINE_SURFACE(((0.989812124691679,0.992466718773227,0.998122319569322,
0.998122319569322,0.998122319569322),(0.989812124691679,0.992466718773227,
0.998122319569322,0.998122319569322,0.998122319569322)))
REPRESENTATION_ITEM('')
SURFACE()
);
#2641=(
BOUNDED_SURFACE()
B_SPLINE_SURFACE(1,2,((#139915,#139916,#139917),(#139918,#139919,#139920)),
 .UNSPECIFIED.,.F.,.F.,.F.)
B_SPLINE_SURFACE_WITH_KNOTS((2,2),(3,3),(0.710192959008441,1.),(0.521917529826141,
0.539102123117535),.UNSPECIFIED.)
GEOMETRIC_REPRESENTATION_ITEM()
RATIONAL_B_SPLINE_SURFACE(((0.989334769731189,0.987004571835916,0.987576759359605),
(0.989334769731189,0.987004571835916,0.987576759359605)))
REPRESENTATION_ITEM('')
SURFACE()
);
#2642=(
BOUNDED_SURFACE()
B_SPLINE_SURFACE(1,2,((#139929,#139930,#139931,#139932,#139933),(#139934,
#139935,#139936,#139937,#139938)),.UNSPECIFIED.,.F.,.F.,.F.)
B_SPLINE_SURFACE_WITH_KNOTS((2,2),(3,2,3),(0.709710709965924,1.),(0.194028469417325,
0.211502584834064,0.21211079067106),.UNSPECIFIED.)
GEOMETRIC_REPRESENTATION_ITEM()
RATIONAL_B_SPLINE_SURFACE(((0.989812124691679,0.992466718773227,0.998122319569322,
0.998122319569322,0.998122319569322),(0.989812124691679,0.992466718773227,
0.998122319569322,0.998122319569322,0.998122319569322)))
REPRESENTATION_ITEM('')
SURFACE()
);
#2643=(
BOUNDED_SURFACE()
B_SPLINE_SURFACE(1,2,((#139940,#139941,#139942),(#139943,#139944,#139945)),
 .UNSPECIFIED.,.F.,.F.,.F.)
B_SPLINE_SURFACE_WITH_KNOTS((2,2),(3,3),(0.710192959008442,1.),(0.521917529826113,
0.539102123117535),.UNSPECIFIED.)
GEOMETRIC_REPRESENTATION_ITEM()
RATIONAL_B_SPLINE_SURFACE(((0.989334769731196,0.987004571835915,0.987576759359605),
(0.989334769731196,0.987004571835915,0.987576759359605)))
REPRESENTATION_ITEM('')
SURFACE()
);
#2644=(
BOUNDED_SURFACE()
B_SPLINE_SURFACE(1,2,((#139954,#139955,#139956,#139957,#139958),(#139959,
#139960,#139961,#139962,#139963)),.UNSPECIFIED.,.F.,.F.,.F.)
B_SPLINE_SURFACE_WITH_KNOTS((2,2),(3,2,3),(0.710051238894138,1.),(0.194028469417325,
0.211502584834064,0.211770261742845),.UNSPECIFIED.)
GEOMETRIC_REPRESENTATION_ITEM()
RATIONAL_B_SPLINE_SURFACE(((0.989812124691679,0.992466718773227,0.998122319569322,
0.998122319569322,0.998122319569322),(0.989812124691679,0.992466718773227,
0.998122319569322,0.998122319569322,0.998122319569322)))
REPRESENTATION_ITEM('')
SURFACE()
);
#2645=(
BOUNDED_SURFACE()
B_SPLINE_SURFACE(1,2,((#139965,#139966,#139967),(#139968,#139969,#139970)),
 .UNSPECIFIED.,.F.,.F.,.F.)
B_SPLINE_SURFACE_WITH_KNOTS((2,2),(3,3),(0.710192959008442,1.),(0.521917529826141,
0.539102123117535),.UNSPECIFIED.)
GEOMETRIC_REPRESENTATION_ITEM()
RATIONAL_B_SPLINE_SURFACE(((0.989334769731189,0.987004571835916,0.987576759359605),
(0.989334769731189,0.987004571835916,0.987576759359605)))
REPRESENTATION_ITEM('')
SURFACE()
);
#2646=(
BOUNDED_SURFACE()
B_SPLINE_SURFACE(1,2,((#139979,#139980,#139981,#139982,#139983),(#139984,
#139985,#139986,#139987,#139988)),.UNSPECIFIED.,.F.,.F.,.F.)
B_SPLINE_SURFACE_WITH_KNOTS((2,2),(3,2,3),(0.709710709982408,1.),(0.194028469417325,
0.211502584834064,0.212110790654572),.UNSPECIFIED.)
GEOMETRIC_REPRESENTATION_ITEM()
RATIONAL_B_SPLINE_SURFACE(((0.989812124691679,0.992466718773227,0.998122319569322,
0.998122319569322,0.998122319569322),(0.989812124691679,0.992466718773227,
0.998122319569322,0.998122319569322,0.998122319569322)))
REPRESENTATION_ITEM('')
SURFACE()
);
#2647=(
BOUNDED_SURFACE()
B_SPLINE_SURFACE(1,2,((#139990,#139991,#139992),(#139993,#139994,#139995)),
 .UNSPECIFIED.,.F.,.F.,.F.)
B_SPLINE_SURFACE_WITH_KNOTS((2,2),(3,3),(0.710192959008443,1.),(0.521917529826141,
0.539102123117535),.UNSPECIFIED.)
GEOMETRIC_REPRESENTATION_ITEM()
RATIONAL_B_SPLINE_SURFACE(((0.989334769731189,0.987004571835916,0.987576759359605),
(0.989334769731189,0.987004571835916,0.987576759359605)))
REPRESENTATION_ITEM('')
SURFACE()
);
#2648=(
BOUNDED_SURFACE()
B_SPLINE_SURFACE(1,2,((#140004,#140005,#140006,#140007,#140008),(#140009,
#140010,#140011,#140012,#140013)),.UNSPECIFIED.,.F.,.F.,.F.)
B_SPLINE_SURFACE_WITH_KNOTS((2,2),(3,2,3),(0.709710709998254,1.),(0.194028469417325,
0.211502584834064,0.212110790638721),.UNSPECIFIED.)
GEOMETRIC_REPRESENTATION_ITEM()
RATIONAL_B_SPLINE_SURFACE(((0.989812124691679,0.992466718773227,0.998122319569322,
0.998122319569322,0.998122319569322),(0.989812124691679,0.992466718773227,
0.998122319569322,0.998122319569322,0.998122319569322)))
REPRESENTATION_ITEM('')
SURFACE()
);
#2649=(
BOUNDED_SURFACE()
B_SPLINE_SURFACE(1,2,((#140015,#140016,#140017),(#140018,#140019,#140020)),
 .UNSPECIFIED.,.F.,.F.,.F.)
B_SPLINE_SURFACE_WITH_KNOTS((2,2),(3,3),(0.710192959008444,1.),(0.521917529826137,
0.539102123117535),.UNSPECIFIED.)
GEOMETRIC_REPRESENTATION_ITEM()
RATIONAL_B_SPLINE_SURFACE(((0.98933476973119,0.987004571835916,0.987576759359605),
(0.98933476973119,0.987004571835916,0.987576759359605)))
REPRESENTATION_ITEM('')
SURFACE()
);
#2650=(
BOUNDED_SURFACE()
B_SPLINE_SURFACE(1,2,((#140029,#140030,#140031,#140032,#140033),(#140034,
#140035,#140036,#140037,#140038)),.UNSPECIFIED.,.F.,.F.,.F.)
B_SPLINE_SURFACE_WITH_KNOTS((2,2),(3,2,3),(0.709710709967905,1.),(0.194028469417325,
0.211502584834064,0.212110790669077),.UNSPECIFIED.)
GEOMETRIC_REPRESENTATION_ITEM()
RATIONAL_B_SPLINE_SURFACE(((0.989812124691679,0.992466718773227,0.998122319569322,
0.998122319569322,0.998122319569322),(0.989812124691679,0.992466718773227,
0.998122319569322,0.998122319569322,0.998122319569322)))
REPRESENTATION_ITEM('')
SURFACE()
);
#2651=(
BOUNDED_SURFACE()
B_SPLINE_SURFACE(1,2,((#140040,#140041,#140042),(#140043,#140044,#140045)),
 .UNSPECIFIED.,.F.,.F.,.F.)
B_SPLINE_SURFACE_WITH_KNOTS((2,2),(3,3),(0.71019295900844,1.),(0.521917529826141,
0.539102123117535),.UNSPECIFIED.)
GEOMETRIC_REPRESENTATION_ITEM()
RATIONAL_B_SPLINE_SURFACE(((0.989334769731189,0.987004571835916,0.987576759359605),
(0.989334769731189,0.987004571835916,0.987576759359605)))
REPRESENTATION_ITEM('')
SURFACE()
);
#2652=(
BOUNDED_SURFACE()
B_SPLINE_SURFACE(1,2,((#140054,#140055,#140056,#140057,#140058),(#140059,
#140060,#140061,#140062,#140063)),.UNSPECIFIED.,.F.,.F.,.F.)
B_SPLINE_SURFACE_WITH_KNOTS((2,2),(3,2,3),(0.709710709971499,1.),(0.194028469417325,
0.211502584834064,0.212110790665475),.UNSPECIFIED.)
GEOMETRIC_REPRESENTATION_ITEM()
RATIONAL_B_SPLINE_SURFACE(((0.989812124691679,0.992466718773227,0.998122319569322,
0.998122319569322,0.998122319569322),(0.989812124691679,0.992466718773227,
0.998122319569322,0.998122319569322,0.998122319569322)))
REPRESENTATION_ITEM('')
SURFACE()
);
#2653=(
BOUNDED_SURFACE()
B_SPLINE_SURFACE(1,2,((#140065,#140066,#140067),(#140068,#140069,#140070)),
 .UNSPECIFIED.,.F.,.F.,.F.)
B_SPLINE_SURFACE_WITH_KNOTS((2,2),(3,3),(0.710192959008441,1.),(0.521917529826102,
0.539102123117535),.UNSPECIFIED.)
GEOMETRIC_REPRESENTATION_ITEM()
RATIONAL_B_SPLINE_SURFACE(((0.989334769731199,0.987004571835914,0.987576759359605),
(0.989334769731199,0.987004571835914,0.987576759359605)))
REPRESENTATION_ITEM('')
SURFACE()
);
#2654=(
BOUNDED_SURFACE()
B_SPLINE_SURFACE(1,2,((#140079,#140080,#140081,#140082,#140083),(#140084,
#140085,#140086,#140087,#140088)),.UNSPECIFIED.,.F.,.F.,.F.)
B_SPLINE_SURFACE_WITH_KNOTS((2,2),(3,2,3),(0.709710709957041,1.),(0.194028469417325,
0.211502584834064,0.212110790679937),.UNSPECIFIED.)
GEOMETRIC_REPRESENTATION_ITEM()
RATIONAL_B_SPLINE_SURFACE(((0.989812124691679,0.992466718773227,0.998122319569322,
0.998122319569322,0.998122319569322),(0.989812124691679,0.992466718773227,
0.998122319569322,0.998122319569322,0.998122319569322)))
REPRESENTATION_ITEM('')
SURFACE()
);
#2655=(
BOUNDED_SURFACE()
B_SPLINE_SURFACE(1,2,((#140090,#140091,#140092),(#140093,#140094,#140095)),
 .UNSPECIFIED.,.F.,.F.,.F.)
B_SPLINE_SURFACE_WITH_KNOTS((2,2),(3,3),(0.710192959008445,1.),(0.521917529826141,
0.539102123117535),.UNSPECIFIED.)
GEOMETRIC_REPRESENTATION_ITEM()
RATIONAL_B_SPLINE_SURFACE(((0.989334769731189,0.987004571835916,0.987576759359605),
(0.989334769731189,0.987004571835916,0.987576759359605)))
REPRESENTATION_ITEM('')
SURFACE()
);
#2656=(
BOUNDED_SURFACE()
B_SPLINE_SURFACE(1,2,((#140104,#140105,#140106,#140107,#140108),(#140109,
#140110,#140111,#140112,#140113)),.UNSPECIFIED.,.F.,.F.,.F.)
B_SPLINE_SURFACE_WITH_KNOTS((2,2),(3,2,3),(0.70971070996417,1.),(0.194028469417325,
0.211502584834064,0.212110790672805),.UNSPECIFIED.)
GEOMETRIC_REPRESENTATION_ITEM()
RATIONAL_B_SPLINE_SURFACE(((0.989812124691679,0.992466718773227,0.998122319569322,
0.998122319569322,0.998122319569322),(0.989812124691679,0.992466718773227,
0.998122319569322,0.998122319569322,0.998122319569322)))
REPRESENTATION_ITEM('')
SURFACE()
);
#2657=(
BOUNDED_SURFACE()
B_SPLINE_SURFACE(1,2,((#140115,#140116,#140117),(#140118,#140119,#140120)),
 .UNSPECIFIED.,.F.,.F.,.F.)
B_SPLINE_SURFACE_WITH_KNOTS((2,2),(3,3),(0.710192959008445,1.),(0.521917529826141,
0.539102123117535),.UNSPECIFIED.)
GEOMETRIC_REPRESENTATION_ITEM()
RATIONAL_B_SPLINE_SURFACE(((0.989334769731189,0.987004571835916,0.987576759359605),
(0.989334769731189,0.987004571835916,0.987576759359605)))
REPRESENTATION_ITEM('')
SURFACE()
);
#2658=(
BOUNDED_SURFACE()
B_SPLINE_SURFACE(1,2,((#140129,#140130,#140131,#140132,#140133),(#140134,
#140135,#140136,#140137,#140138)),.UNSPECIFIED.,.F.,.F.,.F.)
B_SPLINE_SURFACE_WITH_KNOTS((2,2),(3,2,3),(0.709710709982169,1.),(0.194028469417325,
0.211502584834064,0.212110790654813),.UNSPECIFIED.)
GEOMETRIC_REPRESENTATION_ITEM()
RATIONAL_B_SPLINE_SURFACE(((0.989812124691679,0.992466718773227,0.998122319569322,
0.998122319569322,0.998122319569322),(0.989812124691679,0.992466718773227,
0.998122319569322,0.998122319569322,0.998122319569322)))
REPRESENTATION_ITEM('')
SURFACE()
);
#2659=(
BOUNDED_SURFACE()
B_SPLINE_SURFACE(1,2,((#140140,#140141,#140142),(#140143,#140144,#140145)),
 .UNSPECIFIED.,.F.,.F.,.F.)
B_SPLINE_SURFACE_WITH_KNOTS((2,2),(3,3),(0.710192959008441,1.),(0.521917529826049,
0.539102123117536),.UNSPECIFIED.)
GEOMETRIC_REPRESENTATION_ITEM()
RATIONAL_B_SPLINE_SURFACE(((0.989334769731214,0.987004571835913,0.987576759359605),
(0.989334769731214,0.987004571835913,0.987576759359605)))
REPRESENTATION_ITEM('')
SURFACE()
);
#2660=(
BOUNDED_SURFACE()
B_SPLINE_SURFACE(1,2,((#140154,#140155,#140156,#140157,#140158),(#140159,
#140160,#140161,#140162,#140163)),.UNSPECIFIED.,.F.,.F.,.F.)
B_SPLINE_SURFACE_WITH_KNOTS((2,2),(3,2,3),(0.709710709986515,1.),(0.194028469417325,
0.211502584834064,0.212110790650462),.UNSPECIFIED.)
GEOMETRIC_REPRESENTATION_ITEM()
RATIONAL_B_SPLINE_SURFACE(((0.989812124691679,0.992466718773227,0.998122319569322,
0.998122319569322,0.998122319569322),(0.989812124691679,0.992466718773227,
0.998122319569322,0.998122319569322,0.998122319569322)))
REPRESENTATION_ITEM('')
SURFACE()
);
#2661=(
BOUNDED_SURFACE()
B_SPLINE_SURFACE(1,2,((#140165,#140166,#140167),(#140168,#140169,#140170)),
 .UNSPECIFIED.,.F.,.F.,.F.)
B_SPLINE_SURFACE_WITH_KNOTS((2,2),(3,3),(0.71019295900844,1.),(0.521917529825981,
0.539102123117536),.UNSPECIFIED.)
GEOMETRIC_REPRESENTATION_ITEM()
RATIONAL_B_SPLINE_SURFACE(((0.989334769731232,0.98700457183591,0.987576759359605),
(0.989334769731232,0.98700457183591,0.987576759359605)))
REPRESENTATION_ITEM('')
SURFACE()
);
#2662=(
BOUNDED_SURFACE()
B_SPLINE_SURFACE(1,2,((#140179,#140180,#140181,#140182,#140183),(#140184,
#140185,#140186,#140187,#140188)),.UNSPECIFIED.,.F.,.F.,.F.)
B_SPLINE_SURFACE_WITH_KNOTS((2,2),(3,2,3),(0.709710709987791,1.),(0.194028469417325,
0.211502584834064,0.212110790649188),.UNSPECIFIED.)
GEOMETRIC_REPRESENTATION_ITEM()
RATIONAL_B_SPLINE_SURFACE(((0.989812124691679,0.992466718773227,0.998122319569322,
0.998122319569322,0.998122319569322),(0.989812124691679,0.992466718773227,
0.998122319569322,0.998122319569322,0.998122319569322)))
REPRESENTATION_ITEM('')
SURFACE()
);
#2663=(
BOUNDED_SURFACE()
B_SPLINE_SURFACE(1,2,((#140190,#140191,#140192),(#140193,#140194,#140195)),
 .UNSPECIFIED.,.F.,.F.,.F.)
B_SPLINE_SURFACE_WITH_KNOTS((2,2),(3,3),(0.710192959008445,1.),(0.521917529826041,
0.539102123117536),.UNSPECIFIED.)
GEOMETRIC_REPRESENTATION_ITEM()
RATIONAL_B_SPLINE_SURFACE(((0.989334769731216,0.987004571835912,0.987576759359605),
(0.989334769731216,0.987004571835912,0.987576759359605)))
REPRESENTATION_ITEM('')
SURFACE()
);
#2664=(
BOUNDED_SURFACE()
B_SPLINE_SURFACE(1,2,((#140204,#140205,#140206,#140207,#140208),(#140209,
#140210,#140211,#140212,#140213)),.UNSPECIFIED.,.F.,.F.,.F.)
B_SPLINE_SURFACE_WITH_KNOTS((2,2),(3,2,3),(0.709710709992596,1.),(0.194028469417325,
0.211502584834064,0.212110790644383),.UNSPECIFIED.)
GEOMETRIC_REPRESENTATION_ITEM()
RATIONAL_B_SPLINE_SURFACE(((0.989812124691679,0.992466718773227,0.998122319569322,
0.998122319569323,0.998122319569323),(0.989812124691679,0.992466718773227,
0.998122319569322,0.998122319569322,0.998122319569322)))
REPRESENTATION_ITEM('')
SURFACE()
);
#2665=(
BOUNDED_SURFACE()
B_SPLINE_SURFACE(1,2,((#140215,#140216,#140217),(#140218,#140219,#140220)),
 .UNSPECIFIED.,.F.,.F.,.F.)
B_SPLINE_SURFACE_WITH_KNOTS((2,2),(3,3),(0.710192959008442,1.),(0.521917529826013,
0.539102123117536),.UNSPECIFIED.)
GEOMETRIC_REPRESENTATION_ITEM()
RATIONAL_B_SPLINE_SURFACE(((0.989334769731223,0.987004571835911,0.987576759359605),
(0.989334769731223,0.987004571835911,0.987576759359605)))
REPRESENTATION_ITEM('')
SURFACE()
);
#2666=(
BOUNDED_SURFACE()
B_SPLINE_SURFACE(1,2,((#140229,#140230,#140231,#140232,#140233),(#140234,
#140235,#140236,#140237,#140238)),.UNSPECIFIED.,.F.,.F.,.F.)
B_SPLINE_SURFACE_WITH_KNOTS((2,2),(3,2,3),(0.709710709982975,1.),(0.194028469417325,
0.211502584834064,0.212110790654003),.UNSPECIFIED.)
GEOMETRIC_REPRESENTATION_ITEM()
RATIONAL_B_SPLINE_SURFACE(((0.989812124691679,0.992466718773227,0.998122319569322,
0.998122319569323,0.998122319569323),(0.989812124691679,0.992466718773227,
0.998122319569322,0.998122319569322,0.998122319569322)))
REPRESENTATION_ITEM('')
SURFACE()
);
#2667=(
BOUNDED_SURFACE()
B_SPLINE_SURFACE(1,2,((#140240,#140241,#140242),(#140243,#140244,#140245)),
 .UNSPECIFIED.,.F.,.F.,.F.)
B_SPLINE_SURFACE_WITH_KNOTS((2,2),(3,3),(0.710192959008441,1.),(0.521917529825751,
0.539102123117537),.UNSPECIFIED.)
GEOMETRIC_REPRESENTATION_ITEM()
RATIONAL_B_SPLINE_SURFACE(((0.989334769731294,0.987004571835902,0.987576759359605),
(0.989334769731294,0.987004571835902,0.987576759359605)))
REPRESENTATION_ITEM('')
SURFACE()
);
#2668=(
BOUNDED_SURFACE()
B_SPLINE_SURFACE(1,2,((#140254,#140255,#140256,#140257,#140258),(#140259,
#140260,#140261,#140262,#140263)),.UNSPECIFIED.,.F.,.F.,.F.)
B_SPLINE_SURFACE_WITH_KNOTS((2,2),(3,2,3),(0.709710709986856,1.),(0.194028469417325,
0.211502584834064,0.212110790650128),.UNSPECIFIED.)
GEOMETRIC_REPRESENTATION_ITEM()
RATIONAL_B_SPLINE_SURFACE(((0.989812124691679,0.992466718773227,0.998122319569322,
0.998122319569322,0.998122319569322),(0.989812124691679,0.992466718773227,
0.998122319569322,0.998122319569322,0.998122319569322)))
REPRESENTATION_ITEM('')
SURFACE()
);
#2669=(
BOUNDED_SURFACE()
B_SPLINE_SURFACE(1,2,((#140265,#140266,#140267),(#140268,#140269,#140270)),
 .UNSPECIFIED.,.F.,.F.,.F.)
B_SPLINE_SURFACE_WITH_KNOTS((2,2),(3,3),(0.710192959008443,1.),(0.521917529826001,
0.539102123117536),.UNSPECIFIED.)
GEOMETRIC_REPRESENTATION_ITEM()
RATIONAL_B_SPLINE_SURFACE(((0.989334769731227,0.987004571835911,0.987576759359605),
(0.989334769731227,0.987004571835911,0.987576759359605)))
REPRESENTATION_ITEM('')
SURFACE()
);
#2670=(
BOUNDED_SURFACE()
B_SPLINE_SURFACE(1,2,((#140279,#140280,#140281,#140282,#140283),(#140284,
#140285,#140286,#140287,#140288)),.UNSPECIFIED.,.F.,.F.,.F.)
B_SPLINE_SURFACE_WITH_KNOTS((2,2),(3,2,3),(0.709710709984816,1.),(0.194028469417325,
0.211502584834064,0.212110790643416),.UNSPECIFIED.)
GEOMETRIC_REPRESENTATION_ITEM()
RATIONAL_B_SPLINE_SURFACE(((0.989812124691679,0.992466718773227,0.998122319569322,
0.998122319569322,0.998122319569322),(0.989812124691679,0.992466718773227,
0.998122319569322,0.998122319569322,0.998122319569322)))
REPRESENTATION_ITEM('')
SURFACE()
);
#2671=(
BOUNDED_SURFACE()
B_SPLINE_SURFACE(1,2,((#140290,#140291,#140292),(#140293,#140294,#140295)),
 .UNSPECIFIED.,.F.,.F.,.F.)
B_SPLINE_SURFACE_WITH_KNOTS((2,2),(3,3),(0.710192959008051,1.),(0.521917529826138,
0.539102123117534),.UNSPECIFIED.)
GEOMETRIC_REPRESENTATION_ITEM()
RATIONAL_B_SPLINE_SURFACE(((0.98933476973119,0.987004571835916,0.987576759359605),
(0.98933476973119,0.987004571835916,0.987576759359605)))
REPRESENTATION_ITEM('')
SURFACE()
);
#2672=(
BOUNDED_SURFACE()
B_SPLINE_SURFACE(1,2,((#140304,#140305,#140306,#140307,#140308),(#140309,
#140310,#140311,#140312,#140313)),.UNSPECIFIED.,.F.,.F.,.F.)
B_SPLINE_SURFACE_WITH_KNOTS((2,2),(3,2,3),(0.709710709980223,1.),(0.194028469417326,
0.211502584834066,0.212110790656374),.UNSPECIFIED.)
GEOMETRIC_REPRESENTATION_ITEM()
RATIONAL_B_SPLINE_SURFACE(((0.989812124691679,0.992466718773228,0.998122319569323,
0.998122319569323,0.998122319569323),(0.989812124691679,0.992466718773228,
0.998122319569323,0.998122319569323,0.998122319569323)))
REPRESENTATION_ITEM('')
SURFACE()
);
#2673=(
BOUNDED_SURFACE()
B_SPLINE_SURFACE(1,2,((#140315,#140316,#140317),(#140318,#140319,#140320)),
 .UNSPECIFIED.,.F.,.F.,.F.)
B_SPLINE_SURFACE_WITH_KNOTS((2,2),(3,3),(0.710192959006369,1.),(0.521917529826136,
0.539102123117534),.UNSPECIFIED.)
GEOMETRIC_REPRESENTATION_ITEM()
RATIONAL_B_SPLINE_SURFACE(((0.98933476973119,0.987004571835916,0.987576759359605),
(0.98933476973119,0.987004571835916,0.987576759359605)))
REPRESENTATION_ITEM('')
SURFACE()
);
#2674=(
BOUNDED_SURFACE()
B_SPLINE_SURFACE(1,2,((#140329,#140330,#140331,#140332,#140333),(#140334,
#140335,#140336,#140337,#140338)),.UNSPECIFIED.,.F.,.F.,.F.)
B_SPLINE_SURFACE_WITH_KNOTS((2,2),(3,2,3),(0.709710709983031,1.),(0.194028469417326,
0.211502584834067,0.212110790652154),.UNSPECIFIED.)
GEOMETRIC_REPRESENTATION_ITEM()
RATIONAL_B_SPLINE_SURFACE(((0.989812124691679,0.992466718773228,0.998122319569324,
0.998122319569324,0.998122319569324),(0.989812124691679,0.992466718773228,
0.998122319569324,0.998122319569324,0.998122319569324)))
REPRESENTATION_ITEM('')
SURFACE()
);
#2675=(
BOUNDED_SURFACE()
B_SPLINE_SURFACE(1,2,((#140340,#140341,#140342),(#140343,#140344,#140345)),
 .UNSPECIFIED.,.F.,.F.,.F.)
B_SPLINE_SURFACE_WITH_KNOTS((2,2),(3,3),(0.710192959007972,1.),(0.52191752982614,
0.539102123117534),.UNSPECIFIED.)
GEOMETRIC_REPRESENTATION_ITEM()
RATIONAL_B_SPLINE_SURFACE(((0.989334769731189,0.987004571835916,0.987576759359604),
(0.989334769731189,0.987004571835916,0.987576759359605)))
REPRESENTATION_ITEM('')
SURFACE()
);
#2676=(
BOUNDED_SURFACE()
B_SPLINE_SURFACE(1,2,((#140354,#140355,#140356,#140357,#140358),(#140359,
#140360,#140361,#140362,#140363)),.UNSPECIFIED.,.F.,.F.,.F.)
B_SPLINE_SURFACE_WITH_KNOTS((2,2),(3,2,3),(0.709710709977382,1.),(0.194028469417326,
0.211502584834065,0.212110790659135),.UNSPECIFIED.)
GEOMETRIC_REPRESENTATION_ITEM()
RATIONAL_B_SPLINE_SURFACE(((0.989812124691679,0.992466718773227,0.998122319569323,
0.998122319569323,0.998122319569323),(0.989812124691679,0.992466718773227,
0.998122319569323,0.998122319569323,0.998122319569323)))
REPRESENTATION_ITEM('')
SURFACE()
);
#2677=(
BOUNDED_SURFACE()
B_SPLINE_SURFACE(1,2,((#140365,#140366,#140367),(#140368,#140369,#140370)),
 .UNSPECIFIED.,.F.,.F.,.F.)
B_SPLINE_SURFACE_WITH_KNOTS((2,2),(3,3),(0.710192959008356,1.),(0.52191752982614,
0.539102123117534),.UNSPECIFIED.)
GEOMETRIC_REPRESENTATION_ITEM()
RATIONAL_B_SPLINE_SURFACE(((0.989334769731189,0.987004571835916,0.987576759359605),
(0.989334769731189,0.987004571835916,0.987576759359605)))
REPRESENTATION_ITEM('')
SURFACE()
);
#2678=(
BOUNDED_SURFACE()
B_SPLINE_SURFACE(1,2,((#140379,#140380,#140381,#140382,#140383),(#140384,
#140385,#140386,#140387,#140388)),.UNSPECIFIED.,.F.,.F.,.F.)
B_SPLINE_SURFACE_WITH_KNOTS((2,2),(3,2,3),(0.709710709982804,1.),(0.194028469417326,
0.211502584834067,0.212110790654097),.UNSPECIFIED.)
GEOMETRIC_REPRESENTATION_ITEM()
RATIONAL_B_SPLINE_SURFACE(((0.989812124691679,0.992466718773228,0.998122319569324,
0.998122319569324,0.998122319569324),(0.989812124691679,0.992466718773228,
0.998122319569324,0.998122319569324,0.998122319569324)))
REPRESENTATION_ITEM('')
SURFACE()
);
#2679=(
BOUNDED_SURFACE()
B_SPLINE_SURFACE(1,2,((#140390,#140391,#140392),(#140393,#140394,#140395)),
 .UNSPECIFIED.,.F.,.F.,.F.)
B_SPLINE_SURFACE_WITH_KNOTS((2,2),(3,3),(0.71019295900836,1.),(0.521917529826139,
0.539102123117534),.UNSPECIFIED.)
GEOMETRIC_REPRESENTATION_ITEM()
RATIONAL_B_SPLINE_SURFACE(((0.989334769731189,0.987004571835916,0.987576759359605),
(0.989334769731189,0.987004571835916,0.987576759359605)))
REPRESENTATION_ITEM('')
SURFACE()
);
#2680=(
BOUNDED_SURFACE()
B_SPLINE_SURFACE(1,2,((#140404,#140405,#140406,#140407,#140408),(#140409,
#140410,#140411,#140412,#140413)),.UNSPECIFIED.,.F.,.F.,.F.)
B_SPLINE_SURFACE_WITH_KNOTS((2,2),(3,2,3),(0.709710709971706,1.),(0.194028469417326,
0.211502584834067,0.212110790665193),.UNSPECIFIED.)
GEOMETRIC_REPRESENTATION_ITEM()
RATIONAL_B_SPLINE_SURFACE(((0.989812124691679,0.992466718773228,0.998122319569324,
0.998122319569324,0.998122319569324),(0.989812124691679,0.992466718773228,
0.998122319569324,0.998122319569324,0.998122319569324)))
REPRESENTATION_ITEM('')
SURFACE()
);
#2681=(
BOUNDED_SURFACE()
B_SPLINE_SURFACE(1,2,((#140415,#140416,#140417),(#140418,#140419,#140420)),
 .UNSPECIFIED.,.F.,.F.,.F.)
B_SPLINE_SURFACE_WITH_KNOTS((2,2),(3,3),(0.710192959008365,1.),(0.52191752982614,
0.539102123117534),.UNSPECIFIED.)
GEOMETRIC_REPRESENTATION_ITEM()
RATIONAL_B_SPLINE_SURFACE(((0.989334769731189,0.987004571835916,0.987576759359605),
(0.989334769731189,0.987004571835916,0.987576759359605)))
REPRESENTATION_ITEM('')
SURFACE()
);
#2682=(
BOUNDED_SURFACE()
B_SPLINE_SURFACE(1,2,((#140429,#140430,#140431,#140432,#140433),(#140434,
#140435,#140436,#140437,#140438)),.UNSPECIFIED.,.F.,.F.,.F.)
B_SPLINE_SURFACE_WITH_KNOTS((2,2),(3,2,3),(0.709710709972218,1.),(0.194028469417326,
0.211502584834069,0.212110790664693),.UNSPECIFIED.)
GEOMETRIC_REPRESENTATION_ITEM()
RATIONAL_B_SPLINE_SURFACE(((0.989812124691679,0.992466718773228,0.998122319569325,
0.998122319569325,0.998122319569325),(0.989812124691679,0.992466718773228,
0.998122319569325,0.998122319569325,0.998122319569325)))
REPRESENTATION_ITEM('')
SURFACE()
);
#2683=(
BOUNDED_SURFACE()
B_SPLINE_SURFACE(1,2,((#140440,#140441,#140442),(#140443,#140444,#140445)),
 .UNSPECIFIED.,.F.,.F.,.F.)
B_SPLINE_SURFACE_WITH_KNOTS((2,2),(3,3),(0.710192959008044,1.),(0.52191752982614,
0.539102123117534),.UNSPECIFIED.)
GEOMETRIC_REPRESENTATION_ITEM()
RATIONAL_B_SPLINE_SURFACE(((0.989334769731189,0.987004571835916,0.987576759359605),
(0.989334769731189,0.987004571835916,0.987576759359605)))
REPRESENTATION_ITEM('')
SURFACE()
);
#2684=(
BOUNDED_SURFACE()
B_SPLINE_SURFACE(1,2,((#140454,#140455,#140456,#140457,#140458),(#140459,
#140460,#140461,#140462,#140463)),.UNSPECIFIED.,.F.,.F.,.F.)
B_SPLINE_SURFACE_WITH_KNOTS((2,2),(3,2,3),(0.709710709979372,1.),(0.194028469417326,
0.211502584834065,0.212110790657219),.UNSPECIFIED.)
GEOMETRIC_REPRESENTATION_ITEM()
RATIONAL_B_SPLINE_SURFACE(((0.989812124691679,0.992466718773227,0.998122319569323,
0.998122319569323,0.998122319569323),(0.989812124691679,0.992466718773227,
0.998122319569323,0.998122319569323,0.998122319569323)))
REPRESENTATION_ITEM('')
SURFACE()
);
#2685=(
BOUNDED_SURFACE()
B_SPLINE_SURFACE(1,2,((#140465,#140466,#140467),(#140468,#140469,#140470)),
 .UNSPECIFIED.,.F.,.F.,.F.)
B_SPLINE_SURFACE_WITH_KNOTS((2,2),(3,3),(0.710192959008388,1.),(0.52191752982614,
0.539102123117534),.UNSPECIFIED.)
GEOMETRIC_REPRESENTATION_ITEM()
RATIONAL_B_SPLINE_SURFACE(((0.989334769731189,0.987004571835916,0.987576759359605),
(0.989334769731189,0.987004571835916,0.987576759359605)))
REPRESENTATION_ITEM('')
SURFACE()
);
#2686=(
BOUNDED_SURFACE()
B_SPLINE_SURFACE(1,2,((#140479,#140480,#140481,#140482,#140483),(#140484,
#140485,#140486,#140487,#140488)),.UNSPECIFIED.,.F.,.F.,.F.)
B_SPLINE_SURFACE_WITH_KNOTS((2,2),(3,2,3),(0.709710709969892,1.),(0.194028469417326,
0.211502584834065,0.212110790667046),.UNSPECIFIED.)
GEOMETRIC_REPRESENTATION_ITEM()
RATIONAL_B_SPLINE_SURFACE(((0.989812124691679,0.992466718773227,0.998122319569323,
0.998122319569323,0.998122319569323),(0.989812124691679,0.992466718773227,
0.998122319569323,0.998122319569323,0.998122319569323)))
REPRESENTATION_ITEM('')
SURFACE()
);
#2687=(
BOUNDED_SURFACE()
B_SPLINE_SURFACE(1,2,((#140490,#140491,#140492),(#140493,#140494,#140495)),
 .UNSPECIFIED.,.F.,.F.,.F.)
B_SPLINE_SURFACE_WITH_KNOTS((2,2),(3,3),(0.710192959008377,1.),(0.521917529826137,
0.539102123117534),.UNSPECIFIED.)
GEOMETRIC_REPRESENTATION_ITEM()
RATIONAL_B_SPLINE_SURFACE(((0.98933476973119,0.987004571835916,0.987576759359605),
(0.98933476973119,0.987004571835916,0.987576759359605)))
REPRESENTATION_ITEM('')
SURFACE()
);
#2688=(
BOUNDED_SURFACE()
B_SPLINE_SURFACE(1,2,((#140497,#140498,#140499,#140500,#140501),(#140502,
#140503,#140504,#140505,#140506)),.UNSPECIFIED.,.F.,.F.,.F.)
B_SPLINE_SURFACE_WITH_KNOTS((2,2),(3,2,3),(0.,0.289807040991683),(0.573480748819789,
0.57365435021991,0.591014490232052),.UNSPECIFIED.)
GEOMETRIC_REPRESENTATION_ITEM()
RATIONAL_B_SPLINE_SURFACE(((0.99848615229188,0.99848615229188,0.99848615229188,
0.992772345172012,0.990020524139833),(0.99848615229188,0.99848615229188,
0.99848615229188,0.992772345172012,0.990020524139833)))
REPRESENTATION_ITEM('')
SURFACE()
);
#2689=(
BOUNDED_SURFACE()
B_SPLINE_SURFACE(1,2,((#140515,#140516,#140517,#140518,#140519),(#140520,
#140521,#140522,#140523,#140524)),.UNSPECIFIED.,.F.,.F.,.F.)
B_SPLINE_SURFACE_WITH_KNOTS((2,2),(3,2,3),(0.,0.289681084360264),(0.142474614281368,
0.142857142857143,0.159901408087482),.UNSPECIFIED.)
GEOMETRIC_REPRESENTATION_ITEM()
RATIONAL_B_SPLINE_SURFACE(((0.999732896029238,0.999865728939373,1.,0.994017305594881,
0.990889788836284),(0.999732896029238,0.999865728939373,1.,0.994017305594881,
0.990889788836284)))
REPRESENTATION_ITEM('')
SURFACE()
);
#2690=(
BOUNDED_SURFACE()
B_SPLINE_SURFACE(1,2,((#140533,#140534,#140535,#140536,#140537),(#140538,
#140539,#140540,#140541,#140542)),.UNSPECIFIED.,.F.,.F.,.F.)
B_SPLINE_SURFACE_WITH_KNOTS((2,2),(3,2,3),(0.,0.289807040991656),(0.573480748819709,
0.573654350219831,0.591014490232052),.UNSPECIFIED.)
GEOMETRIC_REPRESENTATION_ITEM()
RATIONAL_B_SPLINE_SURFACE(((0.998486152291932,0.998486152291932,0.998486152291932,
0.992772345172024,0.990020524139833),(0.998486152291932,0.998486152291932,
0.998486152291932,0.992772345172024,0.990020524139833)))
REPRESENTATION_ITEM('')
SURFACE()
);
#2691=(
BOUNDED_SURFACE()
B_SPLINE_SURFACE(1,2,((#140544,#140545,#140546,#140547,#140548),(#140549,
#140550,#140551,#140552,#140553)),.UNSPECIFIED.,.F.,.F.,.F.)
B_SPLINE_SURFACE_WITH_KNOTS((2,2),(3,2,3),(0.,0.289681084359915),(0.142474614281368,
0.142857142857143,0.159901408087482),.UNSPECIFIED.)
GEOMETRIC_REPRESENTATION_ITEM()
RATIONAL_B_SPLINE_SURFACE(((0.999732896029238,0.999865728939373,1.,0.994017305594881,
0.990889788836284),(0.999732896029238,0.999865728939373,1.,0.994017305594881,
0.990889788836284)))
REPRESENTATION_ITEM('')
SURFACE()
);
#2692=(
BOUNDED_SURFACE()
B_SPLINE_SURFACE(1,2,((#140562,#140563,#140564,#140565,#140566),(#140567,
#140568,#140569,#140570,#140571)),.UNSPECIFIED.,.F.,.F.,.F.)
B_SPLINE_SURFACE_WITH_KNOTS((2,2),(3,2,3),(0.,0.289807040991664),(0.573480748819789,
0.57365435021991,0.591014490232052),.UNSPECIFIED.)
GEOMETRIC_REPRESENTATION_ITEM()
RATIONAL_B_SPLINE_SURFACE(((0.99848615229188,0.99848615229188,0.99848615229188,
0.992772345172011,0.990020524139833),(0.99848615229188,0.99848615229188,
0.99848615229188,0.992772345172011,0.990020524139833)))
REPRESENTATION_ITEM('')
SURFACE()
);
#2693=(
BOUNDED_SURFACE()
B_SPLINE_SURFACE(1,2,((#140573,#140574,#140575,#140576,#140577),(#140578,
#140579,#140580,#140581,#140582)),.UNSPECIFIED.,.F.,.F.,.F.)
B_SPLINE_SURFACE_WITH_KNOTS((2,2),(3,2,3),(0.,0.289681084359918),(0.142474614281368,
0.142857142857143,0.159901408087482),.UNSPECIFIED.)
GEOMETRIC_REPRESENTATION_ITEM()
RATIONAL_B_SPLINE_SURFACE(((0.999732896029238,0.999865728939373,1.,0.994017305594881,
0.990889788836284),(0.999732896029238,0.999865728939373,1.,0.994017305594881,
0.990889788836284)))
REPRESENTATION_ITEM('')
SURFACE()
);
#2694=(
BOUNDED_SURFACE()
B_SPLINE_SURFACE(1,2,((#140591,#140592,#140593,#140594,#140595),(#140596,
#140597,#140598,#140599,#140600)),.UNSPECIFIED.,.F.,.F.,.F.)
B_SPLINE_SURFACE_WITH_KNOTS((2,2),(3,2,3),(0.,0.289807040992624),(0.573480748819707,
0.573654350219829,0.591014490232052),.UNSPECIFIED.)
GEOMETRIC_REPRESENTATION_ITEM()
RATIONAL_B_SPLINE_SURFACE(((0.998486152291933,0.998486152291933,0.998486152291933,
0.992772345172024,0.990020524139833),(0.998486152291933,0.998486152291933,
0.998486152291933,0.992772345172024,0.990020524139833)))
REPRESENTATION_ITEM('')
SURFACE()
);
#2695=(
BOUNDED_SURFACE()
B_SPLINE_SURFACE(1,2,((#140602,#140603,#140604,#140605,#140606),(#140607,
#140608,#140609,#140610,#140611)),.UNSPECIFIED.,.F.,.F.,.F.)
B_SPLINE_SURFACE_WITH_KNOTS((2,2),(3,2,3),(0.,0.289681084360269),(0.142474614281368,
0.142857142857143,0.159901408087482),.UNSPECIFIED.)
GEOMETRIC_REPRESENTATION_ITEM()
RATIONAL_B_SPLINE_SURFACE(((0.999732896029238,0.999865728939373,1.,0.994017305594881,
0.990889788836284),(0.999732896029238,0.999865728939373,1.,0.994017305594881,
0.990889788836284)))
REPRESENTATION_ITEM('')
SURFACE()
);
#2696=(
BOUNDED_SURFACE()
B_SPLINE_SURFACE(1,2,((#140620,#140621,#140622,#140623,#140624),(#140625,
#140626,#140627,#140628,#140629)),.UNSPECIFIED.,.F.,.F.,.F.)
B_SPLINE_SURFACE_WITH_KNOTS((2,2),(3,2,3),(0.,0.289807040992624),(0.573480748819707,
0.573654350219829,0.591014490232052),.UNSPECIFIED.)
GEOMETRIC_REPRESENTATION_ITEM()
RATIONAL_B_SPLINE_SURFACE(((0.998486152291934,0.998486152291934,0.998486152291934,
0.992772345172024,0.990020524139833),(0.998486152291934,0.998486152291934,
0.998486152291934,0.992772345172024,0.990020524139833)))
REPRESENTATION_ITEM('')
SURFACE()
);
#2697=(
BOUNDED_SURFACE()
B_SPLINE_SURFACE(1,2,((#140631,#140632,#140633,#140634,#140635),(#140636,
#140637,#140638,#140639,#140640),(#140641,#140642,#140643,#140644,#140645)),
 .UNSPECIFIED.,.F.,.F.,.F.)
B_SPLINE_SURFACE_WITH_KNOTS((2,1,2),(3,2,3),(-0.00289681084359923,0.,0.289681084359923),
(0.142474614281368,0.142857142857143,0.159901408087482),.UNSPECIFIED.)
GEOMETRIC_REPRESENTATION_ITEM()
RATIONAL_B_SPLINE_SURFACE(((0.999732896029238,0.999865728939373,1.,0.994017305594881,
0.990889788836284),(0.999732896029238,0.999865728939373,1.,0.994017305594881,
0.990889788836284),(0.999732896029238,0.999865728939373,1.,0.994017305594881,
0.990889788836284)))
REPRESENTATION_ITEM('')
SURFACE()
);
#2698=(
BOUNDED_SURFACE()
B_SPLINE_SURFACE(1,2,((#140654,#140655,#140656,#140657,#140658),(#140659,
#140660,#140661,#140662,#140663)),.UNSPECIFIED.,.F.,.F.,.F.)
B_SPLINE_SURFACE_WITH_KNOTS((2,2),(3,2,3),(0.,0.289807040992624),(0.573480748819789,
0.57365435021991,0.591014490232052),.UNSPECIFIED.)
GEOMETRIC_REPRESENTATION_ITEM()
RATIONAL_B_SPLINE_SURFACE(((0.99848615229188,0.99848615229188,0.99848615229188,
0.992772345172012,0.990020524139833),(0.99848615229188,0.99848615229188,
0.99848615229188,0.992772345172012,0.990020524139833)))
REPRESENTATION_ITEM('')
SURFACE()
);
#2699=(
BOUNDED_SURFACE()
B_SPLINE_SURFACE(1,2,((#140665,#140666,#140667,#140668,#140669),(#140670,
#140671,#140672,#140673,#140674)),.UNSPECIFIED.,.F.,.F.,.F.)
B_SPLINE_SURFACE_WITH_KNOTS((2,2),(3,2,3),(0.,0.28968108435992),(0.142474614281368,
0.142857142857143,0.159901408087482),.UNSPECIFIED.)
GEOMETRIC_REPRESENTATION_ITEM()
RATIONAL_B_SPLINE_SURFACE(((0.999732896029238,0.999865728939373,1.,0.994017305594881,
0.990889788836284),(0.999732896029238,0.999865728939373,1.,0.994017305594881,
0.990889788836284)))
REPRESENTATION_ITEM('')
SURFACE()
);
#2700=(
BOUNDED_SURFACE()
B_SPLINE_SURFACE(1,2,((#140683,#140684,#140685,#140686,#140687),(#140688,
#140689,#140690,#140691,#140692)),.UNSPECIFIED.,.F.,.F.,.F.)
B_SPLINE_SURFACE_WITH_KNOTS((2,2),(3,2,3),(0.,0.289807040993208),(0.573480748819707,
0.573654350219829,0.591014490232052),.UNSPECIFIED.)
GEOMETRIC_REPRESENTATION_ITEM()
RATIONAL_B_SPLINE_SURFACE(((0.998486152291933,0.998486152291933,0.998486152291933,
0.992772345172024,0.990020524139833),(0.998486152291933,0.998486152291933,
0.998486152291933,0.992772345172024,0.990020524139833)))
REPRESENTATION_ITEM('')
SURFACE()
);
#2701=(
BOUNDED_SURFACE()
B_SPLINE_SURFACE(1,2,((#140694,#140695,#140696,#140697,#140698),(#140699,
#140700,#140701,#140702,#140703)),.UNSPECIFIED.,.F.,.F.,.F.)
B_SPLINE_SURFACE_WITH_KNOTS((2,2),(3,2,3),(0.,0.289681084359919),(0.142474614281368,
0.142857142857143,0.159901408087482),.UNSPECIFIED.)
GEOMETRIC_REPRESENTATION_ITEM()
RATIONAL_B_SPLINE_SURFACE(((0.999732896029238,0.999865728939373,1.,0.994017305594881,
0.990889788836284),(0.999732896029238,0.999865728939373,1.,0.994017305594881,
0.990889788836284)))
REPRESENTATION_ITEM('')
SURFACE()
);
#2702=(
BOUNDED_SURFACE()
B_SPLINE_SURFACE(1,2,((#140712,#140713,#140714,#140715,#140716),(#140717,
#140718,#140719,#140720,#140721)),.UNSPECIFIED.,.F.,.F.,.F.)
B_SPLINE_SURFACE_WITH_KNOTS((2,2),(3,2,3),(0.,0.289807040992617),(0.573480748819789,
0.57365435021991,0.591014490232052),.UNSPECIFIED.)
GEOMETRIC_REPRESENTATION_ITEM()
RATIONAL_B_SPLINE_SURFACE(((0.99848615229188,0.99848615229188,0.99848615229188,
0.992772345172011,0.990020524139833),(0.99848615229188,0.99848615229188,
0.99848615229188,0.992772345172011,0.990020524139833)))
REPRESENTATION_ITEM('')
SURFACE()
);
#2703=(
BOUNDED_SURFACE()
B_SPLINE_SURFACE(1,2,((#140723,#140724,#140725,#140726,#140727),(#140728,
#140729,#140730,#140731,#140732)),.UNSPECIFIED.,.F.,.F.,.F.)
B_SPLINE_SURFACE_WITH_KNOTS((2,2),(3,2,3),(0.,0.289681084359923),(0.142474614281368,
0.142857142857143,0.159901408087482),.UNSPECIFIED.)
GEOMETRIC_REPRESENTATION_ITEM()
RATIONAL_B_SPLINE_SURFACE(((0.999732896029238,0.999865728939373,1.,0.994017305594881,
0.990889788836283),(0.999732896029238,0.999865728939373,1.,0.994017305594881,
0.990889788836283)))
REPRESENTATION_ITEM('')
SURFACE()
);
#2704=(
BOUNDED_SURFACE()
B_SPLINE_SURFACE(1,2,((#140741,#140742,#140743,#140744,#140745),(#140746,
#140747,#140748,#140749,#140750)),.UNSPECIFIED.,.F.,.F.,.F.)
B_SPLINE_SURFACE_WITH_KNOTS((2,2),(3,2,3),(0.,0.289807040993175),(0.573480748819789,
0.57365435021991,0.591014490232052),.UNSPECIFIED.)
GEOMETRIC_REPRESENTATION_ITEM()
RATIONAL_B_SPLINE_SURFACE(((0.99848615229188,0.99848615229188,0.99848615229188,
0.992772345172012,0.990020524139833),(0.99848615229188,0.99848615229188,
0.99848615229188,0.992772345172012,0.990020524139833)))
REPRESENTATION_ITEM('')
SURFACE()
);
#2705=(
BOUNDED_SURFACE()
B_SPLINE_SURFACE(1,2,((#140752,#140753,#140754,#140755,#140756),(#140757,
#140758,#140759,#140760,#140761)),.UNSPECIFIED.,.F.,.F.,.F.)
B_SPLINE_SURFACE_WITH_KNOTS((2,2),(3,2,3),(0.,0.289681084360261),(0.142474614281368,
0.142857142857143,0.159901408087482),.UNSPECIFIED.)
GEOMETRIC_REPRESENTATION_ITEM()
RATIONAL_B_SPLINE_SURFACE(((0.999732896029238,0.999865728939373,1.,0.994017305594881,
0.990889788836283),(0.999732896029238,0.999865728939373,1.,0.994017305594881,
0.990889788836284)))
REPRESENTATION_ITEM('')
SURFACE()
);
#2706=(
BOUNDED_SURFACE()
B_SPLINE_SURFACE(1,2,((#140770,#140771,#140772,#140773,#140774),(#140775,
#140776,#140777,#140778,#140779)),.UNSPECIFIED.,.F.,.F.,.F.)
B_SPLINE_SURFACE_WITH_KNOTS((2,2),(3,2,3),(0.,0.289807040992678),(0.57348074881971,
0.573654350219832,0.591014490232052),.UNSPECIFIED.)
GEOMETRIC_REPRESENTATION_ITEM()
RATIONAL_B_SPLINE_SURFACE(((0.998486152291931,0.998486152291931,0.998486152291931,
0.992772345172024,0.990020524139833),(0.998486152291931,0.998486152291931,
0.998486152291931,0.992772345172024,0.990020524139833)))
REPRESENTATION_ITEM('')
SURFACE()
);
#2707=(
BOUNDED_SURFACE()
B_SPLINE_SURFACE(1,2,((#140781,#140782,#140783,#140784,#140785),(#140786,
#140787,#140788,#140789,#140790)),.UNSPECIFIED.,.F.,.F.,.F.)
B_SPLINE_SURFACE_WITH_KNOTS((2,2),(3,2,3),(0.,0.289681084359922),(0.142474614281367,
0.142857142857143,0.159901408087481),.UNSPECIFIED.)
GEOMETRIC_REPRESENTATION_ITEM()
RATIONAL_B_SPLINE_SURFACE(((0.999732896029237,0.999865728939372,1.,0.994017305594881,
0.990889788836284),(0.999732896029237,0.999865728939372,1.,0.994017305594881,
0.990889788836284)))
REPRESENTATION_ITEM('')
SURFACE()
);
#2708=(
BOUNDED_SURFACE()
B_SPLINE_SURFACE(1,2,((#140799,#140800,#140801,#140802,#140803),(#140804,
#140805,#140806,#140807,#140808)),.UNSPECIFIED.,.F.,.F.,.F.)
B_SPLINE_SURFACE_WITH_KNOTS((2,2),(3,2,3),(0.,0.289807040992689),(0.57348074881979,
0.573654350219911,0.591014490232053),.UNSPECIFIED.)
GEOMETRIC_REPRESENTATION_ITEM()
RATIONAL_B_SPLINE_SURFACE(((0.99848615229188,0.99848615229188,0.99848615229188,
0.992772345172011,0.990020524139833),(0.99848615229188,0.99848615229188,
0.99848615229188,0.992772345172011,0.990020524139833)))
REPRESENTATION_ITEM('')
SURFACE()
);
#2709=(
BOUNDED_SURFACE()
B_SPLINE_SURFACE(1,2,((#140810,#140811,#140812,#140813,#140814),(#140815,
#140816,#140817,#140818,#140819)),.UNSPECIFIED.,.F.,.F.,.F.)
B_SPLINE_SURFACE_WITH_KNOTS((2,2),(3,2,3),(0.,0.28968108436027),(0.142474614281367,
0.142857142857143,0.159901408087481),.UNSPECIFIED.)
GEOMETRIC_REPRESENTATION_ITEM()
RATIONAL_B_SPLINE_SURFACE(((0.999732896029238,0.999865728939373,1.,0.994017305594881,
0.990889788836284),(0.999732896029238,0.999865728939373,1.,0.994017305594881,
0.990889788836284)))
REPRESENTATION_ITEM('')
SURFACE()
);
#2710=(
BOUNDED_SURFACE()
B_SPLINE_SURFACE(1,2,((#140828,#140829,#140830,#140831,#140832),(#140833,
#140834,#140835,#140836,#140837)),.UNSPECIFIED.,.F.,.F.,.F.)
B_SPLINE_SURFACE_WITH_KNOTS((2,2),(3,2,3),(0.,0.289807040993298),(0.57348074881979,
0.573654350219911,0.591014490232053),.UNSPECIFIED.)
GEOMETRIC_REPRESENTATION_ITEM()
RATIONAL_B_SPLINE_SURFACE(((0.99848615229188,0.99848615229188,0.99848615229188,
0.992772345172011,0.990020524139833),(0.99848615229188,0.99848615229188,
0.99848615229188,0.992772345172011,0.990020524139833)))
REPRESENTATION_ITEM('')
SURFACE()
);
#2711=(
BOUNDED_SURFACE()
B_SPLINE_SURFACE(1,2,((#140839,#140840,#140841,#140842,#140843),(#140844,
#140845,#140846,#140847,#140848)),.UNSPECIFIED.,.F.,.F.,.F.)
B_SPLINE_SURFACE_WITH_KNOTS((2,2),(3,2,3),(0.,0.289681084360275),(0.142474614281367,
0.142857142857143,0.159901408087481),.UNSPECIFIED.)
GEOMETRIC_REPRESENTATION_ITEM()
RATIONAL_B_SPLINE_SURFACE(((0.999732896029237,0.999865728939372,1.,0.994017305594881,
0.990889788836284),(0.999732896029237,0.999865728939372,1.,0.994017305594881,
0.990889788836284)))
REPRESENTATION_ITEM('')
SURFACE()
);
#2712=(
BOUNDED_SURFACE()
B_SPLINE_SURFACE(1,2,((#140857,#140858,#140859,#140860,#140861),(#140862,
#140863,#140864,#140865,#140866)),.UNSPECIFIED.,.F.,.F.,.F.)
B_SPLINE_SURFACE_WITH_KNOTS((2,2),(3,2,3),(0.,0.28980704099271),(0.573480748819708,
0.57365435021983,0.591014490232053),.UNSPECIFIED.)
GEOMETRIC_REPRESENTATION_ITEM()
RATIONAL_B_SPLINE_SURFACE(((0.998486152291933,0.998486152291933,0.998486152291933,
0.992772345172024,0.990020524139833),(0.998486152291933,0.998486152291933,
0.998486152291933,0.992772345172024,0.990020524139833)))
REPRESENTATION_ITEM('')
SURFACE()
);
#2713=(
BOUNDED_SURFACE()
B_SPLINE_SURFACE(1,2,((#140868,#140869,#140870,#140871,#140872),(#140873,
#140874,#140875,#140876,#140877)),.UNSPECIFIED.,.F.,.F.,.F.)
B_SPLINE_SURFACE_WITH_KNOTS((2,2),(3,2,3),(0.,0.28968108435992),(0.142474614281367,
0.142857142857143,0.159901408087481),.UNSPECIFIED.)
GEOMETRIC_REPRESENTATION_ITEM()
RATIONAL_B_SPLINE_SURFACE(((0.999732896029237,0.999865728939372,1.,0.994017305594881,
0.990889788836284),(0.999732896029237,0.999865728939372,1.,0.994017305594881,
0.990889788836284)))
REPRESENTATION_ITEM('')
SURFACE()
);
#2714=(
BOUNDED_SURFACE()
B_SPLINE_SURFACE(1,2,((#140886,#140887,#140888,#140889,#140890),(#140891,
#140892,#140893,#140894,#140895)),.UNSPECIFIED.,.F.,.F.,.F.)
B_SPLINE_SURFACE_WITH_KNOTS((2,2),(3,2,3),(0.,0.289807040993208),(0.57348074881979,
0.573654350219911,0.591014490232053),.UNSPECIFIED.)
GEOMETRIC_REPRESENTATION_ITEM()
RATIONAL_B_SPLINE_SURFACE(((0.99848615229188,0.99848615229188,0.99848615229188,
0.992772345172011,0.990020524139833),(0.99848615229188,0.99848615229188,
0.99848615229188,0.992772345172011,0.990020524139833)))
REPRESENTATION_ITEM('')
SURFACE()
);
#2715=(
BOUNDED_SURFACE()
B_SPLINE_SURFACE(1,2,((#140897,#140898,#140899,#140900,#140901),(#140902,
#140903,#140904,#140905,#140906),(#140907,#140908,#140909,#140910,#140911)),
 .UNSPECIFIED.,.F.,.F.,.F.)
B_SPLINE_SURFACE_WITH_KNOTS((2,1,2),(3,2,3),(-0.00289681084359918,0.,0.289681084359918),
(0.142474614281366,0.142857142857143,0.159901408087481),.UNSPECIFIED.)
GEOMETRIC_REPRESENTATION_ITEM()
RATIONAL_B_SPLINE_SURFACE(((0.999732896029237,0.999865728939372,1.,0.994017305594881,
0.990889788836284),(0.999732896029237,0.999865728939372,1.,0.994017305594881,
0.990889788836284),(0.999732896029237,0.999865728939372,1.,0.994017305594881,
0.990889788836284)))
REPRESENTATION_ITEM('')
SURFACE()
);
#2716=(
BOUNDED_SURFACE()
B_SPLINE_SURFACE(1,2,((#140920,#140921,#140922,#140923,#140924),(#140925,
#140926,#140927,#140928,#140929)),.UNSPECIFIED.,.F.,.F.,.F.)
B_SPLINE_SURFACE_WITH_KNOTS((2,2),(3,2,3),(0.,0.289807040992711),(0.573480748819708,
0.57365435021983,0.591014490232053),.UNSPECIFIED.)
GEOMETRIC_REPRESENTATION_ITEM()
RATIONAL_B_SPLINE_SURFACE(((0.998486152291933,0.998486152291933,0.998486152291933,
0.992772345172024,0.990020524139833),(0.998486152291933,0.998486152291933,
0.998486152291933,0.992772345172024,0.990020524139833)))
REPRESENTATION_ITEM('')
SURFACE()
);
#2717=(
BOUNDED_SURFACE()
B_SPLINE_SURFACE(1,2,((#140931,#140932,#140933,#140934,#140935),(#140936,
#140937,#140938,#140939,#140940)),.UNSPECIFIED.,.F.,.F.,.F.)
B_SPLINE_SURFACE_WITH_KNOTS((2,2),(3,2,3),(0.,0.289681084360276),(0.142474614281367,
0.142857142857143,0.159901408087481),.UNSPECIFIED.)
GEOMETRIC_REPRESENTATION_ITEM()
RATIONAL_B_SPLINE_SURFACE(((0.999732896029237,0.999865728939372,1.,0.994017305594881,
0.990889788836284),(0.999732896029237,0.999865728939372,1.,0.994017305594881,
0.990889788836284)))
REPRESENTATION_ITEM('')
SURFACE()
);
#2718=(
BOUNDED_SURFACE()
B_SPLINE_SURFACE(1,2,((#140949,#140950,#140951,#140952,#140953),(#140954,
#140955,#140956,#140957,#140958)),.UNSPECIFIED.,.F.,.F.,.F.)
B_SPLINE_SURFACE_WITH_KNOTS((2,2),(3,2,3),(0.,0.289807040993198),(0.57348074881971,
0.573654350219832,0.591014490232053),.UNSPECIFIED.)
GEOMETRIC_REPRESENTATION_ITEM()
RATIONAL_B_SPLINE_SURFACE(((0.998486152291932,0.998486152291932,0.998486152291932,
0.992772345172024,0.990020524139833),(0.998486152291932,0.998486152291932,
0.998486152291932,0.992772345172024,0.990020524139833)))
REPRESENTATION_ITEM('')
SURFACE()
);
#2719=(
BOUNDED_SURFACE()
B_SPLINE_SURFACE(1,2,((#140960,#140961,#140962,#140963,#140964),(#140965,
#140966,#140967,#140968,#140969)),.UNSPECIFIED.,.F.,.F.,.F.)
B_SPLINE_SURFACE_WITH_KNOTS((2,2),(3,2,3),(0.,0.289681084359923),(0.142474614281367,
0.142857142857143,0.159901408087481),.UNSPECIFIED.)
GEOMETRIC_REPRESENTATION_ITEM()
RATIONAL_B_SPLINE_SURFACE(((0.999732896029238,0.999865728939373,1.,0.994017305594881,
0.990889788836284),(0.999732896029238,0.999865728939373,1.,0.994017305594881,
0.990889788836284)))
REPRESENTATION_ITEM('')
SURFACE()
);
#2720=(
BOUNDED_SURFACE()
B_SPLINE_SURFACE(1,2,((#140978,#140979,#140980,#140981,#140982),(#140983,
#140984,#140985,#140986,#140987)),.UNSPECIFIED.,.F.,.F.,.F.)
B_SPLINE_SURFACE_WITH_KNOTS((2,2),(3,2,3),(0.,0.289807040992956),(0.57348074881971,
0.573654350219832,0.591014490232053),.UNSPECIFIED.)
GEOMETRIC_REPRESENTATION_ITEM()
RATIONAL_B_SPLINE_SURFACE(((0.998486152291931,0.998486152291931,0.998486152291931,
0.992772345172023,0.990020524139833),(0.998486152291931,0.998486152291931,
0.998486152291931,0.992772345172023,0.990020524139833)))
REPRESENTATION_ITEM('')
SURFACE()
);
#2721=(
BOUNDED_SURFACE()
B_SPLINE_SURFACE(1,2,((#140989,#140990,#140991,#140992,#140993),(#140994,
#140995,#140996,#140997,#140998)),.UNSPECIFIED.,.F.,.F.,.F.)
B_SPLINE_SURFACE_WITH_KNOTS((2,2),(3,2,3),(0.,0.289681084359924),(0.142474614281367,
0.142857142857143,0.159901408087481),.UNSPECIFIED.)
GEOMETRIC_REPRESENTATION_ITEM()
RATIONAL_B_SPLINE_SURFACE(((0.999732896029237,0.999865728939372,1.,0.994017305594881,
0.990889788836284),(0.999732896029237,0.999865728939372,1.,0.994017305594881,
0.990889788836284)))
REPRESENTATION_ITEM('')
SURFACE()
);
#2722=(
BOUNDED_SURFACE()
B_SPLINE_SURFACE(1,2,((#141007,#141008,#141009,#141010,#141011),(#141012,
#141013,#141014,#141015,#141016)),.UNSPECIFIED.,.F.,.F.,.F.)
B_SPLINE_SURFACE_WITH_KNOTS((2,2),(3,2,3),(0.,0.289807040994019),(0.57348074881979,
0.573654350219911,0.591014490232053),.UNSPECIFIED.)
GEOMETRIC_REPRESENTATION_ITEM()
RATIONAL_B_SPLINE_SURFACE(((0.99848615229188,0.99848615229188,0.99848615229188,
0.992772345172011,0.990020524139833),(0.99848615229188,0.99848615229188,
0.99848615229188,0.992772345172011,0.990020524139833)))
REPRESENTATION_ITEM('')
SURFACE()
);
#2723=(
BOUNDED_SURFACE()
B_SPLINE_SURFACE(1,2,((#141018,#141019,#141020,#141021,#141022),(#141023,
#141024,#141025,#141026,#141027),(#141028,#141029,#141030,#141031,#141032)),
 .UNSPECIFIED.,.F.,.F.,.F.)
B_SPLINE_SURFACE_WITH_KNOTS((2,1,2),(3,2,3),(-0.00289681084360293,0.,0.289681084360293),
(0.142474614281367,0.142857142857143,0.159901408087481),.UNSPECIFIED.)
GEOMETRIC_REPRESENTATION_ITEM()
RATIONAL_B_SPLINE_SURFACE(((0.999732896029237,0.999865728939372,1.,0.994017305594881,
0.990889788836284),(0.999732896029237,0.999865728939372,1.,0.994017305594881,
0.990889788836284),(0.999732896029237,0.999865728939372,1.,0.994017305594881,
0.990889788836284)))
REPRESENTATION_ITEM('')
SURFACE()
);
#2724=(
BOUNDED_SURFACE()
B_SPLINE_SURFACE(1,2,((#141041,#141042,#141043,#141044,#141045),(#141046,
#141047,#141048,#141049,#141050)),.UNSPECIFIED.,.F.,.F.,.F.)
B_SPLINE_SURFACE_WITH_KNOTS((2,2),(3,2,3),(0.,0.28980704099276),(0.573480748819524,
0.573654350219648,0.591014490232054),.UNSPECIFIED.)
GEOMETRIC_REPRESENTATION_ITEM()
RATIONAL_B_SPLINE_SURFACE(((0.998486152292053,0.998486152292053,0.998486152292053,
0.992772345172052,0.990020524139832),(0.998486152292053,0.998486152292053,
0.998486152292053,0.992772345172052,0.990020524139832)))
REPRESENTATION_ITEM('')
SURFACE()
);
#2725=(
BOUNDED_SURFACE()
B_SPLINE_SURFACE(1,2,((#141052,#141053,#141054,#141055,#141056),(#141057,
#141058,#141059,#141060,#141061)),.UNSPECIFIED.,.F.,.F.,.F.)
B_SPLINE_SURFACE_WITH_KNOTS((2,2),(3,2,3),(0.,0.289681084359925),(0.142474614281366,
0.142857142857143,0.159901408087481),.UNSPECIFIED.)
GEOMETRIC_REPRESENTATION_ITEM()
RATIONAL_B_SPLINE_SURFACE(((0.999732896029237,0.999865728939372,1.,0.994017305594881,
0.990889788836284),(0.999732896029237,0.999865728939372,1.,0.994017305594881,
0.990889788836284)))
REPRESENTATION_ITEM('')
SURFACE()
);
#2726=(
BOUNDED_SURFACE()
B_SPLINE_SURFACE(1,2,((#141070,#141071,#141072,#141073,#141074),(#141075,
#141076,#141077,#141078,#141079)),.UNSPECIFIED.,.F.,.F.,.F.)
B_SPLINE_SURFACE_WITH_KNOTS((2,2),(3,2,3),(0.,0.289807040992642),(0.57348074881979,
0.573654350219911,0.591014490232053),.UNSPECIFIED.)
GEOMETRIC_REPRESENTATION_ITEM()
RATIONAL_B_SPLINE_SURFACE(((0.99848615229188,0.99848615229188,0.99848615229188,
0.992772345172011,0.990020524139833),(0.99848615229188,0.99848615229188,
0.99848615229188,0.992772345172011,0.990020524139833)))
REPRESENTATION_ITEM('')
SURFACE()
);
#2727=(
BOUNDED_SURFACE()
B_SPLINE_SURFACE(1,2,((#141081,#141082,#141083,#141084,#141085),(#141086,
#141087,#141088,#141089,#141090)),.UNSPECIFIED.,.F.,.F.,.F.)
B_SPLINE_SURFACE_WITH_KNOTS((2,2),(3,2,3),(0.,0.289681084360439),(0.142474614281367,
0.142857142857143,0.159901408087482),.UNSPECIFIED.)
GEOMETRIC_REPRESENTATION_ITEM()
RATIONAL_B_SPLINE_SURFACE(((0.999732896029237,0.999865728939372,1.,0.994017305594881,
0.990889788836284),(0.999732896029237,0.999865728939372,1.,0.994017305594881,
0.990889788836284)))
REPRESENTATION_ITEM('')
SURFACE()
);
#2728=(
BOUNDED_SURFACE()
B_SPLINE_SURFACE(1,2,((#141099,#141100,#141101,#141102,#141103),(#141104,
#141105,#141106,#141107,#141108)),.UNSPECIFIED.,.F.,.F.,.F.)
B_SPLINE_SURFACE_WITH_KNOTS((2,2),(3,2,3),(0.,0.289807040993272),(0.573480748819715,
0.573654350219837,0.591014490232053),.UNSPECIFIED.)
GEOMETRIC_REPRESENTATION_ITEM()
RATIONAL_B_SPLINE_SURFACE(((0.998486152291929,0.998486152291929,0.998486152291929,
0.992772345172023,0.990020524139833),(0.998486152291929,0.998486152291929,
0.998486152291929,0.992772345172023,0.990020524139833)))
REPRESENTATION_ITEM('')
SURFACE()
);
#2729=(
BOUNDED_SURFACE()
B_SPLINE_SURFACE(1,2,((#141110,#141111,#141112,#141113,#141114),(#141115,
#141116,#141117,#141118,#141119)),.UNSPECIFIED.,.F.,.F.,.F.)
B_SPLINE_SURFACE_WITH_KNOTS((2,2),(3,2,3),(0.,0.289681084360251),(0.142474614281367,
0.142857142857143,0.159901408087481),.UNSPECIFIED.)
GEOMETRIC_REPRESENTATION_ITEM()
RATIONAL_B_SPLINE_SURFACE(((0.999732896029238,0.999865728939373,1.,0.994017305594881,
0.990889788836284),(0.999732896029238,0.999865728939373,1.,0.994017305594881,
0.990889788836284)))
REPRESENTATION_ITEM('')
SURFACE()
);
#2730=(
BOUNDED_SURFACE()
B_SPLINE_SURFACE(1,2,((#141128,#141129,#141130,#141131,#141132),(#141133,
#141134,#141135,#141136,#141137)),.UNSPECIFIED.,.F.,.F.,.F.)
B_SPLINE_SURFACE_WITH_KNOTS((2,2),(3,2,3),(0.,0.289807040991733),(0.57348074881979,
0.573654350219911,0.591014490232053),.UNSPECIFIED.)
GEOMETRIC_REPRESENTATION_ITEM()
RATIONAL_B_SPLINE_SURFACE(((0.99848615229188,0.99848615229188,0.99848615229188,
0.992772345172011,0.990020524139833),(0.99848615229188,0.99848615229188,
0.99848615229188,0.992772345172011,0.990020524139833)))
REPRESENTATION_ITEM('')
SURFACE()
);
#2731=(
BOUNDED_SURFACE()
B_SPLINE_SURFACE(1,2,((#141139,#141140,#141141,#141142,#141143),(#141144,
#141145,#141146,#141147,#141148)),.UNSPECIFIED.,.F.,.F.,.F.)
B_SPLINE_SURFACE_WITH_KNOTS((2,2),(3,2,3),(0.,0.289681084360222),(0.142474614281367,
0.142857142857143,0.159901408087481),.UNSPECIFIED.)
GEOMETRIC_REPRESENTATION_ITEM()
RATIONAL_B_SPLINE_SURFACE(((0.999732896029237,0.999865728939372,1.,0.994017305594881,
0.990889788836284),(0.999732896029237,0.999865728939372,1.,0.994017305594881,
0.990889788836284)))
REPRESENTATION_ITEM('')
SURFACE()
);
#2732=(
BOUNDED_SURFACE()
B_SPLINE_SURFACE(1,2,((#141157,#141158,#141159,#141160,#141161),(#141162,
#141163,#141164,#141165,#141166)),.UNSPECIFIED.,.F.,.F.,.F.)
B_SPLINE_SURFACE_WITH_KNOTS((2,2),(3,2,3),(0.,0.289807040992883),(0.573480748819775,
0.573654350219897,0.591014490232053),.UNSPECIFIED.)
GEOMETRIC_REPRESENTATION_ITEM()
RATIONAL_B_SPLINE_SURFACE(((0.998486152291889,0.998486152291889,0.998486152291889,
0.992772345172013,0.990020524139833),(0.998486152291889,0.998486152291889,
0.998486152291889,0.992772345172013,0.990020524139833)))
REPRESENTATION_ITEM('')
SURFACE()
);
#2733=(
BOUNDED_SURFACE()
B_SPLINE_SURFACE(1,2,((#141168,#141169,#141170,#141171,#141172),(#141173,
#141174,#141175,#141176,#141177)),.UNSPECIFIED.,.F.,.F.,.F.)
B_SPLINE_SURFACE_WITH_KNOTS((2,2),(3,2,3),(0.,0.289681084359925),(0.142474614281367,
0.142857142857143,0.159901408087481),.UNSPECIFIED.)
GEOMETRIC_REPRESENTATION_ITEM()
RATIONAL_B_SPLINE_SURFACE(((0.999732896029237,0.999865728939372,1.,0.994017305594881,
0.990889788836284),(0.999732896029237,0.999865728939372,1.,0.994017305594881,
0.990889788836284)))
REPRESENTATION_ITEM('')
SURFACE()
);
#2734=(
BOUNDED_SURFACE()
B_SPLINE_SURFACE(1,2,((#141186,#141187,#141188,#141189,#141190),(#141191,
#141192,#141193,#141194,#141195)),.UNSPECIFIED.,.F.,.F.,.F.)
B_SPLINE_SURFACE_WITH_KNOTS((2,2),(3,2,3),(0.,0.289807040992693),(0.57348074881979,
0.573654350219911,0.591014490232053),.UNSPECIFIED.)
GEOMETRIC_REPRESENTATION_ITEM()
RATIONAL_B_SPLINE_SURFACE(((0.99848615229188,0.99848615229188,0.99848615229188,
0.992772345172011,0.990020524139833),(0.99848615229188,0.99848615229188,
0.99848615229188,0.992772345172011,0.990020524139833)))
REPRESENTATION_ITEM('')
SURFACE()
);
#2735=(
BOUNDED_SURFACE()
B_SPLINE_SURFACE(1,2,((#141197,#141198,#141199,#141200,#141201),(#141202,
#141203,#141204,#141205,#141206),(#141207,#141208,#141209,#141210,#141211)),
 .UNSPECIFIED.,.F.,.F.,.F.)
B_SPLINE_SURFACE_WITH_KNOTS((2,1,2),(3,2,3),(-0.00289681084359929,0.,0.289681084359929),
(0.142474614281367,0.142857142857143,0.159901408087481),.UNSPECIFIED.)
GEOMETRIC_REPRESENTATION_ITEM()
RATIONAL_B_SPLINE_SURFACE(((0.999732896029238,0.999865728939373,1.,0.994017305594881,
0.990889788836284),(0.999732896029238,0.999865728939373,1.,0.994017305594881,
0.990889788836284),(0.999732896029238,0.999865728939373,1.,0.994017305594881,
0.990889788836284)))
REPRESENTATION_ITEM('')
SURFACE()
);
#2736=(
BOUNDED_SURFACE()
B_SPLINE_SURFACE(1,2,((#141220,#141221,#141222,#141223,#141224),(#141225,
#141226,#141227,#141228,#141229)),.UNSPECIFIED.,.F.,.F.,.F.)
B_SPLINE_SURFACE_WITH_KNOTS((2,2),(3,2,3),(0.,0.289807040993738),(0.573480748819763,
0.573654350219885,0.591014490232053),.UNSPECIFIED.)
GEOMETRIC_REPRESENTATION_ITEM()
RATIONAL_B_SPLINE_SURFACE(((0.998486152291897,0.998486152291897,0.998486152291897,
0.992772345172015,0.990020524139833),(0.998486152291897,0.998486152291897,
0.998486152291897,0.992772345172015,0.990020524139833)))
REPRESENTATION_ITEM('')
SURFACE()
);
#2737=(
BOUNDED_SURFACE()
B_SPLINE_SURFACE(1,2,((#141231,#141232,#141233,#141234,#141235),(#141236,
#141237,#141238,#141239,#141240),(#141241,#141242,#141243,#141244,#141245)),
 .UNSPECIFIED.,.F.,.F.,.F.)
B_SPLINE_SURFACE_WITH_KNOTS((2,1,2),(3,2,3),(-0.00289681084360253,0.,0.289681084360253),
(0.142474614281367,0.142857142857143,0.159901408087481),.UNSPECIFIED.)
GEOMETRIC_REPRESENTATION_ITEM()
RATIONAL_B_SPLINE_SURFACE(((0.999732896029237,0.999865728939372,1.,0.994017305594881,
0.990889788836284),(0.999732896029237,0.999865728939372,1.,0.994017305594881,
0.990889788836284),(0.999732896029237,0.999865728939372,1.,0.994017305594881,
0.990889788836284)))
REPRESENTATION_ITEM('')
SURFACE()
);
#2738=(
BOUNDED_SURFACE()
B_SPLINE_SURFACE(1,2,((#141254,#141255,#141256,#141257,#141258),(#141259,
#141260,#141261,#141262,#141263)),.UNSPECIFIED.,.F.,.F.,.F.)
B_SPLINE_SURFACE_WITH_KNOTS((2,2),(3,2,3),(0.,0.289807040991898),(0.57348074881979,
0.573654350219911,0.591014490232053),.UNSPECIFIED.)
GEOMETRIC_REPRESENTATION_ITEM()
RATIONAL_B_SPLINE_SURFACE(((0.99848615229188,0.99848615229188,0.99848615229188,
0.992772345172011,0.990020524139833),(0.99848615229188,0.99848615229188,
0.99848615229188,0.992772345172011,0.990020524139833)))
REPRESENTATION_ITEM('')
SURFACE()
);
#2739=(
BOUNDED_SURFACE()
B_SPLINE_SURFACE(1,2,((#141265,#141266,#141267,#141268,#141269),(#141270,
#141271,#141272,#141273,#141274)),.UNSPECIFIED.,.F.,.F.,.F.)
B_SPLINE_SURFACE_WITH_KNOTS((2,2),(3,2,3),(0.,0.289681084361046),(0.142474614281368,
0.142857142857143,0.159901408087495),.UNSPECIFIED.)
GEOMETRIC_REPRESENTATION_ITEM()
RATIONAL_B_SPLINE_SURFACE(((0.999732896029238,0.999865728939373,1.,0.994017305594876,
0.990889788836279),(0.999732896029238,0.999865728939373,1.,0.994017305594876,
0.990889788836279)))
REPRESENTATION_ITEM('')
SURFACE()
);
#2740=(
BOUNDED_SURFACE()
B_SPLINE_SURFACE(1,2,((#141283,#141284,#141285,#141286,#141287),(#141288,
#141289,#141290,#141291,#141292)),.UNSPECIFIED.,.F.,.F.,.F.)
B_SPLINE_SURFACE_WITH_KNOTS((2,2),(3,2,3),(0.,0.28980704099156),(0.573480748819789,
0.57365435021991,0.591014490232052),.UNSPECIFIED.)
GEOMETRIC_REPRESENTATION_ITEM()
RATIONAL_B_SPLINE_SURFACE(((0.99848615229188,0.99848615229188,0.99848615229188,
0.992772345172012,0.990020524139833),(0.99848615229188,0.99848615229188,
0.99848615229188,0.992772345172012,0.990020524139833)))
REPRESENTATION_ITEM('')
SURFACE()
);
#2741=(
BOUNDED_SURFACE()
B_SPLINE_SURFACE(1,2,((#141294,#141295,#141296,#141297,#141298),(#141299,
#141300,#141301,#141302,#141303)),.UNSPECIFIED.,.F.,.F.,.F.)
B_SPLINE_SURFACE_WITH_KNOTS((2,2),(3,2,3),(0.,0.289681084360513),(0.142474614281368,
0.142857142857143,0.159901408087482),.UNSPECIFIED.)
GEOMETRIC_REPRESENTATION_ITEM()
RATIONAL_B_SPLINE_SURFACE(((0.999732896029238,0.999865728939373,1.,0.994017305594881,
0.990889788836284),(0.999732896029238,0.999865728939373,1.,0.994017305594881,
0.990889788836284)))
REPRESENTATION_ITEM('')
SURFACE()
);
#2742=(
BOUNDED_SURFACE()
B_SPLINE_SURFACE(1,2,((#141312,#141313,#141314,#141315,#141316),(#141317,
#141318,#141319,#141320,#141321)),.UNSPECIFIED.,.F.,.F.,.F.)
B_SPLINE_SURFACE_WITH_KNOTS((2,2),(3,2,3),(0.,0.289807040991555),(0.573480748819707,
0.573654350219829,0.591014490232052),.UNSPECIFIED.)
GEOMETRIC_REPRESENTATION_ITEM()
RATIONAL_B_SPLINE_SURFACE(((0.998486152291934,0.998486152291934,0.998486152291934,
0.992772345172024,0.990020524139833),(0.998486152291934,0.998486152291934,
0.998486152291934,0.992772345172024,0.990020524139833)))
REPRESENTATION_ITEM('')
SURFACE()
);
#2743=(
BOUNDED_SURFACE()
B_SPLINE_SURFACE(1,2,((#141323,#141324,#141325,#141326,#141327),(#141328,
#141329,#141330,#141331,#141332)),.UNSPECIFIED.,.F.,.F.,.F.)
B_SPLINE_SURFACE_WITH_KNOTS((2,2),(3,2,3),(0.,0.289681084359919),(0.142474614281368,
0.142857142857143,0.159901408087482),.UNSPECIFIED.)
GEOMETRIC_REPRESENTATION_ITEM()
RATIONAL_B_SPLINE_SURFACE(((0.999732896029238,0.999865728939373,1.,0.994017305594881,
0.990889788836283),(0.999732896029238,0.999865728939373,1.,0.994017305594881,
0.990889788836283)))
REPRESENTATION_ITEM('')
SURFACE()
);
#2744=(
BOUNDED_SURFACE()
B_SPLINE_SURFACE(1,2,((#141341,#141342,#141343,#141344,#141345),(#141346,
#141347,#141348,#141349,#141350)),.UNSPECIFIED.,.F.,.F.,.F.)
B_SPLINE_SURFACE_WITH_KNOTS((2,2),(3,2,3),(0.,0.289807040991694),(0.573480748819707,
0.573654350219829,0.591014490232052),.UNSPECIFIED.)
GEOMETRIC_REPRESENTATION_ITEM()
RATIONAL_B_SPLINE_SURFACE(((0.998486152291934,0.998486152291934,0.998486152291934,
0.992772345172024,0.990020524139833),(0.998486152291934,0.998486152291934,
0.998486152291934,0.992772345172024,0.990020524139833)))
REPRESENTATION_ITEM('')
SURFACE()
);
#2745=(
BOUNDED_SURFACE()
B_SPLINE_SURFACE(1,2,((#141352,#141353,#141354,#141355,#141356),(#141357,
#141358,#141359,#141360,#141361),(#141362,#141363,#141364,#141365,#141366)),
 .UNSPECIFIED.,.F.,.F.,.F.)
B_SPLINE_SURFACE_WITH_KNOTS((2,1,2),(3,2,3),(-0.00289681084360272,0.,0.289681084360272),
(0.142474614281368,0.142857142857143,0.159901408087482),.UNSPECIFIED.)
GEOMETRIC_REPRESENTATION_ITEM()
RATIONAL_B_SPLINE_SURFACE(((0.999732896029238,0.999865728939373,1.,0.994017305594881,
0.990889788836284),(0.999732896029238,0.999865728939373,1.,0.994017305594881,
0.990889788836284),(0.999732896029238,0.999865728939373,1.,0.994017305594881,
0.990889788836284)))
REPRESENTATION_ITEM('')
SURFACE()
);
#2746=(
BOUNDED_SURFACE()
B_SPLINE_SURFACE(1,2,((#141368,#141369,#141370),(#141371,#141372,#141373)),
 .UNSPECIFIED.,.F.,.F.,.F.)
B_SPLINE_SURFACE_WITH_KNOTS((2,2),(3,3),(0.,0.289807040991566),(0.194132688793569,
0.211606804210308),.UNSPECIFIED.)
GEOMETRIC_REPRESENTATION_ITEM()
RATIONAL_B_SPLINE_SURFACE(((0.989843896581211,0.992516389311156,0.998189888755648),
(0.989843896581211,0.992516389311156,0.998189888755648)))
REPRESENTATION_ITEM('')
SURFACE()
);
#2747=(
BOUNDED_SURFACE()
B_SPLINE_SURFACE(1,2,((#141390,#141391,#141392,#141393,#141394),(#141395,
#141396,#141397,#141398,#141399)),.UNSPECIFIED.,.F.,.F.,.F.)
B_SPLINE_SURFACE_WITH_KNOTS((2,2),(3,2,3),(0.,0.290272734870772),(0.521815037222016,
0.53899963051341,0.539591284257231),.UNSPECIFIED.)
GEOMETRIC_REPRESENTATION_ITEM()
RATIONAL_B_SPLINE_SURFACE(((0.989362668575565,0.987015160230477,0.987570037304351,
0.987570037304351,0.987570037304351),(0.989362668575565,0.987015160230477,
0.987570037304351,0.987570037304351,0.987570037304351)))
REPRESENTATION_ITEM('')
SURFACE()
);
#2748=(
BOUNDED_SURFACE()
B_SPLINE_SURFACE(1,2,((#141401,#141402,#141403),(#141404,#141405,#141406)),
 .UNSPECIFIED.,.F.,.F.,.F.)
B_SPLINE_SURFACE_WITH_KNOTS((2,2),(3,3),(0.,0.289807040991565),(0.194132688793569,
0.211606804210307),.UNSPECIFIED.)
GEOMETRIC_REPRESENTATION_ITEM()
RATIONAL_B_SPLINE_SURFACE(((0.989843896581211,0.992516389311156,0.998189888755648),
(0.989843896581211,0.992516389311156,0.998189888755648)))
REPRESENTATION_ITEM('')
SURFACE()
);
#2749=(
BOUNDED_SURFACE()
B_SPLINE_SURFACE(1,2,((#141423,#141424,#141425,#141426,#141427),(#141428,
#141429,#141430,#141431,#141432)),.UNSPECIFIED.,.F.,.F.,.F.)
B_SPLINE_SURFACE_WITH_KNOTS((2,2),(3,2,3),(0.,0.290272734853992),(0.521815037222017,
0.538999630513411,0.539591284240711),.UNSPECIFIED.)
GEOMETRIC_REPRESENTATION_ITEM()
RATIONAL_B_SPLINE_SURFACE(((0.989362668575565,0.987015160230477,0.987570037304351,
0.987570037304351,0.987570037304351),(0.989362668575565,0.987015160230477,
0.987570037304351,0.987570037304351,0.987570037304351)))
REPRESENTATION_ITEM('')
SURFACE()
);
#2750=(
BOUNDED_SURFACE()
B_SPLINE_SURFACE(1,2,((#141434,#141435,#141436),(#141437,#141438,#141439)),
 .UNSPECIFIED.,.F.,.F.,.F.)
B_SPLINE_SURFACE_WITH_KNOTS((2,2),(3,3),(0.,0.289807040991569),(0.194132688793568,
0.211606804210307),.UNSPECIFIED.)
GEOMETRIC_REPRESENTATION_ITEM()
RATIONAL_B_SPLINE_SURFACE(((0.989843896581211,0.992516389311156,0.998189888755648),
(0.989843896581211,0.992516389311156,0.998189888755648)))
REPRESENTATION_ITEM('')
SURFACE()
);
#2751=(
BOUNDED_SURFACE()
B_SPLINE_SURFACE(1,2,((#141456,#141457,#141458,#141459,#141460),(#141461,
#141462,#141463,#141464,#141465)),.UNSPECIFIED.,.F.,.F.,.F.)
B_SPLINE_SURFACE_WITH_KNOTS((2,2),(3,2,3),(0.,0.290272734861209),(0.521815037222017,
0.538999630513411,0.539591284247956),.UNSPECIFIED.)
GEOMETRIC_REPRESENTATION_ITEM()
RATIONAL_B_SPLINE_SURFACE(((0.989362668575565,0.987015160230477,0.987570037304351,
0.987570037304351,0.987570037304351),(0.989362668575565,0.987015160230477,
0.987570037304351,0.987570037304351,0.987570037304351)))
REPRESENTATION_ITEM('')
SURFACE()
);
#2752=(
BOUNDED_SURFACE()
B_SPLINE_SURFACE(1,2,((#141467,#141468,#141469),(#141470,#141471,#141472)),
 .UNSPECIFIED.,.F.,.F.,.F.)
B_SPLINE_SURFACE_WITH_KNOTS((2,2),(3,3),(0.,0.289807040991558),(0.194132688793568,
0.211606804210307),.UNSPECIFIED.)
GEOMETRIC_REPRESENTATION_ITEM()
RATIONAL_B_SPLINE_SURFACE(((0.989843896581211,0.992516389311156,0.998189888755648),
(0.989843896581211,0.992516389311156,0.998189888755648)))
REPRESENTATION_ITEM('')
SURFACE()
);
#2753=(
BOUNDED_SURFACE()
B_SPLINE_SURFACE(1,2,((#141489,#141490,#141491,#141492,#141493),(#141494,
#141495,#141496,#141497,#141498)),.UNSPECIFIED.,.F.,.F.,.F.)
B_SPLINE_SURFACE_WITH_KNOTS((2,2),(3,2,3),(0.,0.290272734854879),(0.521815037222017,
0.538999630513411,0.539591284241346),.UNSPECIFIED.)
GEOMETRIC_REPRESENTATION_ITEM()
RATIONAL_B_SPLINE_SURFACE(((0.989362668575565,0.987015160230477,0.987570037304351,
0.987570037304351,0.987570037304351),(0.989362668575565,0.987015160230477,
0.987570037304351,0.987570037304351,0.987570037304351)))
REPRESENTATION_ITEM('')
SURFACE()
);
#2754=(
BOUNDED_SURFACE()
B_SPLINE_SURFACE(1,2,((#141500,#141501,#141502),(#141503,#141504,#141505)),
 .UNSPECIFIED.,.F.,.F.,.F.)
B_SPLINE_SURFACE_WITH_KNOTS((2,2),(3,3),(0.,0.28980704099156),(0.194132688793568,
0.211606804210307),.UNSPECIFIED.)
GEOMETRIC_REPRESENTATION_ITEM()
RATIONAL_B_SPLINE_SURFACE(((0.989843896581211,0.992516389311156,0.998189888755648),
(0.989843896581211,0.992516389311156,0.998189888755648)))
REPRESENTATION_ITEM('')
SURFACE()
);
#2755=(
BOUNDED_SURFACE()
B_SPLINE_SURFACE(1,2,((#141522,#141523,#141524,#141525,#141526),(#141527,
#141528,#141529,#141530,#141531)),.UNSPECIFIED.,.F.,.F.,.F.)
B_SPLINE_SURFACE_WITH_KNOTS((2,2),(3,2,3),(0.,0.290272734843646),(0.521815037222017,
0.538999630513411,0.539591284230401),.UNSPECIFIED.)
GEOMETRIC_REPRESENTATION_ITEM()
RATIONAL_B_SPLINE_SURFACE(((0.989362668575565,0.987015160230477,0.987570037304351,
0.987570037304351,0.987570037304351),(0.989362668575565,0.987015160230477,
0.987570037304351,0.987570037304351,0.987570037304351)))
REPRESENTATION_ITEM('')
SURFACE()
);
#2756=(
BOUNDED_SURFACE()
B_SPLINE_SURFACE(1,2,((#141533,#141534,#141535),(#141536,#141537,#141538)),
 .UNSPECIFIED.,.F.,.F.,.F.)
B_SPLINE_SURFACE_WITH_KNOTS((2,2),(3,3),(0.,0.289807040991562),(0.194132688793568,
0.211606804210307),.UNSPECIFIED.)
GEOMETRIC_REPRESENTATION_ITEM()
RATIONAL_B_SPLINE_SURFACE(((0.989843896581211,0.992516389311156,0.998189888755648),
(0.989843896581211,0.992516389311156,0.998189888755648)))
REPRESENTATION_ITEM('')
SURFACE()
);
#2757=(
BOUNDED_SURFACE()
B_SPLINE_SURFACE(1,2,((#141555,#141556,#141557,#141558,#141559),(#141560,
#141561,#141562,#141563,#141564)),.UNSPECIFIED.,.F.,.F.,.F.)
B_SPLINE_SURFACE_WITH_KNOTS((2,2),(3,2,3),(0.,0.290272734900014),(0.521815037222017,
0.538999630513411,0.53959128428651),.UNSPECIFIED.)
GEOMETRIC_REPRESENTATION_ITEM()
RATIONAL_B_SPLINE_SURFACE(((0.989362668575565,0.987015160230477,0.987570037304351,
0.987570037304351,0.987570037304351),(0.989362668575565,0.987015160230477,
0.987570037304351,0.987570037304351,0.987570037304351)))
REPRESENTATION_ITEM('')
SURFACE()
);
#2758=(
BOUNDED_SURFACE()
B_SPLINE_SURFACE(1,2,((#141566,#141567,#141568),(#141569,#141570,#141571)),
 .UNSPECIFIED.,.F.,.F.,.F.)
B_SPLINE_SURFACE_WITH_KNOTS((2,2),(3,3),(0.,0.289807040991558),(0.194132688793568,
0.211606804210307),.UNSPECIFIED.)
GEOMETRIC_REPRESENTATION_ITEM()
RATIONAL_B_SPLINE_SURFACE(((0.989843896581211,0.992516389311156,0.998189888755648),
(0.98984389658121,0.992516389311155,0.998189888755648)))
REPRESENTATION_ITEM('')
SURFACE()
);
#2759=(
BOUNDED_SURFACE()
B_SPLINE_SURFACE(1,2,((#141588,#141589,#141590,#141591,#141592),(#141593,
#141594,#141595,#141596,#141597)),.UNSPECIFIED.,.F.,.F.,.F.)
B_SPLINE_SURFACE_WITH_KNOTS((2,2),(3,2,3),(0.,0.29027273486563),(0.521815037222018,
0.538999630513412,0.53959128425217),.UNSPECIFIED.)
GEOMETRIC_REPRESENTATION_ITEM()
RATIONAL_B_SPLINE_SURFACE(((0.989362668575565,0.987015160230477,0.987570037304351,
0.987570037304351,0.987570037304351),(0.989362668575565,0.987015160230477,
0.987570037304351,0.987570037304351,0.987570037304351)))
REPRESENTATION_ITEM('')
SURFACE()
);
#2760=(
BOUNDED_SURFACE()
B_SPLINE_SURFACE(1,2,((#141599,#141600,#141601),(#141602,#141603,#141604)),
 .UNSPECIFIED.,.F.,.F.,.F.)
B_SPLINE_SURFACE_WITH_KNOTS((2,2),(3,3),(0.,0.289807040991555),(0.194132688793568,
0.211606804210307),.UNSPECIFIED.)
GEOMETRIC_REPRESENTATION_ITEM()
RATIONAL_B_SPLINE_SURFACE(((0.989843896581211,0.992516389311156,0.998189888755647),
(0.989843896581211,0.992516389311156,0.998189888755647)))
REPRESENTATION_ITEM('')
SURFACE()
);
#2761=(
BOUNDED_SURFACE()
B_SPLINE_SURFACE(1,2,((#141621,#141622,#141623,#141624,#141625),(#141626,
#141627,#141628,#141629,#141630)),.UNSPECIFIED.,.F.,.F.,.F.)
B_SPLINE_SURFACE_WITH_KNOTS((2,2),(3,2,3),(0.,0.290272734845788),(0.521815037222017,
0.538999630513411,0.53959128423262),.UNSPECIFIED.)
GEOMETRIC_REPRESENTATION_ITEM()
RATIONAL_B_SPLINE_SURFACE(((0.989362668575565,0.987015160230477,0.987570037304351,
0.987570037304351,0.987570037304351),(0.989362668575565,0.987015160230477,
0.987570037304351,0.987570037304351,0.987570037304351)))
REPRESENTATION_ITEM('')
SURFACE()
);
#2762=(
BOUNDED_SURFACE()
B_SPLINE_SURFACE(1,2,((#141632,#141633,#141634),(#141635,#141636,#141637)),
 .UNSPECIFIED.,.F.,.F.,.F.)
B_SPLINE_SURFACE_WITH_KNOTS((2,2),(3,3),(0.,0.289807040991559),(0.194132688793568,
0.211606804210307),.UNSPECIFIED.)
GEOMETRIC_REPRESENTATION_ITEM()
RATIONAL_B_SPLINE_SURFACE(((0.989843896581211,0.992516389311155,0.998189888755647),
(0.98984389658121,0.992516389311155,0.998189888755647)))
REPRESENTATION_ITEM('')
SURFACE()
);
#2763=(
BOUNDED_SURFACE()
B_SPLINE_SURFACE(1,2,((#141654,#141655,#141656,#141657,#141658),(#141659,
#141660,#141661,#141662,#141663)),.UNSPECIFIED.,.F.,.F.,.F.)
B_SPLINE_SURFACE_WITH_KNOTS((2,2),(3,2,3),(0.,0.290272734861932),(0.521815037222016,
0.538999630513411,0.539591284248474),.UNSPECIFIED.)
GEOMETRIC_REPRESENTATION_ITEM()
RATIONAL_B_SPLINE_SURFACE(((0.989362668575565,0.987015160230477,0.987570037304351,
0.987570037304351,0.987570037304351),(0.989362668575565,0.987015160230477,
0.987570037304351,0.987570037304351,0.987570037304351)))
REPRESENTATION_ITEM('')
SURFACE()
);
#2764=(
BOUNDED_SURFACE()
B_SPLINE_SURFACE(1,2,((#141665,#141666,#141667),(#141668,#141669,#141670)),
 .UNSPECIFIED.,.F.,.F.,.F.)
B_SPLINE_SURFACE_WITH_KNOTS((2,2),(3,3),(0.,0.289807040991563),(0.194132688793568,
0.211606804210303),.UNSPECIFIED.)
GEOMETRIC_REPRESENTATION_ITEM()
RATIONAL_B_SPLINE_SURFACE(((0.989843896581211,0.992516389311155,0.998189888755645),
(0.989843896581211,0.992516389311155,0.998189888755645)))
REPRESENTATION_ITEM('')
SURFACE()
);
#2765=(
BOUNDED_SURFACE()
B_SPLINE_SURFACE(1,2,((#141687,#141688,#141689,#141690,#141691),(#141692,
#141693,#141694,#141695,#141696)),.UNSPECIFIED.,.F.,.F.,.F.)
B_SPLINE_SURFACE_WITH_KNOTS((2,2),(3,2,3),(0.,0.290272734862812),(0.521815037221715,
0.538999630513411,0.539591284249576),.UNSPECIFIED.)
GEOMETRIC_REPRESENTATION_ITEM()
RATIONAL_B_SPLINE_SURFACE(((0.989362668575647,0.987015160230467,0.987570037304351,
0.987570037304351,0.987570037304351),(0.989362668575647,0.987015160230467,
0.987570037304351,0.987570037304351,0.987570037304351)))
REPRESENTATION_ITEM('')
SURFACE()
);
#2766=(
BOUNDED_SURFACE()
B_SPLINE_SURFACE(1,2,((#141698,#141699,#141700),(#141701,#141702,#141703)),
 .UNSPECIFIED.,.F.,.F.,.F.)
B_SPLINE_SURFACE_WITH_KNOTS((2,2),(3,3),(0.,0.289807040991562),(0.194132688793568,
0.211606804210307),.UNSPECIFIED.)
GEOMETRIC_REPRESENTATION_ITEM()
RATIONAL_B_SPLINE_SURFACE(((0.989843896581211,0.992516389311156,0.998189888755648),
(0.989843896581211,0.992516389311156,0.998189888755648)))
REPRESENTATION_ITEM('')
SURFACE()
);
#2767=(
BOUNDED_SURFACE()
B_SPLINE_SURFACE(1,2,((#141720,#141721,#141722,#141723,#141724),(#141725,
#141726,#141727,#141728,#141729)),.UNSPECIFIED.,.F.,.F.,.F.)
B_SPLINE_SURFACE_WITH_KNOTS((2,2),(3,2,3),(0.,0.290272734843879),(0.521815037222017,
0.538999630513411,0.539591284230428),.UNSPECIFIED.)
GEOMETRIC_REPRESENTATION_ITEM()
RATIONAL_B_SPLINE_SURFACE(((0.989362668575565,0.987015160230477,0.987570037304351,
0.987570037304351,0.987570037304351),(0.989362668575565,0.987015160230477,
0.987570037304351,0.987570037304351,0.987570037304351)))
REPRESENTATION_ITEM('')
SURFACE()
);
#2768=(
BOUNDED_SURFACE()
B_SPLINE_SURFACE(1,2,((#141731,#141732,#141733),(#141734,#141735,#141736)),
 .UNSPECIFIED.,.F.,.F.,.F.)
B_SPLINE_SURFACE_WITH_KNOTS((2,2),(3,3),(0.,0.289807040991565),(0.194132688793568,
0.211606804210307),.UNSPECIFIED.)
GEOMETRIC_REPRESENTATION_ITEM()
RATIONAL_B_SPLINE_SURFACE(((0.989843896581211,0.992516389311156,0.998189888755648),
(0.989843896581211,0.992516389311156,0.998189888755648)))
REPRESENTATION_ITEM('')
SURFACE()
);
#2769=(
BOUNDED_SURFACE()
B_SPLINE_SURFACE(1,2,((#141753,#141754,#141755,#141756,#141757),(#141758,
#141759,#141760,#141761,#141762)),.UNSPECIFIED.,.F.,.F.,.F.)
B_SPLINE_SURFACE_WITH_KNOTS((2,2),(3,2,3),(0.,0.290272734865575),(0.52181503722185,
0.538999630513411,0.539591284252381),.UNSPECIFIED.)
GEOMETRIC_REPRESENTATION_ITEM()
RATIONAL_B_SPLINE_SURFACE(((0.989362668575611,0.987015160230471,0.987570037304351,
0.987570037304351,0.987570037304351),(0.989362668575611,0.987015160230471,
0.987570037304351,0.987570037304351,0.987570037304351)))
REPRESENTATION_ITEM('')
SURFACE()
);
#2770=(
BOUNDED_SURFACE()
B_SPLINE_SURFACE(1,2,((#141764,#141765,#141766),(#141767,#141768,#141769)),
 .UNSPECIFIED.,.F.,.F.,.F.)
B_SPLINE_SURFACE_WITH_KNOTS((2,2),(3,3),(0.,0.289807040991564),(0.194132688793568,
0.211606804210307),.UNSPECIFIED.)
GEOMETRIC_REPRESENTATION_ITEM()
RATIONAL_B_SPLINE_SURFACE(((0.989843896581211,0.992516389311155,0.998189888755648),
(0.989843896581211,0.992516389311155,0.998189888755648)))
REPRESENTATION_ITEM('')
SURFACE()
);
#2771=(
BOUNDED_SURFACE()
B_SPLINE_SURFACE(1,2,((#141786,#141787,#141788,#141789,#141790),(#141791,
#141792,#141793,#141794,#141795)),.UNSPECIFIED.,.F.,.F.,.F.)
B_SPLINE_SURFACE_WITH_KNOTS((2,2),(3,2,3),(0.,0.290272734871367),(0.52181503722181,
0.538999630513411,0.539591284258078),.UNSPECIFIED.)
GEOMETRIC_REPRESENTATION_ITEM()
RATIONAL_B_SPLINE_SURFACE(((0.989362668575621,0.98701516023047,0.987570037304351,
0.987570037304351,0.987570037304351),(0.989362668575621,0.98701516023047,
0.987570037304351,0.987570037304351,0.987570037304351)))
REPRESENTATION_ITEM('')
SURFACE()
);
#2772=(
BOUNDED_SURFACE()
B_SPLINE_SURFACE(1,2,((#141797,#141798,#141799),(#141800,#141801,#141802)),
 .UNSPECIFIED.,.F.,.F.,.F.)
B_SPLINE_SURFACE_WITH_KNOTS((2,2),(3,3),(0.,0.289807040991565),(0.194132688793568,
0.211606804210307),.UNSPECIFIED.)
GEOMETRIC_REPRESENTATION_ITEM()
RATIONAL_B_SPLINE_SURFACE(((0.989843896581211,0.992516389311155,0.998189888755648),
(0.989843896581211,0.992516389311155,0.998189888755648)))
REPRESENTATION_ITEM('')
SURFACE()
);
#2773=(
BOUNDED_SURFACE()
B_SPLINE_SURFACE(1,2,((#141819,#141820,#141821,#141822,#141823),(#141824,
#141825,#141826,#141827,#141828)),.UNSPECIFIED.,.F.,.F.,.F.)
B_SPLINE_SURFACE_WITH_KNOTS((2,2),(3,2,3),(0.,0.290272734855448),(0.521815037221533,
0.538999630513411,0.539591284242046),.UNSPECIFIED.)
GEOMETRIC_REPRESENTATION_ITEM()
RATIONAL_B_SPLINE_SURFACE(((0.989362668575697,0.987015160230461,0.987570037304351,
0.987570037304351,0.987570037304351),(0.989362668575697,0.987015160230461,
0.987570037304351,0.987570037304351,0.987570037304351)))
REPRESENTATION_ITEM('')
SURFACE()
);
#2774=(
BOUNDED_SURFACE()
B_SPLINE_SURFACE(1,2,((#141830,#141831,#141832),(#141833,#141834,#141835)),
 .UNSPECIFIED.,.F.,.F.,.F.)
B_SPLINE_SURFACE_WITH_KNOTS((2,2),(3,3),(0.,0.28980704099156),(0.194132688793568,
0.211606804210307),.UNSPECIFIED.)
GEOMETRIC_REPRESENTATION_ITEM()
RATIONAL_B_SPLINE_SURFACE(((0.989843896581211,0.992516389311155,0.998189888755648),
(0.989843896581211,0.992516389311155,0.998189888755648)))
REPRESENTATION_ITEM('')
SURFACE()
);
#2775=(
BOUNDED_SURFACE()
B_SPLINE_SURFACE(1,2,((#141843,#141844,#141845,#141846,#141847),(#141848,
#141849,#141850,#141851,#141852)),.UNSPECIFIED.,.F.,.F.,.F.)
B_SPLINE_SURFACE_WITH_KNOTS((2,2),(3,2,3),(0.,0.290272734861199),(0.521815037221924,
0.538999630513411,0.539591284247793),.UNSPECIFIED.)
GEOMETRIC_REPRESENTATION_ITEM()
RATIONAL_B_SPLINE_SURFACE(((0.98936266857559,0.987015160230474,0.987570037304351,
0.987570037304351,0.987570037304351),(0.98936266857559,0.987015160230474,
0.987570037304351,0.987570037304351,0.987570037304351)))
REPRESENTATION_ITEM('')
SURFACE()
);
#2776=(
BOUNDED_SURFACE()
B_SPLINE_SURFACE(1,2,((#141854,#141855,#141856),(#141857,#141858,#141859)),
 .UNSPECIFIED.,.F.,.F.,.F.)
B_SPLINE_SURFACE_WITH_KNOTS((2,2),(3,3),(0.,0.289807040991564),(0.194132688793568,
0.211606804210307),.UNSPECIFIED.)
GEOMETRIC_REPRESENTATION_ITEM()
RATIONAL_B_SPLINE_SURFACE(((0.989843896581211,0.992516389311156,0.998189888755648),
(0.989843896581211,0.992516389311156,0.998189888755648)))
REPRESENTATION_ITEM('')
SURFACE()
);
#2777=(
BOUNDED_SURFACE()
B_SPLINE_SURFACE(1,2,((#141876,#141877,#141878,#141879,#141880),(#141881,
#141882,#141883,#141884,#141885)),.UNSPECIFIED.,.F.,.F.,.F.)
B_SPLINE_SURFACE_WITH_KNOTS((2,2),(3,2,3),(0.,0.290272734855005),(0.521815037222017,
0.538999630513411,0.539591284241809),.UNSPECIFIED.)
GEOMETRIC_REPRESENTATION_ITEM()
RATIONAL_B_SPLINE_SURFACE(((0.989362668575565,0.987015160230477,0.987570037304351,
0.987570037304351,0.987570037304351),(0.989362668575565,0.987015160230477,
0.987570037304351,0.987570037304351,0.987570037304351)))
REPRESENTATION_ITEM('')
SURFACE()
);
#2778=(
BOUNDED_SURFACE()
B_SPLINE_SURFACE(1,2,((#141887,#141888,#141889),(#141890,#141891,#141892)),
 .UNSPECIFIED.,.F.,.F.,.F.)
B_SPLINE_SURFACE_WITH_KNOTS((2,2),(3,3),(0.,0.28980704099156),(0.194132688793568,
0.211606804210307),.UNSPECIFIED.)
GEOMETRIC_REPRESENTATION_ITEM()
RATIONAL_B_SPLINE_SURFACE(((0.98984389658121,0.992516389311155,0.998189888755648),
(0.98984389658121,0.992516389311155,0.998189888755648)))
REPRESENTATION_ITEM('')
SURFACE()
);
#2779=(
BOUNDED_SURFACE()
B_SPLINE_SURFACE(1,2,((#141909,#141910,#141911,#141912,#141913),(#141914,
#141915,#141916,#141917,#141918)),.UNSPECIFIED.,.F.,.F.,.F.)
B_SPLINE_SURFACE_WITH_KNOTS((2,2),(3,2,3),(0.,0.290272734863187),(0.521815037222017,
0.538999630513411,0.539591284249797),.UNSPECIFIED.)
GEOMETRIC_REPRESENTATION_ITEM()
RATIONAL_B_SPLINE_SURFACE(((0.989362668575565,0.987015160230477,0.987570037304351,
0.987570037304351,0.987570037304351),(0.989362668575565,0.987015160230477,
0.987570037304351,0.987570037304351,0.987570037304351)))
REPRESENTATION_ITEM('')
SURFACE()
);
#2780=(
BOUNDED_SURFACE()
B_SPLINE_SURFACE(1,2,((#141920,#141921,#141922),(#141923,#141924,#141925)),
 .UNSPECIFIED.,.F.,.F.,.F.)
B_SPLINE_SURFACE_WITH_KNOTS((2,2),(3,3),(0.,0.289807040991561),(0.194132688793568,
0.211606804210307),.UNSPECIFIED.)
GEOMETRIC_REPRESENTATION_ITEM()
RATIONAL_B_SPLINE_SURFACE(((0.989843896581211,0.992516389311156,0.998189888755648),
(0.989843896581211,0.992516389311156,0.998189888755648)))
REPRESENTATION_ITEM('')
SURFACE()
);
#2781=(
BOUNDED_SURFACE()
B_SPLINE_SURFACE(1,2,((#141942,#141943,#141944,#141945,#141946),(#141947,
#141948,#141949,#141950,#141951)),.UNSPECIFIED.,.F.,.F.,.F.)
B_SPLINE_SURFACE_WITH_KNOTS((2,2),(3,2,3),(0.,0.2902727348764),(0.521815037222017,
0.538999630513411,0.539591284262947),.UNSPECIFIED.)
GEOMETRIC_REPRESENTATION_ITEM()
RATIONAL_B_SPLINE_SURFACE(((0.989362668575565,0.987015160230477,0.987570037304351,
0.987570037304351,0.987570037304351),(0.989362668575565,0.987015160230477,
0.987570037304351,0.987570037304351,0.987570037304351)))
REPRESENTATION_ITEM('')
SURFACE()
);
#2782=(
BOUNDED_SURFACE()
B_SPLINE_SURFACE(1,2,((#141953,#141954,#141955),(#141956,#141957,#141958)),
 .UNSPECIFIED.,.F.,.F.,.F.)
B_SPLINE_SURFACE_WITH_KNOTS((2,2),(3,3),(0.,0.289807040991562),(0.194132688793568,
0.211606804210307),.UNSPECIFIED.)
GEOMETRIC_REPRESENTATION_ITEM()
RATIONAL_B_SPLINE_SURFACE(((0.989843896581211,0.992516389311156,0.998189888755648),
(0.989843896581211,0.992516389311156,0.998189888755648)))
REPRESENTATION_ITEM('')
SURFACE()
);
#2783=(
BOUNDED_SURFACE()
B_SPLINE_SURFACE(1,2,((#141975,#141976,#141977,#141978,#141979),(#141980,
#141981,#141982,#141983,#141984)),.UNSPECIFIED.,.F.,.F.,.F.)
B_SPLINE_SURFACE_WITH_KNOTS((2,2),(3,2,3),(0.,0.290272734866835),(0.521815037222017,
0.538999630513411,0.539591284253334),.UNSPECIFIED.)
GEOMETRIC_REPRESENTATION_ITEM()
RATIONAL_B_SPLINE_SURFACE(((0.989362668575565,0.987015160230477,0.987570037304351,
0.987570037304351,0.987570037304351),(0.989362668575565,0.987015160230477,
0.987570037304351,0.987570037304351,0.987570037304351)))
REPRESENTATION_ITEM('')
SURFACE()
);
#2784=(
BOUNDED_SURFACE()
B_SPLINE_SURFACE(1,2,((#141986,#141987,#141988),(#141989,#141990,#141991)),
 .UNSPECIFIED.,.F.,.F.,.F.)
B_SPLINE_SURFACE_WITH_KNOTS((2,2),(3,3),(0.,0.289807040991556),(0.194132688793568,
0.211606804210307),.UNSPECIFIED.)
GEOMETRIC_REPRESENTATION_ITEM()
RATIONAL_B_SPLINE_SURFACE(((0.98984389658121,0.992516389311155,0.998189888755648),
(0.98984389658121,0.992516389311155,0.998189888755648)))
REPRESENTATION_ITEM('')
SURFACE()
);
#2785=(
BOUNDED_SURFACE()
B_SPLINE_SURFACE(1,2,((#142002,#142003,#142004,#142005,#142006),(#142007,
#142008,#142009,#142010,#142011)),.UNSPECIFIED.,.F.,.F.,.F.)
B_SPLINE_SURFACE_WITH_KNOTS((2,2),(3,2,3),(0.,0.290272727434781),(0.521815037222017,
0.538999630513411,0.539591276818006),.UNSPECIFIED.)
GEOMETRIC_REPRESENTATION_ITEM()
RATIONAL_B_SPLINE_SURFACE(((0.989362668575565,0.987015160230477,0.987570037304351,
0.987570037304351,0.987570037304351),(0.989362668575565,0.987015160230477,
0.987570037304351,0.987570037304351,0.987570037304351)))
REPRESENTATION_ITEM('')
SURFACE()
);
#2786=(
BOUNDED_SURFACE()
B_SPLINE_SURFACE(1,2,((#142019,#142020,#142021),(#142022,#142023,#142024)),
 .UNSPECIFIED.,.F.,.F.,.F.)
B_SPLINE_SURFACE_WITH_KNOTS((2,2),(3,3),(0.,0.28980704099156),(0.194132688793264,
0.211606804210309),.UNSPECIFIED.)
GEOMETRIC_REPRESENTATION_ITEM()
RATIONAL_B_SPLINE_SURFACE(((0.989843896581117,0.992516389311057,0.998189888755649),
(0.989843896581118,0.992516389311057,0.998189888755649)))
REPRESENTATION_ITEM('')
SURFACE()
);
#2787=(
BOUNDED_SURFACE()
B_SPLINE_SURFACE(1,2,((#142041,#142042,#142043,#142044,#142045),(#142046,
#142047,#142048,#142049,#142050)),.UNSPECIFIED.,.F.,.F.,.F.)
B_SPLINE_SURFACE_WITH_KNOTS((2,2),(3,2,3),(0.,0.290272734887809),(0.521815037221999,
0.538999630513411,0.539591284274294),.UNSPECIFIED.)
GEOMETRIC_REPRESENTATION_ITEM()
RATIONAL_B_SPLINE_SURFACE(((0.98936266857557,0.987015160230476,0.987570037304351,
0.987570037304351,0.987570037304351),(0.98936266857557,0.987015160230476,
0.987570037304351,0.987570037304351,0.987570037304351)))
REPRESENTATION_ITEM('')
SURFACE()
);
#2788=(
BOUNDED_SURFACE()
B_SPLINE_SURFACE(1,2,((#142052,#142053,#142054),(#142055,#142056,#142057)),
 .UNSPECIFIED.,.F.,.F.,.F.)
B_SPLINE_SURFACE_WITH_KNOTS((2,2),(3,3),(0.,0.289807040991945),(0.194132688793569,
0.211606804210309),.UNSPECIFIED.)
GEOMETRIC_REPRESENTATION_ITEM()
RATIONAL_B_SPLINE_SURFACE(((0.989843896581211,0.992516389311156,0.998189888755649),
(0.989843896581211,0.992516389311156,0.998189888755649)))
REPRESENTATION_ITEM('')
SURFACE()
);
#2789=(
BOUNDED_SURFACE()
B_SPLINE_SURFACE(1,2,((#142074,#142075,#142076,#142077,#142078),(#142079,
#142080,#142081,#142082,#142083)),.UNSPECIFIED.,.F.,.F.,.F.)
B_SPLINE_SURFACE_WITH_KNOTS((2,2),(3,2,3),(0.,0.290272734855651),(0.521815037222016,
0.53899963051341,0.539591284242329),.UNSPECIFIED.)
GEOMETRIC_REPRESENTATION_ITEM()
RATIONAL_B_SPLINE_SURFACE(((0.989362668575565,0.987015160230477,0.987570037304351,
0.987570037304351,0.987570037304351),(0.989362668575565,0.987015160230477,
0.987570037304351,0.987570037304351,0.987570037304351)))
REPRESENTATION_ITEM('')
SURFACE()
);
#2790=(
BOUNDED_SURFACE()
B_SPLINE_SURFACE(1,2,((#142085,#142086,#142087),(#142088,#142089,#142090)),
 .UNSPECIFIED.,.F.,.F.,.F.)
B_SPLINE_SURFACE_WITH_KNOTS((2,2),(3,3),(0.,0.289807040993353),(0.194132688793569,
0.211606804210308),.UNSPECIFIED.)
GEOMETRIC_REPRESENTATION_ITEM()
RATIONAL_B_SPLINE_SURFACE(((0.989843896581211,0.992516389311156,0.998189888755648),
(0.989843896581211,0.992516389311156,0.998189888755648)))
REPRESENTATION_ITEM('')
SURFACE()
);
#2791=(
BOUNDED_SURFACE()
B_SPLINE_SURFACE(1,2,((#142107,#142108,#142109,#142110,#142111),(#142112,
#142113,#142114,#142115,#142116)),.UNSPECIFIED.,.F.,.F.,.F.)
B_SPLINE_SURFACE_WITH_KNOTS((2,2),(3,2,3),(0.,0.290272734899145),(0.521815037222016,
0.53899963051341,0.539591284285509),.UNSPECIFIED.)
GEOMETRIC_REPRESENTATION_ITEM()
RATIONAL_B_SPLINE_SURFACE(((0.989362668575565,0.987015160230477,0.987570037304351,
0.987570037304351,0.987570037304351),(0.989362668575565,0.987015160230477,
0.987570037304351,0.987570037304351,0.987570037304351)))
REPRESENTATION_ITEM('')
SURFACE()
);
#2792=(
BOUNDED_SURFACE()
B_SPLINE_SURFACE(1,2,((#142118,#142119,#142120),(#142121,#142122,#142123)),
 .UNSPECIFIED.,.F.,.F.,.F.)
B_SPLINE_SURFACE_WITH_KNOTS((2,2),(3,3),(0.,0.289807040992025),(0.194132688793569,
0.211606804210308),.UNSPECIFIED.)
GEOMETRIC_REPRESENTATION_ITEM()
RATIONAL_B_SPLINE_SURFACE(((0.989843896581211,0.992516389311156,0.998189888755648),
(0.989843896581211,0.992516389311156,0.998189888755648)))
REPRESENTATION_ITEM('')
SURFACE()
);
#2793=(
BOUNDED_SURFACE()
B_SPLINE_SURFACE(1,2,((#142140,#142141,#142142,#142143,#142144),(#142145,
#142146,#142147,#142148,#142149)),.UNSPECIFIED.,.F.,.F.,.F.)
B_SPLINE_SURFACE_WITH_KNOTS((2,2),(3,2,3),(0.,0.290272734836377),(0.521815037222016,
0.53899963051341,0.539591284223044),.UNSPECIFIED.)
GEOMETRIC_REPRESENTATION_ITEM()
RATIONAL_B_SPLINE_SURFACE(((0.989362668575565,0.987015160230477,0.987570037304351,
0.987570037304351,0.987570037304351),(0.989362668575565,0.987015160230477,
0.987570037304351,0.987570037304351,0.987570037304351)))
REPRESENTATION_ITEM('')
SURFACE()
);
#2794=(
BOUNDED_SURFACE()
B_SPLINE_SURFACE(1,2,((#142151,#142152,#142153),(#142154,#142155,#142156)),
 .UNSPECIFIED.,.F.,.F.,.F.)
B_SPLINE_SURFACE_WITH_KNOTS((2,2),(3,3),(0.,0.289807040991644),(0.194132688793569,
0.211606804210308),.UNSPECIFIED.)
GEOMETRIC_REPRESENTATION_ITEM()
RATIONAL_B_SPLINE_SURFACE(((0.989843896581211,0.992516389311156,0.998189888755648),
(0.989843896581211,0.992516389311156,0.998189888755648)))
REPRESENTATION_ITEM('')
SURFACE()
);
#2795=(
BOUNDED_SURFACE()
B_SPLINE_SURFACE(1,2,((#142173,#142174,#142175,#142176,#142177),(#142178,
#142179,#142180,#142181,#142182)),.UNSPECIFIED.,.F.,.F.,.F.)
B_SPLINE_SURFACE_WITH_KNOTS((2,2),(3,2,3),(0.,0.290272734853426),(0.521815037222016,
0.53899963051341,0.539591284240079),.UNSPECIFIED.)
GEOMETRIC_REPRESENTATION_ITEM()
RATIONAL_B_SPLINE_SURFACE(((0.989362668575565,0.987015160230477,0.987570037304351,
0.987570037304351,0.987570037304351),(0.989362668575565,0.987015160230477,
0.987570037304351,0.987570037304351,0.987570037304351)))
REPRESENTATION_ITEM('')
SURFACE()
);
#2796=(
BOUNDED_SURFACE()
B_SPLINE_SURFACE(1,2,((#142184,#142185,#142186),(#142187,#142188,#142189)),
 .UNSPECIFIED.,.F.,.F.,.F.)
B_SPLINE_SURFACE_WITH_KNOTS((2,2),(3,3),(0.,0.28980704099164),(0.194132688793569,
0.211606804210308),.UNSPECIFIED.)
GEOMETRIC_REPRESENTATION_ITEM()
RATIONAL_B_SPLINE_SURFACE(((0.989843896581211,0.992516389311156,0.998189888755648),
(0.989843896581211,0.992516389311156,0.998189888755648)))
REPRESENTATION_ITEM('')
SURFACE()
);
#2797=(
BOUNDED_SURFACE()
B_SPLINE_SURFACE(1,2,((#142206,#142207,#142208,#142209,#142210),(#142211,
#142212,#142213,#142214,#142215)),.UNSPECIFIED.,.F.,.F.,.F.)
B_SPLINE_SURFACE_WITH_KNOTS((2,2),(3,2,3),(0.,0.290272734846835),(0.521815037222016,
0.53899963051341,0.539591284233596),.UNSPECIFIED.)
GEOMETRIC_REPRESENTATION_ITEM()
RATIONAL_B_SPLINE_SURFACE(((0.989362668575565,0.987015160230477,0.987570037304351,
0.987570037304351,0.987570037304351),(0.989362668575565,0.987015160230477,
0.987570037304351,0.987570037304351,0.987570037304351)))
REPRESENTATION_ITEM('')
SURFACE()
);
#2798=(
BOUNDED_SURFACE()
B_SPLINE_SURFACE(1,2,((#142217,#142218,#142219),(#142220,#142221,#142222)),
 .UNSPECIFIED.,.F.,.F.,.F.)
B_SPLINE_SURFACE_WITH_KNOTS((2,2),(3,3),(0.,0.289807040991632),(0.194132688793569,
0.211606804210308),.UNSPECIFIED.)
GEOMETRIC_REPRESENTATION_ITEM()
RATIONAL_B_SPLINE_SURFACE(((0.989843896581211,0.992516389311156,0.998189888755648),
(0.989843896581211,0.992516389311156,0.998189888755648)))
REPRESENTATION_ITEM('')
SURFACE()
);
#2799=(
BOUNDED_SURFACE()
B_SPLINE_SURFACE(1,2,((#142239,#142240,#142241,#142242,#142243),(#142244,
#142245,#142246,#142247,#142248)),.UNSPECIFIED.,.F.,.F.,.F.)
B_SPLINE_SURFACE_WITH_KNOTS((2,2),(3,2,3),(0.,0.290272734853011),(0.521815037222016,
0.53899963051341,0.539591284239539),.UNSPECIFIED.)
GEOMETRIC_REPRESENTATION_ITEM()
RATIONAL_B_SPLINE_SURFACE(((0.989362668575565,0.987015160230477,0.987570037304351,
0.987570037304351,0.987570037304351),(0.989362668575565,0.987015160230477,
0.987570037304351,0.987570037304351,0.987570037304351)))
REPRESENTATION_ITEM('')
SURFACE()
);
#2800=(
BOUNDED_SURFACE()
B_SPLINE_SURFACE(1,2,((#142250,#142251,#142252),(#142253,#142254,#142255)),
 .UNSPECIFIED.,.F.,.F.,.F.)
B_SPLINE_SURFACE_WITH_KNOTS((2,2),(3,3),(0.,0.289807040991908),(0.194132688793569,
0.211606804210308),.UNSPECIFIED.)
GEOMETRIC_REPRESENTATION_ITEM()
RATIONAL_B_SPLINE_SURFACE(((0.989843896581211,0.992516389311156,0.998189888755648),
(0.989843896581211,0.992516389311156,0.998189888755648)))
REPRESENTATION_ITEM('')
SURFACE()
);
#2801=(
BOUNDED_SURFACE()
B_SPLINE_SURFACE(1,2,((#142272,#142273,#142274,#142275,#142276),(#142277,
#142278,#142279,#142280,#142281)),.UNSPECIFIED.,.F.,.F.,.F.)
B_SPLINE_SURFACE_WITH_KNOTS((2,2),(3,2,3),(0.,0.290272734854809),(0.521815037222016,
0.53899963051341,0.539591284241502),.UNSPECIFIED.)
GEOMETRIC_REPRESENTATION_ITEM()
RATIONAL_B_SPLINE_SURFACE(((0.989362668575565,0.987015160230477,0.987570037304351,
0.987570037304351,0.987570037304351),(0.989362668575565,0.987015160230477,
0.987570037304351,0.987570037304351,0.987570037304351)))
REPRESENTATION_ITEM('')
SURFACE()
);
#2802=(
BOUNDED_SURFACE()
B_SPLINE_SURFACE(1,2,((#142283,#142284,#142285),(#142286,#142287,#142288)),
 .UNSPECIFIED.,.F.,.F.,.F.)
B_SPLINE_SURFACE_WITH_KNOTS((2,2),(3,3),(0.,0.289807040991557),(0.194132688793569,
0.211606804210308),.UNSPECIFIED.)
GEOMETRIC_REPRESENTATION_ITEM()
RATIONAL_B_SPLINE_SURFACE(((0.989843896581211,0.992516389311156,0.998189888755648),
(0.989843896581211,0.992516389311156,0.998189888755648)))
REPRESENTATION_ITEM('')
SURFACE()
);
#2803=(
BOUNDED_SURFACE()
B_SPLINE_SURFACE(1,2,((#142305,#142306,#142307,#142308,#142309),(#142310,
#142311,#142312,#142313,#142314)),.UNSPECIFIED.,.F.,.F.,.F.)
B_SPLINE_SURFACE_WITH_KNOTS((2,2),(3,2,3),(0.,0.290272734849359),(0.521815037222016,
0.53899963051341,0.53959128423595),.UNSPECIFIED.)
GEOMETRIC_REPRESENTATION_ITEM()
RATIONAL_B_SPLINE_SURFACE(((0.989362668575565,0.987015160230477,0.987570037304351,
0.987570037304351,0.987570037304351),(0.989362668575565,0.987015160230477,
0.987570037304351,0.987570037304351,0.987570037304351)))
REPRESENTATION_ITEM('')
SURFACE()
);
#2804=(
BOUNDED_SURFACE()
B_SPLINE_SURFACE(1,2,((#142316,#142317,#142318,#142319,#142320),(#142321,
#142322,#142323,#142324,#142325)),.UNSPECIFIED.,.F.,.F.,.F.)
B_SPLINE_SURFACE_WITH_KNOTS((2,2),(3,2,3),(0.710318915639631,1.),(0.573550810617452,
0.590910950629594,0.591084552029715),.UNSPECIFIED.)
GEOMETRIC_REPRESENTATION_ITEM()
RATIONAL_B_SPLINE_SURFACE(((0.998554414400195,0.992822941359326,0.990053454406147,
0.990053454406147,0.990053454406147),(0.998554414400195,0.992822941359326,
0.990053454406147,0.990053454406147,0.990053454406147)))
REPRESENTATION_ITEM('')
SURFACE()
);
#2805=(
BOUNDED_SURFACE()
B_SPLINE_SURFACE(1,2,((#142336,#142337,#142338,#142339,#142340,#142341,
#142342),(#142343,#142344,#142345,#142346,#142347,#142348,#142349)),
 .UNSPECIFIED.,.F.,.F.,.F.)
B_SPLINE_SURFACE_WITH_KNOTS((2,2),(3,2,2,3),(0.710192959007995,1.),(0.142404283483303,
0.142578551421364,0.142857142857143,0.160005345227479),.UNSPECIFIED.)
GEOMETRIC_REPRESENTATION_ITEM()
RATIONAL_B_SPLINE_SURFACE(((0.999805186472059,0.999805186472059,0.999805186472059,
0.999902211834795,1.,0.993980822699459,0.990851751371591),(0.999805186472059,
0.999805186472059,0.999805186472059,0.999902211834795,1.,0.993980822699459,
0.990851751371591)))
REPRESENTATION_ITEM('')
SURFACE()
);
#2806=(
BOUNDED_SURFACE()
B_SPLINE_SURFACE(1,2,((#142357,#142358,#142359,#142360,#142361),(#142362,
#142363,#142364,#142365,#142366)),.UNSPECIFIED.,.F.,.F.,.F.)
B_SPLINE_SURFACE_WITH_KNOTS((2,2),(3,2,3),(0.71031891563998,1.),(0.573550810617373,
0.590910950629594,0.591084552029716),.UNSPECIFIED.)
GEOMETRIC_REPRESENTATION_ITEM()
RATIONAL_B_SPLINE_SURFACE(((0.998554414400247,0.992822941359339,0.990053454406147,
0.990053454406147,0.990053454406147),(0.998554414400247,0.992822941359339,
0.990053454406147,0.990053454406147,0.990053454406147)))
REPRESENTATION_ITEM('')
SURFACE()
);
#2807=(
BOUNDED_SURFACE()
B_SPLINE_SURFACE(1,2,((#142377,#142378,#142379,#142380,#142381,#142382,
#142383),(#142384,#142385,#142386,#142387,#142388,#142389,#142390)),
 .UNSPECIFIED.,.F.,.F.,.F.)
B_SPLINE_SURFACE_WITH_KNOTS((2,2),(3,2,2,3),(0.710192959008341,1.),(0.142404283483303,
0.142578551421364,0.142857142857143,0.160005345227478),.UNSPECIFIED.)
GEOMETRIC_REPRESENTATION_ITEM()
RATIONAL_B_SPLINE_SURFACE(((0.999805186472059,0.999805186472059,0.999805186472059,
0.999902211834795,1.,0.993980822699459,0.990851751371591),(0.999805186472059,
0.999805186472059,0.999805186472059,0.999902211834795,1.,0.993980822699459,
0.990851751371591)))
REPRESENTATION_ITEM('')
SURFACE()
);
#2808=(
BOUNDED_SURFACE()
B_SPLINE_SURFACE(1,2,((#142398,#142399,#142400,#142401,#142402),(#142403,
#142404,#142405,#142406,#142407)),.UNSPECIFIED.,.F.,.F.,.F.)
B_SPLINE_SURFACE_WITH_KNOTS((2,2),(3,2,3),(0.710318915639972,1.),(0.573550810617452,
0.590910950629594,0.591084552029715),.UNSPECIFIED.)
GEOMETRIC_REPRESENTATION_ITEM()
RATIONAL_B_SPLINE_SURFACE(((0.998554414400195,0.992822941359326,0.990053454406148,
0.990053454406148,0.990053454406148),(0.998554414400195,0.992822941359326,
0.990053454406148,0.990053454406148,0.990053454406148)))
REPRESENTATION_ITEM('')
SURFACE()
);
#2809=(
BOUNDED_SURFACE()
B_SPLINE_SURFACE(1,2,((#142418,#142419,#142420,#142421,#142422,#142423,
#142424),(#142425,#142426,#142427,#142428,#142429,#142430,#142431)),
 .UNSPECIFIED.,.F.,.F.,.F.)
B_SPLINE_SURFACE_WITH_KNOTS((2,2),(3,2,2,3),(0.710192959008339,1.),(0.142404283483303,
0.142578551421364,0.142857142857143,0.160005345227479),.UNSPECIFIED.)
GEOMETRIC_REPRESENTATION_ITEM()
RATIONAL_B_SPLINE_SURFACE(((0.999805186472059,0.999805186472059,0.999805186472059,
0.999902211834795,1.,0.993980822699459,0.990851751371591),(0.999805186472059,
0.999805186472059,0.999805186472059,0.999902211834795,1.,0.993980822699459,
0.990851751371591)))
REPRESENTATION_ITEM('')
SURFACE()
);
#2810=(
BOUNDED_SURFACE()
B_SPLINE_SURFACE(1,2,((#142439,#142440,#142441,#142442,#142443),(#142444,
#142445,#142446,#142447,#142448)),.UNSPECIFIED.,.F.,.F.,.F.)
B_SPLINE_SURFACE_WITH_KNOTS((2,2),(3,2,3),(0.710318915639019,1.),(0.573550810617371,
0.590910950629594,0.591084552029716),.UNSPECIFIED.)
GEOMETRIC_REPRESENTATION_ITEM()
RATIONAL_B_SPLINE_SURFACE(((0.998554414400249,0.992822941359339,0.990053454406148,
0.990053454406148,0.990053454406148),(0.998554414400249,0.992822941359339,
0.990053454406148,0.990053454406148,0.990053454406148)))
REPRESENTATION_ITEM('')
SURFACE()
);
#2811=(
BOUNDED_SURFACE()
B_SPLINE_SURFACE(1,2,((#142459,#142460,#142461,#142462,#142463,#142464,
#142465),(#142466,#142467,#142468,#142469,#142470,#142471,#142472)),
 .UNSPECIFIED.,.F.,.F.,.F.)
B_SPLINE_SURFACE_WITH_KNOTS((2,2),(3,2,2,3),(0.710192959007381,1.),(0.142404283483303,
0.142578551421364,0.142857142857143,0.160005345227478),.UNSPECIFIED.)
GEOMETRIC_REPRESENTATION_ITEM()
RATIONAL_B_SPLINE_SURFACE(((0.999805186472059,0.999805186472059,0.999805186472059,
0.999902211834795,1.,0.993980822699459,0.990851751371591),(0.999805186472059,
0.999805186472059,0.999805186472059,0.999902211834795,1.,0.993980822699459,
0.990851751371591)))
REPRESENTATION_ITEM('')
SURFACE()
);
#2812=(
BOUNDED_SURFACE()
B_SPLINE_SURFACE(1,2,((#142480,#142481,#142482,#142483,#142484),(#142485,
#142486,#142487,#142488,#142489)),.UNSPECIFIED.,.F.,.F.,.F.)
B_SPLINE_SURFACE_WITH_KNOTS((2,2),(3,2,3),(0.710318915639016,1.),(0.57355081061737,
0.590910950629594,0.591084552029716),.UNSPECIFIED.)
GEOMETRIC_REPRESENTATION_ITEM()
RATIONAL_B_SPLINE_SURFACE(((0.998554414400249,0.992822941359339,0.990053454406148,
0.990053454406148,0.990053454406148),(0.998554414400249,0.992822941359339,
0.990053454406148,0.990053454406148,0.990053454406148)))
REPRESENTATION_ITEM('')
SURFACE()
);
#2813=(
BOUNDED_SURFACE()
B_SPLINE_SURFACE(1,2,((#142500,#142501,#142502,#142503,#142504,#142505,
#142506),(#142507,#142508,#142509,#142510,#142511,#142512,#142513)),
 .UNSPECIFIED.,.F.,.F.,.F.)
B_SPLINE_SURFACE_WITH_KNOTS((2,2),(3,2,2,3),(0.710192959007377,1.),(0.142404283483303,
0.142578551421364,0.142857142857143,0.160005345227478),.UNSPECIFIED.)
GEOMETRIC_REPRESENTATION_ITEM()
RATIONAL_B_SPLINE_SURFACE(((0.999805186472059,0.999805186472059,0.999805186472059,
0.999902211834795,1.,0.993980822699459,0.990851751371591),(0.999805186472059,
0.999805186472059,0.999805186472059,0.999902211834795,1.,0.993980822699459,
0.990851751371591)))
REPRESENTATION_ITEM('')
SURFACE()
);
#2814=(
BOUNDED_SURFACE()
B_SPLINE_SURFACE(1,2,((#142521,#142522,#142523,#142524,#142525),(#142526,
#142527,#142528,#142529,#142530)),.UNSPECIFIED.,.F.,.F.,.F.)
B_SPLINE_SURFACE_WITH_KNOTS((2,2),(3,2,3),(0.71031891563902,1.),(0.573550810617172,
0.590910950629594,0.591084552029718),.UNSPECIFIED.)
GEOMETRIC_REPRESENTATION_ITEM()
RATIONAL_B_SPLINE_SURFACE(((0.99855441440038,0.992822941359371,0.990053454406147,
0.990053454406147,0.990053454406147),(0.99855441440038,0.992822941359371,
0.990053454406147,0.990053454406147,0.990053454406147)))
REPRESENTATION_ITEM('')
SURFACE()
);
#2815=(
BOUNDED_SURFACE()
B_SPLINE_SURFACE(1,2,((#142541,#142542,#142543,#142544,#142545,#142546,
#142547),(#142548,#142549,#142550,#142551,#142552,#142553,#142554)),
 .UNSPECIFIED.,.F.,.F.,.F.)
B_SPLINE_SURFACE_WITH_KNOTS((2,2),(3,2,2,3),(0.71019295900738,1.),(0.142404283483303,
0.142578551421364,0.142857142857143,0.160005345227479),.UNSPECIFIED.)
GEOMETRIC_REPRESENTATION_ITEM()
RATIONAL_B_SPLINE_SURFACE(((0.999805186472059,0.999805186472059,0.999805186472059,
0.999902211834795,1.,0.993980822699459,0.990851751371591),(0.999805186472059,
0.999805186472059,0.999805186472059,0.999902211834795,1.,0.993980822699459,
0.990851751371591)))
REPRESENTATION_ITEM('')
SURFACE()
);
#2816=(
BOUNDED_SURFACE()
B_SPLINE_SURFACE(1,2,((#142562,#142563,#142564,#142565,#142566),(#142567,
#142568,#142569,#142570,#142571)),.UNSPECIFIED.,.F.,.F.,.F.)
B_SPLINE_SURFACE_WITH_KNOTS((2,2),(3,2,3),(0.710318915638433,1.),(0.573550810617371,
0.590910950629594,0.591084552029716),.UNSPECIFIED.)
GEOMETRIC_REPRESENTATION_ITEM()
RATIONAL_B_SPLINE_SURFACE(((0.998554414400249,0.992822941359339,0.990053454406148,
0.990053454406148,0.990053454406148),(0.998554414400249,0.992822941359339,
0.990053454406148,0.990053454406148,0.990053454406148)))
REPRESENTATION_ITEM('')
SURFACE()
);
#2817=(
BOUNDED_SURFACE()
B_SPLINE_SURFACE(1,2,((#142582,#142583,#142584,#142585,#142586,#142587,
#142588),(#142589,#142590,#142591,#142592,#142593,#142594,#142595)),
 .UNSPECIFIED.,.F.,.F.,.F.)
B_SPLINE_SURFACE_WITH_KNOTS((2,2),(3,2,2,3),(0.710192959006795,1.),(0.142404283483303,
0.142578551421364,0.142857142857143,0.160005345227478),.UNSPECIFIED.)
GEOMETRIC_REPRESENTATION_ITEM()
RATIONAL_B_SPLINE_SURFACE(((0.999805186472059,0.999805186472059,0.999805186472059,
0.999902211834795,1.,0.993980822699459,0.990851751371591),(0.999805186472059,
0.999805186472059,0.999805186472059,0.999902211834795,1.,0.993980822699459,
0.990851751371591)))
REPRESENTATION_ITEM('')
SURFACE()
);
#2818=(
BOUNDED_SURFACE()
B_SPLINE_SURFACE(1,2,((#142603,#142604,#142605,#142606,#142607),(#142608,
#142609,#142610,#142611,#142612)),.UNSPECIFIED.,.F.,.F.,.F.)
B_SPLINE_SURFACE_WITH_KNOTS((2,2),(3,2,3),(0.710318915639023,1.),(0.573550810617172,
0.590910950629594,0.591084552029718),.UNSPECIFIED.)
GEOMETRIC_REPRESENTATION_ITEM()
RATIONAL_B_SPLINE_SURFACE(((0.99855441440038,0.992822941359371,0.990053454406148,
0.990053454406148,0.990053454406148),(0.99855441440038,0.992822941359371,
0.990053454406148,0.990053454406148,0.990053454406148)))
REPRESENTATION_ITEM('')
SURFACE()
);
#2819=(
BOUNDED_SURFACE()
B_SPLINE_SURFACE(1,2,((#142623,#142624,#142625,#142626,#142627,#142628,
#142629),(#142630,#142631,#142632,#142633,#142634,#142635,#142636)),
 .UNSPECIFIED.,.F.,.F.,.F.)
B_SPLINE_SURFACE_WITH_KNOTS((2,2),(3,2,2,3),(0.710192959007378,1.),(0.142404283483303,
0.142578551421364,0.142857142857143,0.160005345227479),.UNSPECIFIED.)
GEOMETRIC_REPRESENTATION_ITEM()
RATIONAL_B_SPLINE_SURFACE(((0.999805186472059,0.999805186472059,0.999805186472059,
0.999902211834795,1.,0.993980822699459,0.990851751371591),(0.999805186472059,
0.999805186472059,0.999805186472059,0.999902211834795,1.,0.993980822699459,
0.990851751371591)))
REPRESENTATION_ITEM('')
SURFACE()
);
#2820=(
BOUNDED_SURFACE()
B_SPLINE_SURFACE(1,2,((#142644,#142645,#142646,#142647,#142648),(#142649,
#142650,#142651,#142652,#142653)),.UNSPECIFIED.,.F.,.F.,.F.)
B_SPLINE_SURFACE_WITH_KNOTS((2,2),(3,2,3),(0.710318915638463,1.),(0.573550810617452,
0.590910950629594,0.591084552029715),.UNSPECIFIED.)
GEOMETRIC_REPRESENTATION_ITEM()
RATIONAL_B_SPLINE_SURFACE(((0.998554414400195,0.992822941359326,0.990053454406147,
0.990053454406147,0.990053454406147),(0.998554414400195,0.992822941359326,
0.990053454406147,0.990053454406147,0.990053454406147)))
REPRESENTATION_ITEM('')
SURFACE()
);
#2821=(
BOUNDED_SURFACE()
B_SPLINE_SURFACE(1,2,((#142664,#142665,#142666,#142667,#142668,#142669,
#142670),(#142671,#142672,#142673,#142674,#142675,#142676,#142677)),
 .UNSPECIFIED.,.F.,.F.,.F.)
B_SPLINE_SURFACE_WITH_KNOTS((2,2),(3,2,2,3),(0.71019295900683,1.),(0.142404283483303,
0.142578551421364,0.142857142857143,0.160005345227479),.UNSPECIFIED.)
GEOMETRIC_REPRESENTATION_ITEM()
RATIONAL_B_SPLINE_SURFACE(((0.999805186472059,0.999805186472059,0.999805186472059,
0.999902211834795,1.,0.993980822699459,0.990851751371591),(0.999805186472059,
0.999805186472059,0.999805186472059,0.999902211834795,1.,0.993980822699459,
0.990851751371591)))
REPRESENTATION_ITEM('')
SURFACE()
);
#2822=(
BOUNDED_SURFACE()
B_SPLINE_SURFACE(1,2,((#142685,#142686,#142687,#142688,#142689),(#142690,
#142691,#142692,#142693,#142694)),.UNSPECIFIED.,.F.,.F.,.F.)
B_SPLINE_SURFACE_WITH_KNOTS((2,2),(3,2,3),(0.710318915638654,1.),(0.573550810617177,
0.590910950629594,0.591084552029718),.UNSPECIFIED.)
GEOMETRIC_REPRESENTATION_ITEM()
RATIONAL_B_SPLINE_SURFACE(((0.998554414400376,0.99282294135937,0.990053454406147,
0.990053454406147,0.990053454406147),(0.998554414400376,0.99282294135937,
0.990053454406147,0.990053454406147,0.990053454406147)))
REPRESENTATION_ITEM('')
SURFACE()
);
#2823=(
BOUNDED_SURFACE()
B_SPLINE_SURFACE(1,2,((#142705,#142706,#142707,#142708,#142709,#142710,
#142711),(#142712,#142713,#142714,#142715,#142716,#142717,#142718)),
 .UNSPECIFIED.,.F.,.F.,.F.)
B_SPLINE_SURFACE_WITH_KNOTS((2,2),(3,2,2,3),(0.710192959007013,1.),(0.142404283483303,
0.142578551421363,0.142857142857143,0.160005345227404),.UNSPECIFIED.)
GEOMETRIC_REPRESENTATION_ITEM()
RATIONAL_B_SPLINE_SURFACE(((0.999805186472058,0.999805186472058,0.999805186472058,
0.999902211834794,1.,0.993980822699486,0.990851751371619),(0.999805186472058,
0.999805186472058,0.999805186472058,0.999902211834794,1.,0.993980822699486,
0.990851751371619)))
REPRESENTATION_ITEM('')
SURFACE()
);
#2824=(
BOUNDED_SURFACE()
B_SPLINE_SURFACE(1,2,((#142726,#142727,#142728,#142729,#142730),(#142731,
#142732,#142733,#142734,#142735)),.UNSPECIFIED.,.F.,.F.,.F.)
B_SPLINE_SURFACE_WITH_KNOTS((2,2),(3,2,3),(0.710318915638625,1.),(0.573550810617173,
0.590910950629595,0.591084552029719),.UNSPECIFIED.)
GEOMETRIC_REPRESENTATION_ITEM()
RATIONAL_B_SPLINE_SURFACE(((0.998554414400379,0.99282294135937,0.990053454406147,
0.990053454406147,0.990053454406147),(0.998554414400379,0.99282294135937,
0.990053454406147,0.990053454406147,0.990053454406147)))
REPRESENTATION_ITEM('')
SURFACE()
);
#2825=(
BOUNDED_SURFACE()
B_SPLINE_SURFACE(1,2,((#142746,#142747,#142748,#142749,#142750,#142751,
#142752),(#142753,#142754,#142755,#142756,#142757,#142758,#142759)),
 .UNSPECIFIED.,.F.,.F.,.F.)
B_SPLINE_SURFACE_WITH_KNOTS((2,2),(3,2,2,3),(0.710192959006981,1.),(0.142404283483302,
0.142578551421363,0.142857142857143,0.160005345227478),.UNSPECIFIED.)
GEOMETRIC_REPRESENTATION_ITEM()
RATIONAL_B_SPLINE_SURFACE(((0.999805186472059,0.999805186472059,0.999805186472059,
0.999902211834794,1.,0.993980822699459,0.990851751371592),(0.999805186472059,
0.999805186472059,0.999805186472059,0.999902211834794,1.,0.993980822699459,
0.990851751371592)))
REPRESENTATION_ITEM('')
SURFACE()
);
#2826=(
BOUNDED_SURFACE()
B_SPLINE_SURFACE(1,2,((#142767,#142768,#142769,#142770,#142771),(#142772,
#142773,#142774,#142775,#142776)),.UNSPECIFIED.,.F.,.F.,.F.)
B_SPLINE_SURFACE_WITH_KNOTS((2,2),(3,2,3),(0.710318915638347,1.),(0.573550810617173,
0.590910950629595,0.591084552029719),.UNSPECIFIED.)
GEOMETRIC_REPRESENTATION_ITEM()
RATIONAL_B_SPLINE_SURFACE(((0.998554414400379,0.99282294135937,0.990053454406147,
0.990053454406147,0.990053454406147),(0.998554414400379,0.99282294135937,
0.990053454406147,0.990053454406147,0.990053454406147)))
REPRESENTATION_ITEM('')
SURFACE()
);
#2827=(
BOUNDED_SURFACE()
B_SPLINE_SURFACE(1,2,((#142787,#142788,#142789,#142790,#142791,#142792,
#142793),(#142794,#142795,#142796,#142797,#142798,#142799,#142800)),
 .UNSPECIFIED.,.F.,.F.,.F.)
B_SPLINE_SURFACE_WITH_KNOTS((2,2),(3,2,2,3),(0.7101929590067,1.),(0.142404283483302,
0.142578551421363,0.142857142857143,0.160005345227478),.UNSPECIFIED.)
GEOMETRIC_REPRESENTATION_ITEM()
RATIONAL_B_SPLINE_SURFACE(((0.999805186472058,0.999805186472058,0.999805186472058,
0.999902211834794,1.,0.993980822699459,0.990851751371591),(0.999805186472058,
0.999805186472058,0.999805186472058,0.999902211834794,1.,0.993980822699459,
0.990851751371591)))
REPRESENTATION_ITEM('')
SURFACE()
);
#2828=(
BOUNDED_SURFACE()
B_SPLINE_SURFACE(1,2,((#142808,#142809,#142810,#142811,#142812),(#142813,
#142814,#142815,#142816,#142817)),.UNSPECIFIED.,.F.,.F.,.F.)
B_SPLINE_SURFACE_WITH_KNOTS((2,2),(3,2,3),(0.710318915638931,1.),(0.573550810617173,
0.590910950629595,0.591084552029719),.UNSPECIFIED.)
GEOMETRIC_REPRESENTATION_ITEM()
RATIONAL_B_SPLINE_SURFACE(((0.998554414400379,0.99282294135937,0.990053454406147,
0.990053454406147,0.990053454406147),(0.998554414400379,0.99282294135937,
0.990053454406147,0.990053454406147,0.990053454406147)))
REPRESENTATION_ITEM('')
SURFACE()
);
#2829=(
BOUNDED_SURFACE()
B_SPLINE_SURFACE(1,2,((#142828,#142829,#142830,#142831,#142832,#142833,
#142834),(#142835,#142836,#142837,#142838,#142839,#142840,#142841)),
 .UNSPECIFIED.,.F.,.F.,.F.)
B_SPLINE_SURFACE_WITH_KNOTS((2,2),(3,2,2,3),(0.710192959007288,1.),(0.142404283483303,
0.142578551421363,0.142857142857143,0.160005345227401),.UNSPECIFIED.)
GEOMETRIC_REPRESENTATION_ITEM()
RATIONAL_B_SPLINE_SURFACE(((0.999805186472058,0.999805186472058,0.999805186472058,
0.999902211834794,1.,0.993980822699486,0.990851751371619),(0.999805186472058,
0.999805186472058,0.999805186472058,0.999902211834794,1.,0.993980822699486,
0.990851751371619)))
REPRESENTATION_ITEM('')
SURFACE()
);
#2830=(
BOUNDED_SURFACE()
B_SPLINE_SURFACE(1,2,((#142849,#142850,#142851,#142852,#142853),(#142854,
#142855,#142856,#142857,#142858)),.UNSPECIFIED.,.F.,.F.,.F.)
B_SPLINE_SURFACE_WITH_KNOTS((2,2),(3,2,3),(0.710318915638101,1.),(0.573550810617453,
0.590910950629595,0.591084552029716),.UNSPECIFIED.)
GEOMETRIC_REPRESENTATION_ITEM()
RATIONAL_B_SPLINE_SURFACE(((0.998554414400194,0.992822941359325,0.990053454406147,
0.990053454406147,0.990053454406147),(0.998554414400194,0.992822941359325,
0.990053454406147,0.990053454406147,0.990053454406147)))
REPRESENTATION_ITEM('')
SURFACE()
);
#2831=(
BOUNDED_SURFACE()
B_SPLINE_SURFACE(1,2,((#142869,#142870,#142871,#142872,#142873,#142874,
#142875),(#142876,#142877,#142878,#142879,#142880,#142881,#142882)),
 .UNSPECIFIED.,.F.,.F.,.F.)
B_SPLINE_SURFACE_WITH_KNOTS((2,2),(3,2,2,3),(0.710192959006456,1.),(0.142404283483302,
0.142578551421363,0.142857142857143,0.160005345227478),.UNSPECIFIED.)
GEOMETRIC_REPRESENTATION_ITEM()
RATIONAL_B_SPLINE_SURFACE(((0.999805186472058,0.999805186472058,0.999805186472058,
0.999902211834794,1.,0.993980822699459,0.990851751371591),(0.999805186472058,
0.999805186472058,0.999805186472058,0.999902211834794,1.,0.993980822699459,
0.990851751371591)))
REPRESENTATION_ITEM('')
SURFACE()
);
#2832=(
BOUNDED_SURFACE()
B_SPLINE_SURFACE(1,2,((#142890,#142891,#142892,#142893,#142894),(#142895,
#142896,#142897,#142898,#142899)),.UNSPECIFIED.,.F.,.F.,.F.)
B_SPLINE_SURFACE_WITH_KNOTS((2,2),(3,2,3),(0.710318915638601,1.),(0.573550810617173,
0.590910950629595,0.591084552029719),.UNSPECIFIED.)
GEOMETRIC_REPRESENTATION_ITEM()
RATIONAL_B_SPLINE_SURFACE(((0.998554414400379,0.99282294135937,0.990053454406147,
0.990053454406147,0.990053454406147),(0.998554414400379,0.99282294135937,
0.990053454406147,0.990053454406147,0.990053454406147)))
REPRESENTATION_ITEM('')
SURFACE()
);
#2833=(
BOUNDED_SURFACE()
B_SPLINE_SURFACE(1,2,((#142910,#142911,#142912,#142913,#142914,#142915,
#142916),(#142917,#142918,#142919,#142920,#142921,#142922,#142923)),
 .UNSPECIFIED.,.F.,.F.,.F.)
B_SPLINE_SURFACE_WITH_KNOTS((2,2),(3,2,2,3),(0.710192959006956,1.),(0.142404283483303,
0.142578551421363,0.142857142857143,0.160005345227402),.UNSPECIFIED.)
GEOMETRIC_REPRESENTATION_ITEM()
RATIONAL_B_SPLINE_SURFACE(((0.999805186472059,0.999805186472059,0.999805186472059,
0.999902211834794,1.,0.993980822699486,0.990851751371619),(0.999805186472059,
0.999805186472059,0.999805186472059,0.999902211834794,1.,0.993980822699486,
0.990851751371619)))
REPRESENTATION_ITEM('')
SURFACE()
);
#2834=(
BOUNDED_SURFACE()
B_SPLINE_SURFACE(1,2,((#142931,#142932,#142933,#142934,#142935),(#142936,
#142937,#142938,#142939,#142940)),.UNSPECIFIED.,.F.,.F.,.F.)
B_SPLINE_SURFACE_WITH_KNOTS((2,2),(3,2,3),(0.710318915638125,1.),(0.573550810617373,
0.590910950629595,0.591084552029717),.UNSPECIFIED.)
GEOMETRIC_REPRESENTATION_ITEM()
RATIONAL_B_SPLINE_SURFACE(((0.998554414400247,0.992822941359338,0.990053454406147,
0.990053454406147,0.990053454406147),(0.998554414400247,0.992822941359338,
0.990053454406147,0.990053454406147,0.990053454406147)))
REPRESENTATION_ITEM('')
SURFACE()
);
#2835=(
BOUNDED_SURFACE()
B_SPLINE_SURFACE(1,2,((#142951,#142952,#142953,#142954,#142955,#142956,
#142957),(#142958,#142959,#142960,#142961,#142962,#142963,#142964)),
 .UNSPECIFIED.,.F.,.F.,.F.)
B_SPLINE_SURFACE_WITH_KNOTS((2,2),(3,2,2,3),(0.710192959006485,1.),(0.142404283483302,
0.142578551421363,0.142857142857143,0.160005345227477),.UNSPECIFIED.)
GEOMETRIC_REPRESENTATION_ITEM()
RATIONAL_B_SPLINE_SURFACE(((0.999805186472059,0.999805186472059,0.999805186472059,
0.999902211834794,1.,0.99398082269946,0.990851751371592),(0.999805186472059,
0.999805186472059,0.999805186472059,0.999902211834794,1.,0.99398082269946,
0.990851751371592)))
REPRESENTATION_ITEM('')
SURFACE()
);
#2836=(
BOUNDED_SURFACE()
B_SPLINE_SURFACE(1,2,((#142972,#142973,#142974,#142975,#142976),(#142977,
#142978,#142979,#142980,#142981)),.UNSPECIFIED.,.F.,.F.,.F.)
B_SPLINE_SURFACE_WITH_KNOTS((2,2),(3,2,3),(0.710318915638373,1.),(0.573550810617177,
0.590910950629595,0.591084552029719),.UNSPECIFIED.)
GEOMETRIC_REPRESENTATION_ITEM()
RATIONAL_B_SPLINE_SURFACE(((0.998554414400376,0.992822941359369,0.990053454406147,
0.990053454406147,0.990053454406147),(0.998554414400376,0.992822941359369,
0.990053454406147,0.990053454406147,0.990053454406147)))
REPRESENTATION_ITEM('')
SURFACE()
);
#2837=(
BOUNDED_SURFACE()
B_SPLINE_SURFACE(1,2,((#142992,#142993,#142994,#142995,#142996,#142997,
#142998),(#142999,#143000,#143001,#143002,#143003,#143004,#143005)),
 .UNSPECIFIED.,.F.,.F.,.F.)
B_SPLINE_SURFACE_WITH_KNOTS((2,2),(3,2,2,3),(0.710192959006736,1.),(0.142404283483303,
0.142578551421363,0.142857142857143,0.160005345227404),.UNSPECIFIED.)
GEOMETRIC_REPRESENTATION_ITEM()
RATIONAL_B_SPLINE_SURFACE(((0.999805186472058,0.999805186472058,0.999805186472058,
0.999902211834794,1.,0.993980822699486,0.990851751371619),(0.999805186472058,
0.999805186472058,0.999805186472058,0.999902211834794,1.,0.993980822699486,
0.990851751371619)))
REPRESENTATION_ITEM('')
SURFACE()
);
#2838=(
BOUNDED_SURFACE()
B_SPLINE_SURFACE(1,2,((#143013,#143014,#143015,#143016,#143017),(#143018,
#143019,#143020,#143021,#143022)),.UNSPECIFIED.,.F.,.F.,.F.)
B_SPLINE_SURFACE_WITH_KNOTS((2,2),(3,2,3),(0.710318915637221,1.),(0.573550810617203,
0.590910950629595,0.591084552029719),.UNSPECIFIED.)
GEOMETRIC_REPRESENTATION_ITEM()
RATIONAL_B_SPLINE_SURFACE(((0.998554414400359,0.992822941359365,0.990053454406147,
0.990053454406147,0.990053454406147),(0.998554414400359,0.992822941359365,
0.990053454406147,0.990053454406147,0.990053454406147)))
REPRESENTATION_ITEM('')
SURFACE()
);
#2839=(
BOUNDED_SURFACE()
B_SPLINE_SURFACE(1,2,((#143033,#143034,#143035,#143036,#143037,#143038,
#143039),(#143040,#143041,#143042,#143043,#143044,#143045,#143046)),
 .UNSPECIFIED.,.F.,.F.,.F.)
B_SPLINE_SURFACE_WITH_KNOTS((2,2),(3,2,2,3),(0.710192959005574,1.),(0.142404283483302,
0.142578551421363,0.142857142857143,0.160005345227478),.UNSPECIFIED.)
GEOMETRIC_REPRESENTATION_ITEM()
RATIONAL_B_SPLINE_SURFACE(((0.999805186472059,0.999805186472059,0.999805186472059,
0.999902211834794,1.,0.993980822699459,0.990851751371591),(0.999805186472059,
0.999805186472059,0.999805186472059,0.999902211834794,1.,0.993980822699459,
0.990851751371591)))
REPRESENTATION_ITEM('')
SURFACE()
);
#2840=(
BOUNDED_SURFACE()
B_SPLINE_SURFACE(1,2,((#143054,#143055,#143056,#143057,#143058),(#143059,
#143060,#143061,#143062,#143063)),.UNSPECIFIED.,.F.,.F.,.F.)
B_SPLINE_SURFACE_WITH_KNOTS((2,2),(3,2,3),(0.710318915638881,1.),(0.573550810617188,
0.590910950629595,0.591084552029719),.UNSPECIFIED.)
GEOMETRIC_REPRESENTATION_ITEM()
RATIONAL_B_SPLINE_SURFACE(((0.998554414400369,0.992822941359368,0.990053454406147,
0.990053454406147,0.990053454406147),(0.998554414400369,0.992822941359368,
0.990053454406147,0.990053454406147,0.990053454406147)))
REPRESENTATION_ITEM('')
SURFACE()
);
#2841=(
BOUNDED_SURFACE()
B_SPLINE_SURFACE(1,2,((#143074,#143075,#143076,#143077,#143078,#143079,
#143080),(#143081,#143082,#143083,#143084,#143085,#143086,#143087)),
 .UNSPECIFIED.,.F.,.F.,.F.)
B_SPLINE_SURFACE_WITH_KNOTS((2,2),(3,2,2,3),(0.710192959007234,1.),(0.142404283483302,
0.142578551421363,0.142857142857143,0.160005345227477),.UNSPECIFIED.)
GEOMETRIC_REPRESENTATION_ITEM()
RATIONAL_B_SPLINE_SURFACE(((0.999805186472058,0.999805186472058,0.999805186472058,
0.999902211834794,1.,0.99398082269946,0.990851751371592),(0.999805186472058,
0.999805186472058,0.999805186472058,0.999902211834794,1.,0.99398082269946,
0.990851751371592)))
REPRESENTATION_ITEM('')
SURFACE()
);
#2842=(
BOUNDED_SURFACE()
B_SPLINE_SURFACE(1,2,((#143095,#143096,#143097,#143098,#143099),(#143100,
#143101,#143102,#143103,#143104)),.UNSPECIFIED.,.F.,.F.,.F.)
B_SPLINE_SURFACE_WITH_KNOTS((2,2),(3,2,3),(0.710318915638999,1.),(0.573550810617075,
0.590910950629595,0.59108455202972),.UNSPECIFIED.)
GEOMETRIC_REPRESENTATION_ITEM()
RATIONAL_B_SPLINE_SURFACE(((0.998554414400444,0.992822941359386,0.990053454406147,
0.990053454406147,0.990053454406147),(0.998554414400444,0.992822941359386,
0.990053454406147,0.990053454406147,0.990053454406147)))
REPRESENTATION_ITEM('')
SURFACE()
);
#2843=(
BOUNDED_SURFACE()
B_SPLINE_SURFACE(1,2,((#143115,#143116,#143117,#143118,#143119,#143120,
#143121),(#143122,#143123,#143124,#143125,#143126,#143127,#143128)),
 .UNSPECIFIED.,.F.,.F.,.F.)
B_SPLINE_SURFACE_WITH_KNOTS((2,2),(3,2,2,3),(0.710192959007354,1.),(0.142404283483302,
0.142578551421363,0.142857142857143,0.160005345227479),.UNSPECIFIED.)
GEOMETRIC_REPRESENTATION_ITEM()
RATIONAL_B_SPLINE_SURFACE(((0.999805186472058,0.999805186472058,0.999805186472058,
0.999902211834794,1.,0.993980822699459,0.990851751371591),(0.999805186472058,
0.999805186472058,0.999805186472058,0.999902211834794,1.,0.993980822699459,
0.990851751371591)))
REPRESENTATION_ITEM('')
SURFACE()
);
#2844=(
BOUNDED_SURFACE()
B_SPLINE_SURFACE(1,2,((#143136,#143137,#143138,#143139,#143140),(#143141,
#143142,#143143,#143144,#143145)),.UNSPECIFIED.,.F.,.F.,.F.)
B_SPLINE_SURFACE_WITH_KNOTS((2,2),(3,2,3),(0.710318915638156,1.),(0.573550810617127,
0.590910950629595,0.59108455202972),.UNSPECIFIED.)
GEOMETRIC_REPRESENTATION_ITEM()
RATIONAL_B_SPLINE_SURFACE(((0.99855441440041,0.992822941359378,0.990053454406147,
0.990053454406147,0.990053454406147),(0.99855441440041,0.992822941359377,
0.990053454406147,0.990053454406147,0.990053454406147)))
REPRESENTATION_ITEM('')
SURFACE()
);
#2845=(
BOUNDED_SURFACE()
B_SPLINE_SURFACE(1,2,((#143156,#143157,#143158,#143159,#143160,#143161,
#143162),(#143163,#143164,#143165,#143166,#143167,#143168,#143169)),
 .UNSPECIFIED.,.F.,.F.,.F.)
B_SPLINE_SURFACE_WITH_KNOTS((2,2),(3,2,2,3),(0.710192959006509,1.),(0.142404283483303,
0.142578551421363,0.142857142857143,0.160005345227408),.UNSPECIFIED.)
GEOMETRIC_REPRESENTATION_ITEM()
RATIONAL_B_SPLINE_SURFACE(((0.999805186472059,0.999805186472059,0.999805186472059,
0.999902211834794,1.,0.993980822699484,0.990851751371617),(0.999805186472059,
0.999805186472059,0.999805186472059,0.999902211834794,1.,0.993980822699484,
0.990851751371617)))
REPRESENTATION_ITEM('')
SURFACE()
);
#2846=(
BOUNDED_SURFACE()
B_SPLINE_SURFACE(1,2,((#143177,#143178,#143179,#143180,#143181),(#143182,
#143183,#143184,#143185,#143186)),.UNSPECIFIED.,.F.,.F.,.F.)
B_SPLINE_SURFACE_WITH_KNOTS((2,2),(3,2,3),(0.710318915639619,1.),(0.573550810617337,
0.590910950629595,0.591084552029718),.UNSPECIFIED.)
GEOMETRIC_REPRESENTATION_ITEM()
RATIONAL_B_SPLINE_SURFACE(((0.998554414400271,0.992822941359344,0.990053454406147,
0.990053454406147,0.990053454406147),(0.998554414400271,0.992822941359344,
0.990053454406147,0.990053454406147,0.990053454406147)))
REPRESENTATION_ITEM('')
SURFACE()
);
#2847=(
BOUNDED_SURFACE()
B_SPLINE_SURFACE(1,2,((#143194,#143195,#143196,#143197,#143198,#143199,
#143200),(#143201,#143202,#143203,#143204,#143205,#143206,#143207)),
 .UNSPECIFIED.,.F.,.F.,.F.)
B_SPLINE_SURFACE_WITH_KNOTS((2,2),(3,2,2,3),(0.710192959007984,1.),(0.142404283483302,
0.142578551421363,0.142857142857143,0.160005345227478),.UNSPECIFIED.)
GEOMETRIC_REPRESENTATION_ITEM()
RATIONAL_B_SPLINE_SURFACE(((0.999805186472059,0.999805186472059,0.999805186472059,
0.999902211834794,1.,0.993980822699459,0.990851751371592),(0.999805186472059,
0.999805186472059,0.999805186472059,0.999902211834794,1.,0.993980822699459,
0.990851751371591)))
REPRESENTATION_ITEM('')
SURFACE()
);
#2848=(
BOUNDED_SURFACE()
B_SPLINE_SURFACE(1,2,((#143209,#143210,#143211,#143212,#143213),(#143214,
#143215,#143216,#143217,#143218)),.UNSPECIFIED.,.F.,.F.,.F.)
B_SPLINE_SURFACE_WITH_KNOTS((2,2),(3,2,3),(0.710318915638755,1.),(0.573550810617439,
0.590910950629595,0.591084552029717),.UNSPECIFIED.)
GEOMETRIC_REPRESENTATION_ITEM()
RATIONAL_B_SPLINE_SURFACE(((0.998554414400204,0.992822941359328,0.990053454406147,
0.990053454406147,0.990053454406147),(0.998554414400204,0.992822941359328,
0.990053454406147,0.990053454406147,0.990053454406147)))
REPRESENTATION_ITEM('')
SURFACE()
);
#2849=(
BOUNDED_SURFACE()
B_SPLINE_SURFACE(1,2,((#143229,#143230,#143231,#143232,#143233,#143234,
#143235),(#143236,#143237,#143238,#143239,#143240,#143241,#143242)),
 .UNSPECIFIED.,.F.,.F.,.F.)
B_SPLINE_SURFACE_WITH_KNOTS((2,2),(3,2,2,3),(0.710192959007117,1.),(0.142404283483302,
0.142578551421363,0.142857142857143,0.160005345227477),.UNSPECIFIED.)
GEOMETRIC_REPRESENTATION_ITEM()
RATIONAL_B_SPLINE_SURFACE(((0.999805186472059,0.999805186472059,0.999805186472059,
0.999902211834794,1.,0.99398082269946,0.990851751371592),(0.999805186472059,
0.999805186472059,0.999805186472059,0.999902211834794,1.,0.99398082269946,
0.990851751371592)))
REPRESENTATION_ITEM('')
SURFACE()
);
#2850=(
BOUNDED_SURFACE()
B_SPLINE_SURFACE(1,2,((#143250,#143251,#143252,#143253,#143254),(#143255,
#143256,#143257,#143258,#143259)),.UNSPECIFIED.,.F.,.F.,.F.)
B_SPLINE_SURFACE_WITH_KNOTS((2,2),(3,2,3),(0.710318915638949,1.),(0.573550810617453,
0.590910950629595,0.591084552029716),.UNSPECIFIED.)
GEOMETRIC_REPRESENTATION_ITEM()
RATIONAL_B_SPLINE_SURFACE(((0.998554414400194,0.992822941359325,0.990053454406147,
0.990053454406147,0.990053454406147),(0.998554414400194,0.992822941359325,
0.990053454406147,0.990053454406147,0.990053454406147)))
REPRESENTATION_ITEM('')
SURFACE()
);
#2851=(
BOUNDED_SURFACE()
B_SPLINE_SURFACE(1,2,((#143270,#143271,#143272,#143273,#143274,#143275,
#143276),(#143277,#143278,#143279,#143280,#143281,#143282,#143283)),
 .UNSPECIFIED.,.F.,.F.,.F.)
B_SPLINE_SURFACE_WITH_KNOTS((2,2),(3,2,2,3),(0.710192959007312,1.),(0.142404283483302,
0.142578551421363,0.142857142857143,0.160005345227478),.UNSPECIFIED.)
GEOMETRIC_REPRESENTATION_ITEM()
RATIONAL_B_SPLINE_SURFACE(((0.999805186472059,0.999805186472059,0.999805186472059,
0.999902211834794,1.,0.993980822699459,0.990851751371591),(0.999805186472059,
0.999805186472059,0.999805186472059,0.999902211834794,1.,0.993980822699459,
0.990851751371591)))
REPRESENTATION_ITEM('')
SURFACE()
);
#2852=(
BOUNDED_SURFACE()
B_SPLINE_SURFACE(1,2,((#143291,#143292,#143293,#143294,#143295),(#143296,
#143297,#143298,#143299,#143300)),.UNSPECIFIED.,.F.,.F.,.F.)
B_SPLINE_SURFACE_WITH_KNOTS((2,2),(3,2,3),(0.710318915637703,1.),(0.573550810617427,
0.590910950629595,0.591084552029717),.UNSPECIFIED.)
GEOMETRIC_REPRESENTATION_ITEM()
RATIONAL_B_SPLINE_SURFACE(((0.998554414400211,0.992822941359329,0.990053454406147,
0.990053454406147,0.990053454406147),(0.998554414400211,0.992822941359329,
0.990053454406147,0.990053454406147,0.990053454406147)))
REPRESENTATION_ITEM('')
SURFACE()
);
#2853=(
BOUNDED_SURFACE()
B_SPLINE_SURFACE(1,2,((#143311,#143312,#143313,#143314,#143315,#143316,
#143317),(#143318,#143319,#143320,#143321,#143322,#143323,#143324)),
 .UNSPECIFIED.,.F.,.F.,.F.)
B_SPLINE_SURFACE_WITH_KNOTS((2,2),(3,2,2,3),(0.710192959006066,1.),(0.142404283483302,
0.142578551421363,0.142857142857143,0.160005345227477),.UNSPECIFIED.)
GEOMETRIC_REPRESENTATION_ITEM()
RATIONAL_B_SPLINE_SURFACE(((0.999805186472059,0.999805186472059,0.999805186472059,
0.999902211834794,1.,0.99398082269946,0.990851751371592),(0.999805186472059,
0.999805186472059,0.999805186472059,0.999902211834794,1.,0.99398082269946,
0.990851751371592)))
REPRESENTATION_ITEM('')
SURFACE()
);
#2854=(
BOUNDED_SURFACE()
B_SPLINE_SURFACE(1,2,((#143332,#143333,#143334,#143335,#143336),(#143337,
#143338,#143339,#143340,#143341)),.UNSPECIFIED.,.F.,.F.,.F.)
B_SPLINE_SURFACE_WITH_KNOTS((2,2),(3,2,3),(0.710318915639711,1.),(0.573550810617425,
0.590910950629665,0.591084552029787),.UNSPECIFIED.)
GEOMETRIC_REPRESENTATION_ITEM()
RATIONAL_B_SPLINE_SURFACE(((0.998554414400213,0.992822941359307,0.990053454406125,
0.990053454406125,0.990053454406125),(0.998554414400213,0.992822941359307,
0.990053454406125,0.990053454406125,0.990053454406125)))
REPRESENTATION_ITEM('')
SURFACE()
);
#2855=(
BOUNDED_SURFACE()
B_SPLINE_SURFACE(1,2,((#143352,#143353,#143354,#143355,#143356,#143357,
#143358),(#143359,#143360,#143361,#143362,#143363,#143364,#143365)),
 .UNSPECIFIED.,.F.,.F.,.F.)
B_SPLINE_SURFACE_WITH_KNOTS((2,2),(3,2,2,3),(0.71019295900807,1.),(0.142404283483303,
0.142578551421364,0.142857142857143,0.160005345227478),.UNSPECIFIED.)
GEOMETRIC_REPRESENTATION_ITEM()
RATIONAL_B_SPLINE_SURFACE(((0.999805186472059,0.999805186472059,0.999805186472059,
0.999902211834795,1.,0.993980822699459,0.990851751371591),(0.999805186472059,
0.999805186472059,0.999805186472059,0.999902211834795,1.,0.993980822699459,
0.990851751371591)))
REPRESENTATION_ITEM('')
SURFACE()
);
#2856=(
BOUNDED_SURFACE()
B_SPLINE_SURFACE(1,2,((#143373,#143374,#143375,#143376,#143377),(#143378,
#143379,#143380,#143381,#143382)),.UNSPECIFIED.,.F.,.F.,.F.)
B_SPLINE_SURFACE_WITH_KNOTS((2,2),(3,2,3),(0.710318915640079,1.),(0.573550810617452,
0.590910950629594,0.591084552029715),.UNSPECIFIED.)
GEOMETRIC_REPRESENTATION_ITEM()
RATIONAL_B_SPLINE_SURFACE(((0.998554414400195,0.992822941359326,0.990053454406147,
0.990053454406147,0.990053454406147),(0.998554414400195,0.992822941359326,
0.990053454406147,0.990053454406147,0.990053454406147)))
REPRESENTATION_ITEM('')
SURFACE()
);
#2857=(
BOUNDED_SURFACE()
B_SPLINE_SURFACE(1,2,((#143393,#143394,#143395,#143396,#143397,#143398,
#143399),(#143400,#143401,#143402,#143403,#143404,#143405,#143406)),
 .UNSPECIFIED.,.F.,.F.,.F.)
B_SPLINE_SURFACE_WITH_KNOTS((2,2),(3,2,2,3),(0.710192959008443,1.),(0.142404283483303,
0.142578551421364,0.142857142857143,0.160005345227479),.UNSPECIFIED.)
GEOMETRIC_REPRESENTATION_ITEM()
RATIONAL_B_SPLINE_SURFACE(((0.999805186472059,0.999805186472059,0.999805186472059,
0.999902211834795,1.,0.993980822699459,0.990851751371591),(0.999805186472059,
0.999805186472059,0.999805186472059,0.999902211834795,1.,0.993980822699459,
0.990851751371591)))
REPRESENTATION_ITEM('')
SURFACE()
);
#2858=(
BOUNDED_SURFACE()
B_SPLINE_SURFACE(1,2,((#143414,#143415,#143416,#143417,#143418),(#143419,
#143420,#143421,#143422,#143423)),.UNSPECIFIED.,.F.,.F.,.F.)
B_SPLINE_SURFACE_WITH_KNOTS((2,2),(3,2,3),(0.710318915639753,1.),(0.57355081061737,
0.590910950629594,0.591084552029716),.UNSPECIFIED.)
GEOMETRIC_REPRESENTATION_ITEM()
RATIONAL_B_SPLINE_SURFACE(((0.998554414400249,0.992822941359339,0.990053454406148,
0.990053454406148,0.990053454406148),(0.998554414400249,0.992822941359339,
0.990053454406148,0.990053454406148,0.990053454406148)))
REPRESENTATION_ITEM('')
SURFACE()
);
#2859=(
BOUNDED_SURFACE()
B_SPLINE_SURFACE(1,2,((#143434,#143435,#143436,#143437,#143438,#143439,
#143440),(#143441,#143442,#143443,#143444,#143445,#143446,#143447)),
 .UNSPECIFIED.,.F.,.F.,.F.)
B_SPLINE_SURFACE_WITH_KNOTS((2,2),(3,2,2,3),(0.710192959008108,1.),(0.142404283483303,
0.142578551421364,0.142857142857143,0.160005345227478),.UNSPECIFIED.)
GEOMETRIC_REPRESENTATION_ITEM()
RATIONAL_B_SPLINE_SURFACE(((0.999805186472059,0.999805186472059,0.999805186472059,
0.999902211834795,1.,0.993980822699459,0.990851751371591),(0.999805186472059,
0.999805186472059,0.999805186472059,0.999902211834795,1.,0.993980822699459,
0.990851751371591)))
REPRESENTATION_ITEM('')
SURFACE()
);
#2860=(
BOUNDED_SURFACE()
B_SPLINE_SURFACE(1,2,((#143455,#143456,#143457,#143458,#143459),(#143460,
#143461,#143462,#143463,#143464)),.UNSPECIFIED.,.F.,.F.,.F.)
B_SPLINE_SURFACE_WITH_KNOTS((2,2),(3,2,3),(0.710318915639617,1.),(0.573550810617172,
0.590910950629594,0.591084552029718),.UNSPECIFIED.)
GEOMETRIC_REPRESENTATION_ITEM()
RATIONAL_B_SPLINE_SURFACE(((0.99855441440038,0.992822941359371,0.990053454406148,
0.990053454406148,0.990053454406148),(0.99855441440038,0.992822941359371,
0.990053454406147,0.990053454406147,0.990053454406147)))
REPRESENTATION_ITEM('')
SURFACE()
);
#2861=(
BOUNDED_SURFACE()
B_SPLINE_SURFACE(1,2,((#143475,#143476,#143477,#143478,#143479,#143480,
#143481),(#143482,#143483,#143484,#143485,#143486,#143487,#143488)),
 .UNSPECIFIED.,.F.,.F.,.F.)
B_SPLINE_SURFACE_WITH_KNOTS((2,2),(3,2,2,3),(0.710192959007976,1.),(0.142404283483304,
0.142578551421364,0.142857142857143,0.160005345227403),.UNSPECIFIED.)
GEOMETRIC_REPRESENTATION_ITEM()
RATIONAL_B_SPLINE_SURFACE(((0.999805186472059,0.999805186472059,0.999805186472059,
0.999902211834795,1.,0.993980822699486,0.990851751371619),(0.999805186472059,
0.999805186472059,0.999805186472059,0.999902211834795,1.,0.993980822699486,
0.990851751371619)))
REPRESENTATION_ITEM('')
SURFACE()
);
#2862=(
BOUNDED_SURFACE()
B_SPLINE_SURFACE(1,2,((#143496,#143497,#143498),(#143499,#143500,#143501)),
 .UNSPECIFIED.,.F.,.F.,.F.)
B_SPLINE_SURFACE_WITH_KNOTS((2,2),(3,3),(0.710192959008443,1.),(0.53899963051341,
0.556316102183953),.UNSPECIFIED.)
GEOMETRIC_REPRESENTATION_ITEM()
RATIONAL_B_SPLINE_SURFACE(((0.987570037304351,0.988129172627919,0.99163541140107),
(0.987570037304351,0.988129172627919,0.99163541140107)))
REPRESENTATION_ITEM('')
SURFACE()
);
#2863=(
BOUNDED_SURFACE()
B_SPLINE_SURFACE(1,2,((#143510,#143511,#143512,#143513,#143514),(#143515,
#143516,#143517,#143518,#143519)),.UNSPECIFIED.,.F.,.F.,.F.)
B_SPLINE_SURFACE_WITH_KNOTS((2,2),(3,2,3),(0.709720368233181,1.),(0.176864064841898,
0.194132688793569,0.194731236525192),.UNSPECIFIED.)
GEOMETRIC_REPRESENTATION_ITEM()
RATIONAL_B_SPLINE_SURFACE(((0.987492606357657,0.987202831733786,0.989843896581211,
0.989843896581211,0.989843896581211),(0.987492606357657,0.987202831733786,
0.989843896581211,0.989843896581211,0.989843896581211)))
REPRESENTATION_ITEM('')
SURFACE()
);
#2864=(
BOUNDED_SURFACE()
B_SPLINE_SURFACE(1,2,((#143521,#143522,#143523),(#143524,#143525,#143526)),
 .UNSPECIFIED.,.F.,.F.,.F.)
B_SPLINE_SURFACE_WITH_KNOTS((2,2),(3,3),(0.710192959008437,1.),(0.53899963051341,
0.556316102183956),.UNSPECIFIED.)
GEOMETRIC_REPRESENTATION_ITEM()
RATIONAL_B_SPLINE_SURFACE(((0.987570037304351,0.988129172627919,0.991635411401071),
(0.987570037304351,0.988129172627919,0.991635411401071)))
REPRESENTATION_ITEM('')
SURFACE()
);
#2865=(
BOUNDED_SURFACE()
B_SPLINE_SURFACE(1,2,((#143535,#143536,#143537,#143538,#143539),(#143540,
#143541,#143542,#143543,#143544)),.UNSPECIFIED.,.F.,.F.,.F.)
B_SPLINE_SURFACE_WITH_KNOTS((2,2),(3,2,3),(0.70972036823745,1.),(0.176864064841898,
0.194132688793568,0.194731236520925),.UNSPECIFIED.)
GEOMETRIC_REPRESENTATION_ITEM()
RATIONAL_B_SPLINE_SURFACE(((0.987492606357657,0.987202831733786,0.989843896581211,
0.989843896581211,0.989843896581211),(0.987492606357657,0.987202831733786,
0.989843896581211,0.989843896581211,0.989843896581211)))
REPRESENTATION_ITEM('')
SURFACE()
);
#2866=(
BOUNDED_SURFACE()
B_SPLINE_SURFACE(1,2,((#143546,#143547,#143548),(#143549,#143550,#143551)),
 .UNSPECIFIED.,.F.,.F.,.F.)
B_SPLINE_SURFACE_WITH_KNOTS((2,2),(3,3),(0.710192959008441,1.),(0.538999630513411,
0.556316102183955),.UNSPECIFIED.)
GEOMETRIC_REPRESENTATION_ITEM()
RATIONAL_B_SPLINE_SURFACE(((0.987570037304351,0.988129172627919,0.99163541140107),
(0.987570037304351,0.988129172627919,0.99163541140107)))
REPRESENTATION_ITEM('')
SURFACE()
);
#2867=(
BOUNDED_SURFACE()
B_SPLINE_SURFACE(1,2,((#143560,#143561,#143562,#143563,#143564),(#143565,
#143566,#143567,#143568,#143569)),.UNSPECIFIED.,.F.,.F.,.F.)
B_SPLINE_SURFACE_WITH_KNOTS((2,2),(3,2,3),(0.709720368250085,1.),(0.176864064841897,
0.194132688793568,0.194731236508284),.UNSPECIFIED.)
GEOMETRIC_REPRESENTATION_ITEM()
RATIONAL_B_SPLINE_SURFACE(((0.987492606357657,0.987202831733786,0.989843896581211,
0.989843896581211,0.989843896581211),(0.987492606357657,0.987202831733786,
0.989843896581211,0.989843896581211,0.989843896581211)))
REPRESENTATION_ITEM('')
SURFACE()
);
#2868=(
BOUNDED_SURFACE()
B_SPLINE_SURFACE(1,2,((#143571,#143572,#143573),(#143574,#143575,#143576)),
 .UNSPECIFIED.,.F.,.F.,.F.)
B_SPLINE_SURFACE_WITH_KNOTS((2,2),(3,3),(0.71019295900844,1.),(0.538999630513411,
0.556316102183955),.UNSPECIFIED.)
GEOMETRIC_REPRESENTATION_ITEM()
RATIONAL_B_SPLINE_SURFACE(((0.987570037304351,0.988129172627919,0.99163541140107),
(0.987570037304351,0.988129172627919,0.99163541140107)))
REPRESENTATION_ITEM('')
SURFACE()
);
#2869=(
BOUNDED_SURFACE()
B_SPLINE_SURFACE(1,2,((#143585,#143586,#143587,#143588,#143589),(#143590,
#143591,#143592,#143593,#143594)),.UNSPECIFIED.,.F.,.F.,.F.)
B_SPLINE_SURFACE_WITH_KNOTS((2,2),(3,2,3),(0.709720368246354,1.),(0.176864064841897,
0.194132688793568,0.194731236512029),.UNSPECIFIED.)
GEOMETRIC_REPRESENTATION_ITEM()
RATIONAL_B_SPLINE_SURFACE(((0.987492606357657,0.987202831733786,0.989843896581211,
0.989843896581211,0.989843896581211),(0.987492606357657,0.987202831733786,
0.989843896581211,0.989843896581211,0.989843896581211)))
REPRESENTATION_ITEM('')
SURFACE()
);
#2870=(
BOUNDED_SURFACE()
B_SPLINE_SURFACE(1,2,((#143596,#143597,#143598),(#143599,#143600,#143601)),
 .UNSPECIFIED.,.F.,.F.,.F.)
B_SPLINE_SURFACE_WITH_KNOTS((2,2),(3,3),(0.710192959008441,1.),(0.538999630513411,
0.556316102183958),.UNSPECIFIED.)
GEOMETRIC_REPRESENTATION_ITEM()
RATIONAL_B_SPLINE_SURFACE(((0.987570037304351,0.988129172627919,0.991635411401071),
(0.987570037304351,0.988129172627919,0.991635411401071)))
REPRESENTATION_ITEM('')
SURFACE()
);
#2871=(
BOUNDED_SURFACE()
B_SPLINE_SURFACE(1,2,((#143610,#143611,#143612,#143613,#143614),(#143615,
#143616,#143617,#143618,#143619)),.UNSPECIFIED.,.F.,.F.,.F.)
B_SPLINE_SURFACE_WITH_KNOTS((2,2),(3,2,3),(0.709720368243867,1.),(0.176864064841897,
0.194132688793568,0.19473123651451),.UNSPECIFIED.)
GEOMETRIC_REPRESENTATION_ITEM()
RATIONAL_B_SPLINE_SURFACE(((0.987492606357657,0.987202831733786,0.989843896581211,
0.989843896581211,0.989843896581211),(0.987492606357657,0.987202831733786,
0.989843896581211,0.989843896581211,0.989843896581211)))
REPRESENTATION_ITEM('')
SURFACE()
);
#2872=(
BOUNDED_SURFACE()
B_SPLINE_SURFACE(1,2,((#143621,#143622,#143623),(#143624,#143625,#143626)),
 .UNSPECIFIED.,.F.,.F.,.F.)
B_SPLINE_SURFACE_WITH_KNOTS((2,2),(3,3),(0.710192959008442,1.),(0.538999630513411,
0.556316102183957),.UNSPECIFIED.)
GEOMETRIC_REPRESENTATION_ITEM()
RATIONAL_B_SPLINE_SURFACE(((0.987570037304351,0.988129172627919,0.991635411401071),
(0.987570037304351,0.988129172627919,0.991635411401071)))
REPRESENTATION_ITEM('')
SURFACE()
);
#2873=(
BOUNDED_SURFACE()
B_SPLINE_SURFACE(1,2,((#143635,#143636,#143637,#143638,#143639),(#143640,
#143641,#143642,#143643,#143644)),.UNSPECIFIED.,.F.,.F.,.F.)
B_SPLINE_SURFACE_WITH_KNOTS((2,2),(3,2,3),(0.709720368232269,1.),(0.176864064841897,
0.194132688793568,0.194731236526112),.UNSPECIFIED.)
GEOMETRIC_REPRESENTATION_ITEM()
RATIONAL_B_SPLINE_SURFACE(((0.987492606357657,0.987202831733786,0.98984389658121,
0.98984389658121,0.98984389658121),(0.987492606357657,0.987202831733786,
0.98984389658121,0.98984389658121,0.98984389658121)))
REPRESENTATION_ITEM('')
SURFACE()
);
#2874=(
BOUNDED_SURFACE()
B_SPLINE_SURFACE(1,2,((#143646,#143647,#143648),(#143649,#143650,#143651)),
 .UNSPECIFIED.,.F.,.F.,.F.)
B_SPLINE_SURFACE_WITH_KNOTS((2,2),(3,3),(0.710192959008441,1.),(0.538999630513411,
0.556316102183954),.UNSPECIFIED.)
GEOMETRIC_REPRESENTATION_ITEM()
RATIONAL_B_SPLINE_SURFACE(((0.987570037304351,0.988129172627919,0.99163541140107),
(0.987570037304351,0.988129172627919,0.99163541140107)))
REPRESENTATION_ITEM('')
SURFACE()
);
#2875=(
BOUNDED_SURFACE()
B_SPLINE_SURFACE(1,2,((#143660,#143661,#143662,#143663,#143664),(#143665,
#143666,#143667,#143668,#143669)),.UNSPECIFIED.,.F.,.F.,.F.)
B_SPLINE_SURFACE_WITH_KNOTS((2,2),(3,2,3),(0.709720368241591,1.),(0.176864064841897,
0.194132688793568,0.194731236516793),.UNSPECIFIED.)
GEOMETRIC_REPRESENTATION_ITEM()
RATIONAL_B_SPLINE_SURFACE(((0.987492606357657,0.987202831733786,0.989843896581211,
0.989843896581211,0.989843896581211),(0.987492606357657,0.987202831733786,
0.989843896581211,0.989843896581211,0.989843896581211)))
REPRESENTATION_ITEM('')
SURFACE()
);
#2876=(
BOUNDED_SURFACE()
B_SPLINE_SURFACE(1,2,((#143671,#143672,#143673),(#143674,#143675,#143676)),
 .UNSPECIFIED.,.F.,.F.,.F.)
B_SPLINE_SURFACE_WITH_KNOTS((2,2),(3,3),(0.710192959008444,1.),(0.538999630513411,
0.556316102183958),.UNSPECIFIED.)
GEOMETRIC_REPRESENTATION_ITEM()
RATIONAL_B_SPLINE_SURFACE(((0.987570037304351,0.988129172627919,0.991635411401071),
(0.987570037304351,0.988129172627919,0.991635411401071)))
REPRESENTATION_ITEM('')
SURFACE()
);
#2877=(
BOUNDED_SURFACE()
B_SPLINE_SURFACE(1,2,((#143685,#143686,#143687,#143688,#143689),(#143690,
#143691,#143692,#143693,#143694)),.UNSPECIFIED.,.F.,.F.,.F.)
B_SPLINE_SURFACE_WITH_KNOTS((2,2),(3,2,3),(0.709720368224627,1.),(0.176864064841897,
0.194132688793568,0.194731236533751),.UNSPECIFIED.)
GEOMETRIC_REPRESENTATION_ITEM()
RATIONAL_B_SPLINE_SURFACE(((0.987492606357657,0.987202831733786,0.989843896581211,
0.989843896581211,0.989843896581211),(0.987492606357657,0.987202831733786,
0.98984389658121,0.98984389658121,0.98984389658121)))
REPRESENTATION_ITEM('')
SURFACE()
);
#2878=(
BOUNDED_SURFACE()
B_SPLINE_SURFACE(1,2,((#143696,#143697,#143698),(#143699,#143700,#143701)),
 .UNSPECIFIED.,.F.,.F.,.F.)
B_SPLINE_SURFACE_WITH_KNOTS((2,2),(3,3),(0.710192959008446,1.),(0.538999630513411,
0.556316102183958),.UNSPECIFIED.)
GEOMETRIC_REPRESENTATION_ITEM()
RATIONAL_B_SPLINE_SURFACE(((0.987570037304351,0.988129172627919,0.991635411401071),
(0.987570037304351,0.988129172627919,0.991635411401071)))
REPRESENTATION_ITEM('')
SURFACE()
);
#2879=(
BOUNDED_SURFACE()
B_SPLINE_SURFACE(1,2,((#143710,#143711,#143712,#143713,#143714),(#143715,
#143716,#143717,#143718,#143719)),.UNSPECIFIED.,.F.,.F.,.F.)
B_SPLINE_SURFACE_WITH_KNOTS((2,2),(3,2,3),(0.709720368239206,1.),(0.176864064841897,
0.194132688793568,0.194731236519174),.UNSPECIFIED.)
GEOMETRIC_REPRESENTATION_ITEM()
RATIONAL_B_SPLINE_SURFACE(((0.987492606357657,0.987202831733786,0.989843896581211,
0.989843896581211,0.989843896581211),(0.987492606357657,0.987202831733786,
0.989843896581211,0.989843896581211,0.989843896581211)))
REPRESENTATION_ITEM('')
SURFACE()
);
#2880=(
BOUNDED_SURFACE()
B_SPLINE_SURFACE(1,2,((#143721,#143722,#143723),(#143724,#143725,#143726)),
 .UNSPECIFIED.,.F.,.F.,.F.)
B_SPLINE_SURFACE_WITH_KNOTS((2,2),(3,3),(0.710192959008439,1.),(0.538999630513411,
0.556316102183958),.UNSPECIFIED.)
GEOMETRIC_REPRESENTATION_ITEM()
RATIONAL_B_SPLINE_SURFACE(((0.987570037304351,0.988129172627919,0.991635411401071),
(0.987570037304351,0.988129172627919,0.991635411401071)))
REPRESENTATION_ITEM('')
SURFACE()
);
#2881=(
BOUNDED_SURFACE()
B_SPLINE_SURFACE(1,2,((#143735,#143736,#143737,#143738,#143739),(#143740,
#143741,#143742,#143743,#143744)),.UNSPECIFIED.,.F.,.F.,.F.)
B_SPLINE_SURFACE_WITH_KNOTS((2,2),(3,2,3),(0.709720368220064,1.),(0.176864064841897,
0.194132688793568,0.194731236538315),.UNSPECIFIED.)
GEOMETRIC_REPRESENTATION_ITEM()
RATIONAL_B_SPLINE_SURFACE(((0.987492606357657,0.987202831733786,0.98984389658121,
0.98984389658121,0.98984389658121),(0.987492606357657,0.987202831733786,
0.989843896581211,0.989843896581211,0.989843896581211)))
REPRESENTATION_ITEM('')
SURFACE()
);
#2882=(
BOUNDED_SURFACE()
B_SPLINE_SURFACE(1,2,((#143746,#143747,#143748),(#143749,#143750,#143751)),
 .UNSPECIFIED.,.F.,.F.,.F.)
B_SPLINE_SURFACE_WITH_KNOTS((2,2),(3,3),(0.710192959008444,1.),(0.538999630513411,
0.556316102183958),.UNSPECIFIED.)
GEOMETRIC_REPRESENTATION_ITEM()
RATIONAL_B_SPLINE_SURFACE(((0.987570037304351,0.988129172627919,0.991635411401071),
(0.987570037304351,0.988129172627919,0.991635411401071)))
REPRESENTATION_ITEM('')
SURFACE()
);
#2883=(
BOUNDED_SURFACE()
B_SPLINE_SURFACE(1,2,((#143760,#143761,#143762,#143763,#143764),(#143765,
#143766,#143767,#143768,#143769)),.UNSPECIFIED.,.F.,.F.,.F.)
B_SPLINE_SURFACE_WITH_KNOTS((2,2),(3,2,3),(0.709720368252039,1.),(0.176864064841897,
0.194132688793568,0.194731236506339),.UNSPECIFIED.)
GEOMETRIC_REPRESENTATION_ITEM()
RATIONAL_B_SPLINE_SURFACE(((0.987492606357657,0.987202831733786,0.989843896581211,
0.989843896581211,0.989843896581211),(0.987492606357657,0.987202831733786,
0.989843896581211,0.989843896581211,0.989843896581211)))
REPRESENTATION_ITEM('')
SURFACE()
);
#2884=(
BOUNDED_SURFACE()
B_SPLINE_SURFACE(1,2,((#143771,#143772,#143773),(#143774,#143775,#143776)),
 .UNSPECIFIED.,.F.,.F.,.F.)
B_SPLINE_SURFACE_WITH_KNOTS((2,2),(3,3),(0.710192959008441,1.),(0.538999630513411,
0.556316102183958),.UNSPECIFIED.)
GEOMETRIC_REPRESENTATION_ITEM()
RATIONAL_B_SPLINE_SURFACE(((0.987570037304351,0.988129172627919,0.991635411401071),
(0.987570037304351,0.988129172627919,0.991635411401071)))
REPRESENTATION_ITEM('')
SURFACE()
);
#2885=(
BOUNDED_SURFACE()
B_SPLINE_SURFACE(1,2,((#143785,#143786,#143787,#143788,#143789),(#143790,
#143791,#143792,#143793,#143794)),.UNSPECIFIED.,.F.,.F.,.F.)
B_SPLINE_SURFACE_WITH_KNOTS((2,2),(3,2,3),(0.709720368247964,1.),(0.176864064841897,
0.194132688793568,0.194731236510412),.UNSPECIFIED.)
GEOMETRIC_REPRESENTATION_ITEM()
RATIONAL_B_SPLINE_SURFACE(((0.987492606357657,0.987202831733786,0.989843896581211,
0.989843896581211,0.989843896581211),(0.987492606357657,0.987202831733786,
0.989843896581211,0.989843896581211,0.989843896581211)))
REPRESENTATION_ITEM('')
SURFACE()
);
#2886=(
BOUNDED_SURFACE()
B_SPLINE_SURFACE(1,2,((#143796,#143797,#143798),(#143799,#143800,#143801)),
 .UNSPECIFIED.,.F.,.F.,.F.)
B_SPLINE_SURFACE_WITH_KNOTS((2,2),(3,3),(0.71019295900844,1.),(0.538999630513411,
0.556316102183955),.UNSPECIFIED.)
GEOMETRIC_REPRESENTATION_ITEM()
RATIONAL_B_SPLINE_SURFACE(((0.987570037304351,0.988129172627919,0.99163541140107),
(0.987570037304351,0.988129172627919,0.99163541140107)))
REPRESENTATION_ITEM('')
SURFACE()
);
#2887=(
BOUNDED_SURFACE()
B_SPLINE_SURFACE(1,2,((#143810,#143811,#143812,#143813,#143814),(#143815,
#143816,#143817,#143818,#143819)),.UNSPECIFIED.,.F.,.F.,.F.)
B_SPLINE_SURFACE_WITH_KNOTS((2,2),(3,2,3),(0.7097203682361,1.),(0.176864064841897,
0.194132688793568,0.194731236522273),.UNSPECIFIED.)
GEOMETRIC_REPRESENTATION_ITEM()
RATIONAL_B_SPLINE_SURFACE(((0.987492606357657,0.987202831733786,0.989843896581211,
0.989843896581211,0.989843896581211),(0.987492606357657,0.987202831733786,
0.98984389658121,0.98984389658121,0.98984389658121)))
REPRESENTATION_ITEM('')
SURFACE()
);
#2888=(
BOUNDED_SURFACE()
B_SPLINE_SURFACE(1,2,((#143821,#143822,#143823),(#143824,#143825,#143826)),
 .UNSPECIFIED.,.F.,.F.,.F.)
B_SPLINE_SURFACE_WITH_KNOTS((2,2),(3,3),(0.710192959008442,1.),(0.538999630513411,
0.556316102183955),.UNSPECIFIED.)
GEOMETRIC_REPRESENTATION_ITEM()
RATIONAL_B_SPLINE_SURFACE(((0.987570037304351,0.988129172627919,0.99163541140107),
(0.987570037304351,0.988129172627919,0.99163541140107)))
REPRESENTATION_ITEM('')
SURFACE()
);
#2889=(
BOUNDED_SURFACE()
B_SPLINE_SURFACE(1,2,((#143835,#143836,#143837,#143838,#143839),(#143840,
#143841,#143842,#143843,#143844)),.UNSPECIFIED.,.F.,.F.,.F.)
B_SPLINE_SURFACE_WITH_KNOTS((2,2),(3,2,3),(0.709720368226764,1.),(0.176864064841897,
0.194132688793568,0.194731236531613),.UNSPECIFIED.)
GEOMETRIC_REPRESENTATION_ITEM()
RATIONAL_B_SPLINE_SURFACE(((0.987492606357657,0.987202831733786,0.989843896581211,
0.989843896581211,0.989843896581211),(0.987492606357657,0.987202831733786,
0.989843896581211,0.989843896581211,0.989843896581211)))
REPRESENTATION_ITEM('')
SURFACE()
);
#2890=(
BOUNDED_SURFACE()
B_SPLINE_SURFACE(1,2,((#143846,#143847,#143848),(#143849,#143850,#143851)),
 .UNSPECIFIED.,.F.,.F.,.F.)
B_SPLINE_SURFACE_WITH_KNOTS((2,2),(3,3),(0.710192959008444,1.),(0.538999630513411,
0.556316102183958),.UNSPECIFIED.)
GEOMETRIC_REPRESENTATION_ITEM()
RATIONAL_B_SPLINE_SURFACE(((0.987570037304351,0.988129172627919,0.991635411401071),
(0.987570037304351,0.988129172627919,0.991635411401071)))
REPRESENTATION_ITEM('')
SURFACE()
);
#2891=(
BOUNDED_SURFACE()
B_SPLINE_SURFACE(1,2,((#143860,#143861,#143862,#143863,#143864),(#143865,
#143866,#143867,#143868,#143869)),.UNSPECIFIED.,.F.,.F.,.F.)
B_SPLINE_SURFACE_WITH_KNOTS((2,2),(3,2,3),(0.709720368237924,1.),(0.176864064841897,
0.194132688793568,0.194731236520456),.UNSPECIFIED.)
GEOMETRIC_REPRESENTATION_ITEM()
RATIONAL_B_SPLINE_SURFACE(((0.987492606357657,0.987202831733786,0.989843896581211,
0.989843896581211,0.989843896581211),(0.987492606357657,0.987202831733786,
0.989843896581211,0.989843896581211,0.989843896581211)))
REPRESENTATION_ITEM('')
SURFACE()
);
#2892=(
BOUNDED_SURFACE()
B_SPLINE_SURFACE(1,2,((#143871,#143872,#143873),(#143874,#143875,#143876)),
 .UNSPECIFIED.,.F.,.F.,.F.)
B_SPLINE_SURFACE_WITH_KNOTS((2,2),(3,3),(0.710192959008442,1.),(0.538999630513411,
0.556316102183955),.UNSPECIFIED.)
GEOMETRIC_REPRESENTATION_ITEM()
RATIONAL_B_SPLINE_SURFACE(((0.987570037304351,0.988129172627919,0.99163541140107),
(0.987570037304351,0.988129172627919,0.99163541140107)))
REPRESENTATION_ITEM('')
SURFACE()
);
#2893=(
BOUNDED_SURFACE()
B_SPLINE_SURFACE(1,2,((#143885,#143886,#143887,#143888,#143889),(#143890,
#143891,#143892,#143893,#143894)),.UNSPECIFIED.,.F.,.F.,.F.)
B_SPLINE_SURFACE_WITH_KNOTS((2,2),(3,2,3),(0.709720368221021,1.),(0.176864064841897,
0.194132688793568,0.194731236537358),.UNSPECIFIED.)
GEOMETRIC_REPRESENTATION_ITEM()
RATIONAL_B_SPLINE_SURFACE(((0.987492606357657,0.987202831733786,0.98984389658121,
0.98984389658121,0.98984389658121),(0.987492606357657,0.987202831733786,
0.98984389658121,0.98984389658121,0.98984389658121)))
REPRESENTATION_ITEM('')
SURFACE()
);
#2894=(
BOUNDED_SURFACE()
B_SPLINE_SURFACE(1,2,((#143896,#143897,#143898),(#143899,#143900,#143901)),
 .UNSPECIFIED.,.F.,.F.,.F.)
B_SPLINE_SURFACE_WITH_KNOTS((2,2),(3,3),(0.71019295900844,1.),(0.538999630513411,
0.556316102183957),.UNSPECIFIED.)
GEOMETRIC_REPRESENTATION_ITEM()
RATIONAL_B_SPLINE_SURFACE(((0.987570037304351,0.988129172627919,0.991635411401071),
(0.987570037304351,0.988129172627919,0.991635411401071)))
REPRESENTATION_ITEM('')
SURFACE()
);
#2895=(
BOUNDED_SURFACE()
B_SPLINE_SURFACE(1,2,((#143910,#143911,#143912,#143913,#143914),(#143915,
#143916,#143917,#143918,#143919)),.UNSPECIFIED.,.F.,.F.,.F.)
B_SPLINE_SURFACE_WITH_KNOTS((2,2),(3,2,3),(0.709720368226753,1.),(0.176864064841897,
0.194132688793568,0.194731236531624),.UNSPECIFIED.)
GEOMETRIC_REPRESENTATION_ITEM()
RATIONAL_B_SPLINE_SURFACE(((0.987492606357657,0.987202831733786,0.989843896581211,
0.989843896581211,0.989843896581211),(0.987492606357657,0.987202831733786,
0.98984389658121,0.98984389658121,0.98984389658121)))
REPRESENTATION_ITEM('')
SURFACE()
);
#2896=(
BOUNDED_SURFACE()
B_SPLINE_SURFACE(1,2,((#143921,#143922,#143923),(#143924,#143925,#143926)),
 .UNSPECIFIED.,.F.,.F.,.F.)
B_SPLINE_SURFACE_WITH_KNOTS((2,2),(3,3),(0.710192959008443,1.),(0.538999630513411,
0.556316102183958),.UNSPECIFIED.)
GEOMETRIC_REPRESENTATION_ITEM()
RATIONAL_B_SPLINE_SURFACE(((0.987570037304351,0.988129172627919,0.991635411401071),
(0.987570037304351,0.988129172627919,0.991635411401071)))
REPRESENTATION_ITEM('')
SURFACE()
);
#2897=(
BOUNDED_SURFACE()
B_SPLINE_SURFACE(1,2,((#143935,#143936,#143937,#143938,#143939),(#143940,
#143941,#143942,#143943,#143944)),.UNSPECIFIED.,.F.,.F.,.F.)
B_SPLINE_SURFACE_WITH_KNOTS((2,2),(3,2,3),(0.709720368249467,1.),(0.176864064841897,
0.194132688793568,0.19473123650891),.UNSPECIFIED.)
GEOMETRIC_REPRESENTATION_ITEM()
RATIONAL_B_SPLINE_SURFACE(((0.987492606357657,0.987202831733786,0.989843896581211,
0.989843896581211,0.989843896581211),(0.987492606357657,0.987202831733786,
0.989843896581211,0.989843896581211,0.989843896581211)))
REPRESENTATION_ITEM('')
SURFACE()
);
#2898=(
BOUNDED_SURFACE()
B_SPLINE_SURFACE(1,2,((#143946,#143947,#143948),(#143949,#143950,#143951)),
 .UNSPECIFIED.,.F.,.F.,.F.)
B_SPLINE_SURFACE_WITH_KNOTS((2,2),(3,3),(0.710192959008441,1.),(0.538999630513411,
0.556316102183958),.UNSPECIFIED.)
GEOMETRIC_REPRESENTATION_ITEM()
RATIONAL_B_SPLINE_SURFACE(((0.987570037304351,0.988129172627919,0.991635411401071),
(0.987570037304351,0.988129172627919,0.991635411401071)))
REPRESENTATION_ITEM('')
SURFACE()
);
#2899=(
BOUNDED_SURFACE()
B_SPLINE_SURFACE(1,2,((#143960,#143961,#143962,#143963,#143964),(#143965,
#143966,#143967,#143968,#143969)),.UNSPECIFIED.,.F.,.F.,.F.)
B_SPLINE_SURFACE_WITH_KNOTS((2,2),(3,2,3),(0.709720368252126,1.),(0.176864064841897,
0.194132688793568,0.194731236506258),.UNSPECIFIED.)
GEOMETRIC_REPRESENTATION_ITEM()
RATIONAL_B_SPLINE_SURFACE(((0.987492606357657,0.987202831733786,0.989843896581211,
0.989843896581211,0.989843896581211),(0.987492606357657,0.987202831733786,
0.989843896581211,0.989843896581211,0.989843896581211)))
REPRESENTATION_ITEM('')
SURFACE()
);
#2900=(
BOUNDED_SURFACE()
B_SPLINE_SURFACE(1,2,((#143971,#143972,#143973),(#143974,#143975,#143976)),
 .UNSPECIFIED.,.F.,.F.,.F.)
B_SPLINE_SURFACE_WITH_KNOTS((2,2),(3,3),(0.71019295900844,1.),(0.538999630513411,
0.556316102183955),.UNSPECIFIED.)
GEOMETRIC_REPRESENTATION_ITEM()
RATIONAL_B_SPLINE_SURFACE(((0.987570037304351,0.988129172627919,0.99163541140107),
(0.987570037304351,0.988129172627919,0.99163541140107)))
REPRESENTATION_ITEM('')
SURFACE()
);
#2901=(
BOUNDED_SURFACE()
B_SPLINE_SURFACE(1,2,((#143985,#143986,#143987,#143988,#143989),(#143990,
#143991,#143992,#143993,#143994)),.UNSPECIFIED.,.F.,.F.,.F.)
B_SPLINE_SURFACE_WITH_KNOTS((2,2),(3,2,3),(0.709720368257119,1.),(0.176864064841897,
0.194132688793568,0.194731236312158),.UNSPECIFIED.)
GEOMETRIC_REPRESENTATION_ITEM()
RATIONAL_B_SPLINE_SURFACE(((0.987492606357657,0.987202831733786,0.98984389658121,
0.98984389658121,0.98984389658121),(0.987492606357657,0.987202831733786,
0.98984389658121,0.98984389658121,0.98984389658121)))
REPRESENTATION_ITEM('')
SURFACE()
);
#2902=(
BOUNDED_SURFACE()
B_SPLINE_SURFACE(1,2,((#143996,#143997,#143998),(#143999,#144000,#144001)),
 .UNSPECIFIED.,.F.,.F.,.F.)
B_SPLINE_SURFACE_WITH_KNOTS((2,2),(3,3),(0.710192959008293,1.),(0.538999630513123,
0.556316102183955),.UNSPECIFIED.)
GEOMETRIC_REPRESENTATION_ITEM()
RATIONAL_B_SPLINE_SURFACE(((0.987570037304332,0.988129172627861,0.99163541140107),
(0.987570037304332,0.988129172627861,0.99163541140107)))
REPRESENTATION_ITEM('')
SURFACE()
);
#2903=(
BOUNDED_SURFACE()
B_SPLINE_SURFACE(1,2,((#144010,#144011,#144012,#144013,#144014),(#144015,
#144016,#144017,#144018,#144019)),.UNSPECIFIED.,.F.,.F.,.F.)
B_SPLINE_SURFACE_WITH_KNOTS((2,2),(3,2,3),(0.709720368254059,1.),(0.176864064841898,
0.194132688793569,0.194731236504179),.UNSPECIFIED.)
GEOMETRIC_REPRESENTATION_ITEM()
RATIONAL_B_SPLINE_SURFACE(((0.987492606357657,0.987202831733786,0.989843896581211,
0.989843896581211,0.989843896581211),(0.987492606357657,0.987202831733786,
0.989843896581211,0.989843896581211,0.989843896581211)))
REPRESENTATION_ITEM('')
SURFACE()
);
#2904=(
BOUNDED_SURFACE()
B_SPLINE_SURFACE(1,2,((#144021,#144022,#144023),(#144024,#144025,#144026)),
 .UNSPECIFIED.,.F.,.F.,.F.)
B_SPLINE_SURFACE_WITH_KNOTS((2,2),(3,3),(0.71019295900805,1.),(0.53899963051341,
0.556316102183953),.UNSPECIFIED.)
GEOMETRIC_REPRESENTATION_ITEM()
RATIONAL_B_SPLINE_SURFACE(((0.987570037304351,0.988129172627919,0.99163541140107),
(0.987570037304351,0.988129172627919,0.99163541140107)))
REPRESENTATION_ITEM('')
SURFACE()
);
#2905=(
BOUNDED_SURFACE()
B_SPLINE_SURFACE(1,2,((#144035,#144036,#144037,#144038,#144039),(#144040,
#144041,#144042,#144043,#144044)),.UNSPECIFIED.,.F.,.F.,.F.)
B_SPLINE_SURFACE_WITH_KNOTS((2,2),(3,2,3),(0.709720368249968,1.),(0.176864064841898,
0.194132688793569,0.194731236508023),.UNSPECIFIED.)
GEOMETRIC_REPRESENTATION_ITEM()
RATIONAL_B_SPLINE_SURFACE(((0.987492606357657,0.987202831733786,0.989843896581211,
0.989843896581211,0.989843896581211),(0.987492606357657,0.987202831733786,
0.989843896581211,0.989843896581211,0.989843896581211)))
REPRESENTATION_ITEM('')
SURFACE()
);
#2906=(
BOUNDED_SURFACE()
B_SPLINE_SURFACE(1,2,((#144046,#144047,#144048),(#144049,#144050,#144051)),
 .UNSPECIFIED.,.F.,.F.,.F.)
B_SPLINE_SURFACE_WITH_KNOTS((2,2),(3,3),(0.710192959006647,1.),(0.53899963051341,
0.556316102183956),.UNSPECIFIED.)
GEOMETRIC_REPRESENTATION_ITEM()
RATIONAL_B_SPLINE_SURFACE(((0.987570037304351,0.988129172627919,0.991635411401071),
(0.987570037304351,0.988129172627919,0.991635411401071)))
REPRESENTATION_ITEM('')
SURFACE()
);
#2907=(
BOUNDED_SURFACE()
B_SPLINE_SURFACE(1,2,((#144060,#144061,#144062,#144063,#144064),(#144065,
#144066,#144067,#144068,#144069)),.UNSPECIFIED.,.F.,.F.,.F.)
B_SPLINE_SURFACE_WITH_KNOTS((2,2),(3,2,3),(0.709720368240864,1.),(0.176864064841898,
0.194132688793569,0.194731236515723),.UNSPECIFIED.)
GEOMETRIC_REPRESENTATION_ITEM()
RATIONAL_B_SPLINE_SURFACE(((0.987492606357657,0.987202831733786,0.989843896581211,
0.989843896581211,0.989843896581211),(0.987492606357657,0.987202831733786,
0.989843896581211,0.989843896581211,0.989843896581211)))
REPRESENTATION_ITEM('')
SURFACE()
);
#2908=(
BOUNDED_SURFACE()
B_SPLINE_SURFACE(1,2,((#144071,#144072,#144073),(#144074,#144075,#144076)),
 .UNSPECIFIED.,.F.,.F.,.F.)
B_SPLINE_SURFACE_WITH_KNOTS((2,2),(3,3),(0.710192959007974,1.),(0.53899963051341,
0.556316102183953),.UNSPECIFIED.)
GEOMETRIC_REPRESENTATION_ITEM()
RATIONAL_B_SPLINE_SURFACE(((0.987570037304351,0.988129172627919,0.99163541140107),
(0.987570037304351,0.988129172627919,0.99163541140107)))
REPRESENTATION_ITEM('')
SURFACE()
);
#2909=(
BOUNDED_SURFACE()
B_SPLINE_SURFACE(1,2,((#144085,#144086,#144087,#144088,#144089),(#144090,
#144091,#144092,#144093,#144094)),.UNSPECIFIED.,.F.,.F.,.F.)
B_SPLINE_SURFACE_WITH_KNOTS((2,2),(3,2,3),(0.709720368223987,1.),(0.176864064841898,
0.194132688793569,0.194731236533929),.UNSPECIFIED.)
GEOMETRIC_REPRESENTATION_ITEM()
RATIONAL_B_SPLINE_SURFACE(((0.987492606357657,0.987202831733786,0.989843896581211,
0.989843896581211,0.989843896581211),(0.987492606357657,0.987202831733786,
0.989843896581211,0.989843896581211,0.989843896581211)))
REPRESENTATION_ITEM('')
SURFACE()
);
#2910=(
BOUNDED_SURFACE()
B_SPLINE_SURFACE(1,2,((#144096,#144097,#144098),(#144099,#144100,#144101)),
 .UNSPECIFIED.,.F.,.F.,.F.)
B_SPLINE_SURFACE_WITH_KNOTS((2,2),(3,3),(0.710192959008353,1.),(0.53899963051341,
0.556316102183954),.UNSPECIFIED.)
GEOMETRIC_REPRESENTATION_ITEM()
RATIONAL_B_SPLINE_SURFACE(((0.987570037304351,0.988129172627919,0.99163541140107),
(0.987570037304351,0.988129172627919,0.99163541140107)))
REPRESENTATION_ITEM('')
SURFACE()
);
#2911=(
BOUNDED_SURFACE()
B_SPLINE_SURFACE(1,2,((#144110,#144111,#144112,#144113,#144114),(#144115,
#144116,#144117,#144118,#144119)),.UNSPECIFIED.,.F.,.F.,.F.)
B_SPLINE_SURFACE_WITH_KNOTS((2,2),(3,2,3),(0.70972036823388,1.),(0.176864064841898,
0.194132688793569,0.194731236524411),.UNSPECIFIED.)
GEOMETRIC_REPRESENTATION_ITEM()
RATIONAL_B_SPLINE_SURFACE(((0.987492606357657,0.987202831733786,0.989843896581211,
0.989843896581211,0.989843896581211),(0.987492606357657,0.987202831733786,
0.989843896581211,0.989843896581211,0.989843896581211)))
REPRESENTATION_ITEM('')
SURFACE()
);
#2912=(
BOUNDED_SURFACE()
B_SPLINE_SURFACE(1,2,((#144121,#144122,#144123),(#144124,#144125,#144126)),
 .UNSPECIFIED.,.F.,.F.,.F.)
B_SPLINE_SURFACE_WITH_KNOTS((2,2),(3,3),(0.710192959008359,1.),(0.53899963051341,
0.556316102183956),.UNSPECIFIED.)
GEOMETRIC_REPRESENTATION_ITEM()
RATIONAL_B_SPLINE_SURFACE(((0.987570037304351,0.988129172627919,0.991635411401071),
(0.987570037304351,0.988129172627919,0.991635411401071)))
REPRESENTATION_ITEM('')
SURFACE()
);
#2913=(
BOUNDED_SURFACE()
B_SPLINE_SURFACE(1,2,((#144135,#144136,#144137,#144138,#144139),(#144140,
#144141,#144142,#144143,#144144)),.UNSPECIFIED.,.F.,.F.,.F.)
B_SPLINE_SURFACE_WITH_KNOTS((2,2),(3,2,3),(0.709720368257934,1.),(0.176864064841898,
0.194132688793569,0.194731236500374),.UNSPECIFIED.)
GEOMETRIC_REPRESENTATION_ITEM()
RATIONAL_B_SPLINE_SURFACE(((0.987492606357657,0.987202831733786,0.989843896581211,
0.989843896581211,0.989843896581211),(0.987492606357657,0.987202831733786,
0.989843896581211,0.989843896581211,0.989843896581211)))
REPRESENTATION_ITEM('')
SURFACE()
);
#2914=(
BOUNDED_SURFACE()
B_SPLINE_SURFACE(1,2,((#144146,#144147,#144148),(#144149,#144150,#144151)),
 .UNSPECIFIED.,.F.,.F.,.F.)
B_SPLINE_SURFACE_WITH_KNOTS((2,2),(3,3),(0.710192959008367,1.),(0.53899963051341,
0.556316102183953),.UNSPECIFIED.)
GEOMETRIC_REPRESENTATION_ITEM()
RATIONAL_B_SPLINE_SURFACE(((0.987570037304351,0.988129172627919,0.99163541140107),
(0.987570037304351,0.988129172627919,0.99163541140107)))
REPRESENTATION_ITEM('')
SURFACE()
);
#2915=(
BOUNDED_SURFACE()
B_SPLINE_SURFACE(1,2,((#144160,#144161,#144162,#144163,#144164),(#144165,
#144166,#144167,#144168,#144169)),.UNSPECIFIED.,.F.,.F.,.F.)
B_SPLINE_SURFACE_WITH_KNOTS((2,2),(3,2,3),(0.70972036823852,1.),(0.176864064841898,
0.194132688793569,0.194731236519792),.UNSPECIFIED.)
GEOMETRIC_REPRESENTATION_ITEM()
RATIONAL_B_SPLINE_SURFACE(((0.987492606357657,0.987202831733786,0.989843896581211,
0.989843896581211,0.989843896581211),(0.987492606357657,0.987202831733786,
0.989843896581211,0.989843896581211,0.989843896581211)))
REPRESENTATION_ITEM('')
SURFACE()
);
#2916=(
BOUNDED_SURFACE()
B_SPLINE_SURFACE(1,2,((#144171,#144172,#144173),(#144174,#144175,#144176)),
 .UNSPECIFIED.,.F.,.F.,.F.)
B_SPLINE_SURFACE_WITH_KNOTS((2,2),(3,3),(0.710192959008085,1.),(0.53899963051341,
0.556316102183954),.UNSPECIFIED.)
GEOMETRIC_REPRESENTATION_ITEM()
RATIONAL_B_SPLINE_SURFACE(((0.987570037304351,0.988129172627919,0.99163541140107),
(0.987570037304351,0.988129172627919,0.99163541140107)))
REPRESENTATION_ITEM('')
SURFACE()
);
#2917=(
BOUNDED_SURFACE()
B_SPLINE_SURFACE(1,2,((#144185,#144186,#144187,#144188,#144189),(#144190,
#144191,#144192,#144193,#144194)),.UNSPECIFIED.,.F.,.F.,.F.)
B_SPLINE_SURFACE_WITH_KNOTS((2,2),(3,2,3),(0.709720368237269,1.),(0.176864064841898,
0.194132688793569,0.194731236520761),.UNSPECIFIED.)
GEOMETRIC_REPRESENTATION_ITEM()
RATIONAL_B_SPLINE_SURFACE(((0.987492606357657,0.987202831733786,0.989843896581211,
0.989843896581211,0.989843896581211),(0.987492606357657,0.987202831733786,
0.989843896581211,0.989843896581211,0.989843896581211)))
REPRESENTATION_ITEM('')
SURFACE()
);
#2918=(
BOUNDED_SURFACE()
B_SPLINE_SURFACE(1,2,((#144196,#144197,#144198),(#144199,#144200,#144201)),
 .UNSPECIFIED.,.F.,.F.,.F.)
B_SPLINE_SURFACE_WITH_KNOTS((2,2),(3,3),(0.710192959008438,1.),(0.53899963051341,
0.556316102183956),.UNSPECIFIED.)
GEOMETRIC_REPRESENTATION_ITEM()
RATIONAL_B_SPLINE_SURFACE(((0.987570037304351,0.988129172627919,0.991635411401071),
(0.987570037304351,0.988129172627919,0.991635411401071)))
REPRESENTATION_ITEM('')
SURFACE()
);
#2919=(
BOUNDED_SURFACE()
B_SPLINE_SURFACE(1,2,((#144210,#144211,#144212,#144213,#144214),(#144215,
#144216,#144217,#144218,#144219)),.UNSPECIFIED.,.F.,.F.,.F.)
B_SPLINE_SURFACE_WITH_KNOTS((2,2),(3,2,3),(0.70972036823978,1.),(0.176864064841898,
0.194132688793569,0.194731236518602),.UNSPECIFIED.)
GEOMETRIC_REPRESENTATION_ITEM()
RATIONAL_B_SPLINE_SURFACE(((0.987492606357657,0.987202831733786,0.989843896581211,
0.989843896581211,0.989843896581211),(0.987492606357657,0.987202831733786,
0.989843896581211,0.989843896581211,0.989843896581211)))
REPRESENTATION_ITEM('')
SURFACE()
);
#2920=(
BOUNDED_SURFACE()
B_SPLINE_SURFACE(1,2,((#144221,#144222,#144223),(#144224,#144225,#144226)),
 .UNSPECIFIED.,.F.,.F.,.F.)
B_SPLINE_SURFACE_WITH_KNOTS((2,2),(3,3),(0.,0.28968108435992),(0.125066077454537,
0.142578551421365),.UNSPECIFIED.)
GEOMETRIC_REPRESENTATION_ITEM()
RATIONAL_B_SPLINE_SURFACE(((0.990621203777022,0.993706096834649,0.999805186472059),
(0.990621203777022,0.993706096834649,0.999805186472059)))
REPRESENTATION_ITEM('')
SURFACE()
);
#2921=(
BOUNDED_SURFACE()
B_SPLINE_SURFACE(1,2,((#144235,#144236,#144237),(#144238,#144239,#144240)),
 .UNSPECIFIED.,.F.,.F.,.F.)
B_SPLINE_SURFACE_WITH_KNOTS((2,2),(3,3),(0.,0.289807040992006),(0.590910950629593,
0.60808458519997),.UNSPECIFIED.)
GEOMETRIC_REPRESENTATION_ITEM()
RATIONAL_B_SPLINE_SURFACE(((0.990053454406147,0.987313720921968,0.987472672298934),
(0.990053454406147,0.987313720921968,0.987472672298934)))
REPRESENTATION_ITEM('')
SURFACE()
);
#2922=(
BOUNDED_SURFACE()
B_SPLINE_SURFACE(1,2,((#144242,#144243,#144244),(#144245,#144246,#144247)),
 .UNSPECIFIED.,.F.,.F.,.F.)
B_SPLINE_SURFACE_WITH_KNOTS((2,2),(3,3),(0.,0.289681084359914),(0.125066077454537,
0.142578551421365),.UNSPECIFIED.)
GEOMETRIC_REPRESENTATION_ITEM()
RATIONAL_B_SPLINE_SURFACE(((0.990621203777022,0.993706096834649,0.999805186472059),
(0.990621203777022,0.993706096834649,0.999805186472059)))
REPRESENTATION_ITEM('')
SURFACE()
);
#2923=(
BOUNDED_SURFACE()
B_SPLINE_SURFACE(1,2,((#144256,#144257,#144258),(#144259,#144260,#144261)),
 .UNSPECIFIED.,.F.,.F.,.F.)
B_SPLINE_SURFACE_WITH_KNOTS((2,2),(3,3),(0.,0.289807040991665),(0.590910950629593,
0.608084585199969),.UNSPECIFIED.)
GEOMETRIC_REPRESENTATION_ITEM()
RATIONAL_B_SPLINE_SURFACE(((0.990053454406147,0.987313720921968,0.987472672298934),
(0.990053454406147,0.987313720921968,0.987472672298934)))
REPRESENTATION_ITEM('')
SURFACE()
);
#2924=(
BOUNDED_SURFACE()
B_SPLINE_SURFACE(1,2,((#144263,#144264,#144265),(#144266,#144267,#144268)),
 .UNSPECIFIED.,.F.,.F.,.F.)
B_SPLINE_SURFACE_WITH_KNOTS((2,2),(3,3),(0.,0.289681084359915),(0.125066077454537,
0.142578551421364),.UNSPECIFIED.)
GEOMETRIC_REPRESENTATION_ITEM()
RATIONAL_B_SPLINE_SURFACE(((0.990621203777022,0.993706096834649,0.999805186472059),
(0.990621203777022,0.993706096834649,0.999805186472059)))
REPRESENTATION_ITEM('')
SURFACE()
);
#2925=(
BOUNDED_SURFACE()
B_SPLINE_SURFACE(1,2,((#144277,#144278,#144279),(#144280,#144281,#144282)),
 .UNSPECIFIED.,.F.,.F.,.F.)
B_SPLINE_SURFACE_WITH_KNOTS((2,2),(3,3),(0.,0.289807040991665),(0.590910950629593,
0.60808458519997),.UNSPECIFIED.)
GEOMETRIC_REPRESENTATION_ITEM()
RATIONAL_B_SPLINE_SURFACE(((0.990053454406147,0.987313720921968,0.987472672298934),
(0.990053454406147,0.987313720921968,0.987472672298934)))
REPRESENTATION_ITEM('')
SURFACE()
);
#2926=(
BOUNDED_SURFACE()
B_SPLINE_SURFACE(1,2,((#144284,#144285,#144286),(#144287,#144288,#144289)),
 .UNSPECIFIED.,.F.,.F.,.F.)
B_SPLINE_SURFACE_WITH_KNOTS((2,2),(3,3),(0.,0.289681084359919),(0.125066077454537,
0.142578551421365),.UNSPECIFIED.)
GEOMETRIC_REPRESENTATION_ITEM()
RATIONAL_B_SPLINE_SURFACE(((0.990621203777022,0.993706096834649,0.999805186472059),
(0.990621203777022,0.993706096834649,0.999805186472059)))
REPRESENTATION_ITEM('')
SURFACE()
);
#2927=(
BOUNDED_SURFACE()
B_SPLINE_SURFACE(1,2,((#144298,#144299,#144300),(#144301,#144302,#144303)),
 .UNSPECIFIED.,.F.,.F.,.F.)
B_SPLINE_SURFACE_WITH_KNOTS((2,2),(3,3),(0.,0.289807040992624),(0.590910950629593,
0.60808458519997),.UNSPECIFIED.)
GEOMETRIC_REPRESENTATION_ITEM()
RATIONAL_B_SPLINE_SURFACE(((0.990053454406147,0.987313720921968,0.987472672298934),
(0.990053454406147,0.987313720921968,0.987472672298934)))
REPRESENTATION_ITEM('')
SURFACE()
);
#2928=(
BOUNDED_SURFACE()
B_SPLINE_SURFACE(1,2,((#144305,#144306,#144307),(#144308,#144309,#144310)),
 .UNSPECIFIED.,.F.,.F.,.F.)
B_SPLINE_SURFACE_WITH_KNOTS((2,2),(3,3),(0.,0.289681084359914),(0.125066077454537,
0.142578551421365),.UNSPECIFIED.)
GEOMETRIC_REPRESENTATION_ITEM()
RATIONAL_B_SPLINE_SURFACE(((0.990621203777022,0.993706096834649,0.999805186472059),
(0.990621203777022,0.993706096834649,0.999805186472059)))
REPRESENTATION_ITEM('')
SURFACE()
);
#2929=(
BOUNDED_SURFACE()
B_SPLINE_SURFACE(1,2,((#144319,#144320,#144321),(#144322,#144323,#144324)),
 .UNSPECIFIED.,.F.,.F.,.F.)
B_SPLINE_SURFACE_WITH_KNOTS((2,2),(3,3),(0.,0.289807040992624),(0.590910950629593,
0.60808458519997),.UNSPECIFIED.)
GEOMETRIC_REPRESENTATION_ITEM()
RATIONAL_B_SPLINE_SURFACE(((0.990053454406147,0.987313720921968,0.987472672298934),
(0.990053454406147,0.987313720921968,0.987472672298934)))
REPRESENTATION_ITEM('')
SURFACE()
);
#2930=(
BOUNDED_SURFACE()
B_SPLINE_SURFACE(1,2,((#144326,#144327,#144328),(#144329,#144330,#144331)),
 .UNSPECIFIED.,.F.,.F.,.F.)
B_SPLINE_SURFACE_WITH_KNOTS((2,2),(3,3),(0.,0.289681084359924),(0.125066077454536,
0.142578551421364),.UNSPECIFIED.)
GEOMETRIC_REPRESENTATION_ITEM()
RATIONAL_B_SPLINE_SURFACE(((0.990621203777022,0.993706096834649,0.999805186472059),
(0.990621203777022,0.993706096834649,0.999805186472059)))
REPRESENTATION_ITEM('')
SURFACE()
);
#2931=(
BOUNDED_SURFACE()
B_SPLINE_SURFACE(1,2,((#144340,#144341,#144342),(#144343,#144344,#144345)),
 .UNSPECIFIED.,.F.,.F.,.F.)
B_SPLINE_SURFACE_WITH_KNOTS((2,2),(3,3),(0.,0.289807040992623),(0.590910950629593,
0.60808458519997),.UNSPECIFIED.)
GEOMETRIC_REPRESENTATION_ITEM()
RATIONAL_B_SPLINE_SURFACE(((0.990053454406147,0.987313720921968,0.987472672298934),
(0.990053454406147,0.987313720921968,0.987472672298934)))
REPRESENTATION_ITEM('')
SURFACE()
);
#2932=(
BOUNDED_SURFACE()
B_SPLINE_SURFACE(1,2,((#144347,#144348,#144349),(#144350,#144351,#144352)),
 .UNSPECIFIED.,.F.,.F.,.F.)
B_SPLINE_SURFACE_WITH_KNOTS((2,2),(3,3),(0.,0.289681084359918),(0.125066077454537,
0.142578551421364),.UNSPECIFIED.)
GEOMETRIC_REPRESENTATION_ITEM()
RATIONAL_B_SPLINE_SURFACE(((0.990621203777022,0.993706096834649,0.999805186472059),
(0.990621203777022,0.993706096834649,0.999805186472059)))
REPRESENTATION_ITEM('')
SURFACE()
);
#2933=(
BOUNDED_SURFACE()
B_SPLINE_SURFACE(1,2,((#144361,#144362,#144363),(#144364,#144365,#144366)),
 .UNSPECIFIED.,.F.,.F.,.F.)
B_SPLINE_SURFACE_WITH_KNOTS((2,2),(3,3),(0.,0.289807040993204),(0.590910950629594,
0.60808458519997),.UNSPECIFIED.)
GEOMETRIC_REPRESENTATION_ITEM()
RATIONAL_B_SPLINE_SURFACE(((0.990053454406147,0.987313720921968,0.987472672298934),
(0.990053454406147,0.987313720921968,0.987472672298934)))
REPRESENTATION_ITEM('')
SURFACE()
);
#2934=(
BOUNDED_SURFACE()
B_SPLINE_SURFACE(1,2,((#144368,#144369,#144370),(#144371,#144372,#144373)),
 .UNSPECIFIED.,.F.,.F.,.F.)
B_SPLINE_SURFACE_WITH_KNOTS((2,2),(3,3),(0.,0.28968108435992),(0.125066077454537,
0.142578551421364),.UNSPECIFIED.)
GEOMETRIC_REPRESENTATION_ITEM()
RATIONAL_B_SPLINE_SURFACE(((0.990621203777022,0.993706096834649,0.999805186472059),
(0.990621203777022,0.993706096834649,0.999805186472059)))
REPRESENTATION_ITEM('')
SURFACE()
);
#2935=(
BOUNDED_SURFACE()
B_SPLINE_SURFACE(1,2,((#144382,#144383,#144384),(#144385,#144386,#144387)),
 .UNSPECIFIED.,.F.,.F.,.F.)
B_SPLINE_SURFACE_WITH_KNOTS((2,2),(3,3),(0.,0.289807040992621),(0.590910950629593,
0.60808458519997),.UNSPECIFIED.)
GEOMETRIC_REPRESENTATION_ITEM()
RATIONAL_B_SPLINE_SURFACE(((0.990053454406147,0.987313720921968,0.987472672298933),
(0.990053454406147,0.987313720921968,0.987472672298933)))
REPRESENTATION_ITEM('')
SURFACE()
);
#2936=(
BOUNDED_SURFACE()
B_SPLINE_SURFACE(1,2,((#144389,#144390,#144391),(#144392,#144393,#144394)),
 .UNSPECIFIED.,.F.,.F.,.F.)
B_SPLINE_SURFACE_WITH_KNOTS((2,2),(3,3),(0.,0.289681084359924),(0.125066077454537,
0.142578551421365),.UNSPECIFIED.)
GEOMETRIC_REPRESENTATION_ITEM()
RATIONAL_B_SPLINE_SURFACE(((0.990621203777022,0.993706096834649,0.999805186472059),
(0.990621203777022,0.993706096834649,0.999805186472059)))
REPRESENTATION_ITEM('')
SURFACE()
);
#2937=(
BOUNDED_SURFACE()
B_SPLINE_SURFACE(1,2,((#144403,#144404,#144405),(#144406,#144407,#144408)),
 .UNSPECIFIED.,.F.,.F.,.F.)
B_SPLINE_SURFACE_WITH_KNOTS((2,2),(3,3),(0.,0.289807040993174),(0.590910950629593,
0.60808458519997),.UNSPECIFIED.)
GEOMETRIC_REPRESENTATION_ITEM()
RATIONAL_B_SPLINE_SURFACE(((0.990053454406147,0.987313720921968,0.987472672298934),
(0.990053454406147,0.987313720921968,0.987472672298934)))
REPRESENTATION_ITEM('')
SURFACE()
);
#2938=(
BOUNDED_SURFACE()
B_SPLINE_SURFACE(1,2,((#144410,#144411,#144412),(#144413,#144414,#144415)),
 .UNSPECIFIED.,.F.,.F.,.F.)
B_SPLINE_SURFACE_WITH_KNOTS((2,2),(3,3),(0.,0.289681084359917),(0.125066077454537,
0.142578551421364),.UNSPECIFIED.)
GEOMETRIC_REPRESENTATION_ITEM()
RATIONAL_B_SPLINE_SURFACE(((0.990621203777022,0.993706096834649,0.999805186472059),
(0.990621203777022,0.993706096834649,0.999805186472059)))
REPRESENTATION_ITEM('')
SURFACE()
);
#2939=(
BOUNDED_SURFACE()
B_SPLINE_SURFACE(1,2,((#144424,#144425,#144426),(#144427,#144428,#144429)),
 .UNSPECIFIED.,.F.,.F.,.F.)
B_SPLINE_SURFACE_WITH_KNOTS((2,2),(3,3),(0.,0.289807040992982),(0.590910950629594,
0.60808458519997),.UNSPECIFIED.)
GEOMETRIC_REPRESENTATION_ITEM()
RATIONAL_B_SPLINE_SURFACE(((0.990053454406147,0.987313720921968,0.987472672298933),
(0.990053454406147,0.987313720921968,0.987472672298933)))
REPRESENTATION_ITEM('')
SURFACE()
);
#2940=(
BOUNDED_SURFACE()
B_SPLINE_SURFACE(1,2,((#144431,#144432,#144433),(#144434,#144435,#144436)),
 .UNSPECIFIED.,.F.,.F.,.F.)
B_SPLINE_SURFACE_WITH_KNOTS((2,2),(3,3),(0.,0.289681084359923),(0.125066077454536,
0.142578551421363),.UNSPECIFIED.)
GEOMETRIC_REPRESENTATION_ITEM()
RATIONAL_B_SPLINE_SURFACE(((0.990621203777021,0.993706096834649,0.999805186472059),
(0.990621203777021,0.993706096834649,0.999805186472059)))
REPRESENTATION_ITEM('')
SURFACE()
);
#2941=(
BOUNDED_SURFACE()
B_SPLINE_SURFACE(1,2,((#144445,#144446,#144447),(#144448,#144449,#144450)),
 .UNSPECIFIED.,.F.,.F.,.F.)
B_SPLINE_SURFACE_WITH_KNOTS((2,2),(3,3),(0.,0.289807040993021),(0.590910950629594,
0.608084585199971),.UNSPECIFIED.)
GEOMETRIC_REPRESENTATION_ITEM()
RATIONAL_B_SPLINE_SURFACE(((0.990053454406147,0.987313720921968,0.987472672298934),
(0.990053454406147,0.987313720921968,0.987472672298934)))
REPRESENTATION_ITEM('')
SURFACE()
);
#2942=(
BOUNDED_SURFACE()
B_SPLINE_SURFACE(1,2,((#144452,#144453,#144454),(#144455,#144456,#144457)),
 .UNSPECIFIED.,.F.,.F.,.F.)
B_SPLINE_SURFACE_WITH_KNOTS((2,2),(3,3),(0.,0.289681084359917),(0.125066077454535,
0.142578551421363),.UNSPECIFIED.)
GEOMETRIC_REPRESENTATION_ITEM()
RATIONAL_B_SPLINE_SURFACE(((0.990621203777021,0.993706096834649,0.999805186472059),
(0.990621203777021,0.993706096834649,0.999805186472059)))
REPRESENTATION_ITEM('')
SURFACE()
);
#2943=(
BOUNDED_SURFACE()
B_SPLINE_SURFACE(1,2,((#144466,#144467,#144468),(#144469,#144470,#144471)),
 .UNSPECIFIED.,.F.,.F.,.F.)
B_SPLINE_SURFACE_WITH_KNOTS((2,2),(3,3),(0.,0.289807040993297),(0.590910950629594,
0.608084585199971),.UNSPECIFIED.)
GEOMETRIC_REPRESENTATION_ITEM()
RATIONAL_B_SPLINE_SURFACE(((0.990053454406147,0.987313720921968,0.987472672298934),
(0.990053454406147,0.987313720921968,0.987472672298934)))
REPRESENTATION_ITEM('')
SURFACE()
);
#2944=(
BOUNDED_SURFACE()
B_SPLINE_SURFACE(1,2,((#144473,#144474,#144475),(#144476,#144477,#144478)),
 .UNSPECIFIED.,.F.,.F.,.F.)
B_SPLINE_SURFACE_WITH_KNOTS((2,2),(3,3),(0.,0.289681084359922),(0.125066077454535,
0.142578551421363),.UNSPECIFIED.)
GEOMETRIC_REPRESENTATION_ITEM()
RATIONAL_B_SPLINE_SURFACE(((0.990621203777021,0.993706096834649,0.999805186472059),
(0.990621203777021,0.993706096834649,0.999805186472059)))
REPRESENTATION_ITEM('')
SURFACE()
);
#2945=(
BOUNDED_SURFACE()
B_SPLINE_SURFACE(1,2,((#144487,#144488,#144489),(#144490,#144491,#144492)),
 .UNSPECIFIED.,.F.,.F.,.F.)
B_SPLINE_SURFACE_WITH_KNOTS((2,2),(3,3),(0.,0.289807040992709),(0.590910950629594,
0.608084585199971),.UNSPECIFIED.)
GEOMETRIC_REPRESENTATION_ITEM()
RATIONAL_B_SPLINE_SURFACE(((0.990053454406147,0.987313720921968,0.987472672298934),
(0.990053454406147,0.987313720921968,0.987472672298934)))
REPRESENTATION_ITEM('')
SURFACE()
);
#2946=(
BOUNDED_SURFACE()
B_SPLINE_SURFACE(1,2,((#144494,#144495,#144496),(#144497,#144498,#144499)),
 .UNSPECIFIED.,.F.,.F.,.F.)
B_SPLINE_SURFACE_WITH_KNOTS((2,2),(3,3),(0.,0.289681084359921),(0.125066077454536,
0.142578551421363),.UNSPECIFIED.)
GEOMETRIC_REPRESENTATION_ITEM()
RATIONAL_B_SPLINE_SURFACE(((0.990621203777021,0.993706096834649,0.999805186472059),
(0.990621203777021,0.993706096834649,0.999805186472059)))
REPRESENTATION_ITEM('')
SURFACE()
);
#2947=(
BOUNDED_SURFACE()
B_SPLINE_SURFACE(1,2,((#144508,#144509,#144510),(#144511,#144512,#144513)),
 .UNSPECIFIED.,.F.,.F.,.F.)
B_SPLINE_SURFACE_WITH_KNOTS((2,2),(3,3),(0.,0.289807040993544),(0.590910950629594,
0.608084585199971),.UNSPECIFIED.)
GEOMETRIC_REPRESENTATION_ITEM()
RATIONAL_B_SPLINE_SURFACE(((0.990053454406147,0.987313720921967,0.987472672298934),
(0.990053454406147,0.987313720921967,0.987472672298934)))
REPRESENTATION_ITEM('')
SURFACE()
);
#2948=(
BOUNDED_SURFACE()
B_SPLINE_SURFACE(1,2,((#144515,#144516,#144517),(#144518,#144519,#144520)),
 .UNSPECIFIED.,.F.,.F.,.F.)
B_SPLINE_SURFACE_WITH_KNOTS((2,2),(3,3),(0.,0.289681084359919),(0.125066077454536,
0.142578551421363),.UNSPECIFIED.)
GEOMETRIC_REPRESENTATION_ITEM()
RATIONAL_B_SPLINE_SURFACE(((0.990621203777021,0.993706096834649,0.999805186472059),
(0.990621203777021,0.993706096834649,0.999805186472059)))
REPRESENTATION_ITEM('')
SURFACE()
);
#2949=(
BOUNDED_SURFACE()
B_SPLINE_SURFACE(1,2,((#144529,#144530,#144531),(#144532,#144533,#144534)),
 .UNSPECIFIED.,.F.,.F.,.F.)
B_SPLINE_SURFACE_WITH_KNOTS((2,2),(3,3),(0.,0.289807040993043),(0.590910950629594,
0.608084585199971),.UNSPECIFIED.)
GEOMETRIC_REPRESENTATION_ITEM()
RATIONAL_B_SPLINE_SURFACE(((0.990053454406147,0.987313720921967,0.987472672298933),
(0.990053454406147,0.987313720921967,0.987472672298933)))
REPRESENTATION_ITEM('')
SURFACE()
);
#2950=(
BOUNDED_SURFACE()
B_SPLINE_SURFACE(1,2,((#144536,#144537,#144538),(#144539,#144540,#144541)),
 .UNSPECIFIED.,.F.,.F.,.F.)
B_SPLINE_SURFACE_WITH_KNOTS((2,2),(3,3),(0.,0.289681084359923),(0.125066077454536,
0.142578551421363),.UNSPECIFIED.)
GEOMETRIC_REPRESENTATION_ITEM()
RATIONAL_B_SPLINE_SURFACE(((0.990621203777021,0.993706096834649,0.999805186472059),
(0.990621203777021,0.993706096834649,0.999805186472059)))
REPRESENTATION_ITEM('')
SURFACE()
);
#2951=(
BOUNDED_SURFACE()
B_SPLINE_SURFACE(1,2,((#144550,#144551,#144552),(#144553,#144554,#144555)),
 .UNSPECIFIED.,.F.,.F.,.F.)
B_SPLINE_SURFACE_WITH_KNOTS((2,2),(3,3),(0.,0.289807040993516),(0.590910950629594,
0.608084585199971),.UNSPECIFIED.)
GEOMETRIC_REPRESENTATION_ITEM()
RATIONAL_B_SPLINE_SURFACE(((0.990053454406147,0.987313720921967,0.987472672298933),
(0.990053454406147,0.987313720921967,0.987472672298933)))
REPRESENTATION_ITEM('')
SURFACE()
);
#2952=(
BOUNDED_SURFACE()
B_SPLINE_SURFACE(1,2,((#144557,#144558,#144559),(#144560,#144561,#144562)),
 .UNSPECIFIED.,.F.,.F.,.F.)
B_SPLINE_SURFACE_WITH_KNOTS((2,2),(3,3),(0.,0.289681084359921),(0.125066077454535,
0.142578551421364),.UNSPECIFIED.)
GEOMETRIC_REPRESENTATION_ITEM()
RATIONAL_B_SPLINE_SURFACE(((0.990621203777021,0.993706096834649,0.999805186472059),
(0.990621203777021,0.993706096834649,0.999805186472059)))
REPRESENTATION_ITEM('')
SURFACE()
);
#2953=(
BOUNDED_SURFACE()
B_SPLINE_SURFACE(1,2,((#144571,#144572,#144573),(#144574,#144575,#144576)),
 .UNSPECIFIED.,.F.,.F.,.F.)
B_SPLINE_SURFACE_WITH_KNOTS((2,2),(3,3),(0.,0.28980704099326),(0.590910950629594,
0.608084585199971),.UNSPECIFIED.)
GEOMETRIC_REPRESENTATION_ITEM()
RATIONAL_B_SPLINE_SURFACE(((0.990053454406147,0.987313720921968,0.987472672298934),
(0.990053454406147,0.987313720921968,0.987472672298934)))
REPRESENTATION_ITEM('')
SURFACE()
);
#2954=(
BOUNDED_SURFACE()
B_SPLINE_SURFACE(1,2,((#144578,#144579,#144580),(#144581,#144582,#144583)),
 .UNSPECIFIED.,.F.,.F.,.F.)
B_SPLINE_SURFACE_WITH_KNOTS((2,2),(3,3),(0.,0.28968108435992),(0.125066077454535,
0.142578551421363),.UNSPECIFIED.)
GEOMETRIC_REPRESENTATION_ITEM()
RATIONAL_B_SPLINE_SURFACE(((0.990621203777021,0.993706096834649,0.999805186472059),
(0.990621203777021,0.993706096834649,0.999805186472059)))
REPRESENTATION_ITEM('')
SURFACE()
);
#2955=(
BOUNDED_SURFACE()
B_SPLINE_SURFACE(1,2,((#144592,#144593,#144594),(#144595,#144596,#144597)),
 .UNSPECIFIED.,.F.,.F.,.F.)
B_SPLINE_SURFACE_WITH_KNOTS((2,2),(3,3),(0.,0.289807040994422),(0.590910950629595,
0.608084585199971),.UNSPECIFIED.)
GEOMETRIC_REPRESENTATION_ITEM()
RATIONAL_B_SPLINE_SURFACE(((0.990053454406147,0.987313720921968,0.987472672298934),
(0.990053454406147,0.987313720921968,0.987472672298934)))
REPRESENTATION_ITEM('')
SURFACE()
);
#2956=(
BOUNDED_SURFACE()
B_SPLINE_SURFACE(1,2,((#144599,#144600,#144601),(#144602,#144603,#144604)),
 .UNSPECIFIED.,.F.,.F.,.F.)
B_SPLINE_SURFACE_WITH_KNOTS((2,2),(3,3),(0.,0.289681084359924),(0.125066077454535,
0.142578551421363),.UNSPECIFIED.)
GEOMETRIC_REPRESENTATION_ITEM()
RATIONAL_B_SPLINE_SURFACE(((0.990621203777021,0.993706096834649,0.999805186472059),
(0.990621203777021,0.993706096834649,0.999805186472059)))
REPRESENTATION_ITEM('')
SURFACE()
);
#2957=(
BOUNDED_SURFACE()
B_SPLINE_SURFACE(1,2,((#144613,#144614,#144615),(#144616,#144617,#144618)),
 .UNSPECIFIED.,.F.,.F.,.F.)
B_SPLINE_SURFACE_WITH_KNOTS((2,2),(3,3),(0.,0.289807040992761),(0.590910950629594,
0.608084585199971),.UNSPECIFIED.)
GEOMETRIC_REPRESENTATION_ITEM()
RATIONAL_B_SPLINE_SURFACE(((0.990053454406147,0.987313720921967,0.987472672298933),
(0.990053454406147,0.987313720921967,0.987472672298933)))
REPRESENTATION_ITEM('')
SURFACE()
);
#2958=(
BOUNDED_SURFACE()
B_SPLINE_SURFACE(1,2,((#144620,#144621,#144622),(#144623,#144624,#144625)),
 .UNSPECIFIED.,.F.,.F.,.F.)
B_SPLINE_SURFACE_WITH_KNOTS((2,2),(3,3),(0.,0.289681084359926),(0.125066077454535,
0.142578551421363),.UNSPECIFIED.)
GEOMETRIC_REPRESENTATION_ITEM()
RATIONAL_B_SPLINE_SURFACE(((0.990621203777021,0.993706096834649,0.999805186472059),
(0.990621203777021,0.993706096834649,0.999805186472059)))
REPRESENTATION_ITEM('')
SURFACE()
);
#2959=(
BOUNDED_SURFACE()
B_SPLINE_SURFACE(1,2,((#144634,#144635,#144636),(#144637,#144638,#144639)),
 .UNSPECIFIED.,.F.,.F.,.F.)
B_SPLINE_SURFACE_WITH_KNOTS((2,2),(3,3),(0.,0.289807040992643),(0.590910950629594,
0.608084585199971),.UNSPECIFIED.)
GEOMETRIC_REPRESENTATION_ITEM()
RATIONAL_B_SPLINE_SURFACE(((0.990053454406147,0.987313720921968,0.987472672298934),
(0.990053454406147,0.987313720921967,0.987472672298933)))
REPRESENTATION_ITEM('')
SURFACE()
);
#2960=(
BOUNDED_SURFACE()
B_SPLINE_SURFACE(1,2,((#144641,#144642,#144643),(#144644,#144645,#144646)),
 .UNSPECIFIED.,.F.,.F.,.F.)
B_SPLINE_SURFACE_WITH_KNOTS((2,2),(3,3),(0.,0.28968108435992),(0.125066077454535,
0.142578551421364),.UNSPECIFIED.)
GEOMETRIC_REPRESENTATION_ITEM()
RATIONAL_B_SPLINE_SURFACE(((0.990621203777021,0.993706096834649,0.999805186472059),
(0.990621203777021,0.993706096834649,0.999805186472059)))
REPRESENTATION_ITEM('')
SURFACE()
);
#2961=(
BOUNDED_SURFACE()
B_SPLINE_SURFACE(1,2,((#144655,#144656,#144657),(#144658,#144659,#144660)),
 .UNSPECIFIED.,.F.,.F.,.F.)
B_SPLINE_SURFACE_WITH_KNOTS((2,2),(3,3),(0.,0.289807040993492),(0.590910950629594,
0.608084585199971),.UNSPECIFIED.)
GEOMETRIC_REPRESENTATION_ITEM()
RATIONAL_B_SPLINE_SURFACE(((0.990053454406147,0.987313720921968,0.987472672298934),
(0.990053454406147,0.987313720921968,0.987472672298934)))
REPRESENTATION_ITEM('')
SURFACE()
);
#2962=(
BOUNDED_SURFACE()
B_SPLINE_SURFACE(1,2,((#144662,#144663,#144664),(#144665,#144666,#144667)),
 .UNSPECIFIED.,.F.,.F.,.F.)
B_SPLINE_SURFACE_WITH_KNOTS((2,2),(3,3),(0.,0.28968108435993),(0.125066077454536,
0.142578551421364),.UNSPECIFIED.)
GEOMETRIC_REPRESENTATION_ITEM()
RATIONAL_B_SPLINE_SURFACE(((0.990621203777021,0.993706096834649,0.999805186472059),
(0.990621203777021,0.993706096834649,0.999805186472059)))
REPRESENTATION_ITEM('')
SURFACE()
);
#2963=(
BOUNDED_SURFACE()
B_SPLINE_SURFACE(1,2,((#144676,#144677,#144678),(#144679,#144680,#144681)),
 .UNSPECIFIED.,.F.,.F.,.F.)
B_SPLINE_SURFACE_WITH_KNOTS((2,2),(3,3),(0.,0.289807040992016),(0.590910950629594,
0.608084585199971),.UNSPECIFIED.)
GEOMETRIC_REPRESENTATION_ITEM()
RATIONAL_B_SPLINE_SURFACE(((0.990053454406147,0.987313720921968,0.987472672298934),
(0.990053454406147,0.987313720921968,0.987472672298934)))
REPRESENTATION_ITEM('')
SURFACE()
);
#2964=(
BOUNDED_SURFACE()
B_SPLINE_SURFACE(1,2,((#144683,#144684,#144685),(#144686,#144687,#144688)),
 .UNSPECIFIED.,.F.,.F.,.F.)
B_SPLINE_SURFACE_WITH_KNOTS((2,2),(3,3),(0.,0.289681084359924),(0.125066077454536,
0.142578551421363),.UNSPECIFIED.)
GEOMETRIC_REPRESENTATION_ITEM()
RATIONAL_B_SPLINE_SURFACE(((0.990621203777021,0.993706096834649,0.999805186472059),
(0.990621203777021,0.993706096834649,0.999805186472059)))
REPRESENTATION_ITEM('')
SURFACE()
);
#2965=(
BOUNDED_SURFACE()
B_SPLINE_SURFACE(1,2,((#144697,#144698,#144699),(#144700,#144701,#144702)),
 .UNSPECIFIED.,.F.,.F.,.F.)
B_SPLINE_SURFACE_WITH_KNOTS((2,2),(3,3),(0.,0.289807040992888),(0.590910950629594,
0.608084585199975),.UNSPECIFIED.)
GEOMETRIC_REPRESENTATION_ITEM()
RATIONAL_B_SPLINE_SURFACE(((0.990053454406147,0.987313720921967,0.987472672298934),
(0.990053454406147,0.987313720921967,0.987472672298934)))
REPRESENTATION_ITEM('')
SURFACE()
);
#2966=(
BOUNDED_SURFACE()
B_SPLINE_SURFACE(1,2,((#144704,#144705,#144706),(#144707,#144708,#144709)),
 .UNSPECIFIED.,.F.,.F.,.F.)
B_SPLINE_SURFACE_WITH_KNOTS((2,2),(3,3),(0.,0.289681084359926),(0.125066077454535,
0.142578551421364),.UNSPECIFIED.)
GEOMETRIC_REPRESENTATION_ITEM()
RATIONAL_B_SPLINE_SURFACE(((0.990621203777021,0.993706096834649,0.999805186472059),
(0.990621203777021,0.993706096834649,0.999805186472059)))
REPRESENTATION_ITEM('')
SURFACE()
);
#2967=(
BOUNDED_SURFACE()
B_SPLINE_SURFACE(1,2,((#144718,#144719,#144720),(#144721,#144722,#144723)),
 .UNSPECIFIED.,.F.,.F.,.F.)
B_SPLINE_SURFACE_WITH_KNOTS((2,2),(3,3),(0.,0.289807040992692),(0.590910950629594,
0.608084585199971),.UNSPECIFIED.)
GEOMETRIC_REPRESENTATION_ITEM()
RATIONAL_B_SPLINE_SURFACE(((0.990053454406147,0.987313720921968,0.987472672298934),
(0.990053454406147,0.987313720921967,0.987472672298933)))
REPRESENTATION_ITEM('')
SURFACE()
);
#2968=(
BOUNDED_SURFACE()
B_SPLINE_SURFACE(1,2,((#144725,#144726,#144727),(#144728,#144729,#144730)),
 .UNSPECIFIED.,.F.,.F.,.F.)
B_SPLINE_SURFACE_WITH_KNOTS((2,2),(3,3),(0.,0.289681084359928),(0.125066077454535,
0.142578551421363),.UNSPECIFIED.)
GEOMETRIC_REPRESENTATION_ITEM()
RATIONAL_B_SPLINE_SURFACE(((0.990621203777021,0.993706096834649,0.999805186472059),
(0.990621203777021,0.993706096834649,0.999805186472059)))
REPRESENTATION_ITEM('')
SURFACE()
);
#2969=(
BOUNDED_SURFACE()
B_SPLINE_SURFACE(1,2,((#144739,#144740,#144741),(#144742,#144743,#144744)),
 .UNSPECIFIED.,.F.,.F.,.F.)
B_SPLINE_SURFACE_WITH_KNOTS((2,2),(3,3),(0.,0.289807040993932),(0.590910950629594,
0.608084585199971),.UNSPECIFIED.)
GEOMETRIC_REPRESENTATION_ITEM()
RATIONAL_B_SPLINE_SURFACE(((0.990053454406147,0.987313720921968,0.987472672298934),
(0.990053454406147,0.987313720921968,0.987472672298934)))
REPRESENTATION_ITEM('')
SURFACE()
);
#2970=(
BOUNDED_SURFACE()
B_SPLINE_SURFACE(1,2,((#144746,#144747,#144748),(#144749,#144750,#144751)),
 .UNSPECIFIED.,.F.,.F.,.F.)
B_SPLINE_SURFACE_WITH_KNOTS((2,2),(3,3),(0.,0.289681084359915),(0.125066077454536,
0.142578551421431),.UNSPECIFIED.)
GEOMETRIC_REPRESENTATION_ITEM()
RATIONAL_B_SPLINE_SURFACE(((0.990621203777022,0.993706096834661,0.999805186472106),
(0.990621203777022,0.993706096834661,0.999805186472106)))
REPRESENTATION_ITEM('')
SURFACE()
);
#2971=(
BOUNDED_SURFACE()
B_SPLINE_SURFACE(1,2,((#144760,#144761,#144762),(#144763,#144764,#144765)),
 .UNSPECIFIED.,.F.,.F.,.F.)
B_SPLINE_SURFACE_WITH_KNOTS((2,2),(3,3),(0.,0.28980704099156),(0.590910950629593,
0.60808458519997),.UNSPECIFIED.)
GEOMETRIC_REPRESENTATION_ITEM()
RATIONAL_B_SPLINE_SURFACE(((0.990053454406147,0.987313720921968,0.987472672298934),
(0.990053454406147,0.987313720921968,0.987472672298934)))
REPRESENTATION_ITEM('')
SURFACE()
);
#2972=(
BOUNDED_SURFACE()
B_SPLINE_SURFACE(1,2,((#144767,#144768,#144769),(#144770,#144771,#144772)),
 .UNSPECIFIED.,.F.,.F.,.F.)
B_SPLINE_SURFACE_WITH_KNOTS((2,2),(3,3),(0.,0.289681084359916),(0.125066077454537,
0.142578551421365),.UNSPECIFIED.)
GEOMETRIC_REPRESENTATION_ITEM()
RATIONAL_B_SPLINE_SURFACE(((0.990621203777022,0.993706096834649,0.999805186472059),
(0.990621203777022,0.993706096834649,0.999805186472059)))
REPRESENTATION_ITEM('')
SURFACE()
);
#2973=(
BOUNDED_SURFACE()
B_SPLINE_SURFACE(1,2,((#144781,#144782,#144783),(#144784,#144785,#144786)),
 .UNSPECIFIED.,.F.,.F.,.F.)
B_SPLINE_SURFACE_WITH_KNOTS((2,2),(3,3),(0.,0.289807040991557),(0.590910950629593,
0.60808458519997),.UNSPECIFIED.)
GEOMETRIC_REPRESENTATION_ITEM()
RATIONAL_B_SPLINE_SURFACE(((0.990053454406147,0.987313720921968,0.987472672298933),
(0.990053454406147,0.987313720921968,0.987472672298933)))
REPRESENTATION_ITEM('')
SURFACE()
);
#2974=(
BOUNDED_SURFACE()
B_SPLINE_SURFACE(1,2,((#144788,#144789,#144790),(#144791,#144792,#144793)),
 .UNSPECIFIED.,.F.,.F.,.F.)
B_SPLINE_SURFACE_WITH_KNOTS((2,2),(3,3),(0.,0.289681084359917),(0.125066077454537,
0.142578551421365),.UNSPECIFIED.)
GEOMETRIC_REPRESENTATION_ITEM()
RATIONAL_B_SPLINE_SURFACE(((0.990621203777022,0.993706096834649,0.999805186472059),
(0.990621203777022,0.993706096834649,0.999805186472059)))
REPRESENTATION_ITEM('')
SURFACE()
);
#2975=(
BOUNDED_SURFACE()
B_SPLINE_SURFACE(1,2,((#144802,#144803,#144804),(#144805,#144806,#144807)),
 .UNSPECIFIED.,.F.,.F.,.F.)
B_SPLINE_SURFACE_WITH_KNOTS((2,2),(3,3),(0.,0.289807040991893),(0.590910950629593,
0.60808458519997),.UNSPECIFIED.)
GEOMETRIC_REPRESENTATION_ITEM()
RATIONAL_B_SPLINE_SURFACE(((0.990053454406147,0.987313720921968,0.987472672298934),
(0.990053454406147,0.987313720921968,0.987472672298934)))
REPRESENTATION_ITEM('')
SURFACE()
);
#2976=(
BOUNDED_SURFACE()
B_SPLINE_SURFACE(1,2,((#144809,#144810,#144811),(#144812,#144813,#144814)),
 .UNSPECIFIED.,.F.,.F.,.F.)
B_SPLINE_SURFACE_WITH_KNOTS((2,2),(3,3),(0.,0.289681084359919),(0.125066077454537,
0.142578551421364),.UNSPECIFIED.)
GEOMETRIC_REPRESENTATION_ITEM()
RATIONAL_B_SPLINE_SURFACE(((0.990621203777022,0.993706096834649,0.999805186472059),
(0.990621203777022,0.993706096834649,0.999805186472059)))
REPRESENTATION_ITEM('')
SURFACE()
);
#2977=(
BOUNDED_SURFACE()
B_SPLINE_SURFACE(1,2,((#144823,#144824,#144825),(#144826,#144827,#144828)),
 .UNSPECIFIED.,.F.,.F.,.F.)
B_SPLINE_SURFACE_WITH_KNOTS((2,2),(3,3),(0.,0.289807040992024),(0.590910950629593,
0.60808458519997),.UNSPECIFIED.)
GEOMETRIC_REPRESENTATION_ITEM()
RATIONAL_B_SPLINE_SURFACE(((0.990053454406147,0.987313720921968,0.987472672298933),
(0.990053454406147,0.987313720921968,0.987472672298933)))
REPRESENTATION_ITEM('')
SURFACE()
);
#2978=(
BOUNDED_SURFACE()
B_SPLINE_SURFACE(1,2,((#144830,#144831,#144832),(#144833,#144834,#144835)),
 .UNSPECIFIED.,.F.,.F.,.F.)
B_SPLINE_SURFACE_WITH_KNOTS((2,2),(3,3),(0.,0.28968108435992),(0.538896351358318,
0.556212823028861),.UNSPECIFIED.)
GEOMETRIC_REPRESENTATION_ITEM()
RATIONAL_B_SPLINE_SURFACE(((0.987563472532048,0.988105030697865,0.991593692313265),
(0.987563472532048,0.988105030697865,0.991593692313265)))
REPRESENTATION_ITEM('')
SURFACE()
);
#2979=(
BOUNDED_SURFACE()
B_SPLINE_SURFACE(1,2,((#144846,#144847,#144848),(#144849,#144850,#144851)),
 .UNSPECIFIED.,.F.,.F.,.F.)
B_SPLINE_SURFACE_WITH_KNOTS((2,2),(3,3),(0.,0.289807040991565),(0.176967058622922,
0.194235682574593),.UNSPECIFIED.)
GEOMETRIC_REPRESENTATION_ITEM()
RATIONAL_B_SPLINE_SURFACE(((0.98748925405691,0.987216959588932,0.989875504592249),
(0.98748925405691,0.987216959588932,0.989875504592249)))
REPRESENTATION_ITEM('')
SURFACE()
);
#2980=(
BOUNDED_SURFACE()
B_SPLINE_SURFACE(1,2,((#144868,#144869,#144870),(#144871,#144872,#144873)),
 .UNSPECIFIED.,.F.,.F.,.F.)
B_SPLINE_SURFACE_WITH_KNOTS((2,2),(3,3),(0.,0.289681084359927),(0.538896351358318,
0.556212823028864),.UNSPECIFIED.)
GEOMETRIC_REPRESENTATION_ITEM()
RATIONAL_B_SPLINE_SURFACE(((0.987563472532048,0.988105030697865,0.991593692313266),
(0.987563472532048,0.988105030697865,0.991593692313266)))
REPRESENTATION_ITEM('')
SURFACE()
);
#2981=(
BOUNDED_SURFACE()
B_SPLINE_SURFACE(1,2,((#144875,#144876,#144877),(#144878,#144879,#144880)),
 .UNSPECIFIED.,.F.,.F.,.F.)
B_SPLINE_SURFACE_WITH_KNOTS((2,2),(3,3),(0.,0.289807040991563),(0.176967058622922,
0.194235682574592),.UNSPECIFIED.)
GEOMETRIC_REPRESENTATION_ITEM()
RATIONAL_B_SPLINE_SURFACE(((0.98748925405691,0.987216959588932,0.989875504592249),
(0.98748925405691,0.987216959588932,0.989875504592249)))
REPRESENTATION_ITEM('')
SURFACE()
);
#2982=(
BOUNDED_SURFACE()
B_SPLINE_SURFACE(1,2,((#144897,#144898,#144899),(#144900,#144901,#144902)),
 .UNSPECIFIED.,.F.,.F.,.F.)
B_SPLINE_SURFACE_WITH_KNOTS((2,2),(3,3),(0.,0.289681084359915),(0.538896351358319,
0.556212823028862),.UNSPECIFIED.)
GEOMETRIC_REPRESENTATION_ITEM()
RATIONAL_B_SPLINE_SURFACE(((0.987563472532048,0.988105030697866,0.991593692313266),
(0.987563472532048,0.988105030697866,0.991593692313266)))
REPRESENTATION_ITEM('')
SURFACE()
);
#2983=(
BOUNDED_SURFACE()
B_SPLINE_SURFACE(1,2,((#144904,#144905,#144906),(#144907,#144908,#144909)),
 .UNSPECIFIED.,.F.,.F.,.F.)
B_SPLINE_SURFACE_WITH_KNOTS((2,2),(3,3),(0.,0.289807040991566),(0.176967058622921,
0.194235682574592),.UNSPECIFIED.)
GEOMETRIC_REPRESENTATION_ITEM()
RATIONAL_B_SPLINE_SURFACE(((0.98748925405691,0.987216959588932,0.989875504592249),
(0.98748925405691,0.987216959588932,0.989875504592249)))
REPRESENTATION_ITEM('')
SURFACE()
);
#2984=(
BOUNDED_SURFACE()
B_SPLINE_SURFACE(1,2,((#144926,#144927,#144928),(#144929,#144930,#144931)),
 .UNSPECIFIED.,.F.,.F.,.F.)
B_SPLINE_SURFACE_WITH_KNOTS((2,2),(3,3),(0.,0.289681084359933),(0.538896351358319,
0.556212823028862),.UNSPECIFIED.)
GEOMETRIC_REPRESENTATION_ITEM()
RATIONAL_B_SPLINE_SURFACE(((0.987563472532048,0.988105030697866,0.991593692313266),
(0.987563472532048,0.988105030697866,0.991593692313266)))
REPRESENTATION_ITEM('')
SURFACE()
);
#2985=(
BOUNDED_SURFACE()
B_SPLINE_SURFACE(1,2,((#144933,#144934,#144935),(#144936,#144937,#144938)),
 .UNSPECIFIED.,.F.,.F.,.F.)
B_SPLINE_SURFACE_WITH_KNOTS((2,2),(3,3),(0.,0.289807040991557),(0.176967058622921,
0.194235682574592),.UNSPECIFIED.)
GEOMETRIC_REPRESENTATION_ITEM()
RATIONAL_B_SPLINE_SURFACE(((0.98748925405691,0.987216959588932,0.989875504592249),
(0.98748925405691,0.987216959588932,0.989875504592249)))
REPRESENTATION_ITEM('')
SURFACE()
);
#2986=(
BOUNDED_SURFACE()
B_SPLINE_SURFACE(1,2,((#144955,#144956,#144957),(#144958,#144959,#144960)),
 .UNSPECIFIED.,.F.,.F.,.F.)
B_SPLINE_SURFACE_WITH_KNOTS((2,2),(3,3),(0.,0.289681084359922),(0.538896351358319,
0.556212823028865),.UNSPECIFIED.)
GEOMETRIC_REPRESENTATION_ITEM()
RATIONAL_B_SPLINE_SURFACE(((0.987563472532048,0.988105030697866,0.991593692313267),
(0.987563472532048,0.988105030697866,0.991593692313267)))
REPRESENTATION_ITEM('')
SURFACE()
);
#2987=(
BOUNDED_SURFACE()
B_SPLINE_SURFACE(1,2,((#144962,#144963,#144964),(#144965,#144966,#144967)),
 .UNSPECIFIED.,.F.,.F.,.F.)
B_SPLINE_SURFACE_WITH_KNOTS((2,2),(3,3),(0.,0.289807040991562),(0.176967058622921,
0.194235682574592),.UNSPECIFIED.)
GEOMETRIC_REPRESENTATION_ITEM()
RATIONAL_B_SPLINE_SURFACE(((0.98748925405691,0.987216959588932,0.989875504592249),
(0.98748925405691,0.987216959588932,0.989875504592249)))
REPRESENTATION_ITEM('')
SURFACE()
);
#2988=(
BOUNDED_SURFACE()
B_SPLINE_SURFACE(1,2,((#144984,#144985,#144986),(#144987,#144988,#144989)),
 .UNSPECIFIED.,.F.,.F.,.F.)
B_SPLINE_SURFACE_WITH_KNOTS((2,2),(3,3),(0.,0.289681084359927),(0.538896351358319,
0.556212823028865),.UNSPECIFIED.)
GEOMETRIC_REPRESENTATION_ITEM()
RATIONAL_B_SPLINE_SURFACE(((0.987563472532048,0.988105030697866,0.991593692313267),
(0.987563472532048,0.988105030697866,0.991593692313267)))
REPRESENTATION_ITEM('')
SURFACE()
);
#2989=(
BOUNDED_SURFACE()
B_SPLINE_SURFACE(1,2,((#144991,#144992,#144993),(#144994,#144995,#144996)),
 .UNSPECIFIED.,.F.,.F.,.F.)
B_SPLINE_SURFACE_WITH_KNOTS((2,2),(3,3),(0.,0.289807040991562),(0.176967058622921,
0.194235682574592),.UNSPECIFIED.)
GEOMETRIC_REPRESENTATION_ITEM()
RATIONAL_B_SPLINE_SURFACE(((0.98748925405691,0.987216959588931,0.989875504592249),
(0.98748925405691,0.987216959588932,0.989875504592249)))
REPRESENTATION_ITEM('')
SURFACE()
);
#2990=(
BOUNDED_SURFACE()
B_SPLINE_SURFACE(1,2,((#145013,#145014,#145015),(#145016,#145017,#145018)),
 .UNSPECIFIED.,.F.,.F.,.F.)
B_SPLINE_SURFACE_WITH_KNOTS((2,2),(3,3),(0.,0.289681084359927),(0.538896351358319,
0.556212823028862),.UNSPECIFIED.)
GEOMETRIC_REPRESENTATION_ITEM()
RATIONAL_B_SPLINE_SURFACE(((0.987563472532048,0.988105030697866,0.991593692313266),
(0.987563472532048,0.988105030697866,0.991593692313266)))
REPRESENTATION_ITEM('')
SURFACE()
);
#2991=(
BOUNDED_SURFACE()
B_SPLINE_SURFACE(1,2,((#145020,#145021,#145022),(#145023,#145024,#145025)),
 .UNSPECIFIED.,.F.,.F.,.F.)
B_SPLINE_SURFACE_WITH_KNOTS((2,2),(3,3),(0.,0.289807040991558),(0.176967058622921,
0.194235682574592),.UNSPECIFIED.)
GEOMETRIC_REPRESENTATION_ITEM()
RATIONAL_B_SPLINE_SURFACE(((0.98748925405691,0.987216959588932,0.989875504592249),
(0.98748925405691,0.987216959588931,0.989875504592248)))
REPRESENTATION_ITEM('')
SURFACE()
);
#2992=(
BOUNDED_SURFACE()
B_SPLINE_SURFACE(1,2,((#145033,#145034,#145035),(#145036,#145037,#145038)),
 .UNSPECIFIED.,.F.,.F.,.F.)
B_SPLINE_SURFACE_WITH_KNOTS((2,2),(3,3),(0.,0.289681084359916),(0.538896351358319,
0.556212823028865),.UNSPECIFIED.)
GEOMETRIC_REPRESENTATION_ITEM()
RATIONAL_B_SPLINE_SURFACE(((0.987563472532048,0.988105030697866,0.991593692313267),
(0.987563472532048,0.988105030697866,0.991593692313267)))
REPRESENTATION_ITEM('')
SURFACE()
);
#2993=(
BOUNDED_SURFACE()
B_SPLINE_SURFACE(1,2,((#145040,#145041,#145042),(#145043,#145044,#145045)),
 .UNSPECIFIED.,.F.,.F.,.F.)
B_SPLINE_SURFACE_WITH_KNOTS((2,2),(3,3),(0.,0.289807040991561),(0.176967058622921,
0.194235682574592),.UNSPECIFIED.)
GEOMETRIC_REPRESENTATION_ITEM()
RATIONAL_B_SPLINE_SURFACE(((0.98748925405691,0.987216959588931,0.989875504592248),
(0.98748925405691,0.987216959588931,0.989875504592248)))
REPRESENTATION_ITEM('')
SURFACE()
);
#2994=(
BOUNDED_SURFACE()
B_SPLINE_SURFACE(1,2,((#145062,#145063,#145064),(#145065,#145066,#145067)),
 .UNSPECIFIED.,.F.,.F.,.F.)
B_SPLINE_SURFACE_WITH_KNOTS((2,2),(3,3),(0.,0.289681084359916),(0.538896351358319,
0.556212823028865),.UNSPECIFIED.)
GEOMETRIC_REPRESENTATION_ITEM()
RATIONAL_B_SPLINE_SURFACE(((0.987563472532048,0.988105030697866,0.991593692313267),
(0.987563472532048,0.988105030697866,0.991593692313267)))
REPRESENTATION_ITEM('')
SURFACE()
);
#2995=(
BOUNDED_SURFACE()
B_SPLINE_SURFACE(1,2,((#145069,#145070,#145071),(#145072,#145073,#145074)),
 .UNSPECIFIED.,.F.,.F.,.F.)
B_SPLINE_SURFACE_WITH_KNOTS((2,2),(3,3),(0.,0.289807040991563),(0.176967058622921,
0.194235682574592),.UNSPECIFIED.)
GEOMETRIC_REPRESENTATION_ITEM()
RATIONAL_B_SPLINE_SURFACE(((0.98748925405691,0.987216959588931,0.989875504592249),
(0.98748925405691,0.987216959588931,0.989875504592249)))
REPRESENTATION_ITEM('')
SURFACE()
);
#2996=(
BOUNDED_SURFACE()
B_SPLINE_SURFACE(1,2,((#145091,#145092,#145093),(#145094,#145095,#145096)),
 .UNSPECIFIED.,.F.,.F.,.F.)
B_SPLINE_SURFACE_WITH_KNOTS((2,2),(3,3),(0.,0.289681084359914),(0.538896351358319,
0.556212823028865),.UNSPECIFIED.)
GEOMETRIC_REPRESENTATION_ITEM()
RATIONAL_B_SPLINE_SURFACE(((0.987563472532048,0.988105030697866,0.991593692313267),
(0.987563472532048,0.988105030697866,0.991593692313267)))
REPRESENTATION_ITEM('')
SURFACE()
);
#2997=(
BOUNDED_SURFACE()
B_SPLINE_SURFACE(1,2,((#145098,#145099,#145100),(#145101,#145102,#145103)),
 .UNSPECIFIED.,.F.,.F.,.F.)
B_SPLINE_SURFACE_WITH_KNOTS((2,2),(3,3),(0.,0.289807040991564),(0.176967058622921,
0.194235682574592),.UNSPECIFIED.)
GEOMETRIC_REPRESENTATION_ITEM()
RATIONAL_B_SPLINE_SURFACE(((0.98748925405691,0.987216959588931,0.989875504592249),
(0.98748925405691,0.987216959588931,0.989875504592249)))
REPRESENTATION_ITEM('')
SURFACE()
);
#2998=(
BOUNDED_SURFACE()
B_SPLINE_SURFACE(1,2,((#145120,#145121,#145122),(#145123,#145124,#145125)),
 .UNSPECIFIED.,.F.,.F.,.F.)
B_SPLINE_SURFACE_WITH_KNOTS((2,2),(3,3),(0.,0.289681084359916),(0.538896351358319,
0.556212823028865),.UNSPECIFIED.)
GEOMETRIC_REPRESENTATION_ITEM()
RATIONAL_B_SPLINE_SURFACE(((0.987563472532048,0.988105030697866,0.991593692313267),
(0.987563472532048,0.988105030697866,0.991593692313267)))
REPRESENTATION_ITEM('')
SURFACE()
);
#2999=(
BOUNDED_SURFACE()
B_SPLINE_SURFACE(1,2,((#145127,#145128,#145129),(#145130,#145131,#145132)),
 .UNSPECIFIED.,.F.,.F.,.F.)
B_SPLINE_SURFACE_WITH_KNOTS((2,2),(3,3),(0.,0.289807040991562),(0.176967058622921,
0.194235682574592),.UNSPECIFIED.)
GEOMETRIC_REPRESENTATION_ITEM()
RATIONAL_B_SPLINE_SURFACE(((0.98748925405691,0.987216959588931,0.989875504592249),
(0.98748925405691,0.987216959588931,0.989875504592249)))
REPRESENTATION_ITEM('')
SURFACE()
);
#3000=(
BOUNDED_SURFACE()
B_SPLINE_SURFACE(1,2,((#145149,#145150,#145151),(#145152,#145153,#145154)),
 .UNSPECIFIED.,.F.,.F.,.F.)
B_SPLINE_SURFACE_WITH_KNOTS((2,2),(3,3),(0.,0.289681084359921),(0.538896351358319,
0.556212823028865),.UNSPECIFIED.)
GEOMETRIC_REPRESENTATION_ITEM()
RATIONAL_B_SPLINE_SURFACE(((0.987563472532048,0.988105030697866,0.991593692313267),
(0.987563472532048,0.988105030697866,0.991593692313267)))
REPRESENTATION_ITEM('')
SURFACE()
);
#3001=(
BOUNDED_SURFACE()
B_SPLINE_SURFACE(1,2,((#145156,#145157,#145158),(#145159,#145160,#145161)),
 .UNSPECIFIED.,.F.,.F.,.F.)
B_SPLINE_SURFACE_WITH_KNOTS((2,2),(3,3),(0.,0.289807040991563),(0.176967058622921,
0.194235682574592),.UNSPECIFIED.)
GEOMETRIC_REPRESENTATION_ITEM()
RATIONAL_B_SPLINE_SURFACE(((0.98748925405691,0.987216959588931,0.989875504592249),
(0.98748925405691,0.987216959588931,0.989875504592249)))
REPRESENTATION_ITEM('')
SURFACE()
);
#3002=(
BOUNDED_SURFACE()
B_SPLINE_SURFACE(1,2,((#145178,#145179,#145180),(#145181,#145182,#145183)),
 .UNSPECIFIED.,.F.,.F.,.F.)
B_SPLINE_SURFACE_WITH_KNOTS((2,2),(3,3),(0.,0.289681084359926),(0.538896351358319,
0.556212823028862),.UNSPECIFIED.)
GEOMETRIC_REPRESENTATION_ITEM()
RATIONAL_B_SPLINE_SURFACE(((0.987563472532048,0.988105030697866,0.991593692313266),
(0.987563472532048,0.988105030697866,0.991593692313266)))
REPRESENTATION_ITEM('')
SURFACE()
);
#3003=(
BOUNDED_SURFACE()
B_SPLINE_SURFACE(1,2,((#145185,#145186,#145187),(#145188,#145189,#145190)),
 .UNSPECIFIED.,.F.,.F.,.F.)
B_SPLINE_SURFACE_WITH_KNOTS((2,2),(3,3),(0.,0.289807040991567),(0.176967058622921,
0.194235682574592),.UNSPECIFIED.)
GEOMETRIC_REPRESENTATION_ITEM()
RATIONAL_B_SPLINE_SURFACE(((0.98748925405691,0.987216959588931,0.989875504592249),
(0.98748925405691,0.987216959588931,0.989875504592249)))
REPRESENTATION_ITEM('')
SURFACE()
);
#3004=(
BOUNDED_SURFACE()
B_SPLINE_SURFACE(1,2,((#145207,#145208,#145209),(#145210,#145211,#145212)),
 .UNSPECIFIED.,.F.,.F.,.F.)
B_SPLINE_SURFACE_WITH_KNOTS((2,2),(3,3),(0.,0.289681084359921),(0.538896351358319,
0.556212823028862),.UNSPECIFIED.)
GEOMETRIC_REPRESENTATION_ITEM()
RATIONAL_B_SPLINE_SURFACE(((0.987563472532048,0.988105030697866,0.991593692313266),
(0.987563472532048,0.988105030697866,0.991593692313266)))
REPRESENTATION_ITEM('')
SURFACE()
);
#3005=(
BOUNDED_SURFACE()
B_SPLINE_SURFACE(1,2,((#145214,#145215,#145216),(#145217,#145218,#145219)),
 .UNSPECIFIED.,.F.,.F.,.F.)
B_SPLINE_SURFACE_WITH_KNOTS((2,2),(3,3),(0.,0.289807040991564),(0.176967058622921,
0.194235682574592),.UNSPECIFIED.)
GEOMETRIC_REPRESENTATION_ITEM()
RATIONAL_B_SPLINE_SURFACE(((0.98748925405691,0.987216959588932,0.989875504592249),
(0.98748925405691,0.987216959588932,0.989875504592249)))
REPRESENTATION_ITEM('')
SURFACE()
);
#3006=(
BOUNDED_SURFACE()
B_SPLINE_SURFACE(1,2,((#145236,#145237,#145238),(#145239,#145240,#145241)),
 .UNSPECIFIED.,.F.,.F.,.F.)
B_SPLINE_SURFACE_WITH_KNOTS((2,2),(3,3),(0.,0.28968108435992),(0.538896351358319,
0.556212823028865),.UNSPECIFIED.)
GEOMETRIC_REPRESENTATION_ITEM()
RATIONAL_B_SPLINE_SURFACE(((0.987563472532048,0.988105030697866,0.991593692313267),
(0.987563472532048,0.988105030697866,0.991593692313267)))
REPRESENTATION_ITEM('')
SURFACE()
);
#3007=(
BOUNDED_SURFACE()
B_SPLINE_SURFACE(1,2,((#145243,#145244,#145245),(#145246,#145247,#145248)),
 .UNSPECIFIED.,.F.,.F.,.F.)
B_SPLINE_SURFACE_WITH_KNOTS((2,2),(3,3),(0.,0.289807040991561),(0.176967058622921,
0.194235682574592),.UNSPECIFIED.)
GEOMETRIC_REPRESENTATION_ITEM()
RATIONAL_B_SPLINE_SURFACE(((0.98748925405691,0.987216959588932,0.989875504592249),
(0.98748925405691,0.987216959588932,0.989875504592249)))
REPRESENTATION_ITEM('')
SURFACE()
);
#3008=(
BOUNDED_SURFACE()
B_SPLINE_SURFACE(1,2,((#145265,#145266,#145267),(#145268,#145269,#145270)),
 .UNSPECIFIED.,.F.,.F.,.F.)
B_SPLINE_SURFACE_WITH_KNOTS((2,2),(3,3),(0.,0.289681084359919),(0.538896351358319,
0.556212823028862),.UNSPECIFIED.)
GEOMETRIC_REPRESENTATION_ITEM()
RATIONAL_B_SPLINE_SURFACE(((0.987563472532048,0.988105030697866,0.991593692313266),
(0.987563472532048,0.988105030697866,0.991593692313266)))
REPRESENTATION_ITEM('')
SURFACE()
);
#3009=(
BOUNDED_SURFACE()
B_SPLINE_SURFACE(1,2,((#145272,#145273,#145274),(#145275,#145276,#145277)),
 .UNSPECIFIED.,.F.,.F.,.F.)
B_SPLINE_SURFACE_WITH_KNOTS((2,2),(3,3),(0.,0.289807040991558),(0.176967058622921,
0.194235682574592),.UNSPECIFIED.)
GEOMETRIC_REPRESENTATION_ITEM()
RATIONAL_B_SPLINE_SURFACE(((0.98748925405691,0.987216959588931,0.989875504592249),
(0.98748925405691,0.987216959588931,0.989875504592249)))
REPRESENTATION_ITEM('')
SURFACE()
);
#3010=(
BOUNDED_SURFACE()
B_SPLINE_SURFACE(1,2,((#145294,#145295,#145296),(#145297,#145298,#145299)),
 .UNSPECIFIED.,.F.,.F.,.F.)
B_SPLINE_SURFACE_WITH_KNOTS((2,2),(3,3),(0.,0.289681084359921),(0.538896351358319,
0.556212823028865),.UNSPECIFIED.)
GEOMETRIC_REPRESENTATION_ITEM()
RATIONAL_B_SPLINE_SURFACE(((0.987563472532048,0.988105030697866,0.991593692313267),
(0.987563472532048,0.988105030697866,0.991593692313267)))
REPRESENTATION_ITEM('')
SURFACE()
);
#3011=(
BOUNDED_SURFACE()
B_SPLINE_SURFACE(1,2,((#145301,#145302,#145303),(#145304,#145305,#145306)),
 .UNSPECIFIED.,.F.,.F.,.F.)
B_SPLINE_SURFACE_WITH_KNOTS((2,2),(3,3),(0.,0.289807040991562),(0.176967058622921,
0.194235682574592),.UNSPECIFIED.)
GEOMETRIC_REPRESENTATION_ITEM()
RATIONAL_B_SPLINE_SURFACE(((0.98748925405691,0.987216959588931,0.989875504592249),
(0.98748925405691,0.987216959588931,0.989875504592249)))
REPRESENTATION_ITEM('')
SURFACE()
);
#3012=(
BOUNDED_SURFACE()
B_SPLINE_SURFACE(1,2,((#145323,#145324,#145325),(#145326,#145327,#145328)),
 .UNSPECIFIED.,.F.,.F.,.F.)
B_SPLINE_SURFACE_WITH_KNOTS((2,2),(3,3),(0.,0.28968108435992),(0.538896351358319,
0.556212823028865),.UNSPECIFIED.)
GEOMETRIC_REPRESENTATION_ITEM()
RATIONAL_B_SPLINE_SURFACE(((0.987563472532048,0.988105030697866,0.991593692313267),
(0.987563472532048,0.988105030697866,0.991593692313267)))
REPRESENTATION_ITEM('')
SURFACE()
);
#3013=(
BOUNDED_SURFACE()
B_SPLINE_SURFACE(1,2,((#145330,#145331,#145332),(#145333,#145334,#145335)),
 .UNSPECIFIED.,.F.,.F.,.F.)
B_SPLINE_SURFACE_WITH_KNOTS((2,2),(3,3),(0.,0.289807040991561),(0.176967058622921,
0.194235682574592),.UNSPECIFIED.)
GEOMETRIC_REPRESENTATION_ITEM()
RATIONAL_B_SPLINE_SURFACE(((0.98748925405691,0.987216959588931,0.989875504592249),
(0.98748925405691,0.987216959588931,0.989875504592249)))
REPRESENTATION_ITEM('')
SURFACE()
);
#3014=(
BOUNDED_SURFACE()
B_SPLINE_SURFACE(1,2,((#145352,#145353,#145354),(#145355,#145356,#145357)),
 .UNSPECIFIED.,.F.,.F.,.F.)
B_SPLINE_SURFACE_WITH_KNOTS((2,2),(3,3),(0.,0.289681084359922),(0.538896351358319,
0.556212823028865),.UNSPECIFIED.)
GEOMETRIC_REPRESENTATION_ITEM()
RATIONAL_B_SPLINE_SURFACE(((0.987563472532048,0.988105030697866,0.991593692313267),
(0.987563472532048,0.988105030697866,0.991593692313267)))
REPRESENTATION_ITEM('')
SURFACE()
);
#3015=(
BOUNDED_SURFACE()
B_SPLINE_SURFACE(1,2,((#145359,#145360,#145361),(#145362,#145363,#145364)),
 .UNSPECIFIED.,.F.,.F.,.F.)
B_SPLINE_SURFACE_WITH_KNOTS((2,2),(3,3),(0.,0.289807040991556),(0.176967058622921,
0.194235682574592),.UNSPECIFIED.)
GEOMETRIC_REPRESENTATION_ITEM()
RATIONAL_B_SPLINE_SURFACE(((0.98748925405691,0.987216959588931,0.989875504592249),
(0.98748925405691,0.987216959588931,0.989875504592249)))
REPRESENTATION_ITEM('')
SURFACE()
);
#3016=(
BOUNDED_SURFACE()
B_SPLINE_SURFACE(1,2,((#145375,#145376,#145377),(#145378,#145379,#145380)),
 .UNSPECIFIED.,.F.,.F.,.F.)
B_SPLINE_SURFACE_WITH_KNOTS((2,2),(3,3),(0.,0.289681084359922),(0.538896351358319,
0.556212823028862),.UNSPECIFIED.)
GEOMETRIC_REPRESENTATION_ITEM()
RATIONAL_B_SPLINE_SURFACE(((0.987563472532048,0.988105030697866,0.991593692313266),
(0.987563472532048,0.988105030697866,0.991593692313266)))
REPRESENTATION_ITEM('')
SURFACE()
);
#3017=(
BOUNDED_SURFACE()
B_SPLINE_SURFACE(1,2,((#145388,#145389,#145390),(#145391,#145392,#145393)),
 .UNSPECIFIED.,.F.,.F.,.F.)
B_SPLINE_SURFACE_WITH_KNOTS((2,2),(3,3),(0.,0.289807040991561),(0.176967058622921,
0.194235682574592),.UNSPECIFIED.)
GEOMETRIC_REPRESENTATION_ITEM()
RATIONAL_B_SPLINE_SURFACE(((0.98748925405691,0.987216959588932,0.989875504592249),
(0.98748925405691,0.987216959588932,0.989875504592249)))
REPRESENTATION_ITEM('')
SURFACE()
);
#3018=(
BOUNDED_SURFACE()
B_SPLINE_SURFACE(1,2,((#145410,#145411,#145412),(#145413,#145414,#145415)),
 .UNSPECIFIED.,.F.,.F.,.F.)
B_SPLINE_SURFACE_WITH_KNOTS((2,2),(3,3),(0.,0.289681084359924),(0.538896351358319,
0.556212823028861),.UNSPECIFIED.)
GEOMETRIC_REPRESENTATION_ITEM()
RATIONAL_B_SPLINE_SURFACE(((0.987563472532048,0.988105030697866,0.991593692313265),
(0.987563472532048,0.988105030697866,0.991593692313265)))
REPRESENTATION_ITEM('')
SURFACE()
);
#3019=(
BOUNDED_SURFACE()
B_SPLINE_SURFACE(1,2,((#145417,#145418,#145419),(#145420,#145421,#145422)),
 .UNSPECIFIED.,.F.,.F.,.F.)
B_SPLINE_SURFACE_WITH_KNOTS((2,2),(3,3),(0.,0.2898070409917),(0.176967058622922,
0.194235682574593),.UNSPECIFIED.)
GEOMETRIC_REPRESENTATION_ITEM()
RATIONAL_B_SPLINE_SURFACE(((0.98748925405691,0.987216959588932,0.989875504592249),
(0.98748925405691,0.987216959588932,0.989875504592249)))
REPRESENTATION_ITEM('')
SURFACE()
);
#3020=(
BOUNDED_SURFACE()
B_SPLINE_SURFACE(1,2,((#145439,#145440,#145441),(#145442,#145443,#145444)),
 .UNSPECIFIED.,.F.,.F.,.F.)
B_SPLINE_SURFACE_WITH_KNOTS((2,2),(3,3),(0.,0.289681084359922),(0.538896351358318,
0.556212823028861),.UNSPECIFIED.)
GEOMETRIC_REPRESENTATION_ITEM()
RATIONAL_B_SPLINE_SURFACE(((0.987563472532048,0.988105030697865,0.991593692313265),
(0.987563472532048,0.988105030697865,0.991593692313265)))
REPRESENTATION_ITEM('')
SURFACE()
);
#3021=(
BOUNDED_SURFACE()
B_SPLINE_SURFACE(1,2,((#145446,#145447,#145448),(#145449,#145450,#145451)),
 .UNSPECIFIED.,.F.,.F.,.F.)
B_SPLINE_SURFACE_WITH_KNOTS((2,2),(3,3),(0.,0.289807040991948),(0.176967058622922,
0.194235682574593),.UNSPECIFIED.)
GEOMETRIC_REPRESENTATION_ITEM()
RATIONAL_B_SPLINE_SURFACE(((0.98748925405691,0.987216959588932,0.989875504592249),
(0.98748925405691,0.987216959588932,0.989875504592249)))
REPRESENTATION_ITEM('')
SURFACE()
);
#3022=(
BOUNDED_SURFACE()
B_SPLINE_SURFACE(1,2,((#145468,#145469,#145470),(#145471,#145472,#145473)),
 .UNSPECIFIED.,.F.,.F.,.F.)
B_SPLINE_SURFACE_WITH_KNOTS((2,2),(3,3),(0.,0.289681084359918),(0.538896351358318,
0.556212823028864),.UNSPECIFIED.)
GEOMETRIC_REPRESENTATION_ITEM()
RATIONAL_B_SPLINE_SURFACE(((0.987563472532048,0.988105030697865,0.991593692313266),
(0.987563472532048,0.988105030697865,0.991593692313266)))
REPRESENTATION_ITEM('')
SURFACE()
);
#3023=(
BOUNDED_SURFACE()
B_SPLINE_SURFACE(1,2,((#145475,#145476,#145477),(#145478,#145479,#145480)),
 .UNSPECIFIED.,.F.,.F.,.F.)
B_SPLINE_SURFACE_WITH_KNOTS((2,2),(3,3),(0.,0.289807040993356),(0.176967058622922,
0.194235682574593),.UNSPECIFIED.)
GEOMETRIC_REPRESENTATION_ITEM()
RATIONAL_B_SPLINE_SURFACE(((0.98748925405691,0.987216959588932,0.989875504592249),
(0.98748925405691,0.987216959588932,0.989875504592249)))
REPRESENTATION_ITEM('')
SURFACE()
);
#3024=(
BOUNDED_SURFACE()
B_SPLINE_SURFACE(1,2,((#145497,#145498,#145499),(#145500,#145501,#145502)),
 .UNSPECIFIED.,.F.,.F.,.F.)
B_SPLINE_SURFACE_WITH_KNOTS((2,2),(3,3),(0.,0.289681084360124),(0.538896351358318,
0.556212823028861),.UNSPECIFIED.)
GEOMETRIC_REPRESENTATION_ITEM()
RATIONAL_B_SPLINE_SURFACE(((0.987563472532048,0.988105030697865,0.991593692313265),
(0.987563472532048,0.988105030697865,0.991593692313265)))
REPRESENTATION_ITEM('')
SURFACE()
);
#3025=(
BOUNDED_SURFACE()
B_SPLINE_SURFACE(1,2,((#145504,#145505,#145506),(#145507,#145508,#145509)),
 .UNSPECIFIED.,.F.,.F.,.F.)
B_SPLINE_SURFACE_WITH_KNOTS((2,2),(3,3),(0.,0.289807040992024),(0.176967058622922,
0.194235682574593),.UNSPECIFIED.)
GEOMETRIC_REPRESENTATION_ITEM()
RATIONAL_B_SPLINE_SURFACE(((0.98748925405691,0.987216959588932,0.989875504592249),
(0.98748925405691,0.987216959588932,0.989875504592249)))
REPRESENTATION_ITEM('')
SURFACE()
);
#3026=(
BOUNDED_SURFACE()
B_SPLINE_SURFACE(1,2,((#145526,#145527,#145528),(#145529,#145530,#145531)),
 .UNSPECIFIED.,.F.,.F.,.F.)
B_SPLINE_SURFACE_WITH_KNOTS((2,2),(3,3),(0.,0.289681084359929),(0.538896351358318,
0.556212823028861),.UNSPECIFIED.)
GEOMETRIC_REPRESENTATION_ITEM()
RATIONAL_B_SPLINE_SURFACE(((0.987563472532048,0.988105030697865,0.991593692313265),
(0.987563472532048,0.988105030697865,0.991593692313265)))
REPRESENTATION_ITEM('')
SURFACE()
);
#3027=(
BOUNDED_SURFACE()
B_SPLINE_SURFACE(1,2,((#145533,#145534,#145535),(#145536,#145537,#145538)),
 .UNSPECIFIED.,.F.,.F.,.F.)
B_SPLINE_SURFACE_WITH_KNOTS((2,2),(3,3),(0.,0.289807040991646),(0.176967058622922,
0.194235682574593),.UNSPECIFIED.)
GEOMETRIC_REPRESENTATION_ITEM()
RATIONAL_B_SPLINE_SURFACE(((0.98748925405691,0.987216959588932,0.989875504592249),
(0.98748925405691,0.987216959588932,0.989875504592249)))
REPRESENTATION_ITEM('')
SURFACE()
);
#3028=(
BOUNDED_SURFACE()
B_SPLINE_SURFACE(1,2,((#145555,#145556,#145557),(#145558,#145559,#145560)),
 .UNSPECIFIED.,.F.,.F.,.F.)
B_SPLINE_SURFACE_WITH_KNOTS((2,2),(3,3),(0.,0.289681084359921),(0.538896351358318,
0.556212823028864),.UNSPECIFIED.)
GEOMETRIC_REPRESENTATION_ITEM()
RATIONAL_B_SPLINE_SURFACE(((0.987563472532048,0.988105030697865,0.991593692313266),
(0.987563472532048,0.988105030697865,0.991593692313266)))
REPRESENTATION_ITEM('')
SURFACE()
);
#3029=(
BOUNDED_SURFACE()
B_SPLINE_SURFACE(1,2,((#145562,#145563,#145564),(#145565,#145566,#145567)),
 .UNSPECIFIED.,.F.,.F.,.F.)
B_SPLINE_SURFACE_WITH_KNOTS((2,2),(3,3),(0.,0.289807040991639),(0.176967058622922,
0.194235682574593),.UNSPECIFIED.)
GEOMETRIC_REPRESENTATION_ITEM()
RATIONAL_B_SPLINE_SURFACE(((0.98748925405691,0.987216959588932,0.989875504592249),
(0.98748925405691,0.987216959588932,0.989875504592249)))
REPRESENTATION_ITEM('')
SURFACE()
);
#3030=(
BOUNDED_SURFACE()
B_SPLINE_SURFACE(1,2,((#145584,#145585,#145586),(#145587,#145588,#145589)),
 .UNSPECIFIED.,.F.,.F.,.F.)
B_SPLINE_SURFACE_WITH_KNOTS((2,2),(3,3),(0.,0.289681084359917),(0.538896351358318,
0.556212823028861),.UNSPECIFIED.)
GEOMETRIC_REPRESENTATION_ITEM()
RATIONAL_B_SPLINE_SURFACE(((0.987563472532048,0.988105030697865,0.991593692313265),
(0.987563472532048,0.988105030697865,0.991593692313265)))
REPRESENTATION_ITEM('')
SURFACE()
);
#3031=(
BOUNDED_SURFACE()
B_SPLINE_SURFACE(1,2,((#145591,#145592,#145593),(#145594,#145595,#145596)),
 .UNSPECIFIED.,.F.,.F.,.F.)
B_SPLINE_SURFACE_WITH_KNOTS((2,2),(3,3),(0.,0.28980704099163),(0.176967058622922,
0.194235682574593),.UNSPECIFIED.)
GEOMETRIC_REPRESENTATION_ITEM()
RATIONAL_B_SPLINE_SURFACE(((0.98748925405691,0.987216959588932,0.989875504592249),
(0.98748925405691,0.987216959588932,0.989875504592249)))
REPRESENTATION_ITEM('')
SURFACE()
);
#3032=(
BOUNDED_SURFACE()
B_SPLINE_SURFACE(1,2,((#145613,#145614,#145615),(#145616,#145617,#145618)),
 .UNSPECIFIED.,.F.,.F.,.F.)
B_SPLINE_SURFACE_WITH_KNOTS((2,2),(3,3),(0.,0.28968108435992),(0.538896351358318,
0.556212823028861),.UNSPECIFIED.)
GEOMETRIC_REPRESENTATION_ITEM()
RATIONAL_B_SPLINE_SURFACE(((0.987563472532048,0.988105030697865,0.991593692313265),
(0.987563472532048,0.988105030697865,0.991593692313265)))
REPRESENTATION_ITEM('')
SURFACE()
);
#3033=(
BOUNDED_SURFACE()
B_SPLINE_SURFACE(1,2,((#145620,#145621,#145622),(#145623,#145624,#145625)),
 .UNSPECIFIED.,.F.,.F.,.F.)
B_SPLINE_SURFACE_WITH_KNOTS((2,2),(3,3),(0.,0.28980704099191),(0.176967058622922,
0.194235682574593),.UNSPECIFIED.)
GEOMETRIC_REPRESENTATION_ITEM()
RATIONAL_B_SPLINE_SURFACE(((0.98748925405691,0.987216959588932,0.989875504592249),
(0.98748925405691,0.987216959588932,0.989875504592249)))
REPRESENTATION_ITEM('')
SURFACE()
);
#3034=(
BOUNDED_SURFACE()
B_SPLINE_SURFACE(1,2,((#145642,#145643,#145644),(#145645,#145646,#145647)),
 .UNSPECIFIED.,.F.,.F.,.F.)
B_SPLINE_SURFACE_WITH_KNOTS((2,2),(3,3),(0.,0.289681084359926),(0.538896351358318,
0.556212823028864),.UNSPECIFIED.)
GEOMETRIC_REPRESENTATION_ITEM()
RATIONAL_B_SPLINE_SURFACE(((0.987563472532048,0.988105030697865,0.991593692313266),
(0.987563472532048,0.988105030697865,0.991593692313266)))
REPRESENTATION_ITEM('')
SURFACE()
);
#3035=(
BOUNDED_SURFACE()
B_SPLINE_SURFACE(1,2,((#145655,#145656,#145657),(#145658,#145659,#145660)),
 .UNSPECIFIED.,.F.,.F.,.F.)
B_SPLINE_SURFACE_WITH_KNOTS((2,2),(3,3),(0.,0.289807040991561),(0.176967058622922,
0.194235682574593),.UNSPECIFIED.)
GEOMETRIC_REPRESENTATION_ITEM()
RATIONAL_B_SPLINE_SURFACE(((0.98748925405691,0.987216959588932,0.989875504592249),
(0.98748925405691,0.987216959588932,0.989875504592249)))
REPRESENTATION_ITEM('')
SURFACE()
);
#3036=(
BOUNDED_SURFACE()
B_SPLINE_SURFACE(1,2,((#145662,#145663,#145664),(#145665,#145666,#145667)),
 .UNSPECIFIED.,.F.,.F.,.F.)
B_SPLINE_SURFACE_WITH_KNOTS((2,2),(3,3),(0.710192959007979,1.),(0.125170525609408,
0.142682999576236),.UNSPECIFIED.)
GEOMETRIC_REPRESENTATION_ITEM()
RATIONAL_B_SPLINE_SURFACE(((0.990658108926709,0.993760979299921,0.999878046252917),
(0.990658108926709,0.993760979299921,0.999878046252917)))
REPRESENTATION_ITEM('')
SURFACE()
);
#3037=(
BOUNDED_SURFACE()
B_SPLINE_SURFACE(1,2,((#145678,#145679,#145680,#145681,#145682),(#145683,
#145684,#145685,#145686,#145687)),.UNSPECIFIED.,.F.,.F.,.F.)
B_SPLINE_SURFACE_WITH_KNOTS((2,2),(3,2,3),(0.709728555967135,1.),(0.590808523385635,
0.607982157956011,0.608572517827272),.UNSPECIFIED.)
GEOMETRIC_REPRESENTATION_ITEM()
RATIONAL_B_SPLINE_SURFACE(((0.990086238235256,0.987329216372183,0.987470879370256,
0.987470879370256,0.987470879370256),(0.990086238235256,0.987329216372183,
0.987470879370256,0.987470879370256,0.987470879370256)))
REPRESENTATION_ITEM('')
SURFACE()
);
#3038=(
BOUNDED_SURFACE()
B_SPLINE_SURFACE(1,2,((#145698,#145699,#145700),(#145701,#145702,#145703)),
 .UNSPECIFIED.,.F.,.F.,.F.)
B_SPLINE_SURFACE_WITH_KNOTS((2,2),(3,3),(0.710192959007996,1.),(0.125170525609408,
0.142682999576236),.UNSPECIFIED.)
GEOMETRIC_REPRESENTATION_ITEM()
RATIONAL_B_SPLINE_SURFACE(((0.990658108926709,0.993760979299921,0.999878046252917),
(0.990658108926709,0.993760979299921,0.999878046252917)))
REPRESENTATION_ITEM('')
SURFACE()
);
#3039=(
BOUNDED_SURFACE()
B_SPLINE_SURFACE(1,2,((#145711,#145712,#145713,#145714,#145715),(#145716,
#145717,#145718,#145719,#145720)),.UNSPECIFIED.,.F.,.F.,.F.)
B_SPLINE_SURFACE_WITH_KNOTS((2,2),(3,2,3),(0.709728555997542,1.),(0.590808523385635,
0.607982157956011,0.608572517839914),.UNSPECIFIED.)
GEOMETRIC_REPRESENTATION_ITEM()
RATIONAL_B_SPLINE_SURFACE(((0.990086238235256,0.987329216372183,0.987470879370256,
0.987470879370256,0.987470879370256),(0.990086238235256,0.987329216372183,
0.987470879370256,0.987470879370256,0.987470879370256)))
REPRESENTATION_ITEM('')
SURFACE()
);
#3040=(
BOUNDED_SURFACE()
B_SPLINE_SURFACE(1,2,((#145731,#145732,#145733),(#145734,#145735,#145736)),
 .UNSPECIFIED.,.F.,.F.,.F.)
B_SPLINE_SURFACE_WITH_KNOTS((2,2),(3,3),(0.710192959008342,1.),(0.125170525609408,
0.142682999576236),.UNSPECIFIED.)
GEOMETRIC_REPRESENTATION_ITEM()
RATIONAL_B_SPLINE_SURFACE(((0.990658108926709,0.993760979299921,0.999878046252917),
(0.990658108926709,0.993760979299921,0.999878046252917)))
REPRESENTATION_ITEM('')
SURFACE()
);
#3041=(
BOUNDED_SURFACE()
B_SPLINE_SURFACE(1,2,((#145744,#145745,#145746,#145747,#145748),(#145749,
#145750,#145751,#145752,#145753)),.UNSPECIFIED.,.F.,.F.,.F.)
B_SPLINE_SURFACE_WITH_KNOTS((2,2),(3,2,3),(0.709728555976075,1.),(0.590808523385635,
0.607982157956012,0.608572517860657),.UNSPECIFIED.)
GEOMETRIC_REPRESENTATION_ITEM()
RATIONAL_B_SPLINE_SURFACE(((0.990086238235256,0.987329216372183,0.987470879370256,
0.987470879370256,0.987470879370256),(0.990086238235256,0.987329216372183,
0.987470879370256,0.987470879370256,0.987470879370256)))
REPRESENTATION_ITEM('')
SURFACE()
);
#3042=(
BOUNDED_SURFACE()
B_SPLINE_SURFACE(1,2,((#145764,#145765,#145766),(#145767,#145768,#145769)),
 .UNSPECIFIED.,.F.,.F.,.F.)
B_SPLINE_SURFACE_WITH_KNOTS((2,2),(3,3),(0.710192959008336,1.),(0.125170525609409,
0.142682999576236),.UNSPECIFIED.)
GEOMETRIC_REPRESENTATION_ITEM()
RATIONAL_B_SPLINE_SURFACE(((0.990658108926709,0.993760979299921,0.999878046252917),
(0.990658108926709,0.993760979299921,0.999878046252917)))
REPRESENTATION_ITEM('')
SURFACE()
);
#3043=(
BOUNDED_SURFACE()
B_SPLINE_SURFACE(1,2,((#145777,#145778,#145779,#145780,#145781),(#145782,
#145783,#145784,#145785,#145786)),.UNSPECIFIED.,.F.,.F.,.F.)
B_SPLINE_SURFACE_WITH_KNOTS((2,2),(3,2,3),(0.709728555936133,1.),(0.590808523385635,
0.607982157956012,0.608572517857657),.UNSPECIFIED.)
GEOMETRIC_REPRESENTATION_ITEM()
RATIONAL_B_SPLINE_SURFACE(((0.990086238235256,0.987329216372183,0.987470879370255,
0.987470879370255,0.987470879370255),(0.990086238235256,0.987329216372183,
0.987470879370255,0.987470879370255,0.987470879370255)))
REPRESENTATION_ITEM('')
SURFACE()
);
#3044=(
BOUNDED_SURFACE()
B_SPLINE_SURFACE(1,2,((#145797,#145798,#145799),(#145800,#145801,#145802)),
 .UNSPECIFIED.,.F.,.F.,.F.)
B_SPLINE_SURFACE_WITH_KNOTS((2,2),(3,3),(0.71019295900738,1.),(0.125170525609408,
0.142682999576236),.UNSPECIFIED.)
GEOMETRIC_REPRESENTATION_ITEM()
RATIONAL_B_SPLINE_SURFACE(((0.990658108926709,0.993760979299921,0.999878046252917),
(0.990658108926709,0.993760979299921,0.999878046252917)))
REPRESENTATION_ITEM('')
SURFACE()
);
#3045=(
BOUNDED_SURFACE()
B_SPLINE_SURFACE(1,2,((#145810,#145811,#145812,#145813,#145814),(#145815,
#145816,#145817,#145818,#145819)),.UNSPECIFIED.,.F.,.F.,.F.)
B_SPLINE_SURFACE_WITH_KNOTS((2,2),(3,2,3),(0.709728555933635,1.),(0.590808523385635,
0.607982157956011,0.608572517860158),.UNSPECIFIED.)
GEOMETRIC_REPRESENTATION_ITEM()
RATIONAL_B_SPLINE_SURFACE(((0.990086238235256,0.987329216372183,0.987470879370256,
0.987470879370256,0.987470879370256),(0.990086238235256,0.987329216372183,
0.987470879370256,0.987470879370256,0.987470879370256)))
REPRESENTATION_ITEM('')
SURFACE()
);
#3046=(
BOUNDED_SURFACE()
B_SPLINE_SURFACE(1,2,((#145830,#145831,#145832),(#145833,#145834,#145835)),
 .UNSPECIFIED.,.F.,.F.,.F.)
B_SPLINE_SURFACE_WITH_KNOTS((2,2),(3,3),(0.710192959007375,1.),(0.125170525609408,
0.142682999576236),.UNSPECIFIED.)
GEOMETRIC_REPRESENTATION_ITEM()
RATIONAL_B_SPLINE_SURFACE(((0.990658108926709,0.993760979299921,0.999878046252917),
(0.990658108926709,0.993760979299921,0.999878046252917)))
REPRESENTATION_ITEM('')
SURFACE()
);
#3047=(
BOUNDED_SURFACE()
B_SPLINE_SURFACE(1,2,((#145843,#145844,#145845,#145846,#145847),(#145848,
#145849,#145850,#145851,#145852)),.UNSPECIFIED.,.F.,.F.,.F.)
B_SPLINE_SURFACE_WITH_KNOTS((2,2),(3,2,3),(0.709728555952784,1.),(0.590808523385635,
0.607982157956011,0.60857251784101),.UNSPECIFIED.)
GEOMETRIC_REPRESENTATION_ITEM()
RATIONAL_B_SPLINE_SURFACE(((0.990086238235256,0.987329216372183,0.987470879370255,
0.987470879370255,0.987470879370255),(0.990086238235256,0.987329216372183,
0.987470879370255,0.987470879370255,0.987470879370255)))
REPRESENTATION_ITEM('')
SURFACE()
);
#3048=(
BOUNDED_SURFACE()
B_SPLINE_SURFACE(1,2,((#145863,#145864,#145865),(#145866,#145867,#145868)),
 .UNSPECIFIED.,.F.,.F.,.F.)
B_SPLINE_SURFACE_WITH_KNOTS((2,2),(3,3),(0.71019295900738,1.),(0.125170525609408,
0.142682999576236),.UNSPECIFIED.)
GEOMETRIC_REPRESENTATION_ITEM()
RATIONAL_B_SPLINE_SURFACE(((0.990658108926709,0.993760979299922,0.999878046252917),
(0.990658108926709,0.993760979299922,0.999878046252917)))
REPRESENTATION_ITEM('')
SURFACE()
);
#3049=(
BOUNDED_SURFACE()
B_SPLINE_SURFACE(1,2,((#145876,#145877,#145878,#145879,#145880),(#145881,
#145882,#145883,#145884,#145885)),.UNSPECIFIED.,.F.,.F.,.F.)
B_SPLINE_SURFACE_WITH_KNOTS((2,2),(3,2,3),(0.709728555955733,1.),(0.590808523385635,
0.607982157956011,0.608572517837478),.UNSPECIFIED.)
GEOMETRIC_REPRESENTATION_ITEM()
RATIONAL_B_SPLINE_SURFACE(((0.990086238235256,0.987329216372183,0.987470879370255,
0.987470879370255,0.987470879370255),(0.990086238235256,0.987329216372183,
0.987470879370255,0.987470879370255,0.987470879370255)))
REPRESENTATION_ITEM('')
SURFACE()
);
#3050=(
BOUNDED_SURFACE()
B_SPLINE_SURFACE(1,2,((#145896,#145897,#145898),(#145899,#145900,#145901)),
 .UNSPECIFIED.,.F.,.F.,.F.)
B_SPLINE_SURFACE_WITH_KNOTS((2,2),(3,3),(0.710192959006796,1.),(0.125170525609408,
0.142682999576236),.UNSPECIFIED.)
GEOMETRIC_REPRESENTATION_ITEM()
RATIONAL_B_SPLINE_SURFACE(((0.990658108926709,0.993760979299921,0.999878046252917),
(0.990658108926709,0.993760979299921,0.999878046252917)))
REPRESENTATION_ITEM('')
SURFACE()
);
#3051=(
BOUNDED_SURFACE()
B_SPLINE_SURFACE(1,2,((#145909,#145910,#145911,#145912,#145913),(#145914,
#145915,#145916,#145917,#145918)),.UNSPECIFIED.,.F.,.F.,.F.)
B_SPLINE_SURFACE_WITH_KNOTS((2,2),(3,2,3),(0.709728555987901,1.),(0.590808523385635,
0.607982157956011,0.608572517848439),.UNSPECIFIED.)
GEOMETRIC_REPRESENTATION_ITEM()
RATIONAL_B_SPLINE_SURFACE(((0.990086238235256,0.987329216372183,0.987470879370255,
0.987470879370255,0.987470879370255),(0.990086238235256,0.987329216372183,
0.987470879370255,0.987470879370255,0.987470879370255)))
REPRESENTATION_ITEM('')
SURFACE()
);
#3052=(
BOUNDED_SURFACE()
B_SPLINE_SURFACE(1,2,((#145929,#145930,#145931),(#145932,#145933,#145934)),
 .UNSPECIFIED.,.F.,.F.,.F.)
B_SPLINE_SURFACE_WITH_KNOTS((2,2),(3,3),(0.710192959007385,1.),(0.125170525609408,
0.142682999576236),.UNSPECIFIED.)
GEOMETRIC_REPRESENTATION_ITEM()
RATIONAL_B_SPLINE_SURFACE(((0.990658108926709,0.993760979299921,0.999878046252917),
(0.990658108926709,0.993760979299921,0.999878046252917)))
REPRESENTATION_ITEM('')
SURFACE()
);
#3053=(
BOUNDED_SURFACE()
B_SPLINE_SURFACE(1,2,((#145942,#145943,#145944,#145945,#145946),(#145947,
#145948,#145949,#145950,#145951)),.UNSPECIFIED.,.F.,.F.,.F.)
B_SPLINE_SURFACE_WITH_KNOTS((2,2),(3,2,3),(0.709728556004289,1.),(0.590808523385635,
0.607982157956011,0.608572517831713),.UNSPECIFIED.)
GEOMETRIC_REPRESENTATION_ITEM()
RATIONAL_B_SPLINE_SURFACE(((0.990086238235256,0.987329216372183,0.987470879370255,
0.987470879370255,0.987470879370255),(0.990086238235256,0.987329216372183,
0.987470879370255,0.987470879370255,0.987470879370255)))
REPRESENTATION_ITEM('')
SURFACE()
);
#3054=(
BOUNDED_SURFACE()
B_SPLINE_SURFACE(1,2,((#145962,#145963,#145964),(#145965,#145966,#145967)),
 .UNSPECIFIED.,.F.,.F.,.F.)
B_SPLINE_SURFACE_WITH_KNOTS((2,2),(3,3),(0.71019295900683,1.),(0.125170525609408,
0.142682999576236),.UNSPECIFIED.)
GEOMETRIC_REPRESENTATION_ITEM()
RATIONAL_B_SPLINE_SURFACE(((0.990658108926709,0.993760979299921,0.999878046252917),
(0.990658108926709,0.993760979299921,0.999878046252917)))
REPRESENTATION_ITEM('')
SURFACE()
);
#3055=(
BOUNDED_SURFACE()
B_SPLINE_SURFACE(1,2,((#145975,#145976,#145977,#145978,#145979),(#145980,
#145981,#145982,#145983,#145984)),.UNSPECIFIED.,.F.,.F.,.F.)
B_SPLINE_SURFACE_WITH_KNOTS((2,2),(3,2,3),(0.709728556000902,1.),(0.590808523385636,
0.607982157956011,0.6085725178347),.UNSPECIFIED.)
GEOMETRIC_REPRESENTATION_ITEM()
RATIONAL_B_SPLINE_SURFACE(((0.990086238235256,0.987329216372183,0.987470879370255,
0.987470879370255,0.987470879370255),(0.990086238235256,0.987329216372183,
0.987470879370255,0.987470879370255,0.987470879370255)))
REPRESENTATION_ITEM('')
SURFACE()
);
#3056=(
BOUNDED_SURFACE()
B_SPLINE_SURFACE(1,2,((#145995,#145996,#145997),(#145998,#145999,#146000)),
 .UNSPECIFIED.,.F.,.F.,.F.)
B_SPLINE_SURFACE_WITH_KNOTS((2,2),(3,3),(0.710192959007012,1.),(0.125170525609407,
0.142682999576235),.UNSPECIFIED.)
GEOMETRIC_REPRESENTATION_ITEM()
RATIONAL_B_SPLINE_SURFACE(((0.990658108926708,0.993760979299921,0.999878046252916),
(0.990658108926708,0.993760979299921,0.999878046252916)))
REPRESENTATION_ITEM('')
SURFACE()
);
#3057=(
BOUNDED_SURFACE()
B_SPLINE_SURFACE(1,2,((#146008,#146009,#146010,#146011,#146012),(#146013,
#146014,#146015,#146016,#146017)),.UNSPECIFIED.,.F.,.F.,.F.)
B_SPLINE_SURFACE_WITH_KNOTS((2,2),(3,2,3),(0.709728555986702,1.),(0.590808523385636,
0.607982157956012,0.608572517849571),.UNSPECIFIED.)
GEOMETRIC_REPRESENTATION_ITEM()
RATIONAL_B_SPLINE_SURFACE(((0.990086238235256,0.987329216372183,0.987470879370255,
0.987470879370255,0.987470879370255),(0.990086238235256,0.987329216372183,
0.987470879370255,0.987470879370255,0.987470879370255)))
REPRESENTATION_ITEM('')
SURFACE()
);
#3058=(
BOUNDED_SURFACE()
B_SPLINE_SURFACE(1,2,((#146028,#146029,#146030),(#146031,#146032,#146033)),
 .UNSPECIFIED.,.F.,.F.,.F.)
B_SPLINE_SURFACE_WITH_KNOTS((2,2),(3,3),(0.710192959006983,1.),(0.125170525609407,
0.142682999576235),.UNSPECIFIED.)
GEOMETRIC_REPRESENTATION_ITEM()
RATIONAL_B_SPLINE_SURFACE(((0.990658108926708,0.993760979299921,0.999878046252916),
(0.990658108926708,0.993760979299921,0.999878046252916)))
REPRESENTATION_ITEM('')
SURFACE()
);
#3059=(
BOUNDED_SURFACE()
B_SPLINE_SURFACE(1,2,((#146041,#146042,#146043,#146044,#146045),(#146046,
#146047,#146048,#146049,#146050)),.UNSPECIFIED.,.F.,.F.,.F.)
B_SPLINE_SURFACE_WITH_KNOTS((2,2),(3,2,3),(0.709728555941526,1.),(0.590808523385636,
0.607982157956012,0.6085725178516),.UNSPECIFIED.)
GEOMETRIC_REPRESENTATION_ITEM()
RATIONAL_B_SPLINE_SURFACE(((0.990086238235256,0.987329216372183,0.987470879370255,
0.987470879370255,0.987470879370255),(0.990086238235256,0.987329216372183,
0.987470879370255,0.987470879370255,0.987470879370255)))
REPRESENTATION_ITEM('')
SURFACE()
);
#3060=(
BOUNDED_SURFACE()
B_SPLINE_SURFACE(1,2,((#146061,#146062,#146063),(#146064,#146065,#146066)),
 .UNSPECIFIED.,.F.,.F.,.F.)
B_SPLINE_SURFACE_WITH_KNOTS((2,2),(3,3),(0.710192959006704,1.),(0.125170525609407,
0.142682999576235),.UNSPECIFIED.)
GEOMETRIC_REPRESENTATION_ITEM()
RATIONAL_B_SPLINE_SURFACE(((0.990658108926708,0.993760979299921,0.999878046252916),
(0.990658108926708,0.993760979299921,0.999878046252916)))
REPRESENTATION_ITEM('')
SURFACE()
);
#3061=(
BOUNDED_SURFACE()
B_SPLINE_SURFACE(1,2,((#146074,#146075,#146076,#146077,#146078),(#146079,
#146080,#146081,#146082,#146083)),.UNSPECIFIED.,.F.,.F.,.F.)
B_SPLINE_SURFACE_WITH_KNOTS((2,2),(3,2,3),(0.709728555981745,1.),(0.590808523385636,
0.607982157956012,0.608572517854524),.UNSPECIFIED.)
GEOMETRIC_REPRESENTATION_ITEM()
RATIONAL_B_SPLINE_SURFACE(((0.990086238235256,0.987329216372183,0.987470879370255,
0.987470879370255,0.987470879370255),(0.990086238235256,0.987329216372183,
0.987470879370255,0.987470879370255,0.987470879370255)))
REPRESENTATION_ITEM('')
SURFACE()
);
#3062=(
BOUNDED_SURFACE()
B_SPLINE_SURFACE(1,2,((#146094,#146095,#146096),(#146097,#146098,#146099)),
 .UNSPECIFIED.,.F.,.F.,.F.)
B_SPLINE_SURFACE_WITH_KNOTS((2,2),(3,3),(0.710192959007287,1.),(0.125170525609407,
0.142682999576235),.UNSPECIFIED.)
GEOMETRIC_REPRESENTATION_ITEM()
RATIONAL_B_SPLINE_SURFACE(((0.990658108926708,0.993760979299921,0.999878046252916),
(0.990658108926708,0.993760979299921,0.999878046252916)))
REPRESENTATION_ITEM('')
SURFACE()
);
#3063=(
BOUNDED_SURFACE()
B_SPLINE_SURFACE(1,2,((#146107,#146108,#146109,#146110,#146111),(#146112,
#146113,#146114,#146115,#146116)),.UNSPECIFIED.,.F.,.F.,.F.)
B_SPLINE_SURFACE_WITH_KNOTS((2,2),(3,2,3),(0.709728555951994,1.),(0.590808523385636,
0.607982157956013,0.608572517840887),.UNSPECIFIED.)
GEOMETRIC_REPRESENTATION_ITEM()
RATIONAL_B_SPLINE_SURFACE(((0.990086238235256,0.987329216372183,0.987470879370255,
0.987470879370255,0.987470879370255),(0.990086238235256,0.987329216372183,
0.987470879370255,0.987470879370255,0.987470879370255)))
REPRESENTATION_ITEM('')
SURFACE()
);
#3064=(
BOUNDED_SURFACE()
B_SPLINE_SURFACE(1,2,((#146124,#146125,#146126),(#146127,#146128,#146129)),
 .UNSPECIFIED.,.F.,.F.,.F.)
B_SPLINE_SURFACE_WITH_KNOTS((2,2),(3,3),(0.710192959006456,1.),(0.125170525609407,
0.142682999576235),.UNSPECIFIED.)
GEOMETRIC_REPRESENTATION_ITEM()
RATIONAL_B_SPLINE_SURFACE(((0.990658108926708,0.993760979299921,0.999878046252916),
(0.990658108926708,0.993760979299921,0.999878046252916)))
REPRESENTATION_ITEM('')
SURFACE()
);
#3065=(
BOUNDED_SURFACE()
B_SPLINE_SURFACE(1,2,((#146131,#146132,#146133,#146134,#146135),(#146136,
#146137,#146138,#146139,#146140)),.UNSPECIFIED.,.F.,.F.,.F.)
B_SPLINE_SURFACE_WITH_KNOTS((2,2),(3,2,3),(0.709728555938271,1.),(0.590808523385636,
0.607982157956013,0.608572517855104),.UNSPECIFIED.)
GEOMETRIC_REPRESENTATION_ITEM()
RATIONAL_B_SPLINE_SURFACE(((0.990086238235256,0.987329216372183,0.987470879370255,
0.987470879370255,0.987470879370255),(0.990086238235256,0.987329216372183,
0.987470879370255,0.987470879370255,0.987470879370255)))
REPRESENTATION_ITEM('')
SURFACE()
);
#3066=(
BOUNDED_SURFACE()
B_SPLINE_SURFACE(1,2,((#146151,#146152,#146153),(#146154,#146155,#146156)),
 .UNSPECIFIED.,.F.,.F.,.F.)
B_SPLINE_SURFACE_WITH_KNOTS((2,2),(3,3),(0.710192959006957,1.),(0.125170525609407,
0.142682999576235),.UNSPECIFIED.)
GEOMETRIC_REPRESENTATION_ITEM()
RATIONAL_B_SPLINE_SURFACE(((0.990658108926708,0.993760979299921,0.999878046252916),
(0.990658108926708,0.993760979299921,0.999878046252916)))
REPRESENTATION_ITEM('')
SURFACE()
);
#3067=(
BOUNDED_SURFACE()
B_SPLINE_SURFACE(1,2,((#146164,#146165,#146166,#146167,#146168),(#146169,
#146170,#146171,#146172,#146173)),.UNSPECIFIED.,.F.,.F.,.F.)
B_SPLINE_SURFACE_WITH_KNOTS((2,2),(3,2,3),(0.709728555977483,1.),(0.590808523385636,
0.607982157956013,0.608572517858113),.UNSPECIFIED.)
GEOMETRIC_REPRESENTATION_ITEM()
RATIONAL_B_SPLINE_SURFACE(((0.990086238235256,0.987329216372183,0.987470879370256,
0.987470879370256,0.987470879370256),(0.990086238235256,0.987329216372183,
0.987470879370256,0.987470879370256,0.987470879370256)))
REPRESENTATION_ITEM('')
SURFACE()
);
#3068=(
BOUNDED_SURFACE()
B_SPLINE_SURFACE(1,2,((#146184,#146185,#146186),(#146187,#146188,#146189)),
 .UNSPECIFIED.,.F.,.F.,.F.)
B_SPLINE_SURFACE_WITH_KNOTS((2,2),(3,3),(0.710192959006483,1.),(0.125170525609407,
0.142682999576235),.UNSPECIFIED.)
GEOMETRIC_REPRESENTATION_ITEM()
RATIONAL_B_SPLINE_SURFACE(((0.990658108926708,0.993760979299921,0.999878046252916),
(0.990658108926708,0.993760979299921,0.999878046252916)))
REPRESENTATION_ITEM('')
SURFACE()
);
#3069=(
BOUNDED_SURFACE()
B_SPLINE_SURFACE(1,2,((#146197,#146198,#146199,#146200,#146201),(#146202,
#146203,#146204,#146205,#146206)),.UNSPECIFIED.,.F.,.F.,.F.)
B_SPLINE_SURFACE_WITH_KNOTS((2,2),(3,2,3),(0.709728556027411,1.),(0.590808523385636,
0.607982157956012,0.608572517808381),.UNSPECIFIED.)
GEOMETRIC_REPRESENTATION_ITEM()
RATIONAL_B_SPLINE_SURFACE(((0.990086238235256,0.987329216372183,0.987470879370255,
0.987470879370255,0.987470879370255),(0.990086238235256,0.987329216372183,
0.987470879370255,0.987470879370255,0.987470879370255)))
REPRESENTATION_ITEM('')
SURFACE()
);
#3070=(
BOUNDED_SURFACE()
B_SPLINE_SURFACE(1,2,((#146217,#146218,#146219),(#146220,#146221,#146222)),
 .UNSPECIFIED.,.F.,.F.,.F.)
B_SPLINE_SURFACE_WITH_KNOTS((2,2),(3,3),(0.710192959006738,1.),(0.125170525609407,
0.142682999576235),.UNSPECIFIED.)
GEOMETRIC_REPRESENTATION_ITEM()
RATIONAL_B_SPLINE_SURFACE(((0.990658108926708,0.993760979299921,0.999878046252916),
(0.990658108926708,0.993760979299921,0.999878046252916)))
REPRESENTATION_ITEM('')
SURFACE()
);
#3071=(
BOUNDED_SURFACE()
B_SPLINE_SURFACE(1,2,((#146230,#146231,#146232,#146233,#146234),(#146235,
#146236,#146237,#146238,#146239)),.UNSPECIFIED.,.F.,.F.,.F.)
B_SPLINE_SURFACE_WITH_KNOTS((2,2),(3,2,3),(0.709728555976806,1.),(0.590808523385636,
0.607982157956012,0.608572517857857),.UNSPECIFIED.)
GEOMETRIC_REPRESENTATION_ITEM()
RATIONAL_B_SPLINE_SURFACE(((0.990086238235256,0.987329216372183,0.987470879370255,
0.987470879370255,0.987470879370255),(0.990086238235256,0.987329216372183,
0.987470879370255,0.987470879370255,0.987470879370255)))
REPRESENTATION_ITEM('')
SURFACE()
);
#3072=(
BOUNDED_SURFACE()
B_SPLINE_SURFACE(1,2,((#146250,#146251,#146252),(#146253,#146254,#146255)),
 .UNSPECIFIED.,.F.,.F.,.F.)
B_SPLINE_SURFACE_WITH_KNOTS((2,2),(3,3),(0.710192959005573,1.),(0.125170525609407,
0.142682999576235),.UNSPECIFIED.)
GEOMETRIC_REPRESENTATION_ITEM()
RATIONAL_B_SPLINE_SURFACE(((0.990658108926708,0.993760979299921,0.999878046252916),
(0.990658108926708,0.993760979299921,0.999878046252916)))
REPRESENTATION_ITEM('')
SURFACE()
);
#3073=(
BOUNDED_SURFACE()
B_SPLINE_SURFACE(1,2,((#146263,#146264,#146265,#146266,#146267),(#146268,
#146269,#146270,#146271,#146272)),.UNSPECIFIED.,.F.,.F.,.F.)
B_SPLINE_SURFACE_WITH_KNOTS((2,2),(3,2,3),(0.709728555966191,1.),(0.590808523385636,
0.607982157956012,0.608572517827467),.UNSPECIFIED.)
GEOMETRIC_REPRESENTATION_ITEM()
RATIONAL_B_SPLINE_SURFACE(((0.990086238235256,0.987329216372183,0.987470879370255,
0.987470879370255,0.987470879370255),(0.990086238235256,0.987329216372183,
0.987470879370255,0.987470879370255,0.987470879370255)))
REPRESENTATION_ITEM('')
SURFACE()
);
#3074=(
BOUNDED_SURFACE()
B_SPLINE_SURFACE(1,2,((#146283,#146284,#146285),(#146286,#146287,#146288)),
 .UNSPECIFIED.,.F.,.F.,.F.)
B_SPLINE_SURFACE_WITH_KNOTS((2,2),(3,3),(0.710192959007236,1.),(0.125170525609407,
0.142682999576235),.UNSPECIFIED.)
GEOMETRIC_REPRESENTATION_ITEM()
RATIONAL_B_SPLINE_SURFACE(((0.990658108926708,0.993760979299921,0.999878046252916),
(0.990658108926708,0.993760979299921,0.999878046252916)))
REPRESENTATION_ITEM('')
SURFACE()
);
#3075=(
BOUNDED_SURFACE()
B_SPLINE_SURFACE(1,2,((#146296,#146297,#146298,#146299,#146300),(#146301,
#146302,#146303,#146304,#146305)),.UNSPECIFIED.,.F.,.F.,.F.)
B_SPLINE_SURFACE_WITH_KNOTS((2,2),(3,2,3),(0.709728555981059,1.),(0.590808523385636,
0.607982157956012,0.608572517855585),.UNSPECIFIED.)
GEOMETRIC_REPRESENTATION_ITEM()
RATIONAL_B_SPLINE_SURFACE(((0.990086238235256,0.987329216372183,0.987470879370255,
0.987470879370255,0.987470879370255),(0.990086238235256,0.987329216372183,
0.987470879370255,0.987470879370255,0.987470879370255)))
REPRESENTATION_ITEM('')
SURFACE()
);
#3076=(
BOUNDED_SURFACE()
B_SPLINE_SURFACE(1,2,((#146316,#146317,#146318),(#146319,#146320,#146321)),
 .UNSPECIFIED.,.F.,.F.,.F.)
B_SPLINE_SURFACE_WITH_KNOTS((2,2),(3,3),(0.710192959007354,1.),(0.125170525609407,
0.142682999576235),.UNSPECIFIED.)
GEOMETRIC_REPRESENTATION_ITEM()
RATIONAL_B_SPLINE_SURFACE(((0.990658108926708,0.993760979299921,0.999878046252916),
(0.990658108926708,0.993760979299921,0.999878046252916)))
REPRESENTATION_ITEM('')
SURFACE()
);
#3077=(
BOUNDED_SURFACE()
B_SPLINE_SURFACE(1,2,((#146329,#146330,#146331,#146332,#146333),(#146334,
#146335,#146336,#146337,#146338)),.UNSPECIFIED.,.F.,.F.,.F.)
B_SPLINE_SURFACE_WITH_KNOTS((2,2),(3,2,3),(0.709728555961017,1.),(0.590808523385636,
0.607982157956012,0.608572517831906),.UNSPECIFIED.)
GEOMETRIC_REPRESENTATION_ITEM()
RATIONAL_B_SPLINE_SURFACE(((0.990086238235256,0.987329216372183,0.987470879370255,
0.987470879370255,0.987470879370255),(0.990086238235256,0.987329216372183,
0.987470879370255,0.987470879370255,0.987470879370255)))
REPRESENTATION_ITEM('')
SURFACE()
);
#3078=(
BOUNDED_SURFACE()
B_SPLINE_SURFACE(1,2,((#146349,#146350,#146351),(#146352,#146353,#146354)),
 .UNSPECIFIED.,.F.,.F.,.F.)
B_SPLINE_SURFACE_WITH_KNOTS((2,2),(3,3),(0.710192959006508,1.),(0.125170525609407,
0.142682999576236),.UNSPECIFIED.)
GEOMETRIC_REPRESENTATION_ITEM()
RATIONAL_B_SPLINE_SURFACE(((0.990658108926708,0.993760979299921,0.999878046252916),
(0.990658108926708,0.993760979299921,0.999878046252916)))
REPRESENTATION_ITEM('')
SURFACE()
);
#3079=(
BOUNDED_SURFACE()
B_SPLINE_SURFACE(1,2,((#146362,#146363,#146364,#146365,#146366),(#146367,
#146368,#146369,#146370,#146371)),.UNSPECIFIED.,.F.,.F.,.F.)
B_SPLINE_SURFACE_WITH_KNOTS((2,2),(3,2,3),(0.709728555958552,1.),(0.590808523385636,
0.607982157956012,0.608572517835848),.UNSPECIFIED.)
GEOMETRIC_REPRESENTATION_ITEM()
RATIONAL_B_SPLINE_SURFACE(((0.990086238235256,0.987329216372183,0.987470879370255,
0.987470879370255,0.987470879370255),(0.990086238235256,0.987329216372183,
0.987470879370255,0.987470879370255,0.987470879370255)))
REPRESENTATION_ITEM('')
SURFACE()
);
#3080=(
BOUNDED_SURFACE()
B_SPLINE_SURFACE(1,2,((#146382,#146383,#146384),(#146385,#146386,#146387)),
 .UNSPECIFIED.,.F.,.F.,.F.)
B_SPLINE_SURFACE_WITH_KNOTS((2,2),(3,3),(0.710192959007983,1.),(0.125170525609407,
0.142682999576235),.UNSPECIFIED.)
GEOMETRIC_REPRESENTATION_ITEM()
RATIONAL_B_SPLINE_SURFACE(((0.990658108926708,0.993760979299921,0.999878046252916),
(0.990658108926708,0.993760979299921,0.999878046252916)))
REPRESENTATION_ITEM('')
SURFACE()
);
#3081=(
BOUNDED_SURFACE()
B_SPLINE_SURFACE(1,2,((#146395,#146396,#146397,#146398,#146399),(#146400,
#146401,#146402,#146403,#146404)),.UNSPECIFIED.,.F.,.F.,.F.)
B_SPLINE_SURFACE_WITH_KNOTS((2,2),(3,2,3),(0.709728555999848,1.),(0.590808523385636,
0.607982157956017,0.608572517836349),.UNSPECIFIED.)
GEOMETRIC_REPRESENTATION_ITEM()
RATIONAL_B_SPLINE_SURFACE(((0.990086238235256,0.987329216372182,0.987470879370255,
0.987470879370255,0.987470879370255),(0.990086238235256,0.987329216372182,
0.987470879370255,0.987470879370255,0.987470879370255)))
REPRESENTATION_ITEM('')
SURFACE()
);
#3082=(
BOUNDED_SURFACE()
B_SPLINE_SURFACE(1,2,((#146415,#146416,#146417),(#146418,#146419,#146420)),
 .UNSPECIFIED.,.F.,.F.,.F.)
B_SPLINE_SURFACE_WITH_KNOTS((2,2),(3,3),(0.710192959007115,1.),(0.125170525609407,
0.142682999576235),.UNSPECIFIED.)
GEOMETRIC_REPRESENTATION_ITEM()
RATIONAL_B_SPLINE_SURFACE(((0.990658108926708,0.993760979299921,0.999878046252916),
(0.990658108926708,0.993760979299921,0.999878046252916)))
REPRESENTATION_ITEM('')
SURFACE()
);
#3083=(
BOUNDED_SURFACE()
B_SPLINE_SURFACE(1,2,((#146428,#146429,#146430,#146431,#146432),(#146433,
#146434,#146435,#146436,#146437)),.UNSPECIFIED.,.F.,.F.,.F.)
B_SPLINE_SURFACE_WITH_KNOTS((2,2),(3,2,3),(0.709728555987099,1.),(0.590808523385636,
0.607982157956012,0.608572517849034),.UNSPECIFIED.)
GEOMETRIC_REPRESENTATION_ITEM()
RATIONAL_B_SPLINE_SURFACE(((0.990086238235256,0.987329216372183,0.987470879370255,
0.987470879370255,0.987470879370255),(0.990086238235256,0.987329216372183,
0.987470879370255,0.987470879370255,0.987470879370255)))
REPRESENTATION_ITEM('')
SURFACE()
);
#3084=(
BOUNDED_SURFACE()
B_SPLINE_SURFACE(1,2,((#146448,#146449,#146450),(#146451,#146452,#146453)),
 .UNSPECIFIED.,.F.,.F.,.F.)
B_SPLINE_SURFACE_WITH_KNOTS((2,2),(3,3),(0.710192959007309,1.),(0.125170525609407,
0.142682999576235),.UNSPECIFIED.)
GEOMETRIC_REPRESENTATION_ITEM()
RATIONAL_B_SPLINE_SURFACE(((0.990658108926708,0.993760979299921,0.999878046252916),
(0.990658108926708,0.993760979299921,0.999878046252916)))
REPRESENTATION_ITEM('')
SURFACE()
);
#3085=(
BOUNDED_SURFACE()
B_SPLINE_SURFACE(1,2,((#146461,#146462,#146463,#146464,#146465),(#146466,
#146467,#146468,#146469,#146470)),.UNSPECIFIED.,.F.,.F.,.F.)
B_SPLINE_SURFACE_WITH_KNOTS((2,2),(3,2,3),(0.709728555962953,1.),(0.590808523385636,
0.607982157956012,0.608572517871884),.UNSPECIFIED.)
GEOMETRIC_REPRESENTATION_ITEM()
RATIONAL_B_SPLINE_SURFACE(((0.990086238235256,0.987329216372183,0.987470879370255,
0.987470879370255,0.987470879370255),(0.990086238235256,0.987329216372183,
0.987470879370255,0.987470879370255,0.987470879370255)))
REPRESENTATION_ITEM('')
SURFACE()
);
#3086=(
BOUNDED_SURFACE()
B_SPLINE_SURFACE(1,2,((#146481,#146482,#146483),(#146484,#146485,#146486)),
 .UNSPECIFIED.,.F.,.F.,.F.)
B_SPLINE_SURFACE_WITH_KNOTS((2,2),(3,3),(0.710192959006066,1.),(0.125170525609408,
0.142682999576235),.UNSPECIFIED.)
GEOMETRIC_REPRESENTATION_ITEM()
RATIONAL_B_SPLINE_SURFACE(((0.990658108926709,0.993760979299921,0.999878046252916),
(0.990658108926709,0.993760979299921,0.999878046252916)))
REPRESENTATION_ITEM('')
SURFACE()
);
#3087=(
BOUNDED_SURFACE()
B_SPLINE_SURFACE(1,2,((#146494,#146495,#146496,#146497,#146498),(#146499,
#146500,#146501,#146502,#146503)),.UNSPECIFIED.,.F.,.F.,.F.)
B_SPLINE_SURFACE_WITH_KNOTS((2,2),(3,2,3),(0.709728555944512,1.),(0.590808523385635,
0.607982157956011,0.608572517850343),.UNSPECIFIED.)
GEOMETRIC_REPRESENTATION_ITEM()
RATIONAL_B_SPLINE_SURFACE(((0.990086238235256,0.987329216372183,0.987470879370255,
0.987470879370255,0.987470879370255),(0.990086238235256,0.987329216372183,
0.987470879370255,0.987470879370255,0.987470879370255)))
REPRESENTATION_ITEM('')
SURFACE()
);
#3088=(
BOUNDED_SURFACE()
B_SPLINE_SURFACE(1,2,((#146514,#146515,#146516),(#146517,#146518,#146519)),
 .UNSPECIFIED.,.F.,.F.,.F.)
B_SPLINE_SURFACE_WITH_KNOTS((2,2),(3,3),(0.710192959008445,1.),(0.125170525609408,
0.142682999576236),.UNSPECIFIED.)
GEOMETRIC_REPRESENTATION_ITEM()
RATIONAL_B_SPLINE_SURFACE(((0.990658108926709,0.993760979299921,0.999878046252917),
(0.990658108926709,0.993760979299921,0.999878046252917)))
REPRESENTATION_ITEM('')
SURFACE()
);
#3089=(
BOUNDED_SURFACE()
B_SPLINE_SURFACE(1,2,((#146527,#146528,#146529,#146530,#146531),(#146532,
#146533,#146534,#146535,#146536)),.UNSPECIFIED.,.F.,.F.,.F.)
B_SPLINE_SURFACE_WITH_KNOTS((2,2),(3,2,3),(0.709728555951602,1.),(0.590808523385635,
0.607982157956011,0.608572517843256),.UNSPECIFIED.)
GEOMETRIC_REPRESENTATION_ITEM()
RATIONAL_B_SPLINE_SURFACE(((0.990086238235256,0.987329216372183,0.987470879370255,
0.987470879370255,0.987470879370255),(0.990086238235256,0.987329216372183,
0.987470879370255,0.987470879370255,0.987470879370255)))
REPRESENTATION_ITEM('')
SURFACE()
);
#3090=(
BOUNDED_SURFACE()
B_SPLINE_SURFACE(1,2,((#146547,#146548,#146549),(#146550,#146551,#146552)),
 .UNSPECIFIED.,.F.,.F.,.F.)
B_SPLINE_SURFACE_WITH_KNOTS((2,2),(3,3),(0.710192959008442,1.),(0.125170525609408,
0.142682999576236),.UNSPECIFIED.)
GEOMETRIC_REPRESENTATION_ITEM()
RATIONAL_B_SPLINE_SURFACE(((0.990658108926709,0.993760979299921,0.999878046252917),
(0.990658108926709,0.993760979299921,0.999878046252917)))
REPRESENTATION_ITEM('')
SURFACE()
);
#3091=(
BOUNDED_SURFACE()
B_SPLINE_SURFACE(1,2,((#146560,#146561,#146562,#146563,#146564),(#146565,
#146566,#146567,#146568,#146569)),.UNSPECIFIED.,.F.,.F.,.F.)
B_SPLINE_SURFACE_WITH_KNOTS((2,2),(3,2,3),(0.70972855596089,1.),(0.590808523385635,
0.607982157956011,0.608572517833635),.UNSPECIFIED.)
GEOMETRIC_REPRESENTATION_ITEM()
RATIONAL_B_SPLINE_SURFACE(((0.990086238235256,0.987329216372183,0.987470879370256,
0.987470879370256,0.987470879370256),(0.990086238235256,0.987329216372183,
0.987470879370256,0.987470879370256,0.987470879370256)))
REPRESENTATION_ITEM('')
SURFACE()
);
#3092=(
BOUNDED_SURFACE()
B_SPLINE_SURFACE(1,2,((#146580,#146581,#146582),(#146583,#146584,#146585)),
 .UNSPECIFIED.,.F.,.F.,.F.)
B_SPLINE_SURFACE_WITH_KNOTS((2,2),(3,3),(0.71019295900811,1.),(0.125170525609408,
0.142682999576236),.UNSPECIFIED.)
GEOMETRIC_REPRESENTATION_ITEM()
RATIONAL_B_SPLINE_SURFACE(((0.990658108926709,0.993760979299922,0.999878046252917),
(0.990658108926709,0.993760979299922,0.999878046252917)))
REPRESENTATION_ITEM('')
SURFACE()
);
#3093=(
BOUNDED_SURFACE()
B_SPLINE_SURFACE(1,2,((#146599,#146600,#146601,#146602,#146603),(#146604,
#146605,#146606,#146607,#146608)),.UNSPECIFIED.,.F.,.F.,.F.)
B_SPLINE_SURFACE_WITH_KNOTS((2,2),(3,2,3),(0.709728555969186,1.),(0.590808523385635,
0.607982157956011,0.608572517825209),.UNSPECIFIED.)
GEOMETRIC_REPRESENTATION_ITEM()
RATIONAL_B_SPLINE_SURFACE(((0.990086238235256,0.987329216372183,0.987470879370256,
0.987470879370256,0.987470879370256),(0.990086238235256,0.987329216372183,
0.987470879370256,0.987470879370256,0.987470879370256)))
REPRESENTATION_ITEM('')
SURFACE()
);
#3094=(
BOUNDED_SURFACE()
B_SPLINE_SURFACE(1,2,((#146610,#146611,#146612,#146613,#146614),(#146615,
#146616,#146617,#146618,#146619)),.UNSPECIFIED.,.F.,.F.,.F.)
B_SPLINE_SURFACE_WITH_KNOTS((2,2),(3,2,3),(0.709729983312017,1.),(0.159799014184144,
0.176967058622922,0.177555991154001),.UNSPECIFIED.)
GEOMETRIC_REPRESENTATION_ITEM()
RATIONAL_B_SPLINE_SURFACE(((0.990927469170768,0.987759962570789,0.98748925405691,
0.98748925405691,0.98748925405691),(0.990927469170768,0.987759962570789,
0.98748925405691,0.98748925405691,0.98748925405691)))
REPRESENTATION_ITEM('')
SURFACE()
);
#3095=(
BOUNDED_SURFACE()
B_SPLINE_SURFACE(1,2,((#146635,#146636,#146637,#146638,#146639,#146640,
#146641),(#146642,#146643,#146644,#146645,#146646,#146647,#146648)),
 .UNSPECIFIED.,.F.,.F.,.F.)
B_SPLINE_SURFACE_WITH_KNOTS((2,2),(3,2,2,3),(0.710192959008444,1.),(0.556037361265319,
0.556212823028861,0.571428571428571,0.573758999383056),.UNSPECIFIED.)
GEOMETRIC_REPRESENTATION_ITEM()
RATIONAL_B_SPLINE_SURFACE(((0.991593692313265,0.991593692313265,0.991593692313265,
0.994659131878645,1.,0.999181998279397,0.998417372792936),(0.991593692313265,
0.991593692313265,0.991593692313265,0.994659131878644,1.,0.999181998279397,
0.998417372792936)))
REPRESENTATION_ITEM('')
SURFACE()
);
#3096=(
BOUNDED_SURFACE()
B_SPLINE_SURFACE(1,2,((#146670,#146671,#146672,#146673,#146674),(#146675,
#146676,#146677,#146678,#146679)),.UNSPECIFIED.,.F.,.F.,.F.)
B_SPLINE_SURFACE_WITH_KNOTS((2,2),(3,2,3),(0.709729983378474,1.),(0.159799014184072,
0.176967058622925,0.177555991087653),.UNSPECIFIED.)
GEOMETRIC_REPRESENTATION_ITEM()
RATIONAL_B_SPLINE_SURFACE(((0.990927469170795,0.98775996257079,0.98748925405691,
0.98748925405691,0.98748925405691),(0.990927469170795,0.98775996257079,
0.98748925405691,0.98748925405691,0.98748925405691)))
REPRESENTATION_ITEM('')
SURFACE()
);
#3097=(
BOUNDED_SURFACE()
B_SPLINE_SURFACE(1,2,((#146681,#146682,#146683,#146684,#146685,#146686,
#146687),(#146688,#146689,#146690,#146691,#146692,#146693,#146694)),
 .UNSPECIFIED.,.F.,.F.,.F.)
B_SPLINE_SURFACE_WITH_KNOTS((2,2),(3,2,2,3),(0.710192959008435,1.),(0.556037361265319,
0.556212823028861,0.571428571428571,0.573758999383057),.UNSPECIFIED.)
GEOMETRIC_REPRESENTATION_ITEM()
RATIONAL_B_SPLINE_SURFACE(((0.991593692313265,0.991593692313265,0.991593692313265,
0.994659131878645,1.,0.999181998279397,0.998417372792936),(0.991593692313265,
0.991593692313265,0.991593692313265,0.994659131878645,1.,0.999181998279397,
0.998417372792936)))
REPRESENTATION_ITEM('')
SURFACE()
);
#3098=(
BOUNDED_SURFACE()
B_SPLINE_SURFACE(1,2,((#146711,#146712,#146713,#146714,#146715),(#146716,
#146717,#146718,#146719,#146720)),.UNSPECIFIED.,.F.,.F.,.F.)
B_SPLINE_SURFACE_WITH_KNOTS((2,2),(3,2,3),(0.709729983387492,1.),(0.15979901418427,
0.176967058622921,0.177555991079107),.UNSPECIFIED.)
GEOMETRIC_REPRESENTATION_ITEM()
RATIONAL_B_SPLINE_SURFACE(((0.990927469170722,0.987759962570788,0.98748925405691,
0.98748925405691,0.98748925405691),(0.990927469170722,0.987759962570788,
0.98748925405691,0.98748925405691,0.98748925405691)))
REPRESENTATION_ITEM('')
SURFACE()
);
#3099=(
BOUNDED_SURFACE()
B_SPLINE_SURFACE(1,2,((#146722,#146723,#146724,#146725,#146726,#146727,
#146728),(#146729,#146730,#146731,#146732,#146733,#146734,#146735)),
 .UNSPECIFIED.,.F.,.F.,.F.)
B_SPLINE_SURFACE_WITH_KNOTS((2,2),(3,2,2,3),(0.710192959008441,1.),(0.55603736126532,
0.556212823028862,0.571428571428571,0.573758999383058),.UNSPECIFIED.)
GEOMETRIC_REPRESENTATION_ITEM()
RATIONAL_B_SPLINE_SURFACE(((0.991593692313266,0.991593692313266,0.991593692313266,
0.994659131878645,1.,0.999181998279397,0.998417372792936),(0.991593692313266,
0.991593692313266,0.991593692313266,0.994659131878645,1.,0.999181998279397,
0.998417372792936)))
REPRESENTATION_ITEM('')
SURFACE()
);
#3100=(
BOUNDED_SURFACE()
B_SPLINE_SURFACE(1,2,((#146761,#146762,#146763,#146764,#146765),(#146766,
#146767,#146768,#146769,#146770)),.UNSPECIFIED.,.F.,.F.,.F.)
B_SPLINE_SURFACE_WITH_KNOTS((2,2),(3,2,3),(0.709729983410559,1.),(0.159799014184008,
0.176967058622921,0.177555991055812),.UNSPECIFIED.)
GEOMETRIC_REPRESENTATION_ITEM()
RATIONAL_B_SPLINE_SURFACE(((0.990927469170818,0.987759962570791,0.98748925405691,
0.98748925405691,0.98748925405691),(0.990927469170818,0.987759962570792,
0.98748925405691,0.98748925405691,0.98748925405691)))
REPRESENTATION_ITEM('')
SURFACE()
);
#3101=(
BOUNDED_SURFACE()
B_SPLINE_SURFACE(1,2,((#146772,#146773,#146774,#146775,#146776,#146777,
#146778),(#146779,#146780,#146781,#146782,#146783,#146784,#146785)),
 .UNSPECIFIED.,.F.,.F.,.F.)
B_SPLINE_SURFACE_WITH_KNOTS((2,2),(3,2,2,3),(0.710192959008438,1.),(0.55603736126532,
0.556212823028862,0.571428571428571,0.573758999383057),.UNSPECIFIED.)
GEOMETRIC_REPRESENTATION_ITEM()
RATIONAL_B_SPLINE_SURFACE(((0.991593692313266,0.991593692313266,0.991593692313266,
0.994659131878645,1.,0.999181998279397,0.998417372792936),(0.991593692313266,
0.991593692313266,0.991593692313266,0.994659131878645,1.,0.999181998279397,
0.998417372792936)))
REPRESENTATION_ITEM('')
SURFACE()
);
#3102=(
BOUNDED_SURFACE()
B_SPLINE_SURFACE(1,2,((#146802,#146803,#146804,#146805,#146806),(#146807,
#146808,#146809,#146810,#146811)),.UNSPECIFIED.,.F.,.F.,.F.)
B_SPLINE_SURFACE_WITH_KNOTS((2,2),(3,2,3),(0.709729983402952,1.),(0.159799014184145,
0.176967058622924,0.177555991063508),.UNSPECIFIED.)
GEOMETRIC_REPRESENTATION_ITEM()
RATIONAL_B_SPLINE_SURFACE(((0.990927469170767,0.987759962570789,0.98748925405691,
0.98748925405691,0.98748925405691),(0.990927469170767,0.987759962570789,
0.98748925405691,0.98748925405691,0.98748925405691)))
REPRESENTATION_ITEM('')
SURFACE()
);
#3103=(
BOUNDED_SURFACE()
B_SPLINE_SURFACE(1,2,((#146813,#146814,#146815,#146816,#146817,#146818,
#146819),(#146820,#146821,#146822,#146823,#146824,#146825,#146826)),
 .UNSPECIFIED.,.F.,.F.,.F.)
B_SPLINE_SURFACE_WITH_KNOTS((2,2),(3,2,2,3),(0.710192959008438,1.),(0.55603736126532,
0.556212823028862,0.571428571428571,0.573758999383058),.UNSPECIFIED.)
GEOMETRIC_REPRESENTATION_ITEM()
RATIONAL_B_SPLINE_SURFACE(((0.991593692313266,0.991593692313266,0.991593692313266,
0.994659131878645,1.,0.999181998279397,0.998417372792936),(0.991593692313266,
0.991593692313266,0.991593692313266,0.994659131878645,1.,0.999181998279397,
0.998417372792936)))
REPRESENTATION_ITEM('')
SURFACE()
);
#3104=(
BOUNDED_SURFACE()
B_SPLINE_SURFACE(1,2,((#146843,#146844,#146845,#146846,#146847),(#146848,
#146849,#146850,#146851,#146852)),.UNSPECIFIED.,.F.,.F.,.F.)
B_SPLINE_SURFACE_WITH_KNOTS((2,2),(3,2,3),(0.709729983374391,1.),(0.159799014184268,
0.176967058622924,0.177555991091671),.UNSPECIFIED.)
GEOMETRIC_REPRESENTATION_ITEM()
RATIONAL_B_SPLINE_SURFACE(((0.990927469170722,0.987759962570787,0.98748925405691,
0.98748925405691,0.98748925405691),(0.990927469170722,0.987759962570787,
0.98748925405691,0.98748925405691,0.98748925405691)))
REPRESENTATION_ITEM('')
SURFACE()
);
#3105=(
BOUNDED_SURFACE()
B_SPLINE_SURFACE(1,2,((#146854,#146855,#146856,#146857,#146858,#146859,
#146860),(#146861,#146862,#146863,#146864,#146865,#146866,#146867)),
 .UNSPECIFIED.,.F.,.F.,.F.)
B_SPLINE_SURFACE_WITH_KNOTS((2,2),(3,2,2,3),(0.710192959008442,1.),(0.55603736126532,
0.556212823028862,0.571428571428571,0.573758999383058),.UNSPECIFIED.)
GEOMETRIC_REPRESENTATION_ITEM()
RATIONAL_B_SPLINE_SURFACE(((0.991593692313266,0.991593692313266,0.991593692313266,
0.994659131878645,1.,0.999181998279397,0.998417372792936),(0.991593692313266,
0.991593692313266,0.991593692313266,0.994659131878645,1.,0.999181998279397,
0.998417372792936)))
REPRESENTATION_ITEM('')
SURFACE()
);
#3106=(
BOUNDED_SURFACE()
B_SPLINE_SURFACE(1,2,((#146893,#146894,#146895,#146896,#146897),(#146898,
#146899,#146900,#146901,#146902)),.UNSPECIFIED.,.F.,.F.,.F.)
B_SPLINE_SURFACE_WITH_KNOTS((2,2),(3,2,3),(0.709729983359613,1.),(0.159799014184268,
0.176967058622921,0.177555991106485),.UNSPECIFIED.)
GEOMETRIC_REPRESENTATION_ITEM()
RATIONAL_B_SPLINE_SURFACE(((0.990927469170722,0.987759962570787,0.98748925405691,
0.98748925405691,0.98748925405691),(0.990927469170722,0.987759962570787,
0.98748925405691,0.98748925405691,0.98748925405691)))
REPRESENTATION_ITEM('')
SURFACE()
);
#3107=(
BOUNDED_SURFACE()
B_SPLINE_SURFACE(1,2,((#146904,#146905,#146906,#146907,#146908,#146909,
#146910),(#146911,#146912,#146913,#146914,#146915,#146916,#146917)),
 .UNSPECIFIED.,.F.,.F.,.F.)
B_SPLINE_SURFACE_WITH_KNOTS((2,2),(3,2,2,3),(0.71019295900844,1.),(0.55603736126532,
0.556212823028862,0.571428571428571,0.573758999383058),.UNSPECIFIED.)
GEOMETRIC_REPRESENTATION_ITEM()
RATIONAL_B_SPLINE_SURFACE(((0.991593692313266,0.991593692313266,0.991593692313266,
0.994659131878645,1.,0.999181998279397,0.998417372792936),(0.991593692313266,
0.991593692313266,0.991593692313266,0.994659131878645,1.,0.999181998279397,
0.998417372792936)))
REPRESENTATION_ITEM('')
SURFACE()
);
#3108=(
BOUNDED_SURFACE()
B_SPLINE_SURFACE(1,2,((#146943,#146944,#146945,#146946,#146947),(#146948,
#146949,#146950,#146951,#146952)),.UNSPECIFIED.,.F.,.F.,.F.)
B_SPLINE_SURFACE_WITH_KNOTS((2,2),(3,2,3),(0.710058121447169,1.),(0.159799014184268,
0.176967058622924,0.177227853019055),.UNSPECIFIED.)
GEOMETRIC_REPRESENTATION_ITEM()
RATIONAL_B_SPLINE_SURFACE(((0.990927469170722,0.987759962570787,0.98748925405691,
0.98748925405691,0.98748925405691),(0.990927469170722,0.987759962570787,
0.98748925405691,0.98748925405691,0.98748925405691)))
REPRESENTATION_ITEM('')
SURFACE()
);
#3109=(
BOUNDED_SURFACE()
B_SPLINE_SURFACE(1,2,((#146954,#146955,#146956,#146957,#146958,#146959,
#146960),(#146961,#146962,#146963,#146964,#146965,#146966,#146967)),
 .UNSPECIFIED.,.F.,.F.,.F.)
B_SPLINE_SURFACE_WITH_KNOTS((2,2),(3,2,2,3),(0.710192959008443,1.),(0.55603736126532,
0.556212823028862,0.571428571428571,0.573758999383058),.UNSPECIFIED.)
GEOMETRIC_REPRESENTATION_ITEM()
RATIONAL_B_SPLINE_SURFACE(((0.991593692313266,0.991593692313266,0.991593692313266,
0.994659131878645,1.,0.999181998279397,0.998417372792936),(0.991593692313266,
0.991593692313266,0.991593692313266,0.994659131878645,1.,0.999181998279397,
0.998417372792936)))
REPRESENTATION_ITEM('')
SURFACE()
);
#3110=(
BOUNDED_SURFACE()
B_SPLINE_SURFACE(1,2,((#146992,#146993,#146994,#146995,#146996),(#146997,
#146998,#146999,#147000,#147001)),.UNSPECIFIED.,.F.,.F.,.F.)
B_SPLINE_SURFACE_WITH_KNOTS((2,2),(3,2,3),(0.709729983365709,1.),(0.159799014184269,
0.176967058622924,0.177555991099995),.UNSPECIFIED.)
GEOMETRIC_REPRESENTATION_ITEM()
RATIONAL_B_SPLINE_SURFACE(((0.990927469170722,0.987759962570787,0.98748925405691,
0.98748925405691,0.98748925405691),(0.990927469170722,0.987759962570787,
0.98748925405691,0.98748925405691,0.98748925405691)))
REPRESENTATION_ITEM('')
SURFACE()
);
#3111=(
BOUNDED_SURFACE()
B_SPLINE_SURFACE(1,2,((#147003,#147004,#147005,#147006,#147007,#147008,
#147009),(#147010,#147011,#147012,#147013,#147014,#147015,#147016)),
 .UNSPECIFIED.,.F.,.F.,.F.)
B_SPLINE_SURFACE_WITH_KNOTS((2,2),(3,2,2,3),(0.710192959008441,1.),(0.55603736126532,
0.556212823028862,0.571428571428571,0.573758999383058),.UNSPECIFIED.)
GEOMETRIC_REPRESENTATION_ITEM()
RATIONAL_B_SPLINE_SURFACE(((0.991593692313266,0.991593692313266,0.991593692313266,
0.994659131878645,1.,0.999181998279397,0.998417372792936),(0.991593692313266,
0.991593692313266,0.991593692313266,0.994659131878645,1.,0.999181998279397,
0.998417372792936)))
REPRESENTATION_ITEM('')
SURFACE()
);
#3112=(
BOUNDED_SURFACE()
B_SPLINE_SURFACE(1,2,((#147041,#147042,#147043,#147044,#147045),(#147046,
#147047,#147048,#147049,#147050)),.UNSPECIFIED.,.F.,.F.,.F.)
B_SPLINE_SURFACE_WITH_KNOTS((2,2),(3,2,3),(0.709729983361247,1.),(0.159799014184269,
0.176967058622924,0.177555991104612),.UNSPECIFIED.)
GEOMETRIC_REPRESENTATION_ITEM()
RATIONAL_B_SPLINE_SURFACE(((0.990927469170722,0.987759962570787,0.98748925405691,
0.98748925405691,0.98748925405691),(0.990927469170722,0.987759962570787,
0.98748925405691,0.98748925405691,0.98748925405691)))
REPRESENTATION_ITEM('')
SURFACE()
);
#3113=(
BOUNDED_SURFACE()
B_SPLINE_SURFACE(1,2,((#147052,#147053,#147054,#147055,#147056,#147057,
#147058),(#147059,#147060,#147061,#147062,#147063,#147064,#147065)),
 .UNSPECIFIED.,.F.,.F.,.F.)
B_SPLINE_SURFACE_WITH_KNOTS((2,2),(3,2,2,3),(0.71019295900844,1.),(0.556037361265321,
0.556212823028862,0.571428571428571,0.573758999382983),.UNSPECIFIED.)
GEOMETRIC_REPRESENTATION_ITEM()
RATIONAL_B_SPLINE_SURFACE(((0.991593692313266,0.991593692313266,0.991593692313266,
0.994659131878645,1.,0.999181998279423,0.998417372792985),(0.991593692313266,
0.991593692313266,0.991593692313266,0.994659131878645,1.,0.999181998279423,
0.998417372792985)))
REPRESENTATION_ITEM('')
SURFACE()
);
#3114=(
BOUNDED_SURFACE()
B_SPLINE_SURFACE(1,2,((#147091,#147092,#147093,#147094,#147095),(#147096,
#147097,#147098,#147099,#147100)),.UNSPECIFIED.,.F.,.F.,.F.)
B_SPLINE_SURFACE_WITH_KNOTS((2,2),(3,2,3),(0.709729983382268,1.),(0.159799014184052,
0.176967058622924,0.177555991084222),.UNSPECIFIED.)
GEOMETRIC_REPRESENTATION_ITEM()
RATIONAL_B_SPLINE_SURFACE(((0.990927469170802,0.98775996257079,0.98748925405691,
0.98748925405691,0.98748925405691),(0.990927469170802,0.98775996257079,
0.98748925405691,0.98748925405691,0.98748925405691)))
REPRESENTATION_ITEM('')
SURFACE()
);
#3115=(
BOUNDED_SURFACE()
B_SPLINE_SURFACE(1,2,((#147102,#147103,#147104,#147105,#147106,#147107,
#147108),(#147109,#147110,#147111,#147112,#147113,#147114,#147115)),
 .UNSPECIFIED.,.F.,.F.,.F.)
B_SPLINE_SURFACE_WITH_KNOTS((2,2),(3,2,2,3),(0.71019295900844,1.),(0.55603736126532,
0.556212823028862,0.571428571428571,0.573758999383058),.UNSPECIFIED.)
GEOMETRIC_REPRESENTATION_ITEM()
RATIONAL_B_SPLINE_SURFACE(((0.991593692313266,0.991593692313266,0.991593692313266,
0.994659131878645,1.,0.999181998279397,0.998417372792936),(0.991593692313266,
0.991593692313266,0.991593692313266,0.994659131878645,1.,0.999181998279397,
0.998417372792936)))
REPRESENTATION_ITEM('')
SURFACE()
);
#3116=(
BOUNDED_SURFACE()
B_SPLINE_SURFACE(1,2,((#147132,#147133,#147134,#147135,#147136),(#147137,
#147138,#147139,#147140,#147141)),.UNSPECIFIED.,.F.,.F.,.F.)
B_SPLINE_SURFACE_WITH_KNOTS((2,2),(3,2,3),(0.709729983363911,1.),(0.159799014184268,
0.176967058622924,0.177555991102057),.UNSPECIFIED.)
GEOMETRIC_REPRESENTATION_ITEM()
RATIONAL_B_SPLINE_SURFACE(((0.990927469170722,0.987759962570787,0.98748925405691,
0.98748925405691,0.98748925405691),(0.990927469170722,0.987759962570787,
0.98748925405691,0.98748925405691,0.98748925405691)))
REPRESENTATION_ITEM('')
SURFACE()
);
#3117=(
BOUNDED_SURFACE()
B_SPLINE_SURFACE(1,2,((#147143,#147144,#147145,#147146,#147147,#147148,
#147149),(#147150,#147151,#147152,#147153,#147154,#147155,#147156)),
 .UNSPECIFIED.,.F.,.F.,.F.)
B_SPLINE_SURFACE_WITH_KNOTS((2,2),(3,2,2,3),(0.710192959008439,1.),(0.55603736126532,
0.556212823028862,0.571428571428571,0.573758999383058),.UNSPECIFIED.)
GEOMETRIC_REPRESENTATION_ITEM()
RATIONAL_B_SPLINE_SURFACE(((0.991593692313266,0.991593692313266,0.991593692313266,
0.994659131878645,1.,0.999181998279397,0.998417372792936),(0.991593692313266,
0.991593692313266,0.991593692313266,0.994659131878645,1.,0.999181998279397,
0.998417372792936)))
REPRESENTATION_ITEM('')
SURFACE()
);
#3118=(
BOUNDED_SURFACE()
B_SPLINE_SURFACE(1,2,((#147182,#147183,#147184,#147185,#147186),(#147187,
#147188,#147189,#147190,#147191)),.UNSPECIFIED.,.F.,.F.,.F.)
B_SPLINE_SURFACE_WITH_KNOTS((2,2),(3,2,3),(0.709729983383673,1.),(0.159799014184268,
0.176967058622921,0.177555991082457),.UNSPECIFIED.)
GEOMETRIC_REPRESENTATION_ITEM()
RATIONAL_B_SPLINE_SURFACE(((0.990927469170722,0.987759962570787,0.98748925405691,
0.98748925405691,0.98748925405691),(0.990927469170722,0.987759962570787,
0.98748925405691,0.98748925405691,0.98748925405691)))
REPRESENTATION_ITEM('')
SURFACE()
);
#3119=(
BOUNDED_SURFACE()
B_SPLINE_SURFACE(1,2,((#147193,#147194,#147195,#147196,#147197,#147198,
#147199),(#147200,#147201,#147202,#147203,#147204,#147205,#147206)),
 .UNSPECIFIED.,.F.,.F.,.F.)
B_SPLINE_SURFACE_WITH_KNOTS((2,2),(3,2,2,3),(0.710192959008439,1.),(0.55603736126532,
0.556212823028862,0.571428571428571,0.573758999383058),.UNSPECIFIED.)
GEOMETRIC_REPRESENTATION_ITEM()
RATIONAL_B_SPLINE_SURFACE(((0.991593692313266,0.991593692313266,0.991593692313266,
0.994659131878645,1.,0.999181998279397,0.998417372792936),(0.991593692313266,
0.991593692313266,0.991593692313266,0.994659131878645,1.,0.999181998279397,
0.998417372792936)))
REPRESENTATION_ITEM('')
SURFACE()
);
#3120=(
BOUNDED_SURFACE()
B_SPLINE_SURFACE(1,2,((#147226,#147227,#147228,#147229,#147230),(#147231,
#147232,#147233,#147234,#147235)),.UNSPECIFIED.,.F.,.F.,.F.)
B_SPLINE_SURFACE_WITH_KNOTS((2,2),(3,2,3),(0.709729983356482,1.),(0.159799014184268,
0.176967058622921,0.177555991109801),.UNSPECIFIED.)
GEOMETRIC_REPRESENTATION_ITEM()
RATIONAL_B_SPLINE_SURFACE(((0.990927469170722,0.987759962570787,0.98748925405691,
0.98748925405691,0.98748925405691),(0.990927469170722,0.987759962570787,
0.98748925405691,0.98748925405691,0.98748925405691)))
REPRESENTATION_ITEM('')
SURFACE()
);
#3121=(
BOUNDED_SURFACE()
B_SPLINE_SURFACE(1,2,((#147237,#147238,#147239,#147240,#147241,#147242,
#147243),(#147244,#147245,#147246,#147247,#147248,#147249,#147250)),
 .UNSPECIFIED.,.F.,.F.,.F.)
B_SPLINE_SURFACE_WITH_KNOTS((2,2),(3,2,2,3),(0.710192959008445,1.),(0.55603736126532,
0.556212823028862,0.571428571428571,0.573758999383058),.UNSPECIFIED.)
GEOMETRIC_REPRESENTATION_ITEM()
RATIONAL_B_SPLINE_SURFACE(((0.991593692313266,0.991593692313266,0.991593692313266,
0.994659131878645,1.,0.999181998279397,0.998417372792936),(0.991593692313266,
0.991593692313266,0.991593692313266,0.994659131878645,1.,0.999181998279397,
0.998417372792936)))
REPRESENTATION_ITEM('')
SURFACE()
);
#3122=(
BOUNDED_SURFACE()
B_SPLINE_SURFACE(1,2,((#147272,#147273,#147274,#147275,#147276),(#147277,
#147278,#147279,#147280,#147281)),.UNSPECIFIED.,.F.,.F.,.F.)
B_SPLINE_SURFACE_WITH_KNOTS((2,2),(3,2,3),(0.709729983342325,1.),(0.159799014184269,
0.176967058622924,0.177555991123784),.UNSPECIFIED.)
GEOMETRIC_REPRESENTATION_ITEM()
RATIONAL_B_SPLINE_SURFACE(((0.990927469170722,0.987759962570787,0.98748925405691,
0.98748925405691,0.98748925405691),(0.990927469170722,0.987759962570787,
0.98748925405691,0.98748925405691,0.98748925405691)))
REPRESENTATION_ITEM('')
SURFACE()
);
#3123=(
BOUNDED_SURFACE()
B_SPLINE_SURFACE(1,2,((#147283,#147284,#147285,#147286,#147287,#147288,
#147289),(#147290,#147291,#147292,#147293,#147294,#147295,#147296)),
 .UNSPECIFIED.,.F.,.F.,.F.)
B_SPLINE_SURFACE_WITH_KNOTS((2,2),(3,2,2,3),(0.710192959008445,1.),(0.55603736126532,
0.556212823028862,0.571428571428571,0.573758999383058),.UNSPECIFIED.)
GEOMETRIC_REPRESENTATION_ITEM()
RATIONAL_B_SPLINE_SURFACE(((0.991593692313266,0.991593692313266,0.991593692313266,
0.994659131878645,1.,0.999181998279397,0.998417372792936),(0.991593692313266,
0.991593692313266,0.991593692313266,0.994659131878645,1.,0.999181998279397,
0.998417372792936)))
REPRESENTATION_ITEM('')
SURFACE()
);
#3124=(
BOUNDED_SURFACE()
B_SPLINE_SURFACE(1,2,((#147322,#147323,#147324,#147325,#147326),(#147327,
#147328,#147329,#147330,#147331)),.UNSPECIFIED.,.F.,.F.,.F.)
B_SPLINE_SURFACE_WITH_KNOTS((2,2),(3,2,3),(0.709729983366589,1.),(0.159799014184268,
0.176967058622921,0.177555991099152),.UNSPECIFIED.)
GEOMETRIC_REPRESENTATION_ITEM()
RATIONAL_B_SPLINE_SURFACE(((0.990927469170722,0.987759962570787,0.98748925405691,
0.98748925405691,0.98748925405691),(0.990927469170722,0.987759962570787,
0.98748925405691,0.98748925405691,0.98748925405691)))
REPRESENTATION_ITEM('')
SURFACE()
);
#3125=(
BOUNDED_SURFACE()
B_SPLINE_SURFACE(1,2,((#147333,#147334,#147335,#147336,#147337,#147338,
#147339),(#147340,#147341,#147342,#147343,#147344,#147345,#147346)),
 .UNSPECIFIED.,.F.,.F.,.F.)
B_SPLINE_SURFACE_WITH_KNOTS((2,2),(3,2,2,3),(0.710192959008445,1.),(0.55603736126532,
0.556212823028862,0.571428571428571,0.573758999383058),.UNSPECIFIED.)
GEOMETRIC_REPRESENTATION_ITEM()
RATIONAL_B_SPLINE_SURFACE(((0.991593692313266,0.991593692313266,0.991593692313266,
0.994659131878645,1.,0.999181998279397,0.998417372792936),(0.991593692313266,
0.991593692313266,0.991593692313266,0.994659131878645,1.,0.999181998279397,
0.998417372792936)))
REPRESENTATION_ITEM('')
SURFACE()
);
#3126=(
BOUNDED_SURFACE()
B_SPLINE_SURFACE(1,2,((#147368,#147369,#147370,#147371,#147372),(#147373,
#147374,#147375,#147376,#147377)),.UNSPECIFIED.,.F.,.F.,.F.)
B_SPLINE_SURFACE_WITH_KNOTS((2,2),(3,2,3),(0.70972998337526,1.),(0.159799014184269,
0.176967058622924,0.177555991090998),.UNSPECIFIED.)
GEOMETRIC_REPRESENTATION_ITEM()
RATIONAL_B_SPLINE_SURFACE(((0.990927469170722,0.987759962570787,0.98748925405691,
0.98748925405691,0.98748925405691),(0.990927469170722,0.987759962570787,
0.98748925405691,0.98748925405691,0.98748925405691)))
REPRESENTATION_ITEM('')
SURFACE()
);
#3127=(
BOUNDED_SURFACE()
B_SPLINE_SURFACE(1,2,((#147379,#147380,#147381,#147382,#147383,#147384,
#147385),(#147386,#147387,#147388,#147389,#147390,#147391,#147392)),
 .UNSPECIFIED.,.F.,.F.,.F.)
B_SPLINE_SURFACE_WITH_KNOTS((2,2),(3,2,2,3),(0.71019295900844,1.),(0.55603736126532,
0.556212823028862,0.571428571428571,0.573758999383058),.UNSPECIFIED.)
GEOMETRIC_REPRESENTATION_ITEM()
RATIONAL_B_SPLINE_SURFACE(((0.991593692313266,0.991593692313266,0.991593692313266,
0.994659131878645,1.,0.999181998279397,0.998417372792936),(0.991593692313266,
0.991593692313266,0.991593692313266,0.994659131878645,1.,0.999181998279397,
0.998417372792936)))
REPRESENTATION_ITEM('')
SURFACE()
);
#3128=(
BOUNDED_SURFACE()
B_SPLINE_SURFACE(1,2,((#147409,#147410,#147411,#147412,#147413),(#147414,
#147415,#147416,#147417,#147418)),.UNSPECIFIED.,.F.,.F.,.F.)
B_SPLINE_SURFACE_WITH_KNOTS((2,2),(3,2,3),(0.70972998336251,1.),(0.159799014184269,
0.176967058622924,0.177555991103904),.UNSPECIFIED.)
GEOMETRIC_REPRESENTATION_ITEM()
RATIONAL_B_SPLINE_SURFACE(((0.990927469170722,0.987759962570787,0.98748925405691,
0.98748925405691,0.98748925405691),(0.990927469170722,0.987759962570787,
0.98748925405691,0.98748925405691,0.98748925405691)))
REPRESENTATION_ITEM('')
SURFACE()
);
#3129=(
BOUNDED_SURFACE()
B_SPLINE_SURFACE(1,2,((#147420,#147421,#147422,#147423,#147424,#147425,
#147426),(#147427,#147428,#147429,#147430,#147431,#147432,#147433)),
 .UNSPECIFIED.,.F.,.F.,.F.)
B_SPLINE_SURFACE_WITH_KNOTS((2,2),(3,2,2,3),(0.710192959008445,1.),(0.55603736126532,
0.556212823028862,0.571428571428571,0.573758999383058),.UNSPECIFIED.)
GEOMETRIC_REPRESENTATION_ITEM()
RATIONAL_B_SPLINE_SURFACE(((0.991593692313266,0.991593692313266,0.991593692313266,
0.994659131878645,1.,0.999181998279397,0.998417372792936),(0.991593692313266,
0.991593692313266,0.991593692313266,0.994659131878645,1.,0.999181998279397,
0.998417372792936)))
REPRESENTATION_ITEM('')
SURFACE()
);
#3130=(
BOUNDED_SURFACE()
B_SPLINE_SURFACE(1,2,((#147455,#147456,#147457,#147458,#147459),(#147460,
#147461,#147462,#147463,#147464)),.UNSPECIFIED.,.F.,.F.,.F.)
B_SPLINE_SURFACE_WITH_KNOTS((2,2),(3,2,3),(0.709729983362568,1.),(0.159799014184268,
0.176967058622924,0.177555991103127),.UNSPECIFIED.)
GEOMETRIC_REPRESENTATION_ITEM()
RATIONAL_B_SPLINE_SURFACE(((0.990927469170722,0.987759962570787,0.98748925405691,
0.98748925405691,0.98748925405691),(0.990927469170722,0.987759962570787,
0.98748925405691,0.98748925405691,0.98748925405691)))
REPRESENTATION_ITEM('')
SURFACE()
);
#3131=(
BOUNDED_SURFACE()
B_SPLINE_SURFACE(1,2,((#147466,#147467,#147468,#147469,#147470,#147471,
#147472),(#147473,#147474,#147475,#147476,#147477,#147478,#147479)),
 .UNSPECIFIED.,.F.,.F.,.F.)
B_SPLINE_SURFACE_WITH_KNOTS((2,2),(3,2,2,3),(0.71019295900844,1.),(0.55603736126532,
0.556212823028862,0.571428571428571,0.573758999383058),.UNSPECIFIED.)
GEOMETRIC_REPRESENTATION_ITEM()
RATIONAL_B_SPLINE_SURFACE(((0.991593692313266,0.991593692313266,0.991593692313266,
0.994659131878645,1.,0.999181998279397,0.998417372792936),(0.991593692313266,
0.991593692313266,0.991593692313266,0.994659131878645,1.,0.999181998279397,
0.998417372792936)))
REPRESENTATION_ITEM('')
SURFACE()
);
#3132=(
BOUNDED_SURFACE()
B_SPLINE_SURFACE(1,2,((#147505,#147506,#147507,#147508,#147509),(#147510,
#147511,#147512,#147513,#147514)),.UNSPECIFIED.,.F.,.F.,.F.)
B_SPLINE_SURFACE_WITH_KNOTS((2,2),(3,2,3),(0.709729983342911,1.),(0.159799014184268,
0.176967058622921,0.177555991081652),.UNSPECIFIED.)
GEOMETRIC_REPRESENTATION_ITEM()
RATIONAL_B_SPLINE_SURFACE(((0.990927469170722,0.987759962570787,0.98748925405691,
0.98748925405691,0.98748925405691),(0.990927469170722,0.987759962570787,
0.98748925405691,0.98748925405691,0.98748925405691)))
REPRESENTATION_ITEM('')
SURFACE()
);
#3133=(
BOUNDED_SURFACE()
B_SPLINE_SURFACE(1,2,((#147516,#147517,#147518,#147519,#147520,#147521,
#147522),(#147523,#147524,#147525,#147526,#147527,#147528,#147529)),
 .UNSPECIFIED.,.F.,.F.,.F.)
B_SPLINE_SURFACE_WITH_KNOTS((2,2),(3,2,2,3),(0.710192959008303,1.),(0.55603736126532,
0.556212823028862,0.571428571428571,0.573758999383056),.UNSPECIFIED.)
GEOMETRIC_REPRESENTATION_ITEM()
RATIONAL_B_SPLINE_SURFACE(((0.991593692313266,0.991593692313266,0.991593692313266,
0.994659131878645,1.,0.999181998279397,0.998417372792937),(0.991593692313266,
0.991593692313266,0.991593692313266,0.994659131878645,1.,0.999181998279397,
0.998417372792937)))
REPRESENTATION_ITEM('')
SURFACE()
);
#3134=(
BOUNDED_SURFACE()
B_SPLINE_SURFACE(1,2,((#147551,#147552,#147553,#147554,#147555),(#147556,
#147557,#147558,#147559,#147560)),.UNSPECIFIED.,.F.,.F.,.F.)
B_SPLINE_SURFACE_WITH_KNOTS((2,2),(3,2,3),(0.709729983351992,1.),(0.159799014184233,
0.176967058622922,0.177555991114115),.UNSPECIFIED.)
GEOMETRIC_REPRESENTATION_ITEM()
RATIONAL_B_SPLINE_SURFACE(((0.990927469170735,0.987759962570788,0.98748925405691,
0.98748925405691,0.98748925405691),(0.990927469170735,0.987759962570788,
0.98748925405691,0.98748925405691,0.98748925405691)))
REPRESENTATION_ITEM('')
SURFACE()
);
#3135=(
BOUNDED_SURFACE()
B_SPLINE_SURFACE(1,2,((#147562,#147563,#147564,#147565,#147566,#147567,
#147568),(#147569,#147570,#147571,#147572,#147573,#147574,#147575)),
 .UNSPECIFIED.,.F.,.F.,.F.)
B_SPLINE_SURFACE_WITH_KNOTS((2,2),(3,2,2,3),(0.710192959008295,1.),(0.556037361265319,
0.556212823028861,0.571428571428571,0.573758999383057),.UNSPECIFIED.)
GEOMETRIC_REPRESENTATION_ITEM()
RATIONAL_B_SPLINE_SURFACE(((0.991593692313265,0.991593692313265,0.991593692313265,
0.994659131878645,1.,0.999181998279397,0.998417372792936),(0.991593692313265,
0.991593692313265,0.991593692313265,0.994659131878644,1.,0.999181998279397,
0.998417372792936)))
REPRESENTATION_ITEM('')
SURFACE()
);
#3136=(
BOUNDED_SURFACE()
B_SPLINE_SURFACE(1,2,((#147597,#147598,#147599,#147600,#147601),(#147602,
#147603,#147604,#147605,#147606)),.UNSPECIFIED.,.F.,.F.,.F.)
B_SPLINE_SURFACE_WITH_KNOTS((2,2),(3,2,3),(0.709729983356803,1.),(0.159799014184073,
0.176967058622922,0.177555991109014),.UNSPECIFIED.)
GEOMETRIC_REPRESENTATION_ITEM()
RATIONAL_B_SPLINE_SURFACE(((0.990927469170794,0.98775996257079,0.98748925405691,
0.98748925405691,0.98748925405691),(0.990927469170794,0.98775996257079,
0.98748925405691,0.98748925405691,0.98748925405691)))
REPRESENTATION_ITEM('')
SURFACE()
);
#3137=(
BOUNDED_SURFACE()
B_SPLINE_SURFACE(1,2,((#147608,#147609,#147610,#147611,#147612,#147613,
#147614),(#147615,#147616,#147617,#147618,#147619,#147620,#147621)),
 .UNSPECIFIED.,.F.,.F.,.F.)
B_SPLINE_SURFACE_WITH_KNOTS((2,2),(3,2,2,3),(0.710192959008051,1.),(0.556037361265319,
0.556212823028861,0.571428571428571,0.573758999383057),.UNSPECIFIED.)
GEOMETRIC_REPRESENTATION_ITEM()
RATIONAL_B_SPLINE_SURFACE(((0.991593692313265,0.991593692313265,0.991593692313265,
0.994659131878644,1.,0.999181998279397,0.998417372792936),(0.991593692313265,
0.991593692313265,0.991593692313265,0.994659131878644,1.,0.999181998279397,
0.998417372792936)))
REPRESENTATION_ITEM('')
SURFACE()
);
#3138=(
BOUNDED_SURFACE()
B_SPLINE_SURFACE(1,2,((#147647,#147648,#147649,#147650,#147651),(#147652,
#147653,#147654,#147655,#147656)),.UNSPECIFIED.,.F.,.F.,.F.)
B_SPLINE_SURFACE_WITH_KNOTS((2,2),(3,2,3),(0.709729983383856,1.),(0.159799014184014,
0.176967058622925,0.177555991081937),.UNSPECIFIED.)
GEOMETRIC_REPRESENTATION_ITEM()
RATIONAL_B_SPLINE_SURFACE(((0.990927469170816,0.98775996257079,0.98748925405691,
0.98748925405691,0.98748925405691),(0.990927469170816,0.987759962570791,
0.98748925405691,0.98748925405691,0.98748925405691)))
REPRESENTATION_ITEM('')
SURFACE()
);
#3139=(
BOUNDED_SURFACE()
B_SPLINE_SURFACE(1,2,((#147658,#147659,#147660,#147661,#147662,#147663,
#147664),(#147665,#147666,#147667,#147668,#147669,#147670,#147671)),
 .UNSPECIFIED.,.F.,.F.,.F.)
B_SPLINE_SURFACE_WITH_KNOTS((2,2),(3,2,2,3),(0.710192959006645,1.),(0.556037361265319,
0.556212823028861,0.571428571428571,0.573758999383057),.UNSPECIFIED.)
GEOMETRIC_REPRESENTATION_ITEM()
RATIONAL_B_SPLINE_SURFACE(((0.991593692313265,0.991593692313265,0.991593692313265,
0.994659131878645,1.,0.999181998279397,0.998417372792936),(0.991593692313265,
0.991593692313265,0.991593692313265,0.994659131878645,1.,0.999181998279397,
0.998417372792936)))
REPRESENTATION_ITEM('')
SURFACE()
);
#3140=(
BOUNDED_SURFACE()
B_SPLINE_SURFACE(1,2,((#147693,#147694,#147695,#147696,#147697),(#147698,
#147699,#147700,#147701,#147702)),.UNSPECIFIED.,.F.,.F.,.F.)
B_SPLINE_SURFACE_WITH_KNOTS((2,2),(3,2,3),(0.709729983386952,1.),(0.15979901418427,
0.176967058622922,0.177555991076872),.UNSPECIFIED.)
GEOMETRIC_REPRESENTATION_ITEM()
RATIONAL_B_SPLINE_SURFACE(((0.990927469170722,0.987759962570787,0.98748925405691,
0.98748925405691,0.98748925405691),(0.990927469170722,0.987759962570787,
0.98748925405691,0.98748925405691,0.98748925405691)))
REPRESENTATION_ITEM('')
SURFACE()
);
#3141=(
BOUNDED_SURFACE()
B_SPLINE_SURFACE(1,2,((#147704,#147705,#147706,#147707,#147708,#147709,
#147710),(#147711,#147712,#147713,#147714,#147715,#147716,#147717)),
 .UNSPECIFIED.,.F.,.F.,.F.)
B_SPLINE_SURFACE_WITH_KNOTS((2,2),(3,2,2,3),(0.710192959007974,1.),(0.556037361265319,
0.556212823028861,0.571428571428571,0.573758999383056),.UNSPECIFIED.)
GEOMETRIC_REPRESENTATION_ITEM()
RATIONAL_B_SPLINE_SURFACE(((0.991593692313265,0.991593692313265,0.991593692313265,
0.994659131878644,1.,0.999181998279397,0.998417372792936),(0.991593692313265,
0.991593692313265,0.991593692313265,0.994659131878644,1.,0.999181998279397,
0.998417372792936)))
REPRESENTATION_ITEM('')
SURFACE()
);
#3142=(
BOUNDED_SURFACE()
B_SPLINE_SURFACE(1,2,((#147743,#147744,#147745,#147746,#147747),(#147748,
#147749,#147750,#147751,#147752)),.UNSPECIFIED.,.F.,.F.,.F.)
B_SPLINE_SURFACE_WITH_KNOTS((2,2),(3,2,3),(0.709729983394837,1.),(0.159799014184242,
0.176967058622922,0.177555991070855),.UNSPECIFIED.)
GEOMETRIC_REPRESENTATION_ITEM()
RATIONAL_B_SPLINE_SURFACE(((0.990927469170732,0.987759962570788,0.98748925405691,
0.98748925405691,0.98748925405691),(0.990927469170732,0.987759962570788,
0.98748925405691,0.98748925405691,0.98748925405691)))
REPRESENTATION_ITEM('')
SURFACE()
);
#3143=(
BOUNDED_SURFACE()
B_SPLINE_SURFACE(1,2,((#147754,#147755,#147756,#147757,#147758,#147759,
#147760),(#147761,#147762,#147763,#147764,#147765,#147766,#147767)),
 .UNSPECIFIED.,.F.,.F.,.F.)
B_SPLINE_SURFACE_WITH_KNOTS((2,2),(3,2,2,3),(0.710192959008354,1.),(0.556037361265319,
0.556212823028861,0.571428571428571,0.573758999383057),.UNSPECIFIED.)
GEOMETRIC_REPRESENTATION_ITEM()
RATIONAL_B_SPLINE_SURFACE(((0.991593692313265,0.991593692313265,0.991593692313265,
0.994659131878645,1.,0.999181998279397,0.998417372792936),(0.991593692313265,
0.991593692313265,0.991593692313265,0.994659131878645,1.,0.999181998279397,
0.998417372792936)))
REPRESENTATION_ITEM('')
SURFACE()
);
#3144=(
BOUNDED_SURFACE()
B_SPLINE_SURFACE(1,2,((#147792,#147793,#147794,#147795,#147796),(#147797,
#147798,#147799,#147800,#147801)),.UNSPECIFIED.,.F.,.F.,.F.)
B_SPLINE_SURFACE_WITH_KNOTS((2,2),(3,2,3),(0.70972998337482,1.),(0.15979901418427,
0.176967058622925,0.177555991090709),.UNSPECIFIED.)
GEOMETRIC_REPRESENTATION_ITEM()
RATIONAL_B_SPLINE_SURFACE(((0.990927469170721,0.987759962570786,0.98748925405691,
0.98748925405691,0.98748925405691),(0.990927469170722,0.987759962570787,
0.98748925405691,0.98748925405691,0.98748925405691)))
REPRESENTATION_ITEM('')
SURFACE()
);
#3145=(
BOUNDED_SURFACE()
B_SPLINE_SURFACE(1,2,((#147803,#147804,#147805,#147806,#147807,#147808,
#147809),(#147810,#147811,#147812,#147813,#147814,#147815,#147816)),
 .UNSPECIFIED.,.F.,.F.,.F.)
B_SPLINE_SURFACE_WITH_KNOTS((2,2),(3,2,2,3),(0.710192959008358,1.),(0.556037361265319,
0.556212823028861,0.571428571428571,0.573758999383057),.UNSPECIFIED.)
GEOMETRIC_REPRESENTATION_ITEM()
RATIONAL_B_SPLINE_SURFACE(((0.991593692313265,0.991593692313265,0.991593692313265,
0.994659131878645,1.,0.999181998279397,0.998417372792936),(0.991593692313265,
0.991593692313265,0.991593692313265,0.994659131878645,1.,0.999181998279397,
0.998417372792936)))
REPRESENTATION_ITEM('')
SURFACE()
);
#3146=(
BOUNDED_SURFACE()
B_SPLINE_SURFACE(1,2,((#147842,#147843,#147844,#147845,#147846),(#147847,
#147848,#147849,#147850,#147851)),.UNSPECIFIED.,.F.,.F.,.F.)
B_SPLINE_SURFACE_WITH_KNOTS((2,2),(3,2,3),(0.709729983387421,1.),(0.15979901418427,
0.176967058622922,0.177555991078557),.UNSPECIFIED.)
GEOMETRIC_REPRESENTATION_ITEM()
RATIONAL_B_SPLINE_SURFACE(((0.990927469170721,0.987759962570787,0.98748925405691,
0.98748925405691,0.98748925405691),(0.990927469170721,0.987759962570787,
0.98748925405691,0.98748925405691,0.98748925405691)))
REPRESENTATION_ITEM('')
SURFACE()
);
#3147=(
BOUNDED_SURFACE()
B_SPLINE_SURFACE(1,2,((#147853,#147854,#147855,#147856,#147857,#147858,
#147859),(#147860,#147861,#147862,#147863,#147864,#147865,#147866)),
 .UNSPECIFIED.,.F.,.F.,.F.)
B_SPLINE_SURFACE_WITH_KNOTS((2,2),(3,2,2,3),(0.710192959008366,1.),(0.556037361265319,
0.556212823028861,0.571428571428571,0.573758999383057),.UNSPECIFIED.)
GEOMETRIC_REPRESENTATION_ITEM()
RATIONAL_B_SPLINE_SURFACE(((0.991593692313265,0.991593692313265,0.991593692313265,
0.994659131878644,1.,0.999181998279397,0.998417372792936),(0.991593692313265,
0.991593692313265,0.991593692313265,0.994659131878644,1.,0.999181998279397,
0.998417372792936)))
REPRESENTATION_ITEM('')
SURFACE()
);
#3148=(
BOUNDED_SURFACE()
B_SPLINE_SURFACE(1,2,((#147888,#147889,#147890,#147891,#147892),(#147893,
#147894,#147895,#147896,#147897)),.UNSPECIFIED.,.F.,.F.,.F.)
B_SPLINE_SURFACE_WITH_KNOTS((2,2),(3,2,3),(0.709729983360727,1.),(0.159799014183978,
0.176967058622922,0.177555991105049),.UNSPECIFIED.)
GEOMETRIC_REPRESENTATION_ITEM()
RATIONAL_B_SPLINE_SURFACE(((0.990927469170829,0.987759962570792,0.98748925405691,
0.98748925405691,0.98748925405691),(0.990927469170829,0.987759962570792,
0.98748925405691,0.98748925405691,0.98748925405691)))
REPRESENTATION_ITEM('')
SURFACE()
);
#3149=(
BOUNDED_SURFACE()
B_SPLINE_SURFACE(1,2,((#147899,#147900,#147901,#147902,#147903,#147904,
#147905),(#147906,#147907,#147908,#147909,#147910,#147911,#147912)),
 .UNSPECIFIED.,.F.,.F.,.F.)
B_SPLINE_SURFACE_WITH_KNOTS((2,2),(3,2,2,3),(0.710192959008086,1.),(0.556037361265319,
0.556212823028861,0.571428571428571,0.573758999383056),.UNSPECIFIED.)
GEOMETRIC_REPRESENTATION_ITEM()
RATIONAL_B_SPLINE_SURFACE(((0.991593692313265,0.991593692313265,0.991593692313265,
0.994659131878644,1.,0.999181998279397,0.998417372792937),(0.991593692313265,
0.991593692313265,0.991593692313265,0.994659131878644,1.,0.999181998279397,
0.998417372792937)))
REPRESENTATION_ITEM('')
SURFACE()
);
#3150=(
BOUNDED_SURFACE()
B_SPLINE_SURFACE(1,2,((#147938,#147939,#147940,#147941,#147942),(#147943,
#147944,#147945,#147946,#147947)),.UNSPECIFIED.,.F.,.F.,.F.)
B_SPLINE_SURFACE_WITH_KNOTS((2,2),(3,2,3),(0.709729983386537,1.),(0.159799014184215,
0.176967058622925,0.177555991079593),.UNSPECIFIED.)
GEOMETRIC_REPRESENTATION_ITEM()
RATIONAL_B_SPLINE_SURFACE(((0.990927469170742,0.987759962570788,0.98748925405691,
0.98748925405691,0.98748925405691),(0.990927469170742,0.987759962570788,
0.98748925405691,0.98748925405691,0.98748925405691)))
REPRESENTATION_ITEM('')
SURFACE()
);
#3151=(
BOUNDED_SURFACE()
B_SPLINE_SURFACE(1,2,((#147949,#147950,#147951,#147952,#147953,#147954,
#147955),(#147956,#147957,#147958,#147959,#147960,#147961,#147962)),
 .UNSPECIFIED.,.F.,.F.,.F.)
B_SPLINE_SURFACE_WITH_KNOTS((2,2),(3,2,2,3),(0.710192959008437,1.),(0.556037361265319,
0.556212823028861,0.571428571428571,0.573758999383056),.UNSPECIFIED.)
GEOMETRIC_REPRESENTATION_ITEM()
RATIONAL_B_SPLINE_SURFACE(((0.991593692313265,0.991593692313265,0.991593692313265,
0.994659131878644,1.,0.999181998279397,0.998417372792936),(0.991593692313265,
0.991593692313265,0.991593692313265,0.994659131878644,1.,0.999181998279397,
0.998417372792936)))
REPRESENTATION_ITEM('')
SURFACE()
);
#3152=(
BOUNDED_SURFACE()
B_SPLINE_SURFACE(1,2,((#147977,#147978,#147979),(#147980,#147981,#147982)),
 .UNSPECIFIED.,.F.,.F.,.F.)
B_SPLINE_SURFACE_WITH_KNOTS((2,2),(3,3),(0.,0.289807040992016),(0.607982157956011,
0.625273655815328),.UNSPECIFIED.)
GEOMETRIC_REPRESENTATION_ITEM()
RATIONAL_B_SPLINE_SURFACE(((0.987470879370255,0.987613514606721,0.990694758798812),
(0.987470879370255,0.987613514606721,0.990694758798812)))
REPRESENTATION_ITEM('')
SURFACE()
);
#3153=(
BOUNDED_SURFACE()
B_SPLINE_SURFACE(1,2,((#147991,#147992,#147993,#147994,#147995),(#147996,
#147997,#147998,#147999,#148000)),.UNSPECIFIED.,.F.,.F.,.F.)
B_SPLINE_SURFACE_WITH_KNOTS((2,2),(3,2,3),(0.,0.290280981347481),(0.107879027750091,
0.125170525609409,0.125770422812313),.UNSPECIFIED.)
GEOMETRIC_REPRESENTATION_ITEM()
RATIONAL_B_SPLINE_SURFACE(((0.987469282487682,0.987594391229382,0.990658108926709,
0.990658108926709,0.990658108926709),(0.987469282487682,0.987594391229382,
0.990658108926709,0.990658108926709,0.990658108926709)))
REPRESENTATION_ITEM('')
SURFACE()
);
#3154=(
BOUNDED_SURFACE()
B_SPLINE_SURFACE(1,2,((#148009,#148010,#148011),(#148012,#148013,#148014)),
 .UNSPECIFIED.,.F.,.F.,.F.)
B_SPLINE_SURFACE_WITH_KNOTS((2,2),(3,3),(0.,0.289807040992005),(0.607982157956011,
0.625273655815328),.UNSPECIFIED.)
GEOMETRIC_REPRESENTATION_ITEM()
RATIONAL_B_SPLINE_SURFACE(((0.987470879370255,0.98761351460672,0.990694758798812),
(0.987470879370256,0.987613514606721,0.990694758798812)))
REPRESENTATION_ITEM('')
SURFACE()
);
#3155=(
BOUNDED_SURFACE()
B_SPLINE_SURFACE(1,2,((#148016,#148017,#148018,#148019,#148020),(#148021,
#148022,#148023,#148024,#148025)),.UNSPECIFIED.,.F.,.F.,.F.)
B_SPLINE_SURFACE_WITH_KNOTS((2,2),(3,2,3),(0.,0.290280981348683),(0.107879027750092,
0.125170525609408,0.125770422854449),.UNSPECIFIED.)
GEOMETRIC_REPRESENTATION_ITEM()
RATIONAL_B_SPLINE_SURFACE(((0.987469282487682,0.987594391229382,0.990658108926709,
0.990658108926709,0.990658108926709),(0.987469282487682,0.987594391229382,
0.990658108926709,0.990658108926709,0.990658108926709)))
REPRESENTATION_ITEM('')
SURFACE()
);
#3156=(
BOUNDED_SURFACE()
B_SPLINE_SURFACE(1,2,((#148034,#148035,#148036),(#148037,#148038,#148039)),
 .UNSPECIFIED.,.F.,.F.,.F.)
B_SPLINE_SURFACE_WITH_KNOTS((2,2),(3,3),(0.,0.289807040991657),(0.607982157956011,
0.625273655815328),.UNSPECIFIED.)
GEOMETRIC_REPRESENTATION_ITEM()
RATIONAL_B_SPLINE_SURFACE(((0.987470879370255,0.98761351460672,0.990694758798812),
(0.987470879370256,0.987613514606721,0.990694758798812)))
REPRESENTATION_ITEM('')
SURFACE()
);
#3157=(
BOUNDED_SURFACE()
B_SPLINE_SURFACE(1,2,((#148041,#148042,#148043,#148044,#148045),(#148046,
#148047,#148048,#148049,#148050)),.UNSPECIFIED.,.F.,.F.,.F.)
B_SPLINE_SURFACE_WITH_KNOTS((2,2),(3,2,3),(0.,0.290280981345748),(0.107879027750092,
0.125170525609409,0.125770422850796),.UNSPECIFIED.)
GEOMETRIC_REPRESENTATION_ITEM()
RATIONAL_B_SPLINE_SURFACE(((0.987469282487682,0.987594391229382,0.990658108926709,
0.990658108926709,0.990658108926709),(0.987469282487682,0.987594391229382,
0.990658108926709,0.990658108926709,0.990658108926709)))
REPRESENTATION_ITEM('')
SURFACE()
);
#3158=(
BOUNDED_SURFACE()
B_SPLINE_SURFACE(1,2,((#148059,#148060,#148061),(#148062,#148063,#148064)),
 .UNSPECIFIED.,.F.,.F.,.F.)
B_SPLINE_SURFACE_WITH_KNOTS((2,2),(3,3),(0.,0.289807040991666),(0.607982157956011,
0.625273655815328),.UNSPECIFIED.)
GEOMETRIC_REPRESENTATION_ITEM()
RATIONAL_B_SPLINE_SURFACE(((0.987470879370255,0.98761351460672,0.990694758798812),
(0.987470879370256,0.987613514606721,0.990694758798812)))
REPRESENTATION_ITEM('')
SURFACE()
);
#3159=(
BOUNDED_SURFACE()
B_SPLINE_SURFACE(1,2,((#148066,#148067,#148068,#148069,#148070),(#148071,
#148072,#148073,#148074,#148075)),.UNSPECIFIED.,.F.,.F.,.F.)
B_SPLINE_SURFACE_WITH_KNOTS((2,2),(3,2,3),(0.,0.290280981338847),(0.107879027750092,
0.125170525609409,0.125770422803681),.UNSPECIFIED.)
GEOMETRIC_REPRESENTATION_ITEM()
RATIONAL_B_SPLINE_SURFACE(((0.987469282487682,0.987594391229382,0.990658108926709,
0.990658108926709,0.990658108926709),(0.987469282487682,0.987594391229382,
0.990658108926709,0.990658108926709,0.990658108926709)))
REPRESENTATION_ITEM('')
SURFACE()
);
#3160=(
BOUNDED_SURFACE()
B_SPLINE_SURFACE(1,2,((#148084,#148085,#148086),(#148087,#148088,#148089)),
 .UNSPECIFIED.,.F.,.F.,.F.)
B_SPLINE_SURFACE_WITH_KNOTS((2,2),(3,3),(0.,0.289807040992623),(0.607982157956011,
0.625273655815328),.UNSPECIFIED.)
GEOMETRIC_REPRESENTATION_ITEM()
RATIONAL_B_SPLINE_SURFACE(((0.987470879370255,0.98761351460672,0.990694758798812),
(0.987470879370256,0.987613514606721,0.990694758798812)))
REPRESENTATION_ITEM('')
SURFACE()
);
#3161=(
BOUNDED_SURFACE()
B_SPLINE_SURFACE(1,2,((#148091,#148092,#148093,#148094,#148095),(#148096,
#148097,#148098,#148099,#148100)),.UNSPECIFIED.,.F.,.F.,.F.)
B_SPLINE_SURFACE_WITH_KNOTS((2,2),(3,2,3),(0.,0.29028098133501),(0.107879027750092,
0.125170525609408,0.125770422799848),.UNSPECIFIED.)
GEOMETRIC_REPRESENTATION_ITEM()
RATIONAL_B_SPLINE_SURFACE(((0.987469282487682,0.987594391229382,0.990658108926709,
0.990658108926709,0.990658108926709),(0.987469282487682,0.987594391229382,
0.990658108926709,0.990658108926709,0.990658108926709)))
REPRESENTATION_ITEM('')
SURFACE()
);
#3162=(
BOUNDED_SURFACE()
B_SPLINE_SURFACE(1,2,((#148109,#148110,#148111),(#148112,#148113,#148114)),
 .UNSPECIFIED.,.F.,.F.,.F.)
B_SPLINE_SURFACE_WITH_KNOTS((2,2),(3,3),(0.,0.289807040992625),(0.607982157956011,
0.625273655815328),.UNSPECIFIED.)
GEOMETRIC_REPRESENTATION_ITEM()
RATIONAL_B_SPLINE_SURFACE(((0.987470879370255,0.98761351460672,0.990694758798812),
(0.987470879370255,0.987613514606721,0.990694758798812)))
REPRESENTATION_ITEM('')
SURFACE()
);
#3163=(
BOUNDED_SURFACE()
B_SPLINE_SURFACE(1,2,((#148116,#148117,#148118,#148119,#148120),(#148121,
#148122,#148123,#148124,#148125)),.UNSPECIFIED.,.F.,.F.,.F.)
B_SPLINE_SURFACE_WITH_KNOTS((2,2),(3,2,3),(0.,0.290280981347237),(0.107879027750092,
0.125170525609408,0.125770422812067),.UNSPECIFIED.)
GEOMETRIC_REPRESENTATION_ITEM()
RATIONAL_B_SPLINE_SURFACE(((0.987469282487682,0.987594391229382,0.990658108926709,
0.990658108926709,0.990658108926709),(0.987469282487682,0.987594391229382,
0.990658108926709,0.990658108926709,0.990658108926709)))
REPRESENTATION_ITEM('')
SURFACE()
);
#3164=(
BOUNDED_SURFACE()
B_SPLINE_SURFACE(1,2,((#148134,#148135,#148136),(#148137,#148138,#148139)),
 .UNSPECIFIED.,.F.,.F.,.F.)
B_SPLINE_SURFACE_WITH_KNOTS((2,2),(3,3),(0.,0.28980704099262),(0.607982157956011,
0.625273655815328),.UNSPECIFIED.)
GEOMETRIC_REPRESENTATION_ITEM()
RATIONAL_B_SPLINE_SURFACE(((0.987470879370255,0.98761351460672,0.990694758798812),
(0.987470879370255,0.98761351460672,0.990694758798812)))
REPRESENTATION_ITEM('')
SURFACE()
);
#3165=(
BOUNDED_SURFACE()
B_SPLINE_SURFACE(1,2,((#148141,#148142,#148143,#148144,#148145),(#148146,
#148147,#148148,#148149,#148150)),.UNSPECIFIED.,.F.,.F.,.F.)
B_SPLINE_SURFACE_WITH_KNOTS((2,2),(3,2,3),(0.,0.290280981331832),(0.107879027750092,
0.125170525609408,0.125770422796665),.UNSPECIFIED.)
GEOMETRIC_REPRESENTATION_ITEM()
RATIONAL_B_SPLINE_SURFACE(((0.987469282487682,0.987594391229382,0.990658108926709,
0.990658108926709,0.990658108926709),(0.987469282487682,0.987594391229382,
0.990658108926709,0.990658108926709,0.990658108926709)))
REPRESENTATION_ITEM('')
SURFACE()
);
#3166=(
BOUNDED_SURFACE()
B_SPLINE_SURFACE(1,2,((#148159,#148160,#148161),(#148162,#148163,#148164)),
 .UNSPECIFIED.,.F.,.F.,.F.)
B_SPLINE_SURFACE_WITH_KNOTS((2,2),(3,3),(0.,0.289807040993203),(0.607982157956011,
0.625273655815328),.UNSPECIFIED.)
GEOMETRIC_REPRESENTATION_ITEM()
RATIONAL_B_SPLINE_SURFACE(((0.987470879370255,0.98761351460672,0.990694758798812),
(0.987470879370255,0.98761351460672,0.990694758798812)))
REPRESENTATION_ITEM('')
SURFACE()
);
#3167=(
BOUNDED_SURFACE()
B_SPLINE_SURFACE(1,2,((#148166,#148167,#148168,#148169,#148170),(#148171,
#148172,#148173,#148174,#148175)),.UNSPECIFIED.,.F.,.F.,.F.)
B_SPLINE_SURFACE_WITH_KNOTS((2,2),(3,2,3),(0.,0.290280981329886),(0.107879027750092,
0.125170525609408,0.125770422835485),.UNSPECIFIED.)
GEOMETRIC_REPRESENTATION_ITEM()
RATIONAL_B_SPLINE_SURFACE(((0.987469282487682,0.987594391229382,0.990658108926709,
0.990658108926709,0.990658108926709),(0.987469282487682,0.987594391229382,
0.990658108926709,0.990658108926709,0.990658108926709)))
REPRESENTATION_ITEM('')
SURFACE()
);
#3168=(
BOUNDED_SURFACE()
B_SPLINE_SURFACE(1,2,((#148184,#148185,#148186),(#148187,#148188,#148189)),
 .UNSPECIFIED.,.F.,.F.,.F.)
B_SPLINE_SURFACE_WITH_KNOTS((2,2),(3,3),(0.,0.289807040992614),(0.607982157956011,
0.625273655815328),.UNSPECIFIED.)
GEOMETRIC_REPRESENTATION_ITEM()
RATIONAL_B_SPLINE_SURFACE(((0.987470879370255,0.98761351460672,0.990694758798812),
(0.987470879370255,0.98761351460672,0.990694758798812)))
REPRESENTATION_ITEM('')
SURFACE()
);
#3169=(
BOUNDED_SURFACE()
B_SPLINE_SURFACE(1,2,((#148191,#148192,#148193,#148194,#148195),(#148196,
#148197,#148198,#148199,#148200)),.UNSPECIFIED.,.F.,.F.,.F.)
B_SPLINE_SURFACE_WITH_KNOTS((2,2),(3,2,3),(0.,0.290280981327799),(0.107879027750091,
0.125170525609408,0.125770422833613),.UNSPECIFIED.)
GEOMETRIC_REPRESENTATION_ITEM()
RATIONAL_B_SPLINE_SURFACE(((0.987469282487682,0.987594391229382,0.990658108926709,
0.990658108926709,0.990658108926709),(0.987469282487682,0.987594391229382,
0.990658108926709,0.990658108926709,0.990658108926709)))
REPRESENTATION_ITEM('')
SURFACE()
);
#3170=(
BOUNDED_SURFACE()
B_SPLINE_SURFACE(1,2,((#148209,#148210,#148211),(#148212,#148213,#148214)),
 .UNSPECIFIED.,.F.,.F.,.F.)
B_SPLINE_SURFACE_WITH_KNOTS((2,2),(3,3),(0.,0.289807040993169),(0.607982157956011,
0.625273655815328),.UNSPECIFIED.)
GEOMETRIC_REPRESENTATION_ITEM()
RATIONAL_B_SPLINE_SURFACE(((0.987470879370255,0.98761351460672,0.990694758798812),
(0.987470879370255,0.98761351460672,0.990694758798812)))
REPRESENTATION_ITEM('')
SURFACE()
);
#3171=(
BOUNDED_SURFACE()
B_SPLINE_SURFACE(1,2,((#148216,#148217,#148218,#148219,#148220),(#148221,
#148222,#148223,#148224,#148225)),.UNSPECIFIED.,.F.,.F.,.F.)
B_SPLINE_SURFACE_WITH_KNOTS((2,2),(3,2,3),(0.,0.290280981354195),(0.107879027750092,
0.125170525609409,0.125770422859419),.UNSPECIFIED.)
GEOMETRIC_REPRESENTATION_ITEM()
RATIONAL_B_SPLINE_SURFACE(((0.987469282487682,0.987594391229382,0.990658108926709,
0.990658108926709,0.990658108926709),(0.987469282487682,0.987594391229382,
0.990658108926709,0.990658108926709,0.990658108926709)))
REPRESENTATION_ITEM('')
SURFACE()
);
#3172=(
BOUNDED_SURFACE()
B_SPLINE_SURFACE(1,2,((#148234,#148235,#148236),(#148237,#148238,#148239)),
 .UNSPECIFIED.,.F.,.F.,.F.)
B_SPLINE_SURFACE_WITH_KNOTS((2,2),(3,3),(0.,0.289807040992984),(0.607982157956012,
0.625273655815328),.UNSPECIFIED.)
GEOMETRIC_REPRESENTATION_ITEM()
RATIONAL_B_SPLINE_SURFACE(((0.987470879370255,0.987613514606721,0.990694758798812),
(0.987470879370255,0.987613514606721,0.990694758798812)))
REPRESENTATION_ITEM('')
SURFACE()
);
#3173=(
BOUNDED_SURFACE()
B_SPLINE_SURFACE(1,2,((#148241,#148242,#148243,#148244,#148245),(#148246,
#148247,#148248,#148249,#148250)),.UNSPECIFIED.,.F.,.F.,.F.)
B_SPLINE_SURFACE_WITH_KNOTS((2,2),(3,2,3),(0.,0.290280981333798),(0.10787902775009,
0.125170525609407,0.125770422839726),.UNSPECIFIED.)
GEOMETRIC_REPRESENTATION_ITEM()
RATIONAL_B_SPLINE_SURFACE(((0.987469282487682,0.987594391229382,0.990658108926708,
0.990658108926708,0.990658108926708),(0.987469282487682,0.987594391229382,
0.990658108926708,0.990658108926708,0.990658108926708)))
REPRESENTATION_ITEM('')
SURFACE()
);
#3174=(
BOUNDED_SURFACE()
B_SPLINE_SURFACE(1,2,((#148259,#148260,#148261),(#148262,#148263,#148264)),
 .UNSPECIFIED.,.F.,.F.,.F.)
B_SPLINE_SURFACE_WITH_KNOTS((2,2),(3,3),(0.,0.289807040993017),(0.607982157956012,
0.625273655815329),.UNSPECIFIED.)
GEOMETRIC_REPRESENTATION_ITEM()
RATIONAL_B_SPLINE_SURFACE(((0.987470879370255,0.987613514606721,0.990694758798813),
(0.987470879370255,0.987613514606721,0.990694758798813)))
REPRESENTATION_ITEM('')
SURFACE()
);
#3175=(
BOUNDED_SURFACE()
B_SPLINE_SURFACE(1,2,((#148266,#148267,#148268,#148269,#148270),(#148271,
#148272,#148273,#148274,#148275)),.UNSPECIFIED.,.F.,.F.,.F.)
B_SPLINE_SURFACE_WITH_KNOTS((2,2),(3,2,3),(0.,0.290280981342294),(0.10787902775009,
0.125170525609407,0.125770422807127),.UNSPECIFIED.)
GEOMETRIC_REPRESENTATION_ITEM()
RATIONAL_B_SPLINE_SURFACE(((0.987469282487682,0.987594391229382,0.990658108926708,
0.990658108926708,0.990658108926708),(0.987469282487682,0.987594391229382,
0.990658108926708,0.990658108926708,0.990658108926708)))
REPRESENTATION_ITEM('')
SURFACE()
);
#3176=(
BOUNDED_SURFACE()
B_SPLINE_SURFACE(1,2,((#148284,#148285,#148286),(#148287,#148288,#148289)),
 .UNSPECIFIED.,.F.,.F.,.F.)
B_SPLINE_SURFACE_WITH_KNOTS((2,2),(3,3),(0.,0.289807040993289),(0.607982157956012,
0.625273655815329),.UNSPECIFIED.)
GEOMETRIC_REPRESENTATION_ITEM()
RATIONAL_B_SPLINE_SURFACE(((0.987470879370255,0.987613514606721,0.990694758798813),
(0.987470879370255,0.987613514606721,0.990694758798813)))
REPRESENTATION_ITEM('')
SURFACE()
);
#3177=(
BOUNDED_SURFACE()
B_SPLINE_SURFACE(1,2,((#148291,#148292,#148293,#148294,#148295),(#148296,
#148297,#148298,#148299,#148300)),.UNSPECIFIED.,.F.,.F.,.F.)
B_SPLINE_SURFACE_WITH_KNOTS((2,2),(3,2,3),(0.,0.290280981336171),(0.10787902775009,
0.125170525609407,0.125770422841787),.UNSPECIFIED.)
GEOMETRIC_REPRESENTATION_ITEM()
RATIONAL_B_SPLINE_SURFACE(((0.987469282487682,0.987594391229382,0.990658108926709,
0.990658108926709,0.990658108926709),(0.987469282487682,0.987594391229382,
0.990658108926709,0.990658108926709,0.990658108926709)))
REPRESENTATION_ITEM('')
SURFACE()
);
#3178=(
BOUNDED_SURFACE()
B_SPLINE_SURFACE(1,2,((#148309,#148310,#148311),(#148312,#148313,#148314)),
 .UNSPECIFIED.,.F.,.F.,.F.)
B_SPLINE_SURFACE_WITH_KNOTS((2,2),(3,3),(0.,0.28980704099271),(0.607982157956012,
0.625273655815329),.UNSPECIFIED.)
GEOMETRIC_REPRESENTATION_ITEM()
RATIONAL_B_SPLINE_SURFACE(((0.987470879370255,0.987613514606721,0.990694758798813),
(0.987470879370255,0.987613514606721,0.990694758798813)))
REPRESENTATION_ITEM('')
SURFACE()
);
#3179=(
BOUNDED_SURFACE()
B_SPLINE_SURFACE(1,2,((#148316,#148317,#148318,#148319,#148320),(#148321,
#148322,#148323,#148324,#148325)),.UNSPECIFIED.,.F.,.F.,.F.)
B_SPLINE_SURFACE_WITH_KNOTS((2,2),(3,2,3),(0.,0.290280981341405),(0.10787902775009,
0.125170525609408,0.125770422806235),.UNSPECIFIED.)
GEOMETRIC_REPRESENTATION_ITEM()
RATIONAL_B_SPLINE_SURFACE(((0.987469282487682,0.987594391229382,0.990658108926709,
0.990658108926709,0.990658108926709),(0.987469282487682,0.987594391229382,
0.990658108926709,0.990658108926709,0.990658108926709)))
REPRESENTATION_ITEM('')
SURFACE()
);
#3180=(
BOUNDED_SURFACE()
B_SPLINE_SURFACE(1,2,((#148334,#148335,#148336),(#148337,#148338,#148339)),
 .UNSPECIFIED.,.F.,.F.,.F.)
B_SPLINE_SURFACE_WITH_KNOTS((2,2),(3,3),(0.,0.289807040993545),(0.607982157956012,
0.625273655815329),.UNSPECIFIED.)
GEOMETRIC_REPRESENTATION_ITEM()
RATIONAL_B_SPLINE_SURFACE(((0.987470879370255,0.987613514606721,0.990694758798813),
(0.987470879370255,0.987613514606721,0.990694758798813)))
REPRESENTATION_ITEM('')
SURFACE()
);
#3181=(
BOUNDED_SURFACE()
B_SPLINE_SURFACE(1,2,((#148341,#148342,#148343,#148344,#148345),(#148346,
#148347,#148348,#148349,#148350)),.UNSPECIFIED.,.F.,.F.,.F.)
B_SPLINE_SURFACE_WITH_KNOTS((2,2),(3,2,3),(0.,0.29028098133396),(0.107879027750091,
0.125170525609408,0.125770422798795),.UNSPECIFIED.)
GEOMETRIC_REPRESENTATION_ITEM()
RATIONAL_B_SPLINE_SURFACE(((0.987469282487682,0.987594391229382,0.990658108926709,
0.990658108926709,0.990658108926709),(0.987469282487682,0.987594391229382,
0.990658108926709,0.990658108926709,0.990658108926709)))
REPRESENTATION_ITEM('')
SURFACE()
);
#3182=(
BOUNDED_SURFACE()
B_SPLINE_SURFACE(1,2,((#148359,#148360,#148361),(#148362,#148363,#148364)),
 .UNSPECIFIED.,.F.,.F.,.F.)
B_SPLINE_SURFACE_WITH_KNOTS((2,2),(3,3),(0.,0.289807040993042),(0.607982157956012,
0.625273655815329),.UNSPECIFIED.)
GEOMETRIC_REPRESENTATION_ITEM()
RATIONAL_B_SPLINE_SURFACE(((0.987470879370255,0.987613514606721,0.990694758798813),
(0.987470879370255,0.987613514606721,0.990694758798813)))
REPRESENTATION_ITEM('')
SURFACE()
);
#3183=(
BOUNDED_SURFACE()
B_SPLINE_SURFACE(1,2,((#148366,#148367,#148368,#148369,#148370),(#148371,
#148372,#148373,#148374,#148375)),.UNSPECIFIED.,.F.,.F.,.F.)
B_SPLINE_SURFACE_WITH_KNOTS((2,2),(3,2,3),(0.,0.290280981332549),(0.10787902775009,
0.125170525609408,0.125770422838297),.UNSPECIFIED.)
GEOMETRIC_REPRESENTATION_ITEM()
RATIONAL_B_SPLINE_SURFACE(((0.987469282487682,0.987594391229382,0.990658108926708,
0.990658108926708,0.990658108926708),(0.987469282487682,0.987594391229382,
0.990658108926708,0.990658108926708,0.990658108926708)))
REPRESENTATION_ITEM('')
SURFACE()
);
#3184=(
BOUNDED_SURFACE()
B_SPLINE_SURFACE(1,2,((#148384,#148385,#148386),(#148387,#148388,#148389)),
 .UNSPECIFIED.,.F.,.F.,.F.)
B_SPLINE_SURFACE_WITH_KNOTS((2,2),(3,3),(0.,0.289807040993511),(0.607982157956012,
0.625273655815329),.UNSPECIFIED.)
GEOMETRIC_REPRESENTATION_ITEM()
RATIONAL_B_SPLINE_SURFACE(((0.987470879370255,0.987613514606721,0.990694758798813),
(0.987470879370255,0.987613514606721,0.990694758798813)))
REPRESENTATION_ITEM('')
SURFACE()
);
#3185=(
BOUNDED_SURFACE()
B_SPLINE_SURFACE(1,2,((#148391,#148392,#148393,#148394,#148395),(#148396,
#148397,#148398,#148399,#148400)),.UNSPECIFIED.,.F.,.F.,.F.)
B_SPLINE_SURFACE_WITH_KNOTS((2,2),(3,2,3),(0.,0.290280981335985),(0.10787902775009,
0.125170525609407,0.125770422841674),.UNSPECIFIED.)
GEOMETRIC_REPRESENTATION_ITEM()
RATIONAL_B_SPLINE_SURFACE(((0.987469282487682,0.987594391229382,0.990658108926709,
0.990658108926709,0.990658108926709),(0.987469282487682,0.987594391229382,
0.990658108926709,0.990658108926709,0.990658108926709)))
REPRESENTATION_ITEM('')
SURFACE()
);
#3186=(
BOUNDED_SURFACE()
B_SPLINE_SURFACE(1,2,((#148409,#148410,#148411),(#148412,#148413,#148414)),
 .UNSPECIFIED.,.F.,.F.,.F.)
B_SPLINE_SURFACE_WITH_KNOTS((2,2),(3,3),(0.,0.289807040993257),(0.607982157956012,
0.625273655815329),.UNSPECIFIED.)
GEOMETRIC_REPRESENTATION_ITEM()
RATIONAL_B_SPLINE_SURFACE(((0.987470879370255,0.987613514606721,0.990694758798813),
(0.987470879370255,0.987613514606721,0.990694758798813)))
REPRESENTATION_ITEM('')
SURFACE()
);
#3187=(
BOUNDED_SURFACE()
B_SPLINE_SURFACE(1,2,((#148416,#148417,#148418,#148419,#148420),(#148421,
#148422,#148423,#148424,#148425)),.UNSPECIFIED.,.F.,.F.,.F.)
B_SPLINE_SURFACE_WITH_KNOTS((2,2),(3,2,3),(0.,0.290280981317335),(0.10787902775009,
0.125170525609407,0.125770422823056),.UNSPECIFIED.)
GEOMETRIC_REPRESENTATION_ITEM()
RATIONAL_B_SPLINE_SURFACE(((0.987469282487682,0.987594391229382,0.990658108926708,
0.990658108926708,0.990658108926708),(0.987469282487682,0.987594391229382,
0.990658108926708,0.990658108926708,0.990658108926708)))
REPRESENTATION_ITEM('')
SURFACE()
);
#3188=(
BOUNDED_SURFACE()
B_SPLINE_SURFACE(1,2,((#148434,#148435,#148436),(#148437,#148438,#148439)),
 .UNSPECIFIED.,.F.,.F.,.F.)
B_SPLINE_SURFACE_WITH_KNOTS((2,2),(3,3),(0.,0.289807040994421),(0.607982157956012,
0.625273655815329),.UNSPECIFIED.)
GEOMETRIC_REPRESENTATION_ITEM()
RATIONAL_B_SPLINE_SURFACE(((0.987470879370255,0.987613514606721,0.990694758798813),
(0.987470879370255,0.987613514606721,0.990694758798813)))
REPRESENTATION_ITEM('')
SURFACE()
);
#3189=(
BOUNDED_SURFACE()
B_SPLINE_SURFACE(1,2,((#148441,#148442,#148443,#148444,#148445),(#148446,
#148447,#148448,#148449,#148450)),.UNSPECIFIED.,.F.,.F.,.F.)
B_SPLINE_SURFACE_WITH_KNOTS((2,2),(3,2,3),(0.,0.290280981346559),(0.10787902775009,
0.125170525609407,0.125770422811388),.UNSPECIFIED.)
GEOMETRIC_REPRESENTATION_ITEM()
RATIONAL_B_SPLINE_SURFACE(((0.987469282487682,0.987594391229382,0.990658108926708,
0.990658108926708,0.990658108926708),(0.987469282487682,0.987594391229382,
0.990658108926708,0.990658108926708,0.990658108926708)))
REPRESENTATION_ITEM('')
SURFACE()
);
#3190=(
BOUNDED_SURFACE()
B_SPLINE_SURFACE(1,2,((#148459,#148460,#148461),(#148462,#148463,#148464)),
 .UNSPECIFIED.,.F.,.F.,.F.)
B_SPLINE_SURFACE_WITH_KNOTS((2,2),(3,3),(0.,0.28980704099276),(0.607982157956012,
0.625273655815329),.UNSPECIFIED.)
GEOMETRIC_REPRESENTATION_ITEM()
RATIONAL_B_SPLINE_SURFACE(((0.987470879370255,0.987613514606721,0.990694758798813),
(0.987470879370255,0.987613514606721,0.990694758798813)))
REPRESENTATION_ITEM('')
SURFACE()
);
#3191=(
BOUNDED_SURFACE()
B_SPLINE_SURFACE(1,2,((#148466,#148467,#148468,#148469,#148470),(#148471,
#148472,#148473,#148474,#148475)),.UNSPECIFIED.,.F.,.F.,.F.)
B_SPLINE_SURFACE_WITH_KNOTS((2,2),(3,2,3),(0.,0.29028098134186),(0.10787902775009,
0.125170525609407,0.125770422847784),.UNSPECIFIED.)
GEOMETRIC_REPRESENTATION_ITEM()
RATIONAL_B_SPLINE_SURFACE(((0.987469282487682,0.987594391229382,0.990658108926708,
0.990658108926708,0.990658108926708),(0.987469282487682,0.987594391229382,
0.990658108926708,0.990658108926708,0.990658108926708)))
REPRESENTATION_ITEM('')
SURFACE()
);
#3192=(
BOUNDED_SURFACE()
B_SPLINE_SURFACE(1,2,((#148484,#148485,#148486),(#148487,#148488,#148489)),
 .UNSPECIFIED.,.F.,.F.,.F.)
B_SPLINE_SURFACE_WITH_KNOTS((2,2),(3,3),(0.,0.289807040992648),(0.607982157956012,
0.625273655815329),.UNSPECIFIED.)
GEOMETRIC_REPRESENTATION_ITEM()
RATIONAL_B_SPLINE_SURFACE(((0.987470879370255,0.987613514606721,0.990694758798813),
(0.987470879370255,0.987613514606721,0.990694758798813)))
REPRESENTATION_ITEM('')
SURFACE()
);
#3193=(
BOUNDED_SURFACE()
B_SPLINE_SURFACE(1,2,((#148491,#148492,#148493,#148494,#148495),(#148496,
#148497,#148498,#148499,#148500)),.UNSPECIFIED.,.F.,.F.,.F.)
B_SPLINE_SURFACE_WITH_KNOTS((2,2),(3,2,3),(0.,0.290280981333718),(0.107879027750091,
0.125170525609407,0.12577042279855),.UNSPECIFIED.)
GEOMETRIC_REPRESENTATION_ITEM()
RATIONAL_B_SPLINE_SURFACE(((0.987469282487682,0.987594391229382,0.990658108926708,
0.990658108926708,0.990658108926708),(0.987469282487682,0.987594391229382,
0.990658108926708,0.990658108926708,0.990658108926708)))
REPRESENTATION_ITEM('')
SURFACE()
);
#3194=(
BOUNDED_SURFACE()
B_SPLINE_SURFACE(1,2,((#148509,#148510,#148511),(#148512,#148513,#148514)),
 .UNSPECIFIED.,.F.,.F.,.F.)
B_SPLINE_SURFACE_WITH_KNOTS((2,2),(3,3),(0.,0.289807040993488),(0.607982157956012,
0.625273655815329),.UNSPECIFIED.)
GEOMETRIC_REPRESENTATION_ITEM()
RATIONAL_B_SPLINE_SURFACE(((0.987470879370255,0.987613514606721,0.990694758798813),
(0.987470879370255,0.987613514606721,0.990694758798813)))
REPRESENTATION_ITEM('')
SURFACE()
);
#3195=(
BOUNDED_SURFACE()
B_SPLINE_SURFACE(1,2,((#148516,#148517,#148518,#148519,#148520),(#148521,
#148522,#148523,#148524,#148525)),.UNSPECIFIED.,.F.,.F.,.F.)
B_SPLINE_SURFACE_WITH_KNOTS((2,2),(3,2,3),(0.,0.290280981329807),(0.107879027750091,
0.125170525609407,0.125770422794629),.UNSPECIFIED.)
GEOMETRIC_REPRESENTATION_ITEM()
RATIONAL_B_SPLINE_SURFACE(((0.987469282487682,0.987594391229382,0.990658108926708,
0.990658108926708,0.990658108926708),(0.987469282487682,0.987594391229382,
0.990658108926708,0.990658108926708,0.990658108926708)))
REPRESENTATION_ITEM('')
SURFACE()
);
#3196=(
BOUNDED_SURFACE()
B_SPLINE_SURFACE(1,2,((#148534,#148535,#148536),(#148537,#148538,#148539)),
 .UNSPECIFIED.,.F.,.F.,.F.)
B_SPLINE_SURFACE_WITH_KNOTS((2,2),(3,3),(0.,0.289807040992018),(0.607982157956012,
0.62527365581533),.UNSPECIFIED.)
GEOMETRIC_REPRESENTATION_ITEM()
RATIONAL_B_SPLINE_SURFACE(((0.987470879370255,0.987613514606721,0.990694758798813),
(0.987470879370255,0.987613514606721,0.990694758798813)))
REPRESENTATION_ITEM('')
SURFACE()
);
#3197=(
BOUNDED_SURFACE()
B_SPLINE_SURFACE(1,2,((#148541,#148542,#148543,#148544,#148545),(#148546,
#148547,#148548,#148549,#148550)),.UNSPECIFIED.,.F.,.F.,.F.)
B_SPLINE_SURFACE_WITH_KNOTS((2,2),(3,2,3),(0.,0.290280981334961),(0.10787902775009,
0.125170525609412,0.125770422840683),.UNSPECIFIED.)
GEOMETRIC_REPRESENTATION_ITEM()
RATIONAL_B_SPLINE_SURFACE(((0.987469282487682,0.987594391229382,0.99065810892671,
0.99065810892671,0.99065810892671),(0.987469282487682,0.987594391229382,
0.99065810892671,0.99065810892671,0.99065810892671)))
REPRESENTATION_ITEM('')
SURFACE()
);
#3198=(
BOUNDED_SURFACE()
B_SPLINE_SURFACE(1,2,((#148559,#148560,#148561),(#148562,#148563,#148564)),
 .UNSPECIFIED.,.F.,.F.,.F.)
B_SPLINE_SURFACE_WITH_KNOTS((2,2),(3,3),(0.,0.289807040992891),(0.607982157956012,
0.625273655815329),.UNSPECIFIED.)
GEOMETRIC_REPRESENTATION_ITEM()
RATIONAL_B_SPLINE_SURFACE(((0.987470879370255,0.987613514606721,0.990694758798813),
(0.987470879370255,0.987613514606721,0.990694758798813)))
REPRESENTATION_ITEM('')
SURFACE()
);
#3199=(
BOUNDED_SURFACE()
B_SPLINE_SURFACE(1,2,((#148566,#148567,#148568,#148569,#148570),(#148571,
#148572,#148573,#148574,#148575)),.UNSPECIFIED.,.F.,.F.,.F.)
B_SPLINE_SURFACE_WITH_KNOTS((2,2),(3,2,3),(0.,0.290280981350767),(0.10787902775009,
0.125170525609407,0.125770422856224),.UNSPECIFIED.)
GEOMETRIC_REPRESENTATION_ITEM()
RATIONAL_B_SPLINE_SURFACE(((0.987469282487682,0.987594391229382,0.990658108926708,
0.990658108926708,0.990658108926708),(0.987469282487682,0.987594391229382,
0.990658108926708,0.990658108926708,0.990658108926708)))
REPRESENTATION_ITEM('')
SURFACE()
);
#3200=(
BOUNDED_SURFACE()
B_SPLINE_SURFACE(1,2,((#148584,#148585,#148586),(#148587,#148588,#148589)),
 .UNSPECIFIED.,.F.,.F.,.F.)
B_SPLINE_SURFACE_WITH_KNOTS((2,2),(3,3),(0.,0.289807040992687),(0.607982157956012,
0.625273655815329),.UNSPECIFIED.)
GEOMETRIC_REPRESENTATION_ITEM()
RATIONAL_B_SPLINE_SURFACE(((0.987470879370255,0.987613514606721,0.990694758798813),
(0.987470879370255,0.987613514606721,0.990694758798813)))
REPRESENTATION_ITEM('')
SURFACE()
);
#3201=(
BOUNDED_SURFACE()
B_SPLINE_SURFACE(1,2,((#148591,#148592,#148593,#148594,#148595),(#148596,
#148597,#148598,#148599,#148600)),.UNSPECIFIED.,.F.,.F.,.F.)
B_SPLINE_SURFACE_WITH_KNOTS((2,2),(3,2,3),(0.,0.290280981338245),(0.107879027750092,
0.125170525609407,0.125770422843646),.UNSPECIFIED.)
GEOMETRIC_REPRESENTATION_ITEM()
RATIONAL_B_SPLINE_SURFACE(((0.987469282487682,0.987594391229382,0.990658108926709,
0.990658108926709,0.990658108926709),(0.987469282487682,0.987594391229382,
0.990658108926709,0.990658108926709,0.990658108926709)))
REPRESENTATION_ITEM('')
SURFACE()
);
#3202=(
BOUNDED_SURFACE()
B_SPLINE_SURFACE(1,2,((#148609,#148610,#148611),(#148612,#148613,#148614)),
 .UNSPECIFIED.,.F.,.F.,.F.)
B_SPLINE_SURFACE_WITH_KNOTS((2,2),(3,3),(0.,0.28980704099156),(0.607982157956011,
0.625273655815328),.UNSPECIFIED.)
GEOMETRIC_REPRESENTATION_ITEM()
RATIONAL_B_SPLINE_SURFACE(((0.987470879370255,0.98761351460672,0.990694758798812),
(0.987470879370256,0.987613514606721,0.990694758798812)))
REPRESENTATION_ITEM('')
SURFACE()
);
#3203=(
BOUNDED_SURFACE()
B_SPLINE_SURFACE(1,2,((#148616,#148617,#148618,#148619,#148620),(#148621,
#148622,#148623,#148624,#148625)),.UNSPECIFIED.,.F.,.F.,.F.)
B_SPLINE_SURFACE_WITH_KNOTS((2,2),(3,2,3),(0.,0.290280981347015),(0.107879027750092,
0.125170525609408,0.125770422811853),.UNSPECIFIED.)
GEOMETRIC_REPRESENTATION_ITEM()
RATIONAL_B_SPLINE_SURFACE(((0.987469282487682,0.987594391229382,0.990658108926709,
0.990658108926709,0.990658108926709),(0.987469282487682,0.987594391229382,
0.990658108926709,0.990658108926709,0.990658108926709)))
REPRESENTATION_ITEM('')
SURFACE()
);
#3204=(
BOUNDED_SURFACE()
B_SPLINE_SURFACE(1,2,((#148634,#148635,#148636),(#148637,#148638,#148639)),
 .UNSPECIFIED.,.F.,.F.,.F.)
B_SPLINE_SURFACE_WITH_KNOTS((2,2),(3,3),(0.,0.289807040991555),(0.607982157956011,
0.625273655815328),.UNSPECIFIED.)
GEOMETRIC_REPRESENTATION_ITEM()
RATIONAL_B_SPLINE_SURFACE(((0.987470879370255,0.98761351460672,0.990694758798812),
(0.987470879370255,0.98761351460672,0.990694758798812)))
REPRESENTATION_ITEM('')
SURFACE()
);
#3205=(
BOUNDED_SURFACE()
B_SPLINE_SURFACE(1,2,((#148641,#148642,#148643,#148644,#148645),(#148646,
#148647,#148648,#148649,#148650)),.UNSPECIFIED.,.F.,.F.,.F.)
B_SPLINE_SURFACE_WITH_KNOTS((2,2),(3,2,3),(0.,0.29028098134296),(0.107879027750092,
0.125170525609409,0.125770422807798),.UNSPECIFIED.)
GEOMETRIC_REPRESENTATION_ITEM()
RATIONAL_B_SPLINE_SURFACE(((0.987469282487682,0.987594391229382,0.990658108926709,
0.990658108926709,0.990658108926709),(0.987469282487682,0.987594391229382,
0.990658108926709,0.990658108926709,0.990658108926709)))
REPRESENTATION_ITEM('')
SURFACE()
);
#3206=(
BOUNDED_SURFACE()
B_SPLINE_SURFACE(1,2,((#148659,#148660,#148661),(#148662,#148663,#148664)),
 .UNSPECIFIED.,.F.,.F.,.F.)
B_SPLINE_SURFACE_WITH_KNOTS((2,2),(3,3),(0.,0.28980704099156),(0.607982157956011,
0.625273655815328),.UNSPECIFIED.)
GEOMETRIC_REPRESENTATION_ITEM()
RATIONAL_B_SPLINE_SURFACE(((0.987470879370255,0.98761351460672,0.990694758798812),
(0.987470879370256,0.987613514606721,0.990694758798812)))
REPRESENTATION_ITEM('')
SURFACE()
);
#3207=(
BOUNDED_SURFACE()
B_SPLINE_SURFACE(1,2,((#148666,#148667,#148668,#148669,#148670),(#148671,
#148672,#148673,#148674,#148675)),.UNSPECIFIED.,.F.,.F.,.F.)
B_SPLINE_SURFACE_WITH_KNOTS((2,2),(3,2,3),(0.,0.290280981340027),(0.107879027750092,
0.125170525609409,0.125770422804864),.UNSPECIFIED.)
GEOMETRIC_REPRESENTATION_ITEM()
RATIONAL_B_SPLINE_SURFACE(((0.987469282487682,0.987594391229382,0.990658108926709,
0.990658108926709,0.990658108926709),(0.987469282487682,0.987594391229382,
0.990658108926709,0.990658108926709,0.990658108926709)))
REPRESENTATION_ITEM('')
SURFACE()
);
#3208=(
BOUNDED_SURFACE()
B_SPLINE_SURFACE(1,2,((#148684,#148685,#148686),(#148687,#148688,#148689)),
 .UNSPECIFIED.,.F.,.F.,.F.)
B_SPLINE_SURFACE_WITH_KNOTS((2,2),(3,3),(0.,0.289807040991888),(0.607982157956011,
0.625273655815328),.UNSPECIFIED.)
GEOMETRIC_REPRESENTATION_ITEM()
RATIONAL_B_SPLINE_SURFACE(((0.987470879370255,0.98761351460672,0.990694758798812),
(0.987470879370255,0.98761351460672,0.990694758798812)))
REPRESENTATION_ITEM('')
SURFACE()
);
#3209=(
BOUNDED_SURFACE()
B_SPLINE_SURFACE(1,2,((#148691,#148692,#148693,#148694,#148695),(#148696,
#148697,#148698,#148699,#148700)),.UNSPECIFIED.,.F.,.F.,.F.)
B_SPLINE_SURFACE_WITH_KNOTS((2,2),(3,2,3),(0.,0.290280981336771),(0.107879027750092,
0.125170525609409,0.125770422801606),.UNSPECIFIED.)
GEOMETRIC_REPRESENTATION_ITEM()
RATIONAL_B_SPLINE_SURFACE(((0.987469282487682,0.987594391229382,0.990658108926709,
0.990658108926709,0.990658108926709),(0.987469282487682,0.987594391229382,
0.990658108926709,0.990658108926709,0.990658108926709)))
REPRESENTATION_ITEM('')
SURFACE()
);
#3210=(
BOUNDED_SURFACE()
B_SPLINE_SURFACE(1,2,((#148702,#148703,#148704,#148705,#148706),(#148707,
#148708,#148709,#148710,#148711)),.UNSPECIFIED.,.F.,.F.,.F.)
B_SPLINE_SURFACE_WITH_KNOTS((2,2),(3,2,3),(0.,0.29039631629416),(0.159312132641873,
0.159901408087358,0.177069452526136),.UNSPECIFIED.)
GEOMETRIC_REPRESENTATION_ITEM()
RATIONAL_B_SPLINE_SURFACE(((0.990889788836329,0.990889788836329,0.990889788836329,
0.987739559362113,0.987486127973996),(0.990889788836329,0.990889788836329,
0.990889788836329,0.987739559362113,0.987486127973996)))
REPRESENTATION_ITEM('')
SURFACE()
);
#3211=(
BOUNDED_SURFACE()
B_SPLINE_SURFACE(1,2,((#148734,#148735,#148736,#148737,#148738),(#148739,
#148740,#148741,#148742,#148743)),.UNSPECIFIED.,.F.,.F.,.F.)
B_SPLINE_SURFACE_WITH_KNOTS((2,2),(3,2,3),(0.,0.28968108435992),(0.556108173865714,
0.571428571428571,0.57365435021991),.UNSPECIFIED.)
GEOMETRIC_REPRESENTATION_ITEM()
RATIONAL_B_SPLINE_SURFACE(((0.991551633675927,0.994622399056525,1.,0.999218731101516,
0.99848615229188),(0.991551633675927,0.994622399056525,1.,0.999218731101516,
0.99848615229188)))
REPRESENTATION_ITEM('')
SURFACE()
);
#3212=(
BOUNDED_SURFACE()
B_SPLINE_SURFACE(1,2,((#148745,#148746,#148747,#148748,#148749),(#148750,
#148751,#148752,#148753,#148754)),.UNSPECIFIED.,.F.,.F.,.F.)
B_SPLINE_SURFACE_WITH_KNOTS((2,2),(3,2,3),(0.,0.290396316319309),(0.159312132616718,
0.159901408087285,0.177069452526139),.UNSPECIFIED.)
GEOMETRIC_REPRESENTATION_ITEM()
RATIONAL_B_SPLINE_SURFACE(((0.990889788836356,0.990889788836356,0.990889788836356,
0.987739559362113,0.987486127973996),(0.990889788836356,0.990889788836356,
0.990889788836356,0.987739559362113,0.987486127973996)))
REPRESENTATION_ITEM('')
SURFACE()
);
#3213=(
BOUNDED_SURFACE()
B_SPLINE_SURFACE(1,2,((#148777,#148778,#148779,#148780,#148781),(#148782,
#148783,#148784,#148785,#148786)),.UNSPECIFIED.,.F.,.F.,.F.)
B_SPLINE_SURFACE_WITH_KNOTS((2,2),(3,2,3),(0.,0.289681084359924),(0.556108173865715,
0.571428571428571,0.57365435021991),.UNSPECIFIED.)
GEOMETRIC_REPRESENTATION_ITEM()
RATIONAL_B_SPLINE_SURFACE(((0.991551633675927,0.994622399056525,1.,0.999218731101516,
0.99848615229188),(0.991551633675927,0.994622399056525,1.,0.999218731101516,
0.99848615229188)))
REPRESENTATION_ITEM('')
SURFACE()
);
#3214=(
BOUNDED_SURFACE()
B_SPLINE_SURFACE(1,2,((#148788,#148789,#148790,#148791,#148792),(#148793,
#148794,#148795,#148796,#148797)),.UNSPECIFIED.,.F.,.F.,.F.)
B_SPLINE_SURFACE_WITH_KNOTS((2,2),(3,2,3),(0.,0.290396316297934),(0.159312132638105,
0.159901408087482,0.177069452526134),.UNSPECIFIED.)
GEOMETRIC_REPRESENTATION_ITEM()
RATIONAL_B_SPLINE_SURFACE(((0.990889788836284,0.990889788836284,0.990889788836284,
0.987739559362111,0.987486127973996),(0.990889788836283,0.990889788836283,
0.990889788836283,0.987739559362111,0.987486127973996)))
REPRESENTATION_ITEM('')
SURFACE()
);
#3215=(
BOUNDED_SURFACE()
B_SPLINE_SURFACE(1,2,((#148820,#148821,#148822,#148823,#148824),(#148825,
#148826,#148827,#148828,#148829)),.UNSPECIFIED.,.F.,.F.,.F.)
B_SPLINE_SURFACE_WITH_KNOTS((2,2),(3,2,3),(0.,0.289681084359914),(0.556108173865715,
0.571428571428571,0.573654350219911),.UNSPECIFIED.)
GEOMETRIC_REPRESENTATION_ITEM()
RATIONAL_B_SPLINE_SURFACE(((0.991551633675927,0.994622399056526,1.,0.999218731101516,
0.99848615229188),(0.991551633675927,0.994622399056526,1.,0.999218731101516,
0.99848615229188)))
REPRESENTATION_ITEM('')
SURFACE()
);
#3216=(
BOUNDED_SURFACE()
B_SPLINE_SURFACE(1,2,((#148831,#148832,#148833,#148834,#148835),(#148836,
#148837,#148838,#148839,#148840)),.UNSPECIFIED.,.F.,.F.,.F.)
B_SPLINE_SURFACE_WITH_KNOTS((2,2),(3,2,3),(0.,0.290396316309596),(0.159312132626429,
0.159901408087222,0.177069452526135),.UNSPECIFIED.)
GEOMETRIC_REPRESENTATION_ITEM()
RATIONAL_B_SPLINE_SURFACE(((0.990889788836379,0.990889788836379,0.990889788836379,
0.987739559362115,0.987486127973996),(0.990889788836379,0.990889788836379,
0.990889788836379,0.987739559362115,0.987486127973996)))
REPRESENTATION_ITEM('')
SURFACE()
);
#3217=(
BOUNDED_SURFACE()
B_SPLINE_SURFACE(1,2,((#148863,#148864,#148865,#148866,#148867),(#148868,
#148869,#148870,#148871,#148872)),.UNSPECIFIED.,.F.,.F.,.F.)
B_SPLINE_SURFACE_WITH_KNOTS((2,2),(3,2,3),(0.,0.289681084359931),(0.556108173865715,
0.571428571428571,0.573654350219911),.UNSPECIFIED.)
GEOMETRIC_REPRESENTATION_ITEM()
RATIONAL_B_SPLINE_SURFACE(((0.991551633675927,0.994622399056526,1.,0.999218731101516,
0.99848615229188),(0.991551633675927,0.994622399056526,1.,0.999218731101516,
0.99848615229188)))
REPRESENTATION_ITEM('')
SURFACE()
);
#3218=(
BOUNDED_SURFACE()
B_SPLINE_SURFACE(1,2,((#148874,#148875,#148876,#148877,#148878),(#148879,
#148880,#148881,#148882,#148883)),.UNSPECIFIED.,.F.,.F.,.F.)
B_SPLINE_SURFACE_WITH_KNOTS((2,2),(3,2,3),(0.,0.29039631632092),(0.159312132615108,
0.159901408087359,0.177069452526138),.UNSPECIFIED.)
GEOMETRIC_REPRESENTATION_ITEM()
RATIONAL_B_SPLINE_SURFACE(((0.990889788836329,0.990889788836329,0.990889788836329,
0.987739559362112,0.987486127973996),(0.990889788836329,0.990889788836329,
0.990889788836329,0.987739559362112,0.987486127973996)))
REPRESENTATION_ITEM('')
SURFACE()
);
#3219=(
BOUNDED_SURFACE()
B_SPLINE_SURFACE(1,2,((#148906,#148907,#148908,#148909,#148910),(#148911,
#148912,#148913,#148914,#148915)),.UNSPECIFIED.,.F.,.F.,.F.)
B_SPLINE_SURFACE_WITH_KNOTS((2,2),(3,2,3),(0.,0.289681084359921),(0.556108173865716,
0.571428571428571,0.573654350219911),.UNSPECIFIED.)
GEOMETRIC_REPRESENTATION_ITEM()
RATIONAL_B_SPLINE_SURFACE(((0.991551633675927,0.994622399056526,1.,0.999218731101516,
0.99848615229188),(0.991551633675927,0.994622399056526,1.,0.999218731101516,
0.99848615229188)))
REPRESENTATION_ITEM('')
SURFACE()
);
#3220=(
BOUNDED_SURFACE()
B_SPLINE_SURFACE(1,2,((#148917,#148918,#148919,#148920,#148921),(#148922,
#148923,#148924,#148925,#148926)),.UNSPECIFIED.,.F.,.F.,.F.)
B_SPLINE_SURFACE_WITH_KNOTS((2,2),(3,2,3),(0.,0.290396316312529),(0.159312132623513,
0.159901408087481,0.177069452526137),.UNSPECIFIED.)
GEOMETRIC_REPRESENTATION_ITEM()
RATIONAL_B_SPLINE_SURFACE(((0.990889788836284,0.990889788836284,0.990889788836284,
0.987739559362111,0.987486127973996),(0.990889788836284,0.990889788836284,
0.990889788836284,0.987739559362111,0.987486127973996)))
REPRESENTATION_ITEM('')
SURFACE()
);
#3221=(
BOUNDED_SURFACE()
B_SPLINE_SURFACE(1,2,((#148949,#148950,#148951,#148952,#148953),(#148954,
#148955,#148956,#148957,#148958)),.UNSPECIFIED.,.F.,.F.,.F.)
B_SPLINE_SURFACE_WITH_KNOTS((2,2),(3,2,3),(0.,0.289681084359925),(0.556108173865716,
0.571428571428571,0.573654350219911),.UNSPECIFIED.)
GEOMETRIC_REPRESENTATION_ITEM()
RATIONAL_B_SPLINE_SURFACE(((0.991551633675927,0.994622399056526,1.,0.999218731101516,
0.99848615229188),(0.991551633675927,0.994622399056526,1.,0.999218731101516,
0.99848615229188)))
REPRESENTATION_ITEM('')
SURFACE()
);
#3222=(
BOUNDED_SURFACE()
B_SPLINE_SURFACE(1,2,((#148960,#148961,#148962,#148963,#148964),(#148965,
#148966,#148967,#148968,#148969)),.UNSPECIFIED.,.F.,.F.,.F.)
B_SPLINE_SURFACE_WITH_KNOTS((2,2),(3,2,3),(0.,0.290396316323544),(0.159312132612491,
0.159901408087481,0.177069452526134),.UNSPECIFIED.)
GEOMETRIC_REPRESENTATION_ITEM()
RATIONAL_B_SPLINE_SURFACE(((0.990889788836284,0.990889788836284,0.990889788836284,
0.987739559362111,0.987486127973996),(0.990889788836284,0.990889788836284,
0.990889788836284,0.987739559362111,0.987486127973996)))
REPRESENTATION_ITEM('')
SURFACE()
);
#3223=(
BOUNDED_SURFACE()
B_SPLINE_SURFACE(1,2,((#148992,#148993,#148994,#148995,#148996),(#148997,
#148998,#148999,#149000,#149001)),.UNSPECIFIED.,.F.,.F.,.F.)
B_SPLINE_SURFACE_WITH_KNOTS((2,2),(3,2,3),(0.,0.289681084359926),(0.556108173865715,
0.571428571428571,0.573654350219911),.UNSPECIFIED.)
GEOMETRIC_REPRESENTATION_ITEM()
RATIONAL_B_SPLINE_SURFACE(((0.991551633675927,0.994622399056526,1.,0.999218731101516,
0.99848615229188),(0.991551633675927,0.994622399056526,1.,0.999218731101516,
0.99848615229188)))
REPRESENTATION_ITEM('')
SURFACE()
);
#3224=(
BOUNDED_SURFACE()
B_SPLINE_SURFACE(1,2,((#149003,#149004,#149005,#149006,#149007),(#149008,
#149009,#149010,#149011,#149012)),.UNSPECIFIED.,.F.,.F.,.F.)
B_SPLINE_SURFACE_WITH_KNOTS((2,2),(3,2,3),(0.,0.290396316297854),(0.159312132638184,
0.159901408087481,0.177069452526137),.UNSPECIFIED.)
GEOMETRIC_REPRESENTATION_ITEM()
RATIONAL_B_SPLINE_SURFACE(((0.990889788836284,0.990889788836284,0.990889788836284,
0.987739559362111,0.987486127973996),(0.990889788836284,0.990889788836284,
0.990889788836284,0.987739559362111,0.987486127973996)))
REPRESENTATION_ITEM('')
SURFACE()
);
#3225=(
BOUNDED_SURFACE()
B_SPLINE_SURFACE(1,2,((#149035,#149036,#149037,#149038,#149039),(#149040,
#149041,#149042,#149043,#149044)),.UNSPECIFIED.,.F.,.F.,.F.)
B_SPLINE_SURFACE_WITH_KNOTS((2,2),(3,2,3),(0.,0.289681084359916),(0.556108173865716,
0.571428571428571,0.573654350219911),.UNSPECIFIED.)
GEOMETRIC_REPRESENTATION_ITEM()
RATIONAL_B_SPLINE_SURFACE(((0.991551633675927,0.994622399056526,1.,0.999218731101516,
0.99848615229188),(0.991551633675927,0.994622399056526,1.,0.999218731101516,
0.99848615229188)))
REPRESENTATION_ITEM('')
SURFACE()
);
#3226=(
BOUNDED_SURFACE()
B_SPLINE_SURFACE(1,2,((#149046,#149047,#149048,#149049,#149050),(#149051,
#149052,#149053,#149054,#149055)),.UNSPECIFIED.,.F.,.F.,.F.)
B_SPLINE_SURFACE_WITH_KNOTS((2,2),(3,2,3),(0.,0.290396316321037),(0.159312132615002,
0.159901408087481,0.177069452526137),.UNSPECIFIED.)
GEOMETRIC_REPRESENTATION_ITEM()
RATIONAL_B_SPLINE_SURFACE(((0.990889788836284,0.990889788836284,0.990889788836284,
0.987739559362111,0.987486127973996),(0.990889788836284,0.990889788836284,
0.990889788836284,0.987739559362111,0.987486127973996)))
REPRESENTATION_ITEM('')
SURFACE()
);
#3227=(
BOUNDED_SURFACE()
B_SPLINE_SURFACE(1,2,((#149078,#149079,#149080,#149081,#149082),(#149083,
#149084,#149085,#149086,#149087)),.UNSPECIFIED.,.F.,.F.,.F.)
B_SPLINE_SURFACE_WITH_KNOTS((2,2),(3,2,3),(0.,0.289681084359916),(0.556108173865716,
0.571428571428571,0.573654350219911),.UNSPECIFIED.)
GEOMETRIC_REPRESENTATION_ITEM()
RATIONAL_B_SPLINE_SURFACE(((0.991551633675927,0.994622399056526,1.,0.999218731101516,
0.99848615229188),(0.991551633675927,0.994622399056526,1.,0.999218731101516,
0.99848615229188)))
REPRESENTATION_ITEM('')
SURFACE()
);
#3228=(
BOUNDED_SURFACE()
B_SPLINE_SURFACE(1,2,((#149089,#149090,#149091,#149092,#149093),(#149094,
#149095,#149096,#149097,#149098)),.UNSPECIFIED.,.F.,.F.,.F.)
B_SPLINE_SURFACE_WITH_KNOTS((2,2),(3,2,3),(0.,0.290396316329746),(0.159312132606293,
0.159901408087481,0.177069452526137),.UNSPECIFIED.)
GEOMETRIC_REPRESENTATION_ITEM()
RATIONAL_B_SPLINE_SURFACE(((0.990889788836284,0.990889788836284,0.990889788836284,
0.987739559362111,0.987486127973996),(0.990889788836284,0.990889788836284,
0.990889788836284,0.987739559362111,0.987486127973996)))
REPRESENTATION_ITEM('')
SURFACE()
);
#3229=(
BOUNDED_SURFACE()
B_SPLINE_SURFACE(1,2,((#149121,#149122,#149123,#149124,#149125),(#149126,
#149127,#149128,#149129,#149130)),.UNSPECIFIED.,.F.,.F.,.F.)
B_SPLINE_SURFACE_WITH_KNOTS((2,2),(3,2,3),(0.,0.289681084359916),(0.556108173865716,
0.571428571428571,0.573654350219912),.UNSPECIFIED.)
GEOMETRIC_REPRESENTATION_ITEM()
RATIONAL_B_SPLINE_SURFACE(((0.991551633675927,0.994622399056526,1.,0.999218731101516,
0.998486152291879),(0.991551633675927,0.994622399056526,1.,0.999218731101516,
0.998486152291879)))
REPRESENTATION_ITEM('')
SURFACE()
);
#3230=(
BOUNDED_SURFACE()
B_SPLINE_SURFACE(1,2,((#149132,#149133,#149134,#149135,#149136),(#149137,
#149138,#149139,#149140,#149141)),.UNSPECIFIED.,.F.,.F.,.F.)
B_SPLINE_SURFACE_WITH_KNOTS((2,2),(3,2,3),(0.,0.290396316316584),(0.15931213261945,
0.159901408087403,0.177069452526137),.UNSPECIFIED.)
GEOMETRIC_REPRESENTATION_ITEM()
RATIONAL_B_SPLINE_SURFACE(((0.990889788836313,0.990889788836313,0.990889788836313,
0.987739559362112,0.987486127973996),(0.990889788836313,0.990889788836313,
0.990889788836313,0.987739559362112,0.987486127973996)))
REPRESENTATION_ITEM('')
SURFACE()
);
#3231=(
BOUNDED_SURFACE()
B_SPLINE_SURFACE(1,2,((#149164,#149165,#149166,#149167,#149168),(#149169,
#149170,#149171,#149172,#149173)),.UNSPECIFIED.,.F.,.F.,.F.)
B_SPLINE_SURFACE_WITH_KNOTS((2,2),(3,2,3),(0.,0.289681084359918),(0.556108173865716,
0.571428571428571,0.573654350219911),.UNSPECIFIED.)
GEOMETRIC_REPRESENTATION_ITEM()
RATIONAL_B_SPLINE_SURFACE(((0.991551633675927,0.994622399056526,1.,0.999218731101516,
0.99848615229188),(0.991551633675927,0.994622399056526,1.,0.999218731101516,
0.99848615229188)))
REPRESENTATION_ITEM('')
SURFACE()
);
#3232=(
BOUNDED_SURFACE()
B_SPLINE_SURFACE(1,2,((#149175,#149176,#149177,#149178,#149179),(#149180,
#149181,#149182,#149183,#149184)),.UNSPECIFIED.,.F.,.F.,.F.)
B_SPLINE_SURFACE_WITH_KNOTS((2,2),(3,2,3),(0.,0.290396316309421),(0.159312132626621,
0.159901408087481,0.177069452526137),.UNSPECIFIED.)
GEOMETRIC_REPRESENTATION_ITEM()
RATIONAL_B_SPLINE_SURFACE(((0.990889788836284,0.990889788836284,0.990889788836284,
0.987739559362111,0.987486127973996),(0.990889788836284,0.990889788836284,
0.990889788836284,0.987739559362111,0.987486127973996)))
REPRESENTATION_ITEM('')
SURFACE()
);
#3233=(
BOUNDED_SURFACE()
B_SPLINE_SURFACE(1,2,((#149207,#149208,#149209,#149210,#149211),(#149212,
#149213,#149214,#149215,#149216)),.UNSPECIFIED.,.F.,.F.,.F.)
B_SPLINE_SURFACE_WITH_KNOTS((2,2),(3,2,3),(0.,0.28968108435992),(0.556108173865716,
0.571428571428571,0.573654350219911),.UNSPECIFIED.)
GEOMETRIC_REPRESENTATION_ITEM()
RATIONAL_B_SPLINE_SURFACE(((0.991551633675927,0.994622399056526,1.,0.999218731101516,
0.99848615229188),(0.991551633675927,0.994622399056526,1.,0.999218731101516,
0.99848615229188)))
REPRESENTATION_ITEM('')
SURFACE()
);
#3234=(
BOUNDED_SURFACE()
B_SPLINE_SURFACE(1,2,((#149218,#149219,#149220,#149221,#149222),(#149223,
#149224,#149225,#149226,#149227)),.UNSPECIFIED.,.F.,.F.,.F.)
B_SPLINE_SURFACE_WITH_KNOTS((2,2),(3,2,3),(0.,0.290396316330743),(0.159312132605295,
0.159901408087481,0.177069452526134),.UNSPECIFIED.)
GEOMETRIC_REPRESENTATION_ITEM()
RATIONAL_B_SPLINE_SURFACE(((0.990889788836284,0.990889788836284,0.990889788836284,
0.987739559362111,0.987486127973996),(0.990889788836284,0.990889788836284,
0.990889788836284,0.987739559362111,0.987486127973996)))
REPRESENTATION_ITEM('')
SURFACE()
);
#3235=(
BOUNDED_SURFACE()
B_SPLINE_SURFACE(1,2,((#149250,#149251,#149252,#149253,#149254),(#149255,
#149256,#149257,#149258,#149259)),.UNSPECIFIED.,.F.,.F.,.F.)
B_SPLINE_SURFACE_WITH_KNOTS((2,2),(3,2,3),(0.,0.28968108435992),(0.556108173865715,
0.571428571428571,0.573654350219911),.UNSPECIFIED.)
GEOMETRIC_REPRESENTATION_ITEM()
RATIONAL_B_SPLINE_SURFACE(((0.991551633675927,0.994622399056526,1.,0.999218731101516,
0.99848615229188),(0.991551633675927,0.994622399056526,1.,0.999218731101516,
0.99848615229188)))
REPRESENTATION_ITEM('')
SURFACE()
);
#3236=(
BOUNDED_SURFACE()
B_SPLINE_SURFACE(1,2,((#149261,#149262,#149263,#149264,#149265),(#149266,
#149267,#149268,#149269,#149270)),.UNSPECIFIED.,.F.,.F.,.F.)
B_SPLINE_SURFACE_WITH_KNOTS((2,2),(3,2,3),(0.,0.290396316298905),(0.159312132637135,
0.159901408087481,0.177069452526134),.UNSPECIFIED.)
GEOMETRIC_REPRESENTATION_ITEM()
RATIONAL_B_SPLINE_SURFACE(((0.990889788836284,0.990889788836284,0.990889788836284,
0.987739559362111,0.987486127973996),(0.990889788836284,0.990889788836284,
0.990889788836284,0.987739559362111,0.987486127973996)))
REPRESENTATION_ITEM('')
SURFACE()
);
#3237=(
BOUNDED_SURFACE()
B_SPLINE_SURFACE(1,2,((#149293,#149294,#149295,#149296,#149297),(#149298,
#149299,#149300,#149301,#149302)),.UNSPECIFIED.,.F.,.F.,.F.)
B_SPLINE_SURFACE_WITH_KNOTS((2,2),(3,2,3),(0.,0.289681084359918),(0.556108173865715,
0.571428571428571,0.573654350219912),.UNSPECIFIED.)
GEOMETRIC_REPRESENTATION_ITEM()
RATIONAL_B_SPLINE_SURFACE(((0.991551633675927,0.994622399056526,1.,0.999218731101516,
0.998486152291879),(0.991551633675927,0.994622399056526,1.,0.999218731101516,
0.998486152291879)))
REPRESENTATION_ITEM('')
SURFACE()
);
#3238=(
BOUNDED_SURFACE()
B_SPLINE_SURFACE(1,2,((#149304,#149305,#149306,#149307,#149308),(#149309,
#149310,#149311,#149312,#149313)),.UNSPECIFIED.,.F.,.F.,.F.)
B_SPLINE_SURFACE_WITH_KNOTS((2,2),(3,2,3),(0.,0.290030945106622),(0.159677503829416,
0.159901408087481,0.177069452526137),.UNSPECIFIED.)
GEOMETRIC_REPRESENTATION_ITEM()
RATIONAL_B_SPLINE_SURFACE(((0.990889788836284,0.990889788836284,0.990889788836284,
0.987739559362111,0.987486127973996),(0.990889788836284,0.990889788836284,
0.990889788836284,0.987739559362111,0.987486127973996)))
REPRESENTATION_ITEM('')
SURFACE()
);
#3239=(
BOUNDED_SURFACE()
B_SPLINE_SURFACE(1,2,((#149321,#149322,#149323,#149324,#149325),(#149326,
#149327,#149328,#149329,#149330)),.UNSPECIFIED.,.F.,.F.,.F.)
B_SPLINE_SURFACE_WITH_KNOTS((2,2),(3,2,3),(0.,0.289681084359918),(0.556108173865716,
0.571428571428571,0.573654350219912),.UNSPECIFIED.)
GEOMETRIC_REPRESENTATION_ITEM()
RATIONAL_B_SPLINE_SURFACE(((0.991551633675927,0.994622399056526,1.,0.999218731101515,
0.998486152291879),(0.991551633675927,0.994622399056526,1.,0.999218731101515,
0.998486152291879)))
REPRESENTATION_ITEM('')
SURFACE()
);
#3240=(
BOUNDED_SURFACE()
B_SPLINE_SURFACE(1,2,((#149332,#149333,#149334,#149335,#149336),(#149337,
#149338,#149339,#149340,#149341)),.UNSPECIFIED.,.F.,.F.,.F.)
B_SPLINE_SURFACE_WITH_KNOTS((2,2),(3,2,3),(0.,0.290396316295841),(0.159312132640196,
0.159901408087481,0.177069452526134),.UNSPECIFIED.)
GEOMETRIC_REPRESENTATION_ITEM()
RATIONAL_B_SPLINE_SURFACE(((0.990889788836284,0.990889788836284,0.990889788836284,
0.987739559362111,0.987486127973996),(0.990889788836284,0.990889788836284,
0.990889788836284,0.987739559362111,0.987486127973996)))
REPRESENTATION_ITEM('')
SURFACE()
);
#3241=(
BOUNDED_SURFACE()
B_SPLINE_SURFACE(1,2,((#149364,#149365,#149366,#149367,#149368),(#149369,
#149370,#149371,#149372,#149373)),.UNSPECIFIED.,.F.,.F.,.F.)
B_SPLINE_SURFACE_WITH_KNOTS((2,2),(3,2,3),(0.,0.289681084359917),(0.556108173865715,
0.571428571428571,0.573654350219912),.UNSPECIFIED.)
GEOMETRIC_REPRESENTATION_ITEM()
RATIONAL_B_SPLINE_SURFACE(((0.991551633675927,0.994622399056526,1.,0.999218731101515,
0.998486152291879),(0.991551633675927,0.994622399056526,1.,0.999218731101515,
0.998486152291879)))
REPRESENTATION_ITEM('')
SURFACE()
);
#3242=(
BOUNDED_SURFACE()
B_SPLINE_SURFACE(1,2,((#149375,#149376,#149377,#149378,#149379),(#149380,
#149381,#149382,#149383,#149384)),.UNSPECIFIED.,.F.,.F.,.F.)
B_SPLINE_SURFACE_WITH_KNOTS((2,2),(3,2,3),(0.,0.290396316316367),(0.159312132619674,
0.159901408087481,0.177069452526137),.UNSPECIFIED.)
GEOMETRIC_REPRESENTATION_ITEM()
RATIONAL_B_SPLINE_SURFACE(((0.990889788836284,0.990889788836284,0.990889788836284,
0.987739559362111,0.987486127973996),(0.990889788836284,0.990889788836284,
0.990889788836284,0.987739559362111,0.987486127973996)))
REPRESENTATION_ITEM('')
SURFACE()
);
#3243=(
BOUNDED_SURFACE()
B_SPLINE_SURFACE(1,2,((#149407,#149408,#149409,#149410,#149411),(#149412,
#149413,#149414,#149415,#149416)),.UNSPECIFIED.,.F.,.F.,.F.)
B_SPLINE_SURFACE_WITH_KNOTS((2,2),(3,2,3),(0.,0.28968108435992),(0.556108173865716,
0.571428571428571,0.573654350219911),.UNSPECIFIED.)
GEOMETRIC_REPRESENTATION_ITEM()
RATIONAL_B_SPLINE_SURFACE(((0.991551633675927,0.994622399056526,1.,0.999218731101516,
0.99848615229188),(0.991551633675927,0.994622399056526,1.,0.999218731101516,
0.99848615229188)))
REPRESENTATION_ITEM('')
SURFACE()
);
#3244=(
BOUNDED_SURFACE()
B_SPLINE_SURFACE(1,2,((#149418,#149419,#149420,#149421,#149422),(#149423,
#149424,#149425,#149426,#149427)),.UNSPECIFIED.,.F.,.F.,.F.)
B_SPLINE_SURFACE_WITH_KNOTS((2,2),(3,2,3),(0.,0.290396316321617),(0.159312132614422,
0.159901408087481,0.177069452526137),.UNSPECIFIED.)
GEOMETRIC_REPRESENTATION_ITEM()
RATIONAL_B_SPLINE_SURFACE(((0.990889788836284,0.990889788836284,0.990889788836284,
0.987739559362111,0.987486127973996),(0.990889788836284,0.990889788836284,
0.990889788836284,0.987739559362111,0.987486127973996)))
REPRESENTATION_ITEM('')
SURFACE()
);
#3245=(
BOUNDED_SURFACE()
B_SPLINE_SURFACE(1,2,((#149450,#149451,#149452,#149453,#149454),(#149455,
#149456,#149457,#149458,#149459)),.UNSPECIFIED.,.F.,.F.,.F.)
B_SPLINE_SURFACE_WITH_KNOTS((2,2),(3,2,3),(0.,0.289681084359918),(0.556108173865716,
0.571428571428571,0.573654350219911),.UNSPECIFIED.)
GEOMETRIC_REPRESENTATION_ITEM()
RATIONAL_B_SPLINE_SURFACE(((0.991551633675927,0.994622399056526,1.,0.999218731101516,
0.99848615229188),(0.991551633675927,0.994622399056526,1.,0.999218731101516,
0.99848615229188)))
REPRESENTATION_ITEM('')
SURFACE()
);
#3246=(
BOUNDED_SURFACE()
B_SPLINE_SURFACE(1,2,((#149461,#149462,#149463,#149464,#149465),(#149466,
#149467,#149468,#149469,#149470)),.UNSPECIFIED.,.F.,.F.,.F.)
B_SPLINE_SURFACE_WITH_KNOTS((2,2),(3,2,3),(0.,0.290396316324553),(0.15931213261148,
0.159901408087481,0.177069452526137),.UNSPECIFIED.)
GEOMETRIC_REPRESENTATION_ITEM()
RATIONAL_B_SPLINE_SURFACE(((0.990889788836284,0.990889788836284,0.990889788836284,
0.987739559362111,0.987486127973996),(0.990889788836284,0.990889788836284,
0.990889788836284,0.987739559362111,0.987486127973996)))
REPRESENTATION_ITEM('')
SURFACE()
);
#3247=(
BOUNDED_SURFACE()
B_SPLINE_SURFACE(1,2,((#149481,#149482,#149483,#149484,#149485),(#149486,
#149487,#149488,#149489,#149490)),.UNSPECIFIED.,.F.,.F.,.F.)
B_SPLINE_SURFACE_WITH_KNOTS((2,2),(3,2,3),(0.,0.28968108435992),(0.556108173865716,
0.571428571428571,0.573654350219911),.UNSPECIFIED.)
GEOMETRIC_REPRESENTATION_ITEM()
RATIONAL_B_SPLINE_SURFACE(((0.991551633675927,0.994622399056526,1.,0.999218731101516,
0.99848615229188),(0.991551633675927,0.994622399056526,1.,0.999218731101516,
0.99848615229188)))
REPRESENTATION_ITEM('')
SURFACE()
);
#3248=(
BOUNDED_SURFACE()
B_SPLINE_SURFACE(1,2,((#149504,#149505,#149506,#149507,#149508),(#149509,
#149510,#149511,#149512,#149513)),.UNSPECIFIED.,.F.,.F.,.F.)
B_SPLINE_SURFACE_WITH_KNOTS((2,2),(3,2,3),(0.,0.29039631631159),(0.159312132624448,
0.159901408087475,0.177069452526134),.UNSPECIFIED.)
GEOMETRIC_REPRESENTATION_ITEM()
RATIONAL_B_SPLINE_SURFACE(((0.990889788836286,0.990889788836286,0.990889788836286,
0.987739559362111,0.987486127973996),(0.990889788836286,0.990889788836286,
0.990889788836286,0.987739559362112,0.987486127973996)))
REPRESENTATION_ITEM('')
SURFACE()
);
#3249=(
BOUNDED_SURFACE()
B_SPLINE_SURFACE(1,2,((#149536,#149537,#149538,#149539,#149540),(#149541,
#149542,#149543,#149544,#149545)),.UNSPECIFIED.,.F.,.F.,.F.)
B_SPLINE_SURFACE_WITH_KNOTS((2,2),(3,2,3),(0.,0.289681084360114),(0.556108173865715,
0.571428571428571,0.573654350219913),.UNSPECIFIED.)
GEOMETRIC_REPRESENTATION_ITEM()
RATIONAL_B_SPLINE_SURFACE(((0.991551633675927,0.994622399056526,1.,0.999218731101515,
0.998486152291879),(0.991551633675927,0.994622399056526,1.,0.999218731101515,
0.998486152291879)))
REPRESENTATION_ITEM('')
SURFACE()
);
#3250=(
BOUNDED_SURFACE()
B_SPLINE_SURFACE(1,2,((#149547,#149548,#149549,#149550,#149551),(#149552,
#149553,#149554,#149555,#149556)),.UNSPECIFIED.,.F.,.F.,.F.)
B_SPLINE_SURFACE_WITH_KNOTS((2,2),(3,2,3),(0.,0.290396316325579),(0.159312132610595,
0.159901408087482,0.177069452526135),.UNSPECIFIED.)
GEOMETRIC_REPRESENTATION_ITEM()
RATIONAL_B_SPLINE_SURFACE(((0.990889788836284,0.990889788836284,0.990889788836284,
0.987739559362111,0.987486127973996),(0.990889788836284,0.990889788836284,
0.990889788836284,0.987739559362111,0.987486127973996)))
REPRESENTATION_ITEM('')
SURFACE()
);
#3251=(
BOUNDED_SURFACE()
B_SPLINE_SURFACE(1,2,((#149579,#149580,#149581,#149582,#149583),(#149584,
#149585,#149586,#149587,#149588)),.UNSPECIFIED.,.F.,.F.,.F.)
B_SPLINE_SURFACE_WITH_KNOTS((2,2),(3,2,3),(0.,0.289681084360813),(0.556108173865714,
0.571428571428571,0.573654350219921),.UNSPECIFIED.)
GEOMETRIC_REPRESENTATION_ITEM()
RATIONAL_B_SPLINE_SURFACE(((0.991551633675927,0.994622399056525,1.,0.999218731101512,
0.998486152291873),(0.991551633675927,0.994622399056525,1.,0.999218731101512,
0.998486152291873)))
REPRESENTATION_ITEM('')
SURFACE()
);
#3252=(
BOUNDED_SURFACE()
B_SPLINE_SURFACE(1,2,((#149590,#149591,#149592,#149593,#149594),(#149595,
#149596,#149597,#149598,#149599)),.UNSPECIFIED.,.F.,.F.,.F.)
B_SPLINE_SURFACE_WITH_KNOTS((2,2),(3,2,3),(0.,0.290396316336308),(0.159312132599877,
0.159901408087482,0.177069452526135),.UNSPECIFIED.)
GEOMETRIC_REPRESENTATION_ITEM()
RATIONAL_B_SPLINE_SURFACE(((0.990889788836284,0.990889788836284,0.990889788836284,
0.987739559362111,0.987486127973995),(0.990889788836284,0.990889788836284,
0.990889788836284,0.987739559362111,0.987486127973995)))
REPRESENTATION_ITEM('')
SURFACE()
);
#3253=(
BOUNDED_SURFACE()
B_SPLINE_SURFACE(1,2,((#149622,#149623,#149624,#149625,#149626),(#149627,
#149628,#149629,#149630,#149631)),.UNSPECIFIED.,.F.,.F.,.F.)
B_SPLINE_SURFACE_WITH_KNOTS((2,2),(3,2,3),(0.,0.289681084360947),(0.556108173865714,
0.571428571428571,0.57365435021992),.UNSPECIFIED.)
GEOMETRIC_REPRESENTATION_ITEM()
RATIONAL_B_SPLINE_SURFACE(((0.991551633675927,0.994622399056525,1.,0.999218731101513,
0.998486152291874),(0.991551633675927,0.994622399056525,1.,0.999218731101513,
0.998486152291874)))
REPRESENTATION_ITEM('')
SURFACE()
);
#3254=(
BOUNDED_SURFACE()
B_SPLINE_SURFACE(1,2,((#149633,#149634,#149635,#149636,#149637),(#149638,
#149639,#149640,#149641,#149642)),.UNSPECIFIED.,.F.,.F.,.F.)
B_SPLINE_SURFACE_WITH_KNOTS((2,2),(3,2,3),(0.,0.29039631630548),(0.159312132630947,
0.159901408087482,0.177069452526138),.UNSPECIFIED.)
GEOMETRIC_REPRESENTATION_ITEM()
RATIONAL_B_SPLINE_SURFACE(((0.990889788836284,0.990889788836284,0.990889788836284,
0.98773955936211,0.987486127973996),(0.990889788836284,0.990889788836284,
0.990889788836284,0.98773955936211,0.987486127973996)))
REPRESENTATION_ITEM('')
SURFACE()
);
#3255=(
BOUNDED_SURFACE()
B_SPLINE_SURFACE(1,2,((#149665,#149666,#149667,#149668,#149669),(#149670,
#149671,#149672,#149673,#149674)),.UNSPECIFIED.,.F.,.F.,.F.)
B_SPLINE_SURFACE_WITH_KNOTS((2,2),(3,2,3),(0.,0.289681084360913),(0.556108173865715,
0.571428571428571,0.573654350219922),.UNSPECIFIED.)
GEOMETRIC_REPRESENTATION_ITEM()
RATIONAL_B_SPLINE_SURFACE(((0.991551633675927,0.994622399056525,1.,0.999218731101512,
0.998486152291872),(0.991551633675927,0.994622399056525,1.,0.999218731101512,
0.998486152291872)))
REPRESENTATION_ITEM('')
SURFACE()
);
#3256=(
BOUNDED_SURFACE()
B_SPLINE_SURFACE(1,2,((#149676,#149677,#149678,#149679,#149680),(#149681,
#149682,#149683,#149684,#149685)),.UNSPECIFIED.,.F.,.F.,.F.)
B_SPLINE_SURFACE_WITH_KNOTS((2,2),(3,2,3),(0.,0.290396316326519),(0.159312132611315,
0.159901408087482,0.177069452526135),.UNSPECIFIED.)
GEOMETRIC_REPRESENTATION_ITEM()
RATIONAL_B_SPLINE_SURFACE(((0.990889788836284,0.990889788836284,0.990889788836284,
0.987739559362111,0.987486127973996),(0.990889788836284,0.990889788836284,
0.990889788836284,0.987739559362111,0.987486127973996)))
REPRESENTATION_ITEM('')
SURFACE()
);
#3257=(
BOUNDED_SURFACE()
B_SPLINE_SURFACE(1,2,((#149708,#149709,#149710,#149711,#149712),(#149713,
#149714,#149715,#149716,#149717)),.UNSPECIFIED.,.F.,.F.,.F.)
B_SPLINE_SURFACE_WITH_KNOTS((2,2),(3,2,3),(0.,0.289681084360124),(0.556108173865714,
0.571428571428571,0.57365435021991),.UNSPECIFIED.)
GEOMETRIC_REPRESENTATION_ITEM()
RATIONAL_B_SPLINE_SURFACE(((0.991551633675927,0.994622399056525,1.,0.999218731101516,
0.99848615229188),(0.991551633675927,0.994622399056525,1.,0.999218731101516,
0.99848615229188)))
REPRESENTATION_ITEM('')
SURFACE()
);
#3258=(
BOUNDED_SURFACE()
B_SPLINE_SURFACE(1,2,((#149719,#149720,#149721,#149722,#149723),(#149724,
#149725,#149726,#149727,#149728)),.UNSPECIFIED.,.F.,.F.,.F.)
B_SPLINE_SURFACE_WITH_KNOTS((2,2),(3,2,3),(0.,0.290396316316441),(0.159312132620063,
0.159901408087455,0.177069452526135),.UNSPECIFIED.)
GEOMETRIC_REPRESENTATION_ITEM()
RATIONAL_B_SPLINE_SURFACE(((0.990889788836294,0.990889788836294,0.990889788836294,
0.987739559362111,0.987486127973996),(0.990889788836294,0.990889788836294,
0.990889788836294,0.987739559362111,0.987486127973996)))
REPRESENTATION_ITEM('')
SURFACE()
);
#3259=(
BOUNDED_SURFACE()
B_SPLINE_SURFACE(1,2,((#149751,#149752,#149753,#149754,#149755),(#149756,
#149757,#149758,#149759,#149760)),.UNSPECIFIED.,.F.,.F.,.F.)
B_SPLINE_SURFACE_WITH_KNOTS((2,2),(3,2,3),(0.,0.289681084359929),(0.556108173865714,
0.571428571428571,0.57365435021991),.UNSPECIFIED.)
GEOMETRIC_REPRESENTATION_ITEM()
RATIONAL_B_SPLINE_SURFACE(((0.991551633675927,0.994622399056525,1.,0.999218731101516,
0.99848615229188),(0.991551633675927,0.994622399056525,1.,0.999218731101516,
0.99848615229188)))
REPRESENTATION_ITEM('')
SURFACE()
);
#3260=(
BOUNDED_SURFACE()
B_SPLINE_SURFACE(1,2,((#149762,#149763,#149764,#149765,#149766),(#149767,
#149768,#149769,#149770,#149771)),.UNSPECIFIED.,.F.,.F.,.F.)
B_SPLINE_SURFACE_WITH_KNOTS((2,2),(3,2,3),(0.,0.29039631630902),(0.159312132627105,
0.159901408087482,0.177069452526138),.UNSPECIFIED.)
GEOMETRIC_REPRESENTATION_ITEM()
RATIONAL_B_SPLINE_SURFACE(((0.990889788836284,0.990889788836284,0.990889788836284,
0.98773955936211,0.987486127973996),(0.990889788836284,0.990889788836284,
0.990889788836284,0.98773955936211,0.987486127973996)))
REPRESENTATION_ITEM('')
SURFACE()
);
#3261=(
BOUNDED_SURFACE()
B_SPLINE_SURFACE(1,2,((#149794,#149795,#149796,#149797,#149798),(#149799,
#149800,#149801,#149802,#149803)),.UNSPECIFIED.,.F.,.F.,.F.)
B_SPLINE_SURFACE_WITH_KNOTS((2,2),(3,2,3),(0.,0.289681084359923),(0.556108173865714,
0.571428571428571,0.57365435021991),.UNSPECIFIED.)
GEOMETRIC_REPRESENTATION_ITEM()
RATIONAL_B_SPLINE_SURFACE(((0.991551633675927,0.994622399056525,1.,0.999218731101516,
0.99848615229188),(0.991551633675927,0.994622399056525,1.,0.999218731101516,
0.99848615229188)))
REPRESENTATION_ITEM('')
SURFACE()
);
#3262=(
BOUNDED_SURFACE()
B_SPLINE_SURFACE(1,2,((#149805,#149806,#149807,#149808,#149809),(#149810,
#149811,#149812,#149813,#149814)),.UNSPECIFIED.,.F.,.F.,.F.)
B_SPLINE_SURFACE_WITH_KNOTS((2,2),(3,2,3),(0.,0.290396316315867),(0.159312132620248,
0.159901408087482,0.177069452526135),.UNSPECIFIED.)
GEOMETRIC_REPRESENTATION_ITEM()
RATIONAL_B_SPLINE_SURFACE(((0.990889788836284,0.990889788836284,0.990889788836284,
0.987739559362111,0.987486127973996),(0.990889788836284,0.990889788836284,
0.990889788836284,0.987739559362111,0.987486127973996)))
REPRESENTATION_ITEM('')
SURFACE()
);
#3263=(
BOUNDED_SURFACE()
B_SPLINE_SURFACE(1,2,((#149837,#149838,#149839,#149840,#149841),(#149842,
#149843,#149844,#149845,#149846)),.UNSPECIFIED.,.F.,.F.,.F.)
B_SPLINE_SURFACE_WITH_KNOTS((2,2),(3,2,3),(0.,0.289681084359919),(0.556108173865714,
0.571428571428571,0.57365435021991),.UNSPECIFIED.)
GEOMETRIC_REPRESENTATION_ITEM()
RATIONAL_B_SPLINE_SURFACE(((0.991551633675927,0.994622399056525,1.,0.999218731101516,
0.99848615229188),(0.991551633675927,0.994622399056525,1.,0.999218731101516,
0.99848615229188)))
REPRESENTATION_ITEM('')
SURFACE()
);
#3264=(
BOUNDED_SURFACE()
B_SPLINE_SURFACE(1,2,((#149848,#149849,#149850,#149851,#149852),(#149853,
#149854,#149855,#149856,#149857)),.UNSPECIFIED.,.F.,.F.,.F.)
B_SPLINE_SURFACE_WITH_KNOTS((2,2),(3,2,3),(0.,0.290396316320743),(0.159312132615369,
0.159901408087482,0.177069452526135),.UNSPECIFIED.)
GEOMETRIC_REPRESENTATION_ITEM()
RATIONAL_B_SPLINE_SURFACE(((0.990889788836284,0.990889788836284,0.990889788836284,
0.987739559362111,0.987486127973996),(0.990889788836284,0.990889788836284,
0.990889788836284,0.987739559362111,0.987486127973996)))
REPRESENTATION_ITEM('')
SURFACE()
);
#3265=(
BOUNDED_SURFACE()
B_SPLINE_SURFACE(1,2,((#149880,#149881,#149882,#149883,#149884),(#149885,
#149886,#149887,#149888,#149889)),.UNSPECIFIED.,.F.,.F.,.F.)
B_SPLINE_SURFACE_WITH_KNOTS((2,2),(3,2,3),(0.,0.289681084359923),(0.556108173865714,
0.571428571428571,0.57365435021991),.UNSPECIFIED.)
GEOMETRIC_REPRESENTATION_ITEM()
RATIONAL_B_SPLINE_SURFACE(((0.991551633675927,0.994622399056525,1.,0.999218731101516,
0.99848615229188),(0.991551633675927,0.994622399056525,1.,0.999218731101516,
0.99848615229188)))
REPRESENTATION_ITEM('')
SURFACE()
);
#3266=(
BOUNDED_SURFACE()
B_SPLINE_SURFACE(1,2,((#149891,#149892,#149893,#149894,#149895),(#149896,
#149897,#149898,#149899,#149900)),.UNSPECIFIED.,.F.,.F.,.F.)
B_SPLINE_SURFACE_WITH_KNOTS((2,2),(3,2,3),(0.,0.29039631629488),(0.159312132641506,
0.159901408087428,0.177069452526138),.UNSPECIFIED.)
GEOMETRIC_REPRESENTATION_ITEM()
RATIONAL_B_SPLINE_SURFACE(((0.990889788836304,0.990889788836304,0.990889788836304,
0.987739559362111,0.987486127973996),(0.990889788836304,0.990889788836304,
0.990889788836304,0.987739559362111,0.987486127973996)))
REPRESENTATION_ITEM('')
SURFACE()
);
#3267=(
BOUNDED_SURFACE()
B_SPLINE_SURFACE(1,2,((#149923,#149924,#149925,#149926,#149927),(#149928,
#149929,#149930,#149931,#149932)),.UNSPECIFIED.,.F.,.F.,.F.)
B_SPLINE_SURFACE_WITH_KNOTS((2,2),(3,2,3),(0.,0.289681084359927),(0.556108173865715,
0.571428571428571,0.57365435021991),.UNSPECIFIED.)
GEOMETRIC_REPRESENTATION_ITEM()
RATIONAL_B_SPLINE_SURFACE(((0.991551633675927,0.994622399056525,1.,0.999218731101516,
0.99848615229188),(0.991551633675927,0.994622399056525,1.,0.999218731101516,
0.99848615229188)))
REPRESENTATION_ITEM('')
SURFACE()
);
#3268=(
BOUNDED_SURFACE()
B_SPLINE_SURFACE(1,2,((#149934,#149935,#149936,#149937,#149938),(#149939,
#149940,#149941,#149942,#149943)),.UNSPECIFIED.,.F.,.F.,.F.)
B_SPLINE_SURFACE_WITH_KNOTS((2,2),(3,2,3),(0.709719018626781,1.),(0.607879027750091,
0.625170525609407,0.625770422837593),.UNSPECIFIED.)
GEOMETRIC_REPRESENTATION_ITEM()
RATIONAL_B_SPLINE_SURFACE(((0.987469282487682,0.987594391229382,0.990658108926708,
0.990658108926708,0.990658108926708),(0.987469282487682,0.987594391229382,
0.990658108926708,0.990658108926708,0.990658108926708)))
REPRESENTATION_ITEM('')
SURFACE()
);
#3269=(
BOUNDED_SURFACE()
B_SPLINE_SURFACE(1,2,((#149961,#149962,#149963),(#149964,#149965,#149966)),
 .UNSPECIFIED.,.F.,.F.,.F.)
B_SPLINE_SURFACE_WITH_KNOTS((2,2),(3,3),(0.71019295900798,1.),(0.107982157956012,
0.125273655815329),.UNSPECIFIED.)
GEOMETRIC_REPRESENTATION_ITEM()
RATIONAL_B_SPLINE_SURFACE(((0.987470879370255,0.987613514606721,0.990694758798813),
(0.987470879370256,0.987613514606721,0.990694758798813)))
REPRESENTATION_ITEM('')
SURFACE()
);
#3270=(
BOUNDED_SURFACE()
B_SPLINE_SURFACE(1,2,((#149973,#149974,#149975,#149976,#149977),(#149978,
#149979,#149980,#149981,#149982)),.UNSPECIFIED.,.F.,.F.,.F.)
B_SPLINE_SURFACE_WITH_KNOTS((2,2),(3,2,3),(0.709719018636767,1.),(0.607879027750091,
0.625170525609407,0.625770422827617),.UNSPECIFIED.)
GEOMETRIC_REPRESENTATION_ITEM()
RATIONAL_B_SPLINE_SURFACE(((0.987469282487682,0.987594391229382,0.990658108926708,
0.990658108926708,0.990658108926708),(0.987469282487682,0.987594391229382,
0.990658108926708,0.990658108926708,0.990658108926708)))
REPRESENTATION_ITEM('')
SURFACE()
);
#3271=(
BOUNDED_SURFACE()
B_SPLINE_SURFACE(1,2,((#150000,#150001,#150002),(#150003,#150004,#150005)),
 .UNSPECIFIED.,.F.,.F.,.F.)
B_SPLINE_SURFACE_WITH_KNOTS((2,2),(3,3),(0.710192959007998,1.),(0.107982157956012,
0.125273655815329),.UNSPECIFIED.)
GEOMETRIC_REPRESENTATION_ITEM()
RATIONAL_B_SPLINE_SURFACE(((0.987470879370255,0.987613514606721,0.990694758798813),
(0.987470879370256,0.987613514606721,0.990694758798813)))
REPRESENTATION_ITEM('')
SURFACE()
);
#3272=(
BOUNDED_SURFACE()
B_SPLINE_SURFACE(1,2,((#150012,#150013,#150014,#150015,#150016),(#150017,
#150018,#150019,#150020,#150021)),.UNSPECIFIED.,.F.,.F.,.F.)
B_SPLINE_SURFACE_WITH_KNOTS((2,2),(3,2,3),(0.709719018631378,1.),(0.607879027750091,
0.625170525609407,0.625770422833355),.UNSPECIFIED.)
GEOMETRIC_REPRESENTATION_ITEM()
RATIONAL_B_SPLINE_SURFACE(((0.987469282487682,0.987594391229382,0.990658108926709,
0.990658108926709,0.990658108926709),(0.987469282487682,0.987594391229382,
0.990658108926709,0.990658108926709,0.990658108926709)))
REPRESENTATION_ITEM('')
SURFACE()
);
#3273=(
BOUNDED_SURFACE()
B_SPLINE_SURFACE(1,2,((#150039,#150040,#150041),(#150042,#150043,#150044)),
 .UNSPECIFIED.,.F.,.F.,.F.)
B_SPLINE_SURFACE_WITH_KNOTS((2,2),(3,3),(0.710192959008343,1.),(0.107982157956012,
0.125273655815329),.UNSPECIFIED.)
GEOMETRIC_REPRESENTATION_ITEM()
RATIONAL_B_SPLINE_SURFACE(((0.987470879370255,0.987613514606721,0.990694758798813),
(0.987470879370256,0.987613514606721,0.990694758798813)))
REPRESENTATION_ITEM('')
SURFACE()
);
#3274=(
BOUNDED_SURFACE()
B_SPLINE_SURFACE(1,2,((#150051,#150052,#150053,#150054,#150055),(#150056,
#150057,#150058,#150059,#150060)),.UNSPECIFIED.,.F.,.F.,.F.)
B_SPLINE_SURFACE_WITH_KNOTS((2,2),(3,2,3),(0.709719018649857,1.),(0.607879027750091,
0.625170525609407,0.625770422814865),.UNSPECIFIED.)
GEOMETRIC_REPRESENTATION_ITEM()
RATIONAL_B_SPLINE_SURFACE(((0.987469282487682,0.987594391229382,0.990658108926708,
0.990658108926708,0.990658108926708),(0.987469282487682,0.987594391229382,
0.990658108926708,0.990658108926708,0.990658108926708)))
REPRESENTATION_ITEM('')
SURFACE()
);
#3275=(
BOUNDED_SURFACE()
B_SPLINE_SURFACE(1,2,((#150078,#150079,#150080),(#150081,#150082,#150083)),
 .UNSPECIFIED.,.F.,.F.,.F.)
B_SPLINE_SURFACE_WITH_KNOTS((2,2),(3,3),(0.710192959008336,1.),(0.107982157956012,
0.125273655815329),.UNSPECIFIED.)
GEOMETRIC_REPRESENTATION_ITEM()
RATIONAL_B_SPLINE_SURFACE(((0.987470879370256,0.987613514606721,0.990694758798813),
(0.987470879370256,0.987613514606721,0.990694758798813)))
REPRESENTATION_ITEM('')
SURFACE()
);
#3276=(
BOUNDED_SURFACE()
B_SPLINE_SURFACE(1,2,((#150090,#150091,#150092,#150093,#150094),(#150095,
#150096,#150097,#150098,#150099)),.UNSPECIFIED.,.F.,.F.,.F.)
B_SPLINE_SURFACE_WITH_KNOTS((2,2),(3,2,3),(0.709719018614768,1.),(0.607879027750091,
0.625170525609407,0.625770422849006),.UNSPECIFIED.)
GEOMETRIC_REPRESENTATION_ITEM()
RATIONAL_B_SPLINE_SURFACE(((0.987469282487682,0.987594391229382,0.990658108926709,
0.990658108926709,0.990658108926709),(0.987469282487682,0.987594391229382,
0.990658108926709,0.990658108926709,0.990658108926709)))
REPRESENTATION_ITEM('')
SURFACE()
);
#3277=(
BOUNDED_SURFACE()
B_SPLINE_SURFACE(1,2,((#150117,#150118,#150119),(#150120,#150121,#150122)),
 .UNSPECIFIED.,.F.,.F.,.F.)
B_SPLINE_SURFACE_WITH_KNOTS((2,2),(3,3),(0.710192959007384,1.),(0.107982157956012,
0.125273655815329),.UNSPECIFIED.)
GEOMETRIC_REPRESENTATION_ITEM()
RATIONAL_B_SPLINE_SURFACE(((0.987470879370256,0.987613514606721,0.990694758798813),
(0.987470879370256,0.987613514606721,0.990694758798813)))
REPRESENTATION_ITEM('')
SURFACE()
);
#3278=(
BOUNDED_SURFACE()
B_SPLINE_SURFACE(1,2,((#150129,#150130,#150131,#150132,#150133),(#150134,
#150135,#150136,#150137,#150138)),.UNSPECIFIED.,.F.,.F.,.F.)
B_SPLINE_SURFACE_WITH_KNOTS((2,2),(3,2,3),(0.709719018624158,1.),(0.607879027750091,
0.625170525609407,0.625770422839608),.UNSPECIFIED.)
GEOMETRIC_REPRESENTATION_ITEM()
RATIONAL_B_SPLINE_SURFACE(((0.987469282487682,0.987594391229382,0.990658108926709,
0.990658108926709,0.990658108926709),(0.987469282487682,0.987594391229382,
0.990658108926709,0.990658108926709,0.990658108926709)))
REPRESENTATION_ITEM('')
SURFACE()
);
#3279=(
BOUNDED_SURFACE()
B_SPLINE_SURFACE(1,2,((#150156,#150157,#150158),(#150159,#150160,#150161)),
 .UNSPECIFIED.,.F.,.F.,.F.)
B_SPLINE_SURFACE_WITH_KNOTS((2,2),(3,3),(0.710192959007374,1.),(0.107982157956012,
0.125273655815329),.UNSPECIFIED.)
GEOMETRIC_REPRESENTATION_ITEM()
RATIONAL_B_SPLINE_SURFACE(((0.987470879370255,0.987613514606721,0.990694758798813),
(0.987470879370256,0.987613514606721,0.990694758798813)))
REPRESENTATION_ITEM('')
SURFACE()
);
#3280=(
BOUNDED_SURFACE()
B_SPLINE_SURFACE(1,2,((#150168,#150169,#150170,#150171,#150172),(#150173,
#150174,#150175,#150176,#150177)),.UNSPECIFIED.,.F.,.F.,.F.)
B_SPLINE_SURFACE_WITH_KNOTS((2,2),(3,2,3),(0.709719018629564,1.),(0.607879027750091,
0.625170525609407,0.625770422834208),.UNSPECIFIED.)
GEOMETRIC_REPRESENTATION_ITEM()
RATIONAL_B_SPLINE_SURFACE(((0.987469282487682,0.987594391229382,0.990658108926708,
0.990658108926708,0.990658108926708),(0.987469282487682,0.987594391229382,
0.990658108926709,0.990658108926709,0.990658108926709)))
REPRESENTATION_ITEM('')
SURFACE()
);
#3281=(
BOUNDED_SURFACE()
B_SPLINE_SURFACE(1,2,((#150195,#150196,#150197),(#150198,#150199,#150200)),
 .UNSPECIFIED.,.F.,.F.,.F.)
B_SPLINE_SURFACE_WITH_KNOTS((2,2),(3,3),(0.710192959007377,1.),(0.107982157956012,
0.125273655815329),.UNSPECIFIED.)
GEOMETRIC_REPRESENTATION_ITEM()
RATIONAL_B_SPLINE_SURFACE(((0.987470879370256,0.987613514606721,0.990694758798813),
(0.987470879370256,0.987613514606721,0.990694758798813)))
REPRESENTATION_ITEM('')
SURFACE()
);
#3282=(
BOUNDED_SURFACE()
B_SPLINE_SURFACE(1,2,((#150207,#150208,#150209,#150210,#150211),(#150212,
#150213,#150214,#150215,#150216)),.UNSPECIFIED.,.F.,.F.,.F.)
B_SPLINE_SURFACE_WITH_KNOTS((2,2),(3,2,3),(0.709719018632745,1.),(0.607879027750091,
0.625170525609407,0.625770422830443),.UNSPECIFIED.)
GEOMETRIC_REPRESENTATION_ITEM()
RATIONAL_B_SPLINE_SURFACE(((0.987469282487682,0.987594391229382,0.990658108926709,
0.990658108926709,0.990658108926709),(0.987469282487682,0.987594391229382,
0.990658108926709,0.990658108926709,0.990658108926709)))
REPRESENTATION_ITEM('')
SURFACE()
);
#3283=(
BOUNDED_SURFACE()
B_SPLINE_SURFACE(1,2,((#150234,#150235,#150236),(#150237,#150238,#150239)),
 .UNSPECIFIED.,.F.,.F.,.F.)
B_SPLINE_SURFACE_WITH_KNOTS((2,2),(3,3),(0.710192959006796,1.),(0.107982157956012,
0.125273655815329),.UNSPECIFIED.)
GEOMETRIC_REPRESENTATION_ITEM()
RATIONAL_B_SPLINE_SURFACE(((0.987470879370256,0.987613514606721,0.990694758798813),
(0.987470879370256,0.987613514606721,0.990694758798813)))
REPRESENTATION_ITEM('')
SURFACE()
);
#3284=(
BOUNDED_SURFACE()
B_SPLINE_SURFACE(1,2,((#150246,#150247,#150248,#150249,#150250),(#150251,
#150252,#150253,#150254,#150255)),.UNSPECIFIED.,.F.,.F.,.F.)
B_SPLINE_SURFACE_WITH_KNOTS((2,2),(3,2,3),(0.70971901863244,1.),(0.607879027750091,
0.625170525609407,0.625770422831336),.UNSPECIFIED.)
GEOMETRIC_REPRESENTATION_ITEM()
RATIONAL_B_SPLINE_SURFACE(((0.987469282487682,0.987594391229382,0.990658108926708,
0.990658108926708,0.990658108926708),(0.987469282487682,0.987594391229382,
0.990658108926709,0.990658108926709,0.990658108926709)))
REPRESENTATION_ITEM('')
SURFACE()
);
#3285=(
BOUNDED_SURFACE()
B_SPLINE_SURFACE(1,2,((#150273,#150274,#150275),(#150276,#150277,#150278)),
 .UNSPECIFIED.,.F.,.F.,.F.)
B_SPLINE_SURFACE_WITH_KNOTS((2,2),(3,3),(0.710192959007382,1.),(0.107982157956012,
0.125273655815329),.UNSPECIFIED.)
GEOMETRIC_REPRESENTATION_ITEM()
RATIONAL_B_SPLINE_SURFACE(((0.987470879370256,0.987613514606721,0.990694758798813),
(0.987470879370256,0.987613514606721,0.990694758798813)))
REPRESENTATION_ITEM('')
SURFACE()
);
#3286=(
BOUNDED_SURFACE()
B_SPLINE_SURFACE(1,2,((#150285,#150286,#150287,#150288,#150289),(#150290,
#150291,#150292,#150293,#150294)),.UNSPECIFIED.,.F.,.F.,.F.)
B_SPLINE_SURFACE_WITH_KNOTS((2,2),(3,2,3),(0.709719018613158,1.),(0.607879027750091,
0.625170525609407,0.625770422850059),.UNSPECIFIED.)
GEOMETRIC_REPRESENTATION_ITEM()
RATIONAL_B_SPLINE_SURFACE(((0.987469282487682,0.987594391229382,0.990658108926708,
0.990658108926708,0.990658108926708),(0.987469282487682,0.987594391229382,
0.990658108926708,0.990658108926708,0.990658108926708)))
REPRESENTATION_ITEM('')
SURFACE()
);
#3287=(
BOUNDED_SURFACE()
B_SPLINE_SURFACE(1,2,((#150312,#150313,#150314),(#150315,#150316,#150317)),
 .UNSPECIFIED.,.F.,.F.,.F.)
B_SPLINE_SURFACE_WITH_KNOTS((2,2),(3,3),(0.710192959006824,1.),(0.107982157956012,
0.125273655815329),.UNSPECIFIED.)
GEOMETRIC_REPRESENTATION_ITEM()
RATIONAL_B_SPLINE_SURFACE(((0.987470879370256,0.987613514606721,0.990694758798813),
(0.987470879370256,0.987613514606721,0.990694758798813)))
REPRESENTATION_ITEM('')
SURFACE()
);
#3288=(
BOUNDED_SURFACE()
B_SPLINE_SURFACE(1,2,((#150324,#150325,#150326,#150327,#150328),(#150329,
#150330,#150331,#150332,#150333)),.UNSPECIFIED.,.F.,.F.,.F.)
B_SPLINE_SURFACE_WITH_KNOTS((2,2),(3,2,3),(0.70971901862884,1.),(0.607879027750092,
0.625170525609407,0.625770422834571),.UNSPECIFIED.)
GEOMETRIC_REPRESENTATION_ITEM()
RATIONAL_B_SPLINE_SURFACE(((0.987469282487682,0.987594391229382,0.990658108926708,
0.990658108926708,0.990658108926708),(0.987469282487682,0.987594391229382,
0.990658108926708,0.990658108926708,0.990658108926708)))
REPRESENTATION_ITEM('')
SURFACE()
);
#3289=(
BOUNDED_SURFACE()
B_SPLINE_SURFACE(1,2,((#150351,#150352,#150353),(#150354,#150355,#150356)),
 .UNSPECIFIED.,.F.,.F.,.F.)
B_SPLINE_SURFACE_WITH_KNOTS((2,2),(3,3),(0.710192959007015,1.),(0.107982157956011,
0.125273655815328),.UNSPECIFIED.)
GEOMETRIC_REPRESENTATION_ITEM()
RATIONAL_B_SPLINE_SURFACE(((0.987470879370255,0.98761351460672,0.990694758798812),
(0.987470879370255,0.98761351460672,0.990694758798812)))
REPRESENTATION_ITEM('')
SURFACE()
);
#3290=(
BOUNDED_SURFACE()
B_SPLINE_SURFACE(1,2,((#150363,#150364,#150365,#150366,#150367),(#150368,
#150369,#150370,#150371,#150372)),.UNSPECIFIED.,.F.,.F.,.F.)
B_SPLINE_SURFACE_WITH_KNOTS((2,2),(3,2,3),(0.709719018615787,1.),(0.607879027750092,
0.625170525609408,0.625770422847591),.UNSPECIFIED.)
GEOMETRIC_REPRESENTATION_ITEM()
RATIONAL_B_SPLINE_SURFACE(((0.987469282487682,0.987594391229382,0.990658108926709,
0.990658108926709,0.990658108926709),(0.987469282487682,0.987594391229382,
0.990658108926709,0.990658108926709,0.990658108926709)))
REPRESENTATION_ITEM('')
SURFACE()
);
#3291=(
BOUNDED_SURFACE()
B_SPLINE_SURFACE(1,2,((#150390,#150391,#150392),(#150393,#150394,#150395)),
 .UNSPECIFIED.,.F.,.F.,.F.)
B_SPLINE_SURFACE_WITH_KNOTS((2,2),(3,3),(0.710192959006983,1.),(0.107982157956011,
0.125273655815328),.UNSPECIFIED.)
GEOMETRIC_REPRESENTATION_ITEM()
RATIONAL_B_SPLINE_SURFACE(((0.987470879370255,0.98761351460672,0.990694758798812),
(0.987470879370255,0.98761351460672,0.990694758798812)))
REPRESENTATION_ITEM('')
SURFACE()
);
#3292=(
BOUNDED_SURFACE()
B_SPLINE_SURFACE(1,2,((#150402,#150403,#150404,#150405,#150406),(#150407,
#150408,#150409,#150410,#150411)),.UNSPECIFIED.,.F.,.F.,.F.)
B_SPLINE_SURFACE_WITH_KNOTS((2,2),(3,2,3),(0.70971901861887,1.),(0.607879027750092,
0.625170525609408,0.625770422844231),.UNSPECIFIED.)
GEOMETRIC_REPRESENTATION_ITEM()
RATIONAL_B_SPLINE_SURFACE(((0.987469282487682,0.987594391229382,0.990658108926709,
0.990658108926709,0.990658108926709),(0.987469282487682,0.987594391229382,
0.990658108926709,0.990658108926709,0.990658108926709)))
REPRESENTATION_ITEM('')
SURFACE()
);
#3293=(
BOUNDED_SURFACE()
B_SPLINE_SURFACE(1,2,((#150429,#150430,#150431),(#150432,#150433,#150434)),
 .UNSPECIFIED.,.F.,.F.,.F.)
B_SPLINE_SURFACE_WITH_KNOTS((2,2),(3,3),(0.710192959006704,1.),(0.107982157956011,
0.125273655815328),.UNSPECIFIED.)
GEOMETRIC_REPRESENTATION_ITEM()
RATIONAL_B_SPLINE_SURFACE(((0.987470879370255,0.98761351460672,0.990694758798812),
(0.987470879370255,0.98761351460672,0.990694758798812)))
REPRESENTATION_ITEM('')
SURFACE()
);
#3294=(
BOUNDED_SURFACE()
B_SPLINE_SURFACE(1,2,((#150441,#150442,#150443,#150444,#150445),(#150446,
#150447,#150448,#150449,#150450)),.UNSPECIFIED.,.F.,.F.,.F.)
B_SPLINE_SURFACE_WITH_KNOTS((2,2),(3,2,3),(0.709719018626216,1.),(0.607879027750092,
0.625170525609408,0.625770422837466),.UNSPECIFIED.)
GEOMETRIC_REPRESENTATION_ITEM()
RATIONAL_B_SPLINE_SURFACE(((0.987469282487682,0.987594391229382,0.990658108926709,
0.990658108926709,0.990658108926709),(0.987469282487682,0.987594391229382,
0.990658108926709,0.990658108926709,0.990658108926709)))
REPRESENTATION_ITEM('')
SURFACE()
);
#3295=(
BOUNDED_SURFACE()
B_SPLINE_SURFACE(1,2,((#150468,#150469,#150470),(#150471,#150472,#150473)),
 .UNSPECIFIED.,.F.,.F.,.F.)
B_SPLINE_SURFACE_WITH_KNOTS((2,2),(3,3),(0.710192959007287,1.),(0.107982157956011,
0.125273655815328),.UNSPECIFIED.)
GEOMETRIC_REPRESENTATION_ITEM()
RATIONAL_B_SPLINE_SURFACE(((0.987470879370255,0.98761351460672,0.990694758798812),
(0.987470879370255,0.98761351460672,0.990694758798812)))
REPRESENTATION_ITEM('')
SURFACE()
);
#3296=(
BOUNDED_SURFACE()
B_SPLINE_SURFACE(1,2,((#150480,#150481,#150482,#150483,#150484),(#150485,
#150486,#150487,#150488,#150489)),.UNSPECIFIED.,.F.,.F.,.F.)
B_SPLINE_SURFACE_WITH_KNOTS((2,2),(3,2,3),(0.709719018626252,1.),(0.607879027750092,
0.625170525609409,0.625770422836598),.UNSPECIFIED.)
GEOMETRIC_REPRESENTATION_ITEM()
RATIONAL_B_SPLINE_SURFACE(((0.987469282487682,0.987594391229382,0.990658108926709,
0.990658108926709,0.990658108926709),(0.987469282487682,0.987594391229382,
0.990658108926709,0.990658108926709,0.990658108926709)))
REPRESENTATION_ITEM('')
SURFACE()
);
#3297=(
BOUNDED_SURFACE()
B_SPLINE_SURFACE(1,2,((#150507,#150508,#150509),(#150510,#150511,#150512)),
 .UNSPECIFIED.,.F.,.F.,.F.)
B_SPLINE_SURFACE_WITH_KNOTS((2,2),(3,3),(0.710192959006458,1.),(0.107982157956011,
0.125273655815328),.UNSPECIFIED.)
GEOMETRIC_REPRESENTATION_ITEM()
RATIONAL_B_SPLINE_SURFACE(((0.987470879370255,0.98761351460672,0.990694758798812),
(0.987470879370255,0.98761351460672,0.990694758798812)))
REPRESENTATION_ITEM('')
SURFACE()
);
#3298=(
BOUNDED_SURFACE()
B_SPLINE_SURFACE(1,2,((#150519,#150520,#150521,#150522,#150523),(#150524,
#150525,#150526,#150527,#150528)),.UNSPECIFIED.,.F.,.F.,.F.)
B_SPLINE_SURFACE_WITH_KNOTS((2,2),(3,2,3),(0.709719018614626,1.),(0.607879027750092,
0.625170525609408,0.625770422848724),.UNSPECIFIED.)
GEOMETRIC_REPRESENTATION_ITEM()
RATIONAL_B_SPLINE_SURFACE(((0.987469282487682,0.987594391229382,0.990658108926709,
0.990658108926709,0.990658108926709),(0.987469282487682,0.987594391229382,
0.990658108926709,0.990658108926709,0.990658108926709)))
REPRESENTATION_ITEM('')
SURFACE()
);
#3299=(
BOUNDED_SURFACE()
B_SPLINE_SURFACE(1,2,((#150546,#150547,#150548),(#150549,#150550,#150551)),
 .UNSPECIFIED.,.F.,.F.,.F.)
B_SPLINE_SURFACE_WITH_KNOTS((2,2),(3,3),(0.710192959006957,1.),(0.107982157956011,
0.125273655815328),.UNSPECIFIED.)
GEOMETRIC_REPRESENTATION_ITEM()
RATIONAL_B_SPLINE_SURFACE(((0.987470879370255,0.98761351460672,0.990694758798812),
(0.987470879370255,0.98761351460672,0.990694758798812)))
REPRESENTATION_ITEM('')
SURFACE()
);
#3300=(
BOUNDED_SURFACE()
B_SPLINE_SURFACE(1,2,((#150558,#150559,#150560,#150561,#150562),(#150563,
#150564,#150565,#150566,#150567)),.UNSPECIFIED.,.F.,.F.,.F.)
B_SPLINE_SURFACE_WITH_KNOTS((2,2),(3,2,3),(0.709719018620996,1.),(0.607879027750092,
0.625170525609408,0.625770422841884),.UNSPECIFIED.)
GEOMETRIC_REPRESENTATION_ITEM()
RATIONAL_B_SPLINE_SURFACE(((0.987469282487682,0.987594391229382,0.990658108926709,
0.990658108926709,0.990658108926709),(0.987469282487682,0.987594391229382,
0.990658108926709,0.990658108926709,0.990658108926709)))
REPRESENTATION_ITEM('')
SURFACE()
);
#3301=(
BOUNDED_SURFACE()
B_SPLINE_SURFACE(1,2,((#150585,#150586,#150587),(#150588,#150589,#150590)),
 .UNSPECIFIED.,.F.,.F.,.F.)
B_SPLINE_SURFACE_WITH_KNOTS((2,2),(3,3),(0.710192959006483,1.),(0.107982157956011,
0.125273655815328),.UNSPECIFIED.)
GEOMETRIC_REPRESENTATION_ITEM()
RATIONAL_B_SPLINE_SURFACE(((0.987470879370255,0.98761351460672,0.990694758798812),
(0.987470879370255,0.98761351460672,0.990694758798812)))
REPRESENTATION_ITEM('')
SURFACE()
);
#3302=(
BOUNDED_SURFACE()
B_SPLINE_SURFACE(1,2,((#150597,#150598,#150599,#150600,#150601),(#150602,
#150603,#150604,#150605,#150606)),.UNSPECIFIED.,.F.,.F.,.F.)
B_SPLINE_SURFACE_WITH_KNOTS((2,2),(3,2,3),(0.709719018617797,1.),(0.607879027750092,
0.625170525609408,0.625770422845335),.UNSPECIFIED.)
GEOMETRIC_REPRESENTATION_ITEM()
RATIONAL_B_SPLINE_SURFACE(((0.987469282487682,0.987594391229382,0.990658108926709,
0.990658108926709,0.990658108926709),(0.987469282487682,0.987594391229382,
0.990658108926709,0.990658108926709,0.990658108926709)))
REPRESENTATION_ITEM('')
SURFACE()
);
#3303=(
BOUNDED_SURFACE()
B_SPLINE_SURFACE(1,2,((#150624,#150625,#150626),(#150627,#150628,#150629)),
 .UNSPECIFIED.,.F.,.F.,.F.)
B_SPLINE_SURFACE_WITH_KNOTS((2,2),(3,3),(0.710192959006736,1.),(0.107982157956011,
0.125273655815328),.UNSPECIFIED.)
GEOMETRIC_REPRESENTATION_ITEM()
RATIONAL_B_SPLINE_SURFACE(((0.987470879370255,0.98761351460672,0.990694758798812),
(0.987470879370255,0.98761351460672,0.990694758798812)))
REPRESENTATION_ITEM('')
SURFACE()
);
#3304=(
BOUNDED_SURFACE()
B_SPLINE_SURFACE(1,2,((#150636,#150637,#150638,#150639,#150640),(#150641,
#150642,#150643,#150644,#150645)),.UNSPECIFIED.,.F.,.F.,.F.)
B_SPLINE_SURFACE_WITH_KNOTS((2,2),(3,2,3),(0.70971901862028,1.),(0.607879027750092,
0.625170525609408,0.625770422841692),.UNSPECIFIED.)
GEOMETRIC_REPRESENTATION_ITEM()
RATIONAL_B_SPLINE_SURFACE(((0.987469282487682,0.987594391229382,0.990658108926709,
0.990658108926709,0.990658108926709),(0.987469282487682,0.987594391229382,
0.990658108926709,0.990658108926709,0.990658108926709)))
REPRESENTATION_ITEM('')
SURFACE()
);
#3305=(
BOUNDED_SURFACE()
B_SPLINE_SURFACE(1,2,((#150663,#150664,#150665),(#150666,#150667,#150668)),
 .UNSPECIFIED.,.F.,.F.,.F.)
B_SPLINE_SURFACE_WITH_KNOTS((2,2),(3,3),(0.710192959005573,1.),(0.107982157956011,
0.125273655815328),.UNSPECIFIED.)
GEOMETRIC_REPRESENTATION_ITEM()
RATIONAL_B_SPLINE_SURFACE(((0.987470879370255,0.98761351460672,0.990694758798812),
(0.987470879370255,0.98761351460672,0.990694758798812)))
REPRESENTATION_ITEM('')
SURFACE()
);
#3306=(
BOUNDED_SURFACE()
B_SPLINE_SURFACE(1,2,((#150675,#150676,#150677,#150678,#150679),(#150680,
#150681,#150682,#150683,#150684)),.UNSPECIFIED.,.F.,.F.,.F.)
B_SPLINE_SURFACE_WITH_KNOTS((2,2),(3,2,3),(0.709719018631225,1.),(0.607879027750092,
0.625170525609408,0.625770422832408),.UNSPECIFIED.)
GEOMETRIC_REPRESENTATION_ITEM()
RATIONAL_B_SPLINE_SURFACE(((0.987469282487682,0.987594391229382,0.990658108926709,
0.990658108926709,0.990658108926709),(0.987469282487682,0.987594391229382,
0.990658108926709,0.990658108926709,0.990658108926709)))
REPRESENTATION_ITEM('')
SURFACE()
);
#3307=(
BOUNDED_SURFACE()
B_SPLINE_SURFACE(1,2,((#150702,#150703,#150704),(#150705,#150706,#150707)),
 .UNSPECIFIED.,.F.,.F.,.F.)
B_SPLINE_SURFACE_WITH_KNOTS((2,2),(3,3),(0.710192959007235,1.),(0.107982157956011,
0.125273655815328),.UNSPECIFIED.)
GEOMETRIC_REPRESENTATION_ITEM()
RATIONAL_B_SPLINE_SURFACE(((0.987470879370255,0.98761351460672,0.990694758798812),
(0.987470879370255,0.98761351460672,0.990694758798812)))
REPRESENTATION_ITEM('')
SURFACE()
);
#3308=(
BOUNDED_SURFACE()
B_SPLINE_SURFACE(1,2,((#150714,#150715,#150716,#150717,#150718),(#150719,
#150720,#150721,#150722,#150723)),.UNSPECIFIED.,.F.,.F.,.F.)
B_SPLINE_SURFACE_WITH_KNOTS((2,2),(3,2,3),(0.709719018614688,1.),(0.607879027750092,
0.625170525609408,0.625770422849057),.UNSPECIFIED.)
GEOMETRIC_REPRESENTATION_ITEM()
RATIONAL_B_SPLINE_SURFACE(((0.987469282487682,0.987594391229382,0.990658108926709,
0.990658108926709,0.990658108926709),(0.987469282487682,0.987594391229382,
0.990658108926709,0.990658108926709,0.990658108926709)))
REPRESENTATION_ITEM('')
SURFACE()
);
#3309=(
BOUNDED_SURFACE()
B_SPLINE_SURFACE(1,2,((#150741,#150742,#150743),(#150744,#150745,#150746)),
 .UNSPECIFIED.,.F.,.F.,.F.)
B_SPLINE_SURFACE_WITH_KNOTS((2,2),(3,3),(0.710192959007356,1.),(0.107982157956011,
0.125273655815328),.UNSPECIFIED.)
GEOMETRIC_REPRESENTATION_ITEM()
RATIONAL_B_SPLINE_SURFACE(((0.987470879370255,0.98761351460672,0.990694758798812),
(0.987470879370255,0.98761351460672,0.990694758798812)))
REPRESENTATION_ITEM('')
SURFACE()
);
#3310=(
BOUNDED_SURFACE()
B_SPLINE_SURFACE(1,2,((#150753,#150754,#150755,#150756,#150757),(#150758,
#150759,#150760,#150761,#150762)),.UNSPECIFIED.,.F.,.F.,.F.)
B_SPLINE_SURFACE_WITH_KNOTS((2,2),(3,2,3),(0.710057850970234,1.),(0.607879027750092,
0.625170525609408,0.625431590492668),.UNSPECIFIED.)
GEOMETRIC_REPRESENTATION_ITEM()
RATIONAL_B_SPLINE_SURFACE(((0.987469282487682,0.987594391229382,0.990658108926709,
0.990658108926709,0.990658108926709),(0.987469282487682,0.987594391229382,
0.990658108926709,0.990658108926709,0.990658108926709)))
REPRESENTATION_ITEM('')
SURFACE()
);
#3311=(
BOUNDED_SURFACE()
B_SPLINE_SURFACE(1,2,((#150770,#150771,#150772),(#150773,#150774,#150775)),
 .UNSPECIFIED.,.F.,.F.,.F.)
B_SPLINE_SURFACE_WITH_KNOTS((2,2),(3,3),(0.710192959006505,1.),(0.107982157956011,
0.125273655815328),.UNSPECIFIED.)
GEOMETRIC_REPRESENTATION_ITEM()
RATIONAL_B_SPLINE_SURFACE(((0.987470879370255,0.987613514606721,0.990694758798812),
(0.987470879370255,0.98761351460672,0.990694758798812)))
REPRESENTATION_ITEM('')
SURFACE()
);
#3312=(
BOUNDED_SURFACE()
B_SPLINE_SURFACE(1,2,((#150777,#150778,#150779,#150780,#150781),(#150782,
#150783,#150784,#150785,#150786)),.UNSPECIFIED.,.F.,.F.,.F.)
B_SPLINE_SURFACE_WITH_KNOTS((2,2),(3,2,3),(0.709719018638398,1.),(0.607879027750092,
0.62517052560941,0.625770422825979),.UNSPECIFIED.)
GEOMETRIC_REPRESENTATION_ITEM()
RATIONAL_B_SPLINE_SURFACE(((0.987469282487682,0.987594391229382,0.990658108926709,
0.990658108926709,0.990658108926709),(0.987469282487682,0.987594391229382,
0.990658108926709,0.990658108926709,0.990658108926709)))
REPRESENTATION_ITEM('')
SURFACE()
);
#3313=(
BOUNDED_SURFACE()
B_SPLINE_SURFACE(1,2,((#150804,#150805,#150806),(#150807,#150808,#150809)),
 .UNSPECIFIED.,.F.,.F.,.F.)
B_SPLINE_SURFACE_WITH_KNOTS((2,2),(3,3),(0.710192959007984,1.),(0.107982157956011,
0.125273655815332),.UNSPECIFIED.)
GEOMETRIC_REPRESENTATION_ITEM()
RATIONAL_B_SPLINE_SURFACE(((0.987470879370255,0.987613514606721,0.990694758798814),
(0.987470879370255,0.987613514606721,0.990694758798814)))
REPRESENTATION_ITEM('')
SURFACE()
);
#3314=(
BOUNDED_SURFACE()
B_SPLINE_SURFACE(1,2,((#150816,#150817,#150818,#150819,#150820),(#150821,
#150822,#150823,#150824,#150825)),.UNSPECIFIED.,.F.,.F.,.F.)
B_SPLINE_SURFACE_WITH_KNOTS((2,2),(3,2,3),(0.709719018635918,1.),(0.607879027750092,
0.625170525609409,0.625770422827588),.UNSPECIFIED.)
GEOMETRIC_REPRESENTATION_ITEM()
RATIONAL_B_SPLINE_SURFACE(((0.987469282487682,0.987594391229382,0.990658108926709,
0.990658108926709,0.990658108926709),(0.987469282487682,0.987594391229382,
0.990658108926709,0.990658108926709,0.990658108926709)))
REPRESENTATION_ITEM('')
SURFACE()
);
#3315=(
BOUNDED_SURFACE()
B_SPLINE_SURFACE(1,2,((#150843,#150844,#150845),(#150846,#150847,#150848)),
 .UNSPECIFIED.,.F.,.F.,.F.)
B_SPLINE_SURFACE_WITH_KNOTS((2,2),(3,3),(0.710192959007116,1.),(0.107982157956011,
0.125273655815328),.UNSPECIFIED.)
GEOMETRIC_REPRESENTATION_ITEM()
RATIONAL_B_SPLINE_SURFACE(((0.987470879370255,0.98761351460672,0.990694758798812),
(0.987470879370255,0.98761351460672,0.990694758798812)))
REPRESENTATION_ITEM('')
SURFACE()
);
#3316=(
BOUNDED_SURFACE()
B_SPLINE_SURFACE(1,2,((#150855,#150856,#150857,#150858,#150859),(#150860,
#150861,#150862,#150863,#150864)),.UNSPECIFIED.,.F.,.F.,.F.)
B_SPLINE_SURFACE_WITH_KNOTS((2,2),(3,2,3),(0.709719018610881,1.),(0.607879027750092,
0.625170525609408,0.625770422852824),.UNSPECIFIED.)
GEOMETRIC_REPRESENTATION_ITEM()
RATIONAL_B_SPLINE_SURFACE(((0.987469282487682,0.987594391229382,0.990658108926709,
0.990658108926709,0.990658108926709),(0.987469282487682,0.987594391229382,
0.990658108926709,0.990658108926709,0.990658108926709)))
REPRESENTATION_ITEM('')
SURFACE()
);
#3317=(
BOUNDED_SURFACE()
B_SPLINE_SURFACE(1,2,((#150882,#150883,#150884),(#150885,#150886,#150887)),
 .UNSPECIFIED.,.F.,.F.,.F.)
B_SPLINE_SURFACE_WITH_KNOTS((2,2),(3,3),(0.71019295900731,1.),(0.107982157956012,
0.125273655815328),.UNSPECIFIED.)
GEOMETRIC_REPRESENTATION_ITEM()
RATIONAL_B_SPLINE_SURFACE(((0.987470879370256,0.987613514606721,0.990694758798813),
(0.987470879370256,0.987613514606721,0.990694758798813)))
REPRESENTATION_ITEM('')
SURFACE()
);
#3318=(
BOUNDED_SURFACE()
B_SPLINE_SURFACE(1,2,((#150894,#150895,#150896,#150897,#150898),(#150899,
#150900,#150901,#150902,#150903)),.UNSPECIFIED.,.F.,.F.,.F.)
B_SPLINE_SURFACE_WITH_KNOTS((2,2),(3,2,3),(0.709719018631712,1.),(0.607879027750091,
0.625170525609408,0.625770422833119),.UNSPECIFIED.)
GEOMETRIC_REPRESENTATION_ITEM()
RATIONAL_B_SPLINE_SURFACE(((0.987469282487682,0.987594391229382,0.990658108926708,
0.990658108926708,0.990658108926708),(0.987469282487682,0.987594391229382,
0.990658108926708,0.990658108926708,0.990658108926708)))
REPRESENTATION_ITEM('')
SURFACE()
);
#3319=(
BOUNDED_SURFACE()
B_SPLINE_SURFACE(1,2,((#150921,#150922,#150923),(#150924,#150925,#150926)),
 .UNSPECIFIED.,.F.,.F.,.F.)
B_SPLINE_SURFACE_WITH_KNOTS((2,2),(3,3),(0.710192959008443,1.),(0.107982157956012,
0.125273655815329),.UNSPECIFIED.)
GEOMETRIC_REPRESENTATION_ITEM()
RATIONAL_B_SPLINE_SURFACE(((0.987470879370256,0.987613514606721,0.990694758798813),
(0.987470879370256,0.987613514606721,0.990694758798813)))
REPRESENTATION_ITEM('')
SURFACE()
);
#3320=(
BOUNDED_SURFACE()
B_SPLINE_SURFACE(1,2,((#150933,#150934,#150935,#150936,#150937),(#150938,
#150939,#150940,#150941,#150942)),.UNSPECIFIED.,.F.,.F.,.F.)
B_SPLINE_SURFACE_WITH_KNOTS((2,2),(3,2,3),(0.709719018622383,1.),(0.607879027750091,
0.625170525609407,0.625770422842453),.UNSPECIFIED.)
GEOMETRIC_REPRESENTATION_ITEM()
RATIONAL_B_SPLINE_SURFACE(((0.987469282487682,0.987594391229382,0.990658108926708,
0.990658108926708,0.990658108926708),(0.987469282487682,0.987594391229382,
0.990658108926709,0.990658108926709,0.990658108926709)))
REPRESENTATION_ITEM('')
SURFACE()
);
#3321=(
BOUNDED_SURFACE()
B_SPLINE_SURFACE(1,2,((#150960,#150961,#150962),(#150963,#150964,#150965)),
 .UNSPECIFIED.,.F.,.F.,.F.)
B_SPLINE_SURFACE_WITH_KNOTS((2,2),(3,3),(0.710192959008445,1.),(0.107982157956012,
0.125273655815329),.UNSPECIFIED.)
GEOMETRIC_REPRESENTATION_ITEM()
RATIONAL_B_SPLINE_SURFACE(((0.987470879370256,0.987613514606721,0.990694758798813),
(0.987470879370256,0.987613514606721,0.990694758798813)))
REPRESENTATION_ITEM('')
SURFACE()
);
#3322=(
BOUNDED_SURFACE()
B_SPLINE_SURFACE(1,2,((#150972,#150973,#150974,#150975,#150976),(#150977,
#150978,#150979,#150980,#150981)),.UNSPECIFIED.,.F.,.F.,.F.)
B_SPLINE_SURFACE_WITH_KNOTS((2,2),(3,2,3),(0.70971901863218,1.),(0.607879027750091,
0.625170525609407,0.62577042283265),.UNSPECIFIED.)
GEOMETRIC_REPRESENTATION_ITEM()
RATIONAL_B_SPLINE_SURFACE(((0.987469282487682,0.987594391229382,0.990658108926708,
0.990658108926708,0.990658108926708),(0.987469282487682,0.987594391229382,
0.990658108926709,0.990658108926709,0.990658108926709)))
REPRESENTATION_ITEM('')
SURFACE()
);
#3323=(
BOUNDED_SURFACE()
B_SPLINE_SURFACE(1,2,((#150999,#151000,#151001),(#151002,#151003,#151004)),
 .UNSPECIFIED.,.F.,.F.,.F.)
B_SPLINE_SURFACE_WITH_KNOTS((2,2),(3,3),(0.710192959008444,1.),(0.107982157956012,
0.125273655815329),.UNSPECIFIED.)
GEOMETRIC_REPRESENTATION_ITEM()
RATIONAL_B_SPLINE_SURFACE(((0.987470879370256,0.987613514606721,0.990694758798813),
(0.987470879370256,0.987613514606721,0.990694758798813)))
REPRESENTATION_ITEM('')
SURFACE()
);
#3324=(
BOUNDED_SURFACE()
B_SPLINE_SURFACE(1,2,((#151011,#151012,#151013,#151014,#151015),(#151016,
#151017,#151018,#151019,#151020)),.UNSPECIFIED.,.F.,.F.,.F.)
B_SPLINE_SURFACE_WITH_KNOTS((2,2),(3,2,3),(0.70971901862027,1.),(0.607879027750091,
0.625170525609407,0.625770422844233),.UNSPECIFIED.)
GEOMETRIC_REPRESENTATION_ITEM()
RATIONAL_B_SPLINE_SURFACE(((0.987469282487682,0.987594391229382,0.990658108926708,
0.990658108926708,0.990658108926708),(0.987469282487682,0.987594391229382,
0.990658108926709,0.990658108926709,0.990658108926709)))
REPRESENTATION_ITEM('')
SURFACE()
);
#3325=(
BOUNDED_SURFACE()
B_SPLINE_SURFACE(1,2,((#151038,#151039,#151040),(#151041,#151042,#151043)),
 .UNSPECIFIED.,.F.,.F.,.F.)
B_SPLINE_SURFACE_WITH_KNOTS((2,2),(3,3),(0.710192959008112,1.),(0.107982157956012,
0.125273655815329),.UNSPECIFIED.)
GEOMETRIC_REPRESENTATION_ITEM()
RATIONAL_B_SPLINE_SURFACE(((0.987470879370256,0.987613514606721,0.990694758798813),
(0.987470879370256,0.987613514606721,0.990694758798813)))
REPRESENTATION_ITEM('')
SURFACE()
);
#3326=(
BOUNDED_SURFACE()
B_SPLINE_SURFACE(1,2,((#151050,#151051,#151052,#151053,#151054),(#151055,
#151056,#151057,#151058,#151059)),.UNSPECIFIED.,.F.,.F.,.F.)
B_SPLINE_SURFACE_WITH_KNOTS((2,2),(3,2,3),(0.709590617367083,1.),(0.573052008420699,
0.573654350219791,0.591014490232052),.UNSPECIFIED.)
GEOMETRIC_REPRESENTATION_ITEM()
RATIONAL_B_SPLINE_SURFACE(((0.998486152291959,0.998486152291959,0.998486152291959,
0.99277234517203,0.990020524139833),(0.998486152291959,0.998486152291959,
0.998486152291959,0.99277234517203,0.990020524139833)))
REPRESENTATION_ITEM('')
SURFACE()
);
#3327=(
BOUNDED_SURFACE()
B_SPLINE_SURFACE(1,2,((#151068,#151069,#151070,#151071,#151072),(#151073,
#151074,#151075,#151076,#151077)),.UNSPECIFIED.,.F.,.F.,.F.)
B_SPLINE_SURFACE_WITH_KNOTS((2,2),(3,2,3),(0.710318915640075,1.),(0.142474614281353,
0.142857142857143,0.159901408087482),.UNSPECIFIED.)
GEOMETRIC_REPRESENTATION_ITEM()
RATIONAL_B_SPLINE_SURFACE(((0.999732896029228,0.999865728939368,1.,0.994017305594881,
0.990889788836284),(0.999732896029228,0.999865728939368,1.,0.994017305594881,
0.990889788836284)))
REPRESENTATION_ITEM('')
SURFACE()
);
#3328=(
BOUNDED_SURFACE()
B_SPLINE_SURFACE(1,2,((#151079,#151080,#151081,#151082,#151083),(#151084,
#151085,#151086,#151087,#151088)),.UNSPECIFIED.,.F.,.F.,.F.)
B_SPLINE_SURFACE_WITH_KNOTS((2,2),(3,2,3),(0.709590617386171,1.),(0.573052008439665,
0.573654350219722,0.591014490232053),.UNSPECIFIED.)
GEOMETRIC_REPRESENTATION_ITEM()
RATIONAL_B_SPLINE_SURFACE(((0.998486152292004,0.998486152292004,0.998486152292004,
0.992772345172041,0.990020524139833),(0.998486152292004,0.998486152292004,
0.998486152292004,0.992772345172041,0.990020524139833)))
REPRESENTATION_ITEM('')
SURFACE()
);
#3329=(
BOUNDED_SURFACE()
B_SPLINE_SURFACE(1,2,((#151097,#151098,#151099,#151100,#151101),(#151102,
#151103,#151104,#151105,#151106)),.UNSPECIFIED.,.F.,.F.,.F.)
B_SPLINE_SURFACE_WITH_KNOTS((2,2),(3,2,3),(0.710318915640081,1.),(0.142474614281357,
0.142857142857143,0.159901408087483),.UNSPECIFIED.)
GEOMETRIC_REPRESENTATION_ITEM()
RATIONAL_B_SPLINE_SURFACE(((0.999732896029231,0.999865728939369,1.,0.994017305594881,
0.990889788836284),(0.999732896029231,0.999865728939369,1.,0.994017305594881,
0.990889788836284)))
REPRESENTATION_ITEM('')
SURFACE()
);
#3330=(
BOUNDED_SURFACE()
B_SPLINE_SURFACE(1,2,((#151108,#151109,#151110,#151111,#151112),(#151113,
#151114,#151115,#151116,#151117)),.UNSPECIFIED.,.F.,.F.,.F.)
B_SPLINE_SURFACE_WITH_KNOTS((2,2),(3,2,3),(0.709590617383039,1.),(0.573052008436687,
0.57365435021991,0.591014490232044),.UNSPECIFIED.)
GEOMETRIC_REPRESENTATION_ITEM()
RATIONAL_B_SPLINE_SURFACE(((0.99848615229188,0.99848615229188,0.99848615229188,
0.992772345172014,0.990020524139836),(0.99848615229188,0.99848615229188,
0.99848615229188,0.992772345172014,0.990020524139836)))
REPRESENTATION_ITEM('')
SURFACE()
);
#3331=(
BOUNDED_SURFACE()
B_SPLINE_SURFACE(1,2,((#151126,#151127,#151128,#151129,#151130),(#151131,
#151132,#151133,#151134,#151135)),.UNSPECIFIED.,.F.,.F.,.F.)
B_SPLINE_SURFACE_WITH_KNOTS((2,2),(3,2,3),(0.710318915640083,1.),(0.142474614281355,
0.142857142857143,0.159901408087481),.UNSPECIFIED.)
GEOMETRIC_REPRESENTATION_ITEM()
RATIONAL_B_SPLINE_SURFACE(((0.999732896029229,0.999865728939368,1.,0.994017305594881,
0.990889788836284),(0.999732896029229,0.999865728939368,1.,0.994017305594881,
0.990889788836284)))
REPRESENTATION_ITEM('')
SURFACE()
);
#3332=(
BOUNDED_SURFACE()
B_SPLINE_SURFACE(1,2,((#151137,#151138,#151139,#151140,#151141),(#151142,
#151143,#151144,#151145,#151146)),.UNSPECIFIED.,.F.,.F.,.F.)
B_SPLINE_SURFACE_WITH_KNOTS((2,2),(3,2,3),(0.709590617387445,1.),(0.573052008441487,
0.573654350219663,0.591014490232054),.UNSPECIFIED.)
GEOMETRIC_REPRESENTATION_ITEM()
RATIONAL_B_SPLINE_SURFACE(((0.998486152292043,0.998486152292043,0.998486152292043,
0.99277234517205,0.990020524139832),(0.998486152292043,0.998486152292043,
0.998486152292043,0.99277234517205,0.990020524139832)))
REPRESENTATION_ITEM('')
SURFACE()
);
#3333=(
BOUNDED_SURFACE()
B_SPLINE_SURFACE(1,2,((#151155,#151156,#151157,#151158,#151159),(#151160,
#151161,#151162,#151163,#151164),(#151165,#151166,#151167,#151168,#151169)),
 .UNSPECIFIED.,.F.,.F.,.F.)
B_SPLINE_SURFACE_WITH_KNOTS((2,1,2),(3,2,3),(0.710318915640077,1.,1.0028968108436),
(0.14247461428136,0.142857142857143,0.159901408087481),.UNSPECIFIED.)
GEOMETRIC_REPRESENTATION_ITEM()
RATIONAL_B_SPLINE_SURFACE(((0.999732896029233,0.99986572893937,1.,0.994017305594881,
0.990889788836284),(0.999732896029233,0.99986572893937,1.,0.994017305594881,
0.990889788836284),(0.999732896029233,0.99986572893937,1.,0.994017305594881,
0.990889788836284)))
REPRESENTATION_ITEM('')
SURFACE()
);
#3334=(
BOUNDED_SURFACE()
B_SPLINE_SURFACE(1,2,((#151171,#151172,#151173,#151174,#151175),(#151176,
#151177,#151178,#151179,#151180)),.UNSPECIFIED.,.F.,.F.,.F.)
B_SPLINE_SURFACE_WITH_KNOTS((2,2),(3,2,3),(0.710192959008438,1.),(0.573480748819672,
0.573654350219794,0.59101449023205),.UNSPECIFIED.)
GEOMETRIC_REPRESENTATION_ITEM()
RATIONAL_B_SPLINE_SURFACE(((0.998486152291957,0.998486152291957,0.998486152291957,
0.992772345172031,0.990020524139834),(0.998486152291957,0.998486152291957,
0.998486152291957,0.992772345172031,0.990020524139834)))
REPRESENTATION_ITEM('')
SURFACE()
);
#3335=(
BOUNDED_SURFACE()
B_SPLINE_SURFACE(1,2,((#151189,#151190,#151191,#151192,#151193),(#151194,
#151195,#151196,#151197,#151198),(#151199,#151200,#151201,#151202,#151203)),
 .UNSPECIFIED.,.F.,.F.,.F.)
B_SPLINE_SURFACE_WITH_KNOTS((2,1,2),(3,2,3),(0.710318915640083,1.,1.0028968108436),
(0.142474614281359,0.142857142857143,0.159901408087481),.UNSPECIFIED.)
GEOMETRIC_REPRESENTATION_ITEM()
RATIONAL_B_SPLINE_SURFACE(((0.999732896029232,0.99986572893937,1.,0.994017305594881,
0.990889788836284),(0.999732896029232,0.99986572893937,1.,0.994017305594881,
0.990889788836284),(0.999732896029232,0.99986572893937,1.,0.994017305594881,
0.990889788836284)))
REPRESENTATION_ITEM('')
SURFACE()
);
#3336=(
BOUNDED_SURFACE()
B_SPLINE_SURFACE(1,2,((#151205,#151206,#151207,#151208,#151209),(#151210,
#151211,#151212,#151213,#151214)),.UNSPECIFIED.,.F.,.F.,.F.)
B_SPLINE_SURFACE_WITH_KNOTS((2,2),(3,2,3),(0.71019295900844,1.),(0.57348074881979,
0.573654350219911,0.591014490232053),.UNSPECIFIED.)
GEOMETRIC_REPRESENTATION_ITEM()
RATIONAL_B_SPLINE_SURFACE(((0.99848615229188,0.99848615229188,0.99848615229188,
0.992772345172011,0.990020524139833),(0.99848615229188,0.99848615229188,
0.99848615229188,0.992772345172011,0.990020524139833)))
REPRESENTATION_ITEM('')
SURFACE()
);
#3337=(
BOUNDED_SURFACE()
B_SPLINE_SURFACE(1,2,((#151223,#151224,#151225,#151226,#151227),(#151228,
#151229,#151230,#151231,#151232)),.UNSPECIFIED.,.F.,.F.,.F.)
B_SPLINE_SURFACE_WITH_KNOTS((2,2),(3,2,3),(0.710318915640079,1.),(0.142474614281366,
0.142857142857143,0.159901408087481),.UNSPECIFIED.)
GEOMETRIC_REPRESENTATION_ITEM()
RATIONAL_B_SPLINE_SURFACE(((0.999732896029237,0.999865728939372,1.,0.994017305594881,
0.990889788836284),(0.999732896029237,0.999865728939372,1.,0.994017305594881,
0.990889788836284)))
REPRESENTATION_ITEM('')
SURFACE()
);
#3338=(
BOUNDED_SURFACE()
B_SPLINE_SURFACE(1,2,((#151234,#151235,#151236,#151237,#151238),(#151239,
#151240,#151241,#151242,#151243)),.UNSPECIFIED.,.F.,.F.,.F.)
B_SPLINE_SURFACE_WITH_KNOTS((2,2),(3,2,3),(0.709590617369615,1.),(0.573052008423653,
0.573654350219911,0.591014490232053),.UNSPECIFIED.)
GEOMETRIC_REPRESENTATION_ITEM()
RATIONAL_B_SPLINE_SURFACE(((0.99848615229188,0.99848615229188,0.99848615229188,
0.992772345172011,0.990020524139833),(0.99848615229188,0.99848615229188,
0.99848615229188,0.992772345172011,0.990020524139833)))
REPRESENTATION_ITEM('')
SURFACE()
);
#3339=(
BOUNDED_SURFACE()
B_SPLINE_SURFACE(1,2,((#151252,#151253,#151254,#151255,#151256),(#151257,
#151258,#151259,#151260,#151261)),.UNSPECIFIED.,.F.,.F.,.F.)
B_SPLINE_SURFACE_WITH_KNOTS((2,2),(3,2,3),(0.710318915640074,1.),(0.142474614281351,
0.142857142857143,0.159901408087481),.UNSPECIFIED.)
GEOMETRIC_REPRESENTATION_ITEM()
RATIONAL_B_SPLINE_SURFACE(((0.999732896029227,0.999865728939367,1.,0.994017305594881,
0.990889788836284),(0.999732896029227,0.999865728939367,1.,0.994017305594881,
0.990889788836284)))
REPRESENTATION_ITEM('')
SURFACE()
);
#3340=(
BOUNDED_SURFACE()
B_SPLINE_SURFACE(1,2,((#151263,#151264,#151265,#151266,#151267),(#151268,
#151269,#151270,#151271,#151272)),.UNSPECIFIED.,.F.,.F.,.F.)
B_SPLINE_SURFACE_WITH_KNOTS((2,2),(3,2,3),(0.709590617376943,1.),(0.57305200846928,
0.573654350219911,0.591014490232042),.UNSPECIFIED.)
GEOMETRIC_REPRESENTATION_ITEM()
RATIONAL_B_SPLINE_SURFACE(((0.99848615229188,0.99848615229188,0.99848615229188,
0.992772345172015,0.990020524139836),(0.99848615229188,0.99848615229188,
0.99848615229188,0.992772345172015,0.990020524139836)))
REPRESENTATION_ITEM('')
SURFACE()
);
#3341=(
BOUNDED_SURFACE()
B_SPLINE_SURFACE(1,2,((#151281,#151282,#151283,#151284,#151285),(#151286,
#151287,#151288,#151289,#151290)),.UNSPECIFIED.,.F.,.F.,.F.)
B_SPLINE_SURFACE_WITH_KNOTS((2,2),(3,2,3),(0.71031891564008,1.),(0.14247461428135,
0.142857142857143,0.159901408087481),.UNSPECIFIED.)
GEOMETRIC_REPRESENTATION_ITEM()
RATIONAL_B_SPLINE_SURFACE(((0.999732896029226,0.999865728939367,1.,0.994017305594881,
0.990889788836284),(0.999732896029226,0.999865728939367,1.,0.994017305594881,
0.990889788836284)))
REPRESENTATION_ITEM('')
SURFACE()
);
#3342=(
BOUNDED_SURFACE()
B_SPLINE_SURFACE(1,2,((#151292,#151293,#151294,#151295,#151296),(#151297,
#151298,#151299,#151300,#151301)),.UNSPECIFIED.,.F.,.F.,.F.)
B_SPLINE_SURFACE_WITH_KNOTS((2,2),(3,2,3),(0.70959061736192,1.),(0.573052008416099,
0.573654350219911,0.591014490232053),.UNSPECIFIED.)
GEOMETRIC_REPRESENTATION_ITEM()
RATIONAL_B_SPLINE_SURFACE(((0.99848615229188,0.99848615229188,0.99848615229188,
0.992772345172011,0.990020524139833),(0.99848615229188,0.99848615229188,
0.99848615229188,0.992772345172011,0.990020524139833)))
REPRESENTATION_ITEM('')
SURFACE()
);
#3343=(
BOUNDED_SURFACE()
B_SPLINE_SURFACE(1,2,((#151310,#151311,#151312,#151313,#151314),(#151315,
#151316,#151317,#151318,#151319)),.UNSPECIFIED.,.F.,.F.,.F.)
B_SPLINE_SURFACE_WITH_KNOTS((2,2),(3,2,3),(0.710318915640078,1.),(0.142474614281354,
0.142857142857143,0.159901408087481),.UNSPECIFIED.)
GEOMETRIC_REPRESENTATION_ITEM()
RATIONAL_B_SPLINE_SURFACE(((0.999732896029229,0.999865728939368,1.,0.994017305594881,
0.990889788836284),(0.999732896029229,0.999865728939368,1.,0.994017305594881,
0.990889788836284)))
REPRESENTATION_ITEM('')
SURFACE()
);
#3344=(
BOUNDED_SURFACE()
B_SPLINE_SURFACE(1,2,((#151321,#151322,#151323,#151324,#151325),(#151326,
#151327,#151328,#151329,#151330)),.UNSPECIFIED.,.F.,.F.,.F.)
B_SPLINE_SURFACE_WITH_KNOTS((2,2),(3,2,3),(0.709590617385339,1.),(0.573052008438801,
0.573654350219911,0.591014490232053),.UNSPECIFIED.)
GEOMETRIC_REPRESENTATION_ITEM()
RATIONAL_B_SPLINE_SURFACE(((0.99848615229188,0.99848615229188,0.99848615229188,
0.992772345172011,0.990020524139833),(0.99848615229188,0.99848615229188,
0.99848615229188,0.992772345172011,0.990020524139833)))
REPRESENTATION_ITEM('')
SURFACE()
);
#3345=(
BOUNDED_SURFACE()
B_SPLINE_SURFACE(1,2,((#151339,#151340,#151341,#151342,#151343),(#151344,
#151345,#151346,#151347,#151348)),.UNSPECIFIED.,.F.,.F.,.F.)
B_SPLINE_SURFACE_WITH_KNOTS((2,2),(3,2,3),(0.710318915640077,1.),(0.142474614281367,
0.142857142857143,0.159901408087482),.UNSPECIFIED.)
GEOMETRIC_REPRESENTATION_ITEM()
RATIONAL_B_SPLINE_SURFACE(((0.999732896029237,0.999865728939372,1.,0.994017305594881,
0.990889788836284),(0.999732896029237,0.999865728939372,1.,0.994017305594881,
0.990889788836284)))
REPRESENTATION_ITEM('')
SURFACE()
);
#3346=(
BOUNDED_SURFACE()
B_SPLINE_SURFACE(1,2,((#151350,#151351,#151352,#151353,#151354),(#151355,
#151356,#151357,#151358,#151359)),.UNSPECIFIED.,.F.,.F.,.F.)
B_SPLINE_SURFACE_WITH_KNOTS((2,2),(3,2,3),(0.709590617381935,1.),(0.573052008435693,
0.573654350219837,0.591014490232053),.UNSPECIFIED.)
GEOMETRIC_REPRESENTATION_ITEM()
RATIONAL_B_SPLINE_SURFACE(((0.998486152291929,0.998486152291929,0.998486152291929,
0.992772345172023,0.990020524139833),(0.998486152291929,0.998486152291929,
0.998486152291929,0.992772345172023,0.990020524139833)))
REPRESENTATION_ITEM('')
SURFACE()
);
#3347=(
BOUNDED_SURFACE()
B_SPLINE_SURFACE(1,2,((#151368,#151369,#151370,#151371,#151372),(#151373,
#151374,#151375,#151376,#151377),(#151378,#151379,#151380,#151381,#151382)),
 .UNSPECIFIED.,.F.,.F.,.F.)
B_SPLINE_SURFACE_WITH_KNOTS((2,1,2),(3,2,3),(0.710318915640078,1.,1.0028968108436),
(0.142474614281367,0.142857142857143,0.159901408087481),.UNSPECIFIED.)
GEOMETRIC_REPRESENTATION_ITEM()
RATIONAL_B_SPLINE_SURFACE(((0.999732896029237,0.999865728939372,1.,0.994017305594881,
0.990889788836284),(0.999732896029237,0.999865728939372,1.,0.994017305594881,
0.990889788836284),(0.999732896029237,0.999865728939372,1.,0.994017305594881,
0.990889788836284)))
REPRESENTATION_ITEM('')
SURFACE()
);
#3348=(
BOUNDED_SURFACE()
B_SPLINE_SURFACE(1,2,((#151384,#151385,#151386,#151387,#151388),(#151389,
#151390,#151391,#151392,#151393)),.UNSPECIFIED.,.F.,.F.,.F.)
B_SPLINE_SURFACE_WITH_KNOTS((2,2),(3,2,3),(0.709590617367086,1.),(0.573052008457203,
0.573654350219911,0.591014490232053),.UNSPECIFIED.)
GEOMETRIC_REPRESENTATION_ITEM()
RATIONAL_B_SPLINE_SURFACE(((0.99848615229188,0.99848615229188,0.99848615229188,
0.992772345172011,0.990020524139833),(0.99848615229188,0.99848615229188,
0.99848615229188,0.992772345172011,0.990020524139833)))
REPRESENTATION_ITEM('')
SURFACE()
);
#3349=(
BOUNDED_SURFACE()
B_SPLINE_SURFACE(1,2,((#151402,#151403,#151404,#151405,#151406),(#151407,
#151408,#151409,#151410,#151411)),.UNSPECIFIED.,.F.,.F.,.F.)
B_SPLINE_SURFACE_WITH_KNOTS((2,2),(3,2,3),(0.710318915640077,1.),(0.142474614281296,
0.142857142857143,0.159901408087481),.UNSPECIFIED.)
GEOMETRIC_REPRESENTATION_ITEM()
RATIONAL_B_SPLINE_SURFACE(((0.999732896029188,0.999865728939348,1.,0.994017305594881,
0.990889788836284),(0.999732896029188,0.999865728939348,1.,0.994017305594881,
0.990889788836284)))
REPRESENTATION_ITEM('')
SURFACE()
);
#3350=(
BOUNDED_SURFACE()
B_SPLINE_SURFACE(1,2,((#151413,#151414,#151415,#151416,#151417),(#151418,
#151419,#151420,#151421,#151422)),.UNSPECIFIED.,.F.,.F.,.F.)
B_SPLINE_SURFACE_WITH_KNOTS((2,2),(3,2,3),(0.709590617387075,1.),(0.573052008477772,
0.573654350219911,0.591014490232053),.UNSPECIFIED.)
GEOMETRIC_REPRESENTATION_ITEM()
RATIONAL_B_SPLINE_SURFACE(((0.99848615229188,0.99848615229188,0.99848615229188,
0.992772345172011,0.990020524139833),(0.99848615229188,0.99848615229188,
0.99848615229188,0.992772345172011,0.990020524139833)))
REPRESENTATION_ITEM('')
SURFACE()
);
#3351=(
BOUNDED_SURFACE()
B_SPLINE_SURFACE(1,2,((#151431,#151432,#151433,#151434,#151435),(#151436,
#151437,#151438,#151439,#151440)),.UNSPECIFIED.,.F.,.F.,.F.)
B_SPLINE_SURFACE_WITH_KNOTS((2,2),(3,2,3),(0.710318915640081,1.),(0.142474614281367,
0.142857142857143,0.159901408087481),.UNSPECIFIED.)
GEOMETRIC_REPRESENTATION_ITEM()
RATIONAL_B_SPLINE_SURFACE(((0.999732896029237,0.999865728939372,1.,0.994017305594881,
0.990889788836284),(0.999732896029237,0.999865728939372,1.,0.994017305594881,
0.990889788836284)))
REPRESENTATION_ITEM('')
SURFACE()
);
#3352=(
BOUNDED_SURFACE()
B_SPLINE_SURFACE(1,2,((#151442,#151443,#151444,#151445,#151446),(#151447,
#151448,#151449,#151450,#151451)),.UNSPECIFIED.,.F.,.F.,.F.)
B_SPLINE_SURFACE_WITH_KNOTS((2,2),(3,2,3),(0.710192959008437,1.),(0.57348074881979,
0.573654350219911,0.591014490232053),.UNSPECIFIED.)
GEOMETRIC_REPRESENTATION_ITEM()
RATIONAL_B_SPLINE_SURFACE(((0.99848615229188,0.99848615229188,0.99848615229188,
0.992772345172011,0.990020524139833),(0.99848615229188,0.99848615229188,
0.99848615229188,0.992772345172011,0.990020524139833)))
REPRESENTATION_ITEM('')
SURFACE()
);
#3353=(
BOUNDED_SURFACE()
B_SPLINE_SURFACE(1,2,((#151460,#151461,#151462,#151463,#151464),(#151465,
#151466,#151467,#151468,#151469)),.UNSPECIFIED.,.F.,.F.,.F.)
B_SPLINE_SURFACE_WITH_KNOTS((2,2),(3,2,3),(0.710318915640077,1.),(0.142474614281367,
0.142857142857143,0.159901408087482),.UNSPECIFIED.)
GEOMETRIC_REPRESENTATION_ITEM()
RATIONAL_B_SPLINE_SURFACE(((0.999732896029237,0.999865728939372,1.,0.994017305594881,
0.990889788836284),(0.999732896029237,0.999865728939372,1.,0.994017305594881,
0.990889788836284)))
REPRESENTATION_ITEM('')
SURFACE()
);
#3354=(
BOUNDED_SURFACE()
B_SPLINE_SURFACE(1,2,((#151471,#151472,#151473,#151474,#151475),(#151476,
#151477,#151478,#151479,#151480)),.UNSPECIFIED.,.F.,.F.,.F.)
B_SPLINE_SURFACE_WITH_KNOTS((2,2),(3,2,3),(0.709968463042327,1.),(0.573429854103688,
0.573654350219911,0.591014490232053),.UNSPECIFIED.)
GEOMETRIC_REPRESENTATION_ITEM()
RATIONAL_B_SPLINE_SURFACE(((0.99848615229188,0.99848615229188,0.99848615229188,
0.992772345172011,0.990020524139833),(0.99848615229188,0.99848615229188,
0.99848615229188,0.992772345172011,0.990020524139833)))
REPRESENTATION_ITEM('')
SURFACE()
);
#3355=(
BOUNDED_SURFACE()
B_SPLINE_SURFACE(1,2,((#151489,#151490,#151491,#151492,#151493),(#151494,
#151495,#151496,#151497,#151498),(#151499,#151500,#151501,#151502,#151503)),
 .UNSPECIFIED.,.F.,.F.,.F.)
B_SPLINE_SURFACE_WITH_KNOTS((2,1,2),(3,2,3),(0.710318915640081,1.,1.0028968108436),
(0.142474614281367,0.142857142857143,0.159901408087482),.UNSPECIFIED.)
GEOMETRIC_REPRESENTATION_ITEM()
RATIONAL_B_SPLINE_SURFACE(((0.999732896029237,0.999865728939372,1.,0.994017305594881,
0.990889788836284),(0.999732896029237,0.999865728939372,1.,0.994017305594881,
0.990889788836284),(0.999732896029237,0.999865728939372,1.,0.994017305594881,
0.990889788836284)))
REPRESENTATION_ITEM('')
SURFACE()
);
#3356=(
BOUNDED_SURFACE()
B_SPLINE_SURFACE(1,2,((#151505,#151506,#151507,#151508,#151509),(#151510,
#151511,#151512,#151513,#151514)),.UNSPECIFIED.,.F.,.F.,.F.)
B_SPLINE_SURFACE_WITH_KNOTS((2,2),(3,2,3),(0.709590617371185,1.),(0.573052008461026,
0.573654350219911,0.591014490232053),.UNSPECIFIED.)
GEOMETRIC_REPRESENTATION_ITEM()
RATIONAL_B_SPLINE_SURFACE(((0.99848615229188,0.99848615229188,0.99848615229188,
0.992772345172011,0.990020524139833),(0.99848615229188,0.99848615229188,
0.99848615229188,0.992772345172011,0.990020524139833)))
REPRESENTATION_ITEM('')
SURFACE()
);
#3357=(
BOUNDED_SURFACE()
B_SPLINE_SURFACE(1,2,((#151523,#151524,#151525,#151526,#151527),(#151528,
#151529,#151530,#151531,#151532)),.UNSPECIFIED.,.F.,.F.,.F.)
B_SPLINE_SURFACE_WITH_KNOTS((2,2),(3,2,3),(0.71031891564008,1.),(0.142474614281085,
0.142857142857143,0.159901408087482),.UNSPECIFIED.)
GEOMETRIC_REPRESENTATION_ITEM()
RATIONAL_B_SPLINE_SURFACE(((0.999732896029042,0.999865728939274,1.,0.994017305594881,
0.990889788836284),(0.999732896029042,0.999865728939274,1.,0.994017305594881,
0.990889788836284)))
REPRESENTATION_ITEM('')
SURFACE()
);
#3358=(
BOUNDED_SURFACE()
B_SPLINE_SURFACE(1,2,((#151534,#151535,#151536,#151537,#151538),(#151539,
#151540,#151541,#151542,#151543)),.UNSPECIFIED.,.F.,.F.,.F.)
B_SPLINE_SURFACE_WITH_KNOTS((2,2),(3,2,3),(0.709590617399634,1.),(0.573052008453065,
0.573654350219911,0.591014490232053),.UNSPECIFIED.)
GEOMETRIC_REPRESENTATION_ITEM()
RATIONAL_B_SPLINE_SURFACE(((0.99848615229188,0.99848615229188,0.99848615229188,
0.992772345172011,0.990020524139833),(0.99848615229188,0.99848615229188,
0.99848615229188,0.992772345172011,0.990020524139833)))
REPRESENTATION_ITEM('')
SURFACE()
);
#3359=(
BOUNDED_SURFACE()
B_SPLINE_SURFACE(1,2,((#151552,#151553,#151554,#151555,#151556),(#151557,
#151558,#151559,#151560,#151561)),.UNSPECIFIED.,.F.,.F.,.F.)
B_SPLINE_SURFACE_WITH_KNOTS((2,2),(3,2,3),(0.710318915640076,1.),(0.142474614280958,
0.142857142857143,0.159901408087482),.UNSPECIFIED.)
GEOMETRIC_REPRESENTATION_ITEM()
RATIONAL_B_SPLINE_SURFACE(((0.999732896028954,0.999865728939229,1.,0.994017305594881,
0.990889788836284),(0.999732896028954,0.999865728939229,1.,0.994017305594881,
0.990889788836284)))
REPRESENTATION_ITEM('')
SURFACE()
);
#3360=(
BOUNDED_SURFACE()
B_SPLINE_SURFACE(1,2,((#151563,#151564,#151565,#151566,#151567),(#151568,
#151569,#151570,#151571,#151572)),.UNSPECIFIED.,.F.,.F.,.F.)
B_SPLINE_SURFACE_WITH_KNOTS((2,2),(3,2,3),(0.709590617387241,1.),(0.573052008440968,
0.573654350219911,0.591014490232053),.UNSPECIFIED.)
GEOMETRIC_REPRESENTATION_ITEM()
RATIONAL_B_SPLINE_SURFACE(((0.99848615229188,0.99848615229188,0.99848615229188,
0.992772345172011,0.990020524139833),(0.99848615229188,0.99848615229188,
0.99848615229188,0.992772345172011,0.990020524139833)))
REPRESENTATION_ITEM('')
SURFACE()
);
#3361=(
BOUNDED_SURFACE()
B_SPLINE_SURFACE(1,2,((#151581,#151582,#151583,#151584,#151585),(#151586,
#151587,#151588,#151589,#151590)),.UNSPECIFIED.,.F.,.F.,.F.)
B_SPLINE_SURFACE_WITH_KNOTS((2,2),(3,2,3),(0.710318915640086,1.),(0.142474614281367,
0.142857142857143,0.159901408087481),.UNSPECIFIED.)
GEOMETRIC_REPRESENTATION_ITEM()
RATIONAL_B_SPLINE_SURFACE(((0.999732896029237,0.999865728939372,1.,0.994017305594881,
0.990889788836284),(0.999732896029237,0.999865728939372,1.,0.994017305594881,
0.990889788836284)))
REPRESENTATION_ITEM('')
SURFACE()
);
#3362=(
BOUNDED_SURFACE()
B_SPLINE_SURFACE(1,2,((#151592,#151593,#151594,#151595,#151596),(#151597,
#151598,#151599,#151600,#151601)),.UNSPECIFIED.,.F.,.F.,.F.)
B_SPLINE_SURFACE_WITH_KNOTS((2,2),(3,2,3),(0.709590617385605,1.),(0.573052008476401,
0.573654350219911,0.591014490232053),.UNSPECIFIED.)
GEOMETRIC_REPRESENTATION_ITEM()
RATIONAL_B_SPLINE_SURFACE(((0.99848615229188,0.99848615229188,0.99848615229188,
0.992772345172011,0.990020524139833),(0.99848615229188,0.99848615229188,
0.99848615229188,0.992772345172011,0.990020524139833)))
REPRESENTATION_ITEM('')
SURFACE()
);
#3363=(
BOUNDED_SURFACE()
B_SPLINE_SURFACE(1,2,((#151610,#151611,#151612,#151613,#151614),(#151615,
#151616,#151617,#151618,#151619)),.UNSPECIFIED.,.F.,.F.,.F.)
B_SPLINE_SURFACE_WITH_KNOTS((2,2),(3,2,3),(0.710318915640079,1.),(0.142474614281367,
0.142857142857143,0.159901408087481),.UNSPECIFIED.)
GEOMETRIC_REPRESENTATION_ITEM()
RATIONAL_B_SPLINE_SURFACE(((0.999732896029237,0.999865728939372,1.,0.994017305594881,
0.990889788836284),(0.999732896029237,0.999865728939372,1.,0.994017305594881,
0.990889788836284)))
REPRESENTATION_ITEM('')
SURFACE()
);
#3364=(
BOUNDED_SURFACE()
B_SPLINE_SURFACE(1,2,((#151621,#151622,#151623,#151624,#151625),(#151626,
#151627,#151628,#151629,#151630)),.UNSPECIFIED.,.F.,.F.,.F.)
B_SPLINE_SURFACE_WITH_KNOTS((2,2),(3,2,3),(0.709590617380986,1.),(0.573052008470953,
0.573654350219905,0.591014490232052),.UNSPECIFIED.)
GEOMETRIC_REPRESENTATION_ITEM()
RATIONAL_B_SPLINE_SURFACE(((0.998486152291883,0.998486152291883,0.998486152291883,
0.992772345172012,0.990020524139833),(0.998486152291883,0.998486152291883,
0.998486152291883,0.992772345172012,0.990020524139833)))
REPRESENTATION_ITEM('')
SURFACE()
);
#3365=(
BOUNDED_SURFACE()
B_SPLINE_SURFACE(1,2,((#151639,#151640,#151641,#151642,#151643),(#151644,
#151645,#151646,#151647,#151648)),.UNSPECIFIED.,.F.,.F.,.F.)
B_SPLINE_SURFACE_WITH_KNOTS((2,2),(3,2,3),(0.710318915639879,1.),(0.142474614281367,
0.142857142857143,0.159901408087485),.UNSPECIFIED.)
GEOMETRIC_REPRESENTATION_ITEM()
RATIONAL_B_SPLINE_SURFACE(((0.999732896029238,0.999865728939373,1.,0.99401730559488,
0.990889788836283),(0.999732896029238,0.999865728939373,1.,0.99401730559488,
0.990889788836283)))
REPRESENTATION_ITEM('')
SURFACE()
);
#3366=(
BOUNDED_SURFACE()
B_SPLINE_SURFACE(1,2,((#151650,#151651,#151652,#151653,#151654),(#151655,
#151656,#151657,#151658,#151659)),.UNSPECIFIED.,.F.,.F.,.F.)
B_SPLINE_SURFACE_WITH_KNOTS((2,2),(3,2,3),(0.709590617360321,1.),(0.573052008450992,
0.57365435021991,0.591014490232052),.UNSPECIFIED.)
GEOMETRIC_REPRESENTATION_ITEM()
RATIONAL_B_SPLINE_SURFACE(((0.998486152291881,0.998486152291881,0.998486152291881,
0.992772345172012,0.990020524139833),(0.998486152291881,0.998486152291881,
0.998486152291881,0.992772345172012,0.990020524139833)))
REPRESENTATION_ITEM('')
SURFACE()
);
#3367=(
BOUNDED_SURFACE()
B_SPLINE_SURFACE(1,2,((#151668,#151669,#151670,#151671,#151672),(#151673,
#151674,#151675,#151676,#151677)),.UNSPECIFIED.,.F.,.F.,.F.)
B_SPLINE_SURFACE_WITH_KNOTS((2,2),(3,2,3),(0.710318915639129,1.),(0.142474614281368,
0.142857142857143,0.159901408087494),.UNSPECIFIED.)
GEOMETRIC_REPRESENTATION_ITEM()
RATIONAL_B_SPLINE_SURFACE(((0.999732896029238,0.999865728939373,1.,0.994017305594877,
0.990889788836279),(0.999732896029238,0.999865728939373,1.,0.994017305594877,
0.990889788836279)))
REPRESENTATION_ITEM('')
SURFACE()
);
#3368=(
BOUNDED_SURFACE()
B_SPLINE_SURFACE(1,2,((#151679,#151680,#151681,#151682,#151683),(#151684,
#151685,#151686,#151687,#151688)),.UNSPECIFIED.,.F.,.F.,.F.)
B_SPLINE_SURFACE_WITH_KNOTS((2,2),(3,2,3),(0.710192959008292,1.),(0.573480748819789,
0.57365435021991,0.591014490232053),.UNSPECIFIED.)
GEOMETRIC_REPRESENTATION_ITEM()
RATIONAL_B_SPLINE_SURFACE(((0.99848615229188,0.99848615229188,0.99848615229188,
0.992772345172011,0.990020524139833),(0.99848615229188,0.99848615229188,
0.99848615229188,0.992772345172011,0.990020524139833)))
REPRESENTATION_ITEM('')
SURFACE()
);
#3369=(
BOUNDED_SURFACE()
B_SPLINE_SURFACE(1,2,((#151697,#151698,#151699,#151700,#151701),(#151702,
#151703,#151704,#151705,#151706)),.UNSPECIFIED.,.F.,.F.,.F.)
B_SPLINE_SURFACE_WITH_KNOTS((2,2),(3,2,3),(0.710318915638992,1.),(0.142474614281365,
0.142857142857143,0.159901408087493),.UNSPECIFIED.)
GEOMETRIC_REPRESENTATION_ITEM()
RATIONAL_B_SPLINE_SURFACE(((0.999732896029236,0.999865728939372,1.,0.994017305594877,
0.99088978883628),(0.999732896029236,0.999865728939372,1.,0.994017305594877,
0.99088978883628)))
REPRESENTATION_ITEM('')
SURFACE()
);
#3370=(
BOUNDED_SURFACE()
B_SPLINE_SURFACE(1,2,((#151708,#151709,#151710,#151711,#151712),(#151713,
#151714,#151715,#151716,#151717)),.UNSPECIFIED.,.F.,.F.,.F.)
B_SPLINE_SURFACE_WITH_KNOTS((2,2),(3,2,3),(0.709590617378624,1.),(0.573052008469533,
0.57365435021991,0.591014490232052),.UNSPECIFIED.)
GEOMETRIC_REPRESENTATION_ITEM()
RATIONAL_B_SPLINE_SURFACE(((0.99848615229188,0.99848615229188,0.99848615229188,
0.992772345172011,0.990020524139833),(0.99848615229188,0.99848615229188,
0.99848615229188,0.992772345172011,0.990020524139833)))
REPRESENTATION_ITEM('')
SURFACE()
);
#3371=(
BOUNDED_SURFACE()
B_SPLINE_SURFACE(1,2,((#151726,#151727,#151728,#151729,#151730),(#151731,
#151732,#151733,#151734,#151735)),.UNSPECIFIED.,.F.,.F.,.F.)
B_SPLINE_SURFACE_WITH_KNOTS((2,2),(3,2,3),(0.710318915639023,1.),(0.142474614281365,
0.142857142857143,0.159901408087496),.UNSPECIFIED.)
GEOMETRIC_REPRESENTATION_ITEM()
RATIONAL_B_SPLINE_SURFACE(((0.999732896029237,0.999865728939372,1.,0.994017305594876,
0.990889788836279),(0.999732896029237,0.999865728939372,1.,0.994017305594876,
0.990889788836279)))
REPRESENTATION_ITEM('')
SURFACE()
);
#3372=(
BOUNDED_SURFACE()
B_SPLINE_SURFACE(1,2,((#151737,#151738,#151739,#151740,#151741),(#151742,
#151743,#151744,#151745,#151746)),.UNSPECIFIED.,.F.,.F.,.F.)
B_SPLINE_SURFACE_WITH_KNOTS((2,2),(3,2,3),(0.709590617379361,1.),(0.573052008435022,
0.57365435021991,0.591014490232051),.UNSPECIFIED.)
GEOMETRIC_REPRESENTATION_ITEM()
RATIONAL_B_SPLINE_SURFACE(((0.99848615229188,0.99848615229188,0.99848615229188,
0.992772345172012,0.990020524139833),(0.99848615229188,0.99848615229188,
0.99848615229188,0.992772345172012,0.990020524139833)))
REPRESENTATION_ITEM('')
SURFACE()
);
#3373=(
BOUNDED_SURFACE()
B_SPLINE_SURFACE(1,2,((#151755,#151756,#151757,#151758,#151759),(#151760,
#151761,#151762,#151763,#151764),(#151765,#151766,#151767,#151768,#151769)),
 .UNSPECIFIED.,.F.,.F.,.F.)
B_SPLINE_SURFACE_WITH_KNOTS((2,1,2),(3,2,3),(0.710318915638281,1.,1.00289681084362),
(0.142474614281367,0.142857142857143,0.159901408087482),.UNSPECIFIED.)
GEOMETRIC_REPRESENTATION_ITEM()
RATIONAL_B_SPLINE_SURFACE(((0.999732896029237,0.999865728939372,1.,0.994017305594881,
0.990889788836284),(0.999732896029237,0.999865728939372,1.,0.994017305594881,
0.990889788836284),(0.999732896029237,0.999865728939372,1.,0.994017305594881,
0.990889788836284)))
REPRESENTATION_ITEM('')
SURFACE()
);
#3374=(
BOUNDED_SURFACE()
B_SPLINE_SURFACE(1,2,((#151771,#151772,#151773,#151774,#151775),(#151776,
#151777,#151778,#151779,#151780)),.UNSPECIFIED.,.F.,.F.,.F.)
B_SPLINE_SURFACE_WITH_KNOTS((2,2),(3,2,3),(0.7095906173851,1.),(0.573052008439701,
0.573654350219884,0.591014490232052),.UNSPECIFIED.)
GEOMETRIC_REPRESENTATION_ITEM()
RATIONAL_B_SPLINE_SURFACE(((0.998486152291898,0.998486152291898,0.998486152291898,
0.992772345172016,0.990020524139833),(0.998486152291898,0.998486152291898,
0.998486152291898,0.992772345172016,0.990020524139833)))
REPRESENTATION_ITEM('')
SURFACE()
);
#3375=(
BOUNDED_SURFACE()
B_SPLINE_SURFACE(1,2,((#151789,#151790,#151791,#151792,#151793),(#151794,
#151795,#151796,#151797,#151798)),.UNSPECIFIED.,.F.,.F.,.F.)
B_SPLINE_SURFACE_WITH_KNOTS((2,2),(3,2,3),(0.710318915639621,1.),(0.14247461428136,
0.142857142857143,0.159901408087483),.UNSPECIFIED.)
GEOMETRIC_REPRESENTATION_ITEM()
RATIONAL_B_SPLINE_SURFACE(((0.999732896029233,0.99986572893937,1.,0.994017305594881,
0.990889788836283),(0.999732896029233,0.99986572893937,1.,0.994017305594881,
0.990889788836283)))
REPRESENTATION_ITEM('')
SURFACE()
);
#3376=(
BOUNDED_SURFACE()
B_SPLINE_SURFACE(1,2,((#151800,#151801,#151802,#151803,#151804),(#151805,
#151806,#151807,#151808,#151809)),.UNSPECIFIED.,.F.,.F.,.F.)
B_SPLINE_SURFACE_WITH_KNOTS((2,2),(3,2,3),(0.709590617367967,1.),(0.573052008421813,
0.57365435021991,0.591014490232046),.UNSPECIFIED.)
GEOMETRIC_REPRESENTATION_ITEM()
RATIONAL_B_SPLINE_SURFACE(((0.99848615229188,0.99848615229188,0.99848615229188,
0.992772345172013,0.990020524139835),(0.99848615229188,0.99848615229188,
0.99848615229188,0.992772345172013,0.990020524139835)))
REPRESENTATION_ITEM('')
SURFACE()
);
#3377=(
BOUNDED_SURFACE()
B_SPLINE_SURFACE(1,2,((#151818,#151819,#151820,#151821,#151822),(#151823,
#151824,#151825,#151826,#151827)),.UNSPECIFIED.,.F.,.F.,.F.)
B_SPLINE_SURFACE_WITH_KNOTS((2,2),(3,2,3),(0.71031891564,1.),(0.14247461428136,
0.142857142857143,0.159901408087483),.UNSPECIFIED.)
GEOMETRIC_REPRESENTATION_ITEM()
RATIONAL_B_SPLINE_SURFACE(((0.999732896029233,0.99986572893937,1.,0.994017305594881,
0.990889788836283),(0.999732896029233,0.99986572893937,1.,0.994017305594881,
0.990889788836283)))
REPRESENTATION_ITEM('')
SURFACE()
);
#3378=(
BOUNDED_SURFACE()
B_SPLINE_SURFACE(1,2,((#151829,#151830,#151831,#151832,#151833),(#151834,
#151835,#151836,#151837,#151838)),.UNSPECIFIED.,.F.,.F.,.F.)
B_SPLINE_SURFACE_WITH_KNOTS((2,2),(3,2,3),(0.71019295900836,1.),(0.573480748819789,
0.57365435021991,0.591014490232052),.UNSPECIFIED.)
GEOMETRIC_REPRESENTATION_ITEM()
RATIONAL_B_SPLINE_SURFACE(((0.99848615229188,0.99848615229188,0.99848615229188,
0.992772345172012,0.990020524139833),(0.99848615229188,0.99848615229188,
0.99848615229188,0.992772345172012,0.990020524139833)))
REPRESENTATION_ITEM('')
SURFACE()
);
#3379=(
BOUNDED_SURFACE()
B_SPLINE_SURFACE(1,2,((#151847,#151848,#151849,#151850,#151851),(#151852,
#151853,#151854,#151855,#151856)),.UNSPECIFIED.,.F.,.F.,.F.)
B_SPLINE_SURFACE_WITH_KNOTS((2,2),(3,2,3),(0.710318915640007,1.),(0.142474614281363,
0.142857142857143,0.159901408087482),.UNSPECIFIED.)
GEOMETRIC_REPRESENTATION_ITEM()
RATIONAL_B_SPLINE_SURFACE(((0.999732896029235,0.999865728939371,1.,0.994017305594881,
0.990889788836284),(0.999732896029235,0.999865728939371,1.,0.994017305594881,
0.990889788836284)))
REPRESENTATION_ITEM('')
SURFACE()
);
#3380=(
BOUNDED_SURFACE()
B_SPLINE_SURFACE(1,2,((#151858,#151859,#151860,#151861,#151862),(#151863,
#151864,#151865,#151866,#151867)),.UNSPECIFIED.,.F.,.F.,.F.)
B_SPLINE_SURFACE_WITH_KNOTS((2,2),(3,2,3),(0.710192959008365,1.),(0.573480748819789,
0.57365435021991,0.591014490232052),.UNSPECIFIED.)
GEOMETRIC_REPRESENTATION_ITEM()
RATIONAL_B_SPLINE_SURFACE(((0.99848615229188,0.99848615229188,0.99848615229188,
0.992772345172012,0.990020524139833),(0.99848615229188,0.99848615229188,
0.99848615229188,0.992772345172012,0.990020524139833)))
REPRESENTATION_ITEM('')
SURFACE()
);
#3381=(
BOUNDED_SURFACE()
B_SPLINE_SURFACE(1,2,((#151876,#151877,#151878,#151879,#151880),(#151881,
#151882,#151883,#151884,#151885)),.UNSPECIFIED.,.F.,.F.,.F.)
B_SPLINE_SURFACE_WITH_KNOTS((2,2),(3,2,3),(0.710318915640009,1.),(0.142474614281368,
0.142857142857143,0.159901408087482),.UNSPECIFIED.)
GEOMETRIC_REPRESENTATION_ITEM()
RATIONAL_B_SPLINE_SURFACE(((0.999732896029238,0.999865728939373,1.,0.994017305594881,
0.990889788836284),(0.999732896029238,0.999865728939373,1.,0.994017305594881,
0.990889788836284)))
REPRESENTATION_ITEM('')
SURFACE()
);
#3382=(
BOUNDED_SURFACE()
B_SPLINE_SURFACE(1,2,((#151887,#151888,#151889,#151890,#151891),(#151892,
#151893,#151894,#151895,#151896)),.UNSPECIFIED.,.F.,.F.,.F.)
B_SPLINE_SURFACE_WITH_KNOTS((2,2),(3,2,3),(0.710192959008085,1.),(0.573480748819736,
0.573654350219858,0.591014490232052),.UNSPECIFIED.)
GEOMETRIC_REPRESENTATION_ITEM()
RATIONAL_B_SPLINE_SURFACE(((0.998486152291915,0.998486152291915,0.998486152291915,
0.99277234517202,0.990020524139833),(0.998486152291915,0.998486152291915,
0.998486152291915,0.99277234517202,0.990020524139833)))
REPRESENTATION_ITEM('')
SURFACE()
);
#3383=(
BOUNDED_SURFACE()
B_SPLINE_SURFACE(1,2,((#151905,#151906,#151907,#151908,#151909),(#151910,
#151911,#151912,#151913,#151914),(#151915,#151916,#151917,#151918,#151919)),
 .UNSPECIFIED.,.F.,.F.,.F.)
B_SPLINE_SURFACE_WITH_KNOTS((2,1,2),(3,2,3),(0.710318915639726,1.,1.0028968108436),
(0.142474614281368,0.142857142857143,0.159901408087482),.UNSPECIFIED.)
GEOMETRIC_REPRESENTATION_ITEM()
RATIONAL_B_SPLINE_SURFACE(((0.999732896029238,0.999865728939373,1.,0.994017305594881,
0.990889788836284),(0.999732896029238,0.999865728939373,1.,0.994017305594881,
0.990889788836284),(0.999732896029238,0.999865728939373,1.,0.994017305594881,
0.990889788836284)))
REPRESENTATION_ITEM('')
SURFACE()
);
#3384=(
BOUNDED_SURFACE()
B_SPLINE_SURFACE(1,2,((#151921,#151922,#151923,#151924,#151925),(#151926,
#151927,#151928,#151929,#151930)),.UNSPECIFIED.,.F.,.F.,.F.)
B_SPLINE_SURFACE_WITH_KNOTS((2,2),(3,2,3),(0.,0.289940743966858),(0.0908085233856358,
0.107982157956012,0.108241818529102),.UNSPECIFIED.)
GEOMETRIC_REPRESENTATION_ITEM()
RATIONAL_B_SPLINE_SURFACE(((0.990086238235256,0.987329216372183,0.987470879370256,
0.987470879370256,0.987470879370256),(0.990086238235256,0.987329216372183,
0.987470879370256,0.987470879370256,0.987470879370256)))
REPRESENTATION_ITEM('')
SURFACE()
);
#3385=(
BOUNDED_SURFACE()
B_SPLINE_SURFACE(1,2,((#151934,#151935,#151936),(#151937,#151938,#151939)),
 .UNSPECIFIED.,.F.,.F.,.F.)
B_SPLINE_SURFACE_WITH_KNOTS((2,2),(3,3),(0.,0.289807040992019),(0.625170525609407,
0.642682999576235),.UNSPECIFIED.)
GEOMETRIC_REPRESENTATION_ITEM()
RATIONAL_B_SPLINE_SURFACE(((0.990658108926708,0.993760979299921,0.999878046252916),
(0.990658108926708,0.993760979299921,0.999878046252916)))
REPRESENTATION_ITEM('')
SURFACE()
);
#3386=(
BOUNDED_SURFACE()
B_SPLINE_SURFACE(1,2,((#151941,#151942,#151943,#151944,#151945),(#151946,
#151947,#151948,#151949,#151950)),.UNSPECIFIED.,.F.,.F.,.F.)
B_SPLINE_SURFACE_WITH_KNOTS((2,2),(3,2,3),(0.,0.289940743918361),(0.0908085233856356,
0.107982157956012,0.10824181848113),.UNSPECIFIED.)
GEOMETRIC_REPRESENTATION_ITEM()
RATIONAL_B_SPLINE_SURFACE(((0.990086238235256,0.987329216372183,0.987470879370255,
0.987470879370255,0.987470879370255),(0.990086238235256,0.987329216372183,
0.987470879370255,0.987470879370255,0.987470879370255)))
REPRESENTATION_ITEM('')
SURFACE()
);
#3387=(
BOUNDED_SURFACE()
B_SPLINE_SURFACE(1,2,((#151954,#151955,#151956),(#151957,#151958,#151959)),
 .UNSPECIFIED.,.F.,.F.,.F.)
B_SPLINE_SURFACE_WITH_KNOTS((2,2),(3,3),(0.,0.289807040992003),(0.625170525609407,
0.642682999576235),.UNSPECIFIED.)
GEOMETRIC_REPRESENTATION_ITEM()
RATIONAL_B_SPLINE_SURFACE(((0.990658108926708,0.993760979299921,0.999878046252916),
(0.990658108926708,0.993760979299921,0.999878046252916)))
REPRESENTATION_ITEM('')
SURFACE()
);
#3388=(
BOUNDED_SURFACE()
B_SPLINE_SURFACE(1,2,((#151961,#151962,#151963,#151964,#151965),(#151966,
#151967,#151968,#151969,#151970)),.UNSPECIFIED.,.F.,.F.,.F.)
B_SPLINE_SURFACE_WITH_KNOTS((2,2),(3,2,3),(0.,0.289940743918459),(0.0908085233856357,
0.107982157956012,0.108241818481194),.UNSPECIFIED.)
GEOMETRIC_REPRESENTATION_ITEM()
RATIONAL_B_SPLINE_SURFACE(((0.990086238235256,0.987329216372183,0.987470879370256,
0.987470879370256,0.987470879370256),(0.990086238235256,0.987329216372183,
0.987470879370256,0.987470879370256,0.987470879370256)))
REPRESENTATION_ITEM('')
SURFACE()
);
#3389=(
BOUNDED_SURFACE()
B_SPLINE_SURFACE(1,2,((#151974,#151975,#151976),(#151977,#151978,#151979)),
 .UNSPECIFIED.,.F.,.F.,.F.)
B_SPLINE_SURFACE_WITH_KNOTS((2,2),(3,3),(0.,0.289807040991873),(0.625170525609407,
0.642682999576235),.UNSPECIFIED.)
GEOMETRIC_REPRESENTATION_ITEM()
RATIONAL_B_SPLINE_SURFACE(((0.990658108926708,0.993760979299921,0.999878046252916),
(0.990658108926708,0.993760979299921,0.999878046252916)))
REPRESENTATION_ITEM('')
SURFACE()
);
#3390=(
BOUNDED_SURFACE()
B_SPLINE_SURFACE(1,2,((#151981,#151982,#151983,#151984,#151985),(#151986,
#151987,#151988,#151989,#151990)),.UNSPECIFIED.,.F.,.F.,.F.)
B_SPLINE_SURFACE_WITH_KNOTS((2,2),(3,2,3),(0.,0.289940743934797),(0.0908085233856346,
0.107982157956012,0.10824181849756),.UNSPECIFIED.)
GEOMETRIC_REPRESENTATION_ITEM()
RATIONAL_B_SPLINE_SURFACE(((0.990086238235256,0.987329216372183,0.987470879370255,
0.987470879370255,0.987470879370255),(0.990086238235257,0.987329216372183,
0.987470879370256,0.987470879370256,0.987470879370256)))
REPRESENTATION_ITEM('')
SURFACE()
);
#3391=(
BOUNDED_SURFACE()
B_SPLINE_SURFACE(1,2,((#151994,#151995,#151996),(#151997,#151998,#151999)),
 .UNSPECIFIED.,.F.,.F.,.F.)
B_SPLINE_SURFACE_WITH_KNOTS((2,2),(3,3),(0.,0.289807040991872),(0.625170525609407,
0.642682999576234),.UNSPECIFIED.)
GEOMETRIC_REPRESENTATION_ITEM()
RATIONAL_B_SPLINE_SURFACE(((0.990658108926708,0.993760979299921,0.999878046252915),
(0.990658108926708,0.993760979299921,0.999878046252915)))
REPRESENTATION_ITEM('')
SURFACE()
);
#3392=(
BOUNDED_SURFACE()
B_SPLINE_SURFACE(1,2,((#152001,#152002,#152003,#152004,#152005),(#152006,
#152007,#152008,#152009,#152010)),.UNSPECIFIED.,.F.,.F.,.F.)
B_SPLINE_SURFACE_WITH_KNOTS((2,2),(3,2,3),(0.,0.289940743974797),(0.0908085233856356,
0.107982157956012,0.108241818491054),.UNSPECIFIED.)
GEOMETRIC_REPRESENTATION_ITEM()
RATIONAL_B_SPLINE_SURFACE(((0.990086238235256,0.987329216372183,0.987470879370255,
0.987470879370255,0.987470879370255),(0.990086238235256,0.987329216372183,
0.987470879370255,0.987470879370255,0.987470879370255)))
REPRESENTATION_ITEM('')
SURFACE()
);
#3393=(
BOUNDED_SURFACE()
B_SPLINE_SURFACE(1,2,((#152014,#152015,#152016),(#152017,#152018,#152019)),
 .UNSPECIFIED.,.F.,.F.,.F.)
B_SPLINE_SURFACE_WITH_KNOTS((2,2),(3,3),(0.,0.289807040992622),(0.625170525609407,
0.642682999576235),.UNSPECIFIED.)
GEOMETRIC_REPRESENTATION_ITEM()
RATIONAL_B_SPLINE_SURFACE(((0.990658108926708,0.993760979299921,0.999878046252915),
(0.990658108926708,0.993760979299921,0.999878046252915)))
REPRESENTATION_ITEM('')
SURFACE()
);
#3394=(
BOUNDED_SURFACE()
B_SPLINE_SURFACE(1,2,((#152021,#152022,#152023,#152024,#152025),(#152026,
#152027,#152028,#152029,#152030)),.UNSPECIFIED.,.F.,.F.,.F.)
B_SPLINE_SURFACE_WITH_KNOTS((2,2),(3,2,3),(0.,0.289940743935406),(0.0908085233856344,
0.107982157956012,0.108241818452283),.UNSPECIFIED.)
GEOMETRIC_REPRESENTATION_ITEM()
RATIONAL_B_SPLINE_SURFACE(((0.990086238235257,0.987329216372183,0.987470879370256,
0.987470879370256,0.987470879370256),(0.990086238235257,0.987329216372183,
0.987470879370255,0.987470879370255,0.987470879370255)))
REPRESENTATION_ITEM('')
SURFACE()
);
#3395=(
BOUNDED_SURFACE()
B_SPLINE_SURFACE(1,2,((#152034,#152035,#152036),(#152037,#152038,#152039)),
 .UNSPECIFIED.,.F.,.F.,.F.)
B_SPLINE_SURFACE_WITH_KNOTS((2,2),(3,3),(0.,0.289807040992624),(0.625170525609407,
0.642682999576233),.UNSPECIFIED.)
GEOMETRIC_REPRESENTATION_ITEM()
RATIONAL_B_SPLINE_SURFACE(((0.990658108926708,0.99376097929992,0.999878046252915),
(0.990658108926708,0.99376097929992,0.999878046252915)))
REPRESENTATION_ITEM('')
SURFACE()
);
#3396=(
BOUNDED_SURFACE()
B_SPLINE_SURFACE(1,2,((#152041,#152042,#152043,#152044,#152045),(#152046,
#152047,#152048,#152049,#152050)),.UNSPECIFIED.,.F.,.F.,.F.)
B_SPLINE_SURFACE_WITH_KNOTS((2,2),(3,2,3),(0.,0.289940743989111),(0.0908085233856356,
0.107982157956012,0.108241818505293),.UNSPECIFIED.)
GEOMETRIC_REPRESENTATION_ITEM()
RATIONAL_B_SPLINE_SURFACE(((0.990086238235256,0.987329216372183,0.987470879370255,
0.987470879370255,0.987470879370255),(0.990086238235256,0.987329216372183,
0.987470879370255,0.987470879370255,0.987470879370255)))
REPRESENTATION_ITEM('')
SURFACE()
);
#3397=(
BOUNDED_SURFACE()
B_SPLINE_SURFACE(1,2,((#152054,#152055,#152056),(#152057,#152058,#152059)),
 .UNSPECIFIED.,.F.,.F.,.F.)
B_SPLINE_SURFACE_WITH_KNOTS((2,2),(3,3),(0.,0.289807040992625),(0.625170525609407,
0.642682999576235),.UNSPECIFIED.)
GEOMETRIC_REPRESENTATION_ITEM()
RATIONAL_B_SPLINE_SURFACE(((0.990658108926708,0.993760979299921,0.999878046252916),
(0.990658108926708,0.993760979299921,0.999878046252916)))
REPRESENTATION_ITEM('')
SURFACE()
);
#3398=(
BOUNDED_SURFACE()
B_SPLINE_SURFACE(1,2,((#152061,#152062,#152063,#152064,#152065),(#152066,
#152067,#152068,#152069,#152070)),.UNSPECIFIED.,.F.,.F.,.F.)
B_SPLINE_SURFACE_WITH_KNOTS((2,2),(3,2,3),(0.,0.28994074403715),(0.0908085233856358,
0.107982157956012,0.108241818553818),.UNSPECIFIED.)
GEOMETRIC_REPRESENTATION_ITEM()
RATIONAL_B_SPLINE_SURFACE(((0.990086238235256,0.987329216372183,0.987470879370255,
0.987470879370255,0.987470879370255),(0.990086238235256,0.987329216372183,
0.987470879370255,0.987470879370255,0.987470879370255)))
REPRESENTATION_ITEM('')
SURFACE()
);
#3399=(
BOUNDED_SURFACE()
B_SPLINE_SURFACE(1,2,((#152074,#152075,#152076),(#152077,#152078,#152079)),
 .UNSPECIFIED.,.F.,.F.,.F.)
B_SPLINE_SURFACE_WITH_KNOTS((2,2),(3,3),(0.,0.289807040993206),(0.625170525609407,
0.642682999576235),.UNSPECIFIED.)
GEOMETRIC_REPRESENTATION_ITEM()
RATIONAL_B_SPLINE_SURFACE(((0.990658108926708,0.993760979299921,0.999878046252916),
(0.990658108926708,0.993760979299921,0.999878046252916)))
REPRESENTATION_ITEM('')
SURFACE()
);
#3400=(
BOUNDED_SURFACE()
B_SPLINE_SURFACE(1,2,((#152081,#152082,#152083,#152084,#152085),(#152086,
#152087,#152088,#152089,#152090)),.UNSPECIFIED.,.F.,.F.,.F.)
B_SPLINE_SURFACE_WITH_KNOTS((2,2),(3,2,3),(0.,0.289940743903119),(0.0908085233856344,
0.107982157956012,0.108241818465865),.UNSPECIFIED.)
GEOMETRIC_REPRESENTATION_ITEM()
RATIONAL_B_SPLINE_SURFACE(((0.990086238235257,0.987329216372183,0.987470879370255,
0.987470879370255,0.987470879370255),(0.990086238235257,0.987329216372183,
0.987470879370255,0.987470879370255,0.987470879370255)))
REPRESENTATION_ITEM('')
SURFACE()
);
#3401=(
BOUNDED_SURFACE()
B_SPLINE_SURFACE(1,2,((#152094,#152095,#152096),(#152097,#152098,#152099)),
 .UNSPECIFIED.,.F.,.F.,.F.)
B_SPLINE_SURFACE_WITH_KNOTS((2,2),(3,3),(0.,0.289807040992615),(0.625170525609407,
0.642682999576234),.UNSPECIFIED.)
GEOMETRIC_REPRESENTATION_ITEM()
RATIONAL_B_SPLINE_SURFACE(((0.990658108926708,0.99376097929992,0.999878046252915),
(0.990658108926708,0.99376097929992,0.999878046252915)))
REPRESENTATION_ITEM('')
SURFACE()
);
#3402=(
BOUNDED_SURFACE()
B_SPLINE_SURFACE(1,2,((#152101,#152102,#152103,#152104,#152105),(#152106,
#152107,#152108,#152109,#152110)),.UNSPECIFIED.,.F.,.F.,.F.)
B_SPLINE_SURFACE_WITH_KNOTS((2,2),(3,2,3),(0.,0.289940743947236),(0.0908085233856345,
0.107982157956012,0.108241818509775),.UNSPECIFIED.)
GEOMETRIC_REPRESENTATION_ITEM()
RATIONAL_B_SPLINE_SURFACE(((0.990086238235257,0.987329216372183,0.987470879370255,
0.987470879370255,0.987470879370255),(0.990086238235257,0.987329216372183,
0.987470879370255,0.987470879370255,0.987470879370255)))
REPRESENTATION_ITEM('')
SURFACE()
);
#3403=(
BOUNDED_SURFACE()
B_SPLINE_SURFACE(1,2,((#152114,#152115,#152116),(#152117,#152118,#152119)),
 .UNSPECIFIED.,.F.,.F.,.F.)
B_SPLINE_SURFACE_WITH_KNOTS((2,2),(3,3),(0.,0.289807040993176),(0.625170525609407,
0.642682999576233),.UNSPECIFIED.)
GEOMETRIC_REPRESENTATION_ITEM()
RATIONAL_B_SPLINE_SURFACE(((0.990658108926708,0.99376097929992,0.999878046252915),
(0.990658108926708,0.99376097929992,0.999878046252915)))
REPRESENTATION_ITEM('')
SURFACE()
);
#3404=(
BOUNDED_SURFACE()
B_SPLINE_SURFACE(1,2,((#152121,#152122,#152123,#152124,#152125),(#152126,
#152127,#152128,#152129,#152130)),.UNSPECIFIED.,.F.,.F.,.F.)
B_SPLINE_SURFACE_WITH_KNOTS((2,2),(3,2,3),(0.,0.28994074392508),(0.0908085233856357,
0.107982157956012,0.10824181848765),.UNSPECIFIED.)
GEOMETRIC_REPRESENTATION_ITEM()
RATIONAL_B_SPLINE_SURFACE(((0.990086238235256,0.987329216372183,0.987470879370256,
0.987470879370256,0.987470879370256),(0.990086238235256,0.987329216372183,
0.987470879370256,0.987470879370256,0.987470879370256)))
REPRESENTATION_ITEM('')
SURFACE()
);
#3405=(
BOUNDED_SURFACE()
B_SPLINE_SURFACE(1,2,((#152134,#152135,#152136),(#152137,#152138,#152139)),
 .UNSPECIFIED.,.F.,.F.,.F.)
B_SPLINE_SURFACE_WITH_KNOTS((2,2),(3,3),(0.,0.289807040992982),(0.625170525609408,
0.642682999576235),.UNSPECIFIED.)
GEOMETRIC_REPRESENTATION_ITEM()
RATIONAL_B_SPLINE_SURFACE(((0.990658108926709,0.993760979299921,0.999878046252916),
(0.990658108926709,0.993760979299921,0.999878046252916)))
REPRESENTATION_ITEM('')
SURFACE()
);
#3406=(
BOUNDED_SURFACE()
B_SPLINE_SURFACE(1,2,((#152141,#152142,#152143,#152144,#152145),(#152146,
#152147,#152148,#152149,#152150)),.UNSPECIFIED.,.F.,.F.,.F.)
B_SPLINE_SURFACE_WITH_KNOTS((2,2),(3,2,3),(0.,0.289940743933188),(0.0908085233856345,
0.107982157956011,0.108241818495526),.UNSPECIFIED.)
GEOMETRIC_REPRESENTATION_ITEM()
RATIONAL_B_SPLINE_SURFACE(((0.990086238235257,0.987329216372183,0.987470879370255,
0.987470879370255,0.987470879370255),(0.990086238235257,0.987329216372183,
0.987470879370255,0.987470879370255,0.987470879370255)))
REPRESENTATION_ITEM('')
SURFACE()
);
#3407=(
BOUNDED_SURFACE()
B_SPLINE_SURFACE(1,2,((#152154,#152155,#152156),(#152157,#152158,#152159)),
 .UNSPECIFIED.,.F.,.F.,.F.)
B_SPLINE_SURFACE_WITH_KNOTS((2,2),(3,3),(0.,0.289807040993016),(0.625170525609408,
0.642682999576236),.UNSPECIFIED.)
GEOMETRIC_REPRESENTATION_ITEM()
RATIONAL_B_SPLINE_SURFACE(((0.990658108926709,0.993760979299921,0.999878046252916),
(0.990658108926709,0.993760979299921,0.999878046252916)))
REPRESENTATION_ITEM('')
SURFACE()
);
#3408=(
BOUNDED_SURFACE()
B_SPLINE_SURFACE(1,2,((#152161,#152162,#152163,#152164,#152165),(#152166,
#152167,#152168,#152169,#152170)),.UNSPECIFIED.,.F.,.F.,.F.)
B_SPLINE_SURFACE_WITH_KNOTS((2,2),(3,2,3),(0.,0.289940743982799),(0.0908085233856346,
0.107982157956011,0.108241818499096),.UNSPECIFIED.)
GEOMETRIC_REPRESENTATION_ITEM()
RATIONAL_B_SPLINE_SURFACE(((0.990086238235257,0.987329216372183,0.987470879370256,
0.987470879370256,0.987470879370256),(0.990086238235256,0.987329216372183,
0.987470879370255,0.987470879370255,0.987470879370255)))
REPRESENTATION_ITEM('')
SURFACE()
);
#3409=(
BOUNDED_SURFACE()
B_SPLINE_SURFACE(1,2,((#152174,#152175,#152176),(#152177,#152178,#152179)),
 .UNSPECIFIED.,.F.,.F.,.F.)
B_SPLINE_SURFACE_WITH_KNOTS((2,2),(3,3),(0.,0.289807040993292),(0.625170525609408,
0.642682999576236),.UNSPECIFIED.)
GEOMETRIC_REPRESENTATION_ITEM()
RATIONAL_B_SPLINE_SURFACE(((0.990658108926709,0.993760979299921,0.999878046252916),
(0.990658108926709,0.993760979299921,0.999878046252916)))
REPRESENTATION_ITEM('')
SURFACE()
);
#3410=(
BOUNDED_SURFACE()
B_SPLINE_SURFACE(1,2,((#152181,#152182,#152183,#152184,#152185),(#152186,
#152187,#152188,#152189,#152190)),.UNSPECIFIED.,.F.,.F.,.F.)
B_SPLINE_SURFACE_WITH_KNOTS((2,2),(3,2,3),(0.,0.289940743772721),(0.0908085233856349,
0.107982157956011,0.108241818334936),.UNSPECIFIED.)
GEOMETRIC_REPRESENTATION_ITEM()
RATIONAL_B_SPLINE_SURFACE(((0.990086238235256,0.987329216372183,0.987470879370256,
0.987470879370256,0.987470879370256),(0.990086238235256,0.987329216372183,
0.987470879370256,0.987470879370256,0.987470879370256)))
REPRESENTATION_ITEM('')
SURFACE()
);
#3411=(
BOUNDED_SURFACE()
B_SPLINE_SURFACE(1,2,((#152194,#152195,#152196),(#152197,#152198,#152199)),
 .UNSPECIFIED.,.F.,.F.,.F.)
B_SPLINE_SURFACE_WITH_KNOTS((2,2),(3,3),(0.,0.289807040992714),(0.625170525609408,
0.642682999576236),.UNSPECIFIED.)
GEOMETRIC_REPRESENTATION_ITEM()
RATIONAL_B_SPLINE_SURFACE(((0.990658108926709,0.993760979299922,0.999878046252917),
(0.990658108926709,0.993760979299922,0.999878046252917)))
REPRESENTATION_ITEM('')
SURFACE()
);
#3412=(
BOUNDED_SURFACE()
B_SPLINE_SURFACE(1,2,((#152201,#152202,#152203,#152204,#152205),(#152206,
#152207,#152208,#152209,#152210)),.UNSPECIFIED.,.F.,.F.,.F.)
B_SPLINE_SURFACE_WITH_KNOTS((2,2),(3,2,3),(0.,0.289940743946678),(0.0908085233856334,
0.107982157956011,0.108241818509224),.UNSPECIFIED.)
GEOMETRIC_REPRESENTATION_ITEM()
RATIONAL_B_SPLINE_SURFACE(((0.990086238235257,0.987329216372183,0.987470879370256,
0.987470879370256,0.987470879370256),(0.990086238235257,0.987329216372183,
0.987470879370255,0.987470879370255,0.987470879370255)))
REPRESENTATION_ITEM('')
SURFACE()
);
#3413=(
BOUNDED_SURFACE()
B_SPLINE_SURFACE(1,2,((#152214,#152215,#152216),(#152217,#152218,#152219)),
 .UNSPECIFIED.,.F.,.F.,.F.)
B_SPLINE_SURFACE_WITH_KNOTS((2,2),(3,3),(0.,0.289807040993543),(0.625170525609408,
0.642682999576235),.UNSPECIFIED.)
GEOMETRIC_REPRESENTATION_ITEM()
RATIONAL_B_SPLINE_SURFACE(((0.990658108926709,0.993760979299921,0.999878046252916),
(0.990658108926709,0.993760979299921,0.999878046252916)))
REPRESENTATION_ITEM('')
SURFACE()
);
#3414=(
BOUNDED_SURFACE()
B_SPLINE_SURFACE(1,2,((#152221,#152222,#152223,#152224,#152225),(#152226,
#152227,#152228,#152229,#152230)),.UNSPECIFIED.,.F.,.F.,.F.)
B_SPLINE_SURFACE_WITH_KNOTS((2,2),(3,2,3),(0.,0.289940744094116),(0.0908085233856345,
0.107982157956011,0.108241818911241),.UNSPECIFIED.)
GEOMETRIC_REPRESENTATION_ITEM()
RATIONAL_B_SPLINE_SURFACE(((0.990086238235257,0.987329216372183,0.987470879370255,
0.987470879370255,0.987470879370255),(0.990086238235257,0.987329216372183,
0.987470879370255,0.987470879370255,0.987470879370255)))
REPRESENTATION_ITEM('')
SURFACE()
);
#3415=(
BOUNDED_SURFACE()
B_SPLINE_SURFACE(1,2,((#152234,#152235,#152236),(#152237,#152238,#152239)),
 .UNSPECIFIED.,.F.,.F.,.F.)
B_SPLINE_SURFACE_WITH_KNOTS((2,2),(3,3),(0.,0.289807040993038),(0.625170525609408,
0.642682999576236),.UNSPECIFIED.)
GEOMETRIC_REPRESENTATION_ITEM()
RATIONAL_B_SPLINE_SURFACE(((0.990658108926709,0.993760979299921,0.999878046252916),
(0.990658108926709,0.993760979299921,0.999878046252916)))
REPRESENTATION_ITEM('')
SURFACE()
);
#3416=(
BOUNDED_SURFACE()
B_SPLINE_SURFACE(1,2,((#152241,#152242,#152243,#152244,#152245),(#152246,
#152247,#152248,#152249,#152250)),.UNSPECIFIED.,.F.,.F.,.F.)
B_SPLINE_SURFACE_WITH_KNOTS((2,2),(3,2,3),(0.,0.289940743912886),(0.0908085233856345,
0.107982157956011,0.108241818475653),.UNSPECIFIED.)
GEOMETRIC_REPRESENTATION_ITEM()
RATIONAL_B_SPLINE_SURFACE(((0.990086238235257,0.987329216372183,0.987470879370255,
0.987470879370255,0.987470879370255),(0.990086238235257,0.987329216372183,
0.987470879370255,0.987470879370255,0.987470879370255)))
REPRESENTATION_ITEM('')
SURFACE()
);
#3417=(
BOUNDED_SURFACE()
B_SPLINE_SURFACE(1,2,((#152254,#152255,#152256),(#152257,#152258,#152259)),
 .UNSPECIFIED.,.F.,.F.,.F.)
B_SPLINE_SURFACE_WITH_KNOTS((2,2),(3,3),(0.,0.289807040993515),(0.625170525609408,
0.642682999576236),.UNSPECIFIED.)
GEOMETRIC_REPRESENTATION_ITEM()
RATIONAL_B_SPLINE_SURFACE(((0.990658108926709,0.993760979299921,0.999878046252916),
(0.990658108926709,0.993760979299921,0.999878046252916)))
REPRESENTATION_ITEM('')
SURFACE()
);
#3418=(
BOUNDED_SURFACE()
B_SPLINE_SURFACE(1,2,((#152261,#152262,#152263,#152264,#152265),(#152266,
#152267,#152268,#152269,#152270)),.UNSPECIFIED.,.F.,.F.,.F.)
B_SPLINE_SURFACE_WITH_KNOTS((2,2),(3,2,3),(0.,0.289940743945347),(0.0908085233856346,
0.107982157956011,0.108241818507535),.UNSPECIFIED.)
GEOMETRIC_REPRESENTATION_ITEM()
RATIONAL_B_SPLINE_SURFACE(((0.990086238235257,0.987329216372183,0.987470879370255,
0.987470879370255,0.987470879370255),(0.990086238235257,0.987329216372183,
0.987470879370255,0.987470879370255,0.987470879370255)))
REPRESENTATION_ITEM('')
SURFACE()
);
#3419=(
BOUNDED_SURFACE()
B_SPLINE_SURFACE(1,2,((#152274,#152275,#152276),(#152277,#152278,#152279)),
 .UNSPECIFIED.,.F.,.F.,.F.)
B_SPLINE_SURFACE_WITH_KNOTS((2,2),(3,3),(0.,0.289807040993259),(0.625170525609408,
0.642682999576236),.UNSPECIFIED.)
GEOMETRIC_REPRESENTATION_ITEM()
RATIONAL_B_SPLINE_SURFACE(((0.990658108926709,0.993760979299922,0.999878046252917),
(0.990658108926709,0.993760979299921,0.999878046252917)))
REPRESENTATION_ITEM('')
SURFACE()
);
#3420=(
BOUNDED_SURFACE()
B_SPLINE_SURFACE(1,2,((#152281,#152282,#152283,#152284,#152285),(#152286,
#152287,#152288,#152289,#152290)),.UNSPECIFIED.,.F.,.F.,.F.)
B_SPLINE_SURFACE_WITH_KNOTS((2,2),(3,2,3),(0.,0.289940743920806),(0.0908085233856334,
0.107982157956011,0.108241818483558),.UNSPECIFIED.)
GEOMETRIC_REPRESENTATION_ITEM()
RATIONAL_B_SPLINE_SURFACE(((0.990086238235257,0.987329216372183,0.987470879370256,
0.987470879370256,0.987470879370256),(0.990086238235257,0.987329216372183,
0.987470879370256,0.987470879370256,0.987470879370256)))
REPRESENTATION_ITEM('')
SURFACE()
);
#3421=(
BOUNDED_SURFACE()
B_SPLINE_SURFACE(1,2,((#152294,#152295,#152296),(#152297,#152298,#152299)),
 .UNSPECIFIED.,.F.,.F.,.F.)
B_SPLINE_SURFACE_WITH_KNOTS((2,2),(3,3),(0.,0.289807040994425),(0.625170525609408,
0.642682999576235),.UNSPECIFIED.)
GEOMETRIC_REPRESENTATION_ITEM()
RATIONAL_B_SPLINE_SURFACE(((0.990658108926709,0.993760979299921,0.999878046252915),
(0.990658108926709,0.993760979299921,0.999878046252915)))
REPRESENTATION_ITEM('')
SURFACE()
);
#3422=(
BOUNDED_SURFACE()
B_SPLINE_SURFACE(1,2,((#152301,#152302,#152303,#152304,#152305),(#152306,
#152307,#152308,#152309,#152310)),.UNSPECIFIED.,.F.,.F.,.F.)
B_SPLINE_SURFACE_WITH_KNOTS((2,2),(3,2,3),(0.,0.289940743934633),(0.0908085233856309,
0.107982157956011,0.108241818497391),.UNSPECIFIED.)
GEOMETRIC_REPRESENTATION_ITEM()
RATIONAL_B_SPLINE_SURFACE(((0.990086238235258,0.987329216372183,0.987470879370255,
0.987470879370255,0.987470879370255),(0.990086238235258,0.987329216372183,
0.987470879370255,0.987470879370255,0.987470879370255)))
REPRESENTATION_ITEM('')
SURFACE()
);
#3423=(
BOUNDED_SURFACE()
B_SPLINE_SURFACE(1,2,((#152314,#152315,#152316),(#152317,#152318,#152319)),
 .UNSPECIFIED.,.F.,.F.,.F.)
B_SPLINE_SURFACE_WITH_KNOTS((2,2),(3,3),(0.,0.289807040992766),(0.625170525609408,
0.642682999576236),.UNSPECIFIED.)
GEOMETRIC_REPRESENTATION_ITEM()
RATIONAL_B_SPLINE_SURFACE(((0.990658108926709,0.993760979299921,0.999878046252916),
(0.990658108926709,0.993760979299921,0.999878046252916)))
REPRESENTATION_ITEM('')
SURFACE()
);
#3424=(
BOUNDED_SURFACE()
B_SPLINE_SURFACE(1,2,((#152321,#152322,#152323,#152324,#152325),(#152326,
#152327,#152328,#152329,#152330)),.UNSPECIFIED.,.F.,.F.,.F.)
B_SPLINE_SURFACE_WITH_KNOTS((2,2),(3,2,3),(0.,0.289940743936486),(0.0908085233856343,
0.107982157956011,0.108241818453102),.UNSPECIFIED.)
GEOMETRIC_REPRESENTATION_ITEM()
RATIONAL_B_SPLINE_SURFACE(((0.990086238235257,0.987329216372183,0.987470879370255,
0.987470879370255,0.987470879370255),(0.990086238235257,0.987329216372183,
0.987470879370255,0.987470879370255,0.987470879370255)))
REPRESENTATION_ITEM('')
SURFACE()
);
#3425=(
BOUNDED_SURFACE()
B_SPLINE_SURFACE(1,2,((#152334,#152335,#152336),(#152337,#152338,#152339)),
 .UNSPECIFIED.,.F.,.F.,.F.)
B_SPLINE_SURFACE_WITH_KNOTS((2,2),(3,3),(0.,0.289807040992644),(0.625170525609408,
0.642682999576236),.UNSPECIFIED.)
GEOMETRIC_REPRESENTATION_ITEM()
RATIONAL_B_SPLINE_SURFACE(((0.990658108926709,0.993760979299921,0.999878046252916),
(0.990658108926709,0.993760979299921,0.999878046252916)))
REPRESENTATION_ITEM('')
SURFACE()
);
#3426=(
BOUNDED_SURFACE()
B_SPLINE_SURFACE(1,2,((#152341,#152342,#152343,#152344,#152345),(#152346,
#152347,#152348,#152349,#152350)),.UNSPECIFIED.,.F.,.F.,.F.)
B_SPLINE_SURFACE_WITH_KNOTS((2,2),(3,2,3),(0.,0.289940743784212),(0.0908085233856346,
0.107982157956011,0.10824181860138),.UNSPECIFIED.)
GEOMETRIC_REPRESENTATION_ITEM()
RATIONAL_B_SPLINE_SURFACE(((0.990086238235256,0.987329216372183,0.987470879370255,
0.987470879370255,0.987470879370255),(0.990086238235256,0.987329216372183,
0.987470879370255,0.987470879370255,0.987470879370255)))
REPRESENTATION_ITEM('')
SURFACE()
);
#3427=(
BOUNDED_SURFACE()
B_SPLINE_SURFACE(1,2,((#152354,#152355,#152356),(#152357,#152358,#152359)),
 .UNSPECIFIED.,.F.,.F.,.F.)
B_SPLINE_SURFACE_WITH_KNOTS((2,2),(3,3),(0.,0.289807040993496),(0.625170525609408,
0.642682999576236),.UNSPECIFIED.)
GEOMETRIC_REPRESENTATION_ITEM()
RATIONAL_B_SPLINE_SURFACE(((0.990658108926709,0.993760979299921,0.999878046252916),
(0.990658108926709,0.993760979299921,0.999878046252916)))
REPRESENTATION_ITEM('')
SURFACE()
);
#3428=(
BOUNDED_SURFACE()
B_SPLINE_SURFACE(1,2,((#152361,#152362,#152363,#152364,#152365),(#152366,
#152367,#152368,#152369,#152370)),.UNSPECIFIED.,.F.,.F.,.F.)
B_SPLINE_SURFACE_WITH_KNOTS((2,2),(3,2,3),(0.,0.289940743940566),(0.0908085233856347,
0.107982157956012,0.108241818503291),.UNSPECIFIED.)
GEOMETRIC_REPRESENTATION_ITEM()
RATIONAL_B_SPLINE_SURFACE(((0.990086238235256,0.987329216372183,0.987470879370255,
0.987470879370255,0.987470879370255),(0.990086238235256,0.987329216372183,
0.987470879370255,0.987470879370255,0.987470879370255)))
REPRESENTATION_ITEM('')
SURFACE()
);
#3429=(
BOUNDED_SURFACE()
B_SPLINE_SURFACE(1,2,((#152374,#152375,#152376),(#152377,#152378,#152379)),
 .UNSPECIFIED.,.F.,.F.,.F.)
B_SPLINE_SURFACE_WITH_KNOTS((2,2),(3,3),(0.,0.289807040992018),(0.625170525609408,
0.642682999576236),.UNSPECIFIED.)
GEOMETRIC_REPRESENTATION_ITEM()
RATIONAL_B_SPLINE_SURFACE(((0.990658108926709,0.993760979299921,0.999878046252917),
(0.990658108926709,0.993760979299921,0.999878046252917)))
REPRESENTATION_ITEM('')
SURFACE()
);
#3430=(
BOUNDED_SURFACE()
B_SPLINE_SURFACE(1,2,((#152381,#152382,#152383,#152384,#152385),(#152386,
#152387,#152388,#152389,#152390)),.UNSPECIFIED.,.F.,.F.,.F.)
B_SPLINE_SURFACE_WITH_KNOTS((2,2),(3,2,3),(0.,0.289940743943495),(0.0908085233856345,
0.107982157956011,0.108241818506614),.UNSPECIFIED.)
GEOMETRIC_REPRESENTATION_ITEM()
RATIONAL_B_SPLINE_SURFACE(((0.990086238235257,0.987329216372183,0.987470879370256,
0.987470879370256,0.987470879370256),(0.990086238235257,0.987329216372183,
0.987470879370256,0.987470879370256,0.987470879370256)))
REPRESENTATION_ITEM('')
SURFACE()
);
#3431=(
BOUNDED_SURFACE()
B_SPLINE_SURFACE(1,2,((#152394,#152395,#152396),(#152397,#152398,#152399)),
 .UNSPECIFIED.,.F.,.F.,.F.)
B_SPLINE_SURFACE_WITH_KNOTS((2,2),(3,3),(0.,0.289807040992885),(0.625170525609408,
0.642682999576236),.UNSPECIFIED.)
GEOMETRIC_REPRESENTATION_ITEM()
RATIONAL_B_SPLINE_SURFACE(((0.990658108926709,0.993760979299921,0.999878046252916),
(0.990658108926709,0.993760979299921,0.999878046252916)))
REPRESENTATION_ITEM('')
SURFACE()
);
#3432=(
BOUNDED_SURFACE()
B_SPLINE_SURFACE(1,2,((#152401,#152402,#152403,#152404,#152405),(#152406,
#152407,#152408,#152409,#152410)),.UNSPECIFIED.,.F.,.F.,.F.)
B_SPLINE_SURFACE_WITH_KNOTS((2,2),(3,2,3),(0.,0.289940743905968),(0.0908085233856358,
0.107982157956011,0.108241818468637),.UNSPECIFIED.)
GEOMETRIC_REPRESENTATION_ITEM()
RATIONAL_B_SPLINE_SURFACE(((0.990086238235256,0.987329216372183,0.987470879370255,
0.987470879370255,0.987470879370255),(0.990086238235256,0.987329216372183,
0.987470879370255,0.987470879370255,0.987470879370255)))
REPRESENTATION_ITEM('')
SURFACE()
);
#3433=(
BOUNDED_SURFACE()
B_SPLINE_SURFACE(1,2,((#152414,#152415,#152416),(#152417,#152418,#152419)),
 .UNSPECIFIED.,.F.,.F.,.F.)
B_SPLINE_SURFACE_WITH_KNOTS((2,2),(3,3),(0.,0.289807040991562),(0.625170525609407,
0.642682999576235),.UNSPECIFIED.)
GEOMETRIC_REPRESENTATION_ITEM()
RATIONAL_B_SPLINE_SURFACE(((0.990658108926708,0.993760979299921,0.999878046252916),
(0.990658108926708,0.993760979299921,0.999878046252916)))
REPRESENTATION_ITEM('')
SURFACE()
);
#3434=(
BOUNDED_SURFACE()
B_SPLINE_SURFACE(1,2,((#152421,#152422,#152423,#152424,#152425),(#152426,
#152427,#152428,#152429,#152430)),.UNSPECIFIED.,.F.,.F.,.F.)
B_SPLINE_SURFACE_WITH_KNOTS((2,2),(3,2,3),(0.,0.289940743934749),(0.0908085233856343,
0.107982157956012,0.108241818497582),.UNSPECIFIED.)
GEOMETRIC_REPRESENTATION_ITEM()
RATIONAL_B_SPLINE_SURFACE(((0.990086238235257,0.987329216372183,0.987470879370256,
0.987470879370256,0.987470879370256),(0.990086238235257,0.987329216372183,
0.987470879370256,0.987470879370256,0.987470879370256)))
REPRESENTATION_ITEM('')
SURFACE()
);
#3435=(
BOUNDED_SURFACE()
B_SPLINE_SURFACE(1,2,((#152434,#152435,#152436),(#152437,#152438,#152439)),
 .UNSPECIFIED.,.F.,.F.,.F.)
B_SPLINE_SURFACE_WITH_KNOTS((2,2),(3,3),(0.,0.289807040991874),(0.625170525609407,
0.642682999576234),.UNSPECIFIED.)
GEOMETRIC_REPRESENTATION_ITEM()
RATIONAL_B_SPLINE_SURFACE(((0.990658108926708,0.993760979299921,0.999878046252915),
(0.990658108926708,0.993760979299921,0.999878046252915)))
REPRESENTATION_ITEM('')
SURFACE()
);
#3436=(
BOUNDED_SURFACE()
B_SPLINE_SURFACE(1,2,((#152441,#152442,#152443,#152444,#152445),(#152446,
#152447,#152448,#152449,#152450)),.UNSPECIFIED.,.F.,.F.,.F.)
B_SPLINE_SURFACE_WITH_KNOTS((2,2),(3,2,3),(0.,0.289940744047752),(0.0908085233856344,
0.107982157956012,0.10824181886488),.UNSPECIFIED.)
GEOMETRIC_REPRESENTATION_ITEM()
RATIONAL_B_SPLINE_SURFACE(((0.990086238235257,0.987329216372183,0.987470879370255,
0.987470879370255,0.987470879370255),(0.990086238235257,0.987329216372183,
0.987470879370255,0.987470879370255,0.987470879370255)))
REPRESENTATION_ITEM('')
SURFACE()
);
#3437=(
BOUNDED_SURFACE()
B_SPLINE_SURFACE(1,2,((#152454,#152455,#152456),(#152457,#152458,#152459)),
 .UNSPECIFIED.,.F.,.F.,.F.)
B_SPLINE_SURFACE_WITH_KNOTS((2,2),(3,3),(0.,0.289807040991878),(0.625170525609407,
0.642682999576233),.UNSPECIFIED.)
GEOMETRIC_REPRESENTATION_ITEM()
RATIONAL_B_SPLINE_SURFACE(((0.990658108926708,0.99376097929992,0.999878046252915),
(0.990658108926708,0.99376097929992,0.999878046252915)))
REPRESENTATION_ITEM('')
SURFACE()
);
#3438=(
BOUNDED_SURFACE()
B_SPLINE_SURFACE(1,2,((#152461,#152462,#152463,#152464,#152465),(#152466,
#152467,#152468,#152469,#152470)),.UNSPECIFIED.,.F.,.F.,.F.)
B_SPLINE_SURFACE_WITH_KNOTS((2,2),(3,2,3),(0.,0.28994074393988),(0.0908085233856346,
0.107982157956012,0.108241818456526),.UNSPECIFIED.)
GEOMETRIC_REPRESENTATION_ITEM()
RATIONAL_B_SPLINE_SURFACE(((0.990086238235256,0.987329216372183,0.987470879370255,
0.987470879370255,0.987470879370255),(0.990086238235256,0.987329216372183,
0.987470879370255,0.987470879370255,0.987470879370255)))
REPRESENTATION_ITEM('')
SURFACE()
);
#3439=(
BOUNDED_SURFACE()
B_SPLINE_SURFACE(1,2,((#152474,#152475,#152476),(#152477,#152478,#152479)),
 .UNSPECIFIED.,.F.,.F.,.F.)
B_SPLINE_SURFACE_WITH_KNOTS((2,2),(3,3),(0.,0.28980704099187),(0.625170525609407,
0.642682999576234),.UNSPECIFIED.)
GEOMETRIC_REPRESENTATION_ITEM()
RATIONAL_B_SPLINE_SURFACE(((0.990658108926708,0.993760979299921,0.999878046252915),
(0.990658108926708,0.993760979299921,0.999878046252915)))
REPRESENTATION_ITEM('')
SURFACE()
);
#3440=(
BOUNDED_SURFACE()
B_SPLINE_SURFACE(1,2,((#152481,#152482,#152483,#152484,#152485),(#152486,
#152487,#152488,#152489,#152490)),.UNSPECIFIED.,.F.,.F.,.F.)
B_SPLINE_SURFACE_WITH_KNOTS((2,2),(3,2,3),(0.,0.289940743950375),(0.0908085233856344,
0.107982157956012,0.108241818466931),.UNSPECIFIED.)
GEOMETRIC_REPRESENTATION_ITEM()
RATIONAL_B_SPLINE_SURFACE(((0.990086238235257,0.987329216372183,0.987470879370255,
0.987470879370255,0.987470879370255),(0.990086238235256,0.987329216372183,
0.987470879370255,0.987470879370255,0.987470879370255)))
REPRESENTATION_ITEM('')
SURFACE()
);
#3441=(
BOUNDED_SURFACE()
B_SPLINE_SURFACE(1,2,((#152494,#152495,#152496),(#152497,#152498,#152499)),
 .UNSPECIFIED.,.F.,.F.,.F.)
B_SPLINE_SURFACE_WITH_KNOTS((2,2),(3,3),(0.,0.289807040991884),(0.625170525609407,
0.642682999576233),.UNSPECIFIED.)
GEOMETRIC_REPRESENTATION_ITEM()
RATIONAL_B_SPLINE_SURFACE(((0.990658108926708,0.99376097929992,0.999878046252915),
(0.990658108926708,0.99376097929992,0.999878046252915)))
REPRESENTATION_ITEM('')
SURFACE()
);
#3442=(
BOUNDED_SURFACE()
B_SPLINE_SURFACE(1,2,((#152501,#152502,#152503,#152504,#152505),(#152506,
#152507,#152508,#152509,#152510)),.UNSPECIFIED.,.F.,.F.,.F.)
B_SPLINE_SURFACE_WITH_KNOTS((2,2),(3,2,3),(0.,0.289681084359931),(0.573550810617332,
0.590910950629594,0.591084552029717),.UNSPECIFIED.)
GEOMETRIC_REPRESENTATION_ITEM()
RATIONAL_B_SPLINE_SURFACE(((0.998554414400274,0.992822941359345,0.990053454406147,
0.990053454406147,0.990053454406147),(0.998554414400274,0.992822941359345,
0.990053454406148,0.990053454406148,0.990053454406148)))
REPRESENTATION_ITEM('')
SURFACE()
);
#3443=(
BOUNDED_SURFACE()
B_SPLINE_SURFACE(1,2,((#152521,#152522,#152523,#152524,#152525,#152526,
#152527),(#152528,#152529,#152530,#152531,#152532,#152533,#152534)),
 .UNSPECIFIED.,.F.,.F.,.F.)
B_SPLINE_SURFACE_WITH_KNOTS((2,2),(3,2,2,3),(0.,0.289807040991565),(0.142404283483303,
0.142578551421364,0.142857142857143,0.160005345227479),.UNSPECIFIED.)
GEOMETRIC_REPRESENTATION_ITEM()
RATIONAL_B_SPLINE_SURFACE(((0.999805186472059,0.999805186472059,0.999805186472059,
0.999902211834795,1.,0.993980822699459,0.990851751371591),(0.999805186472059,
0.999805186472059,0.999805186472059,0.999902211834795,1.,0.993980822699459,
0.990851751371591)))
REPRESENTATION_ITEM('')
SURFACE()
);
#3444=(
BOUNDED_SURFACE()
B_SPLINE_SURFACE(1,2,((#152551,#152552,#152553,#152554,#152555),(#152556,
#152557,#152558,#152559,#152560)),.UNSPECIFIED.,.F.,.F.,.F.)
B_SPLINE_SURFACE_WITH_KNOTS((2,2),(3,2,3),(0.,0.289681084359923),(0.573550810617263,
0.590910950629593,0.591084552029716),.UNSPECIFIED.)
GEOMETRIC_REPRESENTATION_ITEM()
RATIONAL_B_SPLINE_SURFACE(((0.99855441440032,0.992822941359356,0.990053454406147,
0.990053454406147,0.990053454406147),(0.99855441440032,0.992822941359356,
0.990053454406147,0.990053454406147,0.990053454406147)))
REPRESENTATION_ITEM('')
SURFACE()
);
#3445=(
BOUNDED_SURFACE()
B_SPLINE_SURFACE(1,2,((#152562,#152563,#152564,#152565,#152566,#152567,
#152568),(#152569,#152570,#152571,#152572,#152573,#152574,#152575)),
 .UNSPECIFIED.,.F.,.F.,.F.)
B_SPLINE_SURFACE_WITH_KNOTS((2,2),(3,2,2,3),(0.,0.289807040991559),(0.142404283483179,
0.142578551421241,0.142857142857143,0.16000534522748),.UNSPECIFIED.)
GEOMETRIC_REPRESENTATION_ITEM()
RATIONAL_B_SPLINE_SURFACE(((0.999805186471973,0.999805186471973,0.999805186471973,
0.999902211834752,1.,0.993980822699459,0.990851751371591),(0.999805186471973,
0.999805186471973,0.999805186471973,0.999902211834752,1.,0.993980822699459,
0.990851751371591)))
REPRESENTATION_ITEM('')
SURFACE()
);
#3446=(
BOUNDED_SURFACE()
B_SPLINE_SURFACE(1,2,((#152592,#152593,#152594,#152595,#152596),(#152597,
#152598,#152599,#152600,#152601)),.UNSPECIFIED.,.F.,.F.,.F.)
B_SPLINE_SURFACE_WITH_KNOTS((2,2),(3,2,3),(0.,0.289681084359933),(0.573550810617452,
0.590910950629594,0.591084552029715),.UNSPECIFIED.)
GEOMETRIC_REPRESENTATION_ITEM()
RATIONAL_B_SPLINE_SURFACE(((0.998554414400195,0.992822941359326,0.990053454406148,
0.990053454406148,0.990053454406148),(0.998554414400195,0.992822941359326,
0.990053454406148,0.990053454406148,0.990053454406148)))
REPRESENTATION_ITEM('')
SURFACE()
);
#3447=(
BOUNDED_SURFACE()
B_SPLINE_SURFACE(1,2,((#152603,#152604,#152605,#152606,#152607,#152608,
#152609),(#152610,#152611,#152612,#152613,#152614,#152615,#152616)),
 .UNSPECIFIED.,.F.,.F.,.F.)
B_SPLINE_SURFACE_WITH_KNOTS((2,2),(3,2,2,3),(0.,0.289807040991559),(0.142404283483291,
0.142578551421352,0.142857142857143,0.160005345227478),.UNSPECIFIED.)
GEOMETRIC_REPRESENTATION_ITEM()
RATIONAL_B_SPLINE_SURFACE(((0.99980518647205,0.99980518647205,0.99980518647205,
0.99990221183479,1.,0.993980822699459,0.990851751371592),(0.99980518647205,
0.99980518647205,0.99980518647205,0.99990221183479,1.,0.993980822699459,
0.990851751371592)))
REPRESENTATION_ITEM('')
SURFACE()
);
#3448=(
BOUNDED_SURFACE()
B_SPLINE_SURFACE(1,2,((#152633,#152634,#152635,#152636,#152637),(#152638,
#152639,#152640,#152641,#152642)),.UNSPECIFIED.,.F.,.F.,.F.)
B_SPLINE_SURFACE_WITH_KNOTS((2,2),(3,2,3),(0.,0.289681084359915),(0.573550810617204,
0.590910950629595,0.591084552029719),.UNSPECIFIED.)
GEOMETRIC_REPRESENTATION_ITEM()
RATIONAL_B_SPLINE_SURFACE(((0.998554414400359,0.992822941359365,0.990053454406147,
0.990053454406147,0.990053454406147),(0.998554414400359,0.992822941359365,
0.990053454406147,0.990053454406147,0.990053454406147)))
REPRESENTATION_ITEM('')
SURFACE()
);
#3449=(
BOUNDED_SURFACE()
B_SPLINE_SURFACE(1,2,((#152644,#152645,#152646,#152647,#152648,#152649,
#152650),(#152651,#152652,#152653,#152654,#152655,#152656,#152657)),
 .UNSPECIFIED.,.F.,.F.,.F.)
B_SPLINE_SURFACE_WITH_KNOTS((2,2),(3,2,2,3),(0.,0.289807040991563),(0.142404283483062,
0.142578551421126,0.142857142857143,0.160005345227473),.UNSPECIFIED.)
GEOMETRIC_REPRESENTATION_ITEM()
RATIONAL_B_SPLINE_SURFACE(((0.999805186471894,0.999805186471894,0.999805186471894,
0.999902211834711,1.,0.993980822699461,0.990851751371593),(0.999805186471894,
0.999805186471894,0.999805186471894,0.999902211834711,1.,0.993980822699461,
0.990851751371593)))
REPRESENTATION_ITEM('')
SURFACE()
);
#3450=(
BOUNDED_SURFACE()
B_SPLINE_SURFACE(1,2,((#152674,#152675,#152676,#152677,#152678),(#152679,
#152680,#152681,#152682,#152683)),.UNSPECIFIED.,.F.,.F.,.F.)
B_SPLINE_SURFACE_WITH_KNOTS((2,2),(3,2,3),(0.,0.289681084359931),(0.573550810617335,
0.590910950629595,0.591084552029718),.UNSPECIFIED.)
GEOMETRIC_REPRESENTATION_ITEM()
RATIONAL_B_SPLINE_SURFACE(((0.998554414400272,0.992822941359344,0.990053454406147,
0.990053454406147,0.990053454406147),(0.998554414400272,0.992822941359344,
0.990053454406147,0.990053454406147,0.990053454406147)))
REPRESENTATION_ITEM('')
SURFACE()
);
#3451=(
BOUNDED_SURFACE()
B_SPLINE_SURFACE(1,2,((#152685,#152686,#152687,#152688,#152689,#152690,
#152691),(#152692,#152693,#152694,#152695,#152696,#152697,#152698)),
 .UNSPECIFIED.,.F.,.F.,.F.)
B_SPLINE_SURFACE_WITH_KNOTS((2,2),(3,2,2,3),(0.,0.289807040991561),(0.142404283483294,
0.142578551421355,0.142857142857143,0.160005345227478),.UNSPECIFIED.)
GEOMETRIC_REPRESENTATION_ITEM()
RATIONAL_B_SPLINE_SURFACE(((0.999805186472053,0.999805186472053,0.999805186472053,
0.999902211834792,1.,0.993980822699459,0.990851751371591),(0.999805186472053,
0.999805186472053,0.999805186472053,0.999902211834792,1.,0.993980822699459,
0.990851751371591)))
REPRESENTATION_ITEM('')
SURFACE()
);
#3452=(
BOUNDED_SURFACE()
B_SPLINE_SURFACE(1,2,((#152715,#152716,#152717,#152718,#152719),(#152720,
#152721,#152722,#152723,#152724)),.UNSPECIFIED.,.F.,.F.,.F.)
B_SPLINE_SURFACE_WITH_KNOTS((2,2),(3,2,3),(0.,0.289681084359922),(0.573550810617453,
0.590910950629595,0.591084552029716),.UNSPECIFIED.)
GEOMETRIC_REPRESENTATION_ITEM()
RATIONAL_B_SPLINE_SURFACE(((0.998554414400194,0.992822941359325,0.990053454406147,
0.990053454406147,0.990053454406147),(0.998554414400194,0.992822941359325,
0.990053454406147,0.990053454406147,0.990053454406147)))
REPRESENTATION_ITEM('')
SURFACE()
);
#3453=(
BOUNDED_SURFACE()
B_SPLINE_SURFACE(1,2,((#152726,#152727,#152728,#152729,#152730,#152731,
#152732),(#152733,#152734,#152735,#152736,#152737,#152738,#152739)),
 .UNSPECIFIED.,.F.,.F.,.F.)
B_SPLINE_SURFACE_WITH_KNOTS((2,2),(3,2,2,3),(0.,0.28980704099156),(0.142404283482878,
0.142578551420943,0.142857142857143,0.160005345227481),.UNSPECIFIED.)
GEOMETRIC_REPRESENTATION_ITEM()
RATIONAL_B_SPLINE_SURFACE(((0.999805186471766,0.999805186471766,0.999805186471766,
0.999902211834647,1.,0.993980822699458,0.99085175137159),(0.999805186471766,
0.999805186471766,0.999805186471766,0.999902211834647,1.,0.993980822699458,
0.99085175137159)))
REPRESENTATION_ITEM('')
SURFACE()
);
#3454=(
BOUNDED_SURFACE()
B_SPLINE_SURFACE(1,2,((#152756,#152757,#152758,#152759,#152760),(#152761,
#152762,#152763,#152764,#152765)),.UNSPECIFIED.,.F.,.F.,.F.)
B_SPLINE_SURFACE_WITH_KNOTS((2,2),(3,2,3),(0.,0.289681084359927),(0.573550810617453,
0.590910950629595,0.591084552029716),.UNSPECIFIED.)
GEOMETRIC_REPRESENTATION_ITEM()
RATIONAL_B_SPLINE_SURFACE(((0.998554414400194,0.992822941359325,0.990053454406147,
0.990053454406147,0.990053454406147),(0.998554414400194,0.992822941359325,
0.990053454406147,0.990053454406147,0.990053454406147)))
REPRESENTATION_ITEM('')
SURFACE()
);
#3455=(
BOUNDED_SURFACE()
B_SPLINE_SURFACE(1,2,((#152767,#152768,#152769,#152770,#152771,#152772,
#152773),(#152774,#152775,#152776,#152777,#152778,#152779,#152780)),
 .UNSPECIFIED.,.F.,.F.,.F.)
B_SPLINE_SURFACE_WITH_KNOTS((2,2),(3,2,2,3),(0.,0.289807040991564),(0.142404283483302,
0.142578551421363,0.142857142857143,0.160005345227478),.UNSPECIFIED.)
GEOMETRIC_REPRESENTATION_ITEM()
RATIONAL_B_SPLINE_SURFACE(((0.999805186472059,0.999805186472059,0.999805186472059,
0.999902211834794,1.,0.993980822699459,0.990851751371591),(0.999805186472059,
0.999805186472059,0.999805186472059,0.999902211834794,1.,0.993980822699459,
0.990851751371591)))
REPRESENTATION_ITEM('')
SURFACE()
);
#3456=(
BOUNDED_SURFACE()
B_SPLINE_SURFACE(1,2,((#152788,#152789,#152790,#152791,#152792),(#152793,
#152794,#152795,#152796,#152797)),.UNSPECIFIED.,.F.,.F.,.F.)
B_SPLINE_SURFACE_WITH_KNOTS((2,2),(3,2,3),(0.,0.289681084359926),(0.573550810617453,
0.590910950629595,0.591084552029716),.UNSPECIFIED.)
GEOMETRIC_REPRESENTATION_ITEM()
RATIONAL_B_SPLINE_SURFACE(((0.998554414400194,0.992822941359325,0.990053454406147,
0.990053454406147,0.990053454406147),(0.998554414400194,0.992822941359325,
0.990053454406147,0.990053454406147,0.990053454406147)))
REPRESENTATION_ITEM('')
SURFACE()
);
#3457=(
BOUNDED_SURFACE()
B_SPLINE_SURFACE(1,2,((#152799,#152800,#152801,#152802,#152803,#152804,
#152805),(#152806,#152807,#152808,#152809,#152810,#152811,#152812)),
 .UNSPECIFIED.,.F.,.F.,.F.)
B_SPLINE_SURFACE_WITH_KNOTS((2,2),(3,2,2,3),(0.,0.289807040991561),(0.142404283483292,
0.142578551421353,0.142857142857143,0.160005345227478),.UNSPECIFIED.)
GEOMETRIC_REPRESENTATION_ITEM()
RATIONAL_B_SPLINE_SURFACE(((0.999805186472051,0.999805186472051,0.999805186472051,
0.999902211834791,1.,0.993980822699459,0.990851751371592),(0.999805186472051,
0.999805186472051,0.999805186472051,0.999902211834791,1.,0.993980822699459,
0.990851751371592)))
REPRESENTATION_ITEM('')
SURFACE()
);
#3458=(
BOUNDED_SURFACE()
B_SPLINE_SURFACE(1,2,((#152829,#152830,#152831,#152832,#152833),(#152834,
#152835,#152836,#152837,#152838)),.UNSPECIFIED.,.F.,.F.,.F.)
B_SPLINE_SURFACE_WITH_KNOTS((2,2),(3,2,3),(0.,0.289681084359916),(0.573550810617453,
0.590910950629595,0.591084552029716),.UNSPECIFIED.)
GEOMETRIC_REPRESENTATION_ITEM()
RATIONAL_B_SPLINE_SURFACE(((0.998554414400194,0.992822941359325,0.990053454406147,
0.990053454406147,0.990053454406147),(0.998554414400194,0.992822941359325,
0.990053454406147,0.990053454406147,0.990053454406147)))
REPRESENTATION_ITEM('')
SURFACE()
);
#3459=(
BOUNDED_SURFACE()
B_SPLINE_SURFACE(1,2,((#152840,#152841,#152842,#152843,#152844,#152845,
#152846),(#152847,#152848,#152849,#152850,#152851,#152852,#152853)),
 .UNSPECIFIED.,.F.,.F.,.F.)
B_SPLINE_SURFACE_WITH_KNOTS((2,2),(3,2,2,3),(0.,0.289807040991557),(0.142404283483302,
0.142578551421363,0.142857142857143,0.160005345227478),.UNSPECIFIED.)
GEOMETRIC_REPRESENTATION_ITEM()
RATIONAL_B_SPLINE_SURFACE(((0.999805186472059,0.999805186472059,0.999805186472059,
0.999902211834794,1.,0.993980822699459,0.990851751371592),(0.999805186472059,
0.999805186472059,0.999805186472059,0.999902211834794,1.,0.993980822699459,
0.990851751371592)))
REPRESENTATION_ITEM('')
SURFACE()
);
#3460=(
BOUNDED_SURFACE()
B_SPLINE_SURFACE(1,2,((#152870,#152871,#152872,#152873,#152874),(#152875,
#152876,#152877,#152878,#152879)),.UNSPECIFIED.,.F.,.F.,.F.)
B_SPLINE_SURFACE_WITH_KNOTS((2,2),(3,2,3),(0.,0.289681084359915),(0.573550810617453,
0.590910950629595,0.591084552029716),.UNSPECIFIED.)
GEOMETRIC_REPRESENTATION_ITEM()
RATIONAL_B_SPLINE_SURFACE(((0.998554414400194,0.992822941359325,0.990053454406147,
0.990053454406147,0.990053454406147),(0.998554414400194,0.992822941359325,
0.990053454406147,0.990053454406147,0.990053454406147)))
REPRESENTATION_ITEM('')
SURFACE()
);
#3461=(
BOUNDED_SURFACE()
B_SPLINE_SURFACE(1,2,((#152881,#152882,#152883,#152884,#152885,#152886,
#152887),(#152888,#152889,#152890,#152891,#152892,#152893,#152894)),
 .UNSPECIFIED.,.F.,.F.,.F.)
B_SPLINE_SURFACE_WITH_KNOTS((2,2),(3,2,2,3),(0.,0.289807040991559),(0.142404283482981,
0.142578551421045,0.142857142857143,0.16000534522748),.UNSPECIFIED.)
GEOMETRIC_REPRESENTATION_ITEM()
RATIONAL_B_SPLINE_SURFACE(((0.999805186471836,0.999805186471836,0.999805186471836,
0.999902211834683,1.,0.993980822699459,0.990851751371591),(0.999805186471836,
0.999805186471836,0.999805186471836,0.999902211834683,1.,0.993980822699459,
0.990851751371591)))
REPRESENTATION_ITEM('')
SURFACE()
);
#3462=(
BOUNDED_SURFACE()
B_SPLINE_SURFACE(1,2,((#152911,#152912,#152913,#152914,#152915),(#152916,
#152917,#152918,#152919,#152920)),.UNSPECIFIED.,.F.,.F.,.F.)
B_SPLINE_SURFACE_WITH_KNOTS((2,2),(3,2,3),(0.,0.289681084359914),(0.573550810617378,
0.590910950629595,0.591084552029717),.UNSPECIFIED.)
GEOMETRIC_REPRESENTATION_ITEM()
RATIONAL_B_SPLINE_SURFACE(((0.998554414400244,0.992822941359337,0.990053454406147,
0.990053454406147,0.990053454406147),(0.998554414400244,0.992822941359337,
0.990053454406147,0.990053454406147,0.990053454406147)))
REPRESENTATION_ITEM('')
SURFACE()
);
#3463=(
BOUNDED_SURFACE()
B_SPLINE_SURFACE(1,2,((#152922,#152923,#152924,#152925,#152926,#152927,
#152928),(#152929,#152930,#152931,#152932,#152933,#152934,#152935)),
 .UNSPECIFIED.,.F.,.F.,.F.)
B_SPLINE_SURFACE_WITH_KNOTS((2,2),(3,2,2,3),(0.,0.289807040991562),(0.142404283483302,
0.142578551421363,0.142857142857143,0.160005345227478),.UNSPECIFIED.)
GEOMETRIC_REPRESENTATION_ITEM()
RATIONAL_B_SPLINE_SURFACE(((0.999805186472058,0.999805186472058,0.999805186472058,
0.999902211834794,1.,0.993980822699459,0.990851751371592),(0.999805186472058,
0.999805186472058,0.999805186472058,0.999902211834794,1.,0.993980822699459,
0.990851751371592)))
REPRESENTATION_ITEM('')
SURFACE()
);
#3464=(
BOUNDED_SURFACE()
B_SPLINE_SURFACE(1,2,((#152952,#152953,#152954,#152955,#152956),(#152957,
#152958,#152959,#152960,#152961)),.UNSPECIFIED.,.F.,.F.,.F.)
B_SPLINE_SURFACE_WITH_KNOTS((2,2),(3,2,3),(0.,0.289681084359919),(0.573550810617453,
0.590910950629595,0.591084552029716),.UNSPECIFIED.)
GEOMETRIC_REPRESENTATION_ITEM()
RATIONAL_B_SPLINE_SURFACE(((0.998554414400194,0.992822941359325,0.990053454406147,
0.990053454406147,0.990053454406147),(0.998554414400194,0.992822941359325,
0.990053454406147,0.990053454406147,0.990053454406147)))
REPRESENTATION_ITEM('')
SURFACE()
);
#3465=(
BOUNDED_SURFACE()
B_SPLINE_SURFACE(1,2,((#152963,#152964,#152965,#152966,#152967,#152968,
#152969),(#152970,#152971,#152972,#152973,#152974,#152975,#152976)),
 .UNSPECIFIED.,.F.,.F.,.F.)
B_SPLINE_SURFACE_WITH_KNOTS((2,2),(3,2,2,3),(0.,0.289807040991563),(0.142404283483231,
0.142578551421293,0.142857142857143,0.160005345227479),.UNSPECIFIED.)
GEOMETRIC_REPRESENTATION_ITEM()
RATIONAL_B_SPLINE_SURFACE(((0.999805186472009,0.999805186472009,0.999805186472009,
0.99990221183477,1.,0.993980822699459,0.990851751371591),(0.999805186472009,
0.999805186472009,0.999805186472009,0.99990221183477,1.,0.993980822699459,
0.990851751371591)))
REPRESENTATION_ITEM('')
SURFACE()
);
#3466=(
BOUNDED_SURFACE()
B_SPLINE_SURFACE(1,2,((#152993,#152994,#152995,#152996,#152997),(#152998,
#152999,#153000,#153001,#153002)),.UNSPECIFIED.,.F.,.F.,.F.)
B_SPLINE_SURFACE_WITH_KNOTS((2,2),(3,2,3),(0.,0.28968108435992),(0.573550810617453,
0.590910950629595,0.591084552029716),.UNSPECIFIED.)
GEOMETRIC_REPRESENTATION_ITEM()
RATIONAL_B_SPLINE_SURFACE(((0.998554414400194,0.992822941359325,0.990053454406147,
0.990053454406147,0.990053454406147),(0.998554414400194,0.992822941359325,
0.990053454406147,0.990053454406147,0.990053454406147)))
REPRESENTATION_ITEM('')
SURFACE()
);
#3467=(
BOUNDED_SURFACE()
B_SPLINE_SURFACE(1,2,((#153004,#153005,#153006,#153007,#153008,#153009,
#153010),(#153011,#153012,#153013,#153014,#153015,#153016,#153017)),
 .UNSPECIFIED.,.F.,.F.,.F.)
B_SPLINE_SURFACE_WITH_KNOTS((2,2),(3,2,2,3),(0.,0.28980704099156),(0.142404283483302,
0.142578551421363,0.142857142857143,0.160005345227478),.UNSPECIFIED.)
GEOMETRIC_REPRESENTATION_ITEM()
RATIONAL_B_SPLINE_SURFACE(((0.999805186472059,0.999805186472059,0.999805186472059,
0.999902211834794,1.,0.993980822699459,0.990851751371591),(0.999805186472059,
0.999805186472059,0.999805186472059,0.999902211834794,1.,0.993980822699459,
0.990851751371591)))
REPRESENTATION_ITEM('')
SURFACE()
);
#3468=(
BOUNDED_SURFACE()
B_SPLINE_SURFACE(1,2,((#153034,#153035,#153036,#153037,#153038),(#153039,
#153040,#153041,#153042,#153043)),.UNSPECIFIED.,.F.,.F.,.F.)
B_SPLINE_SURFACE_WITH_KNOTS((2,2),(3,2,3),(0.,0.28968108435992),(0.573550810617453,
0.590910950629595,0.591084552029716),.UNSPECIFIED.)
GEOMETRIC_REPRESENTATION_ITEM()
RATIONAL_B_SPLINE_SURFACE(((0.998554414400194,0.992822941359325,0.990053454406147,
0.990053454406147,0.990053454406147),(0.998554414400194,0.992822941359325,
0.990053454406147,0.990053454406147,0.990053454406147)))
REPRESENTATION_ITEM('')
SURFACE()
);
#3469=(
BOUNDED_SURFACE()
B_SPLINE_SURFACE(1,2,((#153045,#153046,#153047,#153048,#153049,#153050,
#153051),(#153052,#153053,#153054,#153055,#153056,#153057,#153058)),
 .UNSPECIFIED.,.F.,.F.,.F.)
B_SPLINE_SURFACE_WITH_KNOTS((2,2),(3,2,2,3),(0.,0.289807040991565),(0.142404283483023,
0.142578551421087,0.142857142857143,0.16000534522748),.UNSPECIFIED.)
GEOMETRIC_REPRESENTATION_ITEM()
RATIONAL_B_SPLINE_SURFACE(((0.999805186471866,0.999805186471866,0.999805186471866,
0.999902211834697,1.,0.993980822699459,0.990851751371591),(0.999805186471866,
0.999805186471866,0.999805186471866,0.999902211834697,1.,0.993980822699459,
0.990851751371591)))
REPRESENTATION_ITEM('')
SURFACE()
);
#3470=(
BOUNDED_SURFACE()
B_SPLINE_SURFACE(1,2,((#153075,#153076,#153077,#153078,#153079),(#153080,
#153081,#153082,#153083,#153084)),.UNSPECIFIED.,.F.,.F.,.F.)
B_SPLINE_SURFACE_WITH_KNOTS((2,2),(3,2,3),(0.,0.289681084359922),(0.573550810617453,
0.590910950629595,0.591084552029716),.UNSPECIFIED.)
GEOMETRIC_REPRESENTATION_ITEM()
RATIONAL_B_SPLINE_SURFACE(((0.998554414400194,0.992822941359325,0.990053454406147,
0.990053454406147,0.990053454406147),(0.998554414400194,0.992822941359325,
0.990053454406147,0.990053454406147,0.990053454406147)))
REPRESENTATION_ITEM('')
SURFACE()
);
#3471=(
BOUNDED_SURFACE()
B_SPLINE_SURFACE(1,2,((#153086,#153087,#153088,#153089,#153090,#153091,
#153092),(#153093,#153094,#153095,#153096,#153097,#153098,#153099)),
 .UNSPECIFIED.,.F.,.F.,.F.)
B_SPLINE_SURFACE_WITH_KNOTS((2,2),(3,2,2,3),(0.,0.289807040991562),(0.142404283483302,
0.142578551421363,0.142857142857143,0.160005345227478),.UNSPECIFIED.)
GEOMETRIC_REPRESENTATION_ITEM()
RATIONAL_B_SPLINE_SURFACE(((0.999805186472058,0.999805186472058,0.999805186472058,
0.999902211834794,1.,0.993980822699459,0.990851751371591),(0.999805186472058,
0.999805186472058,0.999805186472058,0.999902211834794,1.,0.993980822699459,
0.990851751371591)))
REPRESENTATION_ITEM('')
SURFACE()
);
#3472=(
BOUNDED_SURFACE()
B_SPLINE_SURFACE(1,2,((#153116,#153117,#153118,#153119,#153120),(#153121,
#153122,#153123,#153124,#153125)),.UNSPECIFIED.,.F.,.F.,.F.)
B_SPLINE_SURFACE_WITH_KNOTS((2,2),(3,2,3),(0.,0.289681084359919),(0.573550810617453,
0.590910950629595,0.591084552029716),.UNSPECIFIED.)
GEOMETRIC_REPRESENTATION_ITEM()
RATIONAL_B_SPLINE_SURFACE(((0.998554414400194,0.992822941359325,0.990053454406147,
0.990053454406147,0.990053454406147),(0.998554414400194,0.992822941359325,
0.990053454406147,0.990053454406147,0.990053454406147)))
REPRESENTATION_ITEM('')
SURFACE()
);
#3473=(
BOUNDED_SURFACE()
B_SPLINE_SURFACE(1,2,((#153127,#153128,#153129,#153130,#153131,#153132,
#153133),(#153134,#153135,#153136,#153137,#153138,#153139,#153140)),
 .UNSPECIFIED.,.F.,.F.,.F.)
B_SPLINE_SURFACE_WITH_KNOTS((2,2),(3,2,2,3),(0.,0.289807040991558),(0.142404283483302,
0.142578551421363,0.142857142857143,0.160005345227478),.UNSPECIFIED.)
GEOMETRIC_REPRESENTATION_ITEM()
RATIONAL_B_SPLINE_SURFACE(((0.999805186472058,0.999805186472058,0.999805186472058,
0.999902211834794,1.,0.993980822699459,0.990851751371591),(0.999805186472058,
0.999805186472058,0.999805186472058,0.999902211834794,1.,0.993980822699459,
0.990851751371591)))
REPRESENTATION_ITEM('')
SURFACE()
);
#3474=(
BOUNDED_SURFACE()
B_SPLINE_SURFACE(1,2,((#153157,#153158,#153159,#153160,#153161),(#153162,
#153163,#153164,#153165,#153166)),.UNSPECIFIED.,.F.,.F.,.F.)
B_SPLINE_SURFACE_WITH_KNOTS((2,2),(3,2,3),(0.,0.289681084359915),(0.573550810617453,
0.590910950629595,0.591084552029716),.UNSPECIFIED.)
GEOMETRIC_REPRESENTATION_ITEM()
RATIONAL_B_SPLINE_SURFACE(((0.998554414400194,0.992822941359325,0.990053454406147,
0.990053454406147,0.990053454406147),(0.998554414400194,0.992822941359325,
0.990053454406147,0.990053454406147,0.990053454406147)))
REPRESENTATION_ITEM('')
SURFACE()
);
#3475=(
BOUNDED_SURFACE()
B_SPLINE_SURFACE(1,2,((#153168,#153169,#153170,#153171,#153172,#153173,
#153174),(#153175,#153176,#153177,#153178,#153179,#153180,#153181)),
 .UNSPECIFIED.,.F.,.F.,.F.)
B_SPLINE_SURFACE_WITH_KNOTS((2,2),(3,2,2,3),(0.,0.289807040991559),(0.142404283483302,
0.142578551421363,0.142857142857143,0.160005345227478),.UNSPECIFIED.)
GEOMETRIC_REPRESENTATION_ITEM()
RATIONAL_B_SPLINE_SURFACE(((0.999805186472058,0.999805186472058,0.999805186472058,
0.999902211834794,1.,0.993980822699459,0.990851751371592),(0.999805186472058,
0.999805186472058,0.999805186472058,0.999902211834794,1.,0.993980822699459,
0.990851751371592)))
REPRESENTATION_ITEM('')
SURFACE()
);
#3476=(
BOUNDED_SURFACE()
B_SPLINE_SURFACE(1,2,((#153198,#153199,#153200,#153201,#153202),(#153203,
#153204,#153205,#153206,#153207)),.UNSPECIFIED.,.F.,.F.,.F.)
B_SPLINE_SURFACE_WITH_KNOTS((2,2),(3,2,3),(0.,0.289681084359918),(0.573550810617453,
0.590910950629595,0.591084552029716),.UNSPECIFIED.)
GEOMETRIC_REPRESENTATION_ITEM()
RATIONAL_B_SPLINE_SURFACE(((0.998554414400194,0.992822941359325,0.990053454406147,
0.990053454406147,0.990053454406147),(0.998554414400194,0.992822941359325,
0.990053454406147,0.990053454406147,0.990053454406147)))
REPRESENTATION_ITEM('')
SURFACE()
);
#3477=(
BOUNDED_SURFACE()
B_SPLINE_SURFACE(1,2,((#153209,#153210,#153211,#153212,#153213,#153214,
#153215),(#153216,#153217,#153218,#153219,#153220,#153221,#153222)),
 .UNSPECIFIED.,.F.,.F.,.F.)
B_SPLINE_SURFACE_WITH_KNOTS((2,2),(3,2,2,3),(0.,0.289807040991562),(0.142404283483302,
0.142578551421363,0.142857142857143,0.160005345227478),.UNSPECIFIED.)
GEOMETRIC_REPRESENTATION_ITEM()
RATIONAL_B_SPLINE_SURFACE(((0.999805186472059,0.999805186472059,0.999805186472059,
0.999902211834794,1.,0.993980822699459,0.990851751371591),(0.999805186472059,
0.999805186472059,0.999805186472059,0.999902211834794,1.,0.993980822699459,
0.990851751371591)))
REPRESENTATION_ITEM('')
SURFACE()
);
#3478=(
BOUNDED_SURFACE()
B_SPLINE_SURFACE(1,2,((#153233,#153234,#153235,#153236,#153237),(#153238,
#153239,#153240,#153241,#153242)),.UNSPECIFIED.,.F.,.F.,.F.)
B_SPLINE_SURFACE_WITH_KNOTS((2,2),(3,2,3),(0.,0.289681084360141),(0.573550810617453,
0.590910950629595,0.591084552029716),.UNSPECIFIED.)
GEOMETRIC_REPRESENTATION_ITEM()
RATIONAL_B_SPLINE_SURFACE(((0.998554414400194,0.992822941359325,0.990053454406147,
0.990053454406147,0.990053454406147),(0.998554414400194,0.992822941359325,
0.990053454406147,0.990053454406147,0.990053454406147)))
REPRESENTATION_ITEM('')
SURFACE()
);
#3479=(
BOUNDED_SURFACE()
B_SPLINE_SURFACE(1,2,((#153250,#153251,#153252,#153253,#153254,#153255,
#153256),(#153257,#153258,#153259,#153260,#153261,#153262,#153263)),
 .UNSPECIFIED.,.F.,.F.,.F.)
B_SPLINE_SURFACE_WITH_KNOTS((2,2),(3,2,2,3),(0.,0.289807040991562),(0.142404283483302,
0.142578551421363,0.142857142857143,0.160005345227478),.UNSPECIFIED.)
GEOMETRIC_REPRESENTATION_ITEM()
RATIONAL_B_SPLINE_SURFACE(((0.999805186472059,0.999805186472059,0.999805186472059,
0.999902211834794,1.,0.993980822699459,0.990851751371591),(0.999805186472059,
0.999805186472059,0.999805186472059,0.999902211834794,1.,0.993980822699459,
0.990851751371591)))
REPRESENTATION_ITEM('')
SURFACE()
);
#3480=(
BOUNDED_SURFACE()
B_SPLINE_SURFACE(1,2,((#153280,#153281,#153282,#153283,#153284),(#153285,
#153286,#153287,#153288,#153289)),.UNSPECIFIED.,.F.,.F.,.F.)
B_SPLINE_SURFACE_WITH_KNOTS((2,2),(3,2,3),(0.,0.289681084359929),(0.573550810617453,
0.590910950629594,0.591084552029715),.UNSPECIFIED.)
GEOMETRIC_REPRESENTATION_ITEM()
RATIONAL_B_SPLINE_SURFACE(((0.998554414400194,0.992822941359326,0.990053454406147,
0.990053454406147,0.990053454406147),(0.998554414400194,0.992822941359326,
0.990053454406147,0.990053454406147,0.990053454406147)))
REPRESENTATION_ITEM('')
SURFACE()
);
#3481=(
BOUNDED_SURFACE()
B_SPLINE_SURFACE(1,2,((#153291,#153292,#153293,#153294,#153295,#153296,
#153297),(#153298,#153299,#153300,#153301,#153302,#153303,#153304)),
 .UNSPECIFIED.,.F.,.F.,.F.)
B_SPLINE_SURFACE_WITH_KNOTS((2,2),(3,2,2,3),(0.,0.289807040991557),(0.142404283483303,
0.142578551421364,0.142857142857143,0.160005345227479),.UNSPECIFIED.)
GEOMETRIC_REPRESENTATION_ITEM()
RATIONAL_B_SPLINE_SURFACE(((0.999805186472059,0.999805186472059,0.999805186472059,
0.999902211834795,1.,0.993980822699459,0.990851751371591),(0.999805186472059,
0.999805186472059,0.999805186472059,0.999902211834795,1.,0.993980822699459,
0.990851751371591)))
REPRESENTATION_ITEM('')
SURFACE()
);
#3482=(
BOUNDED_SURFACE()
B_SPLINE_SURFACE(1,2,((#153321,#153322,#153323,#153324,#153325),(#153326,
#153327,#153328,#153329,#153330)),.UNSPECIFIED.,.F.,.F.,.F.)
B_SPLINE_SURFACE_WITH_KNOTS((2,2),(3,2,3),(0.,0.289681084359923),(0.573550810617443,
0.590910950629593,0.591084552029714),.UNSPECIFIED.)
GEOMETRIC_REPRESENTATION_ITEM()
RATIONAL_B_SPLINE_SURFACE(((0.998554414400201,0.992822941359327,0.990053454406148,
0.990053454406148,0.990053454406148),(0.998554414400201,0.992822941359327,
0.990053454406148,0.990053454406148,0.990053454406148)))
REPRESENTATION_ITEM('')
SURFACE()
);
#3483=(
BOUNDED_SURFACE()
B_SPLINE_SURFACE(1,2,((#153332,#153333,#153334,#153335,#153336,#153337,
#153338),(#153339,#153340,#153341,#153342,#153343,#153344,#153345)),
 .UNSPECIFIED.,.F.,.F.,.F.)
B_SPLINE_SURFACE_WITH_KNOTS((2,2),(3,2,2,3),(0.,0.289807040991565),(0.142404283483237,
0.142578551421299,0.142857142857143,0.16000534522748),.UNSPECIFIED.)
GEOMETRIC_REPRESENTATION_ITEM()
RATIONAL_B_SPLINE_SURFACE(((0.999805186472013,0.999805186472013,0.999805186472013,
0.999902211834772,1.,0.993980822699459,0.990851751371591),(0.999805186472013,
0.999805186472013,0.999805186472013,0.999902211834772,1.,0.993980822699459,
0.990851751371591)))
REPRESENTATION_ITEM('')
SURFACE()
);
#3484=(
BOUNDED_SURFACE()
B_SPLINE_SURFACE(1,2,((#153362,#153363,#153364,#153365,#153366),(#153367,
#153368,#153369,#153370,#153371)),.UNSPECIFIED.,.F.,.F.,.F.)
B_SPLINE_SURFACE_WITH_KNOTS((2,2),(3,2,3),(0.,0.289681084359925),(0.573550810617452,
0.590910950629595,0.591084552029716),.UNSPECIFIED.)
GEOMETRIC_REPRESENTATION_ITEM()
RATIONAL_B_SPLINE_SURFACE(((0.998554414400195,0.992822941359326,0.990053454406147,
0.990053454406147,0.990053454406147),(0.998554414400195,0.992822941359326,
0.990053454406147,0.990053454406147,0.990053454406147)))
REPRESENTATION_ITEM('')
SURFACE()
);
#3485=(
BOUNDED_SURFACE()
B_SPLINE_SURFACE(1,2,((#153373,#153374,#153375,#153376,#153377,#153378,
#153379),(#153380,#153381,#153382,#153383,#153384,#153385,#153386)),
 .UNSPECIFIED.,.F.,.F.,.F.)
B_SPLINE_SURFACE_WITH_KNOTS((2,2),(3,2,2,3),(0.,0.28980704099157),(0.142404283483249,
0.142578551421311,0.142857142857143,0.160005345227479),.UNSPECIFIED.)
GEOMETRIC_REPRESENTATION_ITEM()
RATIONAL_B_SPLINE_SURFACE(((0.999805186472022,0.999805186472022,0.999805186472022,
0.999902211834776,1.,0.993980822699459,0.990851751371591),(0.999805186472022,
0.999805186472022,0.999805186472022,0.999902211834776,1.,0.993980822699459,
0.990851751371591)))
REPRESENTATION_ITEM('')
SURFACE()
);
#3486=(
BOUNDED_SURFACE()
B_SPLINE_SURFACE(1,2,((#153403,#153404,#153405,#153406,#153407),(#153408,
#153409,#153410,#153411,#153412)),.UNSPECIFIED.,.F.,.F.,.F.)
B_SPLINE_SURFACE_WITH_KNOTS((2,2),(3,2,3),(0.,0.289681084359923),(0.573550810617452,
0.590910950629593,0.591084552029714),.UNSPECIFIED.)
GEOMETRIC_REPRESENTATION_ITEM()
RATIONAL_B_SPLINE_SURFACE(((0.998554414400195,0.992822941359326,0.990053454406148,
0.990053454406148,0.990053454406148),(0.998554414400195,0.992822941359326,
0.990053454406148,0.990053454406148,0.990053454406148)))
REPRESENTATION_ITEM('')
SURFACE()
);
#3487=(
BOUNDED_SURFACE()
B_SPLINE_SURFACE(1,2,((#153414,#153415,#153416,#153417,#153418,#153419,
#153420),(#153421,#153422,#153423,#153424,#153425,#153426,#153427)),
 .UNSPECIFIED.,.F.,.F.,.F.)
B_SPLINE_SURFACE_WITH_KNOTS((2,2),(3,2,2,3),(0.,0.289807040991713),(0.142404283483303,
0.142578551421364,0.142857142857143,0.160005345227479),.UNSPECIFIED.)
GEOMETRIC_REPRESENTATION_ITEM()
RATIONAL_B_SPLINE_SURFACE(((0.999805186472059,0.999805186472059,0.999805186472059,
0.999902211834795,1.,0.993980822699459,0.990851751371591),(0.999805186472059,
0.999805186472059,0.999805186472059,0.999902211834795,1.,0.993980822699459,
0.990851751371591)))
REPRESENTATION_ITEM('')
SURFACE()
);
#3488=(
BOUNDED_SURFACE()
B_SPLINE_SURFACE(1,2,((#153444,#153445,#153446,#153447,#153448),(#153449,
#153450,#153451,#153452,#153453)),.UNSPECIFIED.,.F.,.F.,.F.)
B_SPLINE_SURFACE_WITH_KNOTS((2,2),(3,2,3),(0.,0.289681084359918),(0.573550810617382,
0.590910950629593,0.591084552029715),.UNSPECIFIED.)
GEOMETRIC_REPRESENTATION_ITEM()
RATIONAL_B_SPLINE_SURFACE(((0.998554414400241,0.992822941359337,0.990053454406148,
0.990053454406148,0.990053454406148),(0.998554414400241,0.992822941359337,
0.990053454406148,0.990053454406148,0.990053454406148)))
REPRESENTATION_ITEM('')
SURFACE()
);
#3489=(
BOUNDED_SURFACE()
B_SPLINE_SURFACE(1,2,((#153455,#153456,#153457,#153458,#153459,#153460,
#153461),(#153462,#153463,#153464,#153465,#153466,#153467,#153468)),
 .UNSPECIFIED.,.F.,.F.,.F.)
B_SPLINE_SURFACE_WITH_KNOTS((2,2),(3,2,2,3),(0.,0.289807040993087),(0.142404283483302,
0.142578551421363,0.142857142857143,0.160005345227479),.UNSPECIFIED.)
GEOMETRIC_REPRESENTATION_ITEM()
RATIONAL_B_SPLINE_SURFACE(((0.999805186472059,0.999805186472059,0.999805186472059,
0.999902211834794,1.,0.993980822699459,0.990851751371591),(0.999805186472059,
0.999805186472059,0.999805186472059,0.999902211834794,1.,0.993980822699459,
0.990851751371591)))
REPRESENTATION_ITEM('')
SURFACE()
);
#3490=(
BOUNDED_SURFACE()
B_SPLINE_SURFACE(1,2,((#153485,#153486,#153487,#153488,#153489),(#153490,
#153491,#153492,#153493,#153494)),.UNSPECIFIED.,.F.,.F.,.F.)
B_SPLINE_SURFACE_WITH_KNOTS((2,2),(3,2,3),(0.,0.289681084360127),(0.573550810617425,
0.590910950629593,0.591084552029715),.UNSPECIFIED.)
GEOMETRIC_REPRESENTATION_ITEM()
RATIONAL_B_SPLINE_SURFACE(((0.998554414400213,0.99282294135933,0.990053454406148,
0.990053454406148,0.990053454406148),(0.998554414400213,0.99282294135933,
0.990053454406147,0.990053454406147,0.990053454406147)))
REPRESENTATION_ITEM('')
SURFACE()
);
#3491=(
BOUNDED_SURFACE()
B_SPLINE_SURFACE(1,2,((#153496,#153497,#153498,#153499,#153500,#153501,
#153502),(#153503,#153504,#153505,#153506,#153507,#153508,#153509)),
 .UNSPECIFIED.,.F.,.F.,.F.)
B_SPLINE_SURFACE_WITH_KNOTS((2,2),(3,2,2,3),(0.,0.289807040991616),(0.142404283483146,
0.142578551421209,0.142857142857143,0.16000534522748),.UNSPECIFIED.)
GEOMETRIC_REPRESENTATION_ITEM()
RATIONAL_B_SPLINE_SURFACE(((0.999805186471951,0.999805186471951,0.999805186471951,
0.99990221183474,1.,0.993980822699459,0.990851751371591),(0.999805186471951,
0.999805186471951,0.999805186471951,0.99990221183474,1.,0.993980822699459,
0.990851751371591)))
REPRESENTATION_ITEM('')
SURFACE()
);
#3492=(
BOUNDED_SURFACE()
B_SPLINE_SURFACE(1,2,((#153526,#153527,#153528,#153529,#153530),(#153531,
#153532,#153533,#153534,#153535)),.UNSPECIFIED.,.F.,.F.,.F.)
B_SPLINE_SURFACE_WITH_KNOTS((2,2),(3,2,3),(0.,0.289681084359932),(0.573550810617452,
0.590910950629593,0.591084552029714),.UNSPECIFIED.)
GEOMETRIC_REPRESENTATION_ITEM()
RATIONAL_B_SPLINE_SURFACE(((0.998554414400195,0.992822941359326,0.990053454406148,
0.990053454406148,0.990053454406148),(0.998554414400195,0.992822941359326,
0.990053454406148,0.990053454406148,0.990053454406148)))
REPRESENTATION_ITEM('')
SURFACE()
);
#3493=(
BOUNDED_SURFACE()
B_SPLINE_SURFACE(1,2,((#153537,#153538,#153539,#153540,#153541,#153542,
#153543),(#153544,#153545,#153546,#153547,#153548,#153549,#153550)),
 .UNSPECIFIED.,.F.,.F.,.F.)
B_SPLINE_SURFACE_WITH_KNOTS((2,2),(3,2,2,3),(0.,0.289807040991645),(0.142404283483298,
0.142578551421359,0.142857142857143,0.160005345227479),.UNSPECIFIED.)
GEOMETRIC_REPRESENTATION_ITEM()
RATIONAL_B_SPLINE_SURFACE(((0.999805186472056,0.999805186472056,0.999805186472056,
0.999902211834793,1.,0.993980822699459,0.990851751371591),(0.999805186472056,
0.999805186472056,0.999805186472056,0.999902211834793,1.,0.993980822699459,
0.990851751371591)))
REPRESENTATION_ITEM('')
SURFACE()
);
#3494=(
BOUNDED_SURFACE()
B_SPLINE_SURFACE(1,2,((#153567,#153568,#153569,#153570,#153571),(#153572,
#153573,#153574,#153575,#153576)),.UNSPECIFIED.,.F.,.F.,.F.)
B_SPLINE_SURFACE_WITH_KNOTS((2,2),(3,2,3),(0.,0.289681084359924),(0.573550810617452,
0.590910950629593,0.591084552029714),.UNSPECIFIED.)
GEOMETRIC_REPRESENTATION_ITEM()
RATIONAL_B_SPLINE_SURFACE(((0.998554414400195,0.992822941359326,0.990053454406148,
0.990053454406148,0.990053454406148),(0.998554414400195,0.992822941359326,
0.990053454406147,0.990053454406147,0.990053454406147)))
REPRESENTATION_ITEM('')
SURFACE()
);
#3495=(
BOUNDED_SURFACE()
B_SPLINE_SURFACE(1,2,((#153578,#153579,#153580,#153581,#153582,#153583,
#153584),(#153585,#153586,#153587,#153588,#153589,#153590,#153591)),
 .UNSPECIFIED.,.F.,.F.,.F.)
B_SPLINE_SURFACE_WITH_KNOTS((2,2),(3,2,2,3),(0.,0.289807040991634),(0.142404283483303,
0.142578551421364,0.142857142857143,0.160005345227479),.UNSPECIFIED.)
GEOMETRIC_REPRESENTATION_ITEM()
RATIONAL_B_SPLINE_SURFACE(((0.999805186472059,0.999805186472059,0.999805186472059,
0.999902211834795,1.,0.993980822699459,0.990851751371591),(0.999805186472059,
0.999805186472059,0.999805186472059,0.999902211834795,1.,0.993980822699459,
0.990851751371591)))
REPRESENTATION_ITEM('')
SURFACE()
);
#3496=(
BOUNDED_SURFACE()
B_SPLINE_SURFACE(1,2,((#153608,#153609,#153610,#153611,#153612),(#153613,
#153614,#153615,#153616,#153617)),.UNSPECIFIED.,.F.,.F.,.F.)
B_SPLINE_SURFACE_WITH_KNOTS((2,2),(3,2,3),(0.,0.289681084359921),(0.573550810617452,
0.590910950629593,0.591084552029714),.UNSPECIFIED.)
GEOMETRIC_REPRESENTATION_ITEM()
RATIONAL_B_SPLINE_SURFACE(((0.998554414400195,0.992822941359326,0.990053454406147,
0.990053454406147,0.990053454406147),(0.998554414400195,0.992822941359326,
0.990053454406147,0.990053454406147,0.990053454406147)))
REPRESENTATION_ITEM('')
SURFACE()
);
#3497=(
BOUNDED_SURFACE()
B_SPLINE_SURFACE(1,2,((#153619,#153620,#153621,#153622,#153623,#153624,
#153625),(#153626,#153627,#153628,#153629,#153630,#153631,#153632)),
 .UNSPECIFIED.,.F.,.F.,.F.)
B_SPLINE_SURFACE_WITH_KNOTS((2,2),(3,2,2,3),(0.,0.289807040991559),(0.142404283483175,
0.142578551421237,0.142857142857143,0.16000534522748),.UNSPECIFIED.)
GEOMETRIC_REPRESENTATION_ITEM()
RATIONAL_B_SPLINE_SURFACE(((0.999805186471971,0.999805186471971,0.999805186471971,
0.99990221183475,1.,0.993980822699459,0.990851751371591),(0.999805186471971,
0.999805186471971,0.999805186471971,0.99990221183475,1.,0.993980822699459,
0.990851751371591)))
REPRESENTATION_ITEM('')
SURFACE()
);
#3498=(
BOUNDED_SURFACE()
B_SPLINE_SURFACE(1,2,((#153649,#153650,#153651,#153652,#153653),(#153654,
#153655,#153656,#153657,#153658)),.UNSPECIFIED.,.F.,.F.,.F.)
B_SPLINE_SURFACE_WITH_KNOTS((2,2),(3,2,3),(0.,0.289681084359924),(0.5735508106174,
0.590910950629593,0.591084552029715),.UNSPECIFIED.)
GEOMETRIC_REPRESENTATION_ITEM()
RATIONAL_B_SPLINE_SURFACE(((0.998554414400229,0.992822941359334,0.990053454406148,
0.990053454406148,0.990053454406148),(0.998554414400229,0.992822941359334,
0.990053454406148,0.990053454406148,0.990053454406148)))
REPRESENTATION_ITEM('')
SURFACE()
);
#3499=(
BOUNDED_SURFACE()
B_SPLINE_SURFACE(1,2,((#153666,#153667,#153668,#153669,#153670,#153671,
#153672),(#153673,#153674,#153675,#153676,#153677,#153678,#153679)),
 .UNSPECIFIED.,.F.,.F.,.F.)
B_SPLINE_SURFACE_WITH_KNOTS((2,2),(3,2,2,3),(0.,0.289807040991565),(0.142404283483079,
0.142578551421142,0.142857142857143,0.160005345227427),.UNSPECIFIED.)
GEOMETRIC_REPRESENTATION_ITEM()
RATIONAL_B_SPLINE_SURFACE(((0.999805186471905,0.999805186471905,0.999805186471905,
0.999902211834717,1.,0.993980822699477,0.99085175137161),(0.999805186471905,
0.999805186471905,0.999805186471905,0.999902211834717,1.,0.993980822699477,
0.99085175137161)))
REPRESENTATION_ITEM('')
SURFACE()
);
#3500=(
BOUNDED_SURFACE()
B_SPLINE_SURFACE(1,2,((#153681,#153682,#153683),(#153684,#153685,#153686),
(#153687,#153688,#153689)),.UNSPECIFIED.,.F.,.F.,.F.)
B_SPLINE_SURFACE_WITH_KNOTS((2,1,2),(3,3),(0.688417832139402,0.710192959008107,
1.),(0.0909109506295426,0.108084585199971),.UNSPECIFIED.)
GEOMETRIC_REPRESENTATION_ITEM()
RATIONAL_B_SPLINE_SURFACE(((0.990053454406164,0.987313720921967,0.987472672298934),
(0.990053454406164,0.987313720921967,0.987472672298934),(0.990053454406164,
0.987313720921967,0.987472672298934)))
REPRESENTATION_ITEM('')
SURFACE()
);
#3501=(
BOUNDED_SURFACE()
B_SPLINE_SURFACE(1,2,((#153705,#153706,#153707),(#153708,#153709,#153710),
(#153711,#153712,#153713)),.UNSPECIFIED.,.F.,.F.,.F.)
B_SPLINE_SURFACE_WITH_KNOTS((2,1,2),(3,3),(0.688516410643263,0.71031891563962,
1.),(0.625066077454535,0.642578551421363),.UNSPECIFIED.)
GEOMETRIC_REPRESENTATION_ITEM()
RATIONAL_B_SPLINE_SURFACE(((0.990621203777021,0.993706096834649,0.999805186472059),
(0.990621203777021,0.993706096834649,0.999805186472059),(0.990621203777021,
0.993706096834649,0.999805186472059)))
REPRESENTATION_ITEM('')
SURFACE()
);
#3502=(
BOUNDED_SURFACE()
B_SPLINE_SURFACE(1,2,((#153754,#153755,#153756),(#153757,#153758,#153759),
(#153760,#153761,#153762)),.UNSPECIFIED.,.F.,.F.,.F.)
B_SPLINE_SURFACE_WITH_KNOTS((2,1,2),(3,3),(0.688417834114171,0.710192959007975,
1.),(0.0909109506295457,0.108084585199971),.UNSPECIFIED.)
GEOMETRIC_REPRESENTATION_ITEM()
RATIONAL_B_SPLINE_SURFACE(((0.990053454406163,0.987313720921967,0.987472672298934),
(0.990053454406163,0.987313720921967,0.987472672298934),(0.990053454406163,
0.987313720921967,0.987472672298934)))
REPRESENTATION_ITEM('')
SURFACE()
);
#3503=(
BOUNDED_SURFACE()
B_SPLINE_SURFACE(1,2,((#153764,#153765,#153766),(#153767,#153768,#153769),
(#153770,#153771,#153772)),.UNSPECIFIED.,.F.,.F.,.F.)
B_SPLINE_SURFACE_WITH_KNOTS((2,1,2),(3,3),(0.688516410654661,0.710318915639632,
1.),(0.625066077454535,0.642578551421363),.UNSPECIFIED.)
GEOMETRIC_REPRESENTATION_ITEM()
RATIONAL_B_SPLINE_SURFACE(((0.990621203777021,0.993706096834649,0.999805186472059),
(0.990621203777021,0.993706096834649,0.999805186472059),(0.990621203777021,
0.993706096834649,0.999805186472059)))
REPRESENTATION_ITEM('')
SURFACE()
);
#3504=(
BOUNDED_SURFACE()
B_SPLINE_SURFACE(1,2,((#153813,#153814,#153815),(#153816,#153817,#153818),
(#153819,#153820,#153821)),.UNSPECIFIED.,.F.,.F.,.F.)
B_SPLINE_SURFACE_WITH_KNOTS((2,1,2),(3,3),(0.688417833968987,0.710192959007994,
1.),(0.0909109506295942,0.10808458519997),.UNSPECIFIED.)
GEOMETRIC_REPRESENTATION_ITEM()
RATIONAL_B_SPLINE_SURFACE(((0.990053454406147,0.987313720921968,0.987472672298934),
(0.990053454406147,0.987313720921968,0.987472672298934),(0.990053454406147,
0.987313720921968,0.987472672298934)))
REPRESENTATION_ITEM('')
SURFACE()
);
#3505=(
BOUNDED_SURFACE()
B_SPLINE_SURFACE(1,2,((#153823,#153824,#153825),(#153826,#153827,#153828),
(#153829,#153830,#153831)),.UNSPECIFIED.,.F.,.F.,.F.)
B_SPLINE_SURFACE_WITH_KNOTS((2,1,2),(3,3),(0.688516410790942,0.71031891563998,
1.),(0.625066077454535,0.642578551421363),.UNSPECIFIED.)
GEOMETRIC_REPRESENTATION_ITEM()
RATIONAL_B_SPLINE_SURFACE(((0.990621203777021,0.993706096834649,0.999805186472059),
(0.990621203777021,0.993706096834649,0.999805186472059),(0.990621203777021,
0.993706096834649,0.999805186472059)))
REPRESENTATION_ITEM('')
SURFACE()
);
#3506=(
BOUNDED_SURFACE()
B_SPLINE_SURFACE(1,2,((#153872,#153873,#153874),(#153875,#153876,#153877),
(#153878,#153879,#153880)),.UNSPECIFIED.,.F.,.F.,.F.)
B_SPLINE_SURFACE_WITH_KNOTS((2,1,2),(3,3),(0.68841783381541,0.710192959008345,
1.),(0.090910950629593,0.10808458519997),.UNSPECIFIED.)
GEOMETRIC_REPRESENTATION_ITEM()
RATIONAL_B_SPLINE_SURFACE(((0.990053454406147,0.987313720921968,0.987472672298934),
(0.990053454406147,0.987313720921968,0.987472672298934),(0.990053454406147,
0.987313720921968,0.987472672298934)))
REPRESENTATION_ITEM('')
SURFACE()
);
#3507=(
BOUNDED_SURFACE()
B_SPLINE_SURFACE(1,2,((#153882,#153883,#153884),(#153885,#153886,#153887),
(#153888,#153889,#153890)),.UNSPECIFIED.,.F.,.F.,.F.)
B_SPLINE_SURFACE_WITH_KNOTS((2,1,2),(3,3),(0.688516410355011,0.710318915639971,
1.),(0.625066077454535,0.642578551421363),.UNSPECIFIED.)
GEOMETRIC_REPRESENTATION_ITEM()
RATIONAL_B_SPLINE_SURFACE(((0.990621203777021,0.993706096834649,0.999805186472059),
(0.990621203777021,0.993706096834649,0.999805186472059),(0.990621203777021,
0.993706096834649,0.999805186472059)))
REPRESENTATION_ITEM('')
SURFACE()
);
#3508=(
BOUNDED_SURFACE()
B_SPLINE_SURFACE(1,2,((#153931,#153932,#153933),(#153934,#153935,#153936),
(#153937,#153938,#153939)),.UNSPECIFIED.,.F.,.F.,.F.)
B_SPLINE_SURFACE_WITH_KNOTS((2,1,2),(3,3),(0.688417834222182,0.710192959008331,
1.),(0.0909109506295941,0.10808458519997),.UNSPECIFIED.)
GEOMETRIC_REPRESENTATION_ITEM()
RATIONAL_B_SPLINE_SURFACE(((0.990053454406147,0.987313720921968,0.987472672298934),
(0.990053454406147,0.987313720921968,0.987472672298934),(0.990053454406147,
0.987313720921968,0.987472672298934)))
REPRESENTATION_ITEM('')
SURFACE()
);
#3509=(
BOUNDED_SURFACE()
B_SPLINE_SURFACE(1,2,((#153941,#153942,#153943),(#153944,#153945,#153946),
(#153947,#153948,#153949)),.UNSPECIFIED.,.F.,.F.,.F.)
B_SPLINE_SURFACE_WITH_KNOTS((2,1,2),(3,3),(0.688516410538964,0.710318915639015,
1.),(0.625066077454535,0.642578551421363),.UNSPECIFIED.)
GEOMETRIC_REPRESENTATION_ITEM()
RATIONAL_B_SPLINE_SURFACE(((0.990621203777021,0.993706096834649,0.999805186472059),
(0.990621203777021,0.993706096834649,0.999805186472059),(0.990621203777021,
0.993706096834649,0.999805186472059)))
REPRESENTATION_ITEM('')
SURFACE()
);
#3510=(
BOUNDED_SURFACE()
B_SPLINE_SURFACE(1,2,((#153990,#153991,#153992),(#153993,#153994,#153995),
(#153996,#153997,#153998)),.UNSPECIFIED.,.F.,.F.,.F.)
B_SPLINE_SURFACE_WITH_KNOTS((2,1,2),(3,3),(0.688417834370893,0.710192959007374,
1.),(0.0909109506295929,0.10808458519997),.UNSPECIFIED.)
GEOMETRIC_REPRESENTATION_ITEM()
RATIONAL_B_SPLINE_SURFACE(((0.990053454406148,0.987313720921968,0.987472672298934),
(0.990053454406148,0.987313720921968,0.987472672298934),(0.990053454406148,
0.987313720921968,0.987472672298934)))
REPRESENTATION_ITEM('')
SURFACE()
);
#3511=(
BOUNDED_SURFACE()
B_SPLINE_SURFACE(1,2,((#154000,#154001,#154002),(#154003,#154004,#154005),
(#154006,#154007,#154008)),.UNSPECIFIED.,.F.,.F.,.F.)
B_SPLINE_SURFACE_WITH_KNOTS((2,1,2),(3,3),(0.688516410279689,0.710318915639017,
1.),(0.625066077454535,0.642578551421363),.UNSPECIFIED.)
GEOMETRIC_REPRESENTATION_ITEM()
RATIONAL_B_SPLINE_SURFACE(((0.990621203777021,0.993706096834649,0.999805186472059),
(0.990621203777021,0.993706096834649,0.999805186472059),(0.990621203777021,
0.993706096834649,0.999805186472059)))
REPRESENTATION_ITEM('')
SURFACE()
);
#3512=(
BOUNDED_SURFACE()
B_SPLINE_SURFACE(1,2,((#154049,#154050,#154051),(#154052,#154053,#154054),
(#154055,#154056,#154057)),.UNSPECIFIED.,.F.,.F.,.F.)
B_SPLINE_SURFACE_WITH_KNOTS((2,1,2),(3,3),(0.688417834245439,0.710192959007374,
1.),(0.0909109506295555,0.108084585199971),.UNSPECIFIED.)
GEOMETRIC_REPRESENTATION_ITEM()
RATIONAL_B_SPLINE_SURFACE(((0.99005345440616,0.987313720921967,0.987472672298934),
(0.99005345440616,0.987313720921967,0.987472672298934),(0.99005345440616,
0.987313720921967,0.987472672298934)))
REPRESENTATION_ITEM('')
SURFACE()
);
#3513=(
BOUNDED_SURFACE()
B_SPLINE_SURFACE(1,2,((#154059,#154060,#154061),(#154062,#154063,#154064),
(#154065,#154066,#154067)),.UNSPECIFIED.,.F.,.F.,.F.)
B_SPLINE_SURFACE_WITH_KNOTS((2,1,2),(3,3),(0.688516410179556,0.710318915639016,
1.),(0.625066077454535,0.642578551421363),.UNSPECIFIED.)
GEOMETRIC_REPRESENTATION_ITEM()
RATIONAL_B_SPLINE_SURFACE(((0.990621203777021,0.993706096834649,0.999805186472059),
(0.990621203777021,0.993706096834649,0.999805186472059),(0.990621203777021,
0.993706096834649,0.999805186472059)))
REPRESENTATION_ITEM('')
SURFACE()
);
#3514=(
BOUNDED_SURFACE()
B_SPLINE_SURFACE(1,2,((#154108,#154109,#154110),(#154111,#154112,#154113),
(#154114,#154115,#154116)),.UNSPECIFIED.,.F.,.F.,.F.)
B_SPLINE_SURFACE_WITH_KNOTS((2,1,2),(3,3),(0.688417833993896,0.710192959007378,
1.),(0.0909109506295549,0.108084585199971),.UNSPECIFIED.)
GEOMETRIC_REPRESENTATION_ITEM()
RATIONAL_B_SPLINE_SURFACE(((0.99005345440616,0.987313720921967,0.987472672298934),
(0.99005345440616,0.987313720921967,0.987472672298934),(0.99005345440616,
0.987313720921967,0.987472672298934)))
REPRESENTATION_ITEM('')
SURFACE()
);
#3515=(
BOUNDED_SURFACE()
B_SPLINE_SURFACE(1,2,((#154118,#154119,#154120),(#154121,#154122,#154123),
(#154124,#154125,#154126)),.UNSPECIFIED.,.F.,.F.,.F.)
B_SPLINE_SURFACE_WITH_KNOTS((2,1,2),(3,3),(0.68851641069385,0.710318915638436,
1.),(0.625066077454535,0.642578551421363),.UNSPECIFIED.)
GEOMETRIC_REPRESENTATION_ITEM()
RATIONAL_B_SPLINE_SURFACE(((0.990621203777021,0.993706096834649,0.999805186472059),
(0.990621203777021,0.993706096834649,0.999805186472059),(0.990621203777021,
0.993706096834649,0.999805186472059)))
REPRESENTATION_ITEM('')
SURFACE()
);
#3516=(
BOUNDED_SURFACE()
B_SPLINE_SURFACE(1,2,((#154167,#154168,#154169),(#154170,#154171,#154172),
(#154173,#154174,#154175)),.UNSPECIFIED.,.F.,.F.,.F.)
B_SPLINE_SURFACE_WITH_KNOTS((2,1,2),(3,3),(0.688417834521045,0.710192959006796,
1.),(0.0909109506295929,0.10808458519997),.UNSPECIFIED.)
GEOMETRIC_REPRESENTATION_ITEM()
RATIONAL_B_SPLINE_SURFACE(((0.990053454406148,0.987313720921968,0.987472672298934),
(0.990053454406148,0.987313720921968,0.987472672298934),(0.990053454406148,
0.987313720921968,0.987472672298934)))
REPRESENTATION_ITEM('')
SURFACE()
);
#3517=(
BOUNDED_SURFACE()
B_SPLINE_SURFACE(1,2,((#154177,#154178,#154179),(#154180,#154181,#154182),
(#154183,#154184,#154185)),.UNSPECIFIED.,.F.,.F.,.F.)
B_SPLINE_SURFACE_WITH_KNOTS((2,1,2),(3,3),(0.688516410378158,0.71031891563903,
1.),(0.625066077454535,0.642578551421363),.UNSPECIFIED.)
GEOMETRIC_REPRESENTATION_ITEM()
RATIONAL_B_SPLINE_SURFACE(((0.990621203777021,0.993706096834649,0.999805186472059),
(0.990621203777021,0.993706096834649,0.999805186472059),(0.990621203777021,
0.993706096834649,0.999805186472059)))
REPRESENTATION_ITEM('')
SURFACE()
);
#3518=(
BOUNDED_SURFACE()
B_SPLINE_SURFACE(1,2,((#154226,#154227,#154228),(#154229,#154230,#154231),
(#154232,#154233,#154234)),.UNSPECIFIED.,.F.,.F.,.F.)
B_SPLINE_SURFACE_WITH_KNOTS((2,1,2),(3,3),(0.688417834350685,0.710192959007387,
1.),(0.090910950629593,0.10808458519997),.UNSPECIFIED.)
GEOMETRIC_REPRESENTATION_ITEM()
RATIONAL_B_SPLINE_SURFACE(((0.990053454406148,0.987313720921968,0.987472672298934),
(0.990053454406148,0.987313720921968,0.987472672298934),(0.990053454406148,
0.987313720921968,0.987472672298934)))
REPRESENTATION_ITEM('')
SURFACE()
);
#3519=(
BOUNDED_SURFACE()
B_SPLINE_SURFACE(1,2,((#154236,#154237,#154238),(#154239,#154240,#154241),
(#154242,#154243,#154244)),.UNSPECIFIED.,.F.,.F.,.F.)
B_SPLINE_SURFACE_WITH_KNOTS((2,1,2),(3,3),(0.688516410525766,0.710318915638467,
1.),(0.625066077454535,0.642578551421363),.UNSPECIFIED.)
GEOMETRIC_REPRESENTATION_ITEM()
RATIONAL_B_SPLINE_SURFACE(((0.990621203777021,0.993706096834649,0.999805186472058),
(0.990621203777021,0.993706096834649,0.999805186472058),(0.990621203777021,
0.993706096834649,0.999805186472058)))
REPRESENTATION_ITEM('')
SURFACE()
);
#3520=(
BOUNDED_SURFACE()
B_SPLINE_SURFACE(1,2,((#154285,#154286,#154287),(#154288,#154289,#154290),
(#154291,#154292,#154293)),.UNSPECIFIED.,.F.,.F.,.F.)
B_SPLINE_SURFACE_WITH_KNOTS((2,1,2),(3,3),(0.688417834091111,0.710192959006829,
1.),(0.0909109506295647,0.108084585199971),.UNSPECIFIED.)
GEOMETRIC_REPRESENTATION_ITEM()
RATIONAL_B_SPLINE_SURFACE(((0.990053454406157,0.987313720921967,0.987472672298934),
(0.990053454406157,0.987313720921967,0.987472672298934),(0.990053454406157,
0.987313720921967,0.987472672298934)))
REPRESENTATION_ITEM('')
SURFACE()
);
#3521=(
BOUNDED_SURFACE()
B_SPLINE_SURFACE(1,2,((#154295,#154296,#154297),(#154298,#154299,#154300),
(#154301,#154302,#154303)),.UNSPECIFIED.,.F.,.F.,.F.)
B_SPLINE_SURFACE_WITH_KNOTS((2,1,2),(3,3),(0.688516410404015,0.710318915638657,
1.),(0.625066077454536,0.642578551421363),.UNSPECIFIED.)
GEOMETRIC_REPRESENTATION_ITEM()
RATIONAL_B_SPLINE_SURFACE(((0.990621203777022,0.993706096834649,0.999805186472059),
(0.990621203777022,0.993706096834649,0.999805186472059),(0.990621203777022,
0.993706096834649,0.999805186472059)))
REPRESENTATION_ITEM('')
SURFACE()
);
#3522=(
BOUNDED_SURFACE()
B_SPLINE_SURFACE(1,2,((#154344,#154345,#154346),(#154347,#154348,#154349),
(#154350,#154351,#154352)),.UNSPECIFIED.,.F.,.F.,.F.)
B_SPLINE_SURFACE_WITH_KNOTS((2,1,2),(3,3),(0.688417834498563,0.710192959007008,
1.),(0.090910950629561,0.10808458519997),.UNSPECIFIED.)
GEOMETRIC_REPRESENTATION_ITEM()
RATIONAL_B_SPLINE_SURFACE(((0.990053454406158,0.987313720921967,0.987472672298934),
(0.990053454406158,0.987313720921967,0.987472672298934),(0.990053454406158,
0.987313720921967,0.987472672298934)))
REPRESENTATION_ITEM('')
SURFACE()
);
#3523=(
BOUNDED_SURFACE()
B_SPLINE_SURFACE(1,2,((#154354,#154355,#154356),(#154357,#154358,#154359),
(#154360,#154361,#154362)),.UNSPECIFIED.,.F.,.F.,.F.)
B_SPLINE_SURFACE_WITH_KNOTS((2,1,2),(3,3),(0.688516410316575,0.710318915638622,
1.),(0.625066077454536,0.642578551421364),.UNSPECIFIED.)
GEOMETRIC_REPRESENTATION_ITEM()
RATIONAL_B_SPLINE_SURFACE(((0.990621203777022,0.993706096834649,0.999805186472059),
(0.990621203777022,0.993706096834649,0.999805186472059),(0.990621203777022,
0.993706096834649,0.999805186472059)))
REPRESENTATION_ITEM('')
SURFACE()
);
#3524=(
BOUNDED_SURFACE()
B_SPLINE_SURFACE(1,2,((#154403,#154404,#154405),(#154406,#154407,#154408),
(#154409,#154410,#154411)),.UNSPECIFIED.,.F.,.F.,.F.)
B_SPLINE_SURFACE_WITH_KNOTS((2,1,2),(3,3),(0.688417834508433,0.710192959006985,
1.),(0.0909109506295931,0.108084585199969),.UNSPECIFIED.)
GEOMETRIC_REPRESENTATION_ITEM()
RATIONAL_B_SPLINE_SURFACE(((0.990053454406148,0.987313720921968,0.987472672298934),
(0.990053454406148,0.987313720921968,0.987472672298934),(0.990053454406148,
0.987313720921968,0.987472672298934)))
REPRESENTATION_ITEM('')
SURFACE()
);
#3525=(
BOUNDED_SURFACE()
B_SPLINE_SURFACE(1,2,((#154413,#154414,#154415),(#154416,#154417,#154418),
(#154419,#154420,#154421)),.UNSPECIFIED.,.F.,.F.,.F.)
B_SPLINE_SURFACE_WITH_KNOTS((2,1,2),(3,3),(0.688516410725903,0.710318915638348,
1.),(0.625066077454536,0.642578551421364),.UNSPECIFIED.)
GEOMETRIC_REPRESENTATION_ITEM()
RATIONAL_B_SPLINE_SURFACE(((0.990621203777022,0.993706096834649,0.999805186472059),
(0.990621203777022,0.993706096834649,0.999805186472059),(0.990621203777022,
0.993706096834649,0.999805186472059)))
REPRESENTATION_ITEM('')
SURFACE()
);
#3526=(
BOUNDED_SURFACE()
B_SPLINE_SURFACE(1,2,((#154462,#154463,#154464),(#154465,#154466,#154467),
(#154468,#154469,#154470)),.UNSPECIFIED.,.F.,.F.,.F.)
B_SPLINE_SURFACE_WITH_KNOTS((2,1,2),(3,3),(0.688417834372287,0.710192959006701,
1.),(0.0909109506295633,0.108084585199969),.UNSPECIFIED.)
GEOMETRIC_REPRESENTATION_ITEM()
RATIONAL_B_SPLINE_SURFACE(((0.990053454406157,0.987313720921968,0.987472672298934),
(0.990053454406157,0.987313720921968,0.987472672298934),(0.990053454406157,
0.987313720921968,0.987472672298934)))
REPRESENTATION_ITEM('')
SURFACE()
);
#3527=(
BOUNDED_SURFACE()
B_SPLINE_SURFACE(1,2,((#154472,#154473,#154474),(#154475,#154476,#154477),
(#154478,#154479,#154480)),.UNSPECIFIED.,.F.,.F.,.F.)
B_SPLINE_SURFACE_WITH_KNOTS((2,1,2),(3,3),(0.688516410487827,0.710318915638921,
1.),(0.625066077454536,0.642578551421365),.UNSPECIFIED.)
GEOMETRIC_REPRESENTATION_ITEM()
RATIONAL_B_SPLINE_SURFACE(((0.990621203777022,0.993706096834649,0.999805186472059),
(0.990621203777022,0.993706096834649,0.999805186472059),(0.990621203777022,
0.993706096834649,0.999805186472059)))
REPRESENTATION_ITEM('')
SURFACE()
);
#3528=(
BOUNDED_SURFACE()
B_SPLINE_SURFACE(1,2,((#154488,#154489,#154490),(#154491,#154492,#154493),
(#154494,#154495,#154496)),.UNSPECIFIED.,.F.,.F.,.F.)
B_SPLINE_SURFACE_WITH_KNOTS((2,1,2),(3,3),(0.688417834510296,0.710192959007285,
1.),(0.0909109506295919,0.108084585199969),.UNSPECIFIED.)
GEOMETRIC_REPRESENTATION_ITEM()
RATIONAL_B_SPLINE_SURFACE(((0.990053454406148,0.987313720921968,0.987472672298934),
(0.990053454406148,0.987313720921968,0.987472672298934),(0.990053454406148,
0.987313720921968,0.987472672298934)))
REPRESENTATION_ITEM('')
SURFACE()
);
#3529=(
BOUNDED_SURFACE()
B_SPLINE_SURFACE(1,2,((#154498,#154499,#154500),(#154501,#154502,#154503),
(#154504,#154505,#154506)),.UNSPECIFIED.,.F.,.F.,.F.)
B_SPLINE_SURFACE_WITH_KNOTS((2,1,2),(3,3),(0.68851641049287,0.710318915638097,
1.),(0.625066077454536,0.642578551421364),.UNSPECIFIED.)
GEOMETRIC_REPRESENTATION_ITEM()
RATIONAL_B_SPLINE_SURFACE(((0.990621203777022,0.993706096834649,0.999805186472059),
(0.990621203777022,0.993706096834649,0.999805186472059),(0.990621203777022,
0.993706096834649,0.999805186472059)))
REPRESENTATION_ITEM('')
SURFACE()
);
#3530=(
BOUNDED_SURFACE()
B_SPLINE_SURFACE(1,2,((#154547,#154548,#154549),(#154550,#154551,#154552),
(#154553,#154554,#154555)),.UNSPECIFIED.,.F.,.F.,.F.)
B_SPLINE_SURFACE_WITH_KNOTS((2,1,2),(3,3),(0.688417834553386,0.710192959006459,
1.),(0.0909109506295633,0.10808458519997),.UNSPECIFIED.)
GEOMETRIC_REPRESENTATION_ITEM()
RATIONAL_B_SPLINE_SURFACE(((0.990053454406157,0.987313720921968,0.987472672298934),
(0.990053454406157,0.987313720921968,0.987472672298934),(0.990053454406157,
0.987313720921968,0.987472672298934)))
REPRESENTATION_ITEM('')
SURFACE()
);
#3531=(
BOUNDED_SURFACE()
B_SPLINE_SURFACE(1,2,((#154557,#154558,#154559),(#154560,#154561,#154562),
(#154563,#154564,#154565)),.UNSPECIFIED.,.F.,.F.,.F.)
B_SPLINE_SURFACE_WITH_KNOTS((2,1,2),(3,3),(0.688516410521495,0.710318915638601,
1.),(0.625066077454536,0.642578551421364),.UNSPECIFIED.)
GEOMETRIC_REPRESENTATION_ITEM()
RATIONAL_B_SPLINE_SURFACE(((0.990621203777022,0.993706096834649,0.999805186472059),
(0.990621203777022,0.993706096834649,0.999805186472059),(0.990621203777022,
0.993706096834649,0.999805186472059)))
REPRESENTATION_ITEM('')
SURFACE()
);
#3532=(
BOUNDED_SURFACE()
B_SPLINE_SURFACE(1,2,((#154606,#154607,#154608),(#154609,#154610,#154611),
(#154612,#154613,#154614)),.UNSPECIFIED.,.F.,.F.,.F.)
B_SPLINE_SURFACE_WITH_KNOTS((2,1,2),(3,3),(0.688417834311866,0.710192959006958,
1.),(0.0909109506295619,0.108084585199969),.UNSPECIFIED.)
GEOMETRIC_REPRESENTATION_ITEM()
RATIONAL_B_SPLINE_SURFACE(((0.990053454406157,0.987313720921967,0.987472672298933),
(0.990053454406157,0.987313720921967,0.987472672298933),(0.990053454406157,
0.987313720921967,0.987472672298933)))
REPRESENTATION_ITEM('')
SURFACE()
);
#3533=(
BOUNDED_SURFACE()
B_SPLINE_SURFACE(1,2,((#154616,#154617,#154618),(#154619,#154620,#154621),
(#154622,#154623,#154624)),.UNSPECIFIED.,.F.,.F.,.F.)
B_SPLINE_SURFACE_WITH_KNOTS((2,1,2),(3,3),(0.688516410815659,0.710318915638127,
1.),(0.625066077454536,0.642578551421364),.UNSPECIFIED.)
GEOMETRIC_REPRESENTATION_ITEM()
RATIONAL_B_SPLINE_SURFACE(((0.990621203777022,0.993706096834649,0.999805186472059),
(0.990621203777022,0.993706096834649,0.999805186472059),(0.990621203777022,
0.993706096834649,0.999805186472059)))
REPRESENTATION_ITEM('')
SURFACE()
);
#3534=(
BOUNDED_SURFACE()
B_SPLINE_SURFACE(1,2,((#154665,#154666,#154667),(#154668,#154669,#154670),
(#154671,#154672,#154673)),.UNSPECIFIED.,.F.,.F.,.F.)
B_SPLINE_SURFACE_WITH_KNOTS((2,1,2),(3,3),(0.688417834306651,0.71019295900648,
1.),(0.0909109506295634,0.108084585199969),.UNSPECIFIED.)
GEOMETRIC_REPRESENTATION_ITEM()
RATIONAL_B_SPLINE_SURFACE(((0.990053454406157,0.987313720921968,0.987472672298934),
(0.990053454406157,0.987313720921968,0.987472672298934),(0.990053454406157,
0.987313720921968,0.987472672298934)))
REPRESENTATION_ITEM('')
SURFACE()
);
#3535=(
BOUNDED_SURFACE()
B_SPLINE_SURFACE(1,2,((#154675,#154676,#154677),(#154678,#154679,#154680),
(#154681,#154682,#154683)),.UNSPECIFIED.,.F.,.F.,.F.)
B_SPLINE_SURFACE_WITH_KNOTS((2,1,2),(3,3),(0.688516410441904,0.710318915638384,
1.),(0.625066077454536,0.642578551421365),.UNSPECIFIED.)
GEOMETRIC_REPRESENTATION_ITEM()
RATIONAL_B_SPLINE_SURFACE(((0.990621203777022,0.993706096834649,0.999805186472059),
(0.990621203777022,0.993706096834649,0.999805186472059),(0.990621203777022,
0.993706096834649,0.999805186472059)))
REPRESENTATION_ITEM('')
SURFACE()
);
#3536=(
BOUNDED_SURFACE()
B_SPLINE_SURFACE(1,2,((#154724,#154725,#154726),(#154727,#154728,#154729),
(#154730,#154731,#154732)),.UNSPECIFIED.,.F.,.F.,.F.)
B_SPLINE_SURFACE_WITH_KNOTS((2,1,2),(3,3),(0.688417834456928,0.710192959006737,
1.),(0.0909109506295919,0.108084585199969),.UNSPECIFIED.)
GEOMETRIC_REPRESENTATION_ITEM()
RATIONAL_B_SPLINE_SURFACE(((0.990053454406148,0.987313720921968,0.987472672298934),
(0.990053454406148,0.987313720921968,0.987472672298934),(0.990053454406148,
0.987313720921968,0.987472672298934)))
REPRESENTATION_ITEM('')
SURFACE()
);
#3537=(
BOUNDED_SURFACE()
B_SPLINE_SURFACE(1,2,((#154734,#154735,#154736),(#154737,#154738,#154739),
(#154740,#154741,#154742)),.UNSPECIFIED.,.F.,.F.,.F.)
B_SPLINE_SURFACE_WITH_KNOTS((2,1,2),(3,3),(0.688516410585266,0.710318915637217,
1.),(0.625066077454536,0.642578551421364),.UNSPECIFIED.)
GEOMETRIC_REPRESENTATION_ITEM()
RATIONAL_B_SPLINE_SURFACE(((0.990621203777022,0.993706096834649,0.999805186472059),
(0.990621203777022,0.993706096834649,0.999805186472059),(0.990621203777022,
0.993706096834649,0.999805186472059)))
REPRESENTATION_ITEM('')
SURFACE()
);
#3538=(
BOUNDED_SURFACE()
B_SPLINE_SURFACE(1,2,((#154783,#154784,#154785),(#154786,#154787,#154788),
(#154789,#154790,#154791)),.UNSPECIFIED.,.F.,.F.,.F.)
B_SPLINE_SURFACE_WITH_KNOTS((2,1,2),(3,3),(0.688417834295043,0.710192959005572,
1.),(0.0909109506295583,0.10808458519997),.UNSPECIFIED.)
GEOMETRIC_REPRESENTATION_ITEM()
RATIONAL_B_SPLINE_SURFACE(((0.990053454406159,0.987313720921968,0.987472672298934),
(0.990053454406159,0.987313720921968,0.987472672298934),(0.990053454406159,
0.987313720921968,0.987472672298934)))
REPRESENTATION_ITEM('')
SURFACE()
);
#3539=(
BOUNDED_SURFACE()
B_SPLINE_SURFACE(1,2,((#154793,#154794,#154795),(#154796,#154797,#154798),
(#154799,#154800,#154801)),.UNSPECIFIED.,.F.,.F.,.F.)
B_SPLINE_SURFACE_WITH_KNOTS((2,1,2),(3,3),(0.688516410846974,0.710318915638875,
1.),(0.625066077454536,0.642578551421364),.UNSPECIFIED.)
GEOMETRIC_REPRESENTATION_ITEM()
RATIONAL_B_SPLINE_SURFACE(((0.990621203777022,0.993706096834649,0.999805186472059),
(0.990621203777022,0.993706096834649,0.999805186472059),(0.990621203777022,
0.993706096834649,0.999805186472059)))
REPRESENTATION_ITEM('')
SURFACE()
);
#3540=(
BOUNDED_SURFACE()
B_SPLINE_SURFACE(1,2,((#154842,#154843,#154844),(#154845,#154846,#154847),
(#154848,#154849,#154850)),.UNSPECIFIED.,.F.,.F.,.F.)
B_SPLINE_SURFACE_WITH_KNOTS((2,1,2),(3,3),(0.688417834346889,0.710192959007236,
1.),(0.0909109506295931,0.108084585199969),.UNSPECIFIED.)
GEOMETRIC_REPRESENTATION_ITEM()
RATIONAL_B_SPLINE_SURFACE(((0.990053454406148,0.987313720921968,0.987472672298934),
(0.990053454406148,0.987313720921968,0.987472672298934),(0.990053454406148,
0.987313720921968,0.987472672298934)))
REPRESENTATION_ITEM('')
SURFACE()
);
#3541=(
BOUNDED_SURFACE()
B_SPLINE_SURFACE(1,2,((#154852,#154853,#154854),(#154855,#154856,#154857),
(#154858,#154859,#154860)),.UNSPECIFIED.,.F.,.F.,.F.)
B_SPLINE_SURFACE_WITH_KNOTS((2,1,2),(3,3),(0.688516410539477,0.710318915638995,
1.),(0.625066077454536,0.642578551421364),.UNSPECIFIED.)
GEOMETRIC_REPRESENTATION_ITEM()
RATIONAL_B_SPLINE_SURFACE(((0.990621203777022,0.993706096834649,0.999805186472059),
(0.990621203777022,0.993706096834649,0.999805186472059),(0.990621203777022,
0.993706096834649,0.999805186472059)))
REPRESENTATION_ITEM('')
SURFACE()
);
#3542=(
BOUNDED_SURFACE()
B_SPLINE_SURFACE(1,2,((#154868,#154869,#154870),(#154871,#154872,#154873),
(#154874,#154875,#154876)),.UNSPECIFIED.,.F.,.F.,.F.)
B_SPLINE_SURFACE_WITH_KNOTS((2,1,2),(3,3),(0.688417834323998,0.710192959007358,
1.),(0.0909109506295931,0.108084585199969),.UNSPECIFIED.)
GEOMETRIC_REPRESENTATION_ITEM()
RATIONAL_B_SPLINE_SURFACE(((0.990053454406148,0.987313720921968,0.987472672298934),
(0.990053454406148,0.987313720921968,0.987472672298934),(0.990053454406148,
0.987313720921968,0.987472672298934)))
REPRESENTATION_ITEM('')
SURFACE()
);
#3543=(
BOUNDED_SURFACE()
B_SPLINE_SURFACE(1,2,((#154878,#154879,#154880),(#154881,#154882,#154883),
(#154884,#154885,#154886)),.UNSPECIFIED.,.F.,.F.,.F.)
B_SPLINE_SURFACE_WITH_KNOTS((2,1,2),(3,3),(0.688516410871803,0.710318915638144,
1.),(0.625066077454538,0.642578551421364),.UNSPECIFIED.)
GEOMETRIC_REPRESENTATION_ITEM()
RATIONAL_B_SPLINE_SURFACE(((0.990621203777022,0.99370609683465,0.999805186472059),
(0.990621203777022,0.99370609683465,0.999805186472059),(0.990621203777022,
0.99370609683465,0.999805186472059)))
REPRESENTATION_ITEM('')
SURFACE()
);
#3544=(
BOUNDED_SURFACE()
B_SPLINE_SURFACE(1,2,((#154927,#154928,#154929),(#154930,#154931,#154932),
(#154933,#154934,#154935)),.UNSPECIFIED.,.F.,.F.,.F.)
B_SPLINE_SURFACE_WITH_KNOTS((2,1,2),(3,3),(0.688417834386786,0.710192959006501,
1.),(0.0909109506295578,0.108084585199971),.UNSPECIFIED.)
GEOMETRIC_REPRESENTATION_ITEM()
RATIONAL_B_SPLINE_SURFACE(((0.990053454406159,0.987313720921967,0.987472672298934),
(0.990053454406159,0.987313720921967,0.987472672298934),(0.990053454406159,
0.987313720921967,0.987472672298934)))
REPRESENTATION_ITEM('')
SURFACE()
);
#3545=(
BOUNDED_SURFACE()
B_SPLINE_SURFACE(1,2,((#154937,#154938,#154939),(#154940,#154941,#154942),
(#154943,#154944,#154945)),.UNSPECIFIED.,.F.,.F.,.F.)
B_SPLINE_SURFACE_WITH_KNOTS((2,1,2),(3,3),(0.688516410587137,0.710318915639622,
1.),(0.625066077454536,0.642578551421365),.UNSPECIFIED.)
GEOMETRIC_REPRESENTATION_ITEM()
RATIONAL_B_SPLINE_SURFACE(((0.990621203777022,0.993706096834649,0.999805186472059),
(0.990621203777022,0.993706096834649,0.999805186472059),(0.990621203777022,
0.993706096834649,0.999805186472059)))
REPRESENTATION_ITEM('')
SURFACE()
);
#3546=(
BOUNDED_SURFACE()
B_SPLINE_SURFACE(1,2,((#154986,#154987,#154988),(#154989,#154990,#154991),
(#154992,#154993,#154994)),.UNSPECIFIED.,.F.,.F.,.F.)
B_SPLINE_SURFACE_WITH_KNOTS((2,1,2),(3,3),(0.688417834258306,0.710192959007977,
1.),(0.090910950629593,0.108084585199969),.UNSPECIFIED.)
GEOMETRIC_REPRESENTATION_ITEM()
RATIONAL_B_SPLINE_SURFACE(((0.990053454406148,0.987313720921968,0.987472672298934),
(0.990053454406148,0.987313720921968,0.987472672298934),(0.990053454406148,
0.987313720921968,0.987472672298934)))
REPRESENTATION_ITEM('')
SURFACE()
);
#3547=(
BOUNDED_SURFACE()
B_SPLINE_SURFACE(1,2,((#154996,#154997,#154998),(#154999,#155000,#155001),
(#155002,#155003,#155004)),.UNSPECIFIED.,.F.,.F.,.F.)
B_SPLINE_SURFACE_WITH_KNOTS((2,1,2),(3,3),(0.688516410278139,0.710318915638757,
1.),(0.625066077454536,0.642578551421365),.UNSPECIFIED.)
GEOMETRIC_REPRESENTATION_ITEM()
RATIONAL_B_SPLINE_SURFACE(((0.990621203777022,0.993706096834649,0.999805186472059),
(0.990621203777022,0.993706096834649,0.999805186472059),(0.990621203777022,
0.993706096834649,0.999805186472059)))
REPRESENTATION_ITEM('')
SURFACE()
);
#3548=(
BOUNDED_SURFACE()
B_SPLINE_SURFACE(1,2,((#155045,#155046,#155047),(#155048,#155049,#155050),
(#155051,#155052,#155053)),.UNSPECIFIED.,.F.,.F.,.F.)
B_SPLINE_SURFACE_WITH_KNOTS((2,1,2),(3,3),(0.68841783418438,0.710192959007111,
1.),(0.0909109506295945,0.108084585199969),.UNSPECIFIED.)
GEOMETRIC_REPRESENTATION_ITEM()
RATIONAL_B_SPLINE_SURFACE(((0.990053454406147,0.987313720921968,0.987472672298934),
(0.990053454406147,0.987313720921968,0.987472672298934),(0.990053454406147,
0.987313720921968,0.987472672298934)))
REPRESENTATION_ITEM('')
SURFACE()
);
#3549=(
BOUNDED_SURFACE()
B_SPLINE_SURFACE(1,2,((#155055,#155056,#155057),(#155058,#155059,#155060),
(#155061,#155062,#155063)),.UNSPECIFIED.,.F.,.F.,.F.)
B_SPLINE_SURFACE_WITH_KNOTS((2,1,2),(3,3),(0.688516410418622,0.710318915639854,
1.),(0.625066077454535,0.642578551421364),.UNSPECIFIED.)
GEOMETRIC_REPRESENTATION_ITEM()
RATIONAL_B_SPLINE_SURFACE(((0.990621203777021,0.993706096834649,0.999805186472059),
(0.990621203777021,0.993706096834649,0.999805186472059),(0.990621203777021,
0.993706096834649,0.999805186472059)))
REPRESENTATION_ITEM('')
SURFACE()
);
#3550=(
BOUNDED_SURFACE()
B_SPLINE_SURFACE(1,2,((#155104,#155105,#155106),(#155107,#155108,#155109),
(#155110,#155111,#155112)),.UNSPECIFIED.,.F.,.F.,.F.)
B_SPLINE_SURFACE_WITH_KNOTS((2,1,2),(3,3),(0.688417834637952,0.710192959008443,
1.),(0.0909109506295929,0.10808458519997),.UNSPECIFIED.)
GEOMETRIC_REPRESENTATION_ITEM()
RATIONAL_B_SPLINE_SURFACE(((0.990053454406148,0.987313720921968,0.987472672298934),
(0.990053454406148,0.987313720921968,0.987472672298934),(0.990053454406148,
0.987313720921968,0.987472672298934)))
REPRESENTATION_ITEM('')
SURFACE()
);
#3551=(
BOUNDED_SURFACE()
B_SPLINE_SURFACE(1,2,((#155114,#155115,#155116),(#155117,#155118,#155119),
(#155120,#155121,#155122)),.UNSPECIFIED.,.F.,.F.,.F.)
B_SPLINE_SURFACE_WITH_KNOTS((2,1,2),(3,3),(0.688516410561936,0.710318915640085,
1.),(0.625066077454535,0.642578551421364),.UNSPECIFIED.)
GEOMETRIC_REPRESENTATION_ITEM()
RATIONAL_B_SPLINE_SURFACE(((0.990621203777021,0.993706096834649,0.999805186472059),
(0.990621203777021,0.993706096834649,0.999805186472059),(0.990621203777021,
0.993706096834649,0.999805186472059)))
REPRESENTATION_ITEM('')
SURFACE()
);
#3552=(
BOUNDED_SURFACE()
B_SPLINE_SURFACE(1,2,((#155163,#155164,#155165),(#155166,#155167,#155168),
(#155169,#155170,#155171)),.UNSPECIFIED.,.F.,.F.,.F.)
B_SPLINE_SURFACE_WITH_KNOTS((2,1,2),(3,3),(0.688417833994755,0.71019295900844,
1.),(0.0909109506295929,0.10808458519997),.UNSPECIFIED.)
GEOMETRIC_REPRESENTATION_ITEM()
RATIONAL_B_SPLINE_SURFACE(((0.990053454406148,0.987313720921968,0.987472672298934),
(0.990053454406148,0.987313720921968,0.987472672298934),(0.990053454406148,
0.987313720921968,0.987472672298934)))
REPRESENTATION_ITEM('')
SURFACE()
);
#3553=(
BOUNDED_SURFACE()
B_SPLINE_SURFACE(1,2,((#155173,#155174,#155175),(#155176,#155177,#155178),
(#155179,#155180,#155181)),.UNSPECIFIED.,.F.,.F.,.F.)
B_SPLINE_SURFACE_WITH_KNOTS((2,1,2),(3,3),(0.688516410541635,0.710318915640077,
1.),(0.625066077454535,0.642578551421363),.UNSPECIFIED.)
GEOMETRIC_REPRESENTATION_ITEM()
RATIONAL_B_SPLINE_SURFACE(((0.990621203777021,0.993706096834649,0.999805186472059),
(0.990621203777021,0.993706096834649,0.999805186472059),(0.990621203777021,
0.993706096834649,0.999805186472059)))
REPRESENTATION_ITEM('')
SURFACE()
);
#3554=(
BOUNDED_SURFACE()
B_SPLINE_SURFACE(1,2,((#155222,#155223,#155224),(#155225,#155226,#155227),
(#155228,#155229,#155230)),.UNSPECIFIED.,.F.,.F.,.F.)
B_SPLINE_SURFACE_WITH_KNOTS((2,1,2),(3,3),(0.688417834118971,0.710192959008438,
1.),(0.0909109506295931,0.10808458519997),.UNSPECIFIED.)
GEOMETRIC_REPRESENTATION_ITEM()
RATIONAL_B_SPLINE_SURFACE(((0.990053454406148,0.987313720921968,0.987472672298933),
(0.990053454406148,0.987313720921968,0.987472672298933),(0.990053454406148,
0.987313720921968,0.987472672298933)))
REPRESENTATION_ITEM('')
SURFACE()
);
#3555=(
BOUNDED_SURFACE()
B_SPLINE_SURFACE(1,2,((#155232,#155233,#155234),(#155235,#155236,#155237),
(#155238,#155239,#155240)),.UNSPECIFIED.,.F.,.F.,.F.)
B_SPLINE_SURFACE_WITH_KNOTS((2,1,2),(3,3),(0.688516410622233,0.710318915640076,
1.),(0.625066077454535,0.642578551421363),.UNSPECIFIED.)
GEOMETRIC_REPRESENTATION_ITEM()
RATIONAL_B_SPLINE_SURFACE(((0.990621203777021,0.993706096834649,0.999805186472059),
(0.990621203777021,0.993706096834649,0.999805186472059),(0.990621203777021,
0.993706096834649,0.999805186472059)))
REPRESENTATION_ITEM('')
SURFACE()
);
#3556=(
BOUNDED_SURFACE()
B_SPLINE_SURFACE(1,2,((#155281,#155282,#155283),(#155284,#155285,#155286),
(#155287,#155288,#155289)),.UNSPECIFIED.,.F.,.F.,.F.)
B_SPLINE_SURFACE_WITH_KNOTS((2,1,2),(3,3),(0.688417834145499,0.710192959008441,
1.),(0.090910950629593,0.10808458519997),.UNSPECIFIED.)
GEOMETRIC_REPRESENTATION_ITEM()
RATIONAL_B_SPLINE_SURFACE(((0.990053454406148,0.987313720921968,0.987472672298934),
(0.990053454406148,0.987313720921968,0.987472672298934),(0.990053454406148,
0.987313720921968,0.987472672298934)))
REPRESENTATION_ITEM('')
SURFACE()
);
#3557=(
BOUNDED_SURFACE()
B_SPLINE_SURFACE(1,2,((#155316,#155317,#155318),(#155319,#155320,#155321),
(#155322,#155323,#155324)),.UNSPECIFIED.,.F.,.F.,.F.)
B_SPLINE_SURFACE_WITH_KNOTS((2,1,2),(3,3),(0.688516412901942,0.710318915639752,
1.),(0.625066077454535,0.642578551421363),.UNSPECIFIED.)
GEOMETRIC_REPRESENTATION_ITEM()
RATIONAL_B_SPLINE_SURFACE(((0.990621203777021,0.993706096834649,0.999805186472059),
(0.990621203777021,0.993706096834649,0.999805186472059),(0.990621203777021,
0.993706096834649,0.999805186472059)))
REPRESENTATION_ITEM('')
SURFACE()
);
#3558=(
BOUNDED_SURFACE()
B_SPLINE_SURFACE(1,2,((#155326,#155327,#155328),(#155329,#155330,#155331)),
 .UNSPECIFIED.,.F.,.F.,.F.)
B_SPLINE_SURFACE_WITH_KNOTS((2,2),(3,3),(0.71031891564007,1.),(0.125066077454536,
0.142578551421365),.UNSPECIFIED.)
GEOMETRIC_REPRESENTATION_ITEM()
RATIONAL_B_SPLINE_SURFACE(((0.990621203777022,0.993706096834649,0.999805186472059),
(0.990621203777022,0.993706096834649,0.999805186472059)))
REPRESENTATION_ITEM('')
SURFACE()
);
#3559=(
BOUNDED_SURFACE()
B_SPLINE_SURFACE(1,2,((#155340,#155341,#155342),(#155343,#155344,#155345)),
 .UNSPECIFIED.,.F.,.F.,.F.)
B_SPLINE_SURFACE_WITH_KNOTS((2,2),(3,3),(0.710192959008436,1.),(0.590910950629593,
0.608084585199969),.UNSPECIFIED.)
GEOMETRIC_REPRESENTATION_ITEM()
RATIONAL_B_SPLINE_SURFACE(((0.990053454406147,0.987313720921968,0.987472672298934),
(0.990053454406147,0.987313720921968,0.987472672298934)))
REPRESENTATION_ITEM('')
SURFACE()
);
#3560=(
BOUNDED_SURFACE()
B_SPLINE_SURFACE(1,2,((#155354,#155355,#155356),(#155357,#155358,#155359)),
 .UNSPECIFIED.,.F.,.F.,.F.)
B_SPLINE_SURFACE_WITH_KNOTS((2,2),(3,3),(0.71031891564008,1.),(0.125066077454536,
0.142578551421364),.UNSPECIFIED.)
GEOMETRIC_REPRESENTATION_ITEM()
RATIONAL_B_SPLINE_SURFACE(((0.990621203777022,0.993706096834649,0.999805186472059),
(0.990621203777022,0.993706096834649,0.999805186472059)))
REPRESENTATION_ITEM('')
SURFACE()
);
#3561=(
BOUNDED_SURFACE()
B_SPLINE_SURFACE(1,2,((#155361,#155362,#155363),(#155364,#155365,#155366)),
 .UNSPECIFIED.,.F.,.F.,.F.)
B_SPLINE_SURFACE_WITH_KNOTS((2,2),(3,3),(0.710192959008444,1.),(0.590910950629471,
0.60808458519997),.UNSPECIFIED.)
GEOMETRIC_REPRESENTATION_ITEM()
RATIONAL_B_SPLINE_SURFACE(((0.990053454406186,0.987313720921966,0.987472672298933),
(0.990053454406186,0.987313720921966,0.987472672298933)))
REPRESENTATION_ITEM('')
SURFACE()
);
#3562=(
BOUNDED_SURFACE()
B_SPLINE_SURFACE(1,2,((#155375,#155376,#155377),(#155378,#155379,#155380)),
 .UNSPECIFIED.,.F.,.F.,.F.)
B_SPLINE_SURFACE_WITH_KNOTS((2,2),(3,3),(0.710318915640072,1.),(0.125066077454536,
0.142578551421364),.UNSPECIFIED.)
GEOMETRIC_REPRESENTATION_ITEM()
RATIONAL_B_SPLINE_SURFACE(((0.990621203777022,0.993706096834649,0.999805186472059),
(0.990621203777022,0.993706096834649,0.999805186472059)))
REPRESENTATION_ITEM('')
SURFACE()
);
#3563=(
BOUNDED_SURFACE()
B_SPLINE_SURFACE(1,2,((#155382,#155383,#155384),(#155385,#155386,#155387)),
 .UNSPECIFIED.,.F.,.F.,.F.)
B_SPLINE_SURFACE_WITH_KNOTS((2,2),(3,3),(0.710192959008435,1.),(0.590910950629581,
0.60808458519997),.UNSPECIFIED.)
GEOMETRIC_REPRESENTATION_ITEM()
RATIONAL_B_SPLINE_SURFACE(((0.990053454406151,0.987313720921968,0.987472672298934),
(0.990053454406151,0.987313720921968,0.987472672298934)))
REPRESENTATION_ITEM('')
SURFACE()
);
#3564=(
BOUNDED_SURFACE()
B_SPLINE_SURFACE(1,2,((#155396,#155397,#155398),(#155399,#155400,#155401)),
 .UNSPECIFIED.,.F.,.F.,.F.)
B_SPLINE_SURFACE_WITH_KNOTS((2,2),(3,3),(0.710318915640081,1.),(0.125066077454536,
0.142578551421363),.UNSPECIFIED.)
GEOMETRIC_REPRESENTATION_ITEM()
RATIONAL_B_SPLINE_SURFACE(((0.990621203777022,0.993706096834649,0.999805186472059),
(0.990621203777022,0.993706096834649,0.999805186472059)))
REPRESENTATION_ITEM('')
SURFACE()
);
#3565=(
BOUNDED_SURFACE()
B_SPLINE_SURFACE(1,2,((#155403,#155404,#155405),(#155406,#155407,#155408)),
 .UNSPECIFIED.,.F.,.F.,.F.)
B_SPLINE_SURFACE_WITH_KNOTS((2,2),(3,3),(0.710192959008441,1.),(0.59091095062936,
0.608084585199972),.UNSPECIFIED.)
GEOMETRIC_REPRESENTATION_ITEM()
RATIONAL_B_SPLINE_SURFACE(((0.990053454406222,0.987313720921965,0.987472672298933),
(0.990053454406222,0.987313720921965,0.987472672298933)))
REPRESENTATION_ITEM('')
SURFACE()
);
#3566=(
BOUNDED_SURFACE()
B_SPLINE_SURFACE(1,2,((#155417,#155418,#155419),(#155420,#155421,#155422)),
 .UNSPECIFIED.,.F.,.F.,.F.)
B_SPLINE_SURFACE_WITH_KNOTS((2,2),(3,3),(0.710318915640076,1.),(0.125066077454535,
0.142578551421363),.UNSPECIFIED.)
GEOMETRIC_REPRESENTATION_ITEM()
RATIONAL_B_SPLINE_SURFACE(((0.990621203777021,0.993706096834649,0.999805186472058),
(0.990621203777021,0.993706096834649,0.999805186472058)))
REPRESENTATION_ITEM('')
SURFACE()
);
#3567=(
BOUNDED_SURFACE()
B_SPLINE_SURFACE(1,2,((#155424,#155425,#155426),(#155427,#155428,#155429)),
 .UNSPECIFIED.,.F.,.F.,.F.)
B_SPLINE_SURFACE_WITH_KNOTS((2,2),(3,3),(0.71019295900844,1.),(0.590910950629587,
0.608084585199971),.UNSPECIFIED.)
GEOMETRIC_REPRESENTATION_ITEM()
RATIONAL_B_SPLINE_SURFACE(((0.99005345440615,0.987313720921968,0.987472672298934),
(0.990053454406149,0.987313720921967,0.987472672298933)))
REPRESENTATION_ITEM('')
SURFACE()
);
#3568=(
BOUNDED_SURFACE()
B_SPLINE_SURFACE(1,2,((#155438,#155439,#155440),(#155441,#155442,#155443)),
 .UNSPECIFIED.,.F.,.F.,.F.)
B_SPLINE_SURFACE_WITH_KNOTS((2,2),(3,3),(0.710318915640084,1.),(0.125066077454535,
0.142578551421363),.UNSPECIFIED.)
GEOMETRIC_REPRESENTATION_ITEM()
RATIONAL_B_SPLINE_SURFACE(((0.990621203777021,0.993706096834649,0.999805186472059),
(0.990621203777021,0.993706096834649,0.999805186472059)))
REPRESENTATION_ITEM('')
SURFACE()
);
#3569=(
BOUNDED_SURFACE()
B_SPLINE_SURFACE(1,2,((#155445,#155446,#155447),(#155448,#155449,#155450)),
 .UNSPECIFIED.,.F.,.F.,.F.)
B_SPLINE_SURFACE_WITH_KNOTS((2,2),(3,3),(0.71019295900844,1.),(0.590910950629178,
0.608084585199973),.UNSPECIFIED.)
GEOMETRIC_REPRESENTATION_ITEM()
RATIONAL_B_SPLINE_SURFACE(((0.99005345440628,0.987313720921964,0.987472672298934),
(0.99005345440628,0.987313720921964,0.987472672298934)))
REPRESENTATION_ITEM('')
SURFACE()
);
#3570=(
BOUNDED_SURFACE()
B_SPLINE_SURFACE(1,2,((#155459,#155460,#155461),(#155462,#155463,#155464)),
 .UNSPECIFIED.,.F.,.F.,.F.)
B_SPLINE_SURFACE_WITH_KNOTS((2,2),(3,3),(0.710318915640074,1.),(0.125066077454535,
0.142578551421363),.UNSPECIFIED.)
GEOMETRIC_REPRESENTATION_ITEM()
RATIONAL_B_SPLINE_SURFACE(((0.990621203777021,0.993706096834649,0.999805186472059),
(0.990621203777021,0.993706096834649,0.999805186472059)))
REPRESENTATION_ITEM('')
SURFACE()
);
#3571=(
BOUNDED_SURFACE()
B_SPLINE_SURFACE(1,2,((#155466,#155467,#155468),(#155469,#155470,#155471)),
 .UNSPECIFIED.,.F.,.F.,.F.)
B_SPLINE_SURFACE_WITH_KNOTS((2,2),(3,3),(0.71019295900844,1.),(0.590910950629594,
0.60808458519997),.UNSPECIFIED.)
GEOMETRIC_REPRESENTATION_ITEM()
RATIONAL_B_SPLINE_SURFACE(((0.990053454406147,0.987313720921968,0.987472672298933),
(0.990053454406147,0.987313720921968,0.987472672298933)))
REPRESENTATION_ITEM('')
SURFACE()
);
#3572=(
BOUNDED_SURFACE()
B_SPLINE_SURFACE(1,2,((#155480,#155481,#155482),(#155483,#155484,#155485)),
 .UNSPECIFIED.,.F.,.F.,.F.)
B_SPLINE_SURFACE_WITH_KNOTS((2,2),(3,3),(0.710318915640075,1.),(0.125066077454535,
0.142578551421363),.UNSPECIFIED.)
GEOMETRIC_REPRESENTATION_ITEM()
RATIONAL_B_SPLINE_SURFACE(((0.990621203777021,0.993706096834649,0.999805186472059),
(0.990621203777021,0.993706096834649,0.999805186472059)))
REPRESENTATION_ITEM('')
SURFACE()
);
#3573=(
BOUNDED_SURFACE()
B_SPLINE_SURFACE(1,2,((#155487,#155488,#155489),(#155490,#155491,#155492)),
 .UNSPECIFIED.,.F.,.F.,.F.)
B_SPLINE_SURFACE_WITH_KNOTS((2,2),(3,3),(0.71019295900844,1.),(0.590910950629584,
0.608084585199971),.UNSPECIFIED.)
GEOMETRIC_REPRESENTATION_ITEM()
RATIONAL_B_SPLINE_SURFACE(((0.99005345440615,0.987313720921968,0.987472672298934),
(0.99005345440615,0.987313720921968,0.987472672298934)))
REPRESENTATION_ITEM('')
SURFACE()
);
#3574=(
BOUNDED_SURFACE()
B_SPLINE_SURFACE(1,2,((#155501,#155502,#155503),(#155504,#155505,#155506)),
 .UNSPECIFIED.,.F.,.F.,.F.)
B_SPLINE_SURFACE_WITH_KNOTS((2,2),(3,3),(0.710318915640083,1.),(0.125066077454536,
0.142578551421363),.UNSPECIFIED.)
GEOMETRIC_REPRESENTATION_ITEM()
RATIONAL_B_SPLINE_SURFACE(((0.990621203777021,0.993706096834649,0.999805186472059),
(0.990621203777021,0.993706096834649,0.999805186472059)))
REPRESENTATION_ITEM('')
SURFACE()
);
#3575=(
BOUNDED_SURFACE()
B_SPLINE_SURFACE(1,2,((#155508,#155509,#155510),(#155511,#155512,#155513)),
 .UNSPECIFIED.,.F.,.F.,.F.)
B_SPLINE_SURFACE_WITH_KNOTS((2,2),(3,3),(0.710192959008443,1.),(0.590910950629594,
0.608084585199971),.UNSPECIFIED.)
GEOMETRIC_REPRESENTATION_ITEM()
RATIONAL_B_SPLINE_SURFACE(((0.990053454406147,0.987313720921968,0.987472672298934),
(0.990053454406147,0.987313720921968,0.987472672298934)))
REPRESENTATION_ITEM('')
SURFACE()
);
#3576=(
BOUNDED_SURFACE()
B_SPLINE_SURFACE(1,2,((#155522,#155523,#155524),(#155525,#155526,#155527)),
 .UNSPECIFIED.,.F.,.F.,.F.)
B_SPLINE_SURFACE_WITH_KNOTS((2,2),(3,3),(0.710318915640079,1.),(0.125066077454535,
0.142578551421363),.UNSPECIFIED.)
GEOMETRIC_REPRESENTATION_ITEM()
RATIONAL_B_SPLINE_SURFACE(((0.990621203777021,0.993706096834649,0.999805186472059),
(0.990621203777021,0.993706096834649,0.999805186472059)))
REPRESENTATION_ITEM('')
SURFACE()
);
#3577=(
BOUNDED_SURFACE()
B_SPLINE_SURFACE(1,2,((#155529,#155530,#155531),(#155532,#155533,#155534)),
 .UNSPECIFIED.,.F.,.F.,.F.)
B_SPLINE_SURFACE_WITH_KNOTS((2,2),(3,3),(0.710192959008436,1.),(0.590910950629279,
0.608084585199973),.UNSPECIFIED.)
GEOMETRIC_REPRESENTATION_ITEM()
RATIONAL_B_SPLINE_SURFACE(((0.990053454406248,0.987313720921964,0.987472672298934),
(0.990053454406248,0.987313720921964,0.987472672298934)))
REPRESENTATION_ITEM('')
SURFACE()
);
#3578=(
BOUNDED_SURFACE()
B_SPLINE_SURFACE(1,2,((#155543,#155544,#155545),(#155546,#155547,#155548)),
 .UNSPECIFIED.,.F.,.F.,.F.)
B_SPLINE_SURFACE_WITH_KNOTS((2,2),(3,3),(0.710318915640077,1.),(0.125066077454535,
0.142578551421363),.UNSPECIFIED.)
GEOMETRIC_REPRESENTATION_ITEM()
RATIONAL_B_SPLINE_SURFACE(((0.990621203777021,0.993706096834649,0.999805186472059),
(0.990621203777021,0.993706096834649,0.999805186472059)))
REPRESENTATION_ITEM('')
SURFACE()
);
#3579=(
BOUNDED_SURFACE()
B_SPLINE_SURFACE(1,2,((#155550,#155551,#155552),(#155553,#155554,#155555)),
 .UNSPECIFIED.,.F.,.F.,.F.)
B_SPLINE_SURFACE_WITH_KNOTS((2,2),(3,3),(0.710192959008443,1.),(0.590910950629594,
0.608084585199971),.UNSPECIFIED.)
GEOMETRIC_REPRESENTATION_ITEM()
RATIONAL_B_SPLINE_SURFACE(((0.990053454406147,0.987313720921967,0.987472672298933),
(0.990053454406147,0.987313720921967,0.987472672298933)))
REPRESENTATION_ITEM('')
SURFACE()
);
#3580=(
BOUNDED_SURFACE()
B_SPLINE_SURFACE(1,2,((#155564,#155565,#155566),(#155567,#155568,#155569)),
 .UNSPECIFIED.,.F.,.F.,.F.)
B_SPLINE_SURFACE_WITH_KNOTS((2,2),(3,3),(0.710318915640078,1.),(0.125066077454536,
0.142578551421364),.UNSPECIFIED.)
GEOMETRIC_REPRESENTATION_ITEM()
RATIONAL_B_SPLINE_SURFACE(((0.990621203777021,0.993706096834649,0.999805186472059),
(0.990621203777021,0.993706096834649,0.999805186472059)))
REPRESENTATION_ITEM('')
SURFACE()
);
#3581=(
BOUNDED_SURFACE()
B_SPLINE_SURFACE(1,2,((#155571,#155572,#155573),(#155574,#155575,#155576)),
 .UNSPECIFIED.,.F.,.F.,.F.)
B_SPLINE_SURFACE_WITH_KNOTS((2,2),(3,3),(0.710192959008436,1.),(0.590910950629528,
0.608084585199971),.UNSPECIFIED.)
GEOMETRIC_REPRESENTATION_ITEM()
RATIONAL_B_SPLINE_SURFACE(((0.990053454406168,0.987313720921967,0.987472672298934),
(0.990053454406168,0.987313720921967,0.987472672298934)))
REPRESENTATION_ITEM('')
SURFACE()
);
#3582=(
BOUNDED_SURFACE()
B_SPLINE_SURFACE(1,2,((#155585,#155586,#155587),(#155588,#155589,#155590)),
 .UNSPECIFIED.,.F.,.F.,.F.)
B_SPLINE_SURFACE_WITH_KNOTS((2,2),(3,3),(0.710318915640075,1.),(0.125066077454535,
0.142578551421363),.UNSPECIFIED.)
GEOMETRIC_REPRESENTATION_ITEM()
RATIONAL_B_SPLINE_SURFACE(((0.990621203777021,0.993706096834648,0.999805186472059),
(0.990621203777021,0.993706096834648,0.999805186472059)))
REPRESENTATION_ITEM('')
SURFACE()
);
#3583=(
BOUNDED_SURFACE()
B_SPLINE_SURFACE(1,2,((#155592,#155593,#155594),(#155595,#155596,#155597)),
 .UNSPECIFIED.,.F.,.F.,.F.)
B_SPLINE_SURFACE_WITH_KNOTS((2,2),(3,3),(0.710192959008441,1.),(0.590910950629594,
0.60808458519997),.UNSPECIFIED.)
GEOMETRIC_REPRESENTATION_ITEM()
RATIONAL_B_SPLINE_SURFACE(((0.990053454406147,0.987313720921967,0.987472672298933),
(0.990053454406147,0.987313720921968,0.987472672298933)))
REPRESENTATION_ITEM('')
SURFACE()
);
#3584=(
BOUNDED_SURFACE()
B_SPLINE_SURFACE(1,2,((#155606,#155607,#155608),(#155609,#155610,#155611)),
 .UNSPECIFIED.,.F.,.F.,.F.)
B_SPLINE_SURFACE_WITH_KNOTS((2,2),(3,3),(0.71031891564008,1.),(0.125066077454535,
0.142578551421364),.UNSPECIFIED.)
GEOMETRIC_REPRESENTATION_ITEM()
RATIONAL_B_SPLINE_SURFACE(((0.990621203777021,0.993706096834649,0.999805186472059),
(0.990621203777021,0.993706096834649,0.999805186472059)))
REPRESENTATION_ITEM('')
SURFACE()
);
#3585=(
BOUNDED_SURFACE()
B_SPLINE_SURFACE(1,2,((#155613,#155614,#155615),(#155616,#155617,#155618)),
 .UNSPECIFIED.,.F.,.F.,.F.)
B_SPLINE_SURFACE_WITH_KNOTS((2,2),(3,3),(0.710192959008435,1.),(0.590910950629321,
0.608084585199972),.UNSPECIFIED.)
GEOMETRIC_REPRESENTATION_ITEM()
RATIONAL_B_SPLINE_SURFACE(((0.990053454406234,0.987313720921965,0.987472672298934),
(0.990053454406234,0.987313720921965,0.987472672298934)))
REPRESENTATION_ITEM('')
SURFACE()
);
#3586=(
BOUNDED_SURFACE()
B_SPLINE_SURFACE(1,2,((#155627,#155628,#155629),(#155630,#155631,#155632)),
 .UNSPECIFIED.,.F.,.F.,.F.)
B_SPLINE_SURFACE_WITH_KNOTS((2,2),(3,3),(0.710318915640079,1.),(0.125066077454536,
0.142578551421363),.UNSPECIFIED.)
GEOMETRIC_REPRESENTATION_ITEM()
RATIONAL_B_SPLINE_SURFACE(((0.990621203777021,0.993706096834649,0.999805186472059),
(0.990621203777021,0.993706096834649,0.999805186472059)))
REPRESENTATION_ITEM('')
SURFACE()
);
#3587=(
BOUNDED_SURFACE()
B_SPLINE_SURFACE(1,2,((#155634,#155635,#155636),(#155637,#155638,#155639)),
 .UNSPECIFIED.,.F.,.F.,.F.)
B_SPLINE_SURFACE_WITH_KNOTS((2,2),(3,3),(0.710192959008445,1.),(0.590910950629594,
0.60808458519997),.UNSPECIFIED.)
GEOMETRIC_REPRESENTATION_ITEM()
RATIONAL_B_SPLINE_SURFACE(((0.990053454406147,0.987313720921968,0.987472672298933),
(0.990053454406147,0.987313720921968,0.987472672298933)))
REPRESENTATION_ITEM('')
SURFACE()
);
#3588=(
BOUNDED_SURFACE()
B_SPLINE_SURFACE(1,2,((#155648,#155649,#155650),(#155651,#155652,#155653)),
 .UNSPECIFIED.,.F.,.F.,.F.)
B_SPLINE_SURFACE_WITH_KNOTS((2,2),(3,3),(0.71031891564008,1.),(0.125066077454535,
0.142578551421363),.UNSPECIFIED.)
GEOMETRIC_REPRESENTATION_ITEM()
RATIONAL_B_SPLINE_SURFACE(((0.990621203777021,0.993706096834649,0.999805186472059),
(0.990621203777021,0.993706096834649,0.999805186472059)))
REPRESENTATION_ITEM('')
SURFACE()
);
#3589=(
BOUNDED_SURFACE()
B_SPLINE_SURFACE(1,2,((#155655,#155656,#155657),(#155658,#155659,#155660)),
 .UNSPECIFIED.,.F.,.F.,.F.)
B_SPLINE_SURFACE_WITH_KNOTS((2,2),(3,3),(0.710192959008442,1.),(0.590910950629594,
0.60808458519997),.UNSPECIFIED.)
GEOMETRIC_REPRESENTATION_ITEM()
RATIONAL_B_SPLINE_SURFACE(((0.990053454406147,0.987313720921968,0.987472672298933),
(0.990053454406147,0.987313720921968,0.987472672298933)))
REPRESENTATION_ITEM('')
SURFACE()
);
#3590=(
BOUNDED_SURFACE()
B_SPLINE_SURFACE(1,2,((#155669,#155670,#155671),(#155672,#155673,#155674)),
 .UNSPECIFIED.,.F.,.F.,.F.)
B_SPLINE_SURFACE_WITH_KNOTS((2,2),(3,3),(0.71031891564008,1.),(0.125066077454535,
0.142578551421363),.UNSPECIFIED.)
GEOMETRIC_REPRESENTATION_ITEM()
RATIONAL_B_SPLINE_SURFACE(((0.990621203777021,0.993706096834649,0.999805186472059),
(0.990621203777021,0.993706096834649,0.999805186472059)))
REPRESENTATION_ITEM('')
SURFACE()
);
#3591=(
BOUNDED_SURFACE()
B_SPLINE_SURFACE(1,2,((#155676,#155677,#155678),(#155679,#155680,#155681)),
 .UNSPECIFIED.,.F.,.F.,.F.)
B_SPLINE_SURFACE_WITH_KNOTS((2,2),(3,3),(0.710192959008445,1.),(0.590910950629594,
0.608084585199971),.UNSPECIFIED.)
GEOMETRIC_REPRESENTATION_ITEM()
RATIONAL_B_SPLINE_SURFACE(((0.990053454406147,0.987313720921968,0.987472672298934),
(0.990053454406147,0.987313720921968,0.987472672298934)))
REPRESENTATION_ITEM('')
SURFACE()
);
#3592=(
BOUNDED_SURFACE()
B_SPLINE_SURFACE(1,2,((#155690,#155691,#155692),(#155693,#155694,#155695)),
 .UNSPECIFIED.,.F.,.F.,.F.)
B_SPLINE_SURFACE_WITH_KNOTS((2,2),(3,3),(0.710318915640083,1.),(0.125066077454535,
0.142578551421363),.UNSPECIFIED.)
GEOMETRIC_REPRESENTATION_ITEM()
RATIONAL_B_SPLINE_SURFACE(((0.990621203777021,0.993706096834649,0.999805186472059),
(0.990621203777021,0.993706096834649,0.999805186472059)))
REPRESENTATION_ITEM('')
SURFACE()
);
#3593=(
BOUNDED_SURFACE()
B_SPLINE_SURFACE(1,2,((#155697,#155698,#155699),(#155700,#155701,#155702)),
 .UNSPECIFIED.,.F.,.F.,.F.)
B_SPLINE_SURFACE_WITH_KNOTS((2,2),(3,3),(0.710192959008439,1.),(0.590910950629594,
0.60808458519997),.UNSPECIFIED.)
GEOMETRIC_REPRESENTATION_ITEM()
RATIONAL_B_SPLINE_SURFACE(((0.990053454406147,0.987313720921968,0.987472672298933),
(0.990053454406147,0.987313720921968,0.987472672298933)))
REPRESENTATION_ITEM('')
SURFACE()
);
#3594=(
BOUNDED_SURFACE()
B_SPLINE_SURFACE(1,2,((#155711,#155712,#155713),(#155714,#155715,#155716)),
 .UNSPECIFIED.,.F.,.F.,.F.)
B_SPLINE_SURFACE_WITH_KNOTS((2,2),(3,3),(0.710318915639847,1.),(0.125066077454535,
0.142578551421363),.UNSPECIFIED.)
GEOMETRIC_REPRESENTATION_ITEM()
RATIONAL_B_SPLINE_SURFACE(((0.990621203777021,0.993706096834649,0.999805186472059),
(0.990621203777021,0.993706096834649,0.999805186472059)))
REPRESENTATION_ITEM('')
SURFACE()
);
#3595=(
BOUNDED_SURFACE()
B_SPLINE_SURFACE(1,2,((#155718,#155719,#155720),(#155721,#155722,#155723)),
 .UNSPECIFIED.,.F.,.F.,.F.)
B_SPLINE_SURFACE_WITH_KNOTS((2,2),(3,3),(0.710192959008435,1.),(0.590910950629594,
0.60808458519997),.UNSPECIFIED.)
GEOMETRIC_REPRESENTATION_ITEM()
RATIONAL_B_SPLINE_SURFACE(((0.990053454406147,0.987313720921968,0.987472672298933),
(0.990053454406147,0.987313720921968,0.987472672298933)))
REPRESENTATION_ITEM('')
SURFACE()
);
#3596=(
BOUNDED_SURFACE()
B_SPLINE_SURFACE(1,2,((#155732,#155733,#155734),(#155735,#155736,#155737)),
 .UNSPECIFIED.,.F.,.F.,.F.)
B_SPLINE_SURFACE_WITH_KNOTS((2,2),(3,3),(0.710318915640079,1.),(0.125066077454536,
0.142578551421364),.UNSPECIFIED.)
GEOMETRIC_REPRESENTATION_ITEM()
RATIONAL_B_SPLINE_SURFACE(((0.990621203777022,0.993706096834649,0.999805186472059),
(0.990621203777022,0.993706096834649,0.999805186472059)))
REPRESENTATION_ITEM('')
SURFACE()
);
#3597=(
BOUNDED_SURFACE()
B_SPLINE_SURFACE(1,2,((#155739,#155740,#155741),(#155742,#155743,#155744)),
 .UNSPECIFIED.,.F.,.F.,.F.)
B_SPLINE_SURFACE_WITH_KNOTS((2,2),(3,3),(0.71019295900844,1.),(0.590910950629593,
0.608084585199969),.UNSPECIFIED.)
GEOMETRIC_REPRESENTATION_ITEM()
RATIONAL_B_SPLINE_SURFACE(((0.990053454406147,0.987313720921968,0.987472672298934),
(0.990053454406147,0.987313720921968,0.987472672298934)))
REPRESENTATION_ITEM('')
SURFACE()
);
#3598=(
BOUNDED_SURFACE()
B_SPLINE_SURFACE(1,2,((#155753,#155754,#155755),(#155756,#155757,#155758)),
 .UNSPECIFIED.,.F.,.F.,.F.)
B_SPLINE_SURFACE_WITH_KNOTS((2,2),(3,3),(0.710318915640078,1.),(0.125066077454536,
0.142578551421364),.UNSPECIFIED.)
GEOMETRIC_REPRESENTATION_ITEM()
RATIONAL_B_SPLINE_SURFACE(((0.990621203777022,0.993706096834649,0.999805186472059),
(0.990621203777022,0.993706096834649,0.999805186472059)))
REPRESENTATION_ITEM('')
SURFACE()
);
#3599=(
BOUNDED_SURFACE()
B_SPLINE_SURFACE(1,2,((#155760,#155761,#155762),(#155763,#155764,#155765)),
 .UNSPECIFIED.,.F.,.F.,.F.)
B_SPLINE_SURFACE_WITH_KNOTS((2,2),(3,3),(0.710192959008301,1.),(0.590910950629528,
0.60808458519997),.UNSPECIFIED.)
GEOMETRIC_REPRESENTATION_ITEM()
RATIONAL_B_SPLINE_SURFACE(((0.990053454406168,0.987313720921967,0.987472672298934),
(0.990053454406168,0.987313720921967,0.987472672298934)))
REPRESENTATION_ITEM('')
SURFACE()
);
#3600=(
BOUNDED_SURFACE()
B_SPLINE_SURFACE(1,2,((#155774,#155775,#155776),(#155777,#155778,#155779)),
 .UNSPECIFIED.,.F.,.F.,.F.)
B_SPLINE_SURFACE_WITH_KNOTS((2,2),(3,3),(0.710318915639942,1.),(0.125066077454536,
0.142578551421366),.UNSPECIFIED.)
GEOMETRIC_REPRESENTATION_ITEM()
RATIONAL_B_SPLINE_SURFACE(((0.990621203777022,0.993706096834649,0.99980518647206),
(0.990621203777022,0.99370609683465,0.99980518647206)))
REPRESENTATION_ITEM('')
SURFACE()
);
#3601=(
BOUNDED_SURFACE()
B_SPLINE_SURFACE(1,2,((#155781,#155782,#155783),(#155784,#155785,#155786)),
 .UNSPECIFIED.,.F.,.F.,.F.)
B_SPLINE_SURFACE_WITH_KNOTS((2,2),(3,3),(0.710192959008294,1.),(0.590910950629541,
0.60808458519997),.UNSPECIFIED.)
GEOMETRIC_REPRESENTATION_ITEM()
RATIONAL_B_SPLINE_SURFACE(((0.990053454406164,0.987313720921967,0.987472672298934),
(0.990053454406164,0.987313720921967,0.987472672298934)))
REPRESENTATION_ITEM('')
SURFACE()
);
#3602=(
BOUNDED_SURFACE()
B_SPLINE_SURFACE(1,2,((#155795,#155796,#155797),(#155798,#155799,#155800)),
 .UNSPECIFIED.,.F.,.F.,.F.)
B_SPLINE_SURFACE_WITH_KNOTS((2,2),(3,3),(0.710318915639933,1.),(0.125066077454536,
0.142578551421364),.UNSPECIFIED.)
GEOMETRIC_REPRESENTATION_ITEM()
RATIONAL_B_SPLINE_SURFACE(((0.990621203777022,0.993706096834649,0.999805186472059),
(0.990621203777022,0.993706096834649,0.999805186472059)))
REPRESENTATION_ITEM('')
SURFACE()
);
#3603=(
BOUNDED_SURFACE()
B_SPLINE_SURFACE(1,2,((#155802,#155803,#155804),(#155805,#155806,#155807)),
 .UNSPECIFIED.,.F.,.F.,.F.)
B_SPLINE_SURFACE_WITH_KNOTS((2,2),(3,3),(0.710192959008284,1.),(0.590910950629593,
0.60808458519997),.UNSPECIFIED.)
GEOMETRIC_REPRESENTATION_ITEM()
RATIONAL_B_SPLINE_SURFACE(((0.990053454406147,0.987313720921968,0.987472672298934),
(0.990053454406147,0.987313720921968,0.987472672298934)))
REPRESENTATION_ITEM('')
SURFACE()
);
#3604=(
BOUNDED_SURFACE()
B_SPLINE_SURFACE(1,2,((#155816,#155817,#155818),(#155819,#155820,#155821)),
 .UNSPECIFIED.,.F.,.F.,.F.)
B_SPLINE_SURFACE_WITH_KNOTS((2,2),(3,3),(0.710318915639924,1.),(0.125066077454536,
0.142578551421364),.UNSPECIFIED.)
GEOMETRIC_REPRESENTATION_ITEM()
RATIONAL_B_SPLINE_SURFACE(((0.990621203777022,0.993706096834649,0.999805186472059),
(0.990621203777022,0.993706096834649,0.999805186472059)))
REPRESENTATION_ITEM('')
SURFACE()
);
#3605=(
BOUNDED_SURFACE()
B_SPLINE_SURFACE(1,2,((#155823,#155824,#155825),(#155826,#155827,#155828)),
 .UNSPECIFIED.,.F.,.F.,.F.)
B_SPLINE_SURFACE_WITH_KNOTS((2,2),(3,3),(0.71019295900691,1.),(0.590910950629592,
0.608084585199969),.UNSPECIFIED.)
GEOMETRIC_REPRESENTATION_ITEM()
RATIONAL_B_SPLINE_SURFACE(((0.990053454406148,0.987313720921968,0.987472672298934),
(0.990053454406148,0.987313720921968,0.987472672298934)))
REPRESENTATION_ITEM('')
SURFACE()
);
#3606=(
BOUNDED_SURFACE()
B_SPLINE_SURFACE(1,2,((#155837,#155838,#155839),(#155840,#155841,#155842)),
 .UNSPECIFIED.,.F.,.F.,.F.)
B_SPLINE_SURFACE_WITH_KNOTS((2,2),(3,3),(0.710318915638558,1.),(0.125066077454536,
0.142578551421364),.UNSPECIFIED.)
GEOMETRIC_REPRESENTATION_ITEM()
RATIONAL_B_SPLINE_SURFACE(((0.990621203777022,0.993706096834649,0.999805186472059),
(0.990621203777022,0.993706096834649,0.999805186472059)))
REPRESENTATION_ITEM('')
SURFACE()
);
#3607=(
BOUNDED_SURFACE()
B_SPLINE_SURFACE(1,2,((#155844,#155845,#155846),(#155847,#155848,#155849)),
 .UNSPECIFIED.,.F.,.F.,.F.)
B_SPLINE_SURFACE_WITH_KNOTS((2,2),(3,3),(0.710192959007976,1.),(0.59091095062944,
0.60808458519997),.UNSPECIFIED.)
GEOMETRIC_REPRESENTATION_ITEM()
RATIONAL_B_SPLINE_SURFACE(((0.990053454406197,0.987313720921966,0.987472672298934),
(0.990053454406197,0.987313720921966,0.987472672298934)))
REPRESENTATION_ITEM('')
SURFACE()
);
#3608=(
BOUNDED_SURFACE()
B_SPLINE_SURFACE(1,2,((#155858,#155859,#155860),(#155861,#155862,#155863)),
 .UNSPECIFIED.,.F.,.F.,.F.)
B_SPLINE_SURFACE_WITH_KNOTS((2,2),(3,3),(0.710318915639623,1.),(0.125066077454536,
0.142578551421364),.UNSPECIFIED.)
GEOMETRIC_REPRESENTATION_ITEM()
RATIONAL_B_SPLINE_SURFACE(((0.990621203777022,0.993706096834649,0.999805186472059),
(0.990621203777022,0.993706096834649,0.999805186472059)))
REPRESENTATION_ITEM('')
SURFACE()
);
#3609=(
BOUNDED_SURFACE()
B_SPLINE_SURFACE(1,2,((#155865,#155866,#155867),(#155868,#155869,#155870)),
 .UNSPECIFIED.,.F.,.F.,.F.)
B_SPLINE_SURFACE_WITH_KNOTS((2,2),(3,3),(0.710192959008351,1.),(0.590910950629588,
0.608084585199969),.UNSPECIFIED.)
GEOMETRIC_REPRESENTATION_ITEM()
RATIONAL_B_SPLINE_SURFACE(((0.990053454406149,0.987313720921968,0.987472672298934),
(0.990053454406149,0.987313720921968,0.987472672298934)))
REPRESENTATION_ITEM('')
SURFACE()
);
#3610=(
BOUNDED_SURFACE()
B_SPLINE_SURFACE(1,2,((#155879,#155880,#155881),(#155882,#155883,#155884)),
 .UNSPECIFIED.,.F.,.F.,.F.)
B_SPLINE_SURFACE_WITH_KNOTS((2,2),(3,3),(0.710318915639997,1.),(0.125066077454536,
0.142578551421364),.UNSPECIFIED.)
GEOMETRIC_REPRESENTATION_ITEM()
RATIONAL_B_SPLINE_SURFACE(((0.990621203777022,0.993706096834649,0.999805186472059),
(0.990621203777022,0.993706096834649,0.999805186472059)))
REPRESENTATION_ITEM('')
SURFACE()
);
#3611=(
BOUNDED_SURFACE()
B_SPLINE_SURFACE(1,2,((#155886,#155887,#155888),(#155889,#155890,#155891)),
 .UNSPECIFIED.,.F.,.F.,.F.)
B_SPLINE_SURFACE_WITH_KNOTS((2,2),(3,3),(0.71019295900836,1.),(0.590910950629593,
0.608084585199969),.UNSPECIFIED.)
GEOMETRIC_REPRESENTATION_ITEM()
RATIONAL_B_SPLINE_SURFACE(((0.990053454406147,0.987313720921968,0.987472672298934),
(0.990053454406147,0.987313720921968,0.987472672298934)))
REPRESENTATION_ITEM('')
SURFACE()
);
#3612=(
BOUNDED_SURFACE()
B_SPLINE_SURFACE(1,2,((#155900,#155901,#155902),(#155903,#155904,#155905)),
 .UNSPECIFIED.,.F.,.F.,.F.)
B_SPLINE_SURFACE_WITH_KNOTS((2,2),(3,3),(0.710318915640007,1.),(0.125066077454536,
0.142578551421364),.UNSPECIFIED.)
GEOMETRIC_REPRESENTATION_ITEM()
RATIONAL_B_SPLINE_SURFACE(((0.990621203777022,0.993706096834649,0.999805186472059),
(0.990621203777022,0.993706096834649,0.999805186472059)))
REPRESENTATION_ITEM('')
SURFACE()
);
#3613=(
BOUNDED_SURFACE()
B_SPLINE_SURFACE(1,2,((#155907,#155908,#155909),(#155910,#155911,#155912)),
 .UNSPECIFIED.,.F.,.F.,.F.)
B_SPLINE_SURFACE_WITH_KNOTS((2,2),(3,3),(0.710192959008365,1.),(0.590910950629467,
0.60808458519997),.UNSPECIFIED.)
GEOMETRIC_REPRESENTATION_ITEM()
RATIONAL_B_SPLINE_SURFACE(((0.990053454406188,0.987313720921966,0.987472672298934),
(0.990053454406188,0.987313720921966,0.987472672298934)))
REPRESENTATION_ITEM('')
SURFACE()
);
#3614=(
BOUNDED_SURFACE()
B_SPLINE_SURFACE(1,2,((#155921,#155922,#155923),(#155924,#155925,#155926)),
 .UNSPECIFIED.,.F.,.F.,.F.)
B_SPLINE_SURFACE_WITH_KNOTS((2,2),(3,3),(0.710318915640004,1.),(0.125066077454536,
0.142578551421364),.UNSPECIFIED.)
GEOMETRIC_REPRESENTATION_ITEM()
RATIONAL_B_SPLINE_SURFACE(((0.990621203777022,0.993706096834649,0.999805186472059),
(0.990621203777022,0.993706096834649,0.999805186472059)))
REPRESENTATION_ITEM('')
SURFACE()
);
#3615=(
BOUNDED_SURFACE()
B_SPLINE_SURFACE(1,2,((#155928,#155929,#155930),(#155931,#155932,#155933)),
 .UNSPECIFIED.,.F.,.F.,.F.)
B_SPLINE_SURFACE_WITH_KNOTS((2,2),(3,3),(0.71019295900844,1.),(0.590910950629373,
0.608084585199971),.UNSPECIFIED.)
GEOMETRIC_REPRESENTATION_ITEM()
RATIONAL_B_SPLINE_SURFACE(((0.990053454406218,0.987313720921966,0.987472672298934),
(0.990053454406218,0.987313720921966,0.987472672298934)))
REPRESENTATION_ITEM('')
SURFACE()
);
#3616=(
BOUNDED_SURFACE()
B_SPLINE_SURFACE(1,2,((#155935,#155936,#155937,#155938,#155939,#155940,
#155941),(#155942,#155943,#155944,#155945,#155946,#155947,#155948)),
 .UNSPECIFIED.,.F.,.F.,.F.)
B_SPLINE_SURFACE_WITH_KNOTS((2,2),(3,2,2,3),(0.,0.211537324447063),(0.642404283483249,
0.642578551421311,0.642857142857143,0.660005345227472),.UNSPECIFIED.)
GEOMETRIC_REPRESENTATION_ITEM()
RATIONAL_B_SPLINE_SURFACE(((0.999805186472022,0.999805186472022,0.999805186472022,
0.999902211834776,1.,0.993980822699462,0.990851751371594),(0.999805186472022,
0.999805186472022,0.999805186472022,0.999902211834776,1.,0.993980822699462,
0.990851751371594)))
REPRESENTATION_ITEM('')
SURFACE()
);
#3617=(
BOUNDED_SURFACE()
B_SPLINE_SURFACE(1,2,((#155955,#155956,#155957,#155958,#155959),(#155960,
#155961,#155962,#155963,#155964),(#155965,#155966,#155967,#155968,#155969)),
 .UNSPECIFIED.,.F.,.F.,.F.)
B_SPLINE_SURFACE_WITH_KNOTS((2,1,2),(3,2,3),(-0.00211445385587017,0.,0.211445385587017),
(0.0724436332512423,0.0909109506295946,0.0921216909780094),
 .UNSPECIFIED.)
GEOMETRIC_REPRESENTATION_ITEM()
RATIONAL_B_SPLINE_SURFACE(((0.999297534414571,0.992999570883536,0.990053454406147,
0.990053454406147,0.990053454406147),(0.999297534414571,0.992999570883536,
0.990053454406147,0.990053454406147,0.990053454406147),(0.999297534414571,
0.992999570883536,0.990053454406147,0.990053454406147,0.990053454406147)))
REPRESENTATION_ITEM('')
SURFACE()
);
#3618=(
BOUNDED_SURFACE()
B_SPLINE_SURFACE(1,2,((#155976,#155977,#155978,#155979,#155980,#155981,
#155982),(#155983,#155984,#155985,#155986,#155987,#155988,#155989),(#155990,
#155991,#155992,#155993,#155994,#155995,#155996)),.UNSPECIFIED.,.F.,.F.,
 .F.)
B_SPLINE_SURFACE_WITH_KNOTS((2,1,2),(3,2,2,3),(-0.00211537324447033,0.,
0.211537324447033),(0.642404283483253,0.642578551421314,0.642857142857143,
0.660005345227463),.UNSPECIFIED.)
GEOMETRIC_REPRESENTATION_ITEM()
RATIONAL_B_SPLINE_SURFACE(((0.999805186472024,0.999805186472024,0.999805186472024,
0.999902211834777,1.,0.993980822699465,0.990851751371597),(0.999805186472024,
0.999805186472024,0.999805186472024,0.999902211834777,1.,0.993980822699465,
0.990851751371597),(0.999805186472024,0.999805186472024,0.999805186472024,
0.999902211834777,1.,0.993980822699465,0.990851751371597)))
REPRESENTATION_ITEM('')
SURFACE()
);
#3619=(
BOUNDED_SURFACE()
B_SPLINE_SURFACE(1,2,((#155998,#155999,#156000,#156001,#156002),(#156003,
#156004,#156005,#156006,#156007),(#156008,#156009,#156010,#156011,#156012)),
 .UNSPECIFIED.,.F.,.F.,.F.)
B_SPLINE_SURFACE_WITH_KNOTS((2,1,2),(3,2,3),(-0.00211445385587015,0.,0.211445385587015),
(0.0724436330381796,0.0909109506295945,0.0921216911828342),
 .UNSPECIFIED.)
GEOMETRIC_REPRESENTATION_ITEM()
RATIONAL_B_SPLINE_SURFACE(((0.999297534559893,0.992999570917526,0.990053454406147,
0.990053454406147,0.990053454406147),(0.999297534559893,0.992999570917526,
0.990053454406147,0.990053454406147,0.990053454406147),(0.999297534559893,
0.992999570917527,0.990053454406147,0.990053454406147,0.990053454406147)))
REPRESENTATION_ITEM('')
SURFACE()
);
#3620=(
BOUNDED_SURFACE()
B_SPLINE_SURFACE(1,2,((#156019,#156020,#156021,#156022,#156023,#156024,
#156025),(#156026,#156027,#156028,#156029,#156030,#156031,#156032),(#156033,
#156034,#156035,#156036,#156037,#156038,#156039)),.UNSPECIFIED.,.F.,.F.,
 .F.)
B_SPLINE_SURFACE_WITH_KNOTS((2,1,2),(3,2,2,3),(-0.00211537324446618,0.,
0.211537324446618),(0.642404283483302,0.642578551421363,0.642857142857143,
0.660005345227472),.UNSPECIFIED.)
GEOMETRIC_REPRESENTATION_ITEM()
RATIONAL_B_SPLINE_SURFACE(((0.999805186472058,0.999805186472058,0.999805186472058,
0.999902211834794,1.,0.993980822699462,0.990851751371594),(0.999805186472058,
0.999805186472058,0.999805186472058,0.999902211834794,1.,0.993980822699462,
0.990851751371594),(0.999805186472058,0.999805186472058,0.999805186472058,
0.999902211834794,1.,0.993980822699462,0.990851751371594)))
REPRESENTATION_ITEM('')
SURFACE()
);
#3621=(
BOUNDED_SURFACE()
B_SPLINE_SURFACE(1,2,((#156041,#156042,#156043,#156044,#156045),(#156046,
#156047,#156048,#156049,#156050),(#156051,#156052,#156053,#156054,#156055)),
 .UNSPECIFIED.,.F.,.F.,.F.)
B_SPLINE_SURFACE_WITH_KNOTS((2,1,2),(3,2,3),(-0.00211445385587009,0.,0.211445385587009),
(0.0724436337108673,0.0909109506295944,0.0921216910718328),
 .UNSPECIFIED.)
GEOMETRIC_REPRESENTATION_ITEM()
RATIONAL_B_SPLINE_SURFACE(((0.999297534101077,0.992999570810212,0.990053454406147,
0.990053454406147,0.990053454406147),(0.999297534101077,0.992999570810212,
0.990053454406147,0.990053454406147,0.990053454406147),(0.999297534101077,
0.992999570810212,0.990053454406147,0.990053454406147,0.990053454406147)))
REPRESENTATION_ITEM('')
SURFACE()
);
#3622=(
BOUNDED_SURFACE()
B_SPLINE_SURFACE(1,2,((#156062,#156063,#156064,#156065,#156066,#156067,
#156068),(#156069,#156070,#156071,#156072,#156073,#156074,#156075),(#156076,
#156077,#156078,#156079,#156080,#156081,#156082)),.UNSPECIFIED.,.F.,.F.,
 .F.)
B_SPLINE_SURFACE_WITH_KNOTS((2,1,2),(3,2,2,3),(-0.0021153732444663,0.,0.21153732444663),
(0.642404283483301,0.642578551421362,0.642857142857143,0.660005345227463),
 .UNSPECIFIED.)
GEOMETRIC_REPRESENTATION_ITEM()
RATIONAL_B_SPLINE_SURFACE(((0.999805186472057,0.999805186472057,0.999805186472057,
0.999902211834794,1.,0.993980822699465,0.990851751371597),(0.999805186472057,
0.999805186472057,0.999805186472057,0.999902211834794,1.,0.993980822699465,
0.990851751371597),(0.999805186472057,0.999805186472057,0.999805186472057,
0.999902211834794,1.,0.993980822699465,0.990851751371597)))
REPRESENTATION_ITEM('')
SURFACE()
);
#3623=(
BOUNDED_SURFACE()
B_SPLINE_SURFACE(1,2,((#156084,#156085,#156086,#156087,#156088),(#156089,
#156090,#156091,#156092,#156093),(#156094,#156095,#156096,#156097,#156098)),
 .UNSPECIFIED.,.F.,.F.,.F.)
B_SPLINE_SURFACE_WITH_KNOTS((2,1,2),(3,2,3),(-0.00211445385587011,0.,0.211445385587011),
(0.0724436338120045,0.0909109506295944,0.0921216909413642),
 .UNSPECIFIED.)
GEOMETRIC_REPRESENTATION_ITEM()
RATIONAL_B_SPLINE_SURFACE(((0.999297534032094,0.992999570794077,0.990053454406147,
0.990053454406147,0.990053454406147),(0.999297534032094,0.992999570794077,
0.990053454406147,0.990053454406147,0.990053454406147),(0.999297534032094,
0.992999570794077,0.990053454406147,0.990053454406147,0.990053454406147)))
REPRESENTATION_ITEM('')
SURFACE()
);
#3624=(
BOUNDED_SURFACE()
B_SPLINE_SURFACE(1,2,((#156105,#156106,#156107,#156108,#156109,#156110,
#156111),(#156112,#156113,#156114,#156115,#156116,#156117,#156118),(#156119,
#156120,#156121,#156122,#156123,#156124,#156125)),.UNSPECIFIED.,.F.,.F.,
 .F.)
B_SPLINE_SURFACE_WITH_KNOTS((2,1,2),(3,2,2,3),(-0.00211537324446619,0.,
0.211537324446619),(0.642404283483302,0.642578551421363,0.642857142857143,
0.660005345227463),.UNSPECIFIED.)
GEOMETRIC_REPRESENTATION_ITEM()
RATIONAL_B_SPLINE_SURFACE(((0.999805186472058,0.999805186472058,0.999805186472058,
0.999902211834794,1.,0.993980822699465,0.990851751371597),(0.999805186472058,
0.999805186472058,0.999805186472058,0.999902211834794,1.,0.993980822699465,
0.990851751371597),(0.999805186472058,0.999805186472058,0.999805186472058,
0.999902211834794,1.,0.993980822699465,0.990851751371597)))
REPRESENTATION_ITEM('')
SURFACE()
);
#3625=(
BOUNDED_SURFACE()
B_SPLINE_SURFACE(1,2,((#156127,#156128,#156129,#156130,#156131),(#156132,
#156133,#156134,#156135,#156136),(#156137,#156138,#156139,#156140,#156141)),
 .UNSPECIFIED.,.F.,.F.,.F.)
B_SPLINE_SURFACE_WITH_KNOTS((2,1,2),(3,2,3),(-0.00211445385587008,0.,0.211445385587008),
(0.0724436337233711,0.0909109506295944,0.092121691069622),.UNSPECIFIED.)
GEOMETRIC_REPRESENTATION_ITEM()
RATIONAL_B_SPLINE_SURFACE(((0.999297534092548,0.992999570808217,0.990053454406147,
0.990053454406147,0.990053454406147),(0.999297534092548,0.992999570808217,
0.990053454406147,0.990053454406147,0.990053454406147),(0.999297534092548,
0.992999570808217,0.990053454406147,0.990053454406147,0.990053454406147)))
REPRESENTATION_ITEM('')
SURFACE()
);
#3626=(
BOUNDED_SURFACE()
B_SPLINE_SURFACE(1,2,((#156148,#156149,#156150,#156151,#156152,#156153,
#156154),(#156155,#156156,#156157,#156158,#156159,#156160,#156161),(#156162,
#156163,#156164,#156165,#156166,#156167,#156168)),.UNSPECIFIED.,.F.,.F.,
 .F.)
B_SPLINE_SURFACE_WITH_KNOTS((2,1,2),(3,2,2,3),(-0.00211537324446629,0.,
0.211537324446629),(0.642404283483301,0.642578551421362,0.642857142857143,
0.660005345227463),.UNSPECIFIED.)
GEOMETRIC_REPRESENTATION_ITEM()
RATIONAL_B_SPLINE_SURFACE(((0.999805186472057,0.999805186472057,0.999805186472057,
0.999902211834794,1.,0.993980822699465,0.990851751371597),(0.999805186472057,
0.999805186472057,0.999805186472057,0.999902211834794,1.,0.993980822699465,
0.990851751371597),(0.999805186472057,0.999805186472057,0.999805186472057,
0.999902211834794,1.,0.993980822699465,0.990851751371597)))
REPRESENTATION_ITEM('')
SURFACE()
);
#3627=(
BOUNDED_SURFACE()
B_SPLINE_SURFACE(1,2,((#156170,#156171,#156172,#156173,#156174),(#156175,
#156176,#156177,#156178,#156179),(#156180,#156181,#156182,#156183,#156184)),
 .UNSPECIFIED.,.F.,.F.,.F.)
B_SPLINE_SURFACE_WITH_KNOTS((2,1,2),(3,2,3),(-0.0021144538558701,0.,0.21144538558701),
(0.0724436329521793,0.0909109506295945,0.092121691285746),.UNSPECIFIED.)
GEOMETRIC_REPRESENTATION_ITEM()
RATIONAL_B_SPLINE_SURFACE(((0.999297534618552,0.992999570931246,0.990053454406147,
0.990053454406147,0.990053454406147),(0.999297534618552,0.992999570931246,
0.990053454406147,0.990053454406147,0.990053454406147),(0.999297534618552,
0.992999570931246,0.990053454406147,0.990053454406147,0.990053454406147)))
REPRESENTATION_ITEM('')
SURFACE()
);
#3628=(
BOUNDED_SURFACE()
B_SPLINE_SURFACE(1,2,((#156191,#156192,#156193,#156194,#156195,#156196,
#156197),(#156198,#156199,#156200,#156201,#156202,#156203,#156204),(#156205,
#156206,#156207,#156208,#156209,#156210,#156211)),.UNSPECIFIED.,.F.,.F.,
 .F.)
B_SPLINE_SURFACE_WITH_KNOTS((2,1,2),(3,2,2,3),(-0.00211537324446949,0.,
0.211537324446949),(0.642404283483263,0.642578551421324,0.642857142857143,
0.660005345227463),.UNSPECIFIED.)
GEOMETRIC_REPRESENTATION_ITEM()
RATIONAL_B_SPLINE_SURFACE(((0.999805186472031,0.999805186472031,0.999805186472031,
0.999902211834781,1.,0.993980822699465,0.990851751371597),(0.999805186472031,
0.999805186472031,0.999805186472031,0.999902211834781,1.,0.993980822699465,
0.990851751371597),(0.999805186472031,0.999805186472031,0.999805186472031,
0.999902211834781,1.,0.993980822699465,0.990851751371597)))
REPRESENTATION_ITEM('')
SURFACE()
);
#3629=(
BOUNDED_SURFACE()
B_SPLINE_SURFACE(1,2,((#156213,#156214,#156215,#156216,#156217),(#156218,
#156219,#156220,#156221,#156222),(#156223,#156224,#156225,#156226,#156227)),
 .UNSPECIFIED.,.F.,.F.,.F.)
B_SPLINE_SURFACE_WITH_KNOTS((2,1,2),(3,2,3),(-0.00211445385587014,0.,0.211445385587014),
(0.0724436336432635,0.0909109506295945,0.0921216911046539),
 .UNSPECIFIED.)
GEOMETRIC_REPRESENTATION_ITEM()
RATIONAL_B_SPLINE_SURFACE(((0.999297534147187,0.992999570820996,0.990053454406147,
0.990053454406147,0.990053454406147),(0.999297534147187,0.992999570820996,
0.990053454406147,0.990053454406147,0.990053454406147),(0.999297534147187,
0.992999570820996,0.990053454406147,0.990053454406147,0.990053454406147)))
REPRESENTATION_ITEM('')
SURFACE()
);
#3630=(
BOUNDED_SURFACE()
B_SPLINE_SURFACE(1,2,((#156234,#156235,#156236,#156237,#156238,#156239,
#156240),(#156241,#156242,#156243,#156244,#156245,#156246,#156247),(#156248,
#156249,#156250,#156251,#156252,#156253,#156254)),.UNSPECIFIED.,.F.,.F.,
 .F.)
B_SPLINE_SURFACE_WITH_KNOTS((2,1,2),(3,2,2,3),(-0.00211537324446956,0.,
0.211537324446956),(0.642404283483262,0.642578551421323,0.642857142857143,
0.660005345227472),.UNSPECIFIED.)
GEOMETRIC_REPRESENTATION_ITEM()
RATIONAL_B_SPLINE_SURFACE(((0.999805186472031,0.999805186472031,0.999805186472031,
0.99990221183478,1.,0.993980822699462,0.990851751371594),(0.999805186472031,
0.999805186472031,0.999805186472031,0.99990221183478,1.,0.993980822699462,
0.990851751371594),(0.999805186472031,0.999805186472031,0.999805186472031,
0.99990221183478,1.,0.993980822699462,0.990851751371594)))
REPRESENTATION_ITEM('')
SURFACE()
);
#3631=(
BOUNDED_SURFACE()
B_SPLINE_SURFACE(1,2,((#156256,#156257,#156258,#156259,#156260),(#156261,
#156262,#156263,#156264,#156265),(#156266,#156267,#156268,#156269,#156270)),
 .UNSPECIFIED.,.F.,.F.,.F.)
B_SPLINE_SURFACE_WITH_KNOTS((2,1,2),(3,2,3),(-0.00211445385587015,0.,0.211445385587015),
(0.0724436332002964,0.0909109506295945,0.0921216910412671),
 .UNSPECIFIED.)
GEOMETRIC_REPRESENTATION_ITEM()
RATIONAL_B_SPLINE_SURFACE(((0.99929753444932,0.992999570891664,0.990053454406147,
0.990053454406147,0.990053454406147),(0.99929753444932,0.992999570891664,
0.990053454406147,0.990053454406147,0.990053454406147),(0.99929753444932,
0.992999570891664,0.990053454406147,0.990053454406147,0.990053454406147)))
REPRESENTATION_ITEM('')
SURFACE()
);
#3632=(
BOUNDED_SURFACE()
B_SPLINE_SURFACE(1,2,((#156277,#156278,#156279,#156280,#156281,#156282,
#156283),(#156284,#156285,#156286,#156287,#156288,#156289,#156290),(#156291,
#156292,#156293,#156294,#156295,#156296,#156297)),.UNSPECIFIED.,.F.,.F.,
 .F.)
B_SPLINE_SURFACE_WITH_KNOTS((2,1,2),(3,2,2,3),(-0.00211537324446625,0.,
0.211537324446625),(0.642404283483301,0.642578551421362,0.642857142857143,
0.660005345227463),.UNSPECIFIED.)
GEOMETRIC_REPRESENTATION_ITEM()
RATIONAL_B_SPLINE_SURFACE(((0.999805186472057,0.999805186472057,0.999805186472057,
0.999902211834794,1.,0.993980822699465,0.990851751371597),(0.999805186472057,
0.999805186472057,0.999805186472057,0.999902211834794,1.,0.993980822699465,
0.990851751371597),(0.999805186472057,0.999805186472057,0.999805186472057,
0.999902211834794,1.,0.993980822699465,0.990851751371597)))
REPRESENTATION_ITEM('')
SURFACE()
);
#3633=(
BOUNDED_SURFACE()
B_SPLINE_SURFACE(1,2,((#156299,#156300,#156301,#156302,#156303),(#156304,
#156305,#156306,#156307,#156308),(#156309,#156310,#156311,#156312,#156313)),
 .UNSPECIFIED.,.F.,.F.,.F.)
B_SPLINE_SURFACE_WITH_KNOTS((2,1,2),(3,2,3),(-0.00211445385587014,0.,0.211445385587014),
(0.0724436338901995,0.0909109506295945,0.0921216908675382),
 .UNSPECIFIED.)
GEOMETRIC_REPRESENTATION_ITEM()
RATIONAL_B_SPLINE_SURFACE(((0.99929753397876,0.992999570781603,0.990053454406147,
0.990053454406147,0.990053454406147),(0.99929753397876,0.992999570781603,
0.990053454406147,0.990053454406147,0.990053454406147),(0.99929753397876,
0.992999570781603,0.990053454406147,0.990053454406147,0.990053454406147)))
REPRESENTATION_ITEM('')
SURFACE()
);
#3634=(
BOUNDED_SURFACE()
B_SPLINE_SURFACE(1,2,((#156320,#156321,#156322,#156323,#156324,#156325,
#156326),(#156327,#156328,#156329,#156330,#156331,#156332,#156333),(#156334,
#156335,#156336,#156337,#156338,#156339,#156340)),.UNSPECIFIED.,.F.,.F.,
 .F.)
B_SPLINE_SURFACE_WITH_KNOTS((2,1,2),(3,2,2,3),(-0.00211537324446629,0.,
0.211537324446629),(0.642404283483301,0.642578551421362,0.642857142857143,
0.660005345227463),.UNSPECIFIED.)
GEOMETRIC_REPRESENTATION_ITEM()
RATIONAL_B_SPLINE_SURFACE(((0.999805186472057,0.999805186472057,0.999805186472057,
0.999902211834794,1.,0.993980822699465,0.990851751371597),(0.999805186472057,
0.999805186472057,0.999805186472057,0.999902211834794,1.,0.993980822699465,
0.990851751371597),(0.999805186472057,0.999805186472057,0.999805186472057,
0.999902211834794,1.,0.993980822699465,0.990851751371597)))
REPRESENTATION_ITEM('')
SURFACE()
);
#3635=(
BOUNDED_SURFACE()
B_SPLINE_SURFACE(1,2,((#156342,#156343,#156344,#156345,#156346),(#156347,
#156348,#156349,#156350,#156351),(#156352,#156353,#156354,#156355,#156356)),
 .UNSPECIFIED.,.F.,.F.,.F.)
B_SPLINE_SURFACE_WITH_KNOTS((2,1,2),(3,2,3),(-0.00211445385587012,0.,0.211445385587012),
(0.0724436330728422,0.0909109506295943,0.092121691180342),.UNSPECIFIED.)
GEOMETRIC_REPRESENTATION_ITEM()
RATIONAL_B_SPLINE_SURFACE(((0.999297534536251,0.992999570911997,0.990053454406147,
0.990053454406147,0.990053454406147),(0.999297534536251,0.992999570911997,
0.990053454406147,0.990053454406147,0.990053454406147),(0.999297534536251,
0.992999570911997,0.990053454406147,0.990053454406147,0.990053454406147)))
REPRESENTATION_ITEM('')
SURFACE()
);
#3636=(
BOUNDED_SURFACE()
B_SPLINE_SURFACE(1,2,((#156363,#156364,#156365,#156366,#156367,#156368,
#156369),(#156370,#156371,#156372,#156373,#156374,#156375,#156376),(#156377,
#156378,#156379,#156380,#156381,#156382,#156383)),.UNSPECIFIED.,.F.,.F.,
 .F.)
B_SPLINE_SURFACE_WITH_KNOTS((2,1,2),(3,2,2,3),(-0.00211537324446862,0.,
0.211537324446862),(0.642404283483273,0.642578551421334,0.642857142857143,
0.660005345227463),.UNSPECIFIED.)
GEOMETRIC_REPRESENTATION_ITEM()
RATIONAL_B_SPLINE_SURFACE(((0.999805186472038,0.999805186472038,0.999805186472038,
0.999902211834784,1.,0.993980822699465,0.990851751371597),(0.999805186472038,
0.999805186472038,0.999805186472038,0.999902211834784,1.,0.993980822699465,
0.990851751371597),(0.999805186472038,0.999805186472038,0.999805186472038,
0.999902211834784,1.,0.993980822699465,0.990851751371597)))
REPRESENTATION_ITEM('')
SURFACE()
);
#3637=(
BOUNDED_SURFACE()
B_SPLINE_SURFACE(1,2,((#156385,#156386,#156387,#156388,#156389),(#156390,
#156391,#156392,#156393,#156394),(#156395,#156396,#156397,#156398,#156399)),
 .UNSPECIFIED.,.F.,.F.,.F.)
B_SPLINE_SURFACE_WITH_KNOTS((2,1,2),(3,2,3),(-0.00211445385587008,0.,0.211445385587008),
(0.0724436334874632,0.0909109506295944,0.0921216912916598),
 .UNSPECIFIED.)
GEOMETRIC_REPRESENTATION_ITEM()
RATIONAL_B_SPLINE_SURFACE(((0.999297534253452,0.992999570845852,0.990053454406147,
0.990053454406147,0.990053454406147),(0.999297534253452,0.992999570845852,
0.990053454406147,0.990053454406147,0.990053454406147),(0.999297534253452,
0.992999570845852,0.990053454406147,0.990053454406147,0.990053454406147)))
REPRESENTATION_ITEM('')
SURFACE()
);
#3638=(
BOUNDED_SURFACE()
B_SPLINE_SURFACE(1,2,((#156406,#156407,#156408,#156409,#156410,#156411,
#156412),(#156413,#156414,#156415,#156416,#156417,#156418,#156419),(#156420,
#156421,#156422,#156423,#156424,#156425,#156426)),.UNSPECIFIED.,.F.,.F.,
 .F.)
B_SPLINE_SURFACE_WITH_KNOTS((2,1,2),(3,2,2,3),(-0.00211537324446876,0.,
0.211537324446876),(0.642404283483271,0.642578551421332,0.642857142857143,
0.660005345227463),.UNSPECIFIED.)
GEOMETRIC_REPRESENTATION_ITEM()
RATIONAL_B_SPLINE_SURFACE(((0.999805186472037,0.999805186472037,0.999805186472037,
0.999902211834783,1.,0.993980822699465,0.990851751371597),(0.999805186472037,
0.999805186472037,0.999805186472037,0.999902211834783,1.,0.993980822699465,
0.990851751371597),(0.999805186472037,0.999805186472037,0.999805186472037,
0.999902211834783,1.,0.993980822699465,0.990851751371597)))
REPRESENTATION_ITEM('')
SURFACE()
);
#3639=(
BOUNDED_SURFACE()
B_SPLINE_SURFACE(1,2,((#156428,#156429,#156430,#156431,#156432),(#156433,
#156434,#156435,#156436,#156437),(#156438,#156439,#156440,#156441,#156442)),
 .UNSPECIFIED.,.F.,.F.,.F.)
B_SPLINE_SURFACE_WITH_KNOTS((2,1,2),(3,2,3),(-0.00211445385587004,0.,0.211445385587004),
(0.072443633212248,0.0909109506295932,0.0921216910014061),.UNSPECIFIED.)
GEOMETRIC_REPRESENTATION_ITEM()
RATIONAL_B_SPLINE_SURFACE(((0.999297534441168,0.992999570889758,0.990053454406148,
0.990053454406149,0.990053454406149),(0.999297534441168,0.992999570889758,
0.990053454406148,0.990053454406149,0.990053454406149),(0.999297534441168,
0.992999570889758,0.990053454406148,0.990053454406149,0.990053454406149)))
REPRESENTATION_ITEM('')
SURFACE()
);
#3640=(
BOUNDED_SURFACE()
B_SPLINE_SURFACE(1,2,((#156449,#156450,#156451,#156452,#156453,#156454,
#156455),(#156456,#156457,#156458,#156459,#156460,#156461,#156462),(#156463,
#156464,#156465,#156466,#156467,#156468,#156469)),.UNSPECIFIED.,.F.,.F.,
 .F.)
B_SPLINE_SURFACE_WITH_KNOTS((2,1,2),(3,2,2,3),(-0.00211537324446606,0.,
0.211537324446606),(0.642404283483303,0.642578551421364,0.642857142857143,
0.660005345227464),.UNSPECIFIED.)
GEOMETRIC_REPRESENTATION_ITEM()
RATIONAL_B_SPLINE_SURFACE(((0.999805186472059,0.999805186472059,0.999805186472059,
0.999902211834795,1.,0.993980822699464,0.990851751371597),(0.999805186472059,
0.999805186472059,0.999805186472059,0.999902211834795,1.,0.993980822699464,
0.990851751371597),(0.999805186472059,0.999805186472059,0.999805186472059,
0.999902211834795,1.,0.993980822699464,0.990851751371597)))
REPRESENTATION_ITEM('')
SURFACE()
);
#3641=(
BOUNDED_SURFACE()
B_SPLINE_SURFACE(1,2,((#156471,#156472,#156473,#156474,#156475),(#156476,
#156477,#156478,#156479,#156480),(#156481,#156482,#156483,#156484,#156485)),
 .UNSPECIFIED.,.F.,.F.,.F.)
B_SPLINE_SURFACE_WITH_KNOTS((2,1,2),(3,2,3),(-0.00211445385586999,0.,0.211445385586999),
(0.0724436332301871,0.0909109506295932,0.0921216910227852),
 .UNSPECIFIED.)
GEOMETRIC_REPRESENTATION_ITEM()
RATIONAL_B_SPLINE_SURFACE(((0.999297534428931,0.992999570886895,0.990053454406147,
0.990053454406147,0.990053454406147),(0.999297534428931,0.992999570886895,
0.990053454406147,0.990053454406147,0.990053454406147),(0.999297534428931,
0.992999570886895,0.990053454406147,0.990053454406147,0.990053454406147)))
REPRESENTATION_ITEM('')
SURFACE()
);
#3642=(
BOUNDED_SURFACE()
B_SPLINE_SURFACE(1,2,((#156492,#156493,#156494,#156495,#156496,#156497,
#156498),(#156499,#156500,#156501,#156502,#156503,#156504,#156505),(#156506,
#156507,#156508,#156509,#156510,#156511,#156512)),.UNSPECIFIED.,.F.,.F.,
 .F.)
B_SPLINE_SURFACE_WITH_KNOTS((2,1,2),(3,2,2,3),(-0.00211537324446848,0.,
0.211537324446848),(0.642404283483275,0.642578551421336,0.642857142857143,
0.660005345227473),.UNSPECIFIED.)
GEOMETRIC_REPRESENTATION_ITEM()
RATIONAL_B_SPLINE_SURFACE(((0.99980518647204,0.99980518647204,0.99980518647204,
0.999902211834785,1.,0.993980822699461,0.990851751371593),(0.99980518647204,
0.99980518647204,0.99980518647204,0.999902211834785,1.,0.993980822699461,
0.990851751371593),(0.99980518647204,0.99980518647204,0.99980518647204,
0.999902211834785,1.,0.993980822699461,0.990851751371593)))
REPRESENTATION_ITEM('')
SURFACE()
);
#3643=(
BOUNDED_SURFACE()
B_SPLINE_SURFACE(1,2,((#156514,#156515,#156516,#156517,#156518),(#156519,
#156520,#156521,#156522,#156523),(#156524,#156525,#156526,#156527,#156528)),
 .UNSPECIFIED.,.F.,.F.,.F.)
B_SPLINE_SURFACE_WITH_KNOTS((2,1,2),(3,2,3),(-0.00211445385587003,0.,0.211445385587003),
(0.0724436338956014,0.0909109506295934,0.0921216908414379),
 .UNSPECIFIED.)
GEOMETRIC_REPRESENTATION_ITEM()
RATIONAL_B_SPLINE_SURFACE(((0.999297533975076,0.992999570780741,0.990053454406147,
0.990053454406147,0.990053454406147),(0.999297533975076,0.992999570780741,
0.990053454406147,0.990053454406147,0.990053454406147),(0.999297533975076,
0.992999570780741,0.990053454406147,0.990053454406147,0.990053454406147)))
REPRESENTATION_ITEM('')
SURFACE()
);
#3644=(
BOUNDED_SURFACE()
B_SPLINE_SURFACE(1,2,((#156535,#156536,#156537,#156538,#156539,#156540,
#156541),(#156542,#156543,#156544,#156545,#156546,#156547,#156548),(#156549,
#156550,#156551,#156552,#156553,#156554,#156555)),.UNSPECIFIED.,.F.,.F.,
 .F.)
B_SPLINE_SURFACE_WITH_KNOTS((2,1,2),(3,2,2,3),(-0.0021153732444662,0.,0.21153732444662),
(0.642404283483302,0.642578551421363,0.642857142857143,0.660005345227473),
 .UNSPECIFIED.)
GEOMETRIC_REPRESENTATION_ITEM()
RATIONAL_B_SPLINE_SURFACE(((0.999805186472058,0.999805186472058,0.999805186472058,
0.999902211834794,1.,0.993980822699461,0.990851751371594),(0.999805186472058,
0.999805186472058,0.999805186472058,0.999902211834794,1.,0.993980822699461,
0.990851751371594),(0.999805186472058,0.999805186472058,0.999805186472058,
0.999902211834794,1.,0.993980822699461,0.990851751371594)))
REPRESENTATION_ITEM('')
SURFACE()
);
#3645=(
BOUNDED_SURFACE()
B_SPLINE_SURFACE(1,2,((#156557,#156558,#156559,#156560,#156561),(#156562,
#156563,#156564,#156565,#156566),(#156567,#156568,#156569,#156570,#156571)),
 .UNSPECIFIED.,.F.,.F.,.F.)
B_SPLINE_SURFACE_WITH_KNOTS((2,1,2),(3,2,3),(-0.00211445385587001,0.,0.211445385587001),
(0.0724436337408151,0.0909109506295932,0.0921216910221661),
 .UNSPECIFIED.)
GEOMETRIC_REPRESENTATION_ITEM()
RATIONAL_B_SPLINE_SURFACE(((0.999297534080651,0.992999570805435,0.990053454406148,
0.990053454406148,0.990053454406148),(0.999297534080651,0.992999570805435,
0.990053454406148,0.990053454406148,0.990053454406148),(0.999297534080651,
0.992999570805435,0.990053454406148,0.990053454406148,0.990053454406148)))
REPRESENTATION_ITEM('')
SURFACE()
);
#3646=(
BOUNDED_SURFACE()
B_SPLINE_SURFACE(1,2,((#156578,#156579,#156580,#156581,#156582,#156583,
#156584),(#156585,#156586,#156587,#156588,#156589,#156590,#156591),(#156592,
#156593,#156594,#156595,#156596,#156597,#156598)),.UNSPECIFIED.,.F.,.F.,
 .F.)
B_SPLINE_SURFACE_WITH_KNOTS((2,1,2),(3,2,2,3),(-0.00211537324446836,0.,
0.211537324446836),(0.642404283483276,0.642578551421337,0.642857142857143,
0.660005345227464),.UNSPECIFIED.)
GEOMETRIC_REPRESENTATION_ITEM()
RATIONAL_B_SPLINE_SURFACE(((0.99980518647204,0.99980518647204,0.99980518647204,
0.999902211834785,1.,0.993980822699464,0.990851751371596),(0.99980518647204,
0.99980518647204,0.99980518647204,0.999902211834785,1.,0.993980822699464,
0.990851751371596),(0.99980518647204,0.99980518647204,0.99980518647204,
0.999902211834785,1.,0.993980822699464,0.990851751371596)))
REPRESENTATION_ITEM('')
SURFACE()
);
#3647=(
BOUNDED_SURFACE()
B_SPLINE_SURFACE(1,2,((#156600,#156601,#156602,#156603,#156604),(#156605,
#156606,#156607,#156608,#156609),(#156610,#156611,#156612,#156613,#156614)),
 .UNSPECIFIED.,.F.,.F.,.F.)
B_SPLINE_SURFACE_WITH_KNOTS((2,1,2),(3,2,3),(-0.00211445385587002,0.,0.211445385587002),
(0.0724436332573611,0.0909109506295931,0.0921216909806424),
 .UNSPECIFIED.)
GEOMETRIC_REPRESENTATION_ITEM()
RATIONAL_B_SPLINE_SURFACE(((0.999297534410397,0.992999570882561,0.990053454406148,
0.990053454406148,0.990053454406148),(0.999297534410397,0.992999570882561,
0.990053454406148,0.990053454406148,0.990053454406148),(0.999297534410397,
0.992999570882561,0.990053454406148,0.990053454406148,0.990053454406148)))
REPRESENTATION_ITEM('')
SURFACE()
);
#3648=(
BOUNDED_SURFACE()
B_SPLINE_SURFACE(1,2,((#156621,#156622,#156623,#156624,#156625,#156626,
#156627),(#156628,#156629,#156630,#156631,#156632,#156633,#156634),(#156635,
#156636,#156637,#156638,#156639,#156640,#156641)),.UNSPECIFIED.,.F.,.F.,
 .F.)
B_SPLINE_SURFACE_WITH_KNOTS((2,1,2),(3,2,2,3),(-0.00211537324446873,0.,
0.211537324446873),(0.642404283483272,0.642578551421333,0.642857142857143,
0.660005345227464),.UNSPECIFIED.)
GEOMETRIC_REPRESENTATION_ITEM()
RATIONAL_B_SPLINE_SURFACE(((0.999805186472037,0.999805186472037,0.999805186472037,
0.999902211834784,1.,0.993980822699464,0.990851751371597),(0.999805186472037,
0.999805186472037,0.999805186472037,0.999902211834784,1.,0.993980822699464,
0.990851751371597),(0.999805186472037,0.999805186472037,0.999805186472037,
0.999902211834784,1.,0.993980822699464,0.990851751371596)))
REPRESENTATION_ITEM('')
SURFACE()
);
#3649=(
BOUNDED_SURFACE()
B_SPLINE_SURFACE(1,2,((#156643,#156644,#156645,#156646,#156647),(#156648,
#156649,#156650,#156651,#156652),(#156653,#156654,#156655,#156656,#156657)),
 .UNSPECIFIED.,.F.,.F.,.F.)
B_SPLINE_SURFACE_WITH_KNOTS((2,1,2),(3,2,3),(-0.00211445385587002,0.,0.211445385587002),
(0.0724436333091787,0.0909109506295932,0.0921216909179953),
 .UNSPECIFIED.)
GEOMETRIC_REPRESENTATION_ITEM()
RATIONAL_B_SPLINE_SURFACE(((0.999297534375055,0.992999570874294,0.990053454406148,
0.990053454406148,0.990053454406148),(0.999297534375055,0.992999570874294,
0.990053454406148,0.990053454406148,0.990053454406148),(0.999297534375055,
0.992999570874294,0.990053454406148,0.990053454406148,0.990053454406148)))
REPRESENTATION_ITEM('')
SURFACE()
);
#3650=(
BOUNDED_SURFACE()
B_SPLINE_SURFACE(1,2,((#156664,#156665,#156666,#156667,#156668,#156669,
#156670),(#156671,#156672,#156673,#156674,#156675,#156676,#156677),(#156678,
#156679,#156680,#156681,#156682,#156683,#156684)),.UNSPECIFIED.,.F.,.F.,
 .F.)
B_SPLINE_SURFACE_WITH_KNOTS((2,1,2),(3,2,2,3),(-0.00211537324446836,0.,
0.211537324446836),(0.642404283483276,0.642578551421337,0.642857142857143,
0.660005345227473),.UNSPECIFIED.)
GEOMETRIC_REPRESENTATION_ITEM()
RATIONAL_B_SPLINE_SURFACE(((0.99980518647204,0.99980518647204,0.99980518647204,
0.999902211834785,1.,0.993980822699461,0.990851751371593),(0.99980518647204,
0.99980518647204,0.99980518647204,0.999902211834785,1.,0.993980822699461,
0.990851751371593),(0.99980518647204,0.99980518647204,0.99980518647204,
0.999902211834785,1.,0.993980822699461,0.990851751371593)))
REPRESENTATION_ITEM('')
SURFACE()
);
#3651=(
BOUNDED_SURFACE()
B_SPLINE_SURFACE(1,2,((#156686,#156687,#156688,#156689,#156690),(#156691,
#156692,#156693,#156694,#156695),(#156696,#156697,#156698,#156699,#156700)),
 .UNSPECIFIED.,.F.,.F.,.F.)
B_SPLINE_SURFACE_WITH_KNOTS((2,1,2),(3,2,3),(-0.00211445385587004,0.,0.211445385587004),
(0.0724436339056056,0.0909109506295934,0.0921216908356061),
 .UNSPECIFIED.)
GEOMETRIC_REPRESENTATION_ITEM()
RATIONAL_B_SPLINE_SURFACE(((0.999297533968253,0.992999570779146,0.990053454406148,
0.990053454406148,0.990053454406148),(0.999297533968253,0.992999570779146,
0.990053454406148,0.990053454406148,0.990053454406148),(0.999297533968253,
0.992999570779145,0.990053454406148,0.990053454406148,0.990053454406148)))
REPRESENTATION_ITEM('')
SURFACE()
);
#3652=(
BOUNDED_SURFACE()
B_SPLINE_SURFACE(1,2,((#156707,#156708,#156709,#156710,#156711,#156712,
#156713),(#156714,#156715,#156716,#156717,#156718,#156719,#156720),(#156721,
#156722,#156723,#156724,#156725,#156726,#156727)),.UNSPECIFIED.,.F.,.F.,
 .F.)
B_SPLINE_SURFACE_WITH_KNOTS((2,1,2),(3,2,2,3),(-0.00211537324446615,0.,
0.211537324446615),(0.642404283483302,0.642578551421363,0.642857142857143,
0.660005345227464),.UNSPECIFIED.)
GEOMETRIC_REPRESENTATION_ITEM()
RATIONAL_B_SPLINE_SURFACE(((0.999805186472058,0.999805186472058,0.999805186472058,
0.999902211834794,1.,0.993980822699464,0.990851751371597),(0.999805186472058,
0.999805186472058,0.999805186472058,0.999902211834794,1.,0.993980822699464,
0.990851751371597),(0.999805186472058,0.999805186472058,0.999805186472058,
0.999902211834794,1.,0.993980822699464,0.990851751371597)))
REPRESENTATION_ITEM('')
SURFACE()
);
#3653=(
BOUNDED_SURFACE()
B_SPLINE_SURFACE(1,2,((#156729,#156730,#156731,#156732,#156733),(#156734,
#156735,#156736,#156737,#156738),(#156739,#156740,#156741,#156742,#156743)),
 .UNSPECIFIED.,.F.,.F.,.F.)
B_SPLINE_SURFACE_WITH_KNOTS((2,1,2),(3,2,3),(-0.00211445385587003,0.,0.211445385587003),
(0.0724436330770667,0.0909109506295932,0.0921216911365676),
 .UNSPECIFIED.)
GEOMETRIC_REPRESENTATION_ITEM()
RATIONAL_B_SPLINE_SURFACE(((0.99929753453337,0.992999570911323,0.990053454406148,
0.990053454406149,0.990053454406149),(0.99929753453337,0.992999570911323,
0.990053454406148,0.990053454406149,0.990053454406149),(0.99929753453337,
0.992999570911323,0.990053454406148,0.990053454406149,0.990053454406149)))
REPRESENTATION_ITEM('')
SURFACE()
);
#3654=(
BOUNDED_SURFACE()
B_SPLINE_SURFACE(1,2,((#156750,#156751,#156752,#156753,#156754,#156755,
#156756),(#156757,#156758,#156759,#156760,#156761,#156762,#156763),(#156764,
#156765,#156766,#156767,#156768,#156769,#156770)),.UNSPECIFIED.,.F.,.F.,
 .F.)
B_SPLINE_SURFACE_WITH_KNOTS((2,1,2),(3,2,2,3),(-0.00211537324446882,0.,
0.211537324446882),(0.642404283483271,0.642578551421332,0.642857142857143,
0.660005345227473),.UNSPECIFIED.)
GEOMETRIC_REPRESENTATION_ITEM()
RATIONAL_B_SPLINE_SURFACE(((0.999805186472037,0.999805186472037,0.999805186472037,
0.999902211834783,1.,0.993980822699461,0.990851751371593),(0.999805186472037,
0.999805186472037,0.999805186472037,0.999902211834783,1.,0.993980822699461,
0.990851751371593),(0.999805186472037,0.999805186472037,0.999805186472037,
0.999902211834783,1.,0.993980822699461,0.990851751371593)))
REPRESENTATION_ITEM('')
SURFACE()
);
#3655=(
BOUNDED_SURFACE()
B_SPLINE_SURFACE(1,2,((#156772,#156773,#156774,#156775,#156776),(#156777,
#156778,#156779,#156780,#156781),(#156782,#156783,#156784,#156785,#156786)),
 .UNSPECIFIED.,.F.,.F.,.F.)
B_SPLINE_SURFACE_WITH_KNOTS((2,1,2),(3,2,3),(-0.00211445385587001,0.,0.211445385587001),
(0.0724436338307542,0.0909109506295933,0.0921216909422942),
 .UNSPECIFIED.)
GEOMETRIC_REPRESENTATION_ITEM()
RATIONAL_B_SPLINE_SURFACE(((0.999297534019306,0.992999570791086,0.990053454406148,
0.990053454406148,0.990053454406148),(0.999297534019306,0.992999570791086,
0.990053454406148,0.990053454406148,0.990053454406148),(0.999297534019306,
0.992999570791086,0.990053454406148,0.990053454406148,0.990053454406148)))
REPRESENTATION_ITEM('')
SURFACE()
);
#3656=(
BOUNDED_SURFACE()
B_SPLINE_SURFACE(1,2,((#156793,#156794,#156795,#156796,#156797,#156798,
#156799),(#156800,#156801,#156802,#156803,#156804,#156805,#156806),(#156807,
#156808,#156809,#156810,#156811,#156812,#156813)),.UNSPECIFIED.,.F.,.F.,
 .F.)
B_SPLINE_SURFACE_WITH_KNOTS((2,1,2),(3,2,2,3),(-0.00211537324446608,0.,
0.211537324446608),(0.642404283483303,0.642578551421364,0.642857142857143,
0.660005345227473),.UNSPECIFIED.)
GEOMETRIC_REPRESENTATION_ITEM()
RATIONAL_B_SPLINE_SURFACE(((0.999805186472059,0.999805186472059,0.999805186472059,
0.999902211834795,1.,0.993980822699461,0.990851751371594),(0.999805186472059,
0.999805186472059,0.999805186472059,0.999902211834795,1.,0.993980822699461,
0.990851751371594),(0.999805186472059,0.999805186472059,0.999805186472059,
0.999902211834795,1.,0.993980822699461,0.990851751371593)))
REPRESENTATION_ITEM('')
SURFACE()
);
#3657=(
BOUNDED_SURFACE()
B_SPLINE_SURFACE(1,2,((#156815,#156816,#156817,#156818,#156819),(#156820,
#156821,#156822,#156823,#156824),(#156825,#156826,#156827,#156828,#156829)),
 .UNSPECIFIED.,.F.,.F.,.F.)
B_SPLINE_SURFACE_WITH_KNOTS((2,1,2),(3,2,3),(-0.00211445385587005,0.,0.211445385587005),
(0.0724436337011242,0.0909109506295933,0.0921216910686723),
 .UNSPECIFIED.)
GEOMETRIC_REPRESENTATION_ITEM()
RATIONAL_B_SPLINE_SURFACE(((0.999297534107722,0.992999570811766,0.990053454406148,
0.990053454406148,0.990053454406148),(0.999297534107722,0.992999570811766,
0.990053454406148,0.990053454406148,0.990053454406148),(0.999297534107722,
0.992999570811766,0.990053454406148,0.990053454406148,0.990053454406148)))
REPRESENTATION_ITEM('')
SURFACE()
);
#3658=(
BOUNDED_SURFACE()
B_SPLINE_SURFACE(1,2,((#156836,#156837,#156838,#156839,#156840,#156841,
#156842),(#156843,#156844,#156845,#156846,#156847,#156848,#156849),(#156850,
#156851,#156852,#156853,#156854,#156855,#156856)),.UNSPECIFIED.,.F.,.F.,
 .F.)
B_SPLINE_SURFACE_WITH_KNOTS((2,1,2),(3,2,2,3),(-0.00211537324446611,0.,
0.211537324446611),(0.642404283483303,0.642578551421364,0.642857142857143,
0.660005345227473),.UNSPECIFIED.)
GEOMETRIC_REPRESENTATION_ITEM()
RATIONAL_B_SPLINE_SURFACE(((0.999805186472059,0.999805186472059,0.999805186472059,
0.999902211834795,1.,0.993980822699461,0.990851751371594),(0.999805186472059,
0.999805186472059,0.999805186472059,0.999902211834795,1.,0.993980822699461,
0.990851751371594),(0.999805186472059,0.999805186472059,0.999805186472059,
0.999902211834795,1.,0.993980822699461,0.990851751371594)))
REPRESENTATION_ITEM('')
SURFACE()
);
#3659=(
BOUNDED_SURFACE()
B_SPLINE_SURFACE(1,2,((#156858,#156859,#156860,#156861,#156862),(#156863,
#156864,#156865,#156866,#156867),(#156868,#156869,#156870,#156871,#156872)),
 .UNSPECIFIED.,.F.,.F.,.F.)
B_SPLINE_SURFACE_WITH_KNOTS((2,1,2),(3,2,3),(-0.00211445385587002,0.,0.211445385587002),
(0.0724436337261546,0.0909109506295934,0.0921216910594916),
 .UNSPECIFIED.)
GEOMETRIC_REPRESENTATION_ITEM()
RATIONAL_B_SPLINE_SURFACE(((0.999297534090649,0.992999570807773,0.990053454406148,
0.990053454406148,0.990053454406148),(0.999297534090649,0.992999570807773,
0.990053454406148,0.990053454406148,0.990053454406148),(0.999297534090649,
0.992999570807773,0.990053454406148,0.990053454406148,0.990053454406148)))
REPRESENTATION_ITEM('')
SURFACE()
);
#3660=(
BOUNDED_SURFACE()
B_SPLINE_SURFACE(1,2,((#156879,#156880,#156881,#156882,#156883,#156884,
#156885),(#156886,#156887,#156888,#156889,#156890,#156891,#156892),(#156893,
#156894,#156895,#156896,#156897,#156898,#156899)),.UNSPECIFIED.,.F.,.F.,
 .F.)
B_SPLINE_SURFACE_WITH_KNOTS((2,1,2),(3,2,2,3),(-0.00211537324446904,0.,
0.211537324446904),(0.642404283483268,0.642578551421329,0.642857142857143,
0.660005345227479),.UNSPECIFIED.)
GEOMETRIC_REPRESENTATION_ITEM()
RATIONAL_B_SPLINE_SURFACE(((0.999805186472035,0.999805186472035,0.999805186472035,
0.999902211834783,1.,0.993980822699459,0.990851751371591),(0.999805186472035,
0.999805186472035,0.999805186472035,0.999902211834783,1.,0.993980822699459,
0.990851751371591),(0.999805186472035,0.999805186472035,0.999805186472035,
0.999902211834783,1.,0.993980822699459,0.990851751371591)))
REPRESENTATION_ITEM('')
SURFACE()
);
#3661=(
BOUNDED_SURFACE()
B_SPLINE_SURFACE(1,2,((#156901,#156902,#156903,#156904,#156905),(#156906,
#156907,#156908,#156909,#156910),(#156911,#156912,#156913,#156914,#156915)),
 .UNSPECIFIED.,.F.,.F.,.F.)
B_SPLINE_SURFACE_WITH_KNOTS((2,1,2),(3,2,3),(-0.00211445385587009,0.,0.211445385587009),
(0.0724436336683128,0.0909109506295935,0.0921216910852292),
 .UNSPECIFIED.)
GEOMETRIC_REPRESENTATION_ITEM()
RATIONAL_B_SPLINE_SURFACE(((0.999297534130102,0.992999570817001,0.990053454406147,
0.990053454406147,0.990053454406147),(0.999297534130102,0.992999570817001,
0.990053454406147,0.990053454406147,0.990053454406147),(0.999297534130102,
0.992999570817001,0.990053454406147,0.990053454406147,0.990053454406147)))
REPRESENTATION_ITEM('')
SURFACE()
);
#3662=(
BOUNDED_SURFACE()
B_SPLINE_SURFACE(1,2,((#156922,#156923,#156924,#156925,#156926,#156927,
#156928),(#156929,#156930,#156931,#156932,#156933,#156934,#156935),(#156936,
#156937,#156938,#156939,#156940,#156941,#156942)),.UNSPECIFIED.,.F.,.F.,
 .F.)
B_SPLINE_SURFACE_WITH_KNOTS((2,1,2),(3,2,2,3),(-0.00211537324446607,0.,
0.211537324446607),(0.642404283483303,0.642578551421364,0.642857142857143,
0.660005345227472),.UNSPECIFIED.)
GEOMETRIC_REPRESENTATION_ITEM()
RATIONAL_B_SPLINE_SURFACE(((0.999805186472059,0.999805186472059,0.999805186472059,
0.999902211834795,1.,0.993980822699462,0.990851751371594),(0.999805186472059,
0.999805186472059,0.999805186472059,0.999902211834795,1.,0.993980822699462,
0.990851751371594),(0.999805186472059,0.999805186472059,0.999805186472059,
0.999902211834795,1.,0.993980822699462,0.990851751371594)))
REPRESENTATION_ITEM('')
SURFACE()
);
#3663=(
BOUNDED_SURFACE()
B_SPLINE_SURFACE(1,2,((#156944,#156945,#156946,#156947,#156948),(#156949,
#156950,#156951,#156952,#156953),(#156954,#156955,#156956,#156957,#156958)),
 .UNSPECIFIED.,.F.,.F.,.F.)
B_SPLINE_SURFACE_WITH_KNOTS((2,1,2),(3,2,3),(-0.00211445385587004,0.,0.211445385587004),
(0.0724436331381984,0.0909109506295934,0.0921216910780853),
 .UNSPECIFIED.)
GEOMETRIC_REPRESENTATION_ITEM()
RATIONAL_B_SPLINE_SURFACE(((0.999297534491675,0.992999570901571,0.990053454406148,
0.990053454406148,0.990053454406148),(0.999297534491675,0.992999570901571,
0.990053454406148,0.990053454406148,0.990053454406148),(0.999297534491675,
0.992999570901571,0.990053454406148,0.990053454406148,0.990053454406148)))
REPRESENTATION_ITEM('')
SURFACE()
);
#3664=(
BOUNDED_SURFACE()
B_SPLINE_SURFACE(1,2,((#156965,#156966,#156967,#156968,#156969,#156970,
#156971),(#156972,#156973,#156974,#156975,#156976,#156977,#156978),(#156979,
#156980,#156981,#156982,#156983,#156984,#156985)),.UNSPECIFIED.,.F.,.F.,
 .F.)
B_SPLINE_SURFACE_WITH_KNOTS((2,1,2),(3,2,2,3),(-0.00211537324446616,0.,
0.211537324446616),(0.642404283483302,0.642578551421363,0.642857142857143,
0.660005345227471),.UNSPECIFIED.)
GEOMETRIC_REPRESENTATION_ITEM()
RATIONAL_B_SPLINE_SURFACE(((0.999805186472059,0.999805186472059,0.999805186472059,
0.999902211834794,1.,0.993980822699462,0.990851751371594),(0.999805186472059,
0.999805186472059,0.999805186472059,0.999902211834794,1.,0.993980822699462,
0.990851751371594),(0.999805186472059,0.999805186472059,0.999805186472059,
0.999902211834794,1.,0.993980822699462,0.990851751371594)))
REPRESENTATION_ITEM('')
SURFACE()
);
#3665=(
BOUNDED_SURFACE()
B_SPLINE_SURFACE(1,2,((#156987,#156988,#156989,#156990,#156991),(#156992,
#156993,#156994,#156995,#156996),(#156997,#156998,#156999,#157000,#157001)),
 .UNSPECIFIED.,.F.,.F.,.F.)
B_SPLINE_SURFACE_WITH_KNOTS((2,1,2),(3,2,3),(-0.00211445385587011,0.,0.211445385587011),
(0.0724436338486829,0.0909109506295947,0.0921216908958231),
 .UNSPECIFIED.)
GEOMETRIC_REPRESENTATION_ITEM()
RATIONAL_B_SPLINE_SURFACE(((0.999297534007077,0.992999570788226,0.990053454406147,
0.990053454406147,0.990053454406147),(0.999297534007077,0.992999570788226,
0.990053454406147,0.990053454406147,0.990053454406147),(0.999297534007077,
0.992999570788226,0.990053454406147,0.990053454406147,0.990053454406147)))
REPRESENTATION_ITEM('')
SURFACE()
);
#3666=(
BOUNDED_SURFACE()
B_SPLINE_SURFACE(1,2,((#157008,#157009,#157010,#157011,#157012,#157013,
#157014),(#157015,#157016,#157017,#157018,#157019,#157020,#157021),(#157022,
#157023,#157024,#157025,#157026,#157027,#157028)),.UNSPECIFIED.,.F.,.F.,
 .F.)
B_SPLINE_SURFACE_WITH_KNOTS((2,1,2),(3,2,2,3),(-0.00211537324446625,0.,
0.211537324446625),(0.642404283483301,0.642578551421362,0.642857142857143,
0.660005345227463),.UNSPECIFIED.)
GEOMETRIC_REPRESENTATION_ITEM()
RATIONAL_B_SPLINE_SURFACE(((0.999805186472057,0.999805186472057,0.999805186472057,
0.999902211834794,1.,0.993980822699465,0.990851751371597),(0.999805186472057,
0.999805186472057,0.999805186472057,0.999902211834794,1.,0.993980822699465,
0.990851751371597),(0.999805186472057,0.999805186472057,0.999805186472057,
0.999902211834794,1.,0.993980822699465,0.990851751371597)))
REPRESENTATION_ITEM('')
SURFACE()
);
#3667=(
BOUNDED_SURFACE()
B_SPLINE_SURFACE(1,2,((#157030,#157031,#157032,#157033,#157034),(#157035,
#157036,#157037,#157038,#157039),(#157040,#157041,#157042,#157043,#157044)),
 .UNSPECIFIED.,.F.,.F.,.F.)
B_SPLINE_SURFACE_WITH_KNOTS((2,1,2),(3,2,3),(-0.0021144538558701,0.,0.21144538558701),
(0.0724436336675499,0.0909109506295944,0.0921216910926114),
 .UNSPECIFIED.)
GEOMETRIC_REPRESENTATION_ITEM()
RATIONAL_B_SPLINE_SURFACE(((0.999297534130622,0.992999570817122,0.990053454406147,
0.990053454406147,0.990053454406147),(0.999297534130622,0.992999570817122,
0.990053454406147,0.990053454406147,0.990053454406147),(0.999297534130622,
0.992999570817122,0.990053454406147,0.990053454406147,0.990053454406147)))
REPRESENTATION_ITEM('')
SURFACE()
);
#3668=(
BOUNDED_SURFACE()
B_SPLINE_SURFACE(1,2,((#157051,#157052,#157053,#157054,#157055,#157056,
#157057),(#157058,#157059,#157060,#157061,#157062,#157063,#157064),(#157065,
#157066,#157067,#157068,#157069,#157070,#157071)),.UNSPECIFIED.,.F.,.F.,
 .F.)
B_SPLINE_SURFACE_WITH_KNOTS((2,1,2),(3,2,2,3),(-0.0021153732444663,0.,0.21153732444663),
(0.642404283483301,0.642578551421362,0.642857142857143,0.660005345227463),
 .UNSPECIFIED.)
GEOMETRIC_REPRESENTATION_ITEM()
RATIONAL_B_SPLINE_SURFACE(((0.999805186472057,0.999805186472057,0.999805186472057,
0.999902211834794,1.,0.993980822699465,0.990851751371597),(0.999805186472057,
0.999805186472057,0.999805186472057,0.999902211834794,1.,0.993980822699465,
0.990851751371597),(0.999805186472057,0.999805186472057,0.999805186472057,
0.999902211834794,1.,0.993980822699465,0.990851751371597)))
REPRESENTATION_ITEM('')
SURFACE()
);
#3669=(
BOUNDED_SURFACE()
B_SPLINE_SURFACE(1,2,((#157073,#157074,#157075,#157076,#157077),(#157078,
#157079,#157080,#157081,#157082),(#157083,#157084,#157085,#157086,#157087)),
 .UNSPECIFIED.,.F.,.F.,.F.)
B_SPLINE_SURFACE_WITH_KNOTS((2,1,2),(3,2,3),(-0.0021144538558701,0.,0.21144538558701),
(0.0724436336107497,0.0909109506295944,0.0921216911633498),
 .UNSPECIFIED.)
GEOMETRIC_REPRESENTATION_ITEM()
RATIONAL_B_SPLINE_SURFACE(((0.999297534169364,0.992999570826184,0.990053454406147,
0.990053454406147,0.990053454406147),(0.999297534169364,0.992999570826184,
0.990053454406147,0.990053454406147,0.990053454406147),(0.999297534169364,
0.992999570826184,0.990053454406147,0.990053454406147,0.990053454406147)))
REPRESENTATION_ITEM('')
SURFACE()
);
#3670=(
BOUNDED_SURFACE()
B_SPLINE_SURFACE(1,2,((#157094,#157095,#157096,#157097,#157098,#157099,
#157100),(#157101,#157102,#157103,#157104,#157105,#157106,#157107),(#157108,
#157109,#157110,#157111,#157112,#157113,#157114)),.UNSPECIFIED.,.F.,.F.,
 .F.)
B_SPLINE_SURFACE_WITH_KNOTS((2,1,2),(3,2,2,3),(-0.0021153732444663,0.,0.21153732444663),
(0.642404283483301,0.642578551421362,0.642857142857143,0.660005345227463),
 .UNSPECIFIED.)
GEOMETRIC_REPRESENTATION_ITEM()
RATIONAL_B_SPLINE_SURFACE(((0.999805186472057,0.999805186472057,0.999805186472057,
0.999902211834794,1.,0.993980822699465,0.990851751371597),(0.999805186472057,
0.999805186472057,0.999805186472057,0.999902211834794,1.,0.993980822699465,
0.990851751371597),(0.999805186472057,0.999805186472057,0.999805186472057,
0.999902211834794,1.,0.993980822699465,0.990851751371597)))
REPRESENTATION_ITEM('')
SURFACE()
);
#3671=(
BOUNDED_SURFACE()
B_SPLINE_SURFACE(1,2,((#157116,#157117,#157118,#157119,#157120),(#157121,
#157122,#157123,#157124,#157125),(#157126,#157127,#157128,#157129,#157130)),
 .UNSPECIFIED.,.F.,.F.,.F.)
B_SPLINE_SURFACE_WITH_KNOTS((2,1,2),(3,2,3),(-0.00211445385587009,0.,0.211445385587009),
(0.0724436336951236,0.0909109506295944,0.0921216910686102),
 .UNSPECIFIED.)
GEOMETRIC_REPRESENTATION_ITEM()
RATIONAL_B_SPLINE_SURFACE(((0.999297534111815,0.992999570812723,0.990053454406147,
0.990053454406147,0.990053454406147),(0.999297534111815,0.992999570812723,
0.990053454406147,0.990053454406147,0.990053454406147),(0.999297534111815,
0.992999570812723,0.990053454406147,0.990053454406147,0.990053454406147)))
REPRESENTATION_ITEM('')
SURFACE()
);
#3672=(
BOUNDED_SURFACE()
B_SPLINE_SURFACE(1,2,((#157137,#157138,#157139,#157140,#157141,#157142,
#157143),(#157144,#157145,#157146,#157147,#157148,#157149,#157150),(#157151,
#157152,#157153,#157154,#157155,#157156,#157157)),.UNSPECIFIED.,.F.,.F.,
 .F.)
B_SPLINE_SURFACE_WITH_KNOTS((2,1,2),(3,2,2,3),(-0.00211537324446626,0.,
0.211537324446626),(0.642404283483301,0.642578551421362,0.642857142857143,
0.660005345227463),.UNSPECIFIED.)
GEOMETRIC_REPRESENTATION_ITEM()
RATIONAL_B_SPLINE_SURFACE(((0.999805186472057,0.999805186472057,0.999805186472057,
0.999902211834794,1.,0.993980822699465,0.990851751371597),(0.999805186472057,
0.999805186472057,0.999805186472057,0.999902211834794,1.,0.993980822699465,
0.990851751371597),(0.999805186472057,0.999805186472057,0.999805186472057,
0.999902211834794,1.,0.993980822699465,0.990851751371597)))
REPRESENTATION_ITEM('')
SURFACE()
);
#3673=(
BOUNDED_SURFACE()
B_SPLINE_SURFACE(1,2,((#157159,#157160,#157161,#157162,#157163),(#157164,
#157165,#157166,#157167,#157168)),.UNSPECIFIED.,.F.,.F.,.F.)
B_SPLINE_SURFACE_WITH_KNOTS((2,2),(3,2,3),(0.,0.211445385587011),(0.073550810617375,
0.0909109506295944,0.0910845520297166),.UNSPECIFIED.)
GEOMETRIC_REPRESENTATION_ITEM()
RATIONAL_B_SPLINE_SURFACE(((0.998554414400246,0.992822941359338,0.990053454406147,
0.990053454406147,0.990053454406147),(0.998554414400246,0.992822941359338,
0.990053454406147,0.990053454406147,0.990053454406147)))
REPRESENTATION_ITEM('')
SURFACE()
);
#3674=(
BOUNDED_SURFACE()
B_SPLINE_SURFACE(1,2,((#157170,#157171,#157172),(#157173,#157174,#157175)),
 .UNSPECIFIED.,.F.,.F.,.F.)
B_SPLINE_SURFACE_WITH_KNOTS((2,2),(3,3),(0.,0.28980704099168),(0.125170525609408,
0.142682999576236),.UNSPECIFIED.)
GEOMETRIC_REPRESENTATION_ITEM()
RATIONAL_B_SPLINE_SURFACE(((0.990658108926709,0.993760979299921,0.999878046252917),
(0.990658108926709,0.993760979299921,0.999878046252917)))
REPRESENTATION_ITEM('')
SURFACE()
);
#3675=(
BOUNDED_SURFACE()
B_SPLINE_SURFACE(1,2,((#157192,#157193,#157194,#157195,#157196),(#157197,
#157198,#157199,#157200,#157201)),.UNSPECIFIED.,.F.,.F.,.F.)
B_SPLINE_SURFACE_WITH_KNOTS((2,2),(3,2,3),(0.,0.290271444040998),(0.590808523385635,
0.607982157956011,0.608572517835734),.UNSPECIFIED.)
GEOMETRIC_REPRESENTATION_ITEM()
RATIONAL_B_SPLINE_SURFACE(((0.990086238235256,0.987329216372183,0.987470879370255,
0.987470879370255,0.987470879370255),(0.990086238235256,0.987329216372183,
0.987470879370255,0.987470879370255,0.987470879370255)))
REPRESENTATION_ITEM('')
SURFACE()
);
#3676=(
BOUNDED_SURFACE()
B_SPLINE_SURFACE(1,2,((#157203,#157204,#157205),(#157206,#157207,#157208)),
 .UNSPECIFIED.,.F.,.F.,.F.)
B_SPLINE_SURFACE_WITH_KNOTS((2,2),(3,3),(0.,0.289807040991667),(0.125170525609408,
0.142682999576236),.UNSPECIFIED.)
GEOMETRIC_REPRESENTATION_ITEM()
RATIONAL_B_SPLINE_SURFACE(((0.990658108926709,0.993760979299921,0.999878046252917),
(0.990658108926709,0.993760979299921,0.999878046252917)))
REPRESENTATION_ITEM('')
SURFACE()
);
#3677=(
BOUNDED_SURFACE()
B_SPLINE_SURFACE(1,2,((#157225,#157226,#157227,#157228,#157229),(#157230,
#157231,#157232,#157233,#157234)),.UNSPECIFIED.,.F.,.F.,.F.)
B_SPLINE_SURFACE_WITH_KNOTS((2,2),(3,2,3),(0.,0.290271444029068),(0.590808523385632,
0.607982157956011,0.608572517823816),.UNSPECIFIED.)
GEOMETRIC_REPRESENTATION_ITEM()
RATIONAL_B_SPLINE_SURFACE(((0.990086238235257,0.987329216372183,0.987470879370255,
0.987470879370255,0.987470879370255),(0.990086238235257,0.987329216372183,
0.987470879370255,0.987470879370255,0.987470879370255)))
REPRESENTATION_ITEM('')
SURFACE()
);
#3678=(
BOUNDED_SURFACE()
B_SPLINE_SURFACE(1,2,((#157236,#157237,#157238),(#157239,#157240,#157241)),
 .UNSPECIFIED.,.F.,.F.,.F.)
B_SPLINE_SURFACE_WITH_KNOTS((2,2),(3,3),(0.,0.289807040991662),(0.125170525609408,
0.14268299957623),.UNSPECIFIED.)
GEOMETRIC_REPRESENTATION_ITEM()
RATIONAL_B_SPLINE_SURFACE(((0.990658108926709,0.99376097929992,0.999878046252913),
(0.990658108926709,0.99376097929992,0.999878046252913)))
REPRESENTATION_ITEM('')
SURFACE()
);
#3679=(
BOUNDED_SURFACE()
B_SPLINE_SURFACE(1,2,((#157258,#157259,#157260,#157261,#157262),(#157263,
#157264,#157265,#157266,#157267)),.UNSPECIFIED.,.F.,.F.,.F.)
B_SPLINE_SURFACE_WITH_KNOTS((2,2),(3,2,3),(0.,0.29027144404043),(0.590808523385623,
0.607982157956011,0.608572517835178),.UNSPECIFIED.)
GEOMETRIC_REPRESENTATION_ITEM()
RATIONAL_B_SPLINE_SURFACE(((0.99008623823526,0.987329216372183,0.987470879370255,
0.987470879370255,0.987470879370255),(0.99008623823526,0.987329216372183,
0.987470879370255,0.987470879370255,0.987470879370255)))
REPRESENTATION_ITEM('')
SURFACE()
);
#3680=(
BOUNDED_SURFACE()
B_SPLINE_SURFACE(1,2,((#157269,#157270,#157271),(#157272,#157273,#157274)),
 .UNSPECIFIED.,.F.,.F.,.F.)
B_SPLINE_SURFACE_WITH_KNOTS((2,2),(3,3),(0.,0.289807040991601),(0.125170525609408,
0.142682999576235),.UNSPECIFIED.)
GEOMETRIC_REPRESENTATION_ITEM()
RATIONAL_B_SPLINE_SURFACE(((0.990658108926709,0.993760979299921,0.999878046252916),
(0.990658108926709,0.993760979299921,0.999878046252916)))
REPRESENTATION_ITEM('')
SURFACE()
);
#3681=(
BOUNDED_SURFACE()
B_SPLINE_SURFACE(1,2,((#157291,#157292,#157293,#157294,#157295),(#157296,
#157297,#157298,#157299,#157300)),.UNSPECIFIED.,.F.,.F.,.F.)
B_SPLINE_SURFACE_WITH_KNOTS((2,2),(3,2,3),(0.,0.290271444033733),(0.590808523385632,
0.607982157956012,0.608572517870902),.UNSPECIFIED.)
GEOMETRIC_REPRESENTATION_ITEM()
RATIONAL_B_SPLINE_SURFACE(((0.990086238235257,0.987329216372183,0.987470879370255,
0.987470879370255,0.987470879370255),(0.990086238235257,0.987329216372183,
0.987470879370255,0.987470879370255,0.987470879370255)))
REPRESENTATION_ITEM('')
SURFACE()
);
#3682=(
BOUNDED_SURFACE()
B_SPLINE_SURFACE(1,2,((#157302,#157303,#157304),(#157305,#157306,#157307)),
 .UNSPECIFIED.,.F.,.F.,.F.)
B_SPLINE_SURFACE_WITH_KNOTS((2,2),(3,3),(0.,0.289807040991605),(0.125170525609407,
0.142682999576233),.UNSPECIFIED.)
GEOMETRIC_REPRESENTATION_ITEM()
RATIONAL_B_SPLINE_SURFACE(((0.990658108926708,0.99376097929992,0.999878046252915),
(0.990658108926708,0.99376097929992,0.999878046252915)))
REPRESENTATION_ITEM('')
SURFACE()
);
#3683=(
BOUNDED_SURFACE()
B_SPLINE_SURFACE(1,2,((#157324,#157325,#157326,#157327,#157328),(#157329,
#157330,#157331,#157332,#157333)),.UNSPECIFIED.,.F.,.F.,.F.)
B_SPLINE_SURFACE_WITH_KNOTS((2,2),(3,2,3),(0.,0.290271444020211),(0.590808523385629,
0.607982157956012,0.60857251785743),.UNSPECIFIED.)
GEOMETRIC_REPRESENTATION_ITEM()
RATIONAL_B_SPLINE_SURFACE(((0.990086238235258,0.987329216372183,0.987470879370255,
0.987470879370255,0.987470879370255),(0.990086238235258,0.987329216372183,
0.987470879370255,0.987470879370255,0.987470879370255)))
REPRESENTATION_ITEM('')
SURFACE()
);
#3684=(
BOUNDED_SURFACE()
B_SPLINE_SURFACE(1,2,((#157335,#157336,#157337),(#157338,#157339,#157340)),
 .UNSPECIFIED.,.F.,.F.,.F.)
B_SPLINE_SURFACE_WITH_KNOTS((2,2),(3,3),(0.,0.289807040991593),(0.125170525609407,
0.142682999576235),.UNSPECIFIED.)
GEOMETRIC_REPRESENTATION_ITEM()
RATIONAL_B_SPLINE_SURFACE(((0.990658108926708,0.993760979299921,0.999878046252916),
(0.990658108926708,0.993760979299921,0.999878046252916)))
REPRESENTATION_ITEM('')
SURFACE()
);
#3685=(
BOUNDED_SURFACE()
B_SPLINE_SURFACE(1,2,((#157357,#157358,#157359,#157360,#157361),(#157362,
#157363,#157364,#157365,#157366)),.UNSPECIFIED.,.F.,.F.,.F.)
B_SPLINE_SURFACE_WITH_KNOTS((2,2),(3,2,3),(0.,0.290271444018325),(0.590808523385636,
0.607982157956012,0.608572517813142),.UNSPECIFIED.)
GEOMETRIC_REPRESENTATION_ITEM()
RATIONAL_B_SPLINE_SURFACE(((0.990086238235256,0.987329216372183,0.987470879370255,
0.987470879370255,0.987470879370255),(0.990086238235256,0.987329216372183,
0.987470879370255,0.987470879370255,0.987470879370255)))
REPRESENTATION_ITEM('')
SURFACE()
);
#3686=(
BOUNDED_SURFACE()
B_SPLINE_SURFACE(1,2,((#157368,#157369,#157370),(#157371,#157372,#157373)),
 .UNSPECIFIED.,.F.,.F.,.F.)
B_SPLINE_SURFACE_WITH_KNOTS((2,2),(3,3),(0.,0.289807040991612),(0.125170525609407,
0.142682999576235),.UNSPECIFIED.)
GEOMETRIC_REPRESENTATION_ITEM()
RATIONAL_B_SPLINE_SURFACE(((0.990658108926708,0.993760979299921,0.999878046252916),
(0.990658108926708,0.993760979299921,0.999878046252916)))
REPRESENTATION_ITEM('')
SURFACE()
);
#3687=(
BOUNDED_SURFACE()
B_SPLINE_SURFACE(1,2,((#157390,#157391,#157392,#157393,#157394),(#157395,
#157396,#157397,#157398,#157399)),.UNSPECIFIED.,.F.,.F.,.F.)
B_SPLINE_SURFACE_WITH_KNOTS((2,2),(3,2,3),(0.,0.290271444050794),(0.590808523385632,
0.607982157956012,0.608572517845598),.UNSPECIFIED.)
GEOMETRIC_REPRESENTATION_ITEM()
RATIONAL_B_SPLINE_SURFACE(((0.990086238235257,0.987329216372183,0.987470879370256,
0.987470879370256,0.987470879370256),(0.990086238235257,0.987329216372183,
0.987470879370256,0.987470879370256,0.987470879370256)))
REPRESENTATION_ITEM('')
SURFACE()
);
#3688=(
BOUNDED_SURFACE()
B_SPLINE_SURFACE(1,2,((#157401,#157402,#157403),(#157404,#157405,#157406)),
 .UNSPECIFIED.,.F.,.F.,.F.)
B_SPLINE_SURFACE_WITH_KNOTS((2,2),(3,3),(0.,0.289807040991564),(0.125170525609407,
0.142682999576235),.UNSPECIFIED.)
GEOMETRIC_REPRESENTATION_ITEM()
RATIONAL_B_SPLINE_SURFACE(((0.990658108926708,0.993760979299921,0.999878046252916),
(0.990658108926708,0.993760979299921,0.999878046252916)))
REPRESENTATION_ITEM('')
SURFACE()
);
#3689=(
BOUNDED_SURFACE()
B_SPLINE_SURFACE(1,2,((#157423,#157424,#157425,#157426,#157427),(#157428,
#157429,#157430,#157431,#157432)),.UNSPECIFIED.,.F.,.F.,.F.)
B_SPLINE_SURFACE_WITH_KNOTS((2,2),(3,2,3),(0.,0.290271444021746),(0.590808523385626,
0.607982157956012,0.608572517858504),.UNSPECIFIED.)
GEOMETRIC_REPRESENTATION_ITEM()
RATIONAL_B_SPLINE_SURFACE(((0.990086238235259,0.987329216372183,0.987470879370255,
0.987470879370255,0.987470879370255),(0.990086238235259,0.987329216372183,
0.987470879370255,0.987470879370255,0.987470879370255)))
REPRESENTATION_ITEM('')
SURFACE()
);
#3690=(
BOUNDED_SURFACE()
B_SPLINE_SURFACE(1,2,((#157434,#157435,#157436),(#157437,#157438,#157439)),
 .UNSPECIFIED.,.F.,.F.,.F.)
B_SPLINE_SURFACE_WITH_KNOTS((2,2),(3,3),(0.,0.289807040991559),(0.125170525609407,
0.142682999576235),.UNSPECIFIED.)
GEOMETRIC_REPRESENTATION_ITEM()
RATIONAL_B_SPLINE_SURFACE(((0.990658108926708,0.993760979299921,0.999878046252916),
(0.990658108926708,0.993760979299921,0.999878046252916)))
REPRESENTATION_ITEM('')
SURFACE()
);
#3691=(
BOUNDED_SURFACE()
B_SPLINE_SURFACE(1,2,((#157456,#157457,#157458,#157459,#157460),(#157461,
#157462,#157463,#157464,#157465)),.UNSPECIFIED.,.F.,.F.,.F.)
B_SPLINE_SURFACE_WITH_KNOTS((2,2),(3,2,3),(0.,0.290271444051793),(0.590808523385636,
0.607982157956012,0.608572517846652),.UNSPECIFIED.)
GEOMETRIC_REPRESENTATION_ITEM()
RATIONAL_B_SPLINE_SURFACE(((0.990086238235256,0.987329216372183,0.987470879370255,
0.987470879370255,0.987470879370255),(0.990086238235256,0.987329216372183,
0.987470879370255,0.987470879370255,0.987470879370255)))
REPRESENTATION_ITEM('')
SURFACE()
);
#3692=(
BOUNDED_SURFACE()
B_SPLINE_SURFACE(1,2,((#157467,#157468,#157469),(#157470,#157471,#157472)),
 .UNSPECIFIED.,.F.,.F.,.F.)
B_SPLINE_SURFACE_WITH_KNOTS((2,2),(3,3),(0.,0.289807040991559),(0.125170525609407,
0.142682999576235),.UNSPECIFIED.)
GEOMETRIC_REPRESENTATION_ITEM()
RATIONAL_B_SPLINE_SURFACE(((0.990658108926708,0.993760979299921,0.999878046252916),
(0.990658108926708,0.993760979299921,0.999878046252916)))
REPRESENTATION_ITEM('')
SURFACE()
);
#3693=(
BOUNDED_SURFACE()
B_SPLINE_SURFACE(1,2,((#157489,#157490,#157491,#157492,#157493),(#157494,
#157495,#157496,#157497,#157498)),.UNSPECIFIED.,.F.,.F.,.F.)
B_SPLINE_SURFACE_WITH_KNOTS((2,2),(3,2,3),(0.,0.290271444048056),(0.590808523385636,
0.607982157956012,0.608572517842917),.UNSPECIFIED.)
GEOMETRIC_REPRESENTATION_ITEM()
RATIONAL_B_SPLINE_SURFACE(((0.990086238235256,0.987329216372183,0.987470879370255,
0.987470879370255,0.987470879370255),(0.990086238235256,0.987329216372183,
0.987470879370255,0.987470879370255,0.987470879370255)))
REPRESENTATION_ITEM('')
SURFACE()
);
#3694=(
BOUNDED_SURFACE()
B_SPLINE_SURFACE(1,2,((#157500,#157501,#157502),(#157503,#157504,#157505)),
 .UNSPECIFIED.,.F.,.F.,.F.)
B_SPLINE_SURFACE_WITH_KNOTS((2,2),(3,3),(0.,0.289807040991562),(0.125170525609407,
0.142682999576235),.UNSPECIFIED.)
GEOMETRIC_REPRESENTATION_ITEM()
RATIONAL_B_SPLINE_SURFACE(((0.990658108926708,0.993760979299921,0.999878046252916),
(0.990658108926708,0.993760979299921,0.999878046252916)))
REPRESENTATION_ITEM('')
SURFACE()
);
#3695=(
BOUNDED_SURFACE()
B_SPLINE_SURFACE(1,2,((#157522,#157523,#157524,#157525,#157526),(#157527,
#157528,#157529,#157530,#157531)),.UNSPECIFIED.,.F.,.F.,.F.)
B_SPLINE_SURFACE_WITH_KNOTS((2,2),(3,2,3),(0.,0.29027144400483),(0.590808523385636,
0.607982157956012,0.60857251784236),.UNSPECIFIED.)
GEOMETRIC_REPRESENTATION_ITEM()
RATIONAL_B_SPLINE_SURFACE(((0.990086238235256,0.987329216372183,0.987470879370255,
0.987470879370255,0.987470879370255),(0.990086238235256,0.987329216372183,
0.987470879370255,0.987470879370255,0.987470879370255)))
REPRESENTATION_ITEM('')
SURFACE()
);
#3696=(
BOUNDED_SURFACE()
B_SPLINE_SURFACE(1,2,((#157533,#157534,#157535),(#157536,#157537,#157538)),
 .UNSPECIFIED.,.F.,.F.,.F.)
B_SPLINE_SURFACE_WITH_KNOTS((2,2),(3,3),(0.,0.289807040991561),(0.125170525609407,
0.142682999576235),.UNSPECIFIED.)
GEOMETRIC_REPRESENTATION_ITEM()
RATIONAL_B_SPLINE_SURFACE(((0.990658108926708,0.993760979299921,0.999878046252916),
(0.990658108926708,0.993760979299921,0.999878046252916)))
REPRESENTATION_ITEM('')
SURFACE()
);
#3697=(
BOUNDED_SURFACE()
B_SPLINE_SURFACE(1,2,((#157555,#157556,#157557,#157558,#157559),(#157560,
#157561,#157562,#157563,#157564)),.UNSPECIFIED.,.F.,.F.,.F.)
B_SPLINE_SURFACE_WITH_KNOTS((2,2),(3,2,3),(0.,0.290271443966874),(0.59080852338557,
0.607982157956012,0.608572517804365),.UNSPECIFIED.)
GEOMETRIC_REPRESENTATION_ITEM()
RATIONAL_B_SPLINE_SURFACE(((0.990086238235277,0.987329216372182,0.987470879370255,
0.987470879370255,0.987470879370255),(0.990086238235277,0.987329216372182,
0.987470879370255,0.987470879370255,0.987470879370255)))
REPRESENTATION_ITEM('')
SURFACE()
);
#3698=(
BOUNDED_SURFACE()
B_SPLINE_SURFACE(1,2,((#157566,#157567,#157568),(#157569,#157570,#157571)),
 .UNSPECIFIED.,.F.,.F.,.F.)
B_SPLINE_SURFACE_WITH_KNOTS((2,2),(3,3),(0.,0.289807040991565),(0.125170525609406,
0.142682999576235),.UNSPECIFIED.)
GEOMETRIC_REPRESENTATION_ITEM()
RATIONAL_B_SPLINE_SURFACE(((0.990658108926708,0.99376097929992,0.999878046252916),
(0.990658108926708,0.993760979299921,0.999878046252916)))
REPRESENTATION_ITEM('')
SURFACE()
);
#3699=(
BOUNDED_SURFACE()
B_SPLINE_SURFACE(1,2,((#157588,#157589,#157590,#157591,#157592),(#157593,
#157594,#157595,#157596,#157597)),.UNSPECIFIED.,.F.,.F.,.F.)
B_SPLINE_SURFACE_WITH_KNOTS((2,2),(3,2,3),(0.,0.290271444008694),(0.590808523385636,
0.607982157956012,0.608572517846246),.UNSPECIFIED.)
GEOMETRIC_REPRESENTATION_ITEM()
RATIONAL_B_SPLINE_SURFACE(((0.990086238235256,0.987329216372183,0.987470879370255,
0.987470879370255,0.987470879370255),(0.990086238235256,0.987329216372183,
0.987470879370255,0.987470879370255,0.987470879370255)))
REPRESENTATION_ITEM('')
SURFACE()
);
#3700=(
BOUNDED_SURFACE()
B_SPLINE_SURFACE(1,2,((#157599,#157600,#157601),(#157602,#157603,#157604)),
 .UNSPECIFIED.,.F.,.F.,.F.)
B_SPLINE_SURFACE_WITH_KNOTS((2,2),(3,3),(0.,0.289807040991559),(0.125170525609407,
0.142682999576235),.UNSPECIFIED.)
GEOMETRIC_REPRESENTATION_ITEM()
RATIONAL_B_SPLINE_SURFACE(((0.990658108926708,0.993760979299921,0.999878046252916),
(0.990658108926708,0.993760979299921,0.999878046252916)))
REPRESENTATION_ITEM('')
SURFACE()
);
#3701=(
BOUNDED_SURFACE()
B_SPLINE_SURFACE(1,2,((#157621,#157622,#157623,#157624,#157625),(#157626,
#157627,#157628,#157629,#157630)),.UNSPECIFIED.,.F.,.F.,.F.)
B_SPLINE_SURFACE_WITH_KNOTS((2,2),(3,2,3),(0.,0.290271444064358),(0.590808523385636,
0.607982157956012,0.608572517859214),.UNSPECIFIED.)
GEOMETRIC_REPRESENTATION_ITEM()
RATIONAL_B_SPLINE_SURFACE(((0.990086238235256,0.987329216372183,0.987470879370255,
0.987470879370255,0.987470879370255),(0.990086238235256,0.987329216372183,
0.987470879370255,0.987470879370255,0.987470879370255)))
REPRESENTATION_ITEM('')
SURFACE()
);
#3702=(
BOUNDED_SURFACE()
B_SPLINE_SURFACE(1,2,((#157632,#157633,#157634),(#157635,#157636,#157637)),
 .UNSPECIFIED.,.F.,.F.,.F.)
B_SPLINE_SURFACE_WITH_KNOTS((2,2),(3,3),(0.,0.289807040991563),(0.125170525609407,
0.142682999576235),.UNSPECIFIED.)
GEOMETRIC_REPRESENTATION_ITEM()
RATIONAL_B_SPLINE_SURFACE(((0.990658108926708,0.993760979299921,0.999878046252916),
(0.990658108926708,0.993760979299921,0.999878046252916)))
REPRESENTATION_ITEM('')
SURFACE()
);
#3703=(
BOUNDED_SURFACE()
B_SPLINE_SURFACE(1,2,((#157645,#157646,#157647,#157648,#157649),(#157650,
#157651,#157652,#157653,#157654)),.UNSPECIFIED.,.F.,.F.,.F.)
B_SPLINE_SURFACE_WITH_KNOTS((2,2),(3,2,3),(0.,0.290271444031163),(0.590808523385636,
0.607982157956012,0.608572517826022),.UNSPECIFIED.)
GEOMETRIC_REPRESENTATION_ITEM()
RATIONAL_B_SPLINE_SURFACE(((0.990086238235256,0.987329216372183,0.987470879370255,
0.987470879370255,0.987470879370255),(0.990086238235256,0.987329216372183,
0.987470879370255,0.987470879370255,0.987470879370255)))
REPRESENTATION_ITEM('')
SURFACE()
);
#3704=(
BOUNDED_SURFACE()
B_SPLINE_SURFACE(1,2,((#157656,#157657,#157658),(#157659,#157660,#157661)),
 .UNSPECIFIED.,.F.,.F.,.F.)
B_SPLINE_SURFACE_WITH_KNOTS((2,2),(3,3),(0.,0.289807040991562),(0.125170525609407,
0.142682999576235),.UNSPECIFIED.)
GEOMETRIC_REPRESENTATION_ITEM()
RATIONAL_B_SPLINE_SURFACE(((0.990658108926708,0.993760979299921,0.999878046252916),
(0.990658108926708,0.993760979299921,0.999878046252916)))
REPRESENTATION_ITEM('')
SURFACE()
);
#3705=(
BOUNDED_SURFACE()
B_SPLINE_SURFACE(1,2,((#157678,#157679,#157680,#157681,#157682),(#157683,
#157684,#157685,#157686,#157687)),.UNSPECIFIED.,.F.,.F.,.F.)
B_SPLINE_SURFACE_WITH_KNOTS((2,2),(3,2,3),(0.,0.290271444056828),(0.590808523385636,
0.607982157956012,0.608572517851688),.UNSPECIFIED.)
GEOMETRIC_REPRESENTATION_ITEM()
RATIONAL_B_SPLINE_SURFACE(((0.990086238235256,0.987329216372183,0.987470879370255,
0.987470879370255,0.987470879370255),(0.990086238235256,0.987329216372183,
0.987470879370255,0.987470879370255,0.987470879370255)))
REPRESENTATION_ITEM('')
SURFACE()
);
#3706=(
BOUNDED_SURFACE()
B_SPLINE_SURFACE(1,2,((#157689,#157690,#157691),(#157692,#157693,#157694)),
 .UNSPECIFIED.,.F.,.F.,.F.)
B_SPLINE_SURFACE_WITH_KNOTS((2,2),(3,3),(0.,0.289807040991562),(0.125170525609407,
0.142682999576235),.UNSPECIFIED.)
GEOMETRIC_REPRESENTATION_ITEM()
RATIONAL_B_SPLINE_SURFACE(((0.990658108926708,0.993760979299921,0.999878046252916),
(0.990658108926708,0.993760979299921,0.999878046252916)))
REPRESENTATION_ITEM('')
SURFACE()
);
#3707=(
BOUNDED_SURFACE()
B_SPLINE_SURFACE(1,2,((#157711,#157712,#157713,#157714,#157715),(#157716,
#157717,#157718,#157719,#157720)),.UNSPECIFIED.,.F.,.F.,.F.)
B_SPLINE_SURFACE_WITH_KNOTS((2,2),(3,2,3),(0.,0.290271444018615),(0.590808523385636,
0.607982157956012,0.60857251785571),.UNSPECIFIED.)
GEOMETRIC_REPRESENTATION_ITEM()
RATIONAL_B_SPLINE_SURFACE(((0.990086238235256,0.987329216372183,0.987470879370255,
0.987470879370255,0.987470879370255),(0.990086238235256,0.987329216372183,
0.987470879370255,0.987470879370255,0.987470879370255)))
REPRESENTATION_ITEM('')
SURFACE()
);
#3708=(
BOUNDED_SURFACE()
B_SPLINE_SURFACE(1,2,((#157722,#157723,#157724),(#157725,#157726,#157727)),
 .UNSPECIFIED.,.F.,.F.,.F.)
B_SPLINE_SURFACE_WITH_KNOTS((2,2),(3,3),(0.,0.289807040991559),(0.125170525609407,
0.142682999576235),.UNSPECIFIED.)
GEOMETRIC_REPRESENTATION_ITEM()
RATIONAL_B_SPLINE_SURFACE(((0.990658108926708,0.993760979299921,0.999878046252916),
(0.990658108926708,0.993760979299921,0.999878046252916)))
REPRESENTATION_ITEM('')
SURFACE()
);
#3709=(
BOUNDED_SURFACE()
B_SPLINE_SURFACE(1,2,((#157738,#157739,#157740,#157741,#157742),(#157743,
#157744,#157745,#157746,#157747)),.UNSPECIFIED.,.F.,.F.,.F.)
B_SPLINE_SURFACE_WITH_KNOTS((2,2),(3,2,3),(0.,0.290271444082965),(0.590808523385636,
0.607982157956012,0.608572517823633),.UNSPECIFIED.)
GEOMETRIC_REPRESENTATION_ITEM()
RATIONAL_B_SPLINE_SURFACE(((0.990086238235256,0.987329216372183,0.987470879370255,
0.987470879370255,0.987470879370255),(0.990086238235256,0.987329216372183,
0.987470879370255,0.987470879370255,0.987470879370255)))
REPRESENTATION_ITEM('')
SURFACE()
);
#3710=(
BOUNDED_SURFACE()
B_SPLINE_SURFACE(1,2,((#157755,#157756,#157757),(#157758,#157759,#157760)),
 .UNSPECIFIED.,.F.,.F.,.F.)
B_SPLINE_SURFACE_WITH_KNOTS((2,2),(3,3),(0.,0.289807040991562),(0.125170525609398,
0.142682999576235),.UNSPECIFIED.)
GEOMETRIC_REPRESENTATION_ITEM()
RATIONAL_B_SPLINE_SURFACE(((0.990658108926705,0.993760979299918,0.999878046252916),
(0.990658108926705,0.993760979299918,0.999878046252916)))
REPRESENTATION_ITEM('')
SURFACE()
);
#3711=(
BOUNDED_SURFACE()
B_SPLINE_SURFACE(1,2,((#157777,#157778,#157779,#157780,#157781),(#157782,
#157783,#157784,#157785,#157786)),.UNSPECIFIED.,.F.,.F.,.F.)
B_SPLINE_SURFACE_WITH_KNOTS((2,2),(3,2,3),(0.,0.290271443996391),(0.590808523385636,
0.607982157956011,0.608572517833416),.UNSPECIFIED.)
GEOMETRIC_REPRESENTATION_ITEM()
RATIONAL_B_SPLINE_SURFACE(((0.990086238235256,0.987329216372183,0.987470879370255,
0.987470879370255,0.987470879370255),(0.990086238235256,0.987329216372183,
0.987470879370255,0.987470879370255,0.987470879370255)))
REPRESENTATION_ITEM('')
SURFACE()
);
#3712=(
BOUNDED_SURFACE()
B_SPLINE_SURFACE(1,2,((#157788,#157789,#157790),(#157791,#157792,#157793)),
 .UNSPECIFIED.,.F.,.F.,.F.)
B_SPLINE_SURFACE_WITH_KNOTS((2,2),(3,3),(0.,0.289807040991562),(0.125170525609408,
0.142682999576236),.UNSPECIFIED.)
GEOMETRIC_REPRESENTATION_ITEM()
RATIONAL_B_SPLINE_SURFACE(((0.990658108926709,0.993760979299921,0.999878046252917),
(0.990658108926709,0.993760979299921,0.999878046252917)))
REPRESENTATION_ITEM('')
SURFACE()
);
#3713=(
BOUNDED_SURFACE()
B_SPLINE_SURFACE(1,2,((#157810,#157811,#157812,#157813,#157814),(#157815,
#157816,#157817,#157818,#157819)),.UNSPECIFIED.,.F.,.F.,.F.)
B_SPLINE_SURFACE_WITH_KNOTS((2,2),(3,2,3),(0.,0.290271443980373),(0.590808523385635,
0.607982157956011,0.608572517817981),.UNSPECIFIED.)
GEOMETRIC_REPRESENTATION_ITEM()
RATIONAL_B_SPLINE_SURFACE(((0.990086238235256,0.987329216372183,0.987470879370256,
0.987470879370256,0.987470879370256),(0.990086238235256,0.987329216372183,
0.987470879370255,0.987470879370255,0.987470879370255)))
REPRESENTATION_ITEM('')
SURFACE()
);
#3714=(
BOUNDED_SURFACE()
B_SPLINE_SURFACE(1,2,((#157821,#157822,#157823),(#157824,#157825,#157826)),
 .UNSPECIFIED.,.F.,.F.,.F.)
B_SPLINE_SURFACE_WITH_KNOTS((2,2),(3,3),(0.,0.289807040991884),(0.125170525609408,
0.142682999576236),.UNSPECIFIED.)
GEOMETRIC_REPRESENTATION_ITEM()
RATIONAL_B_SPLINE_SURFACE(((0.990658108926709,0.993760979299921,0.999878046252917),
(0.990658108926709,0.993760979299921,0.999878046252917)))
REPRESENTATION_ITEM('')
SURFACE()
);
#3715=(
BOUNDED_SURFACE()
B_SPLINE_SURFACE(1,2,((#157843,#157844,#157845,#157846,#157847),(#157848,
#157849,#157850,#157851,#157852)),.UNSPECIFIED.,.F.,.F.,.F.)
B_SPLINE_SURFACE_WITH_KNOTS((2,2),(3,2,3),(0.,0.290271444022386),(0.590808523385635,
0.607982157956011,0.608572517816915),.UNSPECIFIED.)
GEOMETRIC_REPRESENTATION_ITEM()
RATIONAL_B_SPLINE_SURFACE(((0.990086238235256,0.987329216372183,0.987470879370256,
0.987470879370256,0.987470879370256),(0.990086238235256,0.987329216372183,
0.987470879370256,0.987470879370256,0.987470879370256)))
REPRESENTATION_ITEM('')
SURFACE()
);
#3716=(
BOUNDED_SURFACE()
B_SPLINE_SURFACE(1,2,((#157854,#157855,#157856),(#157857,#157858,#157859)),
 .UNSPECIFIED.,.F.,.F.,.F.)
B_SPLINE_SURFACE_WITH_KNOTS((2,2),(3,3),(0.,0.28980704099189),(0.125170525609408,
0.142682999576237),.UNSPECIFIED.)
GEOMETRIC_REPRESENTATION_ITEM()
RATIONAL_B_SPLINE_SURFACE(((0.990658108926709,0.993760979299922,0.999878046252918),
(0.990658108926709,0.993760979299922,0.999878046252918)))
REPRESENTATION_ITEM('')
SURFACE()
);
#3717=(
BOUNDED_SURFACE()
B_SPLINE_SURFACE(1,2,((#157876,#157877,#157878,#157879,#157880),(#157881,
#157882,#157883,#157884,#157885)),.UNSPECIFIED.,.F.,.F.,.F.)
B_SPLINE_SURFACE_WITH_KNOTS((2,2),(3,2,3),(0.,0.290271444028045),(0.590808523385635,
0.607982157956011,0.608572517822572),.UNSPECIFIED.)
GEOMETRIC_REPRESENTATION_ITEM()
RATIONAL_B_SPLINE_SURFACE(((0.990086238235256,0.987329216372183,0.987470879370255,
0.987470879370255,0.987470879370255),(0.990086238235256,0.987329216372183,
0.987470879370255,0.987470879370255,0.987470879370255)))
REPRESENTATION_ITEM('')
SURFACE()
);
#3718=(
BOUNDED_SURFACE()
B_SPLINE_SURFACE(1,2,((#157887,#157888,#157889),(#157890,#157891,#157892)),
 .UNSPECIFIED.,.F.,.F.,.F.)
B_SPLINE_SURFACE_WITH_KNOTS((2,2),(3,3),(0.,0.289807040991888),(0.125170525609408,
0.142682999576236),.UNSPECIFIED.)
GEOMETRIC_REPRESENTATION_ITEM()
RATIONAL_B_SPLINE_SURFACE(((0.990658108926709,0.993760979299921,0.999878046252917),
(0.990658108926709,0.993760979299921,0.999878046252917)))
REPRESENTATION_ITEM('')
SURFACE()
);
#3719=(
BOUNDED_SURFACE()
B_SPLINE_SURFACE(1,2,((#157909,#157910,#157911,#157912,#157913),(#157914,
#157915,#157916,#157917,#157918)),.UNSPECIFIED.,.F.,.F.,.F.)
B_SPLINE_SURFACE_WITH_KNOTS((2,2),(3,2,3),(0.,0.290271444049221),(0.590808523385635,
0.607982157956011,0.608572517843748),.UNSPECIFIED.)
GEOMETRIC_REPRESENTATION_ITEM()
RATIONAL_B_SPLINE_SURFACE(((0.990086238235256,0.987329216372183,0.987470879370255,
0.987470879370255,0.987470879370255),(0.990086238235256,0.987329216372183,
0.987470879370255,0.987470879370255,0.987470879370255)))
REPRESENTATION_ITEM('')
SURFACE()
);
#3720=(
BOUNDED_SURFACE()
B_SPLINE_SURFACE(1,2,((#157920,#157921,#157922),(#157923,#157924,#157925)),
 .UNSPECIFIED.,.F.,.F.,.F.)
B_SPLINE_SURFACE_WITH_KNOTS((2,2),(3,3),(0.,0.289807040991882),(0.125170525609408,
0.142682999576236),.UNSPECIFIED.)
GEOMETRIC_REPRESENTATION_ITEM()
RATIONAL_B_SPLINE_SURFACE(((0.990658108926709,0.993760979299921,0.999878046252917),
(0.990658108926709,0.993760979299921,0.999878046252917)))
REPRESENTATION_ITEM('')
SURFACE()
);
#3721=(
BOUNDED_SURFACE()
B_SPLINE_SURFACE(1,2,((#157942,#157943,#157944,#157945,#157946),(#157947,
#157948,#157949,#157950,#157951)),.UNSPECIFIED.,.F.,.F.,.F.)
B_SPLINE_SURFACE_WITH_KNOTS((2,2),(3,2,3),(0.,0.290271444045601),(0.590808523385634,
0.607982157956011,0.608572517840137),.UNSPECIFIED.)
GEOMETRIC_REPRESENTATION_ITEM()
RATIONAL_B_SPLINE_SURFACE(((0.990086238235257,0.987329216372183,0.987470879370255,
0.987470879370255,0.987470879370255),(0.990086238235256,0.987329216372183,
0.987470879370255,0.987470879370255,0.987470879370255)))
REPRESENTATION_ITEM('')
SURFACE()
);
#3722=(
BOUNDED_SURFACE()
B_SPLINE_SURFACE(1,2,((#157953,#157954,#157955),(#157956,#157957,#157958)),
 .UNSPECIFIED.,.F.,.F.,.F.)
B_SPLINE_SURFACE_WITH_KNOTS((2,2),(3,3),(0.,0.289807040993083),(0.125170525609408,
0.142682999576236),.UNSPECIFIED.)
GEOMETRIC_REPRESENTATION_ITEM()
RATIONAL_B_SPLINE_SURFACE(((0.990658108926709,0.993760979299921,0.999878046252917),
(0.990658108926709,0.993760979299921,0.999878046252917)))
REPRESENTATION_ITEM('')
SURFACE()
);
#3723=(
BOUNDED_SURFACE()
B_SPLINE_SURFACE(1,2,((#157975,#157976,#157977,#157978,#157979),(#157980,
#157981,#157982,#157983,#157984)),.UNSPECIFIED.,.F.,.F.,.F.)
B_SPLINE_SURFACE_WITH_KNOTS((2,2),(3,2,3),(0.,0.290271444054627),(0.590808523385635,
0.607982157956011,0.608572517849008),.UNSPECIFIED.)
GEOMETRIC_REPRESENTATION_ITEM()
RATIONAL_B_SPLINE_SURFACE(((0.990086238235256,0.987329216372183,0.987470879370255,
0.987470879370255,0.987470879370255),(0.990086238235256,0.987329216372183,
0.987470879370255,0.987470879370255,0.987470879370255)))
REPRESENTATION_ITEM('')
SURFACE()
);
#3724=(
BOUNDED_SURFACE()
B_SPLINE_SURFACE(1,2,((#157986,#157987,#157988),(#157989,#157990,#157991)),
 .UNSPECIFIED.,.F.,.F.,.F.)
B_SPLINE_SURFACE_WITH_KNOTS((2,2),(3,3),(0.,0.289807040991932),(0.125170525609408,
0.142682999576236),.UNSPECIFIED.)
GEOMETRIC_REPRESENTATION_ITEM()
RATIONAL_B_SPLINE_SURFACE(((0.990658108926709,0.993760979299921,0.999878046252917),
(0.990658108926709,0.993760979299921,0.999878046252917)))
REPRESENTATION_ITEM('')
SURFACE()
);
#3725=(
BOUNDED_SURFACE()
B_SPLINE_SURFACE(1,2,((#158008,#158009,#158010,#158011,#158012),(#158013,
#158014,#158015,#158016,#158017)),.UNSPECIFIED.,.F.,.F.,.F.)
B_SPLINE_SURFACE_WITH_KNOTS((2,2),(3,2,3),(0.,0.290271444013195),(0.59080852338563,
0.607982157956011,0.608572517849775),.UNSPECIFIED.)
GEOMETRIC_REPRESENTATION_ITEM()
RATIONAL_B_SPLINE_SURFACE(((0.990086238235258,0.987329216372183,0.987470879370255,
0.987470879370255,0.987470879370255),(0.990086238235258,0.987329216372183,
0.987470879370255,0.987470879370255,0.987470879370255)))
REPRESENTATION_ITEM('')
SURFACE()
);
#3726=(
BOUNDED_SURFACE()
B_SPLINE_SURFACE(1,2,((#158019,#158020,#158021),(#158022,#158023,#158024)),
 .UNSPECIFIED.,.F.,.F.,.F.)
B_SPLINE_SURFACE_WITH_KNOTS((2,2),(3,3),(0.,0.289807040991816),(0.125170525609408,
0.142682999576236),.UNSPECIFIED.)
GEOMETRIC_REPRESENTATION_ITEM()
RATIONAL_B_SPLINE_SURFACE(((0.990658108926709,0.993760979299921,0.999878046252917),
(0.990658108926709,0.993760979299921,0.999878046252917)))
REPRESENTATION_ITEM('')
SURFACE()
);
#3727=(
BOUNDED_SURFACE()
B_SPLINE_SURFACE(1,2,((#158041,#158042,#158043,#158044,#158045),(#158046,
#158047,#158048,#158049,#158050)),.UNSPECIFIED.,.F.,.F.,.F.)
B_SPLINE_SURFACE_WITH_KNOTS((2,2),(3,2,3),(0.,0.290271443990268),(0.590808523385635,
0.607982157956011,0.608572517827565),.UNSPECIFIED.)
GEOMETRIC_REPRESENTATION_ITEM()
RATIONAL_B_SPLINE_SURFACE(((0.990086238235256,0.987329216372183,0.987470879370255,
0.987470879370255,0.987470879370255),(0.990086238235256,0.987329216372183,
0.987470879370255,0.987470879370255,0.987470879370255)))
REPRESENTATION_ITEM('')
SURFACE()
);
#3728=(
BOUNDED_SURFACE()
B_SPLINE_SURFACE(1,2,((#158052,#158053,#158054),(#158055,#158056,#158057)),
 .UNSPECIFIED.,.F.,.F.,.F.)
B_SPLINE_SURFACE_WITH_KNOTS((2,2),(3,3),(0.,0.289807040991841),(0.125170525609408,
0.142682999576236),.UNSPECIFIED.)
GEOMETRIC_REPRESENTATION_ITEM()
RATIONAL_B_SPLINE_SURFACE(((0.990658108926709,0.993760979299921,0.999878046252917),
(0.990658108926709,0.993760979299921,0.999878046252917)))
REPRESENTATION_ITEM('')
SURFACE()
);
#3729=(
BOUNDED_SURFACE()
B_SPLINE_SURFACE(1,2,((#158074,#158075,#158076,#158077,#158078),(#158079,
#158080,#158081,#158082,#158083)),.UNSPECIFIED.,.F.,.F.,.F.)
B_SPLINE_SURFACE_WITH_KNOTS((2,2),(3,2,3),(0.,0.290271444010518),(0.590808523385628,
0.607982157956011,0.608572517847049),.UNSPECIFIED.)
GEOMETRIC_REPRESENTATION_ITEM()
RATIONAL_B_SPLINE_SURFACE(((0.990086238235258,0.987329216372183,0.987470879370255,
0.987470879370255,0.987470879370255),(0.990086238235258,0.987329216372183,
0.987470879370255,0.987470879370255,0.987470879370255)))
REPRESENTATION_ITEM('')
SURFACE()
);
#3730=(
BOUNDED_SURFACE()
B_SPLINE_SURFACE(1,2,((#158085,#158086,#158087),(#158088,#158089,#158090)),
 .UNSPECIFIED.,.F.,.F.,.F.)
B_SPLINE_SURFACE_WITH_KNOTS((2,2),(3,3),(0.,0.289807040991684),(0.125170525609408,
0.142682999576236),.UNSPECIFIED.)
GEOMETRIC_REPRESENTATION_ITEM()
RATIONAL_B_SPLINE_SURFACE(((0.990658108926709,0.993760979299921,0.999878046252917),
(0.990658108926709,0.993760979299921,0.999878046252917)))
REPRESENTATION_ITEM('')
SURFACE()
);
#3731=(
BOUNDED_SURFACE()
B_SPLINE_SURFACE(1,2,((#158107,#158108,#158109,#158110,#158111),(#158112,
#158113,#158114,#158115,#158116)),.UNSPECIFIED.,.F.,.F.,.F.)
B_SPLINE_SURFACE_WITH_KNOTS((2,2),(3,2,3),(0.,0.290271444030255),(0.590808523385629,
0.607982157956011,0.608572517824984),.UNSPECIFIED.)
GEOMETRIC_REPRESENTATION_ITEM()
RATIONAL_B_SPLINE_SURFACE(((0.990086238235258,0.987329216372183,0.987470879370256,
0.987470879370256,0.987470879370256),(0.990086238235258,0.987329216372183,
0.987470879370256,0.987470879370256,0.987470879370256)))
REPRESENTATION_ITEM('')
SURFACE()
);
#3732=(
BOUNDED_SURFACE()
B_SPLINE_SURFACE(1,2,((#158118,#158119,#158120,#158121,#158122),(#158123,
#158124,#158125,#158126,#158127)),.UNSPECIFIED.,.F.,.F.,.F.)
B_SPLINE_SURFACE_WITH_KNOTS((2,2),(3,2,3),(-1.00825488574708E-5,0.0614498483524471),
(0.659832011354081,0.659901408087475,0.666841081426897),.UNSPECIFIED.)
GEOMETRIC_REPRESENTATION_ITEM()
RATIONAL_B_SPLINE_SURFACE(((0.990889788836286,0.990889788836286,0.990889788836286,
0.989616401900861,0.988816334712145),(0.990889788836286,0.990889788836286,
0.990889788836286,0.989616401900861,0.988816334712145)))
REPRESENTATION_ITEM('')
SURFACE()
);
#3733=(
BOUNDED_SURFACE()
B_SPLINE_SURFACE(1,2,((#158130,#158131,#158132),(#158133,#158134,#158135)),
 .UNSPECIFIED.,.F.,.F.,.F.)
B_SPLINE_SURFACE_WITH_KNOTS((2,2),(3,3),(0.947118453120166,1.),(0.659860018385649,
0.666841081426897),.UNSPECIFIED.)
GEOMETRIC_REPRESENTATION_ITEM()
RATIONAL_B_SPLINE_SURFACE(((0.990904995179337,0.989621173673358,0.988816334712145),
(0.990904995179337,0.989621173673358,0.988816334712145)))
REPRESENTATION_ITEM('')
SURFACE()
);
#3734=(
BOUNDED_SURFACE()
B_SPLINE_SURFACE(1,2,((#158146,#158147,#158148,#158149,#158150),(#158151,
#158152,#158153,#158154,#158155)),.UNSPECIFIED.,.F.,.F.,.F.)
B_SPLINE_SURFACE_WITH_KNOTS((2,2),(3,2,3),(0.947095459621871,1.),(0.0665257254736561,
0.0714285714285714,0.0736968668684971),.UNSPECIFIED.)
GEOMETRIC_REPRESENTATION_ITEM()
RATIONAL_B_SPLINE_SURFACE(((0.996794362316491,0.998279055819231,1.,0.999203807365457,
0.998458182734336),(0.996794362316491,0.998279055819231,1.,0.999203807365457,
0.998458182734336)))
REPRESENTATION_ITEM('')
SURFACE()
);
#3735=(
BOUNDED_SURFACE()
B_SPLINE_SURFACE(1,2,((#158163,#158164,#158165,#158166,#158167),(#158168,
#158169,#158170,#158171,#158172)),.UNSPECIFIED.,.F.,.F.,.F.)
B_SPLINE_SURFACE_WITH_KNOTS((2,2),(3,2,3),(0.,0.0614231408718267),(0.0665257254736561,
0.0714285714285714,0.0736543502199108),.UNSPECIFIED.)
GEOMETRIC_REPRESENTATION_ITEM()
RATIONAL_B_SPLINE_SURFACE(((0.996794362316491,0.998279055819231,1.,0.999218731101516,
0.99848615229188),(0.996794362316491,0.998279055819231,1.,0.999218731101516,
0.99848615229188)))
REPRESENTATION_ITEM('')
SURFACE()
);
#3736=(
BOUNDED_SURFACE()
B_SPLINE_SURFACE(1,2,((#158174,#158175,#158176,#158177,#158178),(#158179,
#158180,#158181,#158182,#158183)),.UNSPECIFIED.,.F.,.F.,.F.)
B_SPLINE_SURFACE_WITH_KNOTS((2,2),(3,2,3),(0.817194107660842,1.),(0.642474614281367,
0.642857142857143,0.659901408087504),.UNSPECIFIED.)
GEOMETRIC_REPRESENTATION_ITEM()
RATIONAL_B_SPLINE_SURFACE(((0.999732896029237,0.999865728939372,1.,0.994017305594873,
0.990889788836276),(0.999732896029237,0.999865728939372,1.,0.994017305594873,
0.990889788836276)))
REPRESENTATION_ITEM('')
SURFACE()
);
#3737=(
BOUNDED_SURFACE()
B_SPLINE_SURFACE(1,2,((#158194,#158195,#158196,#158197,#158198),(#158199,
#158200,#158201,#158202,#158203)),.UNSPECIFIED.,.F.,.F.,.F.)
B_SPLINE_SURFACE_WITH_KNOTS((2,2),(3,2,3),(0.817114621578809,1.),(0.0734807488197752,
0.0736543502198967,0.0910144902320528),.UNSPECIFIED.)
GEOMETRIC_REPRESENTATION_ITEM()
RATIONAL_B_SPLINE_SURFACE(((0.998486152291889,0.998486152291889,0.998486152291889,
0.992772345172013,0.990020524139833),(0.998486152291889,0.998486152291889,
0.998486152291889,0.992772345172013,0.990020524139833)))
REPRESENTATION_ITEM('')
SURFACE()
);
#3738=(
BOUNDED_SURFACE()
B_SPLINE_SURFACE(1,2,((#158205,#158206,#158207,#158208,#158209),(#158210,
#158211,#158212,#158213,#158214)),.UNSPECIFIED.,.F.,.F.,.F.)
B_SPLINE_SURFACE_WITH_KNOTS((2,2),(3,2,3),(0.,0.0614498483525203),(0.659832011354072,
0.659901408087466,0.666841081426897),.UNSPECIFIED.)
GEOMETRIC_REPRESENTATION_ITEM()
RATIONAL_B_SPLINE_SURFACE(((0.99088978883629,0.99088978883629,0.99088978883629,
0.989616401900862,0.988816334712145),(0.990889788836289,0.990889788836289,
0.990889788836289,0.989616401900862,0.988816334712145)))
REPRESENTATION_ITEM('')
SURFACE()
);
#3739=(
BOUNDED_SURFACE()
B_SPLINE_SURFACE(1,2,((#158216,#158217,#158218),(#158219,#158220,#158221)),
 .UNSPECIFIED.,.F.,.F.,.F.)
B_SPLINE_SURFACE_WITH_KNOTS((2,2),(3,3),(0.947118453120169,1.),(0.659860018385515,
0.666841081426898),.UNSPECIFIED.)
GEOMETRIC_REPRESENTATION_ITEM()
RATIONAL_B_SPLINE_SURFACE(((0.990904995179386,0.989621173673374,0.988816334712145),
(0.990904995179386,0.989621173673374,0.988816334712145)))
REPRESENTATION_ITEM('')
SURFACE()
);
#3740=(
BOUNDED_SURFACE()
B_SPLINE_SURFACE(1,2,((#158232,#158233,#158234,#158235,#158236),(#158237,
#158238,#158239,#158240,#158241)),.UNSPECIFIED.,.F.,.F.,.F.)
B_SPLINE_SURFACE_WITH_KNOTS((2,2),(3,2,3),(0.947095459621871,1.),(0.066525725473656,
0.0714285714285714,0.0736968668684826),.UNSPECIFIED.)
GEOMETRIC_REPRESENTATION_ITEM()
RATIONAL_B_SPLINE_SURFACE(((0.996794362316491,0.998279055819231,1.,0.999203807365462,
0.998458182734345),(0.996794362316491,0.998279055819231,1.,0.999203807365462,
0.998458182734345)))
REPRESENTATION_ITEM('')
SURFACE()
);
#3741=(
BOUNDED_SURFACE()
B_SPLINE_SURFACE(1,2,((#158249,#158250,#158251,#158252,#158253),(#158254,
#158255,#158256,#158257,#158258)),.UNSPECIFIED.,.F.,.F.,.F.)
B_SPLINE_SURFACE_WITH_KNOTS((2,2),(3,2,3),(0.,0.0614231408718294),(0.0665257254736559,
0.0714285714285714,0.073654350219911),.UNSPECIFIED.)
GEOMETRIC_REPRESENTATION_ITEM()
RATIONAL_B_SPLINE_SURFACE(((0.996794362316491,0.998279055819231,1.,0.999218731101516,
0.99848615229188),(0.996794362316491,0.998279055819231,1.,0.999218731101516,
0.99848615229188)))
REPRESENTATION_ITEM('')
SURFACE()
);
#3742=(
BOUNDED_SURFACE()
B_SPLINE_SURFACE(1,2,((#158260,#158261,#158262,#158263,#158264),(#158265,
#158266,#158267,#158268,#158269)),.UNSPECIFIED.,.F.,.F.,.F.)
B_SPLINE_SURFACE_WITH_KNOTS((2,2),(3,2,3),(0.817194107660843,1.),(0.642474614281366,
0.642857142857143,0.659901408087509),.UNSPECIFIED.)
GEOMETRIC_REPRESENTATION_ITEM()
RATIONAL_B_SPLINE_SURFACE(((0.999732896029237,0.999865728939372,1.,0.994017305594872,
0.990889788836274),(0.999732896029237,0.999865728939372,1.,0.994017305594872,
0.990889788836274)))
REPRESENTATION_ITEM('')
SURFACE()
);
#3743=(
BOUNDED_SURFACE()
B_SPLINE_SURFACE(1,2,((#158280,#158281,#158282,#158283,#158284),(#158285,
#158286,#158287,#158288,#158289)),.UNSPECIFIED.,.F.,.F.,.F.)
B_SPLINE_SURFACE_WITH_KNOTS((2,2),(3,2,3),(0.817114621578807,1.),(0.0734807488197834,
0.0736543502199049,0.0910144902320525),.UNSPECIFIED.)
GEOMETRIC_REPRESENTATION_ITEM()
RATIONAL_B_SPLINE_SURFACE(((0.998486152291884,0.998486152291884,0.998486152291884,
0.992772345172012,0.990020524139833),(0.998486152291884,0.998486152291884,
0.998486152291884,0.992772345172012,0.990020524139833)))
REPRESENTATION_ITEM('')
SURFACE()
);
#3744=(
BOUNDED_SURFACE()
B_SPLINE_SURFACE(1,2,((#158291,#158292,#158293,#158294,#158295),(#158296,
#158297,#158298,#158299,#158300)),.UNSPECIFIED.,.F.,.F.,.F.)
B_SPLINE_SURFACE_WITH_KNOTS((2,2),(3,2,3),(0.,0.0614498483524406),(0.659832011354081,
0.659901408087475,0.666841081426897),.UNSPECIFIED.)
GEOMETRIC_REPRESENTATION_ITEM()
RATIONAL_B_SPLINE_SURFACE(((0.990889788836286,0.990889788836286,0.990889788836286,
0.989616401900861,0.988816334712145),(0.990889788836286,0.990889788836286,
0.990889788836286,0.989616401900861,0.988816334712145)))
REPRESENTATION_ITEM('')
SURFACE()
);
#3745=(
BOUNDED_SURFACE()
B_SPLINE_SURFACE(1,2,((#158302,#158303,#158304),(#158305,#158306,#158307)),
 .UNSPECIFIED.,.F.,.F.,.F.)
B_SPLINE_SURFACE_WITH_KNOTS((2,2),(3,3),(0.947118453120167,1.),(0.659860018385649,
0.666841081426897),.UNSPECIFIED.)
GEOMETRIC_REPRESENTATION_ITEM()
RATIONAL_B_SPLINE_SURFACE(((0.990904995179337,0.989621173673358,0.988816334712146),
(0.990904995179337,0.989621173673358,0.988816334712146)))
REPRESENTATION_ITEM('')
SURFACE()
);
#3746=(
BOUNDED_SURFACE()
B_SPLINE_SURFACE(1,2,((#158318,#158319,#158320,#158321,#158322),(#158323,
#158324,#158325,#158326,#158327)),.UNSPECIFIED.,.F.,.F.,.F.)
B_SPLINE_SURFACE_WITH_KNOTS((2,2),(3,2,3),(0.947095459621869,1.),(0.0665257254736559,
0.0714285714285714,0.0736968668684971),.UNSPECIFIED.)
GEOMETRIC_REPRESENTATION_ITEM()
RATIONAL_B_SPLINE_SURFACE(((0.996794362316491,0.998279055819231,1.,0.999203807365457,
0.998458182734336),(0.996794362316491,0.998279055819231,1.,0.999203807365457,
0.998458182734336)))
REPRESENTATION_ITEM('')
SURFACE()
);
#3747=(
BOUNDED_SURFACE()
B_SPLINE_SURFACE(1,2,((#158334,#158335,#158336,#158337,#158338),(#158339,
#158340,#158341,#158342,#158343)),.UNSPECIFIED.,.F.,.F.,.F.)
B_SPLINE_SURFACE_WITH_KNOTS((2,2),(3,2,3),(0.,0.0614231408718315),(0.0665257254736559,
0.0714285714285714,0.0736543502199111),.UNSPECIFIED.)
GEOMETRIC_REPRESENTATION_ITEM()
RATIONAL_B_SPLINE_SURFACE(((0.996794362316491,0.998279055819231,1.,0.999218731101516,
0.99848615229188),(0.996794362316491,0.998279055819231,1.,0.999218731101516,
0.99848615229188)))
REPRESENTATION_ITEM('')
SURFACE()
);
#3748=(
BOUNDED_SURFACE()
B_SPLINE_SURFACE(1,2,((#158345,#158346,#158347,#158348,#158349),(#158350,
#158351,#158352,#158353,#158354)),.UNSPECIFIED.,.F.,.F.,.F.)
B_SPLINE_SURFACE_WITH_KNOTS((2,2),(3,2,3),(0.817194107660842,1.),(0.642474614281366,
0.642857142857143,0.659901408087507),.UNSPECIFIED.)
GEOMETRIC_REPRESENTATION_ITEM()
RATIONAL_B_SPLINE_SURFACE(((0.999732896029237,0.999865728939372,1.,0.994017305594872,
0.990889788836274),(0.999732896029237,0.999865728939372,1.,0.994017305594872,
0.990889788836274)))
REPRESENTATION_ITEM('')
SURFACE()
);
#3749=(
BOUNDED_SURFACE()
B_SPLINE_SURFACE(1,2,((#158365,#158366,#158367,#158368,#158369),(#158370,
#158371,#158372,#158373,#158374)),.UNSPECIFIED.,.F.,.F.,.F.)
B_SPLINE_SURFACE_WITH_KNOTS((2,2),(3,2,3),(0.817114621578812,1.),(0.0734807488197752,
0.0736543502198967,0.0910144902320527),.UNSPECIFIED.)
GEOMETRIC_REPRESENTATION_ITEM()
RATIONAL_B_SPLINE_SURFACE(((0.998486152291889,0.998486152291889,0.998486152291889,
0.992772345172013,0.990020524139833),(0.998486152291889,0.998486152291889,
0.998486152291889,0.992772345172013,0.990020524139833)))
REPRESENTATION_ITEM('')
SURFACE()
);
#3750=(
BOUNDED_SURFACE()
B_SPLINE_SURFACE(1,2,((#158376,#158377,#158378,#158379,#158380),(#158381,
#158382,#158383,#158384,#158385)),.UNSPECIFIED.,.F.,.F.,.F.)
B_SPLINE_SURFACE_WITH_KNOTS((2,2),(3,2,3),(0.,0.0614498483525165),(0.659832011354072,
0.659901408087466,0.666841081426897),.UNSPECIFIED.)
GEOMETRIC_REPRESENTATION_ITEM()
RATIONAL_B_SPLINE_SURFACE(((0.99088978883629,0.99088978883629,0.99088978883629,
0.989616401900862,0.988816334712146),(0.99088978883629,0.99088978883629,
0.99088978883629,0.989616401900862,0.988816334712146)))
REPRESENTATION_ITEM('')
SURFACE()
);
#3751=(
BOUNDED_SURFACE()
B_SPLINE_SURFACE(1,2,((#158387,#158388,#158389),(#158390,#158391,#158392)),
 .UNSPECIFIED.,.F.,.F.,.F.)
B_SPLINE_SURFACE_WITH_KNOTS((2,2),(3,3),(0.947118453120169,1.),(0.659860018385517,
0.666841081426898),.UNSPECIFIED.)
GEOMETRIC_REPRESENTATION_ITEM()
RATIONAL_B_SPLINE_SURFACE(((0.990904995179385,0.989621173673373,0.988816334712145),
(0.990904995179385,0.989621173673373,0.988816334712145)))
REPRESENTATION_ITEM('')
SURFACE()
);
#3752=(
BOUNDED_SURFACE()
B_SPLINE_SURFACE(1,2,((#158403,#158404,#158405,#158406,#158407),(#158408,
#158409,#158410,#158411,#158412)),.UNSPECIFIED.,.F.,.F.,.F.)
B_SPLINE_SURFACE_WITH_KNOTS((2,2),(3,2,3),(0.947095459621873,1.),(0.0665257254736564,
0.0714285714285714,0.0736968668684826),.UNSPECIFIED.)
GEOMETRIC_REPRESENTATION_ITEM()
RATIONAL_B_SPLINE_SURFACE(((0.996794362316492,0.998279055819231,1.,0.999203807365462,
0.998458182734346),(0.996794362316492,0.998279055819231,1.,0.999203807365462,
0.998458182734346)))
REPRESENTATION_ITEM('')
SURFACE()
);
#3753=(
BOUNDED_SURFACE()
B_SPLINE_SURFACE(1,2,((#158420,#158421,#158422,#158423,#158424),(#158425,
#158426,#158427,#158428,#158429)),.UNSPECIFIED.,.F.,.F.,.F.)
B_SPLINE_SURFACE_WITH_KNOTS((2,2),(3,2,3),(0.,0.0614231408718255),(0.0665257254736564,
0.0714285714285714,0.073654350219911),.UNSPECIFIED.)
GEOMETRIC_REPRESENTATION_ITEM()
RATIONAL_B_SPLINE_SURFACE(((0.996794362316491,0.998279055819231,1.,0.999218731101516,
0.99848615229188),(0.996794362316491,0.998279055819231,1.,0.999218731101516,
0.99848615229188)))
REPRESENTATION_ITEM('')
SURFACE()
);
#3754=(
BOUNDED_SURFACE()
B_SPLINE_SURFACE(1,2,((#158431,#158432,#158433,#158434,#158435),(#158436,
#158437,#158438,#158439,#158440)),.UNSPECIFIED.,.F.,.F.,.F.)
B_SPLINE_SURFACE_WITH_KNOTS((2,2),(3,2,3),(0.817194107660841,1.),(0.642474614281365,
0.642857142857143,0.659901408087507),.UNSPECIFIED.)
GEOMETRIC_REPRESENTATION_ITEM()
RATIONAL_B_SPLINE_SURFACE(((0.999732896029236,0.999865728939372,1.,0.994017305594872,
0.990889788836274),(0.999732896029236,0.999865728939372,1.,0.994017305594872,
0.990889788836274)))
REPRESENTATION_ITEM('')
SURFACE()
);
#3755=(
BOUNDED_SURFACE()
B_SPLINE_SURFACE(1,2,((#158451,#158452,#158453,#158454,#158455),(#158456,
#158457,#158458,#158459,#158460)),.UNSPECIFIED.,.F.,.F.,.F.)
B_SPLINE_SURFACE_WITH_KNOTS((2,2),(3,2,3),(0.817114621578807,1.),(0.073480748819775,
0.0736543502198966,0.0910144902320526),.UNSPECIFIED.)
GEOMETRIC_REPRESENTATION_ITEM()
RATIONAL_B_SPLINE_SURFACE(((0.998486152291889,0.998486152291889,0.998486152291889,
0.992772345172014,0.990020524139833),(0.998486152291889,0.998486152291889,
0.998486152291889,0.992772345172014,0.990020524139833)))
REPRESENTATION_ITEM('')
SURFACE()
);
#3756=(
BOUNDED_SURFACE()
B_SPLINE_SURFACE(1,2,((#158462,#158463,#158464,#158465,#158466),(#158467,
#158468,#158469,#158470,#158471)),.UNSPECIFIED.,.F.,.F.,.F.)
B_SPLINE_SURFACE_WITH_KNOTS((2,2),(3,2,3),(0.,0.0614498483525202),(0.659832011354072,
0.659901408087466,0.666841081426897),.UNSPECIFIED.)
GEOMETRIC_REPRESENTATION_ITEM()
RATIONAL_B_SPLINE_SURFACE(((0.99088978883629,0.99088978883629,0.99088978883629,
0.989616401900862,0.988816334712146),(0.99088978883629,0.99088978883629,
0.99088978883629,0.989616401900862,0.988816334712146)))
REPRESENTATION_ITEM('')
SURFACE()
);
#3757=(
BOUNDED_SURFACE()
B_SPLINE_SURFACE(1,2,((#158473,#158474,#158475),(#158476,#158477,#158478)),
 .UNSPECIFIED.,.F.,.F.,.F.)
B_SPLINE_SURFACE_WITH_KNOTS((2,2),(3,3),(0.947118453120166,1.),(0.659860018385517,
0.666841081426898),.UNSPECIFIED.)
GEOMETRIC_REPRESENTATION_ITEM()
RATIONAL_B_SPLINE_SURFACE(((0.990904995179385,0.989621173673373,0.988816334712145),
(0.990904995179385,0.989621173673373,0.988816334712145)))
REPRESENTATION_ITEM('')
SURFACE()
);
#3758=(
BOUNDED_SURFACE()
B_SPLINE_SURFACE(1,2,((#158489,#158490,#158491,#158492,#158493),(#158494,
#158495,#158496,#158497,#158498)),.UNSPECIFIED.,.F.,.F.,.F.)
B_SPLINE_SURFACE_WITH_KNOTS((2,2),(3,2,3),(0.94741099344175,1.),(0.0665682420727563,
0.0714285714285714,0.0736543913087671),.UNSPECIFIED.)
GEOMETRIC_REPRESENTATION_ITEM()
RATIONAL_B_SPLINE_SURFACE(((0.996820130073177,0.99829397953792,1.,0.999218716678948,
0.998486125244442),(0.996820130073177,0.99829397953792,1.,0.999218716678948,
0.998486125244442)))
REPRESENTATION_ITEM('')
SURFACE()
);
#3759=(
BOUNDED_SURFACE()
B_SPLINE_SURFACE(1,2,((#158504,#158505,#158506,#158507,#158508),(#158509,
#158510,#158511,#158512,#158513)),.UNSPECIFIED.,.F.,.F.,.F.)
B_SPLINE_SURFACE_WITH_KNOTS((2,2),(3,2,3),(0.,0.0614231408718235),(0.0665257254736563,
0.0714285714285714,0.073654350219911),.UNSPECIFIED.)
GEOMETRIC_REPRESENTATION_ITEM()
RATIONAL_B_SPLINE_SURFACE(((0.996794362316491,0.998279055819231,1.,0.999218731101516,
0.99848615229188),(0.996794362316491,0.998279055819231,1.,0.999218731101516,
0.99848615229188)))
REPRESENTATION_ITEM('')
SURFACE()
);
#3760=(
BOUNDED_SURFACE()
B_SPLINE_SURFACE(1,2,((#158515,#158516,#158517,#158518,#158519),(#158520,
#158521,#158522,#158523,#158524)),.UNSPECIFIED.,.F.,.F.,.F.)
B_SPLINE_SURFACE_WITH_KNOTS((2,2),(3,2,3),(0.817194107660847,1.),(0.642474614281366,
0.642857142857143,0.659901408087507),.UNSPECIFIED.)
GEOMETRIC_REPRESENTATION_ITEM()
RATIONAL_B_SPLINE_SURFACE(((0.999732896029237,0.999865728939372,1.,0.994017305594872,
0.990889788836274),(0.999732896029237,0.999865728939372,1.,0.994017305594872,
0.990889788836274)))
REPRESENTATION_ITEM('')
SURFACE()
);
#3761=(
BOUNDED_SURFACE()
B_SPLINE_SURFACE(1,2,((#158535,#158536,#158537,#158538,#158539),(#158540,
#158541,#158542,#158543,#158544)),.UNSPECIFIED.,.F.,.F.,.F.)
B_SPLINE_SURFACE_WITH_KNOTS((2,2),(3,2,3),(0.817114621578816,1.),(0.073480748819775,
0.0736543502198966,0.0910144902320526),.UNSPECIFIED.)
GEOMETRIC_REPRESENTATION_ITEM()
RATIONAL_B_SPLINE_SURFACE(((0.998486152291889,0.998486152291889,0.998486152291889,
0.992772345172013,0.990020524139833),(0.998486152291889,0.998486152291889,
0.998486152291889,0.992772345172013,0.990020524139833)))
REPRESENTATION_ITEM('')
SURFACE()
);
#3762=(
BOUNDED_SURFACE()
B_SPLINE_SURFACE(1,2,((#158546,#158547,#158548,#158549,#158550),(#158551,
#158552,#158553,#158554,#158555)),.UNSPECIFIED.,.F.,.F.,.F.)
B_SPLINE_SURFACE_WITH_KNOTS((2,2),(3,2,3),(0.,0.06144984835252),(0.659832011354072,
0.659901408087466,0.666841081426897),.UNSPECIFIED.)
GEOMETRIC_REPRESENTATION_ITEM()
RATIONAL_B_SPLINE_SURFACE(((0.99088978883629,0.99088978883629,0.99088978883629,
0.989616401900862,0.988816334712146),(0.99088978883629,0.99088978883629,
0.99088978883629,0.989616401900862,0.988816334712146)))
REPRESENTATION_ITEM('')
SURFACE()
);
#3763=(
BOUNDED_SURFACE()
B_SPLINE_SURFACE(1,2,((#158557,#158558,#158559),(#158560,#158561,#158562)),
 .UNSPECIFIED.,.F.,.F.,.F.)
B_SPLINE_SURFACE_WITH_KNOTS((2,2),(3,3),(0.947118453120172,1.),(0.659860018385641,
0.666841081426897),.UNSPECIFIED.)
GEOMETRIC_REPRESENTATION_ITEM()
RATIONAL_B_SPLINE_SURFACE(((0.99090499517934,0.989621173673359,0.988816334712146),
(0.99090499517934,0.989621173673359,0.988816334712146)))
REPRESENTATION_ITEM('')
SURFACE()
);
#3764=(
BOUNDED_SURFACE()
B_SPLINE_SURFACE(1,2,((#158573,#158574,#158575,#158576,#158577),(#158578,
#158579,#158580,#158581,#158582)),.UNSPECIFIED.,.F.,.F.,.F.)
B_SPLINE_SURFACE_WITH_KNOTS((2,2),(3,2,3),(0.947095459621874,1.),(0.0665257254736566,
0.0714285714285714,0.0736968668684971),.UNSPECIFIED.)
GEOMETRIC_REPRESENTATION_ITEM()
RATIONAL_B_SPLINE_SURFACE(((0.996794362316492,0.998279055819231,1.,0.999203807365457,
0.998458182734336),(0.996794362316492,0.998279055819231,1.,0.999203807365457,
0.998458182734336)))
REPRESENTATION_ITEM('')
SURFACE()
);
#3765=(
BOUNDED_SURFACE()
B_SPLINE_SURFACE(1,2,((#158590,#158591,#158592,#158593,#158594),(#158595,
#158596,#158597,#158598,#158599)),.UNSPECIFIED.,.F.,.F.,.F.)
B_SPLINE_SURFACE_WITH_KNOTS((2,2),(3,2,3),(0.,0.0614231408718235),(0.0665257254736566,
0.0714285714285714,0.0736543502199111),.UNSPECIFIED.)
GEOMETRIC_REPRESENTATION_ITEM()
RATIONAL_B_SPLINE_SURFACE(((0.996794362316492,0.998279055819231,1.,0.999218731101516,
0.99848615229188),(0.996794362316492,0.998279055819231,1.,0.999218731101516,
0.99848615229188)))
REPRESENTATION_ITEM('')
SURFACE()
);
#3766=(
BOUNDED_SURFACE()
B_SPLINE_SURFACE(1,2,((#158601,#158602,#158603,#158604,#158605),(#158606,
#158607,#158608,#158609,#158610)),.UNSPECIFIED.,.F.,.F.,.F.)
B_SPLINE_SURFACE_WITH_KNOTS((2,2),(3,2,3),(0.817194107660845,1.),(0.642474614281363,
0.642857142857143,0.659901408087508),.UNSPECIFIED.)
GEOMETRIC_REPRESENTATION_ITEM()
RATIONAL_B_SPLINE_SURFACE(((0.999732896029235,0.999865728939371,1.,0.994017305594872,
0.990889788836274),(0.999732896029235,0.999865728939371,1.,0.994017305594872,
0.990889788836274)))
REPRESENTATION_ITEM('')
SURFACE()
);
#3767=(
BOUNDED_SURFACE()
B_SPLINE_SURFACE(1,2,((#158621,#158622,#158623,#158624,#158625),(#158626,
#158627,#158628,#158629,#158630)),.UNSPECIFIED.,.F.,.F.,.F.)
B_SPLINE_SURFACE_WITH_KNOTS((2,2),(3,2,3),(0.817114621578811,1.),(0.0734807488197752,
0.0736543502198967,0.0910144902320511),.UNSPECIFIED.)
GEOMETRIC_REPRESENTATION_ITEM()
RATIONAL_B_SPLINE_SURFACE(((0.998486152291889,0.998486152291889,0.998486152291889,
0.992772345172014,0.990020524139833),(0.998486152291889,0.998486152291889,
0.998486152291889,0.992772345172014,0.990020524139833)))
REPRESENTATION_ITEM('')
SURFACE()
);
#3768=(
BOUNDED_SURFACE()
B_SPLINE_SURFACE(1,2,((#158632,#158633,#158634,#158635,#158636),(#158637,
#158638,#158639,#158640,#158641)),.UNSPECIFIED.,.F.,.F.,.F.)
B_SPLINE_SURFACE_WITH_KNOTS((2,2),(3,2,3),(0.,0.0614498483525208),(0.659832011354072,
0.659901408087466,0.666841081426897),.UNSPECIFIED.)
GEOMETRIC_REPRESENTATION_ITEM()
RATIONAL_B_SPLINE_SURFACE(((0.990889788836289,0.990889788836289,0.990889788836289,
0.989616401900862,0.988816334712145),(0.990889788836289,0.990889788836289,
0.990889788836289,0.989616401900862,0.988816334712145)))
REPRESENTATION_ITEM('')
SURFACE()
);
#3769=(
BOUNDED_SURFACE()
B_SPLINE_SURFACE(1,2,((#158643,#158644,#158645),(#158646,#158647,#158648)),
 .UNSPECIFIED.,.F.,.F.,.F.)
B_SPLINE_SURFACE_WITH_KNOTS((2,2),(3,3),(0.947118453120167,1.),(0.659860018385514,
0.666841081426898),.UNSPECIFIED.)
GEOMETRIC_REPRESENTATION_ITEM()
RATIONAL_B_SPLINE_SURFACE(((0.990904995179386,0.989621173673373,0.988816334712145),
(0.990904995179386,0.989621173673373,0.988816334712145)))
REPRESENTATION_ITEM('')
SURFACE()
);
#3770=(
BOUNDED_SURFACE()
B_SPLINE_SURFACE(1,2,((#158659,#158660,#158661,#158662,#158663),(#158664,
#158665,#158666,#158667,#158668)),.UNSPECIFIED.,.F.,.F.,.F.)
B_SPLINE_SURFACE_WITH_KNOTS((2,2),(3,2,3),(0.947095459621876,1.),(0.0665257254736565,
0.0714285714285714,0.0736968668684827),.UNSPECIFIED.)
GEOMETRIC_REPRESENTATION_ITEM()
RATIONAL_B_SPLINE_SURFACE(((0.996794362316492,0.998279055819231,1.,0.999203807365462,
0.998458182734345),(0.996794362316492,0.998279055819231,1.,0.999203807365462,
0.998458182734345)))
REPRESENTATION_ITEM('')
SURFACE()
);
#3771=(
BOUNDED_SURFACE()
B_SPLINE_SURFACE(1,2,((#158675,#158676,#158677,#158678,#158679),(#158680,
#158681,#158682,#158683,#158684)),.UNSPECIFIED.,.F.,.F.,.F.)
B_SPLINE_SURFACE_WITH_KNOTS((2,2),(3,2,3),(0.,0.0614231408718282),(0.0665257254736563,
0.0714285714285714,0.0736543502199112),.UNSPECIFIED.)
GEOMETRIC_REPRESENTATION_ITEM()
RATIONAL_B_SPLINE_SURFACE(((0.996794362316491,0.998279055819231,1.,0.999218731101516,
0.99848615229188),(0.996794362316491,0.998279055819231,1.,0.999218731101516,
0.99848615229188)))
REPRESENTATION_ITEM('')
SURFACE()
);
#3772=(
BOUNDED_SURFACE()
B_SPLINE_SURFACE(1,2,((#158686,#158687,#158688,#158689,#158690),(#158691,
#158692,#158693,#158694,#158695)),.UNSPECIFIED.,.F.,.F.,.F.)
B_SPLINE_SURFACE_WITH_KNOTS((2,2),(3,2,3),(0.817194107660841,1.),(0.642474614281363,
0.642857142857143,0.659901408087504),.UNSPECIFIED.)
GEOMETRIC_REPRESENTATION_ITEM()
RATIONAL_B_SPLINE_SURFACE(((0.999732896029235,0.999865728939371,1.,0.994017305594873,
0.990889788836276),(0.999732896029235,0.999865728939371,1.,0.994017305594873,
0.990889788836276)))
REPRESENTATION_ITEM('')
SURFACE()
);
#3773=(
BOUNDED_SURFACE()
B_SPLINE_SURFACE(1,2,((#158706,#158707,#158708,#158709,#158710),(#158711,
#158712,#158713,#158714,#158715)),.UNSPECIFIED.,.F.,.F.,.F.)
B_SPLINE_SURFACE_WITH_KNOTS((2,2),(3,2,3),(0.817114621578807,1.),(0.0734807488197835,
0.073654350219905,0.0910144902320526),.UNSPECIFIED.)
GEOMETRIC_REPRESENTATION_ITEM()
RATIONAL_B_SPLINE_SURFACE(((0.998486152291884,0.998486152291884,0.998486152291884,
0.992772345172012,0.990020524139833),(0.998486152291884,0.998486152291884,
0.998486152291884,0.992772345172012,0.990020524139833)))
REPRESENTATION_ITEM('')
SURFACE()
);
#3774=(
BOUNDED_SURFACE()
B_SPLINE_SURFACE(1,2,((#158717,#158718,#158719,#158720,#158721),(#158722,
#158723,#158724,#158725,#158726)),.UNSPECIFIED.,.F.,.F.,.F.)
B_SPLINE_SURFACE_WITH_KNOTS((2,2),(3,2,3),(0.,0.0614498483524431),(0.659832011354081,
0.659901408087475,0.666841081426897),.UNSPECIFIED.)
GEOMETRIC_REPRESENTATION_ITEM()
RATIONAL_B_SPLINE_SURFACE(((0.990889788836286,0.990889788836286,0.990889788836286,
0.989616401900861,0.988816334712145),(0.990889788836286,0.990889788836286,
0.990889788836286,0.989616401900861,0.988816334712145)))
REPRESENTATION_ITEM('')
SURFACE()
);
#3775=(
BOUNDED_SURFACE()
B_SPLINE_SURFACE(1,2,((#158728,#158729,#158730),(#158731,#158732,#158733)),
 .UNSPECIFIED.,.F.,.F.,.F.)
B_SPLINE_SURFACE_WITH_KNOTS((2,2),(3,3),(0.94711845312017,1.),(0.659860018385515,
0.666841081426897),.UNSPECIFIED.)
GEOMETRIC_REPRESENTATION_ITEM()
RATIONAL_B_SPLINE_SURFACE(((0.990904995179386,0.989621173673373,0.988816334712145),
(0.990904995179386,0.989621173673373,0.988816334712145)))
REPRESENTATION_ITEM('')
SURFACE()
);
#3776=(
BOUNDED_SURFACE()
B_SPLINE_SURFACE(1,2,((#158744,#158745,#158746,#158747,#158748),(#158749,
#158750,#158751,#158752,#158753)),.UNSPECIFIED.,.F.,.F.,.F.)
B_SPLINE_SURFACE_WITH_KNOTS((2,2),(3,2,3),(0.947095459621868,1.),(0.0665257254736558,
0.0714285714285714,0.0736968668684909),.UNSPECIFIED.)
GEOMETRIC_REPRESENTATION_ITEM()
RATIONAL_B_SPLINE_SURFACE(((0.996794362316491,0.998279055819231,1.,0.999203807365459,
0.99845818273434),(0.996794362316491,0.998279055819231,1.,0.999203807365459,
0.99845818273434)))
REPRESENTATION_ITEM('')
SURFACE()
);
#3777=(
BOUNDED_SURFACE()
B_SPLINE_SURFACE(1,2,((#158761,#158762,#158763,#158764,#158765),(#158766,
#158767,#158768,#158769,#158770)),.UNSPECIFIED.,.F.,.F.,.F.)
B_SPLINE_SURFACE_WITH_KNOTS((2,2),(3,2,3),(0.,0.0614231408718295),(0.0665257254736558,
0.0714285714285714,0.0736543502199111),.UNSPECIFIED.)
GEOMETRIC_REPRESENTATION_ITEM()
RATIONAL_B_SPLINE_SURFACE(((0.996794362316491,0.998279055819231,1.,0.999218731101516,
0.99848615229188),(0.996794362316491,0.998279055819231,1.,0.999218731101516,
0.99848615229188)))
REPRESENTATION_ITEM('')
SURFACE()
);
#3778=(
BOUNDED_SURFACE()
B_SPLINE_SURFACE(1,2,((#158772,#158773,#158774,#158775,#158776),(#158777,
#158778,#158779,#158780,#158781)),.UNSPECIFIED.,.F.,.F.,.F.)
B_SPLINE_SURFACE_WITH_KNOTS((2,2),(3,2,3),(0.817194107660844,1.),(0.642474614281363,
0.642857142857143,0.659901408087509),.UNSPECIFIED.)
GEOMETRIC_REPRESENTATION_ITEM()
RATIONAL_B_SPLINE_SURFACE(((0.999732896029235,0.999865728939371,1.,0.994017305594872,
0.990889788836274),(0.999732896029235,0.999865728939371,1.,0.994017305594872,
0.990889788836274)))
REPRESENTATION_ITEM('')
SURFACE()
);
#3779=(
BOUNDED_SURFACE()
B_SPLINE_SURFACE(1,2,((#158792,#158793,#158794,#158795,#158796),(#158797,
#158798,#158799,#158800,#158801)),.UNSPECIFIED.,.F.,.F.,.F.)
B_SPLINE_SURFACE_WITH_KNOTS((2,2),(3,2,3),(0.817114621578811,1.),(0.073480748819775,
0.0736543502198966,0.0910144902320527),.UNSPECIFIED.)
GEOMETRIC_REPRESENTATION_ITEM()
RATIONAL_B_SPLINE_SURFACE(((0.998486152291889,0.998486152291889,0.998486152291889,
0.992772345172014,0.990020524139833),(0.998486152291889,0.998486152291889,
0.998486152291889,0.992772345172014,0.990020524139833)))
REPRESENTATION_ITEM('')
SURFACE()
);
#3780=(
BOUNDED_SURFACE()
B_SPLINE_SURFACE(1,2,((#158803,#158804,#158805,#158806,#158807),(#158808,
#158809,#158810,#158811,#158812)),.UNSPECIFIED.,.F.,.F.,.F.)
B_SPLINE_SURFACE_WITH_KNOTS((2,2),(3,2,3),(0.,0.0614498483525196),(0.659832011354072,
0.659901408087466,0.666841081426896),.UNSPECIFIED.)
GEOMETRIC_REPRESENTATION_ITEM()
RATIONAL_B_SPLINE_SURFACE(((0.99088978883629,0.99088978883629,0.99088978883629,
0.989616401900862,0.988816334712146),(0.990889788836289,0.990889788836289,
0.990889788836289,0.989616401900862,0.988816334712146)))
REPRESENTATION_ITEM('')
SURFACE()
);
#3781=(
BOUNDED_SURFACE()
B_SPLINE_SURFACE(1,2,((#158814,#158815,#158816),(#158817,#158818,#158819)),
 .UNSPECIFIED.,.F.,.F.,.F.)
B_SPLINE_SURFACE_WITH_KNOTS((2,2),(3,3),(0.947118453120172,1.),(0.659860018385514,
0.666841081426897),.UNSPECIFIED.)
GEOMETRIC_REPRESENTATION_ITEM()
RATIONAL_B_SPLINE_SURFACE(((0.990904995179386,0.989621173673374,0.988816334712145),
(0.990904995179386,0.989621173673374,0.988816334712145)))
REPRESENTATION_ITEM('')
SURFACE()
);
#3782=(
BOUNDED_SURFACE()
B_SPLINE_SURFACE(1,2,((#158830,#158831,#158832,#158833,#158834),(#158835,
#158836,#158837,#158838,#158839)),.UNSPECIFIED.,.F.,.F.,.F.)
B_SPLINE_SURFACE_WITH_KNOTS((2,2),(3,2,3),(0.94709545962187,1.),(0.0665257254736561,
0.0714285714285714,0.0736968668684826),.UNSPECIFIED.)
GEOMETRIC_REPRESENTATION_ITEM()
RATIONAL_B_SPLINE_SURFACE(((0.996794362316491,0.998279055819231,1.,0.999203807365462,
0.998458182734345),(0.996794362316491,0.998279055819231,1.,0.999203807365462,
0.998458182734345)))
REPRESENTATION_ITEM('')
SURFACE()
);
#3783=(
BOUNDED_SURFACE()
B_SPLINE_SURFACE(1,2,((#158846,#158847,#158848,#158849,#158850),(#158851,
#158852,#158853,#158854,#158855)),.UNSPECIFIED.,.F.,.F.,.F.)
B_SPLINE_SURFACE_WITH_KNOTS((2,2),(3,2,3),(0.,0.0614231408718267),(0.066525725473656,
0.0714285714285714,0.073654350219911),.UNSPECIFIED.)
GEOMETRIC_REPRESENTATION_ITEM()
RATIONAL_B_SPLINE_SURFACE(((0.996794362316491,0.998279055819231,1.,0.999218731101516,
0.99848615229188),(0.996794362316491,0.998279055819231,1.,0.999218731101516,
0.99848615229188)))
REPRESENTATION_ITEM('')
SURFACE()
);
#3784=(
BOUNDED_SURFACE()
B_SPLINE_SURFACE(1,2,((#158857,#158858,#158859,#158860,#158861),(#158862,
#158863,#158864,#158865,#158866)),.UNSPECIFIED.,.F.,.F.,.F.)
B_SPLINE_SURFACE_WITH_KNOTS((2,2),(3,2,3),(0.817194107660851,1.),(0.642474614281365,
0.642857142857143,0.659901408087504),.UNSPECIFIED.)
GEOMETRIC_REPRESENTATION_ITEM()
RATIONAL_B_SPLINE_SURFACE(((0.999732896029236,0.999865728939372,1.,0.994017305594874,
0.990889788836276),(0.999732896029236,0.999865728939372,1.,0.994017305594874,
0.990889788836276)))
REPRESENTATION_ITEM('')
SURFACE()
);
#3785=(
BOUNDED_SURFACE()
B_SPLINE_SURFACE(1,2,((#158877,#158878,#158879,#158880,#158881),(#158882,
#158883,#158884,#158885,#158886)),.UNSPECIFIED.,.F.,.F.,.F.)
B_SPLINE_SURFACE_WITH_KNOTS((2,2),(3,2,3),(0.81711462157881,1.),(0.073480748819775,
0.0736543502198966,0.0910144902320525),.UNSPECIFIED.)
GEOMETRIC_REPRESENTATION_ITEM()
RATIONAL_B_SPLINE_SURFACE(((0.998486152291889,0.998486152291889,0.998486152291889,
0.992772345172014,0.990020524139833),(0.998486152291889,0.998486152291889,
0.998486152291889,0.992772345172013,0.990020524139833)))
REPRESENTATION_ITEM('')
SURFACE()
);
#3786=(
BOUNDED_SURFACE()
B_SPLINE_SURFACE(1,2,((#158888,#158889,#158890,#158891,#158892),(#158893,
#158894,#158895,#158896,#158897)),.UNSPECIFIED.,.F.,.F.,.F.)
B_SPLINE_SURFACE_WITH_KNOTS((2,2),(3,2,3),(0.,0.0614498483525191),(0.659832011354072,
0.659901408087466,0.666841081426896),.UNSPECIFIED.)
GEOMETRIC_REPRESENTATION_ITEM()
RATIONAL_B_SPLINE_SURFACE(((0.99088978883629,0.99088978883629,0.99088978883629,
0.989616401900862,0.988816334712146),(0.99088978883629,0.99088978883629,
0.99088978883629,0.989616401900862,0.988816334712146)))
REPRESENTATION_ITEM('')
SURFACE()
);
#3787=(
BOUNDED_SURFACE()
B_SPLINE_SURFACE(1,2,((#158899,#158900,#158901),(#158902,#158903,#158904)),
 .UNSPECIFIED.,.F.,.F.,.F.)
B_SPLINE_SURFACE_WITH_KNOTS((2,2),(3,3),(0.947118453120174,1.),(0.659860018385517,
0.666841081426897),.UNSPECIFIED.)
GEOMETRIC_REPRESENTATION_ITEM()
RATIONAL_B_SPLINE_SURFACE(((0.990904995179385,0.989621173673373,0.988816334712145),
(0.990904995179385,0.989621173673373,0.988816334712145)))
REPRESENTATION_ITEM('')
SURFACE()
);
#3788=(
BOUNDED_SURFACE()
B_SPLINE_SURFACE(1,2,((#158915,#158916,#158917,#158918,#158919),(#158920,
#158921,#158922,#158923,#158924)),.UNSPECIFIED.,.F.,.F.,.F.)
B_SPLINE_SURFACE_WITH_KNOTS((2,2),(3,2,3),(0.94709545962187,1.),(0.066525725473656,
0.0714285714285714,0.0736968668684825),.UNSPECIFIED.)
GEOMETRIC_REPRESENTATION_ITEM()
RATIONAL_B_SPLINE_SURFACE(((0.996794362316491,0.998279055819231,1.,0.999203807365462,
0.998458182734346),(0.996794362316491,0.998279055819231,1.,0.999203807365462,
0.998458182734346)))
REPRESENTATION_ITEM('')
SURFACE()
);
#3789=(
BOUNDED_SURFACE()
B_SPLINE_SURFACE(1,2,((#158932,#158933,#158934,#158935,#158936),(#158937,
#158938,#158939,#158940,#158941)),.UNSPECIFIED.,.F.,.F.,.F.)
B_SPLINE_SURFACE_WITH_KNOTS((2,2),(3,2,3),(0.,0.0614231408718213),(0.0665257254736561,
0.0714285714285714,0.0736543502199202),.UNSPECIFIED.)
GEOMETRIC_REPRESENTATION_ITEM()
RATIONAL_B_SPLINE_SURFACE(((0.996794362316491,0.998279055819231,1.,0.999218731101513,
0.998486152291874),(0.996794362316491,0.998279055819231,1.,0.999218731101513,
0.998486152291874)))
REPRESENTATION_ITEM('')
SURFACE()
);
#3790=(
BOUNDED_SURFACE()
B_SPLINE_SURFACE(1,2,((#158943,#158944,#158945,#158946,#158947),(#158948,
#158949,#158950,#158951,#158952)),.UNSPECIFIED.,.F.,.F.,.F.)
B_SPLINE_SURFACE_WITH_KNOTS((2,2),(3,2,3),(0.81719410766085,1.),(0.642474614281365,
0.642857142857143,0.659901408087502),.UNSPECIFIED.)
GEOMETRIC_REPRESENTATION_ITEM()
RATIONAL_B_SPLINE_SURFACE(((0.999732896029236,0.999865728939372,1.,0.994017305594874,
0.990889788836276),(0.999732896029236,0.999865728939372,1.,0.994017305594874,
0.990889788836276)))
REPRESENTATION_ITEM('')
SURFACE()
);
#3791=(
BOUNDED_SURFACE()
B_SPLINE_SURFACE(1,2,((#158963,#158964,#158965,#158966,#158967),(#158968,
#158969,#158970,#158971,#158972)),.UNSPECIFIED.,.F.,.F.,.F.)
B_SPLINE_SURFACE_WITH_KNOTS((2,2),(3,2,3),(0.817114621578809,1.),(0.0734807488197752,
0.0736543502198967,0.0910144902320525),.UNSPECIFIED.)
GEOMETRIC_REPRESENTATION_ITEM()
RATIONAL_B_SPLINE_SURFACE(((0.998486152291889,0.998486152291889,0.998486152291889,
0.992772345172014,0.990020524139833),(0.998486152291889,0.998486152291889,
0.998486152291889,0.992772345172014,0.990020524139833)))
REPRESENTATION_ITEM('')
SURFACE()
);
#3792=(
BOUNDED_SURFACE()
B_SPLINE_SURFACE(1,2,((#158974,#158975,#158976,#158977,#158978),(#158979,
#158980,#158981,#158982,#158983)),.UNSPECIFIED.,.F.,.F.,.F.)
B_SPLINE_SURFACE_WITH_KNOTS((2,2),(3,2,3),(0.,0.0614498483525196),(0.659832011354072,
0.659901408087466,0.666841081426897),.UNSPECIFIED.)
GEOMETRIC_REPRESENTATION_ITEM()
RATIONAL_B_SPLINE_SURFACE(((0.99088978883629,0.99088978883629,0.99088978883629,
0.989616401900862,0.988816334712146),(0.99088978883629,0.99088978883629,
0.99088978883629,0.989616401900862,0.988816334712146)))
REPRESENTATION_ITEM('')
SURFACE()
);
#3793=(
BOUNDED_SURFACE()
B_SPLINE_SURFACE(1,2,((#158985,#158986,#158987),(#158988,#158989,#158990)),
 .UNSPECIFIED.,.F.,.F.,.F.)
B_SPLINE_SURFACE_WITH_KNOTS((2,2),(3,3),(0.947118453120175,1.),(0.659860018385517,
0.666841081426897),.UNSPECIFIED.)
GEOMETRIC_REPRESENTATION_ITEM()
RATIONAL_B_SPLINE_SURFACE(((0.990904995179386,0.989621173673373,0.988816334712145),
(0.990904995179386,0.989621173673373,0.988816334712145)))
REPRESENTATION_ITEM('')
SURFACE()
);
#3794=(
BOUNDED_SURFACE()
B_SPLINE_SURFACE(1,2,((#159001,#159002,#159003,#159004,#159005),(#159006,
#159007,#159008,#159009,#159010)),.UNSPECIFIED.,.F.,.F.,.F.)
B_SPLINE_SURFACE_WITH_KNOTS((2,2),(3,2,3),(0.947095459621871,1.),(0.0665257254736559,
0.0714285714285714,0.0736968668684826),.UNSPECIFIED.)
GEOMETRIC_REPRESENTATION_ITEM()
RATIONAL_B_SPLINE_SURFACE(((0.996794362316491,0.998279055819231,1.,0.999203807365462,
0.998458182734345),(0.996794362316491,0.998279055819231,1.,0.999203807365462,
0.998458182734345)))
REPRESENTATION_ITEM('')
SURFACE()
);
#3795=(
BOUNDED_SURFACE()
B_SPLINE_SURFACE(1,2,((#159018,#159019,#159020,#159021,#159022),(#159023,
#159024,#159025,#159026,#159027)),.UNSPECIFIED.,.F.,.F.,.F.)
B_SPLINE_SURFACE_WITH_KNOTS((2,2),(3,2,3),(0.,0.0614231408718263),(0.0665257254736557,
0.0714285714285714,0.0736543502199203),.UNSPECIFIED.)
GEOMETRIC_REPRESENTATION_ITEM()
RATIONAL_B_SPLINE_SURFACE(((0.996794362316491,0.998279055819231,1.,0.999218731101513,
0.998486152291874),(0.996794362316491,0.998279055819231,1.,0.999218731101513,
0.998486152291874)))
REPRESENTATION_ITEM('')
SURFACE()
);
#3796=(
BOUNDED_SURFACE()
B_SPLINE_SURFACE(1,2,((#159029,#159030,#159031,#159032,#159033),(#159034,
#159035,#159036,#159037,#159038)),.UNSPECIFIED.,.F.,.F.,.F.)
B_SPLINE_SURFACE_WITH_KNOTS((2,2),(3,2,3),(0.817194107660848,1.),(0.642474614281366,
0.642857142857143,0.659901408087502),.UNSPECIFIED.)
GEOMETRIC_REPRESENTATION_ITEM()
RATIONAL_B_SPLINE_SURFACE(((0.999732896029237,0.999865728939372,1.,0.994017305594874,
0.990889788836277),(0.999732896029237,0.999865728939372,1.,0.994017305594874,
0.990889788836277)))
REPRESENTATION_ITEM('')
SURFACE()
);
#3797=(
BOUNDED_SURFACE()
B_SPLINE_SURFACE(1,2,((#159049,#159050,#159051,#159052,#159053),(#159054,
#159055,#159056,#159057,#159058)),.UNSPECIFIED.,.F.,.F.,.F.)
B_SPLINE_SURFACE_WITH_KNOTS((2,2),(3,2,3),(0.817114621578814,1.),(0.0734807488197752,
0.0736543502198967,0.0910144902320526),.UNSPECIFIED.)
GEOMETRIC_REPRESENTATION_ITEM()
RATIONAL_B_SPLINE_SURFACE(((0.998486152291889,0.998486152291889,0.998486152291889,
0.992772345172013,0.990020524139833),(0.998486152291889,0.998486152291889,
0.998486152291889,0.992772345172013,0.990020524139833)))
REPRESENTATION_ITEM('')
SURFACE()
);
#3798=(
BOUNDED_SURFACE()
B_SPLINE_SURFACE(1,2,((#159060,#159061,#159062,#159063,#159064),(#159065,
#159066,#159067,#159068,#159069)),.UNSPECIFIED.,.F.,.F.,.F.)
B_SPLINE_SURFACE_WITH_KNOTS((2,2),(3,2,3),(0.,0.0614498483525172),(0.659832011354072,
0.659901408087466,0.666841081426896),.UNSPECIFIED.)
GEOMETRIC_REPRESENTATION_ITEM()
RATIONAL_B_SPLINE_SURFACE(((0.99088978883629,0.99088978883629,0.99088978883629,
0.989616401900862,0.988816334712146),(0.99088978883629,0.99088978883629,
0.99088978883629,0.989616401900862,0.988816334712146)))
REPRESENTATION_ITEM('')
SURFACE()
);
#3799=(
BOUNDED_SURFACE()
B_SPLINE_SURFACE(1,2,((#159071,#159072,#159073),(#159074,#159075,#159076)),
 .UNSPECIFIED.,.F.,.F.,.F.)
B_SPLINE_SURFACE_WITH_KNOTS((2,2),(3,3),(0.947118453120173,1.),(0.659860018385517,
0.666841081426897),.UNSPECIFIED.)
GEOMETRIC_REPRESENTATION_ITEM()
RATIONAL_B_SPLINE_SURFACE(((0.990904995179385,0.989621173673373,0.988816334712145),
(0.990904995179385,0.989621173673373,0.988816334712145)))
REPRESENTATION_ITEM('')
SURFACE()
);
#3800=(
BOUNDED_SURFACE()
B_SPLINE_SURFACE(1,2,((#159087,#159088,#159089,#159090,#159091),(#159092,
#159093,#159094,#159095,#159096)),.UNSPECIFIED.,.F.,.F.,.F.)
B_SPLINE_SURFACE_WITH_KNOTS((2,2),(3,2,3),(0.947095459621873,1.),(0.0665257254736566,
0.0714285714285714,0.0736968668684826),.UNSPECIFIED.)
GEOMETRIC_REPRESENTATION_ITEM()
RATIONAL_B_SPLINE_SURFACE(((0.996794362316492,0.998279055819231,1.,0.999203807365462,
0.998458182734345),(0.996794362316492,0.998279055819231,1.,0.999203807365462,
0.998458182734345)))
REPRESENTATION_ITEM('')
SURFACE()
);
#3801=(
BOUNDED_SURFACE()
B_SPLINE_SURFACE(1,2,((#159104,#159105,#159106,#159107,#159108),(#159109,
#159110,#159111,#159112,#159113)),.UNSPECIFIED.,.F.,.F.,.F.)
B_SPLINE_SURFACE_WITH_KNOTS((2,2),(3,2,3),(0.,0.0614231408718205),(0.0665257254736566,
0.0714285714285714,0.0736543502199202),.UNSPECIFIED.)
GEOMETRIC_REPRESENTATION_ITEM()
RATIONAL_B_SPLINE_SURFACE(((0.996794362316492,0.998279055819231,1.,0.999218731101513,
0.998486152291874),(0.996794362316492,0.998279055819231,1.,0.999218731101513,
0.998486152291874)))
REPRESENTATION_ITEM('')
SURFACE()
);
#3802=(
BOUNDED_SURFACE()
B_SPLINE_SURFACE(1,2,((#159115,#159116,#159117,#159118,#159119),(#159120,
#159121,#159122,#159123,#159124)),.UNSPECIFIED.,.F.,.F.,.F.)
B_SPLINE_SURFACE_WITH_KNOTS((2,2),(3,2,3),(0.817194107660853,1.),(0.642474614281367,
0.642857142857143,0.659901408087502),.UNSPECIFIED.)
GEOMETRIC_REPRESENTATION_ITEM()
RATIONAL_B_SPLINE_SURFACE(((0.999732896029238,0.999865728939373,1.,0.994017305594874,
0.990889788836276),(0.999732896029238,0.999865728939373,1.,0.994017305594874,
0.990889788836276)))
REPRESENTATION_ITEM('')
SURFACE()
);
#3803=(
BOUNDED_SURFACE()
B_SPLINE_SURFACE(1,2,((#159135,#159136,#159137,#159138,#159139),(#159140,
#159141,#159142,#159143,#159144)),.UNSPECIFIED.,.F.,.F.,.F.)
B_SPLINE_SURFACE_WITH_KNOTS((2,2),(3,2,3),(0.817114621578814,1.),(0.0734807488197738,
0.0736543502198954,0.0910144902320515),.UNSPECIFIED.)
GEOMETRIC_REPRESENTATION_ITEM()
RATIONAL_B_SPLINE_SURFACE(((0.99848615229189,0.99848615229189,0.99848615229189,
0.992772345172014,0.990020524139833),(0.99848615229189,0.99848615229189,
0.99848615229189,0.992772345172014,0.990020524139833)))
REPRESENTATION_ITEM('')
SURFACE()
);
#3804=(
BOUNDED_SURFACE()
B_SPLINE_SURFACE(1,2,((#159146,#159147,#159148,#159149,#159150),(#159151,
#159152,#159153,#159154,#159155)),.UNSPECIFIED.,.F.,.F.,.F.)
B_SPLINE_SURFACE_WITH_KNOTS((2,2),(3,2,3),(0.,0.061449848352509),(0.659832011354073,
0.659901408087467,0.666841081426896),.UNSPECIFIED.)
GEOMETRIC_REPRESENTATION_ITEM()
RATIONAL_B_SPLINE_SURFACE(((0.990889788836289,0.990889788836289,0.990889788836289,
0.989616401900862,0.988816334712146),(0.990889788836289,0.990889788836289,
0.990889788836289,0.989616401900862,0.988816334712146)))
REPRESENTATION_ITEM('')
SURFACE()
);
#3805=(
BOUNDED_SURFACE()
B_SPLINE_SURFACE(1,2,((#159157,#159158,#159159),(#159160,#159161,#159162)),
 .UNSPECIFIED.,.F.,.F.,.F.)
B_SPLINE_SURFACE_WITH_KNOTS((2,2),(3,3),(0.947118453120178,1.),(0.659860018385642,
0.666841081426896),.UNSPECIFIED.)
GEOMETRIC_REPRESENTATION_ITEM()
RATIONAL_B_SPLINE_SURFACE(((0.990904995179339,0.989621173673359,0.988816334712145),
(0.990904995179339,0.989621173673359,0.988816334712145)))
REPRESENTATION_ITEM('')
SURFACE()
);
#3806=(
BOUNDED_SURFACE()
B_SPLINE_SURFACE(1,2,((#159173,#159174,#159175,#159176,#159177),(#159178,
#159179,#159180,#159181,#159182)),.UNSPECIFIED.,.F.,.F.,.F.)
B_SPLINE_SURFACE_WITH_KNOTS((2,2),(3,2,3),(0.947095459621874,1.),(0.0665257254736559,
0.0714285714285714,0.073696866868496),.UNSPECIFIED.)
GEOMETRIC_REPRESENTATION_ITEM()
RATIONAL_B_SPLINE_SURFACE(((0.996794362316491,0.998279055819231,1.,0.999203807365457,
0.998458182734337),(0.996794362316491,0.998279055819231,1.,0.999203807365457,
0.998458182734337)))
REPRESENTATION_ITEM('')
SURFACE()
);
#3807=(
BOUNDED_SURFACE()
B_SPLINE_SURFACE(1,2,((#159189,#159190,#159191,#159192,#159193),(#159194,
#159195,#159196,#159197,#159198)),.UNSPECIFIED.,.F.,.F.,.F.)
B_SPLINE_SURFACE_WITH_KNOTS((2,2),(3,2,3),(0.,0.0614231408718213),(0.0665257254736558,
0.0714285714285714,0.0736543502199218),.UNSPECIFIED.)
GEOMETRIC_REPRESENTATION_ITEM()
RATIONAL_B_SPLINE_SURFACE(((0.996794362316491,0.998279055819231,1.,0.999218731101512,
0.998486152291873),(0.996794362316491,0.998279055819231,1.,0.999218731101512,
0.998486152291873)))
REPRESENTATION_ITEM('')
SURFACE()
);
#3808=(
BOUNDED_SURFACE()
B_SPLINE_SURFACE(1,2,((#159200,#159201,#159202,#159203,#159204),(#159205,
#159206,#159207,#159208,#159209)),.UNSPECIFIED.,.F.,.F.,.F.)
B_SPLINE_SURFACE_WITH_KNOTS((2,2),(3,2,3),(0.817194107660858,1.),(0.642474614281364,
0.642857142857143,0.659901408087509),.UNSPECIFIED.)
GEOMETRIC_REPRESENTATION_ITEM()
RATIONAL_B_SPLINE_SURFACE(((0.999732896029236,0.999865728939372,1.,0.994017305594872,
0.990889788836274),(0.999732896029236,0.999865728939372,1.,0.994017305594872,
0.990889788836274)))
REPRESENTATION_ITEM('')
SURFACE()
);
#3809=(
BOUNDED_SURFACE()
B_SPLINE_SURFACE(1,2,((#159220,#159221,#159222,#159223,#159224),(#159225,
#159226,#159227,#159228,#159229)),.UNSPECIFIED.,.F.,.F.,.F.)
B_SPLINE_SURFACE_WITH_KNOTS((2,2),(3,2,3),(0.817114621578823,1.),(0.0734807488197823,
0.0736543502199038,0.0910144902320512),.UNSPECIFIED.)
GEOMETRIC_REPRESENTATION_ITEM()
RATIONAL_B_SPLINE_SURFACE(((0.998486152291885,0.998486152291885,0.998486152291885,
0.992772345172013,0.990020524139833),(0.998486152291885,0.998486152291885,
0.998486152291885,0.992772345172013,0.990020524139833)))
REPRESENTATION_ITEM('')
SURFACE()
);
#3810=(
BOUNDED_SURFACE()
B_SPLINE_SURFACE(1,2,((#159231,#159232,#159233,#159234,#159235),(#159236,
#159237,#159238,#159239,#159240)),.UNSPECIFIED.,.F.,.F.,.F.)
B_SPLINE_SURFACE_WITH_KNOTS((2,2),(3,2,3),(0.,0.061449848352437),(0.659832011354082,
0.659901408087476,0.666841081426897),.UNSPECIFIED.)
GEOMETRIC_REPRESENTATION_ITEM()
RATIONAL_B_SPLINE_SURFACE(((0.990889788836286,0.990889788836286,0.990889788836286,
0.989616401900861,0.988816334712145),(0.990889788836286,0.990889788836286,
0.990889788836286,0.989616401900861,0.988816334712145)))
REPRESENTATION_ITEM('')
SURFACE()
);
#3811=(
BOUNDED_SURFACE()
B_SPLINE_SURFACE(1,2,((#159242,#159243,#159244),(#159245,#159246,#159247)),
 .UNSPECIFIED.,.F.,.F.,.F.)
B_SPLINE_SURFACE_WITH_KNOTS((2,2),(3,3),(0.947118453120176,1.),(0.659860018385516,
0.666841081426898),.UNSPECIFIED.)
GEOMETRIC_REPRESENTATION_ITEM()
RATIONAL_B_SPLINE_SURFACE(((0.990904995179386,0.989621173673373,0.988816334712145),
(0.990904995179386,0.989621173673373,0.988816334712145)))
REPRESENTATION_ITEM('')
SURFACE()
);
#3812=(
BOUNDED_SURFACE()
B_SPLINE_SURFACE(1,2,((#159258,#159259,#159260,#159261,#159262),(#159263,
#159264,#159265,#159266,#159267)),.UNSPECIFIED.,.F.,.F.,.F.)
B_SPLINE_SURFACE_WITH_KNOTS((2,2),(3,2,3),(0.947095459621877,1.),(0.0665257254736565,
0.0714285714285714,0.0736968668684898),.UNSPECIFIED.)
GEOMETRIC_REPRESENTATION_ITEM()
RATIONAL_B_SPLINE_SURFACE(((0.996794362316492,0.998279055819231,1.,0.999203807365459,
0.998458182734341),(0.996794362316492,0.998279055819231,1.,0.999203807365459,
0.998458182734341)))
REPRESENTATION_ITEM('')
SURFACE()
);
#3813=(
BOUNDED_SURFACE()
B_SPLINE_SURFACE(1,2,((#159274,#159275,#159276,#159277,#159278),(#159279,
#159280,#159281,#159282,#159283)),.UNSPECIFIED.,.F.,.F.,.F.)
B_SPLINE_SURFACE_WITH_KNOTS((2,2),(3,2,3),(0.,0.0614231408718177),(0.0665257254736564,
0.0714285714285714,0.0736543502199223),.UNSPECIFIED.)
GEOMETRIC_REPRESENTATION_ITEM()
RATIONAL_B_SPLINE_SURFACE(((0.996794362316491,0.998279055819231,1.,0.999218731101512,
0.998486152291872),(0.996794362316491,0.998279055819231,1.,0.999218731101512,
0.998486152291872)))
REPRESENTATION_ITEM('')
SURFACE()
);
#3814=(
BOUNDED_SURFACE()
B_SPLINE_SURFACE(1,2,((#159285,#159286,#159287,#159288,#159289),(#159290,
#159291,#159292,#159293,#159294)),.UNSPECIFIED.,.F.,.F.,.F.)
B_SPLINE_SURFACE_WITH_KNOTS((2,2),(3,2,3),(0.81719410766085,1.),(0.642474614281364,
0.642857142857143,0.65990140808751),.UNSPECIFIED.)
GEOMETRIC_REPRESENTATION_ITEM()
RATIONAL_B_SPLINE_SURFACE(((0.999732896029236,0.999865728939372,1.,0.994017305594871,
0.990889788836273),(0.999732896029236,0.999865728939372,1.,0.994017305594871,
0.990889788836273)))
REPRESENTATION_ITEM('')
SURFACE()
);
#3815=(
BOUNDED_SURFACE()
B_SPLINE_SURFACE(1,2,((#159305,#159306,#159307,#159308,#159309),(#159310,
#159311,#159312,#159313,#159314)),.UNSPECIFIED.,.F.,.F.,.F.)
B_SPLINE_SURFACE_WITH_KNOTS((2,2),(3,2,3),(0.817114621578814,1.),(0.0734807488197824,
0.0736543502199039,0.0910144902320515),.UNSPECIFIED.)
GEOMETRIC_REPRESENTATION_ITEM()
RATIONAL_B_SPLINE_SURFACE(((0.998486152291885,0.998486152291885,0.998486152291885,
0.992772345172013,0.990020524139833),(0.998486152291885,0.998486152291885,
0.998486152291885,0.992772345172013,0.990020524139833)))
REPRESENTATION_ITEM('')
SURFACE()
);
#3816=(
BOUNDED_SURFACE()
B_SPLINE_SURFACE(1,2,((#159316,#159317,#159318,#159319,#159320),(#159321,
#159322,#159323,#159324,#159325)),.UNSPECIFIED.,.F.,.F.,.F.)
B_SPLINE_SURFACE_WITH_KNOTS((2,2),(3,2,3),(0.,0.0614498483524338),(0.659832011354082,
0.659901408087476,0.666841081426897),.UNSPECIFIED.)
GEOMETRIC_REPRESENTATION_ITEM()
RATIONAL_B_SPLINE_SURFACE(((0.990889788836286,0.990889788836286,0.990889788836286,
0.989616401900861,0.988816334712145),(0.990889788836286,0.990889788836286,
0.990889788836286,0.989616401900861,0.988816334712145)))
REPRESENTATION_ITEM('')
SURFACE()
);
#3817=(
BOUNDED_SURFACE()
B_SPLINE_SURFACE(1,2,((#159327,#159328,#159329),(#159330,#159331,#159332)),
 .UNSPECIFIED.,.F.,.F.,.F.)
B_SPLINE_SURFACE_WITH_KNOTS((2,2),(3,3),(0.947118453120174,1.),(0.65986001838565,
0.666841081426897),.UNSPECIFIED.)
GEOMETRIC_REPRESENTATION_ITEM()
RATIONAL_B_SPLINE_SURFACE(((0.990904995179336,0.989621173673358,0.988816334712146),
(0.990904995179336,0.989621173673358,0.988816334712146)))
REPRESENTATION_ITEM('')
SURFACE()
);
#3818=(
BOUNDED_SURFACE()
B_SPLINE_SURFACE(1,2,((#159343,#159344,#159345,#159346,#159347),(#159348,
#159349,#159350,#159351,#159352)),.UNSPECIFIED.,.F.,.F.,.F.)
B_SPLINE_SURFACE_WITH_KNOTS((2,2),(3,2,3),(0.947095459621875,1.),(0.066525725473656,
0.0714285714285714,0.0736968668684961),.UNSPECIFIED.)
GEOMETRIC_REPRESENTATION_ITEM()
RATIONAL_B_SPLINE_SURFACE(((0.996794362316491,0.998279055819231,1.,0.999203807365457,
0.998458182734336),(0.996794362316491,0.998279055819231,1.,0.999203807365457,
0.998458182734336)))
REPRESENTATION_ITEM('')
SURFACE()
);
#3819=(
BOUNDED_SURFACE()
B_SPLINE_SURFACE(1,2,((#159360,#159361,#159362,#159363,#159364),(#159365,
#159366,#159367,#159368,#159369)),.UNSPECIFIED.,.F.,.F.,.F.)
B_SPLINE_SURFACE_WITH_KNOTS((2,2),(3,2,3),(0.,0.0614231408718178),(0.0665257254736559,
0.0714285714285714,0.0736543502199197),.UNSPECIFIED.)
GEOMETRIC_REPRESENTATION_ITEM()
RATIONAL_B_SPLINE_SURFACE(((0.996794362316491,0.998279055819231,1.,0.999218731101513,
0.998486152291874),(0.996794362316491,0.998279055819231,1.,0.999218731101513,
0.998486152291874)))
REPRESENTATION_ITEM('')
SURFACE()
);
#3820=(
BOUNDED_SURFACE()
B_SPLINE_SURFACE(1,2,((#159371,#159372,#159373,#159374,#159375),(#159376,
#159377,#159378,#159379,#159380)),.UNSPECIFIED.,.F.,.F.,.F.)
B_SPLINE_SURFACE_WITH_KNOTS((2,2),(3,2,3),(0.817194107660853,1.),(0.642474614281364,
0.642857142857143,0.659901408087504),.UNSPECIFIED.)
GEOMETRIC_REPRESENTATION_ITEM()
RATIONAL_B_SPLINE_SURFACE(((0.999732896029236,0.999865728939372,1.,0.994017305594873,
0.990889788836276),(0.999732896029236,0.999865728939372,1.,0.994017305594873,
0.990889788836276)))
REPRESENTATION_ITEM('')
SURFACE()
);
#3821=(
BOUNDED_SURFACE()
B_SPLINE_SURFACE(1,2,((#159391,#159392,#159393,#159394,#159395),(#159396,
#159397,#159398,#159399,#159400)),.UNSPECIFIED.,.F.,.F.,.F.)
B_SPLINE_SURFACE_WITH_KNOTS((2,2),(3,2,3),(0.817114621578816,1.),(0.0734807488197741,
0.0736543502198956,0.09101449023205),.UNSPECIFIED.)
GEOMETRIC_REPRESENTATION_ITEM()
RATIONAL_B_SPLINE_SURFACE(((0.99848615229189,0.99848615229189,0.99848615229189,
0.992772345172014,0.990020524139834),(0.99848615229189,0.99848615229189,
0.99848615229189,0.992772345172014,0.990020524139834)))
REPRESENTATION_ITEM('')
SURFACE()
);
#3822=(
BOUNDED_SURFACE()
B_SPLINE_SURFACE(1,2,((#159402,#159403,#159404,#159405,#159406),(#159407,
#159408,#159409,#159410,#159411)),.UNSPECIFIED.,.F.,.F.,.F.)
B_SPLINE_SURFACE_WITH_KNOTS((2,2),(3,2,3),(0.,0.0614498483525083),(0.659832011354073,
0.659901408087467,0.666841081426896),.UNSPECIFIED.)
GEOMETRIC_REPRESENTATION_ITEM()
RATIONAL_B_SPLINE_SURFACE(((0.990889788836289,0.990889788836289,0.990889788836289,
0.989616401900862,0.988816334712146),(0.990889788836289,0.990889788836289,
0.990889788836289,0.989616401900862,0.988816334712146)))
REPRESENTATION_ITEM('')
SURFACE()
);
#3823=(
BOUNDED_SURFACE()
B_SPLINE_SURFACE(1,2,((#159413,#159414,#159415),(#159416,#159417,#159418)),
 .UNSPECIFIED.,.F.,.F.,.F.)
B_SPLINE_SURFACE_WITH_KNOTS((2,2),(3,3),(0.947118453120185,1.),(0.659860018385516,
0.666841081426897),.UNSPECIFIED.)
GEOMETRIC_REPRESENTATION_ITEM()
RATIONAL_B_SPLINE_SURFACE(((0.990904995179386,0.989621173673373,0.988816334712145),
(0.990904995179386,0.989621173673373,0.988816334712145)))
REPRESENTATION_ITEM('')
SURFACE()
);
#3824=(
BOUNDED_SURFACE()
B_SPLINE_SURFACE(1,2,((#159429,#159430,#159431,#159432,#159433),(#159434,
#159435,#159436,#159437,#159438)),.UNSPECIFIED.,.F.,.F.,.F.)
B_SPLINE_SURFACE_WITH_KNOTS((2,2),(3,2,3),(0.947095459621886,1.),(0.0665257254736562,
0.0714285714285714,0.0736968668684815),.UNSPECIFIED.)
GEOMETRIC_REPRESENTATION_ITEM()
RATIONAL_B_SPLINE_SURFACE(((0.996794362316491,0.998279055819231,1.,0.999203807365462,
0.998458182734346),(0.996794362316491,0.998279055819231,1.,0.999203807365462,
0.998458182734346)))
REPRESENTATION_ITEM('')
SURFACE()
);
#3825=(
BOUNDED_SURFACE()
B_SPLINE_SURFACE(1,2,((#159446,#159447,#159448,#159449,#159450),(#159451,
#159452,#159453,#159454,#159455)),.UNSPECIFIED.,.F.,.F.,.F.)
B_SPLINE_SURFACE_WITH_KNOTS((2,2),(3,2,3),(0.,0.0614231408718172),(0.0665257254736562,
0.0714285714285714,0.07365435021992),.UNSPECIFIED.)
GEOMETRIC_REPRESENTATION_ITEM()
RATIONAL_B_SPLINE_SURFACE(((0.996794362316491,0.998279055819231,1.,0.999218731101513,
0.998486152291874),(0.996794362316491,0.998279055819231,1.,0.999218731101513,
0.998486152291874)))
REPRESENTATION_ITEM('')
SURFACE()
);
#3826=(
BOUNDED_SURFACE()
B_SPLINE_SURFACE(1,2,((#159457,#159458,#159459,#159460,#159461),(#159462,
#159463,#159464,#159465,#159466)),.UNSPECIFIED.,.F.,.F.,.F.)
B_SPLINE_SURFACE_WITH_KNOTS((2,2),(3,2,3),(0.817194107660859,1.),(0.642474614281367,
0.642857142857143,0.659901408087505),.UNSPECIFIED.)
GEOMETRIC_REPRESENTATION_ITEM()
RATIONAL_B_SPLINE_SURFACE(((0.999732896029238,0.999865728939373,1.,0.994017305594873,
0.990889788836275),(0.999732896029238,0.999865728939373,1.,0.994017305594873,
0.990889788836275)))
REPRESENTATION_ITEM('')
SURFACE()
);
#3827=(
BOUNDED_SURFACE()
B_SPLINE_SURFACE(1,2,((#159477,#159478,#159479,#159480,#159481),(#159482,
#159483,#159484,#159485,#159486)),.UNSPECIFIED.,.F.,.F.,.F.)
B_SPLINE_SURFACE_WITH_KNOTS((2,2),(3,2,3),(0.817114621578821,1.),(0.0734807488197739,
0.0736543502198955,0.0910144902320515),.UNSPECIFIED.)
GEOMETRIC_REPRESENTATION_ITEM()
RATIONAL_B_SPLINE_SURFACE(((0.99848615229189,0.99848615229189,0.99848615229189,
0.992772345172014,0.990020524139833),(0.99848615229189,0.99848615229189,
0.99848615229189,0.992772345172014,0.990020524139833)))
REPRESENTATION_ITEM('')
SURFACE()
);
#3828=(
BOUNDED_SURFACE()
B_SPLINE_SURFACE(1,2,((#159488,#159489,#159490,#159491,#159492),(#159493,
#159494,#159495,#159496,#159497)),.UNSPECIFIED.,.F.,.F.,.F.)
B_SPLINE_SURFACE_WITH_KNOTS((2,2),(3,2,3),(0.,0.0614498483525092),(0.659832011354073,
0.659901408087467,0.666841081426896),.UNSPECIFIED.)
GEOMETRIC_REPRESENTATION_ITEM()
RATIONAL_B_SPLINE_SURFACE(((0.990889788836289,0.990889788836289,0.990889788836289,
0.989616401900862,0.988816334712146),(0.990889788836289,0.990889788836289,
0.990889788836289,0.989616401900862,0.988816334712146)))
REPRESENTATION_ITEM('')
SURFACE()
);
#3829=(
BOUNDED_SURFACE()
B_SPLINE_SURFACE(1,2,((#159499,#159500,#159501),(#159502,#159503,#159504)),
 .UNSPECIFIED.,.F.,.F.,.F.)
B_SPLINE_SURFACE_WITH_KNOTS((2,2),(3,3),(0.947118453120178,1.),(0.659860018385642,
0.666841081426896),.UNSPECIFIED.)
GEOMETRIC_REPRESENTATION_ITEM()
RATIONAL_B_SPLINE_SURFACE(((0.990904995179339,0.989621173673359,0.988816334712145),
(0.990904995179339,0.989621173673359,0.988816334712145)))
REPRESENTATION_ITEM('')
SURFACE()
);
#3830=(
BOUNDED_SURFACE()
B_SPLINE_SURFACE(1,2,((#159515,#159516,#159517,#159518,#159519),(#159520,
#159521,#159522,#159523,#159524)),.UNSPECIFIED.,.F.,.F.,.F.)
B_SPLINE_SURFACE_WITH_KNOTS((2,2),(3,2,3),(0.947095459621876,1.),(0.0665257254736561,
0.0714285714285714,0.073696866868496),.UNSPECIFIED.)
GEOMETRIC_REPRESENTATION_ITEM()
RATIONAL_B_SPLINE_SURFACE(((0.996794362316491,0.998279055819231,1.,0.999203807365457,
0.998458182734337),(0.996794362316491,0.998279055819231,1.,0.999203807365457,
0.998458182734337)))
REPRESENTATION_ITEM('')
SURFACE()
);
#3831=(
BOUNDED_SURFACE()
B_SPLINE_SURFACE(1,2,((#159531,#159532,#159533,#159534,#159535),(#159536,
#159537,#159538,#159539,#159540)),.UNSPECIFIED.,.F.,.F.,.F.)
B_SPLINE_SURFACE_WITH_KNOTS((2,2),(3,2,3),(0.,0.0614231408718195),(0.066525725473656,
0.0714285714285714,0.0736543502199191),.UNSPECIFIED.)
GEOMETRIC_REPRESENTATION_ITEM()
RATIONAL_B_SPLINE_SURFACE(((0.996794362316491,0.998279055819231,1.,0.999218731101513,
0.998486152291874),(0.996794362316491,0.998279055819231,1.,0.999218731101513,
0.998486152291874)))
REPRESENTATION_ITEM('')
SURFACE()
);
#3832=(
BOUNDED_SURFACE()
B_SPLINE_SURFACE(1,2,((#159542,#159543,#159544,#159545,#159546),(#159547,
#159548,#159549,#159550,#159551)),.UNSPECIFIED.,.F.,.F.,.F.)
B_SPLINE_SURFACE_WITH_KNOTS((2,2),(3,2,3),(0.817194107660853,1.),(0.642474614281367,
0.642857142857143,0.659901408087503),.UNSPECIFIED.)
GEOMETRIC_REPRESENTATION_ITEM()
RATIONAL_B_SPLINE_SURFACE(((0.999732896029238,0.999865728939373,1.,0.994017305594874,
0.990889788836276),(0.999732896029238,0.999865728939373,1.,0.994017305594874,
0.990889788836276)))
REPRESENTATION_ITEM('')
SURFACE()
);
#3833=(
BOUNDED_SURFACE()
B_SPLINE_SURFACE(1,2,((#159562,#159563,#159564,#159565,#159566),(#159567,
#159568,#159569,#159570,#159571)),.UNSPECIFIED.,.F.,.F.,.F.)
B_SPLINE_SURFACE_WITH_KNOTS((2,2),(3,2,3),(0.817114621578811,1.),(0.0734807488197823,
0.0736543502199038,0.0910144902320515),.UNSPECIFIED.)
GEOMETRIC_REPRESENTATION_ITEM()
RATIONAL_B_SPLINE_SURFACE(((0.998486152291884,0.998486152291884,0.998486152291884,
0.992772345172013,0.990020524139833),(0.998486152291884,0.998486152291884,
0.998486152291884,0.992772345172013,0.990020524139833)))
REPRESENTATION_ITEM('')
SURFACE()
);
#3834=(
BOUNDED_SURFACE()
B_SPLINE_SURFACE(1,2,((#159573,#159574,#159575,#159576,#159577),(#159578,
#159579,#159580,#159581,#159582)),.UNSPECIFIED.,.F.,.F.,.F.)
B_SPLINE_SURFACE_WITH_KNOTS((2,2),(3,2,3),(0.,0.0614498483524293),(0.659832011354082,
0.659901408087476,0.666841081426896),.UNSPECIFIED.)
GEOMETRIC_REPRESENTATION_ITEM()
RATIONAL_B_SPLINE_SURFACE(((0.990889788836286,0.990889788836286,0.990889788836286,
0.989616401900861,0.988816334712146),(0.990889788836286,0.990889788836286,
0.990889788836286,0.989616401900861,0.988816334712146)))
REPRESENTATION_ITEM('')
SURFACE()
);
#3835=(
BOUNDED_SURFACE()
B_SPLINE_SURFACE(1,2,((#159584,#159585,#159586),(#159587,#159588,#159589)),
 .UNSPECIFIED.,.F.,.F.,.F.)
B_SPLINE_SURFACE_WITH_KNOTS((2,2),(3,3),(0.947118453120178,1.),(0.65986001838565,
0.666841081426896),.UNSPECIFIED.)
GEOMETRIC_REPRESENTATION_ITEM()
RATIONAL_B_SPLINE_SURFACE(((0.990904995179336,0.989621173673358,0.988816334712146),
(0.990904995179336,0.989621173673358,0.988816334712146)))
REPRESENTATION_ITEM('')
SURFACE()
);
#3836=(
BOUNDED_SURFACE()
B_SPLINE_SURFACE(1,2,((#159600,#159601,#159602,#159603,#159604),(#159605,
#159606,#159607,#159608,#159609)),.UNSPECIFIED.,.F.,.F.,.F.)
B_SPLINE_SURFACE_WITH_KNOTS((2,2),(3,2,3),(0.947095459621872,1.),(0.0665257254736559,
0.0714285714285714,0.0736968668684958),.UNSPECIFIED.)
GEOMETRIC_REPRESENTATION_ITEM()
RATIONAL_B_SPLINE_SURFACE(((0.996794362316491,0.998279055819231,1.,0.999203807365457,
0.998458182734337),(0.996794362316491,0.998279055819231,1.,0.999203807365457,
0.998458182734337)))
REPRESENTATION_ITEM('')
SURFACE()
);
#3837=(
BOUNDED_SURFACE()
B_SPLINE_SURFACE(1,2,((#159616,#159617,#159618,#159619,#159620),(#159621,
#159622,#159623,#159624,#159625)),.UNSPECIFIED.,.F.,.F.,.F.)
B_SPLINE_SURFACE_WITH_KNOTS((2,2),(3,2,3),(0.,0.0614231408718199),(0.066525725473656,
0.0714285714285714,0.0736543502199191),.UNSPECIFIED.)
GEOMETRIC_REPRESENTATION_ITEM()
RATIONAL_B_SPLINE_SURFACE(((0.996794362316491,0.998279055819231,1.,0.999218731101513,
0.998486152291874),(0.996794362316491,0.998279055819231,1.,0.999218731101513,
0.998486152291874)))
REPRESENTATION_ITEM('')
SURFACE()
);
#3838=(
BOUNDED_SURFACE()
B_SPLINE_SURFACE(1,2,((#159627,#159628,#159629,#159630,#159631),(#159632,
#159633,#159634,#159635,#159636)),.UNSPECIFIED.,.F.,.F.,.F.)
B_SPLINE_SURFACE_WITH_KNOTS((2,2),(3,2,3),(0.817194107660855,1.),(0.642474614281364,
0.642857142857143,0.659901408087503),.UNSPECIFIED.)
GEOMETRIC_REPRESENTATION_ITEM()
RATIONAL_B_SPLINE_SURFACE(((0.999732896029236,0.999865728939372,1.,0.994017305594874,
0.990889788836276),(0.999732896029236,0.999865728939372,1.,0.994017305594874,
0.990889788836276)))
REPRESENTATION_ITEM('')
SURFACE()
);
#3839=(
BOUNDED_SURFACE()
B_SPLINE_SURFACE(1,2,((#159647,#159648,#159649,#159650,#159651),(#159652,
#159653,#159654,#159655,#159656)),.UNSPECIFIED.,.F.,.F.,.F.)
B_SPLINE_SURFACE_WITH_KNOTS((2,2),(3,2,3),(0.817114621578814,1.),(0.0734807488197738,
0.0736543502198954,0.0910144902320515),.UNSPECIFIED.)
GEOMETRIC_REPRESENTATION_ITEM()
RATIONAL_B_SPLINE_SURFACE(((0.99848615229189,0.99848615229189,0.99848615229189,
0.992772345172014,0.990020524139833),(0.99848615229189,0.99848615229189,
0.99848615229189,0.992772345172014,0.990020524139833)))
REPRESENTATION_ITEM('')
SURFACE()
);
#3840=(
BOUNDED_SURFACE()
B_SPLINE_SURFACE(1,2,((#159658,#159659,#159660,#159661,#159662),(#159663,
#159664,#159665,#159666,#159667)),.UNSPECIFIED.,.F.,.F.,.F.)
B_SPLINE_SURFACE_WITH_KNOTS((2,2),(3,2,3),(0.,0.0614498483525101),(0.659832011354073,
0.659901408087467,0.666841081426897),.UNSPECIFIED.)
GEOMETRIC_REPRESENTATION_ITEM()
RATIONAL_B_SPLINE_SURFACE(((0.990889788836289,0.990889788836289,0.990889788836289,
0.989616401900862,0.988816334712145),(0.990889788836289,0.990889788836289,
0.990889788836289,0.989616401900862,0.988816334712145)))
REPRESENTATION_ITEM('')
SURFACE()
);
#3841=(
BOUNDED_SURFACE()
B_SPLINE_SURFACE(1,2,((#159669,#159670,#159671),(#159672,#159673,#159674)),
 .UNSPECIFIED.,.F.,.F.,.F.)
B_SPLINE_SURFACE_WITH_KNOTS((2,2),(3,3),(0.947118453120179,1.),(0.659860018385518,
0.666841081426897),.UNSPECIFIED.)
GEOMETRIC_REPRESENTATION_ITEM()
RATIONAL_B_SPLINE_SURFACE(((0.990904995179385,0.989621173673373,0.988816334712145),
(0.990904995179385,0.989621173673373,0.988816334712145)))
REPRESENTATION_ITEM('')
SURFACE()
);
#3842=(
BOUNDED_SURFACE()
B_SPLINE_SURFACE(1,2,((#159685,#159686,#159687,#159688,#159689),(#159690,
#159691,#159692,#159693,#159694)),.UNSPECIFIED.,.F.,.F.,.F.)
B_SPLINE_SURFACE_WITH_KNOTS((2,2),(3,2,3),(0.947095459621877,1.),(0.0665257254736561,
0.0714285714285714,0.0736968668684814),.UNSPECIFIED.)
GEOMETRIC_REPRESENTATION_ITEM()
RATIONAL_B_SPLINE_SURFACE(((0.996794362316491,0.998279055819231,1.,0.999203807365462,
0.998458182734346),(0.996794362316491,0.998279055819231,1.,0.999203807365462,
0.998458182734346)))
REPRESENTATION_ITEM('')
SURFACE()
);
#3843=(
BOUNDED_SURFACE()
B_SPLINE_SURFACE(1,2,((#159702,#159703,#159704,#159705,#159706),(#159707,
#159708,#159709,#159710,#159711)),.UNSPECIFIED.,.F.,.F.,.F.)
B_SPLINE_SURFACE_WITH_KNOTS((2,2),(3,2,3),(0.,0.0614231408718166),(0.066525725473656,
0.0714285714285714,0.0736543502199191),.UNSPECIFIED.)
GEOMETRIC_REPRESENTATION_ITEM()
RATIONAL_B_SPLINE_SURFACE(((0.996794362316491,0.998279055819231,1.,0.999218731101513,
0.998486152291874),(0.996794362316491,0.998279055819231,1.,0.999218731101513,
0.998486152291874)))
REPRESENTATION_ITEM('')
SURFACE()
);
#3844=(
BOUNDED_SURFACE()
B_SPLINE_SURFACE(1,2,((#159713,#159714,#159715,#159716,#159717),(#159718,
#159719,#159720,#159721,#159722)),.UNSPECIFIED.,.F.,.F.,.F.)
B_SPLINE_SURFACE_WITH_KNOTS((2,2),(3,2,3),(0.817194107660858,1.),(0.642474614281366,
0.642857142857143,0.659901408087503),.UNSPECIFIED.)
GEOMETRIC_REPRESENTATION_ITEM()
RATIONAL_B_SPLINE_SURFACE(((0.999732896029237,0.999865728939372,1.,0.994017305594874,
0.990889788836276),(0.999732896029237,0.999865728939372,1.,0.994017305594874,
0.990889788836276)))
REPRESENTATION_ITEM('')
SURFACE()
);
#3845=(
BOUNDED_SURFACE()
B_SPLINE_SURFACE(1,2,((#159733,#159734,#159735,#159736,#159737),(#159738,
#159739,#159740,#159741,#159742)),.UNSPECIFIED.,.F.,.F.,.F.)
B_SPLINE_SURFACE_WITH_KNOTS((2,2),(3,2,3),(0.817114621578819,1.),(0.0734807488197824,
0.0736543502199039,0.0910144902320514),.UNSPECIFIED.)
GEOMETRIC_REPRESENTATION_ITEM()
RATIONAL_B_SPLINE_SURFACE(((0.998486152291884,0.998486152291884,0.998486152291884,
0.992772345172013,0.990020524139833),(0.998486152291884,0.998486152291884,
0.998486152291884,0.992772345172013,0.990020524139833)))
REPRESENTATION_ITEM('')
SURFACE()
);
#3846=(
BOUNDED_SURFACE()
B_SPLINE_SURFACE(1,2,((#159744,#159745,#159746,#159747,#159748),(#159749,
#159750,#159751,#159752,#159753)),.UNSPECIFIED.,.F.,.F.,.F.)
B_SPLINE_SURFACE_WITH_KNOTS((2,2),(3,2,3),(0.,0.0614498483524375),(0.659832011354082,
0.659901408087476,0.666841081426897),.UNSPECIFIED.)
GEOMETRIC_REPRESENTATION_ITEM()
RATIONAL_B_SPLINE_SURFACE(((0.990889788836286,0.990889788836286,0.990889788836286,
0.989616401900861,0.988816334712146),(0.990889788836286,0.990889788836286,
0.990889788836286,0.989616401900861,0.988816334712146)))
REPRESENTATION_ITEM('')
SURFACE()
);
#3847=(
BOUNDED_SURFACE()
B_SPLINE_SURFACE(1,2,((#159755,#159756,#159757),(#159758,#159759,#159760)),
 .UNSPECIFIED.,.F.,.F.,.F.)
B_SPLINE_SURFACE_WITH_KNOTS((2,2),(3,3),(0.947118453120176,1.),(0.65986001838565,
0.666841081426897),.UNSPECIFIED.)
GEOMETRIC_REPRESENTATION_ITEM()
RATIONAL_B_SPLINE_SURFACE(((0.990904995179336,0.989621173673358,0.988816334712145),
(0.990904995179336,0.989621173673358,0.988816334712145)))
REPRESENTATION_ITEM('')
SURFACE()
);
#3848=(
BOUNDED_SURFACE()
B_SPLINE_SURFACE(1,2,((#159771,#159772,#159773,#159774,#159775),(#159776,
#159777,#159778,#159779,#159780)),.UNSPECIFIED.,.F.,.F.,.F.)
B_SPLINE_SURFACE_WITH_KNOTS((2,2),(3,2,3),(0.947095459621878,1.),(0.0665257254736558,
0.0714285714285714,0.0736968668684962),.UNSPECIFIED.)
GEOMETRIC_REPRESENTATION_ITEM()
RATIONAL_B_SPLINE_SURFACE(((0.996794362316491,0.998279055819231,1.,0.999203807365457,
0.998458182734337),(0.996794362316491,0.998279055819231,1.,0.999203807365457,
0.998458182734337)))
REPRESENTATION_ITEM('')
SURFACE()
);
#3849=(
BOUNDED_SURFACE()
B_SPLINE_SURFACE(1,2,((#159787,#159788,#159789,#159790,#159791),(#159792,
#159793,#159794,#159795,#159796)),.UNSPECIFIED.,.F.,.F.,.F.)
B_SPLINE_SURFACE_WITH_KNOTS((2,2),(3,2,3),(0.,0.0614231408718161),(0.0665257254736557,
0.0714285714285714,0.0736543502199191),.UNSPECIFIED.)
GEOMETRIC_REPRESENTATION_ITEM()
RATIONAL_B_SPLINE_SURFACE(((0.996794362316491,0.998279055819231,1.,0.999218731101513,
0.998486152291874),(0.996794362316491,0.998279055819231,1.,0.999218731101513,
0.998486152291874)))
REPRESENTATION_ITEM('')
SURFACE()
);
#3850=(
BOUNDED_SURFACE()
B_SPLINE_SURFACE(1,2,((#159798,#159799,#159800,#159801,#159802),(#159803,
#159804,#159805,#159806,#159807)),.UNSPECIFIED.,.F.,.F.,.F.)
B_SPLINE_SURFACE_WITH_KNOTS((2,2),(3,2,3),(0.817194107660851,1.),(0.642474614281365,
0.642857142857143,0.659901408087503),.UNSPECIFIED.)
GEOMETRIC_REPRESENTATION_ITEM()
RATIONAL_B_SPLINE_SURFACE(((0.999732896029236,0.999865728939372,1.,0.994017305594874,
0.990889788836276),(0.999732896029236,0.999865728939372,1.,0.994017305594874,
0.990889788836276)))
REPRESENTATION_ITEM('')
SURFACE()
);
#3851=(
BOUNDED_SURFACE()
B_SPLINE_SURFACE(1,2,((#159818,#159819,#159820,#159821,#159822),(#159823,
#159824,#159825,#159826,#159827)),.UNSPECIFIED.,.F.,.F.,.F.)
B_SPLINE_SURFACE_WITH_KNOTS((2,2),(3,2,3),(0.817114621578816,1.),(0.0734807488197823,
0.0736543502199038,0.0910144902320513),.UNSPECIFIED.)
GEOMETRIC_REPRESENTATION_ITEM()
RATIONAL_B_SPLINE_SURFACE(((0.998486152291884,0.998486152291884,0.998486152291884,
0.992772345172013,0.990020524139833),(0.998486152291884,0.998486152291884,
0.998486152291884,0.992772345172013,0.990020524139833)))
REPRESENTATION_ITEM('')
SURFACE()
);
#3852=(
BOUNDED_SURFACE()
B_SPLINE_SURFACE(1,2,((#159829,#159830,#159831,#159832,#159833),(#159834,
#159835,#159836,#159837,#159838)),.UNSPECIFIED.,.F.,.F.,.F.)
B_SPLINE_SURFACE_WITH_KNOTS((2,2),(3,2,3),(0.,0.0614498483524345),(0.659832011354082,
0.659901408087476,0.666841081426897),.UNSPECIFIED.)
GEOMETRIC_REPRESENTATION_ITEM()
RATIONAL_B_SPLINE_SURFACE(((0.990889788836286,0.990889788836286,0.990889788836286,
0.989616401900861,0.988816334712145),(0.990889788836286,0.990889788836286,
0.990889788836286,0.989616401900861,0.988816334712145)))
REPRESENTATION_ITEM('')
SURFACE()
);
#3853=(
BOUNDED_SURFACE()
B_SPLINE_SURFACE(1,2,((#159840,#159841,#159842),(#159843,#159844,#159845)),
 .UNSPECIFIED.,.F.,.F.,.F.)
B_SPLINE_SURFACE_WITH_KNOTS((2,2),(3,3),(0.947118453120174,1.),(0.659860018385524,
0.666841081426897),.UNSPECIFIED.)
GEOMETRIC_REPRESENTATION_ITEM()
RATIONAL_B_SPLINE_SURFACE(((0.990904995179383,0.989621173673372,0.988816334712145),
(0.990904995179383,0.989621173673372,0.988816334712145)))
REPRESENTATION_ITEM('')
SURFACE()
);
#3854=(
BOUNDED_SURFACE()
B_SPLINE_SURFACE(1,2,((#159856,#159857,#159858,#159859,#159860),(#159861,
#159862,#159863,#159864,#159865)),.UNSPECIFIED.,.F.,.F.,.F.)
B_SPLINE_SURFACE_WITH_KNOTS((2,2),(3,2,3),(0.947095459621876,1.),(0.066525725473656,
0.0714285714285714,0.0736968668684898),.UNSPECIFIED.)
GEOMETRIC_REPRESENTATION_ITEM()
RATIONAL_B_SPLINE_SURFACE(((0.996794362316491,0.998279055819231,1.,0.999203807365459,
0.998458182734341),(0.996794362316491,0.998279055819231,1.,0.999203807365459,
0.998458182734341)))
REPRESENTATION_ITEM('')
SURFACE()
);
#3855=(
BOUNDED_SURFACE()
B_SPLINE_SURFACE(1,2,((#159873,#159874,#159875,#159876,#159877),(#159878,
#159879,#159880,#159881,#159882)),.UNSPECIFIED.,.F.,.F.,.F.)
B_SPLINE_SURFACE_WITH_KNOTS((2,2),(3,2,3),(0.,0.061423140871819),(0.0665257254736559,
0.0714285714285714,0.0736543502199201),.UNSPECIFIED.)
GEOMETRIC_REPRESENTATION_ITEM()
RATIONAL_B_SPLINE_SURFACE(((0.996794362316491,0.998279055819231,1.,0.999218731101513,
0.998486152291874),(0.996794362316491,0.998279055819231,1.,0.999218731101513,
0.998486152291874)))
REPRESENTATION_ITEM('')
SURFACE()
);
#3856=(
BOUNDED_SURFACE()
B_SPLINE_SURFACE(1,2,((#159884,#159885,#159886,#159887,#159888),(#159889,
#159890,#159891,#159892,#159893)),.UNSPECIFIED.,.F.,.F.,.F.)
B_SPLINE_SURFACE_WITH_KNOTS((2,2),(3,2,3),(0.817194107660853,1.),(0.642474614281365,
0.642857142857143,0.659901408087505),.UNSPECIFIED.)
GEOMETRIC_REPRESENTATION_ITEM()
RATIONAL_B_SPLINE_SURFACE(((0.999732896029237,0.999865728939372,1.,0.994017305594873,
0.990889788836275),(0.999732896029237,0.999865728939372,1.,0.994017305594873,
0.990889788836275)))
REPRESENTATION_ITEM('')
SURFACE()
);
#3857=(
BOUNDED_SURFACE()
B_SPLINE_SURFACE(1,2,((#159904,#159905,#159906,#159907,#159908),(#159909,
#159910,#159911,#159912,#159913)),.UNSPECIFIED.,.F.,.F.,.F.)
B_SPLINE_SURFACE_WITH_KNOTS((2,2),(3,2,3),(0.817114621578814,1.),(0.0734807488197823,
0.0736543502199038,0.0910144902320513),.UNSPECIFIED.)
GEOMETRIC_REPRESENTATION_ITEM()
RATIONAL_B_SPLINE_SURFACE(((0.998486152291885,0.998486152291885,0.998486152291885,
0.992772345172013,0.990020524139833),(0.998486152291885,0.998486152291885,
0.998486152291885,0.992772345172013,0.990020524139833)))
REPRESENTATION_ITEM('')
SURFACE()
);
#3858=(
BOUNDED_SURFACE()
B_SPLINE_SURFACE(1,2,((#159915,#159916,#159917,#159918,#159919),(#159920,
#159921,#159922,#159923,#159924)),.UNSPECIFIED.,.F.,.F.,.F.)
B_SPLINE_SURFACE_WITH_KNOTS((2,2),(3,2,3),(0.,0.0614498483524357),(0.659832011354082,
0.659901408087476,0.666841081426897),.UNSPECIFIED.)
GEOMETRIC_REPRESENTATION_ITEM()
RATIONAL_B_SPLINE_SURFACE(((0.990889788836286,0.990889788836286,0.990889788836286,
0.989616401900861,0.988816334712146),(0.990889788836286,0.990889788836286,
0.990889788836286,0.989616401900861,0.988816334712146)))
REPRESENTATION_ITEM('')
SURFACE()
);
#3859=(
BOUNDED_SURFACE()
B_SPLINE_SURFACE(1,2,((#159926,#159927,#159928),(#159929,#159930,#159931)),
 .UNSPECIFIED.,.F.,.F.,.F.)
B_SPLINE_SURFACE_WITH_KNOTS((2,2),(3,3),(0.947118453120176,1.),(0.659860018385401,
0.666841081426898),.UNSPECIFIED.)
GEOMETRIC_REPRESENTATION_ITEM()
RATIONAL_B_SPLINE_SURFACE(((0.990904995179428,0.989621173673386,0.988816334712145),
(0.990904995179428,0.989621173673386,0.988816334712145)))
REPRESENTATION_ITEM('')
SURFACE()
);
#3860=(
BOUNDED_SURFACE()
B_SPLINE_SURFACE(1,2,((#159942,#159943,#159944,#159945,#159946),(#159947,
#159948,#159949,#159950,#159951)),.UNSPECIFIED.,.F.,.F.,.F.)
B_SPLINE_SURFACE_WITH_KNOTS((2,2),(3,2,3),(0.947095459621873,1.),(0.0665257254736559,
0.0714285714285714,0.0736968668684897),.UNSPECIFIED.)
GEOMETRIC_REPRESENTATION_ITEM()
RATIONAL_B_SPLINE_SURFACE(((0.996794362316491,0.998279055819231,1.,0.999203807365459,
0.998458182734341),(0.996794362316491,0.998279055819231,1.,0.999203807365459,
0.998458182734341)))
REPRESENTATION_ITEM('')
SURFACE()
);
#3861=(
BOUNDED_SURFACE()
B_SPLINE_SURFACE(1,2,((#159959,#159960,#159961,#159962,#159963),(#159964,
#159965,#159966,#159967,#159968)),.UNSPECIFIED.,.F.,.F.,.F.)
B_SPLINE_SURFACE_WITH_KNOTS((2,2),(3,2,3),(0.,0.0614231408718203),(0.0665257254736559,
0.0714285714285714,0.0736543502199224),.UNSPECIFIED.)
GEOMETRIC_REPRESENTATION_ITEM()
RATIONAL_B_SPLINE_SURFACE(((0.996794362316491,0.998279055819231,1.,0.999218731101512,
0.998486152291872),(0.996794362316491,0.998279055819231,1.,0.999218731101512,
0.998486152291872)))
REPRESENTATION_ITEM('')
SURFACE()
);
#3862=(
BOUNDED_SURFACE()
B_SPLINE_SURFACE(1,2,((#159970,#159971,#159972,#159973,#159974),(#159975,
#159976,#159977,#159978,#159979)),.UNSPECIFIED.,.F.,.F.,.F.)
B_SPLINE_SURFACE_WITH_KNOTS((2,2),(3,2,3),(0.817194107660857,1.),(0.642474614281367,
0.642857142857143,0.65990140808751),.UNSPECIFIED.)
GEOMETRIC_REPRESENTATION_ITEM()
RATIONAL_B_SPLINE_SURFACE(((0.999732896029238,0.999865728939373,1.,0.994017305594871,
0.990889788836273),(0.999732896029238,0.999865728939373,1.,0.994017305594871,
0.990889788836273)))
REPRESENTATION_ITEM('')
SURFACE()
);
#3863=(
BOUNDED_SURFACE()
B_SPLINE_SURFACE(1,2,((#159990,#159991,#159992,#159993,#159994),(#159995,
#159996,#159997,#159998,#159999)),.UNSPECIFIED.,.F.,.F.,.F.)
B_SPLINE_SURFACE_WITH_KNOTS((2,2),(3,2,3),(0.817114621578821,1.),(0.073480748819731,
0.073654350219853,0.0910144902320518),.UNSPECIFIED.)
GEOMETRIC_REPRESENTATION_ITEM()
RATIONAL_B_SPLINE_SURFACE(((0.998486152291918,0.998486152291918,0.998486152291918,
0.992772345172021,0.990020524139833),(0.998486152291918,0.998486152291918,
0.998486152291918,0.992772345172021,0.990020524139833)))
REPRESENTATION_ITEM('')
SURFACE()
);
#3864=(
BOUNDED_SURFACE()
B_SPLINE_SURFACE(1,2,((#160001,#160002,#160003,#160004,#160005),(#160006,
#160007,#160008,#160009,#160010)),.UNSPECIFIED.,.F.,.F.,.F.)
B_SPLINE_SURFACE_WITH_KNOTS((2,2),(3,2,3),(0.,0.0614498483528877),(0.65983201135403,
0.659901408087425,0.666841081426897),.UNSPECIFIED.)
GEOMETRIC_REPRESENTATION_ITEM()
RATIONAL_B_SPLINE_SURFACE(((0.990889788836305,0.990889788836305,0.990889788836305,
0.989616401900867,0.988816334712145),(0.990889788836305,0.990889788836305,
0.990889788836305,0.989616401900867,0.988816334712145)))
REPRESENTATION_ITEM('')
SURFACE()
);
#3865=(
BOUNDED_SURFACE()
B_SPLINE_SURFACE(1,2,((#160012,#160013,#160014),(#160015,#160016,#160017)),
 .UNSPECIFIED.,.F.,.F.,.F.)
B_SPLINE_SURFACE_WITH_KNOTS((2,2),(3,3),(0.947118453120172,1.),(0.659860018385599,
0.666841081426897),.UNSPECIFIED.)
GEOMETRIC_REPRESENTATION_ITEM()
RATIONAL_B_SPLINE_SURFACE(((0.990904995179355,0.989621173673364,0.988816334712145),
(0.990904995179355,0.989621173673364,0.988816334712145)))
REPRESENTATION_ITEM('')
SURFACE()
);
#3866=(
BOUNDED_SURFACE()
B_SPLINE_SURFACE(1,2,((#160028,#160029,#160030,#160031,#160032),(#160033,
#160034,#160035,#160036,#160037)),.UNSPECIFIED.,.F.,.F.,.F.)
B_SPLINE_SURFACE_WITH_KNOTS((2,2),(3,2,3),(0.947095459621873,1.),(0.066525725473656,
0.0714285714285714,0.073696866868496),.UNSPECIFIED.)
GEOMETRIC_REPRESENTATION_ITEM()
RATIONAL_B_SPLINE_SURFACE(((0.996794362316491,0.998279055819231,1.,0.999203807365457,
0.998458182734337),(0.996794362316491,0.998279055819231,1.,0.999203807365457,
0.998458182734337)))
REPRESENTATION_ITEM('')
SURFACE()
);
#3867=(
BOUNDED_SURFACE()
B_SPLINE_SURFACE(1,2,((#160045,#160046,#160047,#160048,#160049),(#160050,
#160051,#160052,#160053,#160054)),.UNSPECIFIED.,.F.,.F.,.F.)
B_SPLINE_SURFACE_WITH_KNOTS((2,2),(3,2,3),(0.,0.0614231408718192),(0.0665257254736563,
0.0714285714285714,0.073654350219921),.UNSPECIFIED.)
GEOMETRIC_REPRESENTATION_ITEM()
RATIONAL_B_SPLINE_SURFACE(((0.996794362316491,0.998279055819231,1.,0.999218731101512,
0.998486152291873),(0.996794362316491,0.998279055819231,1.,0.999218731101512,
0.998486152291873)))
REPRESENTATION_ITEM('')
SURFACE()
);
#3868=(
BOUNDED_SURFACE()
B_SPLINE_SURFACE(1,2,((#160056,#160057,#160058,#160059,#160060),(#160061,
#160062,#160063,#160064,#160065)),.UNSPECIFIED.,.F.,.F.,.F.)
B_SPLINE_SURFACE_WITH_KNOTS((2,2),(3,2,3),(0.817194107660852,1.),(0.642474614281367,
0.642857142857143,0.659901408087507),.UNSPECIFIED.)
GEOMETRIC_REPRESENTATION_ITEM()
RATIONAL_B_SPLINE_SURFACE(((0.999732896029238,0.999865728939373,1.,0.994017305594872,
0.990889788836274),(0.999732896029238,0.999865728939373,1.,0.994017305594872,
0.990889788836274)))
REPRESENTATION_ITEM('')
SURFACE()
);
#3869=(
BOUNDED_SURFACE()
B_SPLINE_SURFACE(1,2,((#160076,#160077,#160078,#160079,#160080),(#160081,
#160082,#160083,#160084,#160085)),.UNSPECIFIED.,.F.,.F.,.F.)
B_SPLINE_SURFACE_WITH_KNOTS((2,2),(3,2,3),(0.817114621578816,1.),(0.0734807488197815,
0.073654350219903,0.0910144902320514),.UNSPECIFIED.)
GEOMETRIC_REPRESENTATION_ITEM()
RATIONAL_B_SPLINE_SURFACE(((0.998486152291885,0.998486152291885,0.998486152291885,
0.992772345172013,0.990020524139833),(0.998486152291885,0.998486152291885,
0.998486152291885,0.992772345172013,0.990020524139833)))
REPRESENTATION_ITEM('')
SURFACE()
);
#3870=(
BOUNDED_SURFACE()
B_SPLINE_SURFACE(1,2,((#160087,#160088,#160089,#160090,#160091),(#160092,
#160093,#160094,#160095,#160096)),.UNSPECIFIED.,.F.,.F.,.F.)
B_SPLINE_SURFACE_WITH_KNOTS((2,2),(3,2,3),(0.,0.0614498483524432),(0.659832011354081,
0.659901408087475,0.666841081426896),.UNSPECIFIED.)
GEOMETRIC_REPRESENTATION_ITEM()
RATIONAL_B_SPLINE_SURFACE(((0.990889788836286,0.990889788836286,0.990889788836286,
0.989616401900861,0.988816334712146),(0.990889788836286,0.990889788836286,
0.990889788836286,0.989616401900861,0.988816334712146)))
REPRESENTATION_ITEM('')
SURFACE()
);
#3871=(
BOUNDED_SURFACE()
B_SPLINE_SURFACE(1,2,((#160098,#160099,#160100),(#160101,#160102,#160103)),
 .UNSPECIFIED.,.F.,.F.,.F.)
B_SPLINE_SURFACE_WITH_KNOTS((2,2),(3,3),(0.94711845312018,1.),(0.65986001838565,
0.666841081426896),.UNSPECIFIED.)
GEOMETRIC_REPRESENTATION_ITEM()
RATIONAL_B_SPLINE_SURFACE(((0.990904995179337,0.989621173673358,0.988816334712145),
(0.990904995179337,0.989621173673358,0.988816334712145)))
REPRESENTATION_ITEM('')
SURFACE()
);
#3872=(
BOUNDED_SURFACE()
B_SPLINE_SURFACE(1,2,((#160114,#160115,#160116,#160117,#160118),(#160119,
#160120,#160121,#160122,#160123)),.UNSPECIFIED.,.F.,.F.,.F.)
B_SPLINE_SURFACE_WITH_KNOTS((2,2),(3,2,3),(0.947095459621876,1.),(0.0665257254736558,
0.0714285714285714,0.0736968668684959),.UNSPECIFIED.)
GEOMETRIC_REPRESENTATION_ITEM()
RATIONAL_B_SPLINE_SURFACE(((0.996794362316491,0.998279055819231,1.,0.999203807365457,
0.998458182734337),(0.996794362316491,0.998279055819231,1.,0.999203807365457,
0.998458182734337)))
REPRESENTATION_ITEM('')
SURFACE()
);
#3873=(
BOUNDED_SURFACE()
B_SPLINE_SURFACE(1,2,((#160131,#160132,#160133,#160134,#160135),(#160136,
#160137,#160138,#160139,#160140)),.UNSPECIFIED.,.F.,.F.,.F.)
B_SPLINE_SURFACE_WITH_KNOTS((2,2),(3,2,3),(0.,0.0614231408718359),(0.0665257254736558,
0.0714285714285714,0.0736543502199115),.UNSPECIFIED.)
GEOMETRIC_REPRESENTATION_ITEM()
RATIONAL_B_SPLINE_SURFACE(((0.996794362316491,0.998279055819231,1.,0.999218731101516,
0.99848615229188),(0.996794362316491,0.998279055819231,1.,0.999218731101516,
0.99848615229188)))
REPRESENTATION_ITEM('')
SURFACE()
);
#3874=(
BOUNDED_SURFACE()
B_SPLINE_SURFACE(1,2,((#160142,#160143,#160144,#160145,#160146),(#160147,
#160148,#160149,#160150,#160151)),.UNSPECIFIED.,.F.,.F.,.F.)
B_SPLINE_SURFACE_WITH_KNOTS((2,2),(3,2,3),(0.817194107660858,1.),(0.642474614281367,
0.642857142857143,0.659901408087488),.UNSPECIFIED.)
GEOMETRIC_REPRESENTATION_ITEM()
RATIONAL_B_SPLINE_SURFACE(((0.999732896029238,0.999865728939373,1.,0.994017305594879,
0.990889788836282),(0.999732896029238,0.999865728939373,1.,0.994017305594879,
0.990889788836282)))
REPRESENTATION_ITEM('')
SURFACE()
);
#3875=(
BOUNDED_SURFACE()
B_SPLINE_SURFACE(1,2,((#160162,#160163,#160164,#160165,#160166),(#160167,
#160168,#160169,#160170,#160171)),.UNSPECIFIED.,.F.,.F.,.F.)
B_SPLINE_SURFACE_WITH_KNOTS((2,2),(3,2,3),(0.817114621578819,1.),(0.0734807488197832,
0.0736543502199047,0.0910144902320511),.UNSPECIFIED.)
GEOMETRIC_REPRESENTATION_ITEM()
RATIONAL_B_SPLINE_SURFACE(((0.998486152291884,0.998486152291884,0.998486152291884,
0.992772345172013,0.990020524139834),(0.998486152291884,0.998486152291884,
0.998486152291884,0.992772345172013,0.990020524139834)))
REPRESENTATION_ITEM('')
SURFACE()
);
#3876=(
BOUNDED_SURFACE()
B_SPLINE_SURFACE(1,2,((#160173,#160174,#160175,#160176,#160177),(#160178,
#160179,#160180,#160181,#160182)),.UNSPECIFIED.,.F.,.F.,.F.)
B_SPLINE_SURFACE_WITH_KNOTS((2,2),(3,2,3),(0.,0.0614498483524474),(0.659832011354081,
0.659901408087475,0.666841081426896),.UNSPECIFIED.)
GEOMETRIC_REPRESENTATION_ITEM()
RATIONAL_B_SPLINE_SURFACE(((0.990889788836286,0.990889788836286,0.990889788836286,
0.989616401900861,0.988816334712146),(0.990889788836286,0.990889788836286,
0.990889788836286,0.989616401900861,0.988816334712146)))
REPRESENTATION_ITEM('')
SURFACE()
);
#3877=(
BOUNDED_SURFACE()
B_SPLINE_SURFACE(1,2,((#160184,#160185,#160186),(#160187,#160188,#160189)),
 .UNSPECIFIED.,.F.,.F.,.F.)
B_SPLINE_SURFACE_WITH_KNOTS((2,2),(3,3),(0.947118453120166,1.),(0.659860018385649,
0.666841081426897),.UNSPECIFIED.)
GEOMETRIC_REPRESENTATION_ITEM()
RATIONAL_B_SPLINE_SURFACE(((0.990904995179337,0.989621173673358,0.988816334712146),
(0.990904995179337,0.989621173673358,0.988816334712146)))
REPRESENTATION_ITEM('')
SURFACE()
);
#3878=(
BOUNDED_SURFACE()
B_SPLINE_SURFACE(1,2,((#160200,#160201,#160202,#160203,#160204),(#160205,
#160206,#160207,#160208,#160209)),.UNSPECIFIED.,.F.,.F.,.F.)
B_SPLINE_SURFACE_WITH_KNOTS((2,2),(3,2,3),(0.947095459621867,1.),(0.066525725473656,
0.0714285714285714,0.073696866868497),.UNSPECIFIED.)
GEOMETRIC_REPRESENTATION_ITEM()
RATIONAL_B_SPLINE_SURFACE(((0.996794362316491,0.998279055819231,1.,0.999203807365457,
0.998458182734336),(0.996794362316491,0.998279055819231,1.,0.999203807365457,
0.998458182734336)))
REPRESENTATION_ITEM('')
SURFACE()
);
#3879=(
BOUNDED_SURFACE()
B_SPLINE_SURFACE(1,2,((#160216,#160217,#160218,#160219,#160220),(#160221,
#160222,#160223,#160224,#160225)),.UNSPECIFIED.,.F.,.F.,.F.)
B_SPLINE_SURFACE_WITH_KNOTS((2,2),(3,2,3),(0.,0.0614231408718302),(0.066525725473656,
0.0714285714285714,0.0736543502199111),.UNSPECIFIED.)
GEOMETRIC_REPRESENTATION_ITEM()
RATIONAL_B_SPLINE_SURFACE(((0.996794362316491,0.998279055819231,1.,0.999218731101516,
0.99848615229188),(0.996794362316491,0.998279055819231,1.,0.999218731101516,
0.99848615229188)))
REPRESENTATION_ITEM('')
SURFACE()
);
#3880=(
BOUNDED_SURFACE()
B_SPLINE_SURFACE(1,2,((#160227,#160228,#160229,#160230,#160231),(#160232,
#160233,#160234,#160235,#160236)),.UNSPECIFIED.,.F.,.F.,.F.)
B_SPLINE_SURFACE_WITH_KNOTS((2,2),(3,2,3),(0.817194107660843,1.),(0.642474614281367,
0.642857142857143,0.659901408087482),.UNSPECIFIED.)
GEOMETRIC_REPRESENTATION_ITEM()
RATIONAL_B_SPLINE_SURFACE(((0.999732896029238,0.999865728939373,1.,0.994017305594881,
0.990889788836284),(0.999732896029238,0.999865728939373,1.,0.994017305594881,
0.990889788836284)))
REPRESENTATION_ITEM('')
SURFACE()
);
#3881=(
BOUNDED_SURFACE()
B_SPLINE_SURFACE(1,2,((#160247,#160248,#160249,#160250,#160251),(#160252,
#160253,#160254,#160255,#160256)),.UNSPECIFIED.,.F.,.F.,.F.)
B_SPLINE_SURFACE_WITH_KNOTS((2,2),(3,2,3),(0.817114621578812,1.),(0.073480748819775,
0.0736543502198966,0.0910144902320529),.UNSPECIFIED.)
GEOMETRIC_REPRESENTATION_ITEM()
RATIONAL_B_SPLINE_SURFACE(((0.998486152291889,0.998486152291889,0.998486152291889,
0.992772345172014,0.990020524139833),(0.998486152291889,0.998486152291889,
0.998486152291889,0.992772345172014,0.990020524139833)))
REPRESENTATION_ITEM('')
SURFACE()
);
#3882=(
BOUNDED_SURFACE()
B_SPLINE_SURFACE(1,2,((#160258,#160259,#160260,#160261,#160262),(#160263,
#160264,#160265,#160266,#160267)),.UNSPECIFIED.,.F.,.F.,.F.)
B_SPLINE_SURFACE_WITH_KNOTS((2,2),(3,2,3),(0.,0.0614498483525183),(0.659832011354072,
0.659901408087466,0.666841081426896),.UNSPECIFIED.)
GEOMETRIC_REPRESENTATION_ITEM()
RATIONAL_B_SPLINE_SURFACE(((0.99088978883629,0.99088978883629,0.99088978883629,
0.989616401900862,0.988816334712146),(0.99088978883629,0.99088978883629,
0.99088978883629,0.989616401900862,0.988816334712146)))
REPRESENTATION_ITEM('')
SURFACE()
);
#3883=(
BOUNDED_SURFACE()
B_SPLINE_SURFACE(1,2,((#160269,#160270,#160271),(#160272,#160273,#160274)),
 .UNSPECIFIED.,.F.,.F.,.F.)
B_SPLINE_SURFACE_WITH_KNOTS((2,2),(3,3),(0.947118453120172,1.),(0.659860018385517,
0.666841081426897),.UNSPECIFIED.)
GEOMETRIC_REPRESENTATION_ITEM()
RATIONAL_B_SPLINE_SURFACE(((0.990904995179385,0.989621173673373,0.988816334712145),
(0.990904995179385,0.989621173673373,0.988816334712145)))
REPRESENTATION_ITEM('')
SURFACE()
);
#3884=(
BOUNDED_SURFACE()
B_SPLINE_SURFACE(1,2,((#160285,#160286,#160287,#160288,#160289),(#160290,
#160291,#160292,#160293,#160294)),.UNSPECIFIED.,.F.,.F.,.F.)
B_SPLINE_SURFACE_WITH_KNOTS((2,2),(3,2,3),(0.94709545962187,1.),(0.0665257254736565,
0.0714285714285714,0.0736968668684826),.UNSPECIFIED.)
GEOMETRIC_REPRESENTATION_ITEM()
RATIONAL_B_SPLINE_SURFACE(((0.996794362316492,0.998279055819231,1.,0.999203807365462,
0.998458182734345),(0.996794362316492,0.998279055819231,1.,0.999203807365462,
0.998458182734345)))
REPRESENTATION_ITEM('')
SURFACE()
);
#3885=(
BOUNDED_SURFACE()
B_SPLINE_SURFACE(1,2,((#160302,#160303,#160304,#160305,#160306),(#160307,
#160308,#160309,#160310,#160311)),.UNSPECIFIED.,.F.,.F.,.F.)
B_SPLINE_SURFACE_WITH_KNOTS((2,2),(3,2,3),(0.,0.0614231408718237),(0.0665257254736564,
0.0714285714285714,0.0736543502199109),.UNSPECIFIED.)
GEOMETRIC_REPRESENTATION_ITEM()
RATIONAL_B_SPLINE_SURFACE(((0.996794362316491,0.998279055819231,1.,0.999218731101516,
0.99848615229188),(0.996794362316491,0.998279055819231,1.,0.999218731101516,
0.99848615229188)))
REPRESENTATION_ITEM('')
SURFACE()
);
#3886=(
BOUNDED_SURFACE()
B_SPLINE_SURFACE(1,2,((#160313,#160314,#160315,#160316,#160317),(#160318,
#160319,#160320,#160321,#160322)),.UNSPECIFIED.,.F.,.F.,.F.)
B_SPLINE_SURFACE_WITH_KNOTS((2,2),(3,2,3),(0.817194107660847,1.),(0.642474614281365,
0.642857142857143,0.659901408087502),.UNSPECIFIED.)
GEOMETRIC_REPRESENTATION_ITEM()
RATIONAL_B_SPLINE_SURFACE(((0.999732896029236,0.999865728939372,1.,0.994017305594874,
0.990889788836277),(0.999732896029236,0.999865728939372,1.,0.994017305594874,
0.990889788836277)))
REPRESENTATION_ITEM('')
SURFACE()
);
#3887=(
BOUNDED_SURFACE()
B_SPLINE_SURFACE(1,2,((#160333,#160334,#160335,#160336,#160337),(#160338,
#160339,#160340,#160341,#160342)),.UNSPECIFIED.,.F.,.F.,.F.)
B_SPLINE_SURFACE_WITH_KNOTS((2,2),(3,2,3),(0.81711462157881,1.),(0.073480748819775,
0.0736543502198966,0.0910144902320526),.UNSPECIFIED.)
GEOMETRIC_REPRESENTATION_ITEM()
RATIONAL_B_SPLINE_SURFACE(((0.998486152291889,0.998486152291889,0.998486152291889,
0.992772345172013,0.990020524139833),(0.998486152291889,0.998486152291889,
0.998486152291889,0.992772345172013,0.990020524139833)))
REPRESENTATION_ITEM('')
SURFACE()
);
#3888=(
BOUNDED_SURFACE()
B_SPLINE_SURFACE(1,2,((#160344,#160345,#160346,#160347,#160348),(#160349,
#160350,#160351,#160352,#160353)),.UNSPECIFIED.,.F.,.F.,.F.)
B_SPLINE_SURFACE_WITH_KNOTS((2,2),(3,2,3),(0.,0.0614498483525201),(0.659832011354072,
0.659901408087466,0.666841081426897),.UNSPECIFIED.)
GEOMETRIC_REPRESENTATION_ITEM()
RATIONAL_B_SPLINE_SURFACE(((0.99088978883629,0.99088978883629,0.99088978883629,
0.989616401900862,0.988816334712146),(0.990889788836289,0.990889788836289,
0.990889788836289,0.989616401900862,0.988816334712146)))
REPRESENTATION_ITEM('')
SURFACE()
);
#3889=(
BOUNDED_SURFACE()
B_SPLINE_SURFACE(1,2,((#160355,#160356,#160357),(#160358,#160359,#160360)),
 .UNSPECIFIED.,.F.,.F.,.F.)
B_SPLINE_SURFACE_WITH_KNOTS((2,2),(3,3),(0.94711845312017,1.),(0.659860018385641,
0.666841081426897),.UNSPECIFIED.)
GEOMETRIC_REPRESENTATION_ITEM()
RATIONAL_B_SPLINE_SURFACE(((0.99090499517934,0.989621173673359,0.988816334712145),
(0.99090499517934,0.989621173673359,0.988816334712145)))
REPRESENTATION_ITEM('')
SURFACE()
);
#3890=(
BOUNDED_SURFACE()
B_SPLINE_SURFACE(1,2,((#160371,#160372,#160373,#160374,#160375),(#160376,
#160377,#160378,#160379,#160380)),.UNSPECIFIED.,.F.,.F.,.F.)
B_SPLINE_SURFACE_WITH_KNOTS((2,2),(3,2,3),(0.947095459621873,1.),(0.0665257254736562,
0.0714285714285714,0.0736968668684971),.UNSPECIFIED.)
GEOMETRIC_REPRESENTATION_ITEM()
RATIONAL_B_SPLINE_SURFACE(((0.996794362316491,0.998279055819231,1.,0.999203807365457,
0.998458182734336),(0.996794362316491,0.998279055819231,1.,0.999203807365457,
0.998458182734336)))
REPRESENTATION_ITEM('')
SURFACE()
);
#3891=(
BOUNDED_SURFACE()
B_SPLINE_SURFACE(1,2,((#160388,#160389,#160390,#160391,#160392),(#160393,
#160394,#160395,#160396,#160397)),.UNSPECIFIED.,.F.,.F.,.F.)
B_SPLINE_SURFACE_WITH_KNOTS((2,2),(3,2,3),(0.,0.0614231408718238),(0.0665257254736562,
0.0714285714285714,0.073654350219911),.UNSPECIFIED.)
GEOMETRIC_REPRESENTATION_ITEM()
RATIONAL_B_SPLINE_SURFACE(((0.996794362316491,0.998279055819231,1.,0.999218731101516,
0.99848615229188),(0.996794362316491,0.998279055819231,1.,0.999218731101516,
0.99848615229188)))
REPRESENTATION_ITEM('')
SURFACE()
);
#3892=(
BOUNDED_SURFACE()
B_SPLINE_SURFACE(1,2,((#160399,#160400,#160401,#160402,#160403),(#160404,
#160405,#160406,#160407,#160408)),.UNSPECIFIED.,.F.,.F.,.F.)
B_SPLINE_SURFACE_WITH_KNOTS((2,2),(3,2,3),(0.817194107660843,1.),(0.642474614281365,
0.642857142857143,0.659901408087508),.UNSPECIFIED.)
GEOMETRIC_REPRESENTATION_ITEM()
RATIONAL_B_SPLINE_SURFACE(((0.999732896029236,0.999865728939372,1.,0.994017305594872,
0.990889788836274),(0.999732896029236,0.999865728939372,1.,0.994017305594872,
0.990889788836274)))
REPRESENTATION_ITEM('')
SURFACE()
);
#3893=(
BOUNDED_SURFACE()
B_SPLINE_SURFACE(1,2,((#160419,#160420,#160421,#160422,#160423),(#160424,
#160425,#160426,#160427,#160428)),.UNSPECIFIED.,.F.,.F.,.F.)
B_SPLINE_SURFACE_WITH_KNOTS((2,2),(3,2,3),(0.817114621578812,1.),(0.0734807488197753,
0.0736543502198968,0.0910144902320527),.UNSPECIFIED.)
GEOMETRIC_REPRESENTATION_ITEM()
RATIONAL_B_SPLINE_SURFACE(((0.998486152291889,0.998486152291889,0.998486152291889,
0.992772345172013,0.990020524139833),(0.998486152291889,0.998486152291889,
0.998486152291889,0.992772345172013,0.990020524139833)))
REPRESENTATION_ITEM('')
SURFACE()
);
#3894=(
BOUNDED_SURFACE()
B_SPLINE_SURFACE(1,2,((#160430,#160431,#160432,#160433,#160434),(#160435,
#160436,#160437,#160438,#160439)),.UNSPECIFIED.,.F.,.F.,.F.)
B_SPLINE_SURFACE_WITH_KNOTS((2,2),(3,2,3),(0.,0.0614498483525222),(0.659832011354072,
0.659901408087466,0.666841081426897),.UNSPECIFIED.)
GEOMETRIC_REPRESENTATION_ITEM()
RATIONAL_B_SPLINE_SURFACE(((0.99088978883629,0.99088978883629,0.99088978883629,
0.989616401900862,0.988816334712145),(0.99088978883629,0.99088978883629,
0.99088978883629,0.989616401900862,0.988816334712145)))
REPRESENTATION_ITEM('')
SURFACE()
);
#3895=(
BOUNDED_SURFACE()
B_SPLINE_SURFACE(1,2,((#160441,#160442,#160443),(#160444,#160445,#160446)),
 .UNSPECIFIED.,.F.,.F.,.F.)
B_SPLINE_SURFACE_WITH_KNOTS((2,2),(3,3),(0.94711845312017,1.),(0.659860018385515,
0.666841081426897),.UNSPECIFIED.)
GEOMETRIC_REPRESENTATION_ITEM()
RATIONAL_B_SPLINE_SURFACE(((0.990904995179386,0.989621173673373,0.988816334712145),
(0.990904995179386,0.989621173673373,0.988816334712145)))
REPRESENTATION_ITEM('')
SURFACE()
);
#3896=(
BOUNDED_SURFACE()
B_SPLINE_SURFACE(1,2,((#160457,#160458,#160459,#160460,#160461),(#160462,
#160463,#160464,#160465,#160466)),.UNSPECIFIED.,.F.,.F.,.F.)
B_SPLINE_SURFACE_WITH_KNOTS((2,2),(3,2,3),(0.947095459621873,1.),(0.0665257254736565,
0.0714285714285714,0.0736968668684827),.UNSPECIFIED.)
GEOMETRIC_REPRESENTATION_ITEM()
RATIONAL_B_SPLINE_SURFACE(((0.996794362316492,0.998279055819231,1.,0.999203807365462,
0.998458182734345),(0.996794362316492,0.998279055819231,1.,0.999203807365462,
0.998458182734345)))
REPRESENTATION_ITEM('')
SURFACE()
);
#3897=(
BOUNDED_SURFACE()
B_SPLINE_SURFACE(1,2,((#160474,#160475,#160476,#160477,#160478),(#160479,
#160480,#160481,#160482,#160483)),.UNSPECIFIED.,.F.,.F.,.F.)
B_SPLINE_SURFACE_WITH_KNOTS((2,2),(3,2,3),(0.,0.0614231408718247),(0.0665257254736564,
0.0714285714285714,0.073654350219911),.UNSPECIFIED.)
GEOMETRIC_REPRESENTATION_ITEM()
RATIONAL_B_SPLINE_SURFACE(((0.996794362316491,0.998279055819231,1.,0.999218731101516,
0.99848615229188),(0.996794362316491,0.998279055819231,1.,0.999218731101516,
0.99848615229188)))
REPRESENTATION_ITEM('')
SURFACE()
);
#3898=(
BOUNDED_SURFACE()
B_SPLINE_SURFACE(1,2,((#160485,#160486,#160487,#160488,#160489),(#160490,
#160491,#160492,#160493,#160494)),.UNSPECIFIED.,.F.,.F.,.F.)
B_SPLINE_SURFACE_WITH_KNOTS((2,2),(3,2,3),(0.817194107660843,1.),(0.642474614281365,
0.642857142857143,0.659901408087509),.UNSPECIFIED.)
GEOMETRIC_REPRESENTATION_ITEM()
RATIONAL_B_SPLINE_SURFACE(((0.999732896029236,0.999865728939372,1.,0.994017305594872,
0.990889788836274),(0.999732896029236,0.999865728939372,1.,0.994017305594872,
0.990889788836274)))
REPRESENTATION_ITEM('')
SURFACE()
);
#3899=(
BOUNDED_SURFACE()
B_SPLINE_SURFACE(1,2,((#160505,#160506,#160507,#160508,#160509),(#160510,
#160511,#160512,#160513,#160514)),.UNSPECIFIED.,.F.,.F.,.F.)
B_SPLINE_SURFACE_WITH_KNOTS((2,2),(3,2,3),(0.817114621578811,1.),(0.0734807488197753,
0.0736543502198968,0.0910144902320527),.UNSPECIFIED.)
GEOMETRIC_REPRESENTATION_ITEM()
RATIONAL_B_SPLINE_SURFACE(((0.998486152291889,0.998486152291889,0.998486152291889,
0.992772345172013,0.990020524139833),(0.998486152291889,0.998486152291889,
0.998486152291889,0.992772345172013,0.990020524139833)))
REPRESENTATION_ITEM('')
SURFACE()
);
#3900=(
BOUNDED_SURFACE()
B_SPLINE_SURFACE(1,2,((#160516,#160517,#160518,#160519,#160520),(#160521,
#160522,#160523,#160524,#160525)),.UNSPECIFIED.,.F.,.F.,.F.)
B_SPLINE_SURFACE_WITH_KNOTS((2,2),(3,2,3),(0.,0.061449848352517),(0.659832011354072,
0.659901408087466,0.666841081426897),.UNSPECIFIED.)
GEOMETRIC_REPRESENTATION_ITEM()
RATIONAL_B_SPLINE_SURFACE(((0.990889788836289,0.990889788836289,0.990889788836289,
0.989616401900862,0.988816334712145),(0.99088978883629,0.99088978883629,
0.99088978883629,0.989616401900862,0.988816334712146)))
REPRESENTATION_ITEM('')
SURFACE()
);
#3901=(
BOUNDED_SURFACE()
B_SPLINE_SURFACE(1,2,((#160527,#160528,#160529),(#160530,#160531,#160532)),
 .UNSPECIFIED.,.F.,.F.,.F.)
B_SPLINE_SURFACE_WITH_KNOTS((2,2),(3,3),(0.947118453120168,1.),(0.659860018385514,
0.666841081426898),.UNSPECIFIED.)
GEOMETRIC_REPRESENTATION_ITEM()
RATIONAL_B_SPLINE_SURFACE(((0.990904995179386,0.989621173673373,0.988816334712145),
(0.990904995179386,0.989621173673373,0.988816334712145)))
REPRESENTATION_ITEM('')
SURFACE()
);
#3902=(
BOUNDED_SURFACE()
B_SPLINE_SURFACE(1,2,((#160543,#160544,#160545,#160546,#160547),(#160548,
#160549,#160550,#160551,#160552)),.UNSPECIFIED.,.F.,.F.,.F.)
B_SPLINE_SURFACE_WITH_KNOTS((2,2),(3,2,3),(0.947095459621871,1.),(0.0665257254736566,
0.0714285714285714,0.0736968668684827),.UNSPECIFIED.)
GEOMETRIC_REPRESENTATION_ITEM()
RATIONAL_B_SPLINE_SURFACE(((0.996794362316492,0.998279055819231,1.,0.999203807365462,
0.998458182734345),(0.996794362316492,0.998279055819231,1.,0.999203807365462,
0.998458182734345)))
REPRESENTATION_ITEM('')
SURFACE()
);
#3903=(
BOUNDED_SURFACE()
B_SPLINE_SURFACE(1,2,((#160560,#160561,#160562,#160563,#160564),(#160565,
#160566,#160567,#160568,#160569)),.UNSPECIFIED.,.F.,.F.,.F.)
B_SPLINE_SURFACE_WITH_KNOTS((2,2),(3,2,3),(0.,0.0614231408718261),(0.0665257254736565,
0.0714285714285714,0.073654350219911),.UNSPECIFIED.)
GEOMETRIC_REPRESENTATION_ITEM()
RATIONAL_B_SPLINE_SURFACE(((0.996794362316492,0.998279055819231,1.,0.999218731101516,
0.99848615229188),(0.996794362316492,0.998279055819231,1.,0.999218731101516,
0.99848615229188)))
REPRESENTATION_ITEM('')
SURFACE()
);
#3904=(
BOUNDED_SURFACE()
B_SPLINE_SURFACE(1,2,((#160571,#160572,#160573,#160574,#160575),(#160576,
#160577,#160578,#160579,#160580)),.UNSPECIFIED.,.F.,.F.,.F.)
B_SPLINE_SURFACE_WITH_KNOTS((2,2),(3,2,3),(0.817194107660846,1.),(0.642474614281365,
0.642857142857143,0.659901408087504),.UNSPECIFIED.)
GEOMETRIC_REPRESENTATION_ITEM()
RATIONAL_B_SPLINE_SURFACE(((0.999732896029236,0.999865728939372,1.,0.994017305594873,
0.990889788836276),(0.999732896029236,0.999865728939372,1.,0.994017305594873,
0.990889788836276)))
REPRESENTATION_ITEM('')
SURFACE()
);
#3905=(
BOUNDED_SURFACE()
B_SPLINE_SURFACE(1,2,((#160591,#160592,#160593,#160594,#160595),(#160596,
#160597,#160598,#160599,#160600)),.UNSPECIFIED.,.F.,.F.,.F.)
B_SPLINE_SURFACE_WITH_KNOTS((2,2),(3,2,3),(0.817114621578813,1.),(0.0734807488197834,
0.0736543502199049,0.0910144902320528),.UNSPECIFIED.)
GEOMETRIC_REPRESENTATION_ITEM()
RATIONAL_B_SPLINE_SURFACE(((0.998486152291884,0.998486152291884,0.998486152291884,
0.992772345172012,0.990020524139833),(0.998486152291884,0.998486152291884,
0.998486152291884,0.992772345172012,0.990020524139833)))
REPRESENTATION_ITEM('')
SURFACE()
);
#3906=(
BOUNDED_SURFACE()
B_SPLINE_SURFACE(1,2,((#160601,#160602,#160603),(#160604,#160605,#160606)),
 .UNSPECIFIED.,.F.,.F.,.F.)
B_SPLINE_SURFACE_WITH_KNOTS((2,2),(3,3),(0.710192959008443,1.),(0.607982157956011,
0.625273655815328),.UNSPECIFIED.)
GEOMETRIC_REPRESENTATION_ITEM()
RATIONAL_B_SPLINE_SURFACE(((0.987470879370255,0.98761351460672,0.990694758798812),
(0.987470879370255,0.98761351460672,0.990694758798812)))
REPRESENTATION_ITEM('')
SURFACE()
);
#3907=(
BOUNDED_SURFACE()
B_SPLINE_SURFACE(1,2,((#160615,#160616,#160617,#160618,#160619),(#160620,
#160621,#160622,#160623,#160624)),.UNSPECIFIED.,.F.,.F.,.F.)
B_SPLINE_SURFACE_WITH_KNOTS((2,2),(3,2,3),(0.709719018660168,1.),(0.107879027750092,
0.125170525609408,0.125770422804668),.UNSPECIFIED.)
GEOMETRIC_REPRESENTATION_ITEM()
RATIONAL_B_SPLINE_SURFACE(((0.987469282487682,0.987594391229382,0.990658108926709,
0.990658108926709,0.990658108926709),(0.987469282487682,0.987594391229382,
0.990658108926709,0.990658108926709,0.990658108926709)))
REPRESENTATION_ITEM('')
SURFACE()
);
#3908=(
BOUNDED_SURFACE()
B_SPLINE_SURFACE(1,2,((#160626,#160627,#160628),(#160629,#160630,#160631)),
 .UNSPECIFIED.,.F.,.F.,.F.)
B_SPLINE_SURFACE_WITH_KNOTS((2,2),(3,3),(0.710192959008439,1.),(0.607982157956011,
0.625273655815328),.UNSPECIFIED.)
GEOMETRIC_REPRESENTATION_ITEM()
RATIONAL_B_SPLINE_SURFACE(((0.987470879370255,0.98761351460672,0.990694758798812),
(0.987470879370255,0.98761351460672,0.990694758798812)))
REPRESENTATION_ITEM('')
SURFACE()
);
#3909=(
BOUNDED_SURFACE()
B_SPLINE_SURFACE(1,2,((#160640,#160641,#160642,#160643,#160644),(#160645,
#160646,#160647,#160648,#160649)),.UNSPECIFIED.,.F.,.F.,.F.)
B_SPLINE_SURFACE_WITH_KNOTS((2,2),(3,2,3),(0.709719018657229,1.),(0.107879027750092,
0.125170525609408,0.125770422807604),.UNSPECIFIED.)
GEOMETRIC_REPRESENTATION_ITEM()
RATIONAL_B_SPLINE_SURFACE(((0.987469282487682,0.987594391229382,0.990658108926709,
0.990658108926709,0.990658108926709),(0.987469282487682,0.987594391229382,
0.990658108926709,0.990658108926709,0.990658108926709)))
REPRESENTATION_ITEM('')
SURFACE()
);
#3910=(
BOUNDED_SURFACE()
B_SPLINE_SURFACE(1,2,((#160651,#160652,#160653),(#160654,#160655,#160656)),
 .UNSPECIFIED.,.F.,.F.,.F.)
B_SPLINE_SURFACE_WITH_KNOTS((2,2),(3,3),(0.710192959008444,1.),(0.607982157956011,
0.625273655815328),.UNSPECIFIED.)
GEOMETRIC_REPRESENTATION_ITEM()
RATIONAL_B_SPLINE_SURFACE(((0.987470879370255,0.98761351460672,0.990694758798812),
(0.987470879370255,0.98761351460672,0.990694758798812)))
REPRESENTATION_ITEM('')
SURFACE()
);
#3911=(
BOUNDED_SURFACE()
B_SPLINE_SURFACE(1,2,((#160665,#160666,#160667,#160668,#160669),(#160670,
#160671,#160672,#160673,#160674)),.UNSPECIFIED.,.F.,.F.,.F.)
B_SPLINE_SURFACE_WITH_KNOTS((2,2),(3,2,3),(0.709719018653174,1.),(0.107879027750092,
0.125170525609408,0.12577042281166),.UNSPECIFIED.)
GEOMETRIC_REPRESENTATION_ITEM()
RATIONAL_B_SPLINE_SURFACE(((0.987469282487682,0.987594391229382,0.990658108926709,
0.990658108926709,0.990658108926709),(0.987469282487682,0.987594391229382,
0.990658108926709,0.990658108926709,0.990658108926709)))
REPRESENTATION_ITEM('')
SURFACE()
);
#3912=(
BOUNDED_SURFACE()
B_SPLINE_SURFACE(1,2,((#160676,#160677,#160678),(#160679,#160680,#160681)),
 .UNSPECIFIED.,.F.,.F.,.F.)
B_SPLINE_SURFACE_WITH_KNOTS((2,2),(3,3),(0.710192959008439,1.),(0.607982157956011,
0.625273655815328),.UNSPECIFIED.)
GEOMETRIC_REPRESENTATION_ITEM()
RATIONAL_B_SPLINE_SURFACE(((0.987470879370255,0.98761351460672,0.990694758798812),
(0.987470879370255,0.98761351460672,0.990694758798812)))
REPRESENTATION_ITEM('')
SURFACE()
);
#3913=(
BOUNDED_SURFACE()
B_SPLINE_SURFACE(1,2,((#160690,#160691,#160692,#160693,#160694),(#160695,
#160696,#160697,#160698,#160699)),.UNSPECIFIED.,.F.,.F.,.F.)
B_SPLINE_SURFACE_WITH_KNOTS((2,2),(3,2,3),(0.709719018660876,1.),(0.107879027750092,
0.125170525609407,0.125770422844536),.UNSPECIFIED.)
GEOMETRIC_REPRESENTATION_ITEM()
RATIONAL_B_SPLINE_SURFACE(((0.987469282487682,0.987594391229382,0.990658108926709,
0.990658108926709,0.990658108926709),(0.987469282487682,0.987594391229382,
0.990658108926709,0.990658108926709,0.990658108926709)))
REPRESENTATION_ITEM('')
SURFACE()
);
#3914=(
BOUNDED_SURFACE()
B_SPLINE_SURFACE(1,2,((#160701,#160702,#160703),(#160704,#160705,#160706)),
 .UNSPECIFIED.,.F.,.F.,.F.)
B_SPLINE_SURFACE_WITH_KNOTS((2,2),(3,3),(0.710192959008442,1.),(0.607982157956012,
0.625273655815329),.UNSPECIFIED.)
GEOMETRIC_REPRESENTATION_ITEM()
RATIONAL_B_SPLINE_SURFACE(((0.987470879370256,0.987613514606721,0.990694758798813),
(0.987470879370256,0.987613514606721,0.990694758798813)))
REPRESENTATION_ITEM('')
SURFACE()
);
#3915=(
BOUNDED_SURFACE()
B_SPLINE_SURFACE(1,2,((#160715,#160716,#160717,#160718,#160719),(#160720,
#160721,#160722,#160723,#160724)),.UNSPECIFIED.,.F.,.F.,.F.)
B_SPLINE_SURFACE_WITH_KNOTS((2,2),(3,2,3),(0.709719018647908,1.),(0.10787902775009,
0.125170525609407,0.125770422857558),.UNSPECIFIED.)
GEOMETRIC_REPRESENTATION_ITEM()
RATIONAL_B_SPLINE_SURFACE(((0.987469282487682,0.987594391229382,0.990658108926708,
0.990658108926708,0.990658108926708),(0.987469282487682,0.987594391229382,
0.990658108926708,0.990658108926708,0.990658108926708)))
REPRESENTATION_ITEM('')
SURFACE()
);
#3916=(
BOUNDED_SURFACE()
B_SPLINE_SURFACE(1,2,((#160726,#160727,#160728),(#160729,#160730,#160731)),
 .UNSPECIFIED.,.F.,.F.,.F.)
B_SPLINE_SURFACE_WITH_KNOTS((2,2),(3,3),(0.710192959008439,1.),(0.607982157956012,
0.625273655815329),.UNSPECIFIED.)
GEOMETRIC_REPRESENTATION_ITEM()
RATIONAL_B_SPLINE_SURFACE(((0.987470879370256,0.987613514606721,0.990694758798813),
(0.987470879370256,0.987613514606721,0.990694758798813)))
REPRESENTATION_ITEM('')
SURFACE()
);
#3917=(
BOUNDED_SURFACE()
B_SPLINE_SURFACE(1,2,((#160740,#160741,#160742,#160743,#160744),(#160745,
#160746,#160747,#160748,#160749)),.UNSPECIFIED.,.F.,.F.,.F.)
B_SPLINE_SURFACE_WITH_KNOTS((2,2),(3,2,3),(0.709719018670347,1.),(0.10787902775009,
0.125170525609407,0.125770422794484),.UNSPECIFIED.)
GEOMETRIC_REPRESENTATION_ITEM()
RATIONAL_B_SPLINE_SURFACE(((0.987469282487682,0.987594391229382,0.990658108926708,
0.990658108926708,0.990658108926708),(0.987469282487682,0.987594391229382,
0.990658108926708,0.990658108926708,0.990658108926708)))
REPRESENTATION_ITEM('')
SURFACE()
);
#3918=(
BOUNDED_SURFACE()
B_SPLINE_SURFACE(1,2,((#160751,#160752,#160753),(#160754,#160755,#160756)),
 .UNSPECIFIED.,.F.,.F.,.F.)
B_SPLINE_SURFACE_WITH_KNOTS((2,2),(3,3),(0.710192959008438,1.),(0.607982157956012,
0.625273655815329),.UNSPECIFIED.)
GEOMETRIC_REPRESENTATION_ITEM()
RATIONAL_B_SPLINE_SURFACE(((0.987470879370255,0.987613514606721,0.990694758798813),
(0.987470879370255,0.987613514606721,0.990694758798813)))
REPRESENTATION_ITEM('')
SURFACE()
);
#3919=(
BOUNDED_SURFACE()
B_SPLINE_SURFACE(1,2,((#160765,#160766,#160767,#160768,#160769),(#160770,
#160771,#160772,#160773,#160774)),.UNSPECIFIED.,.F.,.F.,.F.)
B_SPLINE_SURFACE_WITH_KNOTS((2,2),(3,2,3),(0.709719018669977,1.),(0.10787902775009,
0.125170525609407,0.125770422794847),.UNSPECIFIED.)
GEOMETRIC_REPRESENTATION_ITEM()
RATIONAL_B_SPLINE_SURFACE(((0.987469282487682,0.987594391229382,0.990658108926708,
0.990658108926708,0.990658108926708),(0.987469282487682,0.987594391229382,
0.990658108926708,0.990658108926708,0.990658108926708)))
REPRESENTATION_ITEM('')
SURFACE()
);
#3920=(
BOUNDED_SURFACE()
B_SPLINE_SURFACE(1,2,((#160776,#160777,#160778),(#160779,#160780,#160781)),
 .UNSPECIFIED.,.F.,.F.,.F.)
B_SPLINE_SURFACE_WITH_KNOTS((2,2),(3,3),(0.710192959008442,1.),(0.607982157956012,
0.625273655815329),.UNSPECIFIED.)
GEOMETRIC_REPRESENTATION_ITEM()
RATIONAL_B_SPLINE_SURFACE(((0.987470879370256,0.987613514606721,0.990694758798813),
(0.987470879370256,0.987613514606721,0.990694758798813)))
REPRESENTATION_ITEM('')
SURFACE()
);
#3921=(
BOUNDED_SURFACE()
B_SPLINE_SURFACE(1,2,((#160790,#160791,#160792,#160793,#160794),(#160795,
#160796,#160797,#160798,#160799)),.UNSPECIFIED.,.F.,.F.,.F.)
B_SPLINE_SURFACE_WITH_KNOTS((2,2),(3,2,3),(0.709719018661188,1.),(0.10787902775009,
0.125170525609407,0.125770422843774),.UNSPECIFIED.)
GEOMETRIC_REPRESENTATION_ITEM()
RATIONAL_B_SPLINE_SURFACE(((0.987469282487682,0.987594391229382,0.990658108926708,
0.990658108926708,0.990658108926708),(0.987469282487682,0.987594391229382,
0.990658108926708,0.990658108926708,0.990658108926708)))
REPRESENTATION_ITEM('')
SURFACE()
);
#3922=(
BOUNDED_SURFACE()
B_SPLINE_SURFACE(1,2,((#160801,#160802,#160803),(#160804,#160805,#160806)),
 .UNSPECIFIED.,.F.,.F.,.F.)
B_SPLINE_SURFACE_WITH_KNOTS((2,2),(3,3),(0.71019295900844,1.),(0.607982157956012,
0.625273655815329),.UNSPECIFIED.)
GEOMETRIC_REPRESENTATION_ITEM()
RATIONAL_B_SPLINE_SURFACE(((0.987470879370256,0.987613514606721,0.990694758798813),
(0.987470879370256,0.987613514606721,0.990694758798813)))
REPRESENTATION_ITEM('')
SURFACE()
);
#3923=(
BOUNDED_SURFACE()
B_SPLINE_SURFACE(1,2,((#160815,#160816,#160817,#160818,#160819),(#160820,
#160821,#160822,#160823,#160824)),.UNSPECIFIED.,.F.,.F.,.F.)
B_SPLINE_SURFACE_WITH_KNOTS((2,2),(3,2,3),(0.709719018663442,1.),(0.107879027750091,
0.125170525609407,0.125770422801386),.UNSPECIFIED.)
GEOMETRIC_REPRESENTATION_ITEM()
RATIONAL_B_SPLINE_SURFACE(((0.987469282487682,0.987594391229382,0.990658108926709,
0.990658108926709,0.990658108926709),(0.987469282487682,0.987594391229382,
0.990658108926709,0.990658108926709,0.990658108926709)))
REPRESENTATION_ITEM('')
SURFACE()
);
#3924=(
BOUNDED_SURFACE()
B_SPLINE_SURFACE(1,2,((#160826,#160827,#160828),(#160829,#160830,#160831)),
 .UNSPECIFIED.,.F.,.F.,.F.)
B_SPLINE_SURFACE_WITH_KNOTS((2,2),(3,3),(0.710192959008444,1.),(0.607982157956012,
0.625273655815329),.UNSPECIFIED.)
GEOMETRIC_REPRESENTATION_ITEM()
RATIONAL_B_SPLINE_SURFACE(((0.987470879370255,0.987613514606721,0.990694758798813),
(0.987470879370255,0.987613514606721,0.990694758798813)))
REPRESENTATION_ITEM('')
SURFACE()
);
#3925=(
BOUNDED_SURFACE()
B_SPLINE_SURFACE(1,2,((#160840,#160841,#160842,#160843,#160844),(#160845,
#160846,#160847,#160848,#160849)),.UNSPECIFIED.,.F.,.F.,.F.)
B_SPLINE_SURFACE_WITH_KNOTS((2,2),(3,2,3),(0.709719018653236,1.),(0.107879027750091,
0.125170525609407,0.125770422811596),.UNSPECIFIED.)
GEOMETRIC_REPRESENTATION_ITEM()
RATIONAL_B_SPLINE_SURFACE(((0.987469282487682,0.987594391229382,0.990658108926708,
0.990658108926708,0.990658108926708),(0.987469282487682,0.987594391229382,
0.990658108926708,0.990658108926708,0.990658108926708)))
REPRESENTATION_ITEM('')
SURFACE()
);
#3926=(
BOUNDED_SURFACE()
B_SPLINE_SURFACE(1,2,((#160851,#160852,#160853),(#160854,#160855,#160856)),
 .UNSPECIFIED.,.F.,.F.,.F.)
B_SPLINE_SURFACE_WITH_KNOTS((2,2),(3,3),(0.71019295900844,1.),(0.607982157956012,
0.625273655815329),.UNSPECIFIED.)
GEOMETRIC_REPRESENTATION_ITEM()
RATIONAL_B_SPLINE_SURFACE(((0.987470879370255,0.987613514606721,0.990694758798813),
(0.987470879370255,0.987613514606721,0.990694758798813)))
REPRESENTATION_ITEM('')
SURFACE()
);
#3927=(
BOUNDED_SURFACE()
B_SPLINE_SURFACE(1,2,((#160865,#160866,#160867,#160868,#160869),(#160870,
#160871,#160872,#160873,#160874)),.UNSPECIFIED.,.F.,.F.,.F.)
B_SPLINE_SURFACE_WITH_KNOTS((2,2),(3,2,3),(0.709719018681401,1.),(0.107879027750091,
0.125170525609407,0.125770422824321),.UNSPECIFIED.)
GEOMETRIC_REPRESENTATION_ITEM()
RATIONAL_B_SPLINE_SURFACE(((0.987469282487682,0.987594391229382,0.990658108926708,
0.990658108926708,0.990658108926708),(0.987469282487682,0.987594391229382,
0.990658108926708,0.990658108926708,0.990658108926708)))
REPRESENTATION_ITEM('')
SURFACE()
);
#3928=(
BOUNDED_SURFACE()
B_SPLINE_SURFACE(1,2,((#160876,#160877,#160878),(#160879,#160880,#160881)),
 .UNSPECIFIED.,.F.,.F.,.F.)
B_SPLINE_SURFACE_WITH_KNOTS((2,2),(3,3),(0.710192959008443,1.),(0.607982157956012,
0.625273655815329),.UNSPECIFIED.)
GEOMETRIC_REPRESENTATION_ITEM()
RATIONAL_B_SPLINE_SURFACE(((0.987470879370255,0.987613514606721,0.990694758798813),
(0.987470879370255,0.987613514606721,0.990694758798813)))
REPRESENTATION_ITEM('')
SURFACE()
);
#3929=(
BOUNDED_SURFACE()
B_SPLINE_SURFACE(1,2,((#160890,#160891,#160892,#160893,#160894),(#160895,
#160896,#160897,#160898,#160899)),.UNSPECIFIED.,.F.,.F.,.F.)
B_SPLINE_SURFACE_WITH_KNOTS((2,2),(3,2,3),(0.709719018663075,1.),(0.107879027750091,
0.125170525609407,0.125770422842613),.UNSPECIFIED.)
GEOMETRIC_REPRESENTATION_ITEM()
RATIONAL_B_SPLINE_SURFACE(((0.987469282487682,0.987594391229382,0.990658108926709,
0.990658108926709,0.990658108926709),(0.987469282487682,0.987594391229382,
0.990658108926708,0.990658108926708,0.990658108926708)))
REPRESENTATION_ITEM('')
SURFACE()
);
#3930=(
BOUNDED_SURFACE()
B_SPLINE_SURFACE(1,2,((#160901,#160902,#160903),(#160904,#160905,#160906)),
 .UNSPECIFIED.,.F.,.F.,.F.)
B_SPLINE_SURFACE_WITH_KNOTS((2,2),(3,3),(0.710192959008438,1.),(0.607982157956011,
0.625273655815329),.UNSPECIFIED.)
GEOMETRIC_REPRESENTATION_ITEM()
RATIONAL_B_SPLINE_SURFACE(((0.987470879370256,0.987613514606721,0.990694758798813),
(0.987470879370256,0.987613514606721,0.990694758798813)))
REPRESENTATION_ITEM('')
SURFACE()
);
#3931=(
BOUNDED_SURFACE()
B_SPLINE_SURFACE(1,2,((#160915,#160916,#160917,#160918,#160919),(#160920,
#160921,#160922,#160923,#160924)),.UNSPECIFIED.,.F.,.F.,.F.)
B_SPLINE_SURFACE_WITH_KNOTS((2,2),(3,2,3),(0.709719018666025,1.),(0.107879027750091,
0.125170525609407,0.125770422839723),.UNSPECIFIED.)
GEOMETRIC_REPRESENTATION_ITEM()
RATIONAL_B_SPLINE_SURFACE(((0.987469282487682,0.987594391229382,0.990658108926708,
0.990658108926708,0.990658108926708),(0.987469282487682,0.987594391229382,
0.990658108926708,0.990658108926708,0.990658108926708)))
REPRESENTATION_ITEM('')
SURFACE()
);
#3932=(
BOUNDED_SURFACE()
B_SPLINE_SURFACE(1,2,((#160926,#160927,#160928),(#160929,#160930,#160931)),
 .UNSPECIFIED.,.F.,.F.,.F.)
B_SPLINE_SURFACE_WITH_KNOTS((2,2),(3,3),(0.710192959008441,1.),(0.607982157956012,
0.625273655815329),.UNSPECIFIED.)
GEOMETRIC_REPRESENTATION_ITEM()
RATIONAL_B_SPLINE_SURFACE(((0.987470879370256,0.987613514606721,0.990694758798813),
(0.987470879370256,0.987613514606721,0.990694758798813)))
REPRESENTATION_ITEM('')
SURFACE()
);
#3933=(
BOUNDED_SURFACE()
B_SPLINE_SURFACE(1,2,((#160940,#160941,#160942,#160943,#160944),(#160945,
#160946,#160947,#160948,#160949)),.UNSPECIFIED.,.F.,.F.,.F.)
B_SPLINE_SURFACE_WITH_KNOTS((2,2),(3,2,3),(0.709719018663549,1.),(0.10787902775009,
0.125170525609407,0.125770422801283),.UNSPECIFIED.)
GEOMETRIC_REPRESENTATION_ITEM()
RATIONAL_B_SPLINE_SURFACE(((0.987469282487682,0.987594391229382,0.990658108926708,
0.990658108926708,0.990658108926708),(0.987469282487682,0.987594391229382,
0.990658108926708,0.990658108926708,0.990658108926708)))
REPRESENTATION_ITEM('')
SURFACE()
);
#3934=(
BOUNDED_SURFACE()
B_SPLINE_SURFACE(1,2,((#160951,#160952,#160953),(#160954,#160955,#160956)),
 .UNSPECIFIED.,.F.,.F.,.F.)
B_SPLINE_SURFACE_WITH_KNOTS((2,2),(3,3),(0.710192959008435,1.),(0.607982157956012,
0.625273655815329),.UNSPECIFIED.)
GEOMETRIC_REPRESENTATION_ITEM()
RATIONAL_B_SPLINE_SURFACE(((0.987470879370255,0.987613514606721,0.990694758798813),
(0.987470879370255,0.987613514606721,0.990694758798813)))
REPRESENTATION_ITEM('')
SURFACE()
);
#3935=(
BOUNDED_SURFACE()
B_SPLINE_SURFACE(1,2,((#160965,#160966,#160967,#160968,#160969),(#160970,
#160971,#160972,#160973,#160974)),.UNSPECIFIED.,.F.,.F.,.F.)
B_SPLINE_SURFACE_WITH_KNOTS((2,2),(3,2,3),(0.709719018657777,1.),(0.107879027750091,
0.125170525609407,0.125770422807052),.UNSPECIFIED.)
GEOMETRIC_REPRESENTATION_ITEM()
RATIONAL_B_SPLINE_SURFACE(((0.987469282487682,0.987594391229382,0.990658108926708,
0.990658108926708,0.990658108926708),(0.987469282487682,0.987594391229382,
0.990658108926708,0.990658108926708,0.990658108926708)))
REPRESENTATION_ITEM('')
SURFACE()
);
#3936=(
BOUNDED_SURFACE()
B_SPLINE_SURFACE(1,2,((#160976,#160977,#160978),(#160979,#160980,#160981)),
 .UNSPECIFIED.,.F.,.F.,.F.)
B_SPLINE_SURFACE_WITH_KNOTS((2,2),(3,3),(0.710192959008442,1.),(0.607982157956012,
0.625273655815329),.UNSPECIFIED.)
GEOMETRIC_REPRESENTATION_ITEM()
RATIONAL_B_SPLINE_SURFACE(((0.987470879370255,0.987613514606721,0.990694758798813),
(0.987470879370255,0.987613514606721,0.990694758798813)))
REPRESENTATION_ITEM('')
SURFACE()
);
#3937=(
BOUNDED_SURFACE()
B_SPLINE_SURFACE(1,2,((#160990,#160991,#160992,#160993,#160994),(#160995,
#160996,#160997,#160998,#160999)),.UNSPECIFIED.,.F.,.F.,.F.)
B_SPLINE_SURFACE_WITH_KNOTS((2,2),(3,2,3),(0.709719018667416,1.),(0.107879027750091,
0.125170525609407,0.125770422797416),.UNSPECIFIED.)
GEOMETRIC_REPRESENTATION_ITEM()
RATIONAL_B_SPLINE_SURFACE(((0.987469282487682,0.987594391229382,0.990658108926708,
0.990658108926708,0.990658108926708),(0.987469282487682,0.987594391229382,
0.990658108926708,0.990658108926708,0.990658108926708)))
REPRESENTATION_ITEM('')
SURFACE()
);
#3938=(
BOUNDED_SURFACE()
B_SPLINE_SURFACE(1,2,((#161001,#161002,#161003),(#161004,#161005,#161006)),
 .UNSPECIFIED.,.F.,.F.,.F.)
B_SPLINE_SURFACE_WITH_KNOTS((2,2),(3,3),(0.710192959008442,1.),(0.607982157956012,
0.625273655815329),.UNSPECIFIED.)
GEOMETRIC_REPRESENTATION_ITEM()
RATIONAL_B_SPLINE_SURFACE(((0.987470879370256,0.987613514606721,0.990694758798813),
(0.987470879370256,0.987613514606721,0.990694758798813)))
REPRESENTATION_ITEM('')
SURFACE()
);
#3939=(
BOUNDED_SURFACE()
B_SPLINE_SURFACE(1,2,((#161015,#161016,#161017,#161018,#161019),(#161020,
#161021,#161022,#161023,#161024)),.UNSPECIFIED.,.F.,.F.,.F.)
B_SPLINE_SURFACE_WITH_KNOTS((2,2),(3,2,3),(0.70971901865264,1.),(0.107879027750091,
0.125170525609407,0.125770422852652),.UNSPECIFIED.)
GEOMETRIC_REPRESENTATION_ITEM()
RATIONAL_B_SPLINE_SURFACE(((0.987469282487682,0.987594391229382,0.990658108926708,
0.990658108926708,0.990658108926708),(0.987469282487682,0.987594391229382,
0.990658108926708,0.990658108926708,0.990658108926708)))
REPRESENTATION_ITEM('')
SURFACE()
);
#3940=(
BOUNDED_SURFACE()
B_SPLINE_SURFACE(1,2,((#161026,#161027,#161028),(#161029,#161030,#161031)),
 .UNSPECIFIED.,.F.,.F.,.F.)
B_SPLINE_SURFACE_WITH_KNOTS((2,2),(3,3),(0.710192959008445,1.),(0.607982157956012,
0.625273655815329),.UNSPECIFIED.)
GEOMETRIC_REPRESENTATION_ITEM()
RATIONAL_B_SPLINE_SURFACE(((0.987470879370255,0.987613514606721,0.990694758798813),
(0.987470879370255,0.987613514606721,0.990694758798813)))
REPRESENTATION_ITEM('')
SURFACE()
);
#3941=(
BOUNDED_SURFACE()
B_SPLINE_SURFACE(1,2,((#161040,#161041,#161042,#161043,#161044),(#161045,
#161046,#161047,#161048,#161049)),.UNSPECIFIED.,.F.,.F.,.F.)
B_SPLINE_SURFACE_WITH_KNOTS((2,2),(3,2,3),(0.709719018677328,1.),(0.107879027750091,
0.125170525609407,0.125770422723825),.UNSPECIFIED.)
GEOMETRIC_REPRESENTATION_ITEM()
RATIONAL_B_SPLINE_SURFACE(((0.987469282487682,0.987594391229382,0.990658108926708,
0.990658108926708,0.990658108926708),(0.987469282487682,0.987594391229382,
0.990658108926708,0.990658108926708,0.990658108926708)))
REPRESENTATION_ITEM('')
SURFACE()
);
#3942=(
BOUNDED_SURFACE()
B_SPLINE_SURFACE(1,2,((#161051,#161052,#161053),(#161054,#161055,#161056)),
 .UNSPECIFIED.,.F.,.F.,.F.)
B_SPLINE_SURFACE_WITH_KNOTS((2,2),(3,3),(0.710192959008401,1.),(0.607982157956004,
0.625273655815328),.UNSPECIFIED.)
GEOMETRIC_REPRESENTATION_ITEM()
RATIONAL_B_SPLINE_SURFACE(((0.987470879370255,0.987613514606719,0.990694758798812),
(0.987470879370255,0.987613514606719,0.990694758798812)))
REPRESENTATION_ITEM('')
SURFACE()
);
#3943=(
BOUNDED_SURFACE()
B_SPLINE_SURFACE(1,2,((#161065,#161066,#161067,#161068,#161069),(#161070,
#161071,#161072,#161073,#161074)),.UNSPECIFIED.,.F.,.F.,.F.)
B_SPLINE_SURFACE_WITH_KNOTS((2,2),(3,2,3),(0.709719018645982,1.),(0.107879027750092,
0.125170525609408,0.125770422859206),.UNSPECIFIED.)
GEOMETRIC_REPRESENTATION_ITEM()
RATIONAL_B_SPLINE_SURFACE(((0.987469282487682,0.987594391229382,0.990658108926709,
0.990658108926709,0.990658108926709),(0.987469282487682,0.987594391229382,
0.990658108926709,0.990658108926709,0.990658108926709)))
REPRESENTATION_ITEM('')
SURFACE()
);
#3944=(
BOUNDED_SURFACE()
B_SPLINE_SURFACE(1,2,((#161076,#161077,#161078),(#161079,#161080,#161081)),
 .UNSPECIFIED.,.F.,.F.,.F.)
B_SPLINE_SURFACE_WITH_KNOTS((2,2),(3,3),(0.710192959008439,1.),(0.607982157956011,
0.625273655815328),.UNSPECIFIED.)
GEOMETRIC_REPRESENTATION_ITEM()
RATIONAL_B_SPLINE_SURFACE(((0.987470879370255,0.98761351460672,0.990694758798812),
(0.987470879370255,0.98761351460672,0.990694758798812)))
REPRESENTATION_ITEM('')
SURFACE()
);
#3945=(
BOUNDED_SURFACE()
B_SPLINE_SURFACE(1,2,((#161090,#161091,#161092,#161093,#161094),(#161095,
#161096,#161097,#161098,#161099)),.UNSPECIFIED.,.F.,.F.,.F.)
B_SPLINE_SURFACE_WITH_KNOTS((2,2),(3,2,3),(0.709719018671277,1.),(0.107879027750092,
0.125170525609409,0.125770422834533),.UNSPECIFIED.)
GEOMETRIC_REPRESENTATION_ITEM()
RATIONAL_B_SPLINE_SURFACE(((0.987469282487682,0.987594391229382,0.990658108926709,
0.990658108926709,0.990658108926709),(0.987469282487682,0.987594391229382,
0.990658108926709,0.990658108926709,0.990658108926709)))
REPRESENTATION_ITEM('')
SURFACE()
);
#3946=(
BOUNDED_SURFACE()
B_SPLINE_SURFACE(1,2,((#161101,#161102,#161103),(#161104,#161105,#161106)),
 .UNSPECIFIED.,.F.,.F.,.F.)
B_SPLINE_SURFACE_WITH_KNOTS((2,2),(3,3),(0.710192959008442,1.),(0.607982157956011,
0.625273655815328),.UNSPECIFIED.)
GEOMETRIC_REPRESENTATION_ITEM()
RATIONAL_B_SPLINE_SURFACE(((0.987470879370255,0.98761351460672,0.990694758798812),
(0.987470879370255,0.98761351460672,0.990694758798812)))
REPRESENTATION_ITEM('')
SURFACE()
);
#3947=(
BOUNDED_SURFACE()
B_SPLINE_SURFACE(1,2,((#161115,#161116,#161117,#161118,#161119),(#161120,
#161121,#161122,#161123,#161124)),.UNSPECIFIED.,.F.,.F.,.F.)
B_SPLINE_SURFACE_WITH_KNOTS((2,2),(3,2,3),(0.709719018674124,1.),(0.107879027750092,
0.125170525609408,0.125770422790709),.UNSPECIFIED.)
GEOMETRIC_REPRESENTATION_ITEM()
RATIONAL_B_SPLINE_SURFACE(((0.987469282487682,0.987594391229382,0.990658108926709,
0.990658108926709,0.990658108926709),(0.987469282487682,0.987594391229382,
0.990658108926709,0.990658108926709,0.990658108926709)))
REPRESENTATION_ITEM('')
SURFACE()
);
#3948=(
BOUNDED_SURFACE()
B_SPLINE_SURFACE(1,2,((#161126,#161127,#161128),(#161129,#161130,#161131)),
 .UNSPECIFIED.,.F.,.F.,.F.)
B_SPLINE_SURFACE_WITH_KNOTS((2,2),(3,3),(0.710192959008299,1.),(0.607982157956011,
0.625273655815328),.UNSPECIFIED.)
GEOMETRIC_REPRESENTATION_ITEM()
RATIONAL_B_SPLINE_SURFACE(((0.987470879370255,0.98761351460672,0.990694758798812),
(0.987470879370255,0.98761351460672,0.990694758798812)))
REPRESENTATION_ITEM('')
SURFACE()
);
#3949=(
BOUNDED_SURFACE()
B_SPLINE_SURFACE(1,2,((#161140,#161141,#161142,#161143,#161144),(#161145,
#161146,#161147,#161148,#161149)),.UNSPECIFIED.,.F.,.F.,.F.)
B_SPLINE_SURFACE_WITH_KNOTS((2,2),(3,2,3),(0.709719018668243,1.),(0.107879027750092,
0.125170525609408,0.125770422796449),.UNSPECIFIED.)
GEOMETRIC_REPRESENTATION_ITEM()
RATIONAL_B_SPLINE_SURFACE(((0.987469282487682,0.987594391229382,0.990658108926709,
0.990658108926709,0.990658108926709),(0.987469282487682,0.987594391229382,
0.990658108926709,0.990658108926709,0.990658108926709)))
REPRESENTATION_ITEM('')
SURFACE()
);
#3950=(
BOUNDED_SURFACE()
B_SPLINE_SURFACE(1,2,((#161151,#161152,#161153),(#161154,#161155,#161156)),
 .UNSPECIFIED.,.F.,.F.,.F.)
B_SPLINE_SURFACE_WITH_KNOTS((2,2),(3,3),(0.710192959008295,1.),(0.607982157956011,
0.625273655815328),.UNSPECIFIED.)
GEOMETRIC_REPRESENTATION_ITEM()
RATIONAL_B_SPLINE_SURFACE(((0.987470879370255,0.98761351460672,0.990694758798812),
(0.987470879370255,0.98761351460672,0.990694758798812)))
REPRESENTATION_ITEM('')
SURFACE()
);
#3951=(
BOUNDED_SURFACE()
B_SPLINE_SURFACE(1,2,((#161165,#161166,#161167,#161168,#161169),(#161170,
#161171,#161172,#161173,#161174)),.UNSPECIFIED.,.F.,.F.,.F.)
B_SPLINE_SURFACE_WITH_KNOTS((2,2),(3,2,3),(0.709719018652826,1.),(0.107879027750092,
0.125170525609408,0.125770422811858),.UNSPECIFIED.)
GEOMETRIC_REPRESENTATION_ITEM()
RATIONAL_B_SPLINE_SURFACE(((0.987469282487682,0.987594391229382,0.990658108926709,
0.990658108926709,0.990658108926709),(0.987469282487682,0.987594391229382,
0.990658108926709,0.990658108926709,0.990658108926709)))
REPRESENTATION_ITEM('')
SURFACE()
);
#3952=(
BOUNDED_SURFACE()
B_SPLINE_SURFACE(1,2,((#161176,#161177,#161178),(#161179,#161180,#161181)),
 .UNSPECIFIED.,.F.,.F.,.F.)
B_SPLINE_SURFACE_WITH_KNOTS((2,2),(3,3),(0.710192959008283,1.),(0.607982157956011,
0.625273655815328),.UNSPECIFIED.)
GEOMETRIC_REPRESENTATION_ITEM()
RATIONAL_B_SPLINE_SURFACE(((0.987470879370255,0.98761351460672,0.990694758798812),
(0.987470879370255,0.98761351460672,0.990694758798812)))
REPRESENTATION_ITEM('')
SURFACE()
);
#3953=(
BOUNDED_SURFACE()
B_SPLINE_SURFACE(1,2,((#161190,#161191,#161192,#161193,#161194),(#161195,
#161196,#161197,#161198,#161199)),.UNSPECIFIED.,.F.,.F.,.F.)
B_SPLINE_SURFACE_WITH_KNOTS((2,2),(3,2,3),(0.709719018665039,1.),(0.107879027750092,
0.125170525609408,0.125770422799641),.UNSPECIFIED.)
GEOMETRIC_REPRESENTATION_ITEM()
RATIONAL_B_SPLINE_SURFACE(((0.987469282487682,0.987594391229382,0.990658108926709,
0.990658108926709,0.990658108926709),(0.987469282487682,0.987594391229382,
0.990658108926709,0.990658108926709,0.990658108926709)))
REPRESENTATION_ITEM('')
SURFACE()
);
#3954=(
BOUNDED_SURFACE()
B_SPLINE_SURFACE(1,2,((#161201,#161202,#161203),(#161204,#161205,#161206)),
 .UNSPECIFIED.,.F.,.F.,.F.)
B_SPLINE_SURFACE_WITH_KNOTS((2,2),(3,3),(0.710192959006913,1.),(0.607982157956011,
0.625273655815328),.UNSPECIFIED.)
GEOMETRIC_REPRESENTATION_ITEM()
RATIONAL_B_SPLINE_SURFACE(((0.987470879370255,0.98761351460672,0.990694758798812),
(0.987470879370255,0.98761351460672,0.990694758798812)))
REPRESENTATION_ITEM('')
SURFACE()
);
#3955=(
BOUNDED_SURFACE()
B_SPLINE_SURFACE(1,2,((#161215,#161216,#161217,#161218,#161219),(#161220,
#161221,#161222,#161223,#161224)),.UNSPECIFIED.,.F.,.F.,.F.)
B_SPLINE_SURFACE_WITH_KNOTS((2,2),(3,2,3),(0.709719018659893,1.),(0.107879027750092,
0.125170525609408,0.12577042280342),.UNSPECIFIED.)
GEOMETRIC_REPRESENTATION_ITEM()
RATIONAL_B_SPLINE_SURFACE(((0.987469282487682,0.987594391229382,0.990658108926709,
0.990658108926709,0.990658108926709),(0.987469282487682,0.987594391229382,
0.990658108926709,0.990658108926709,0.990658108926709)))
REPRESENTATION_ITEM('')
SURFACE()
);
#3956=(
BOUNDED_SURFACE()
B_SPLINE_SURFACE(1,2,((#161226,#161227,#161228),(#161229,#161230,#161231)),
 .UNSPECIFIED.,.F.,.F.,.F.)
B_SPLINE_SURFACE_WITH_KNOTS((2,2),(3,3),(0.710192959008063,1.),(0.607982157956011,
0.625273655815328),.UNSPECIFIED.)
GEOMETRIC_REPRESENTATION_ITEM()
RATIONAL_B_SPLINE_SURFACE(((0.987470879370255,0.98761351460672,0.990694758798812),
(0.987470879370255,0.98761351460672,0.990694758798812)))
REPRESENTATION_ITEM('')
SURFACE()
);
#3957=(
BOUNDED_SURFACE()
B_SPLINE_SURFACE(1,2,((#161240,#161241,#161242,#161243,#161244),(#161245,
#161246,#161247,#161248,#161249)),.UNSPECIFIED.,.F.,.F.,.F.)
B_SPLINE_SURFACE_WITH_KNOTS((2,2),(3,2,3),(0.709719018652961,1.),(0.107879027750092,
0.125170525609408,0.125770422851709),.UNSPECIFIED.)
GEOMETRIC_REPRESENTATION_ITEM()
RATIONAL_B_SPLINE_SURFACE(((0.987469282487682,0.987594391229382,0.990658108926709,
0.990658108926709,0.990658108926709),(0.987469282487682,0.987594391229382,
0.990658108926709,0.990658108926709,0.990658108926709)))
REPRESENTATION_ITEM('')
SURFACE()
);
#3958=(
BOUNDED_SURFACE()
B_SPLINE_SURFACE(1,2,((#161251,#161252,#161253),(#161254,#161255,#161256)),
 .UNSPECIFIED.,.F.,.F.,.F.)
B_SPLINE_SURFACE_WITH_KNOTS((2,2),(3,3),(0.710192959008438,1.),(0.607982157956011,
0.625273655815328),.UNSPECIFIED.)
GEOMETRIC_REPRESENTATION_ITEM()
RATIONAL_B_SPLINE_SURFACE(((0.987470879370255,0.98761351460672,0.990694758798812),
(0.987470879370255,0.98761351460672,0.990694758798812)))
REPRESENTATION_ITEM('')
SURFACE()
);
#3959=(
BOUNDED_SURFACE()
B_SPLINE_SURFACE(1,2,((#161265,#161266,#161267,#161268,#161269),(#161270,
#161271,#161272,#161273,#161274)),.UNSPECIFIED.,.F.,.F.,.F.)
B_SPLINE_SURFACE_WITH_KNOTS((2,2),(3,2,3),(0.709719018650375,1.),(0.107879027750092,
0.125170525609408,0.125770422855389),.UNSPECIFIED.)
GEOMETRIC_REPRESENTATION_ITEM()
RATIONAL_B_SPLINE_SURFACE(((0.987469282487682,0.987594391229382,0.990658108926709,
0.990658108926709,0.990658108926709),(0.987469282487682,0.987594391229382,
0.990658108926709,0.990658108926709,0.990658108926709)))
REPRESENTATION_ITEM('')
SURFACE()
);
#3960=(
BOUNDED_SURFACE()
B_SPLINE_SURFACE(1,2,((#161276,#161277,#161278),(#161279,#161280,#161281)),
 .UNSPECIFIED.,.F.,.F.,.F.)
B_SPLINE_SURFACE_WITH_KNOTS((2,2),(3,3),(0.71019295900844,1.),(0.607982157956011,
0.625273655815328),.UNSPECIFIED.)
GEOMETRIC_REPRESENTATION_ITEM()
RATIONAL_B_SPLINE_SURFACE(((0.987470879370255,0.987613514606721,0.990694758798812),
(0.987470879370255,0.98761351460672,0.990694758798812)))
REPRESENTATION_ITEM('')
SURFACE()
);
#3961=(
BOUNDED_SURFACE()
B_SPLINE_SURFACE(1,2,((#161290,#161291,#161292,#161293,#161294),(#161295,
#161296,#161297,#161298,#161299)),.UNSPECIFIED.,.F.,.F.,.F.)
B_SPLINE_SURFACE_WITH_KNOTS((2,2),(3,2,3),(0.709719018647816,1.),(0.107879027750092,
0.125170525609408,0.125770422857201),.UNSPECIFIED.)
GEOMETRIC_REPRESENTATION_ITEM()
RATIONAL_B_SPLINE_SURFACE(((0.987469282487682,0.987594391229382,0.990658108926709,
0.990658108926709,0.990658108926709),(0.987469282487682,0.987594391229382,
0.990658108926709,0.990658108926709,0.990658108926709)))
REPRESENTATION_ITEM('')
SURFACE()
);
#3962=(
BOUNDED_SURFACE()
B_SPLINE_SURFACE(1,2,((#161301,#161302,#161303),(#161304,#161305,#161306)),
 .UNSPECIFIED.,.F.,.F.,.F.)
B_SPLINE_SURFACE_WITH_KNOTS((2,2),(3,3),(0.710192959008442,1.),(0.607982157956011,
0.625273655815328),.UNSPECIFIED.)
GEOMETRIC_REPRESENTATION_ITEM()
RATIONAL_B_SPLINE_SURFACE(((0.987470879370255,0.98761351460672,0.990694758798812),
(0.987470879370255,0.98761351460672,0.990694758798812)))
REPRESENTATION_ITEM('')
SURFACE()
);
#3963=(
BOUNDED_SURFACE()
B_SPLINE_SURFACE(1,2,((#161315,#161316,#161317,#161318,#161319),(#161320,
#161321,#161322,#161323,#161324)),.UNSPECIFIED.,.F.,.F.,.F.)
B_SPLINE_SURFACE_WITH_KNOTS((2,2),(3,2,3),(0.709719018663423,1.),(0.107879027750092,
0.125170525609408,0.125770422801407),.UNSPECIFIED.)
GEOMETRIC_REPRESENTATION_ITEM()
RATIONAL_B_SPLINE_SURFACE(((0.987469282487682,0.987594391229382,0.990658108926709,
0.990658108926709,0.990658108926709),(0.987469282487682,0.987594391229382,
0.990658108926709,0.990658108926709,0.990658108926709)))
REPRESENTATION_ITEM('')
SURFACE()
);
#3964=(
BOUNDED_SURFACE()
B_SPLINE_SURFACE(1,2,((#161326,#161327,#161328,#161329,#161330),(#161331,
#161332,#161333,#161334,#161335)),.UNSPECIFIED.,.F.,.F.,.F.)
B_SPLINE_SURFACE_WITH_KNOTS((2,2),(3,2,3),(0.,0.290280981336755),(0.607879027750091,
0.625170525609408,0.625770422759447),.UNSPECIFIED.)
GEOMETRIC_REPRESENTATION_ITEM()
RATIONAL_B_SPLINE_SURFACE(((0.987469282487682,0.987594391229382,0.990658108926708,
0.990658108926708,0.990658108926708),(0.987469282487682,0.987594391229382,
0.990658108926708,0.990658108926708,0.990658108926708)))
REPRESENTATION_ITEM('')
SURFACE()
);
#3965=(
BOUNDED_SURFACE()
B_SPLINE_SURFACE(1,2,((#161346,#161347,#161348),(#161349,#161350,#161351)),
 .UNSPECIFIED.,.F.,.F.,.F.)
B_SPLINE_SURFACE_WITH_KNOTS((2,2),(3,3),(0.,0.289807040991561),(0.107982157956012,
0.125273655815329),.UNSPECIFIED.)
GEOMETRIC_REPRESENTATION_ITEM()
RATIONAL_B_SPLINE_SURFACE(((0.987470879370255,0.987613514606721,0.990694758798813),
(0.987470879370255,0.987613514606721,0.990694758798813)))
REPRESENTATION_ITEM('')
SURFACE()
);
#3966=(
BOUNDED_SURFACE()
B_SPLINE_SURFACE(1,2,((#161369,#161370,#161371,#161372,#161373),(#161374,
#161375,#161376,#161377,#161378)),.UNSPECIFIED.,.F.,.F.,.F.)
B_SPLINE_SURFACE_WITH_KNOTS((2,2),(3,2,3),(0.,0.290280981329489),(0.607879027750091,
0.625170525609407,0.625770422752178),.UNSPECIFIED.)
GEOMETRIC_REPRESENTATION_ITEM()
RATIONAL_B_SPLINE_SURFACE(((0.987469282487682,0.987594391229382,0.990658108926708,
0.990658108926708,0.990658108926708),(0.987469282487682,0.987594391229382,
0.990658108926708,0.990658108926708,0.990658108926708)))
REPRESENTATION_ITEM('')
SURFACE()
);
#3967=(
BOUNDED_SURFACE()
B_SPLINE_SURFACE(1,2,((#161385,#161386,#161387),(#161388,#161389,#161390)),
 .UNSPECIFIED.,.F.,.F.,.F.)
B_SPLINE_SURFACE_WITH_KNOTS((2,2),(3,3),(0.,0.289807040991559),(0.107982157956012,
0.125273655815329),.UNSPECIFIED.)
GEOMETRIC_REPRESENTATION_ITEM()
RATIONAL_B_SPLINE_SURFACE(((0.987470879370256,0.987613514606721,0.990694758798813),
(0.987470879370255,0.987613514606721,0.990694758798813)))
REPRESENTATION_ITEM('')
SURFACE()
);
#3968=(
BOUNDED_SURFACE()
B_SPLINE_SURFACE(1,2,((#161408,#161409,#161410,#161411,#161412),(#161413,
#161414,#161415,#161416,#161417)),.UNSPECIFIED.,.F.,.F.,.F.)
B_SPLINE_SURFACE_WITH_KNOTS((2,2),(3,2,3),(0.,0.290280981342653),(0.607879027750091,
0.625170525609407,0.625770422765346),.UNSPECIFIED.)
GEOMETRIC_REPRESENTATION_ITEM()
RATIONAL_B_SPLINE_SURFACE(((0.987469282487682,0.987594391229382,0.990658108926708,
0.990658108926708,0.990658108926708),(0.987469282487682,0.987594391229382,
0.990658108926708,0.990658108926708,0.990658108926708)))
REPRESENTATION_ITEM('')
SURFACE()
);
#3969=(
BOUNDED_SURFACE()
B_SPLINE_SURFACE(1,2,((#161424,#161425,#161426),(#161427,#161428,#161429)),
 .UNSPECIFIED.,.F.,.F.,.F.)
B_SPLINE_SURFACE_WITH_KNOTS((2,2),(3,3),(0.,0.289807040991559),(0.107982157956012,
0.125273655815329),.UNSPECIFIED.)
GEOMETRIC_REPRESENTATION_ITEM()
RATIONAL_B_SPLINE_SURFACE(((0.987470879370255,0.987613514606721,0.990694758798813),
(0.987470879370255,0.987613514606721,0.990694758798813)))
REPRESENTATION_ITEM('')
SURFACE()
);
#3970=(
BOUNDED_SURFACE()
B_SPLINE_SURFACE(1,2,((#161447,#161448,#161449,#161450,#161451),(#161452,
#161453,#161454,#161455,#161456)),.UNSPECIFIED.,.F.,.F.,.F.)
B_SPLINE_SURFACE_WITH_KNOTS((2,2),(3,2,3),(0.,0.290280981329113),(0.607879027750091,
0.625170525609408,0.625770422751802),.UNSPECIFIED.)
GEOMETRIC_REPRESENTATION_ITEM()
RATIONAL_B_SPLINE_SURFACE(((0.987469282487682,0.987594391229382,0.990658108926708,
0.990658108926708,0.990658108926708),(0.987469282487682,0.987594391229382,
0.990658108926708,0.990658108926708,0.990658108926708)))
REPRESENTATION_ITEM('')
SURFACE()
);
#3971=(
BOUNDED_SURFACE()
B_SPLINE_SURFACE(1,2,((#161463,#161464,#161465),(#161466,#161467,#161468)),
 .UNSPECIFIED.,.F.,.F.,.F.)
B_SPLINE_SURFACE_WITH_KNOTS((2,2),(3,3),(0.,0.289807040991557),(0.107982157956012,
0.125273655815328),.UNSPECIFIED.)
GEOMETRIC_REPRESENTATION_ITEM()
RATIONAL_B_SPLINE_SURFACE(((0.987470879370256,0.987613514606721,0.990694758798812),
(0.987470879370256,0.987613514606721,0.990694758798812)))
REPRESENTATION_ITEM('')
SURFACE()
);
#3972=(
BOUNDED_SURFACE()
B_SPLINE_SURFACE(1,2,((#161486,#161487,#161488,#161489,#161490),(#161491,
#161492,#161493,#161494,#161495)),.UNSPECIFIED.,.F.,.F.,.F.)
B_SPLINE_SURFACE_WITH_KNOTS((2,2),(3,2,3),(0.,0.290280981348175),(0.607879027750092,
0.625170525609408,0.625770422770872),.UNSPECIFIED.)
GEOMETRIC_REPRESENTATION_ITEM()
RATIONAL_B_SPLINE_SURFACE(((0.987469282487682,0.987594391229382,0.990658108926709,
0.990658108926709,0.990658108926709),(0.987469282487682,0.987594391229382,
0.990658108926709,0.990658108926709,0.990658108926709)))
REPRESENTATION_ITEM('')
SURFACE()
);
#3973=(
BOUNDED_SURFACE()
B_SPLINE_SURFACE(1,2,((#161502,#161503,#161504),(#161505,#161506,#161507)),
 .UNSPECIFIED.,.F.,.F.,.F.)
B_SPLINE_SURFACE_WITH_KNOTS((2,2),(3,3),(0.,0.289807040991561),(0.107982157956011,
0.125273655815328),.UNSPECIFIED.)
GEOMETRIC_REPRESENTATION_ITEM()
RATIONAL_B_SPLINE_SURFACE(((0.987470879370255,0.98761351460672,0.990694758798812),
(0.987470879370255,0.98761351460672,0.990694758798812)))
REPRESENTATION_ITEM('')
SURFACE()
);
#3974=(
BOUNDED_SURFACE()
B_SPLINE_SURFACE(1,2,((#161525,#161526,#161527,#161528,#161529),(#161530,
#161531,#161532,#161533,#161534)),.UNSPECIFIED.,.F.,.F.,.F.)
B_SPLINE_SURFACE_WITH_KNOTS((2,2),(3,2,3),(0.,0.290280981322439),(0.607879027750092,
0.625170525609409,0.625770422745125),.UNSPECIFIED.)
GEOMETRIC_REPRESENTATION_ITEM()
RATIONAL_B_SPLINE_SURFACE(((0.987469282487682,0.987594391229382,0.990658108926709,
0.990658108926709,0.990658108926709),(0.987469282487682,0.987594391229382,
0.990658108926709,0.990658108926709,0.990658108926709)))
REPRESENTATION_ITEM('')
SURFACE()
);
#3975=(
BOUNDED_SURFACE()
B_SPLINE_SURFACE(1,2,((#161541,#161542,#161543),(#161544,#161545,#161546)),
 .UNSPECIFIED.,.F.,.F.,.F.)
B_SPLINE_SURFACE_WITH_KNOTS((2,2),(3,3),(0.,0.289807040991559),(0.107982157956011,
0.125273655815328),.UNSPECIFIED.)
GEOMETRIC_REPRESENTATION_ITEM()
RATIONAL_B_SPLINE_SURFACE(((0.987470879370255,0.98761351460672,0.990694758798812),
(0.987470879370255,0.98761351460672,0.990694758798812)))
REPRESENTATION_ITEM('')
SURFACE()
);
#3976=(
BOUNDED_SURFACE()
B_SPLINE_SURFACE(1,2,((#161564,#161565,#161566,#161567,#161568),(#161569,
#161570,#161571,#161572,#161573)),.UNSPECIFIED.,.F.,.F.,.F.)
B_SPLINE_SURFACE_WITH_KNOTS((2,2),(3,2,3),(0.,0.290280981323384),(0.607879027750092,
0.625170525609408,0.625770422746075),.UNSPECIFIED.)
GEOMETRIC_REPRESENTATION_ITEM()
RATIONAL_B_SPLINE_SURFACE(((0.987469282487682,0.987594391229382,0.990658108926709,
0.990658108926709,0.990658108926709),(0.987469282487682,0.987594391229382,
0.990658108926709,0.990658108926709,0.990658108926709)))
REPRESENTATION_ITEM('')
SURFACE()
);
#3977=(
BOUNDED_SURFACE()
B_SPLINE_SURFACE(1,2,((#161580,#161581,#161582),(#161583,#161584,#161585)),
 .UNSPECIFIED.,.F.,.F.,.F.)
B_SPLINE_SURFACE_WITH_KNOTS((2,2),(3,3),(0.,0.289807040991564),(0.107982157956011,
0.125273655815328),.UNSPECIFIED.)
GEOMETRIC_REPRESENTATION_ITEM()
RATIONAL_B_SPLINE_SURFACE(((0.987470879370255,0.98761351460672,0.990694758798812),
(0.987470879370255,0.98761351460672,0.990694758798812)))
REPRESENTATION_ITEM('')
SURFACE()
);
#3978=(
BOUNDED_SURFACE()
B_SPLINE_SURFACE(1,2,((#161597,#161598,#161599,#161600,#161601),(#161602,
#161603,#161604,#161605,#161606)),.UNSPECIFIED.,.F.,.F.,.F.)
B_SPLINE_SURFACE_WITH_KNOTS((2,2),(3,2,3),(0.,0.289942149041009),(0.607879027750092,
0.625170525609408,0.625431590463695),.UNSPECIFIED.)
GEOMETRIC_REPRESENTATION_ITEM()
RATIONAL_B_SPLINE_SURFACE(((0.987469282487682,0.987594391229382,0.990658108926709,
0.990658108926709,0.990658108926709),(0.987469282487682,0.987594391229382,
0.990658108926709,0.990658108926709,0.990658108926709)))
REPRESENTATION_ITEM('')
SURFACE()
);
#3979=(
BOUNDED_SURFACE()
B_SPLINE_SURFACE(1,2,((#161608,#161609,#161610),(#161611,#161612,#161613)),
 .UNSPECIFIED.,.F.,.F.,.F.)
B_SPLINE_SURFACE_WITH_KNOTS((2,2),(3,3),(0.,0.289807040991559),(0.107982157956011,
0.125273655815328),.UNSPECIFIED.)
GEOMETRIC_REPRESENTATION_ITEM()
RATIONAL_B_SPLINE_SURFACE(((0.987470879370255,0.98761351460672,0.990694758798812),
(0.987470879370255,0.98761351460672,0.990694758798812)))
REPRESENTATION_ITEM('')
SURFACE()
);
#3980=(
BOUNDED_SURFACE()
B_SPLINE_SURFACE(1,2,((#161631,#161632,#161633,#161634,#161635),(#161636,
#161637,#161638,#161639,#161640)),.UNSPECIFIED.,.F.,.F.,.F.)
B_SPLINE_SURFACE_WITH_KNOTS((2,2),(3,2,3),(0.,0.290280981345223),(0.607879027750092,
0.625170525609409,0.625770422767914),.UNSPECIFIED.)
GEOMETRIC_REPRESENTATION_ITEM()
RATIONAL_B_SPLINE_SURFACE(((0.987469282487682,0.987594391229382,0.990658108926709,
0.990658108926709,0.990658108926709),(0.987469282487682,0.987594391229382,
0.990658108926709,0.990658108926709,0.990658108926709)))
REPRESENTATION_ITEM('')
SURFACE()
);
#3981=(
BOUNDED_SURFACE()
B_SPLINE_SURFACE(1,2,((#161647,#161648,#161649),(#161650,#161651,#161652)),
 .UNSPECIFIED.,.F.,.F.,.F.)
B_SPLINE_SURFACE_WITH_KNOTS((2,2),(3,3),(0.,0.289807040991563),(0.107982157956011,
0.125273655815328),.UNSPECIFIED.)
GEOMETRIC_REPRESENTATION_ITEM()
RATIONAL_B_SPLINE_SURFACE(((0.987470879370255,0.987613514606721,0.990694758798812),
(0.987470879370255,0.987613514606721,0.990694758798812)))
REPRESENTATION_ITEM('')
SURFACE()
);
#3982=(
BOUNDED_SURFACE()
B_SPLINE_SURFACE(1,2,((#161670,#161671,#161672,#161673,#161674),(#161675,
#161676,#161677,#161678,#161679)),.UNSPECIFIED.,.F.,.F.,.F.)
B_SPLINE_SURFACE_WITH_KNOTS((2,2),(3,2,3),(0.,0.290280981333581),(0.607879027750092,
0.625170525609408,0.625770422756274),.UNSPECIFIED.)
GEOMETRIC_REPRESENTATION_ITEM()
RATIONAL_B_SPLINE_SURFACE(((0.987469282487682,0.987594391229382,0.990658108926709,
0.990658108926709,0.990658108926709),(0.987469282487682,0.987594391229382,
0.990658108926709,0.990658108926709,0.990658108926709)))
REPRESENTATION_ITEM('')
SURFACE()
);
#3983=(
BOUNDED_SURFACE()
B_SPLINE_SURFACE(1,2,((#161686,#161687,#161688),(#161689,#161690,#161691)),
 .UNSPECIFIED.,.F.,.F.,.F.)
B_SPLINE_SURFACE_WITH_KNOTS((2,2),(3,3),(0.,0.28980704099156),(0.107982157956011,
0.125273655815328),.UNSPECIFIED.)
GEOMETRIC_REPRESENTATION_ITEM()
RATIONAL_B_SPLINE_SURFACE(((0.987470879370255,0.98761351460672,0.990694758798812),
(0.987470879370256,0.987613514606721,0.990694758798812)))
REPRESENTATION_ITEM('')
SURFACE()
);
#3984=(
BOUNDED_SURFACE()
B_SPLINE_SURFACE(1,2,((#161709,#161710,#161711,#161712,#161713),(#161714,
#161715,#161716,#161717,#161718)),.UNSPECIFIED.,.F.,.F.,.F.)
B_SPLINE_SURFACE_WITH_KNOTS((2,2),(3,2,3),(0.,0.290280981337563),(0.607879027750092,
0.625170525609408,0.625770422760259),.UNSPECIFIED.)
GEOMETRIC_REPRESENTATION_ITEM()
RATIONAL_B_SPLINE_SURFACE(((0.987469282487682,0.987594391229382,0.990658108926709,
0.990658108926709,0.990658108926709),(0.987469282487682,0.987594391229382,
0.990658108926709,0.990658108926709,0.990658108926709)))
REPRESENTATION_ITEM('')
SURFACE()
);
#3985=(
BOUNDED_SURFACE()
B_SPLINE_SURFACE(1,2,((#161725,#161726,#161727),(#161728,#161729,#161730)),
 .UNSPECIFIED.,.F.,.F.,.F.)
B_SPLINE_SURFACE_WITH_KNOTS((2,2),(3,3),(0.,0.289807040991559),(0.107982157956011,
0.125273655815328),.UNSPECIFIED.)
GEOMETRIC_REPRESENTATION_ITEM()
RATIONAL_B_SPLINE_SURFACE(((0.987470879370255,0.98761351460672,0.990694758798812),
(0.987470879370255,0.98761351460672,0.990694758798812)))
REPRESENTATION_ITEM('')
SURFACE()
);
#3986=(
BOUNDED_SURFACE()
B_SPLINE_SURFACE(1,2,((#161748,#161749,#161750,#161751,#161752),(#161753,
#161754,#161755,#161756,#161757)),.UNSPECIFIED.,.F.,.F.,.F.)
B_SPLINE_SURFACE_WITH_KNOTS((2,2),(3,2,3),(0.,0.290280981340732),(0.607879027750092,
0.625170525609409,0.62577042276343),.UNSPECIFIED.)
GEOMETRIC_REPRESENTATION_ITEM()
RATIONAL_B_SPLINE_SURFACE(((0.987469282487682,0.987594391229382,0.990658108926709,
0.990658108926709,0.990658108926709),(0.987469282487682,0.987594391229382,
0.990658108926709,0.990658108926709,0.990658108926709)))
REPRESENTATION_ITEM('')
SURFACE()
);
#3987=(
BOUNDED_SURFACE()
B_SPLINE_SURFACE(1,2,((#161764,#161765,#161766),(#161767,#161768,#161769)),
 .UNSPECIFIED.,.F.,.F.,.F.)
B_SPLINE_SURFACE_WITH_KNOTS((2,2),(3,3),(0.,0.289807040991564),(0.107982157956011,
0.125273655815328),.UNSPECIFIED.)
GEOMETRIC_REPRESENTATION_ITEM()
RATIONAL_B_SPLINE_SURFACE(((0.987470879370255,0.98761351460672,0.990694758798812),
(0.987470879370255,0.98761351460672,0.990694758798812)))
REPRESENTATION_ITEM('')
SURFACE()
);
#3988=(
BOUNDED_SURFACE()
B_SPLINE_SURFACE(1,2,((#161787,#161788,#161789,#161790,#161791),(#161792,
#161793,#161794,#161795,#161796)),.UNSPECIFIED.,.F.,.F.,.F.)
B_SPLINE_SURFACE_WITH_KNOTS((2,2),(3,2,3),(0.,0.290280981343082),(0.607879027750091,
0.625170525609408,0.625770422765774),.UNSPECIFIED.)
GEOMETRIC_REPRESENTATION_ITEM()
RATIONAL_B_SPLINE_SURFACE(((0.987469282487682,0.987594391229382,0.990658108926709,
0.990658108926709,0.990658108926709),(0.987469282487682,0.987594391229382,
0.990658108926709,0.990658108926709,0.990658108926709)))
REPRESENTATION_ITEM('')
SURFACE()
);
#3989=(
BOUNDED_SURFACE()
B_SPLINE_SURFACE(1,2,((#161803,#161804,#161805),(#161806,#161807,#161808)),
 .UNSPECIFIED.,.F.,.F.,.F.)
B_SPLINE_SURFACE_WITH_KNOTS((2,2),(3,3),(0.,0.289807040991561),(0.107982157956011,
0.125273655815328),.UNSPECIFIED.)
GEOMETRIC_REPRESENTATION_ITEM()
RATIONAL_B_SPLINE_SURFACE(((0.987470879370255,0.98761351460672,0.990694758798812),
(0.987470879370256,0.987613514606721,0.990694758798812)))
REPRESENTATION_ITEM('')
SURFACE()
);
#3990=(
BOUNDED_SURFACE()
B_SPLINE_SURFACE(1,2,((#161826,#161827,#161828,#161829,#161830),(#161831,
#161832,#161833,#161834,#161835)),.UNSPECIFIED.,.F.,.F.,.F.)
B_SPLINE_SURFACE_WITH_KNOTS((2,2),(3,2,3),(0.,0.290280981344683),(0.607879027750092,
0.625170525609408,0.625770422767375),.UNSPECIFIED.)
GEOMETRIC_REPRESENTATION_ITEM()
RATIONAL_B_SPLINE_SURFACE(((0.987469282487682,0.987594391229382,0.990658108926709,
0.990658108926709,0.990658108926709),(0.987469282487682,0.987594391229382,
0.990658108926709,0.990658108926709,0.990658108926709)))
REPRESENTATION_ITEM('')
SURFACE()
);
#3991=(
BOUNDED_SURFACE()
B_SPLINE_SURFACE(1,2,((#161842,#161843,#161844),(#161845,#161846,#161847)),
 .UNSPECIFIED.,.F.,.F.,.F.)
B_SPLINE_SURFACE_WITH_KNOTS((2,2),(3,3),(0.,0.289807040991559),(0.107982157956011,
0.125273655815328),.UNSPECIFIED.)
GEOMETRIC_REPRESENTATION_ITEM()
RATIONAL_B_SPLINE_SURFACE(((0.987470879370255,0.98761351460672,0.990694758798812),
(0.987470879370255,0.98761351460672,0.990694758798812)))
REPRESENTATION_ITEM('')
SURFACE()
);
#3992=(
BOUNDED_SURFACE()
B_SPLINE_SURFACE(1,2,((#161865,#161866,#161867,#161868,#161869),(#161870,
#161871,#161872,#161873,#161874)),.UNSPECIFIED.,.F.,.F.,.F.)
B_SPLINE_SURFACE_WITH_KNOTS((2,2),(3,2,3),(0.,0.290280981333494),(0.607879027750092,
0.625170525609409,0.625770422756186),.UNSPECIFIED.)
GEOMETRIC_REPRESENTATION_ITEM()
RATIONAL_B_SPLINE_SURFACE(((0.987469282487682,0.987594391229382,0.990658108926709,
0.990658108926709,0.990658108926709),(0.987469282487682,0.987594391229382,
0.990658108926709,0.990658108926709,0.990658108926709)))
REPRESENTATION_ITEM('')
SURFACE()
);
#3993=(
BOUNDED_SURFACE()
B_SPLINE_SURFACE(1,2,((#161881,#161882,#161883),(#161884,#161885,#161886)),
 .UNSPECIFIED.,.F.,.F.,.F.)
B_SPLINE_SURFACE_WITH_KNOTS((2,2),(3,3),(0.,0.289807040991563),(0.107982157956011,
0.125273655815328),.UNSPECIFIED.)
GEOMETRIC_REPRESENTATION_ITEM()
RATIONAL_B_SPLINE_SURFACE(((0.987470879370255,0.98761351460672,0.990694758798812),
(0.987470879370255,0.98761351460672,0.990694758798812)))
REPRESENTATION_ITEM('')
SURFACE()
);
#3994=(
BOUNDED_SURFACE()
B_SPLINE_SURFACE(1,2,((#161904,#161905,#161906,#161907,#161908),(#161909,
#161910,#161911,#161912,#161913)),.UNSPECIFIED.,.F.,.F.,.F.)
B_SPLINE_SURFACE_WITH_KNOTS((2,2),(3,2,3),(0.,0.290280981335216),(0.607879027750091,
0.625170525609408,0.625770422757911),.UNSPECIFIED.)
GEOMETRIC_REPRESENTATION_ITEM()
RATIONAL_B_SPLINE_SURFACE(((0.987469282487682,0.987594391229382,0.990658108926709,
0.990658108926709,0.990658108926709),(0.987469282487682,0.987594391229382,
0.990658108926709,0.990658108926709,0.990658108926709)))
REPRESENTATION_ITEM('')
SURFACE()
);
#3995=(
BOUNDED_SURFACE()
B_SPLINE_SURFACE(1,2,((#161920,#161921,#161922),(#161923,#161924,#161925)),
 .UNSPECIFIED.,.F.,.F.,.F.)
B_SPLINE_SURFACE_WITH_KNOTS((2,2),(3,3),(0.,0.289807040991561),(0.107982157956011,
0.125273655815328),.UNSPECIFIED.)
GEOMETRIC_REPRESENTATION_ITEM()
RATIONAL_B_SPLINE_SURFACE(((0.987470879370255,0.98761351460672,0.990694758798812),
(0.987470879370255,0.98761351460672,0.990694758798812)))
REPRESENTATION_ITEM('')
SURFACE()
);
#3996=(
BOUNDED_SURFACE()
B_SPLINE_SURFACE(1,2,((#161943,#161944,#161945,#161946,#161947),(#161948,
#161949,#161950,#161951,#161952)),.UNSPECIFIED.,.F.,.F.,.F.)
B_SPLINE_SURFACE_WITH_KNOTS((2,2),(3,2,3),(0.,0.290280981343155),(0.607879027750092,
0.625170525609409,0.625770422765852),.UNSPECIFIED.)
GEOMETRIC_REPRESENTATION_ITEM()
RATIONAL_B_SPLINE_SURFACE(((0.987469282487682,0.987594391229382,0.990658108926709,
0.990658108926709,0.990658108926709),(0.987469282487682,0.987594391229382,
0.990658108926709,0.990658108926709,0.990658108926709)))
REPRESENTATION_ITEM('')
SURFACE()
);
#3997=(
BOUNDED_SURFACE()
B_SPLINE_SURFACE(1,2,((#161959,#161960,#161961),(#161962,#161963,#161964)),
 .UNSPECIFIED.,.F.,.F.,.F.)
B_SPLINE_SURFACE_WITH_KNOTS((2,2),(3,3),(0.,0.289807040991557),(0.107982157956011,
0.125273655815328),.UNSPECIFIED.)
GEOMETRIC_REPRESENTATION_ITEM()
RATIONAL_B_SPLINE_SURFACE(((0.987470879370255,0.98761351460672,0.990694758798812),
(0.987470879370255,0.98761351460672,0.990694758798812)))
REPRESENTATION_ITEM('')
SURFACE()
);
#3998=(
BOUNDED_SURFACE()
B_SPLINE_SURFACE(1,2,((#161982,#161983,#161984,#161985,#161986),(#161987,
#161988,#161989,#161990,#161991)),.UNSPECIFIED.,.F.,.F.,.F.)
B_SPLINE_SURFACE_WITH_KNOTS((2,2),(3,2,3),(0.,0.290280981344033),(0.607879027750092,
0.625170525609408,0.625770422766729),.UNSPECIFIED.)
GEOMETRIC_REPRESENTATION_ITEM()
RATIONAL_B_SPLINE_SURFACE(((0.987469282487682,0.987594391229382,0.990658108926709,
0.990658108926709,0.990658108926709),(0.987469282487682,0.987594391229382,
0.990658108926709,0.990658108926709,0.990658108926709)))
REPRESENTATION_ITEM('')
SURFACE()
);
#3999=(
BOUNDED_SURFACE()
B_SPLINE_SURFACE(1,2,((#161998,#161999,#162000),(#162001,#162002,#162003)),
 .UNSPECIFIED.,.F.,.F.,.F.)
B_SPLINE_SURFACE_WITH_KNOTS((2,2),(3,3),(0.,0.28980704099156),(0.107982157956006,
0.125273655815328),.UNSPECIFIED.)
GEOMETRIC_REPRESENTATION_ITEM()
RATIONAL_B_SPLINE_SURFACE(((0.987470879370255,0.98761351460672,0.990694758798812),
(0.987470879370255,0.98761351460672,0.990694758798812)))
REPRESENTATION_ITEM('')
SURFACE()
);
#4000=(
BOUNDED_SURFACE()
B_SPLINE_SURFACE(1,2,((#162021,#162022,#162023,#162024,#162025),(#162026,
#162027,#162028,#162029,#162030)),.UNSPECIFIED.,.F.,.F.,.F.)
B_SPLINE_SURFACE_WITH_KNOTS((2,2),(3,2,3),(0.,0.290280981330619),(0.607879027750092,
0.625170525609407,0.625770422753314),.UNSPECIFIED.)
GEOMETRIC_REPRESENTATION_ITEM()
RATIONAL_B_SPLINE_SURFACE(((0.987469282487682,0.987594391229382,0.990658108926708,
0.990658108926708,0.990658108926708),(0.987469282487682,0.987594391229382,
0.990658108926708,0.990658108926708,0.990658108926708)))
REPRESENTATION_ITEM('')
SURFACE()
);
#4001=(
BOUNDED_SURFACE()
B_SPLINE_SURFACE(1,2,((#162037,#162038,#162039),(#162040,#162041,#162042)),
 .UNSPECIFIED.,.F.,.F.,.F.)
B_SPLINE_SURFACE_WITH_KNOTS((2,2),(3,3),(0.,0.289807040991596),(0.107982157956012,
0.125273655815329),.UNSPECIFIED.)
GEOMETRIC_REPRESENTATION_ITEM()
RATIONAL_B_SPLINE_SURFACE(((0.987470879370256,0.987613514606721,0.990694758798813),
(0.987470879370256,0.987613514606721,0.990694758798813)))
REPRESENTATION_ITEM('')
SURFACE()
);
#4002=(
BOUNDED_SURFACE()
B_SPLINE_SURFACE(1,2,((#162060,#162061,#162062,#162063,#162064),(#162065,
#162066,#162067,#162068,#162069)),.UNSPECIFIED.,.F.,.F.,.F.)
B_SPLINE_SURFACE_WITH_KNOTS((2,2),(3,2,3),(0.,0.290280981345742),(0.607879027750091,
0.625170525609407,0.625770422768438),.UNSPECIFIED.)
GEOMETRIC_REPRESENTATION_ITEM()
RATIONAL_B_SPLINE_SURFACE(((0.987469282487682,0.987594391229382,0.990658108926708,
0.990658108926708,0.990658108926708),(0.987469282487682,0.987594391229382,
0.990658108926708,0.990658108926708,0.990658108926708)))
REPRESENTATION_ITEM('')
SURFACE()
);
#4003=(
BOUNDED_SURFACE()
B_SPLINE_SURFACE(1,2,((#162076,#162077,#162078),(#162079,#162080,#162081)),
 .UNSPECIFIED.,.F.,.F.,.F.)
B_SPLINE_SURFACE_WITH_KNOTS((2,2),(3,3),(0.,0.289807040991564),(0.107982157956012,
0.125273655815329),.UNSPECIFIED.)
GEOMETRIC_REPRESENTATION_ITEM()
RATIONAL_B_SPLINE_SURFACE(((0.987470879370256,0.987613514606721,0.990694758798813),
(0.987470879370255,0.987613514606721,0.990694758798813)))
REPRESENTATION_ITEM('')
SURFACE()
);
#4004=(
BOUNDED_SURFACE()
B_SPLINE_SURFACE(1,2,((#162099,#162100,#162101,#162102,#162103),(#162104,
#162105,#162106,#162107,#162108)),.UNSPECIFIED.,.F.,.F.,.F.)
B_SPLINE_SURFACE_WITH_KNOTS((2,2),(3,2,3),(0.,0.290280981329602),(0.607879027750091,
0.625170525609407,0.625770422752291),.UNSPECIFIED.)
GEOMETRIC_REPRESENTATION_ITEM()
RATIONAL_B_SPLINE_SURFACE(((0.987469282487682,0.987594391229382,0.990658108926708,
0.990658108926708,0.990658108926708),(0.987469282487682,0.987594391229382,
0.990658108926708,0.990658108926708,0.990658108926708)))
REPRESENTATION_ITEM('')
SURFACE()
);
#4005=(
BOUNDED_SURFACE()
B_SPLINE_SURFACE(1,2,((#162115,#162116,#162117),(#162118,#162119,#162120)),
 .UNSPECIFIED.,.F.,.F.,.F.)
B_SPLINE_SURFACE_WITH_KNOTS((2,2),(3,3),(0.,0.289807040991561),(0.107982157956012,
0.125273655815329),.UNSPECIFIED.)
GEOMETRIC_REPRESENTATION_ITEM()
RATIONAL_B_SPLINE_SURFACE(((0.987470879370255,0.987613514606721,0.990694758798813),
(0.987470879370255,0.987613514606721,0.990694758798813)))
REPRESENTATION_ITEM('')
SURFACE()
);
#4006=(
BOUNDED_SURFACE()
B_SPLINE_SURFACE(1,2,((#162138,#162139,#162140,#162141,#162142),(#162143,
#162144,#162145,#162146,#162147)),.UNSPECIFIED.,.F.,.F.,.F.)
B_SPLINE_SURFACE_WITH_KNOTS((2,2),(3,2,3),(0.,0.290280981329769),(0.607879027750091,
0.625170525609408,0.625770422752459),.UNSPECIFIED.)
GEOMETRIC_REPRESENTATION_ITEM()
RATIONAL_B_SPLINE_SURFACE(((0.987469282487682,0.987594391229382,0.990658108926708,
0.990658108926708,0.990658108926708),(0.987469282487682,0.987594391229382,
0.990658108926708,0.990658108926708,0.990658108926708)))
REPRESENTATION_ITEM('')
SURFACE()
);
#4007=(
BOUNDED_SURFACE()
B_SPLINE_SURFACE(1,2,((#162154,#162155,#162156),(#162157,#162158,#162159)),
 .UNSPECIFIED.,.F.,.F.,.F.)
B_SPLINE_SURFACE_WITH_KNOTS((2,2),(3,3),(0.,0.289807040991696),(0.107982157956012,
0.125273655815329),.UNSPECIFIED.)
GEOMETRIC_REPRESENTATION_ITEM()
RATIONAL_B_SPLINE_SURFACE(((0.987470879370256,0.987613514606721,0.990694758798813),
(0.987470879370255,0.987613514606721,0.990694758798813)))
REPRESENTATION_ITEM('')
SURFACE()
);
#4008=(
BOUNDED_SURFACE()
B_SPLINE_SURFACE(1,2,((#162177,#162178,#162179,#162180,#162181),(#162182,
#162183,#162184,#162185,#162186)),.UNSPECIFIED.,.F.,.F.,.F.)
B_SPLINE_SURFACE_WITH_KNOTS((2,2),(3,2,3),(0.,0.290280981331014),(0.607879027750091,
0.625170525609407,0.625770422753705),.UNSPECIFIED.)
GEOMETRIC_REPRESENTATION_ITEM()
RATIONAL_B_SPLINE_SURFACE(((0.987469282487682,0.987594391229382,0.990658108926708,
0.990658108926708,0.990658108926708),(0.987469282487682,0.987594391229382,
0.990658108926708,0.990658108926708,0.990658108926708)))
REPRESENTATION_ITEM('')
SURFACE()
);
#4009=(
BOUNDED_SURFACE()
B_SPLINE_SURFACE(1,2,((#162193,#162194,#162195),(#162196,#162197,#162198)),
 .UNSPECIFIED.,.F.,.F.,.F.)
B_SPLINE_SURFACE_WITH_KNOTS((2,2),(3,3),(0.,0.289807040991704),(0.107982157956012,
0.125273655815329),.UNSPECIFIED.)
GEOMETRIC_REPRESENTATION_ITEM()
RATIONAL_B_SPLINE_SURFACE(((0.987470879370256,0.987613514606721,0.990694758798813),
(0.987470879370256,0.987613514606721,0.990694758798813)))
REPRESENTATION_ITEM('')
SURFACE()
);
#4010=(
BOUNDED_SURFACE()
B_SPLINE_SURFACE(1,2,((#162216,#162217,#162218,#162219,#162220),(#162221,
#162222,#162223,#162224,#162225)),.UNSPECIFIED.,.F.,.F.,.F.)
B_SPLINE_SURFACE_WITH_KNOTS((2,2),(3,2,3),(0.,0.290280981334896),(0.607879027750091,
0.625170525609407,0.625770422757586),.UNSPECIFIED.)
GEOMETRIC_REPRESENTATION_ITEM()
RATIONAL_B_SPLINE_SURFACE(((0.987469282487682,0.987594391229382,0.990658108926708,
0.990658108926708,0.990658108926708),(0.987469282487682,0.987594391229382,
0.990658108926709,0.990658108926709,0.990658108926709)))
REPRESENTATION_ITEM('')
SURFACE()
);
#4011=(
BOUNDED_SURFACE()
B_SPLINE_SURFACE(1,2,((#162232,#162233,#162234),(#162235,#162236,#162237)),
 .UNSPECIFIED.,.F.,.F.,.F.)
B_SPLINE_SURFACE_WITH_KNOTS((2,2),(3,3),(0.,0.289807040991712),(0.107982157956012,
0.125273655815329),.UNSPECIFIED.)
GEOMETRIC_REPRESENTATION_ITEM()
RATIONAL_B_SPLINE_SURFACE(((0.987470879370256,0.987613514606721,0.990694758798813),
(0.987470879370256,0.987613514606721,0.990694758798813)))
REPRESENTATION_ITEM('')
SURFACE()
);
#4012=(
BOUNDED_SURFACE()
B_SPLINE_SURFACE(1,2,((#162255,#162256,#162257,#162258,#162259),(#162260,
#162261,#162262,#162263,#162264)),.UNSPECIFIED.,.F.,.F.,.F.)
B_SPLINE_SURFACE_WITH_KNOTS((2,2),(3,2,3),(0.,0.290280981346236),(0.607879027750091,
0.625170525609407,0.62577042276893),.UNSPECIFIED.)
GEOMETRIC_REPRESENTATION_ITEM()
RATIONAL_B_SPLINE_SURFACE(((0.987469282487682,0.987594391229382,0.990658108926708,
0.990658108926708,0.990658108926708),(0.987469282487682,0.987594391229382,
0.990658108926708,0.990658108926708,0.990658108926708)))
REPRESENTATION_ITEM('')
SURFACE()
);
#4013=(
BOUNDED_SURFACE()
B_SPLINE_SURFACE(1,2,((#162271,#162272,#162273),(#162274,#162275,#162276)),
 .UNSPECIFIED.,.F.,.F.,.F.)
B_SPLINE_SURFACE_WITH_KNOTS((2,2),(3,3),(0.,0.289807040993084),(0.107982157956012,
0.125273655815329),.UNSPECIFIED.)
GEOMETRIC_REPRESENTATION_ITEM()
RATIONAL_B_SPLINE_SURFACE(((0.987470879370255,0.987613514606721,0.990694758798813),
(0.987470879370255,0.987613514606721,0.990694758798813)))
REPRESENTATION_ITEM('')
SURFACE()
);
#4014=(
BOUNDED_SURFACE()
B_SPLINE_SURFACE(1,2,((#162294,#162295,#162296,#162297,#162298),(#162299,
#162300,#162301,#162302,#162303)),.UNSPECIFIED.,.F.,.F.,.F.)
B_SPLINE_SURFACE_WITH_KNOTS((2,2),(3,2,3),(0.,0.290280981314508),(0.607879027750091,
0.625170525609407,0.625770422736998),.UNSPECIFIED.)
GEOMETRIC_REPRESENTATION_ITEM()
RATIONAL_B_SPLINE_SURFACE(((0.987469282487682,0.987594391229382,0.990658108926708,
0.990658108926708,0.990658108926708),(0.987469282487682,0.987594391229382,
0.990658108926708,0.990658108926708,0.990658108926708)))
REPRESENTATION_ITEM('')
SURFACE()
);
#4015=(
BOUNDED_SURFACE()
B_SPLINE_SURFACE(1,2,((#162310,#162311,#162312),(#162313,#162314,#162315)),
 .UNSPECIFIED.,.F.,.F.,.F.)
B_SPLINE_SURFACE_WITH_KNOTS((2,2),(3,3),(0.,0.289807040991928),(0.107982157956012,
0.125273655815329),.UNSPECIFIED.)
GEOMETRIC_REPRESENTATION_ITEM()
RATIONAL_B_SPLINE_SURFACE(((0.987470879370256,0.987613514606721,0.990694758798813),
(0.987470879370256,0.987613514606721,0.990694758798813)))
REPRESENTATION_ITEM('')
SURFACE()
);
#4016=(
BOUNDED_SURFACE()
B_SPLINE_SURFACE(1,2,((#162333,#162334,#162335,#162336,#162337),(#162338,
#162339,#162340,#162341,#162342)),.UNSPECIFIED.,.F.,.F.,.F.)
B_SPLINE_SURFACE_WITH_KNOTS((2,2),(3,2,3),(0.,0.290280981329288),(0.607879027750091,
0.625170525609407,0.625770422751973),.UNSPECIFIED.)
GEOMETRIC_REPRESENTATION_ITEM()
RATIONAL_B_SPLINE_SURFACE(((0.987469282487682,0.987594391229382,0.990658108926708,
0.990658108926708,0.990658108926708),(0.987469282487682,0.987594391229382,
0.990658108926709,0.990658108926709,0.990658108926709)))
REPRESENTATION_ITEM('')
SURFACE()
);
#4017=(
BOUNDED_SURFACE()
B_SPLINE_SURFACE(1,2,((#162349,#162350,#162351),(#162352,#162353,#162354)),
 .UNSPECIFIED.,.F.,.F.,.F.)
B_SPLINE_SURFACE_WITH_KNOTS((2,2),(3,3),(0.,0.289807040991557),(0.107982157956012,
0.125273655815329),.UNSPECIFIED.)
GEOMETRIC_REPRESENTATION_ITEM()
RATIONAL_B_SPLINE_SURFACE(((0.987470879370255,0.987613514606721,0.990694758798813),
(0.987470879370255,0.987613514606721,0.990694758798813)))
REPRESENTATION_ITEM('')
SURFACE()
);
#4018=(
BOUNDED_SURFACE()
B_SPLINE_SURFACE(1,2,((#162372,#162373,#162374,#162375,#162376),(#162377,
#162378,#162379,#162380,#162381)),.UNSPECIFIED.,.F.,.F.,.F.)
B_SPLINE_SURFACE_WITH_KNOTS((2,2),(3,2,3),(0.,0.290280981324863),(0.607879027750091,
0.625170525609408,0.625770422747553),.UNSPECIFIED.)
GEOMETRIC_REPRESENTATION_ITEM()
RATIONAL_B_SPLINE_SURFACE(((0.987469282487682,0.987594391229382,0.990658108926708,
0.990658108926708,0.990658108926708),(0.987469282487682,0.987594391229382,
0.990658108926708,0.990658108926708,0.990658108926708)))
REPRESENTATION_ITEM('')
SURFACE()
);
#4019=(
BOUNDED_SURFACE()
B_SPLINE_SURFACE(1,2,((#162388,#162389,#162390),(#162391,#162392,#162393)),
 .UNSPECIFIED.,.F.,.F.,.F.)
B_SPLINE_SURFACE_WITH_KNOTS((2,2),(3,3),(0.,0.289807040991562),(0.107982157956012,
0.125273655815329),.UNSPECIFIED.)
GEOMETRIC_REPRESENTATION_ITEM()
RATIONAL_B_SPLINE_SURFACE(((0.987470879370256,0.987613514606721,0.990694758798813),
(0.987470879370255,0.987613514606721,0.990694758798813)))
REPRESENTATION_ITEM('')
SURFACE()
);
#4020=(
BOUNDED_SURFACE()
B_SPLINE_SURFACE(1,2,((#162411,#162412,#162413,#162414,#162415),(#162416,
#162417,#162418,#162419,#162420)),.UNSPECIFIED.,.F.,.F.,.F.)
B_SPLINE_SURFACE_WITH_KNOTS((2,2),(3,2,3),(0.,0.290280981331528),(0.607879027750091,
0.625170525609407,0.625770422754222),.UNSPECIFIED.)
GEOMETRIC_REPRESENTATION_ITEM()
RATIONAL_B_SPLINE_SURFACE(((0.987469282487682,0.987594391229382,0.990658108926708,
0.990658108926708,0.990658108926708),(0.987469282487682,0.987594391229382,
0.990658108926709,0.990658108926709,0.990658108926709)))
REPRESENTATION_ITEM('')
SURFACE()
);
#4021=(
BOUNDED_SURFACE()
B_SPLINE_SURFACE(1,2,((#162439,#162440,#162441),(#162442,#162443,#162444)),
 .UNSPECIFIED.,.F.,.F.,.F.)
B_SPLINE_SURFACE_WITH_KNOTS((2,2),(3,3),(0.,0.289807040991564),(0.107982157956012,
0.125273655815329),.UNSPECIFIED.)
GEOMETRIC_REPRESENTATION_ITEM()
RATIONAL_B_SPLINE_SURFACE(((0.987470879370255,0.987613514606721,0.990694758798813),
(0.987470879370255,0.987613514606721,0.990694758798813)))
REPRESENTATION_ITEM('')
SURFACE()
);
#4022=(
BOUNDED_SURFACE()
B_SPLINE_SURFACE(1,2,((#162447,#162448,#162449,#162450,#162451),(#162452,
#162453,#162454,#162455,#162456)),.UNSPECIFIED.,.F.,.F.,.F.)
B_SPLINE_SURFACE_WITH_KNOTS((2,2),(3,2,3),(0.71005925781061,1.),(0.0908085233856358,
0.107982157956013,0.108241816694656),.UNSPECIFIED.)
GEOMETRIC_REPRESENTATION_ITEM()
RATIONAL_B_SPLINE_SURFACE(((0.990086238235256,0.987329216372183,0.987470879370256,
0.987470879370256,0.987470879370256),(0.990086238235256,0.987329216372183,
0.987470879370256,0.987470879370256,0.987470879370256)))
REPRESENTATION_ITEM('')
SURFACE()
);
#4023=(
BOUNDED_SURFACE()
B_SPLINE_SURFACE(1,2,((#162460,#162461,#162462),(#162463,#162464,#162465)),
 .UNSPECIFIED.,.F.,.F.,.F.)
B_SPLINE_SURFACE_WITH_KNOTS((2,2),(3,3),(0.710192959008442,1.),(0.625170525609407,
0.642682999576235),.UNSPECIFIED.)
GEOMETRIC_REPRESENTATION_ITEM()
RATIONAL_B_SPLINE_SURFACE(((0.990658108926708,0.993760979299921,0.999878046252916),
(0.990658108926708,0.993760979299921,0.999878046252916)))
REPRESENTATION_ITEM('')
SURFACE()
);
#4024=(
BOUNDED_SURFACE()
B_SPLINE_SURFACE(1,2,((#162469,#162470,#162471,#162472,#162473),(#162474,
#162475,#162476,#162477,#162478)),.UNSPECIFIED.,.F.,.F.,.F.)
B_SPLINE_SURFACE_WITH_KNOTS((2,2),(3,2,3),(0.710059257949577,1.),(0.0908085233856358,
0.107982157956012,0.10824181686735),.UNSPECIFIED.)
GEOMETRIC_REPRESENTATION_ITEM()
RATIONAL_B_SPLINE_SURFACE(((0.990086238235256,0.987329216372183,0.987470879370255,
0.987470879370255,0.987470879370255),(0.990086238235256,0.987329216372183,
0.987470879370255,0.987470879370255,0.987470879370255)))
REPRESENTATION_ITEM('')
SURFACE()
);
#4025=(
BOUNDED_SURFACE()
B_SPLINE_SURFACE(1,2,((#162480,#162481,#162482),(#162483,#162484,#162485)),
 .UNSPECIFIED.,.F.,.F.,.F.)
B_SPLINE_SURFACE_WITH_KNOTS((2,2),(3,3),(0.710192959008438,1.),(0.625170525609407,
0.642682999576235),.UNSPECIFIED.)
GEOMETRIC_REPRESENTATION_ITEM()
RATIONAL_B_SPLINE_SURFACE(((0.990658108926708,0.993760979299921,0.999878046252916),
(0.990658108926708,0.993760979299921,0.999878046252916)))
REPRESENTATION_ITEM('')
SURFACE()
);
#4026=(
BOUNDED_SURFACE()
B_SPLINE_SURFACE(1,2,((#162489,#162490,#162491,#162492,#162493),(#162494,
#162495,#162496,#162497,#162498)),.UNSPECIFIED.,.F.,.F.,.F.)
B_SPLINE_SURFACE_WITH_KNOTS((2,2),(3,2,3),(0.710059257875638,1.),(0.0908085233856357,
0.107982157956012,0.108241816941263),.UNSPECIFIED.)
GEOMETRIC_REPRESENTATION_ITEM()
RATIONAL_B_SPLINE_SURFACE(((0.990086238235256,0.987329216372183,0.987470879370255,
0.987470879370255,0.987470879370255),(0.990086238235256,0.987329216372183,
0.987470879370255,0.987470879370255,0.987470879370255)))
REPRESENTATION_ITEM('')
SURFACE()
);
#4027=(
BOUNDED_SURFACE()
B_SPLINE_SURFACE(1,2,((#162500,#162501,#162502),(#162503,#162504,#162505)),
 .UNSPECIFIED.,.F.,.F.,.F.)
B_SPLINE_SURFACE_WITH_KNOTS((2,2),(3,3),(0.710192959008443,1.),(0.625170525609407,
0.642682999576235),.UNSPECIFIED.)
GEOMETRIC_REPRESENTATION_ITEM()
RATIONAL_B_SPLINE_SURFACE(((0.990658108926708,0.993760979299921,0.999878046252916),
(0.990658108926708,0.993760979299921,0.999878046252916)))
REPRESENTATION_ITEM('')
SURFACE()
);
#4028=(
BOUNDED_SURFACE()
B_SPLINE_SURFACE(1,2,((#162509,#162510,#162511,#162512,#162513),(#162514,
#162515,#162516,#162517,#162518)),.UNSPECIFIED.,.F.,.F.,.F.)
B_SPLINE_SURFACE_WITH_KNOTS((2,2),(3,2,3),(0.710059257951385,1.),(0.0908085233856357,
0.107982157956012,0.10824181686549),.UNSPECIFIED.)
GEOMETRIC_REPRESENTATION_ITEM()
RATIONAL_B_SPLINE_SURFACE(((0.990086238235256,0.987329216372183,0.987470879370255,
0.987470879370255,0.987470879370255),(0.990086238235256,0.987329216372183,
0.987470879370255,0.987470879370255,0.987470879370255)))
REPRESENTATION_ITEM('')
SURFACE()
);
#4029=(
BOUNDED_SURFACE()
B_SPLINE_SURFACE(1,2,((#162520,#162521,#162522),(#162523,#162524,#162525)),
 .UNSPECIFIED.,.F.,.F.,.F.)
B_SPLINE_SURFACE_WITH_KNOTS((2,2),(3,3),(0.710192959008438,1.),(0.625170525609407,
0.642682999576235),.UNSPECIFIED.)
GEOMETRIC_REPRESENTATION_ITEM()
RATIONAL_B_SPLINE_SURFACE(((0.990658108926708,0.993760979299921,0.999878046252916),
(0.990658108926708,0.993760979299921,0.999878046252916)))
REPRESENTATION_ITEM('')
SURFACE()
);
#4030=(
BOUNDED_SURFACE()
B_SPLINE_SURFACE(1,2,((#162529,#162530,#162531,#162532,#162533),(#162534,
#162535,#162536,#162537,#162538)),.UNSPECIFIED.,.F.,.F.,.F.)
B_SPLINE_SURFACE_WITH_KNOTS((2,2),(3,2,3),(0.71005925795596,1.),(0.0908085233856358,
0.107982157956011,0.108241816860967),.UNSPECIFIED.)
GEOMETRIC_REPRESENTATION_ITEM()
RATIONAL_B_SPLINE_SURFACE(((0.990086238235256,0.987329216372183,0.987470879370255,
0.987470879370255,0.987470879370255),(0.990086238235256,0.987329216372183,
0.987470879370255,0.987470879370255,0.987470879370255)))
REPRESENTATION_ITEM('')
SURFACE()
);
#4031=(
BOUNDED_SURFACE()
B_SPLINE_SURFACE(1,2,((#162540,#162541,#162542),(#162543,#162544,#162545)),
 .UNSPECIFIED.,.F.,.F.,.F.)
B_SPLINE_SURFACE_WITH_KNOTS((2,2),(3,3),(0.710192959008441,1.),(0.625170525609408,
0.642682999576236),.UNSPECIFIED.)
GEOMETRIC_REPRESENTATION_ITEM()
RATIONAL_B_SPLINE_SURFACE(((0.990658108926709,0.993760979299921,0.999878046252917),
(0.990658108926709,0.993760979299922,0.999878046252917)))
REPRESENTATION_ITEM('')
SURFACE()
);
#4032=(
BOUNDED_SURFACE()
B_SPLINE_SURFACE(1,2,((#162549,#162550,#162551,#162552,#162553),(#162554,
#162555,#162556,#162557,#162558)),.UNSPECIFIED.,.F.,.F.,.F.)
B_SPLINE_SURFACE_WITH_KNOTS((2,2),(3,2,3),(0.710059258013954,1.),(0.0908085233856347,
0.107982157956011,0.10824181680298),.UNSPECIFIED.)
GEOMETRIC_REPRESENTATION_ITEM()
RATIONAL_B_SPLINE_SURFACE(((0.990086238235256,0.987329216372183,0.987470879370256,
0.987470879370256,0.987470879370256),(0.990086238235256,0.987329216372183,
0.987470879370256,0.987470879370256,0.987470879370256)))
REPRESENTATION_ITEM('')
SURFACE()
);
#4033=(
BOUNDED_SURFACE()
B_SPLINE_SURFACE(1,2,((#162560,#162561,#162562),(#162563,#162564,#162565)),
 .UNSPECIFIED.,.F.,.F.,.F.)
B_SPLINE_SURFACE_WITH_KNOTS((2,2),(3,3),(0.710192959008439,1.),(0.625170525609408,
0.642682999576236),.UNSPECIFIED.)
GEOMETRIC_REPRESENTATION_ITEM()
RATIONAL_B_SPLINE_SURFACE(((0.990658108926709,0.993760979299921,0.999878046252917),
(0.990658108926709,0.993760979299921,0.999878046252917)))
REPRESENTATION_ITEM('')
SURFACE()
);
#4034=(
BOUNDED_SURFACE()
B_SPLINE_SURFACE(1,2,((#162569,#162570,#162571,#162572,#162573),(#162574,
#162575,#162576,#162577,#162578)),.UNSPECIFIED.,.F.,.F.,.F.)
B_SPLINE_SURFACE_WITH_KNOTS((2,2),(3,2,3),(0.710059257951645,1.),(0.0908085233856347,
0.107982157956011,0.108241816865274),.UNSPECIFIED.)
GEOMETRIC_REPRESENTATION_ITEM()
RATIONAL_B_SPLINE_SURFACE(((0.990086238235256,0.987329216372183,0.987470879370255,
0.987470879370255,0.987470879370255),(0.990086238235256,0.987329216372183,
0.987470879370255,0.987470879370255,0.987470879370255)))
REPRESENTATION_ITEM('')
SURFACE()
);
#4035=(
BOUNDED_SURFACE()
B_SPLINE_SURFACE(1,2,((#162580,#162581,#162582),(#162583,#162584,#162585)),
 .UNSPECIFIED.,.F.,.F.,.F.)
B_SPLINE_SURFACE_WITH_KNOTS((2,2),(3,3),(0.710192959008438,1.),(0.625170525609408,
0.642682999576236),.UNSPECIFIED.)
GEOMETRIC_REPRESENTATION_ITEM()
RATIONAL_B_SPLINE_SURFACE(((0.990658108926709,0.993760979299921,0.999878046252917),
(0.990658108926709,0.993760979299921,0.999878046252917)))
REPRESENTATION_ITEM('')
SURFACE()
);
#4036=(
BOUNDED_SURFACE()
B_SPLINE_SURFACE(1,2,((#162589,#162590,#162591,#162592,#162593),(#162594,
#162595,#162596,#162597,#162598)),.UNSPECIFIED.,.F.,.F.,.F.)
B_SPLINE_SURFACE_WITH_KNOTS((2,2),(3,2,3),(0.710059257776109,1.),(0.0908085233856348,
0.107982157956011,0.108241816729418),.UNSPECIFIED.)
GEOMETRIC_REPRESENTATION_ITEM()
RATIONAL_B_SPLINE_SURFACE(((0.990086238235256,0.987329216372183,0.987470879370255,
0.987470879370255,0.987470879370255),(0.990086238235256,0.987329216372183,
0.987470879370255,0.987470879370255,0.987470879370255)))
REPRESENTATION_ITEM('')
SURFACE()
);
#4037=(
BOUNDED_SURFACE()
B_SPLINE_SURFACE(1,2,((#162600,#162601,#162602),(#162603,#162604,#162605)),
 .UNSPECIFIED.,.F.,.F.,.F.)
B_SPLINE_SURFACE_WITH_KNOTS((2,2),(3,3),(0.710192959008441,1.),(0.625170525609408,
0.642682999576236),.UNSPECIFIED.)
GEOMETRIC_REPRESENTATION_ITEM()
RATIONAL_B_SPLINE_SURFACE(((0.990658108926709,0.993760979299921,0.999878046252917),
(0.990658108926709,0.993760979299921,0.999878046252917)))
REPRESENTATION_ITEM('')
SURFACE()
);
#4038=(
BOUNDED_SURFACE()
B_SPLINE_SURFACE(1,2,((#162609,#162610,#162611,#162612,#162613),(#162614,
#162615,#162616,#162617,#162618)),.UNSPECIFIED.,.F.,.F.,.F.)
B_SPLINE_SURFACE_WITH_KNOTS((2,2),(3,2,3),(0.710059257948746,1.),(0.0908085233856347,
0.107982157956011,0.108241816868152),.UNSPECIFIED.)
GEOMETRIC_REPRESENTATION_ITEM()
RATIONAL_B_SPLINE_SURFACE(((0.990086238235257,0.987329216372183,0.987470879370256,
0.987470879370256,0.987470879370256),(0.990086238235257,0.987329216372183,
0.987470879370256,0.987470879370256,0.987470879370256)))
REPRESENTATION_ITEM('')
SURFACE()
);
#4039=(
BOUNDED_SURFACE()
B_SPLINE_SURFACE(1,2,((#162620,#162621,#162622),(#162623,#162624,#162625)),
 .UNSPECIFIED.,.F.,.F.,.F.)
B_SPLINE_SURFACE_WITH_KNOTS((2,2),(3,3),(0.71019295900844,1.),(0.625170525609408,
0.642682999576236),.UNSPECIFIED.)
GEOMETRIC_REPRESENTATION_ITEM()
RATIONAL_B_SPLINE_SURFACE(((0.990658108926709,0.993760979299921,0.999878046252917),
(0.990658108926709,0.993760979299921,0.999878046252917)))
REPRESENTATION_ITEM('')
SURFACE()
);
#4040=(
BOUNDED_SURFACE()
B_SPLINE_SURFACE(1,2,((#162629,#162630,#162631,#162632,#162633),(#162634,
#162635,#162636,#162637,#162638)),.UNSPECIFIED.,.F.,.F.,.F.)
B_SPLINE_SURFACE_WITH_KNOTS((2,2),(3,2,3),(0.710059257948785,1.),(0.0908085233856347,
0.107982157956011,0.108241816868058),.UNSPECIFIED.)
GEOMETRIC_REPRESENTATION_ITEM()
RATIONAL_B_SPLINE_SURFACE(((0.990086238235256,0.987329216372183,0.987470879370255,
0.987470879370255,0.987470879370255),(0.990086238235256,0.987329216372183,
0.987470879370255,0.987470879370255,0.987470879370255)))
REPRESENTATION_ITEM('')
SURFACE()
);
#4041=(
BOUNDED_SURFACE()
B_SPLINE_SURFACE(1,2,((#162640,#162641,#162642),(#162643,#162644,#162645)),
 .UNSPECIFIED.,.F.,.F.,.F.)
B_SPLINE_SURFACE_WITH_KNOTS((2,2),(3,3),(0.710192959008442,1.),(0.625170525609408,
0.642682999576236),.UNSPECIFIED.)
GEOMETRIC_REPRESENTATION_ITEM()
RATIONAL_B_SPLINE_SURFACE(((0.990658108926709,0.993760979299921,0.999878046252917),
(0.990658108926709,0.993760979299921,0.999878046252917)))
REPRESENTATION_ITEM('')
SURFACE()
);
#4042=(
BOUNDED_SURFACE()
B_SPLINE_SURFACE(1,2,((#162649,#162650,#162651,#162652,#162653),(#162654,
#162655,#162656,#162657,#162658)),.UNSPECIFIED.,.F.,.F.,.F.)
B_SPLINE_SURFACE_WITH_KNOTS((2,2),(3,2,3),(0.710059257952301,1.),(0.0908085233856347,
0.107982157956011,0.108241816864594),.UNSPECIFIED.)
GEOMETRIC_REPRESENTATION_ITEM()
RATIONAL_B_SPLINE_SURFACE(((0.990086238235257,0.987329216372183,0.987470879370255,
0.987470879370255,0.987470879370255),(0.990086238235257,0.987329216372183,
0.987470879370255,0.987470879370255,0.987470879370255)))
REPRESENTATION_ITEM('')
SURFACE()
);
#4043=(
BOUNDED_SURFACE()
B_SPLINE_SURFACE(1,2,((#162660,#162661,#162662),(#162663,#162664,#162665)),
 .UNSPECIFIED.,.F.,.F.,.F.)
B_SPLINE_SURFACE_WITH_KNOTS((2,2),(3,3),(0.710192959008441,1.),(0.625170525609408,
0.642682999576236),.UNSPECIFIED.)
GEOMETRIC_REPRESENTATION_ITEM()
RATIONAL_B_SPLINE_SURFACE(((0.990658108926709,0.993760979299921,0.999878046252917),
(0.990658108926709,0.993760979299921,0.999878046252917)))
REPRESENTATION_ITEM('')
SURFACE()
);
#4044=(
BOUNDED_SURFACE()
B_SPLINE_SURFACE(1,2,((#162669,#162670,#162671,#162672,#162673),(#162674,
#162675,#162676,#162677,#162678)),.UNSPECIFIED.,.F.,.F.,.F.)
B_SPLINE_SURFACE_WITH_KNOTS((2,2),(3,2,3),(0.710059257867479,1.),(0.0908085233856346,
0.107982157956011,0.108241816949409),.UNSPECIFIED.)
GEOMETRIC_REPRESENTATION_ITEM()
RATIONAL_B_SPLINE_SURFACE(((0.990086238235256,0.987329216372183,0.987470879370255,
0.987470879370255,0.987470879370255),(0.990086238235256,0.987329216372183,
0.987470879370255,0.987470879370255,0.987470879370255)))
REPRESENTATION_ITEM('')
SURFACE()
);
#4045=(
BOUNDED_SURFACE()
B_SPLINE_SURFACE(1,2,((#162680,#162681,#162682),(#162683,#162684,#162685)),
 .UNSPECIFIED.,.F.,.F.,.F.)
B_SPLINE_SURFACE_WITH_KNOTS((2,2),(3,3),(0.710192959008446,1.),(0.625170525609408,
0.642682999576237),.UNSPECIFIED.)
GEOMETRIC_REPRESENTATION_ITEM()
RATIONAL_B_SPLINE_SURFACE(((0.990658108926709,0.993760979299922,0.999878046252917),
(0.990658108926709,0.993760979299922,0.999878046252917)))
REPRESENTATION_ITEM('')
SURFACE()
);
#4046=(
BOUNDED_SURFACE()
B_SPLINE_SURFACE(1,2,((#162689,#162690,#162691,#162692,#162693),(#162694,
#162695,#162696,#162697,#162698)),.UNSPECIFIED.,.F.,.F.,.F.)
B_SPLINE_SURFACE_WITH_KNOTS((2,2),(3,2,3),(0.710059257964262,1.),(0.0908085233856348,
0.107982157956011,0.108241816852688),.UNSPECIFIED.)
GEOMETRIC_REPRESENTATION_ITEM()
RATIONAL_B_SPLINE_SURFACE(((0.990086238235256,0.987329216372183,0.987470879370255,
0.987470879370255,0.987470879370255),(0.990086238235256,0.987329216372183,
0.987470879370255,0.987470879370255,0.987470879370255)))
REPRESENTATION_ITEM('')
SURFACE()
);
#4047=(
BOUNDED_SURFACE()
B_SPLINE_SURFACE(1,2,((#162700,#162701,#162702),(#162703,#162704,#162705)),
 .UNSPECIFIED.,.F.,.F.,.F.)
B_SPLINE_SURFACE_WITH_KNOTS((2,2),(3,3),(0.710192959008443,1.),(0.625170525609408,
0.642682999576236),.UNSPECIFIED.)
GEOMETRIC_REPRESENTATION_ITEM()
RATIONAL_B_SPLINE_SURFACE(((0.990658108926709,0.993760979299921,0.999878046252917),
(0.990658108926709,0.993760979299921,0.999878046252917)))
REPRESENTATION_ITEM('')
SURFACE()
);
#4048=(
BOUNDED_SURFACE()
B_SPLINE_SURFACE(1,2,((#162709,#162710,#162711,#162712,#162713),(#162714,
#162715,#162716,#162717,#162718)),.UNSPECIFIED.,.F.,.F.,.F.)
B_SPLINE_SURFACE_WITH_KNOTS((2,2),(3,2,3),(0.710059257941329,1.),(0.0908085233856347,
0.107982157956011,0.108241816875574),.UNSPECIFIED.)
GEOMETRIC_REPRESENTATION_ITEM()
RATIONAL_B_SPLINE_SURFACE(((0.990086238235256,0.987329216372183,0.987470879370256,
0.987470879370256,0.987470879370256),(0.990086238235256,0.987329216372183,
0.987470879370256,0.987470879370256,0.987470879370256)))
REPRESENTATION_ITEM('')
SURFACE()
);
#4049=(
BOUNDED_SURFACE()
B_SPLINE_SURFACE(1,2,((#162720,#162721,#162722),(#162723,#162724,#162725)),
 .UNSPECIFIED.,.F.,.F.,.F.)
B_SPLINE_SURFACE_WITH_KNOTS((2,2),(3,3),(0.710192959008441,1.),(0.625170525609408,
0.642682999576236),.UNSPECIFIED.)
GEOMETRIC_REPRESENTATION_ITEM()
RATIONAL_B_SPLINE_SURFACE(((0.990658108926709,0.993760979299921,0.999878046252917),
(0.990658108926709,0.993760979299921,0.999878046252917)))
REPRESENTATION_ITEM('')
SURFACE()
);
#4050=(
BOUNDED_SURFACE()
B_SPLINE_SURFACE(1,2,((#162729,#162730,#162731,#162732,#162733),(#162734,
#162735,#162736,#162737,#162738)),.UNSPECIFIED.,.F.,.F.,.F.)
B_SPLINE_SURFACE_WITH_KNOTS((2,2),(3,2,3),(0.710059257942299,1.),(0.0908085233856346,
0.107982157956011,0.108241816874653),.UNSPECIFIED.)
GEOMETRIC_REPRESENTATION_ITEM()
RATIONAL_B_SPLINE_SURFACE(((0.990086238235257,0.987329216372183,0.987470879370256,
0.987470879370256,0.987470879370256),(0.990086238235257,0.987329216372183,
0.987470879370256,0.987470879370256,0.987470879370256)))
REPRESENTATION_ITEM('')
SURFACE()
);
#4051=(
BOUNDED_SURFACE()
B_SPLINE_SURFACE(1,2,((#162740,#162741,#162742),(#162743,#162744,#162745)),
 .UNSPECIFIED.,.F.,.F.,.F.)
B_SPLINE_SURFACE_WITH_KNOTS((2,2),(3,3),(0.710192959008435,1.),(0.625170525609408,
0.642682999576236),.UNSPECIFIED.)
GEOMETRIC_REPRESENTATION_ITEM()
RATIONAL_B_SPLINE_SURFACE(((0.990658108926709,0.993760979299922,0.999878046252917),
(0.990658108926709,0.993760979299922,0.999878046252917)))
REPRESENTATION_ITEM('')
SURFACE()
);
#4052=(
BOUNDED_SURFACE()
B_SPLINE_SURFACE(1,2,((#162749,#162750,#162751,#162752,#162753),(#162754,
#162755,#162756,#162757,#162758)),.UNSPECIFIED.,.F.,.F.,.F.)
B_SPLINE_SURFACE_WITH_KNOTS((2,2),(3,2,3),(0.710059258506232,1.),(0.0908085233856347,
0.107982157956011,0.108241816310694),.UNSPECIFIED.)
GEOMETRIC_REPRESENTATION_ITEM()
RATIONAL_B_SPLINE_SURFACE(((0.990086238235256,0.987329216372183,0.987470879370255,
0.987470879370255,0.987470879370255),(0.990086238235256,0.987329216372183,
0.987470879370255,0.987470879370255,0.987470879370255)))
REPRESENTATION_ITEM('')
SURFACE()
);
#4053=(
BOUNDED_SURFACE()
B_SPLINE_SURFACE(1,2,((#162760,#162761,#162762),(#162763,#162764,#162765)),
 .UNSPECIFIED.,.F.,.F.,.F.)
B_SPLINE_SURFACE_WITH_KNOTS((2,2),(3,3),(0.71019295900844,1.),(0.625170525609408,
0.642682999576236),.UNSPECIFIED.)
GEOMETRIC_REPRESENTATION_ITEM()
RATIONAL_B_SPLINE_SURFACE(((0.990658108926709,0.993760979299922,0.999878046252917),
(0.990658108926709,0.993760979299922,0.999878046252917)))
REPRESENTATION_ITEM('')
SURFACE()
);
#4054=(
BOUNDED_SURFACE()
B_SPLINE_SURFACE(1,2,((#162769,#162770,#162771,#162772,#162773),(#162774,
#162775,#162776,#162777,#162778)),.UNSPECIFIED.,.F.,.F.,.F.)
B_SPLINE_SURFACE_WITH_KNOTS((2,2),(3,2,3),(0.71005925774851,1.),(0.0908085233856347,
0.107982157956011,0.108241817068402),.UNSPECIFIED.)
GEOMETRIC_REPRESENTATION_ITEM()
RATIONAL_B_SPLINE_SURFACE(((0.990086238235256,0.987329216372183,0.987470879370255,
0.987470879370255,0.987470879370255),(0.990086238235256,0.987329216372183,
0.987470879370255,0.987470879370255,0.987470879370255)))
REPRESENTATION_ITEM('')
SURFACE()
);
#4055=(
BOUNDED_SURFACE()
B_SPLINE_SURFACE(1,2,((#162780,#162781,#162782),(#162783,#162784,#162785)),
 .UNSPECIFIED.,.F.,.F.,.F.)
B_SPLINE_SURFACE_WITH_KNOTS((2,2),(3,3),(0.710192959008443,1.),(0.625170525609409,
0.642682999576236),.UNSPECIFIED.)
GEOMETRIC_REPRESENTATION_ITEM()
RATIONAL_B_SPLINE_SURFACE(((0.990658108926709,0.993760979299921,0.999878046252917),
(0.990658108926709,0.993760979299921,0.999878046252917)))
REPRESENTATION_ITEM('')
SURFACE()
);
#4056=(
BOUNDED_SURFACE()
B_SPLINE_SURFACE(1,2,((#162789,#162790,#162791,#162792,#162793),(#162794,
#162795,#162796,#162797,#162798)),.UNSPECIFIED.,.F.,.F.,.F.)
B_SPLINE_SURFACE_WITH_KNOTS((2,2),(3,2,3),(0.710059257944843,1.),(0.0908085233856348,
0.107982157956011,0.108241816872063),.UNSPECIFIED.)
GEOMETRIC_REPRESENTATION_ITEM()
RATIONAL_B_SPLINE_SURFACE(((0.990086238235256,0.987329216372183,0.987470879370255,
0.987470879370255,0.987470879370255),(0.990086238235256,0.987329216372183,
0.987470879370255,0.987470879370255,0.987470879370255)))
REPRESENTATION_ITEM('')
SURFACE()
);
#4057=(
BOUNDED_SURFACE()
B_SPLINE_SURFACE(1,2,((#162800,#162801,#162802),(#162803,#162804,#162805)),
 .UNSPECIFIED.,.F.,.F.,.F.)
B_SPLINE_SURFACE_WITH_KNOTS((2,2),(3,3),(0.710192959008253,1.),(0.625170525609404,
0.642682999576235),.UNSPECIFIED.)
GEOMETRIC_REPRESENTATION_ITEM()
RATIONAL_B_SPLINE_SURFACE(((0.990658108926707,0.99376097929992,0.999878046252916),
(0.990658108926707,0.99376097929992,0.999878046252916)))
REPRESENTATION_ITEM('')
SURFACE()
);
#4058=(
BOUNDED_SURFACE()
B_SPLINE_SURFACE(1,2,((#162809,#162810,#162811,#162812,#162813),(#162814,
#162815,#162816,#162817,#162818)),.UNSPECIFIED.,.F.,.F.,.F.)
B_SPLINE_SURFACE_WITH_KNOTS((2,2),(3,2,3),(0.710059257864338,1.),(0.0908085233856356,
0.107982157956012,0.108241816952354),.UNSPECIFIED.)
GEOMETRIC_REPRESENTATION_ITEM()
RATIONAL_B_SPLINE_SURFACE(((0.990086238235256,0.987329216372183,0.987470879370256,
0.987470879370256,0.987470879370256),(0.990086238235256,0.987329216372183,
0.987470879370256,0.987470879370256,0.987470879370256)))
REPRESENTATION_ITEM('')
SURFACE()
);
#4059=(
BOUNDED_SURFACE()
B_SPLINE_SURFACE(1,2,((#162820,#162821,#162822),(#162823,#162824,#162825)),
 .UNSPECIFIED.,.F.,.F.,.F.)
B_SPLINE_SURFACE_WITH_KNOTS((2,2),(3,3),(0.710192959008401,1.),(0.625170525609407,
0.642682999576235),.UNSPECIFIED.)
GEOMETRIC_REPRESENTATION_ITEM()
RATIONAL_B_SPLINE_SURFACE(((0.990658108926708,0.993760979299921,0.999878046252916),
(0.990658108926708,0.993760979299921,0.999878046252916)))
REPRESENTATION_ITEM('')
SURFACE()
);
#4060=(
BOUNDED_SURFACE()
B_SPLINE_SURFACE(1,2,((#162829,#162830,#162831,#162832,#162833),(#162834,
#162835,#162836,#162837,#162838)),.UNSPECIFIED.,.F.,.F.,.F.)
B_SPLINE_SURFACE_WITH_KNOTS((2,2),(3,2,3),(0.710059257951225,1.),(0.0908085233856358,
0.107982157956012,0.108241816865715),.UNSPECIFIED.)
GEOMETRIC_REPRESENTATION_ITEM()
RATIONAL_B_SPLINE_SURFACE(((0.990086238235256,0.987329216372183,0.987470879370255,
0.987470879370255,0.987470879370255),(0.990086238235256,0.987329216372183,
0.987470879370255,0.987470879370255,0.987470879370255)))
REPRESENTATION_ITEM('')
SURFACE()
);
#4061=(
BOUNDED_SURFACE()
B_SPLINE_SURFACE(1,2,((#162840,#162841,#162842),(#162843,#162844,#162845)),
 .UNSPECIFIED.,.F.,.F.,.F.)
B_SPLINE_SURFACE_WITH_KNOTS((2,2),(3,3),(0.71019295900844,1.),(0.625170525609407,
0.642682999576235),.UNSPECIFIED.)
GEOMETRIC_REPRESENTATION_ITEM()
RATIONAL_B_SPLINE_SURFACE(((0.990658108926708,0.993760979299921,0.999878046252916),
(0.990658108926708,0.993760979299921,0.999878046252916)))
REPRESENTATION_ITEM('')
SURFACE()
);
#4062=(
BOUNDED_SURFACE()
B_SPLINE_SURFACE(1,2,((#162849,#162850,#162851,#162852,#162853),(#162854,
#162855,#162856,#162857,#162858)),.UNSPECIFIED.,.F.,.F.,.F.)
B_SPLINE_SURFACE_WITH_KNOTS((2,2),(3,2,3),(0.710059258002317,1.),(0.0908085233856358,
0.107982157956012,0.108241816814637),.UNSPECIFIED.)
GEOMETRIC_REPRESENTATION_ITEM()
RATIONAL_B_SPLINE_SURFACE(((0.990086238235256,0.987329216372183,0.987470879370256,
0.987470879370256,0.987470879370256),(0.990086238235256,0.987329216372183,
0.987470879370256,0.987470879370256,0.987470879370256)))
REPRESENTATION_ITEM('')
SURFACE()
);
#4063=(
BOUNDED_SURFACE()
B_SPLINE_SURFACE(1,2,((#162860,#162861,#162862),(#162863,#162864,#162865)),
 .UNSPECIFIED.,.F.,.F.,.F.)
B_SPLINE_SURFACE_WITH_KNOTS((2,2),(3,3),(0.71019295900844,1.),(0.625170525609407,
0.642682999576235),.UNSPECIFIED.)
GEOMETRIC_REPRESENTATION_ITEM()
RATIONAL_B_SPLINE_SURFACE(((0.990658108926708,0.993760979299921,0.999878046252916),
(0.990658108926708,0.993760979299921,0.999878046252916)))
REPRESENTATION_ITEM('')
SURFACE()
);
#4064=(
BOUNDED_SURFACE()
B_SPLINE_SURFACE(1,2,((#162869,#162870,#162871,#162872,#162873),(#162874,
#162875,#162876,#162877,#162878)),.UNSPECIFIED.,.F.,.F.,.F.)
B_SPLINE_SURFACE_WITH_KNOTS((2,2),(3,2,3),(0.710059257948496,1.),(0.0908085233856358,
0.107982157956012,0.108241816868451),.UNSPECIFIED.)
GEOMETRIC_REPRESENTATION_ITEM()
RATIONAL_B_SPLINE_SURFACE(((0.990086238235256,0.987329216372183,0.987470879370256,
0.987470879370256,0.987470879370256),(0.990086238235256,0.987329216372183,
0.987470879370256,0.987470879370256,0.987470879370256)))
REPRESENTATION_ITEM('')
SURFACE()
);
#4065=(
BOUNDED_SURFACE()
B_SPLINE_SURFACE(1,2,((#162880,#162881,#162882),(#162883,#162884,#162885)),
 .UNSPECIFIED.,.F.,.F.,.F.)
B_SPLINE_SURFACE_WITH_KNOTS((2,2),(3,3),(0.7101929590083,1.),(0.625170525609407,
0.642682999576235),.UNSPECIFIED.)
GEOMETRIC_REPRESENTATION_ITEM()
RATIONAL_B_SPLINE_SURFACE(((0.990658108926708,0.993760979299921,0.999878046252916),
(0.990658108926708,0.993760979299921,0.999878046252916)))
REPRESENTATION_ITEM('')
SURFACE()
);
#4066=(
BOUNDED_SURFACE()
B_SPLINE_SURFACE(1,2,((#162889,#162890,#162891,#162892,#162893),(#162894,
#162895,#162896,#162897,#162898)),.UNSPECIFIED.,.F.,.F.,.F.)
B_SPLINE_SURFACE_WITH_KNOTS((2,2),(3,2,3),(0.710059258485914,1.),(0.0908085233856358,
0.107982157956012,0.108241816330897),.UNSPECIFIED.)
GEOMETRIC_REPRESENTATION_ITEM()
RATIONAL_B_SPLINE_SURFACE(((0.990086238235256,0.987329216372183,0.987470879370256,
0.987470879370256,0.987470879370256),(0.990086238235256,0.987329216372183,
0.987470879370256,0.987470879370256,0.987470879370256)))
REPRESENTATION_ITEM('')
SURFACE()
);
#4067=(
BOUNDED_SURFACE()
B_SPLINE_SURFACE(1,2,((#162900,#162901,#162902),(#162903,#162904,#162905)),
 .UNSPECIFIED.,.F.,.F.,.F.)
B_SPLINE_SURFACE_WITH_KNOTS((2,2),(3,3),(0.710192959008298,1.),(0.625170525609407,
0.642682999576235),.UNSPECIFIED.)
GEOMETRIC_REPRESENTATION_ITEM()
RATIONAL_B_SPLINE_SURFACE(((0.990658108926708,0.993760979299921,0.999878046252916),
(0.990658108926708,0.993760979299921,0.999878046252916)))
REPRESENTATION_ITEM('')
SURFACE()
);
#4068=(
BOUNDED_SURFACE()
B_SPLINE_SURFACE(1,2,((#162909,#162910,#162911,#162912,#162913),(#162914,
#162915,#162916,#162917,#162918)),.UNSPECIFIED.,.F.,.F.,.F.)
B_SPLINE_SURFACE_WITH_KNOTS((2,2),(3,2,3),(0.710059257984503,1.),(0.0908085233856357,
0.107982157956012,0.108241816832277),.UNSPECIFIED.)
GEOMETRIC_REPRESENTATION_ITEM()
RATIONAL_B_SPLINE_SURFACE(((0.990086238235256,0.987329216372183,0.987470879370256,
0.987470879370256,0.987470879370256),(0.990086238235256,0.987329216372183,
0.987470879370256,0.987470879370256,0.987470879370256)))
REPRESENTATION_ITEM('')
SURFACE()
);
#4069=(
BOUNDED_SURFACE()
B_SPLINE_SURFACE(1,2,((#162920,#162921,#162922),(#162923,#162924,#162925)),
 .UNSPECIFIED.,.F.,.F.,.F.)
B_SPLINE_SURFACE_WITH_KNOTS((2,2),(3,3),(0.710192959008281,1.),(0.625170525609407,
0.642682999576235),.UNSPECIFIED.)
GEOMETRIC_REPRESENTATION_ITEM()
RATIONAL_B_SPLINE_SURFACE(((0.990658108926708,0.993760979299921,0.999878046252916),
(0.990658108926708,0.993760979299921,0.999878046252916)))
REPRESENTATION_ITEM('')
SURFACE()
);
#4070=(
BOUNDED_SURFACE()
B_SPLINE_SURFACE(1,2,((#162929,#162930,#162931,#162932,#162933),(#162934,
#162935,#162936,#162937,#162938)),.UNSPECIFIED.,.F.,.F.,.F.)
B_SPLINE_SURFACE_WITH_KNOTS((2,2),(3,2,3),(0.710059257931992,1.),(0.0908085233856358,
0.107982157956012,0.108241816884714),.UNSPECIFIED.)
GEOMETRIC_REPRESENTATION_ITEM()
RATIONAL_B_SPLINE_SURFACE(((0.990086238235256,0.987329216372183,0.987470879370256,
0.987470879370256,0.987470879370256),(0.990086238235256,0.987329216372183,
0.987470879370256,0.987470879370256,0.987470879370256)))
REPRESENTATION_ITEM('')
SURFACE()
);
#4071=(
BOUNDED_SURFACE()
B_SPLINE_SURFACE(1,2,((#162940,#162941,#162942),(#162943,#162944,#162945)),
 .UNSPECIFIED.,.F.,.F.,.F.)
B_SPLINE_SURFACE_WITH_KNOTS((2,2),(3,3),(0.71019295900691,1.),(0.625170525609407,
0.642682999576235),.UNSPECIFIED.)
GEOMETRIC_REPRESENTATION_ITEM()
RATIONAL_B_SPLINE_SURFACE(((0.990658108926708,0.993760979299921,0.999878046252916),
(0.990658108926708,0.993760979299921,0.999878046252916)))
REPRESENTATION_ITEM('')
SURFACE()
);
#4072=(
BOUNDED_SURFACE()
B_SPLINE_SURFACE(1,2,((#162949,#162950,#162951,#162952,#162953),(#162954,
#162955,#162956,#162957,#162958)),.UNSPECIFIED.,.F.,.F.,.F.)
B_SPLINE_SURFACE_WITH_KNOTS((2,2),(3,2,3),(0.71005925787149,1.),(0.0908085233856358,
0.107982157956012,0.108241816944409),.UNSPECIFIED.)
GEOMETRIC_REPRESENTATION_ITEM()
RATIONAL_B_SPLINE_SURFACE(((0.990086238235256,0.987329216372183,0.987470879370256,
0.987470879370256,0.987470879370256),(0.990086238235256,0.987329216372183,
0.987470879370255,0.987470879370255,0.987470879370255)))
REPRESENTATION_ITEM('')
SURFACE()
);
#4073=(
BOUNDED_SURFACE()
B_SPLINE_SURFACE(1,2,((#162960,#162961,#162962),(#162963,#162964,#162965)),
 .UNSPECIFIED.,.F.,.F.,.F.)
B_SPLINE_SURFACE_WITH_KNOTS((2,2),(3,3),(0.710192959008067,1.),(0.625170525609407,
0.642682999576233),.UNSPECIFIED.)
GEOMETRIC_REPRESENTATION_ITEM()
RATIONAL_B_SPLINE_SURFACE(((0.990658108926708,0.99376097929992,0.999878046252914),
(0.990658108926708,0.99376097929992,0.999878046252914)))
REPRESENTATION_ITEM('')
SURFACE()
);
#4074=(
BOUNDED_SURFACE()
B_SPLINE_SURFACE(1,2,((#162969,#162970,#162971,#162972,#162973),(#162974,
#162975,#162976,#162977,#162978)),.UNSPECIFIED.,.F.,.F.,.F.)
B_SPLINE_SURFACE_WITH_KNOTS((2,2),(3,2,3),(0.710059258140776,1.),(0.0908085233856304,
0.107982157956012,0.108241816675822),.UNSPECIFIED.)
GEOMETRIC_REPRESENTATION_ITEM()
RATIONAL_B_SPLINE_SURFACE(((0.990086238235258,0.987329216372183,0.987470879370256,
0.987470879370256,0.987470879370256),(0.990086238235258,0.987329216372183,
0.987470879370255,0.987470879370255,0.987470879370255)))
REPRESENTATION_ITEM('')
SURFACE()
);
#4075=(
BOUNDED_SURFACE()
B_SPLINE_SURFACE(1,2,((#162980,#162981,#162982),(#162983,#162984,#162985)),
 .UNSPECIFIED.,.F.,.F.,.F.)
B_SPLINE_SURFACE_WITH_KNOTS((2,2),(3,3),(0.71019295900844,1.),(0.625170525609407,
0.642682999576235),.UNSPECIFIED.)
GEOMETRIC_REPRESENTATION_ITEM()
RATIONAL_B_SPLINE_SURFACE(((0.990658108926708,0.993760979299921,0.999878046252916),
(0.990658108926708,0.993760979299921,0.999878046252916)))
REPRESENTATION_ITEM('')
SURFACE()
);
#4076=(
BOUNDED_SURFACE()
B_SPLINE_SURFACE(1,2,((#162989,#162990,#162991,#162992,#162993),(#162994,
#162995,#162996,#162997,#162998)),.UNSPECIFIED.,.F.,.F.,.F.)
B_SPLINE_SURFACE_WITH_KNOTS((2,2),(3,2,3),(0.710059257748965,1.),(0.0908085233856358,
0.107982157956012,0.108241817067853),.UNSPECIFIED.)
GEOMETRIC_REPRESENTATION_ITEM()
RATIONAL_B_SPLINE_SURFACE(((0.990086238235256,0.987329216372183,0.987470879370256,
0.987470879370256,0.987470879370256),(0.990086238235256,0.987329216372183,
0.987470879370256,0.987470879370256,0.987470879370256)))
REPRESENTATION_ITEM('')
SURFACE()
);
#4077=(
BOUNDED_SURFACE()
B_SPLINE_SURFACE(1,2,((#163000,#163001,#163002),(#163003,#163004,#163005)),
 .UNSPECIFIED.,.F.,.F.,.F.)
B_SPLINE_SURFACE_WITH_KNOTS((2,2),(3,3),(0.710192959008438,1.),(0.625170525609407,
0.642682999576235),.UNSPECIFIED.)
GEOMETRIC_REPRESENTATION_ITEM()
RATIONAL_B_SPLINE_SURFACE(((0.990658108926708,0.993760979299921,0.999878046252916),
(0.990658108926708,0.993760979299921,0.999878046252916)))
REPRESENTATION_ITEM('')
SURFACE()
);
#4078=(
BOUNDED_SURFACE()
B_SPLINE_SURFACE(1,2,((#163009,#163010,#163011,#163012,#163013),(#163014,
#163015,#163016,#163017,#163018)),.UNSPECIFIED.,.F.,.F.,.F.)
B_SPLINE_SURFACE_WITH_KNOTS((2,2),(3,2,3),(0.710059257935878,1.),(0.0908085233856358,
0.107982157956012,0.108241816880996),.UNSPECIFIED.)
GEOMETRIC_REPRESENTATION_ITEM()
RATIONAL_B_SPLINE_SURFACE(((0.990086238235256,0.987329216372183,0.987470879370255,
0.987470879370255,0.987470879370255),(0.990086238235256,0.987329216372183,
0.987470879370255,0.987470879370255,0.987470879370255)))
REPRESENTATION_ITEM('')
SURFACE()
);
#4079=(
BOUNDED_SURFACE()
B_SPLINE_SURFACE(1,2,((#163020,#163021,#163022),(#163023,#163024,#163025)),
 .UNSPECIFIED.,.F.,.F.,.F.)
B_SPLINE_SURFACE_WITH_KNOTS((2,2),(3,3),(0.710192959008437,1.),(0.625170525609407,
0.642682999576235),.UNSPECIFIED.)
GEOMETRIC_REPRESENTATION_ITEM()
RATIONAL_B_SPLINE_SURFACE(((0.990658108926708,0.993760979299921,0.999878046252916),
(0.990658108926708,0.993760979299921,0.999878046252916)))
REPRESENTATION_ITEM('')
SURFACE()
);
#4080=(
BOUNDED_SURFACE()
B_SPLINE_SURFACE(1,2,((#163027,#163028,#163029),(#163030,#163031,#163032),
(#163033,#163034,#163035)),.UNSPECIFIED.,.F.,.F.,.F.)
B_SPLINE_SURFACE_WITH_KNOTS((2,1,2),(3,3),(0.,0.289807040991559,0.311582168299949),
(0.0909109506295943,0.108084585199971),.UNSPECIFIED.)
GEOMETRIC_REPRESENTATION_ITEM()
RATIONAL_B_SPLINE_SURFACE(((0.990053454406147,0.987313720921968,0.987472672298934),
(0.990053454406147,0.987313720921967,0.987472672298933),(0.990053454406147,
0.987313720921967,0.987472672298933)))
REPRESENTATION_ITEM('')
SURFACE()
);
#4081=(
BOUNDED_SURFACE()
B_SPLINE_SURFACE(1,2,((#163076,#163077,#163078),(#163079,#163080,#163081),
(#163082,#163083,#163084)),.UNSPECIFIED.,.F.,.F.,.F.)
B_SPLINE_SURFACE_WITH_KNOTS((2,1,2),(3,3),(0.,0.289681084359918,0.311483586954517),
(0.625066077454536,0.642578551421363),.UNSPECIFIED.)
GEOMETRIC_REPRESENTATION_ITEM()
RATIONAL_B_SPLINE_SURFACE(((0.990621203777021,0.993706096834649,0.999805186472059),
(0.990621203777021,0.993706096834649,0.999805186472059),(0.990621203777021,
0.993706096834649,0.999805186472059)))
REPRESENTATION_ITEM('')
SURFACE()
);
#4082=(
BOUNDED_SURFACE()
B_SPLINE_SURFACE(1,2,((#163086,#163087,#163088),(#163089,#163090,#163091),
(#163092,#163093,#163094)),.UNSPECIFIED.,.F.,.F.,.F.)
B_SPLINE_SURFACE_WITH_KNOTS((2,1,2),(3,3),(0.,0.289807040991555,0.311582168338885),
(0.0909109506295943,0.108084585199971),.UNSPECIFIED.)
GEOMETRIC_REPRESENTATION_ITEM()
RATIONAL_B_SPLINE_SURFACE(((0.990053454406147,0.987313720921968,0.987472672298934),
(0.990053454406147,0.987313720921968,0.987472672298934),(0.990053454406147,
0.987313720921968,0.987472672298934)))
REPRESENTATION_ITEM('')
SURFACE()
);
#4083=(
BOUNDED_SURFACE()
B_SPLINE_SURFACE(1,2,((#163135,#163136,#163137),(#163138,#163139,#163140),
(#163141,#163142,#163143)),.UNSPECIFIED.,.F.,.F.,.F.)
B_SPLINE_SURFACE_WITH_KNOTS((2,1,2),(3,3),(0.,0.289681084359919,0.311483587022812),
(0.625066077454535,0.642578551421363),.UNSPECIFIED.)
GEOMETRIC_REPRESENTATION_ITEM()
RATIONAL_B_SPLINE_SURFACE(((0.990621203777021,0.993706096834649,0.999805186472059),
(0.990621203777021,0.993706096834649,0.999805186472059),(0.990621203777021,
0.993706096834649,0.999805186472059)))
REPRESENTATION_ITEM('')
SURFACE()
);
#4084=(
BOUNDED_SURFACE()
B_SPLINE_SURFACE(1,2,((#163145,#163146,#163147),(#163148,#163149,#163150),
(#163151,#163152,#163153)),.UNSPECIFIED.,.F.,.F.,.F.)
B_SPLINE_SURFACE_WITH_KNOTS((2,1,2),(3,3),(0.,0.289807040991561,0.311582168422346),
(0.0909109506295943,0.108084585199971),.UNSPECIFIED.)
GEOMETRIC_REPRESENTATION_ITEM()
RATIONAL_B_SPLINE_SURFACE(((0.990053454406147,0.987313720921968,0.987472672298934),
(0.990053454406147,0.987313720921968,0.987472672298934),(0.990053454406147,
0.987313720921968,0.987472672298934)))
REPRESENTATION_ITEM('')
SURFACE()
);
#4085=(
BOUNDED_SURFACE()
B_SPLINE_SURFACE(1,2,((#163194,#163195,#163196),(#163197,#163198,#163199),
(#163200,#163201,#163202)),.UNSPECIFIED.,.F.,.F.,.F.)
B_SPLINE_SURFACE_WITH_KNOTS((2,1,2),(3,3),(0.,0.289681084359919,0.31148358704291),
(0.625066077454535,0.642578551421363),.UNSPECIFIED.)
GEOMETRIC_REPRESENTATION_ITEM()
RATIONAL_B_SPLINE_SURFACE(((0.990621203777021,0.993706096834649,0.999805186472059),
(0.990621203777021,0.993706096834649,0.999805186472059),(0.990621203777021,
0.993706096834649,0.999805186472059)))
REPRESENTATION_ITEM('')
SURFACE()
);
#4086=(
BOUNDED_SURFACE()
B_SPLINE_SURFACE(1,2,((#163204,#163205,#163206),(#163207,#163208,#163209),
(#163210,#163211,#163212)),.UNSPECIFIED.,.F.,.F.,.F.)
B_SPLINE_SURFACE_WITH_KNOTS((2,1,2),(3,3),(0.,0.289807040991562,0.311582167804269),
(0.0909109506295943,0.10808458519997),.UNSPECIFIED.)
GEOMETRIC_REPRESENTATION_ITEM()
RATIONAL_B_SPLINE_SURFACE(((0.990053454406147,0.987313720921968,0.987472672298934),
(0.990053454406147,0.987313720921967,0.987472672298933),(0.990053454406147,
0.987313720921967,0.987472672298933)))
REPRESENTATION_ITEM('')
SURFACE()
);
#4087=(
BOUNDED_SURFACE()
B_SPLINE_SURFACE(1,2,((#163253,#163254,#163255),(#163256,#163257,#163258),
(#163259,#163260,#163261)),.UNSPECIFIED.,.F.,.F.,.F.)
B_SPLINE_SURFACE_WITH_KNOTS((2,1,2),(3,3),(0.,0.289681084359921,0.311483587161093),
(0.625066077454535,0.642578551421363),.UNSPECIFIED.)
GEOMETRIC_REPRESENTATION_ITEM()
RATIONAL_B_SPLINE_SURFACE(((0.990621203777021,0.993706096834649,0.999805186472059),
(0.990621203777021,0.993706096834649,0.999805186472059),(0.990621203777021,
0.993706096834649,0.999805186472059)))
REPRESENTATION_ITEM('')
SURFACE()
);
#4088=(
BOUNDED_SURFACE()
B_SPLINE_SURFACE(1,2,((#163263,#163264,#163265),(#163266,#163267,#163268),
(#163269,#163270,#163271)),.UNSPECIFIED.,.F.,.F.,.F.)
B_SPLINE_SURFACE_WITH_KNOTS((2,1,2),(3,3),(0.,0.289807040991556,0.3115821682498),
(0.0909109506295943,0.108084585199969),.UNSPECIFIED.)
GEOMETRIC_REPRESENTATION_ITEM()
RATIONAL_B_SPLINE_SURFACE(((0.990053454406147,0.987313720921968,0.987472672298934),
(0.990053454406147,0.987313720921968,0.987472672298934),(0.990053454406147,
0.987313720921968,0.987472672298934)))
REPRESENTATION_ITEM('')
SURFACE()
);
#4089=(
BOUNDED_SURFACE()
B_SPLINE_SURFACE(1,2,((#163312,#163313,#163314),(#163315,#163316,#163317),
(#163318,#163319,#163320)),.UNSPECIFIED.,.F.,.F.,.F.)
B_SPLINE_SURFACE_WITH_KNOTS((2,1,2),(3,3),(0.,0.289681084359916,0.311483587306944),
(0.625066077454536,0.642578551421364),.UNSPECIFIED.)
GEOMETRIC_REPRESENTATION_ITEM()
RATIONAL_B_SPLINE_SURFACE(((0.990621203777022,0.993706096834649,0.999805186472059),
(0.990621203777022,0.993706096834649,0.999805186472059),(0.990621203777022,
0.993706096834649,0.999805186472059)))
REPRESENTATION_ITEM('')
SURFACE()
);
#4090=(
BOUNDED_SURFACE()
B_SPLINE_SURFACE(1,2,((#163322,#163323,#163324),(#163325,#163326,#163327),
(#163328,#163329,#163330)),.UNSPECIFIED.,.F.,.F.,.F.)
B_SPLINE_SURFACE_WITH_KNOTS((2,1,2),(3,3),(0.,0.289807040991564,0.311582168172586),
(0.0909109506295932,0.108084585199969),.UNSPECIFIED.)
GEOMETRIC_REPRESENTATION_ITEM()
RATIONAL_B_SPLINE_SURFACE(((0.990053454406148,0.987313720921968,0.987472672298934),
(0.990053454406147,0.987313720921968,0.987472672298934),(0.990053454406147,
0.987313720921968,0.987472672298934)))
REPRESENTATION_ITEM('')
SURFACE()
);
#4091=(
BOUNDED_SURFACE()
B_SPLINE_SURFACE(1,2,((#163371,#163372,#163373),(#163374,#163375,#163376),
(#163377,#163378,#163379)),.UNSPECIFIED.,.F.,.F.,.F.)
B_SPLINE_SURFACE_WITH_KNOTS((2,1,2),(3,3),(0.,0.289681084359926,0.311483587003064),
(0.625066077454536,0.642578551421364),.UNSPECIFIED.)
GEOMETRIC_REPRESENTATION_ITEM()
RATIONAL_B_SPLINE_SURFACE(((0.990621203777022,0.993706096834649,0.999805186472059),
(0.990621203777022,0.993706096834649,0.999805186472059),(0.990621203777022,
0.993706096834649,0.999805186472059)))
REPRESENTATION_ITEM('')
SURFACE()
);
#4092=(
BOUNDED_SURFACE()
B_SPLINE_SURFACE(1,2,((#163381,#163382,#163383),(#163384,#163385,#163386),
(#163387,#163388,#163389)),.UNSPECIFIED.,.F.,.F.,.F.)
B_SPLINE_SURFACE_WITH_KNOTS((2,1,2),(3,3),(0.,0.289807040991566,0.311582168018321),
(0.0909109506295932,0.108084585199969),.UNSPECIFIED.)
GEOMETRIC_REPRESENTATION_ITEM()
RATIONAL_B_SPLINE_SURFACE(((0.990053454406148,0.987313720921968,0.987472672298934),
(0.990053454406148,0.987313720921968,0.987472672298934),(0.990053454406148,
0.987313720921968,0.987472672298934)))
REPRESENTATION_ITEM('')
SURFACE()
);
#4093=(
BOUNDED_SURFACE()
B_SPLINE_SURFACE(1,2,((#163430,#163431,#163432),(#163433,#163434,#163435),
(#163436,#163437,#163438)),.UNSPECIFIED.,.F.,.F.,.F.)
B_SPLINE_SURFACE_WITH_KNOTS((2,1,2),(3,3),(0.,0.289681084359925,0.311483586740803),
(0.625066077454536,0.642578551421364),.UNSPECIFIED.)
GEOMETRIC_REPRESENTATION_ITEM()
RATIONAL_B_SPLINE_SURFACE(((0.990621203777022,0.993706096834649,0.999805186472059),
(0.990621203777022,0.993706096834649,0.999805186472059),(0.990621203777022,
0.993706096834649,0.999805186472059)))
REPRESENTATION_ITEM('')
SURFACE()
);
#4094=(
BOUNDED_SURFACE()
B_SPLINE_SURFACE(1,2,((#163440,#163441,#163442),(#163443,#163444,#163445),
(#163446,#163447,#163448)),.UNSPECIFIED.,.F.,.F.,.F.)
B_SPLINE_SURFACE_WITH_KNOTS((2,1,2),(3,3),(0.,0.289807040991568,0.311582168115042),
(0.0909109506295933,0.10808458519997),.UNSPECIFIED.)
GEOMETRIC_REPRESENTATION_ITEM()
RATIONAL_B_SPLINE_SURFACE(((0.990053454406148,0.987313720921968,0.987472672298934),
(0.990053454406148,0.987313720921968,0.987472672298934),(0.990053454406148,
0.987313720921968,0.987472672298934)))
REPRESENTATION_ITEM('')
SURFACE()
);
#4095=(
BOUNDED_SURFACE()
B_SPLINE_SURFACE(1,2,((#163489,#163490,#163491),(#163492,#163493,#163494),
(#163495,#163496,#163497)),.UNSPECIFIED.,.F.,.F.,.F.)
B_SPLINE_SURFACE_WITH_KNOTS((2,1,2),(3,3),(0.,0.289681084359926,0.31148358704133),
(0.625066077454536,0.642578551421364),.UNSPECIFIED.)
GEOMETRIC_REPRESENTATION_ITEM()
RATIONAL_B_SPLINE_SURFACE(((0.990621203777022,0.993706096834649,0.999805186472059),
(0.990621203777022,0.993706096834649,0.999805186472059),(0.990621203777022,
0.993706096834649,0.999805186472059)))
REPRESENTATION_ITEM('')
SURFACE()
);
#4096=(
BOUNDED_SURFACE()
B_SPLINE_SURFACE(1,2,((#163499,#163500,#163501),(#163502,#163503,#163504),
(#163505,#163506,#163507)),.UNSPECIFIED.,.F.,.F.,.F.)
B_SPLINE_SURFACE_WITH_KNOTS((2,1,2),(3,3),(0.,0.289807040991563,0.311582168082872),
(0.0909109506295932,0.10808458519997),.UNSPECIFIED.)
GEOMETRIC_REPRESENTATION_ITEM()
RATIONAL_B_SPLINE_SURFACE(((0.990053454406148,0.987313720921968,0.987472672298934),
(0.990053454406147,0.987313720921968,0.987472672298933),(0.990053454406147,
0.987313720921968,0.987472672298933)))
REPRESENTATION_ITEM('')
SURFACE()
);
#4097=(
BOUNDED_SURFACE()
B_SPLINE_SURFACE(1,2,((#163548,#163549,#163550),(#163551,#163552,#163553),
(#163554,#163555,#163556)),.UNSPECIFIED.,.F.,.F.,.F.)
B_SPLINE_SURFACE_WITH_KNOTS((2,1,2),(3,3),(0.,0.289681084359922,0.311483586742761),
(0.625066077454537,0.642578551421364),.UNSPECIFIED.)
GEOMETRIC_REPRESENTATION_ITEM()
RATIONAL_B_SPLINE_SURFACE(((0.990621203777022,0.993706096834649,0.999805186472059),
(0.990621203777022,0.993706096834649,0.999805186472059),(0.990621203777022,
0.993706096834649,0.999805186472059)))
REPRESENTATION_ITEM('')
SURFACE()
);
#4098=(
BOUNDED_SURFACE()
B_SPLINE_SURFACE(1,2,((#163558,#163559,#163560),(#163561,#163562,#163563),
(#163564,#163565,#163566)),.UNSPECIFIED.,.F.,.F.,.F.)
B_SPLINE_SURFACE_WITH_KNOTS((2,1,2),(3,3),(0.,0.289807040991562,0.311582168130035),
(0.0909109506295931,0.108084585199969),.UNSPECIFIED.)
GEOMETRIC_REPRESENTATION_ITEM()
RATIONAL_B_SPLINE_SURFACE(((0.990053454406148,0.987313720921968,0.987472672298934),
(0.990053454406147,0.987313720921968,0.987472672298933),(0.990053454406147,
0.987313720921968,0.987472672298933)))
REPRESENTATION_ITEM('')
SURFACE()
);
#4099=(
BOUNDED_SURFACE()
B_SPLINE_SURFACE(1,2,((#163607,#163608,#163609),(#163610,#163611,#163612),
(#163613,#163614,#163615)),.UNSPECIFIED.,.F.,.F.,.F.)
B_SPLINE_SURFACE_WITH_KNOTS((2,1,2),(3,3),(0.,0.289681084359916,0.311483587005553),
(0.625066077454537,0.642578551421365),.UNSPECIFIED.)
GEOMETRIC_REPRESENTATION_ITEM()
RATIONAL_B_SPLINE_SURFACE(((0.990621203777022,0.993706096834649,0.999805186472059),
(0.990621203777022,0.993706096834649,0.999805186472059),(0.990621203777022,
0.993706096834649,0.999805186472059)))
REPRESENTATION_ITEM('')
SURFACE()
);
#4100=(
BOUNDED_SURFACE()
B_SPLINE_SURFACE(1,2,((#163617,#163618,#163619),(#163620,#163621,#163622),
(#163623,#163624,#163625)),.UNSPECIFIED.,.F.,.F.,.F.)
B_SPLINE_SURFACE_WITH_KNOTS((2,1,2),(3,3),(0.,0.289807040991561,0.311582167973507),
(0.0909109506295932,0.10808458519997),.UNSPECIFIED.)
GEOMETRIC_REPRESENTATION_ITEM()
RATIONAL_B_SPLINE_SURFACE(((0.990053454406147,0.987313720921968,0.987472672298934),
(0.990053454406147,0.987313720921968,0.987472672298934),(0.990053454406147,
0.987313720921968,0.987472672298934)))
REPRESENTATION_ITEM('')
SURFACE()
);
#4101=(
BOUNDED_SURFACE()
B_SPLINE_SURFACE(1,2,((#163666,#163667,#163668),(#163669,#163670,#163671),
(#163672,#163673,#163674)),.UNSPECIFIED.,.F.,.F.,.F.)
B_SPLINE_SURFACE_WITH_KNOTS((2,1,2),(3,3),(0.,0.289681084359914,0.311483587146096),
(0.625066077454537,0.642578551421365),.UNSPECIFIED.)
GEOMETRIC_REPRESENTATION_ITEM()
RATIONAL_B_SPLINE_SURFACE(((0.990621203777022,0.993706096834649,0.999805186472059),
(0.990621203777022,0.993706096834649,0.999805186472059),(0.990621203777022,
0.993706096834649,0.999805186472059)))
REPRESENTATION_ITEM('')
SURFACE()
);
#4102=(
BOUNDED_SURFACE()
B_SPLINE_SURFACE(1,2,((#163676,#163677,#163678),(#163679,#163680,#163681),
(#163682,#163683,#163684)),.UNSPECIFIED.,.F.,.F.,.F.)
B_SPLINE_SURFACE_WITH_KNOTS((2,1,2),(3,3),(0.,0.289807040991563,0.311582168117811),
(0.090910950629593,0.10808458519997),.UNSPECIFIED.)
GEOMETRIC_REPRESENTATION_ITEM()
RATIONAL_B_SPLINE_SURFACE(((0.990053454406148,0.987313720921968,0.987472672298934),
(0.990053454406148,0.987313720921968,0.987472672298934),(0.990053454406148,
0.987313720921968,0.987472672298934)))
REPRESENTATION_ITEM('')
SURFACE()
);
#4103=(
BOUNDED_SURFACE()
B_SPLINE_SURFACE(1,2,((#163725,#163726,#163727),(#163728,#163729,#163730),
(#163731,#163732,#163733)),.UNSPECIFIED.,.F.,.F.,.F.)
B_SPLINE_SURFACE_WITH_KNOTS((2,1,2),(3,3),(0.,0.289681084359914,0.311483586777713),
(0.625066077454537,0.642578551421365),.UNSPECIFIED.)
GEOMETRIC_REPRESENTATION_ITEM()
RATIONAL_B_SPLINE_SURFACE(((0.990621203777022,0.99370609683465,0.99980518647206),
(0.990621203777022,0.99370609683465,0.99980518647206),(0.990621203777022,
0.99370609683465,0.99980518647206)))
REPRESENTATION_ITEM('')
SURFACE()
);
#4104=(
BOUNDED_SURFACE()
B_SPLINE_SURFACE(1,2,((#163735,#163736,#163737),(#163738,#163739,#163740),
(#163741,#163742,#163743)),.UNSPECIFIED.,.F.,.F.,.F.)
B_SPLINE_SURFACE_WITH_KNOTS((2,1,2),(3,3),(0.,0.289807040991564,0.311582168145372),
(0.0909109506295933,0.108084585199969),.UNSPECIFIED.)
GEOMETRIC_REPRESENTATION_ITEM()
RATIONAL_B_SPLINE_SURFACE(((0.990053454406148,0.987313720921968,0.987472672298934),
(0.990053454406148,0.987313720921968,0.987472672298934),(0.990053454406148,
0.987313720921968,0.987472672298934)))
REPRESENTATION_ITEM('')
SURFACE()
);
#4105=(
BOUNDED_SURFACE()
B_SPLINE_SURFACE(1,2,((#163784,#163785,#163786),(#163787,#163788,#163789),
(#163790,#163791,#163792)),.UNSPECIFIED.,.F.,.F.,.F.)
B_SPLINE_SURFACE_WITH_KNOTS((2,1,2),(3,3),(0.,0.289681084359918,0.311483587040421),
(0.625066077454537,0.642578551421364),.UNSPECIFIED.)
GEOMETRIC_REPRESENTATION_ITEM()
RATIONAL_B_SPLINE_SURFACE(((0.990621203777022,0.993706096834649,0.999805186472059),
(0.990621203777022,0.993706096834649,0.999805186472059),(0.990621203777022,
0.993706096834649,0.999805186472059)))
REPRESENTATION_ITEM('')
SURFACE()
);
#4106=(
BOUNDED_SURFACE()
B_SPLINE_SURFACE(1,2,((#163794,#163795,#163796),(#163797,#163798,#163799),
(#163800,#163801,#163802)),.UNSPECIFIED.,.F.,.F.,.F.)
B_SPLINE_SURFACE_WITH_KNOTS((2,1,2),(3,3),(0.,0.289807040991562,0.311582167901583),
(0.0909109506295932,0.108084585199969),.UNSPECIFIED.)
GEOMETRIC_REPRESENTATION_ITEM()
RATIONAL_B_SPLINE_SURFACE(((0.990053454406148,0.987313720921968,0.987472672298934),
(0.990053454406148,0.987313720921968,0.987472672298934),(0.990053454406148,
0.987313720921968,0.987472672298934)))
REPRESENTATION_ITEM('')
SURFACE()
);
#4107=(
BOUNDED_SURFACE()
B_SPLINE_SURFACE(1,2,((#163843,#163844,#163845),(#163846,#163847,#163848),
(#163849,#163850,#163851)),.UNSPECIFIED.,.F.,.F.,.F.)
B_SPLINE_SURFACE_WITH_KNOTS((2,1,2),(3,3),(0.,0.28968108435992,0.311483587070223),
(0.625066077454536,0.642578551421364),.UNSPECIFIED.)
GEOMETRIC_REPRESENTATION_ITEM()
RATIONAL_B_SPLINE_SURFACE(((0.990621203777022,0.993706096834649,0.999805186472059),
(0.990621203777022,0.993706096834649,0.999805186472059),(0.990621203777022,
0.993706096834649,0.999805186472059)))
REPRESENTATION_ITEM('')
SURFACE()
);
#4108=(
BOUNDED_SURFACE()
B_SPLINE_SURFACE(1,2,((#163853,#163854,#163855),(#163856,#163857,#163858),
(#163859,#163860,#163861)),.UNSPECIFIED.,.F.,.F.,.F.)
B_SPLINE_SURFACE_WITH_KNOTS((2,1,2),(3,3),(0.,0.28980704099156,0.311582167938859),
(0.0909109506295931,0.10808458519997),.UNSPECIFIED.)
GEOMETRIC_REPRESENTATION_ITEM()
RATIONAL_B_SPLINE_SURFACE(((0.990053454406148,0.987313720921968,0.987472672298934),
(0.990053454406148,0.987313720921968,0.987472672298934),(0.990053454406148,
0.987313720921968,0.987472672298934)))
REPRESENTATION_ITEM('')
SURFACE()
);
#4109=(
BOUNDED_SURFACE()
B_SPLINE_SURFACE(1,2,((#163902,#163903,#163904),(#163905,#163906,#163907),
(#163908,#163909,#163910)),.UNSPECIFIED.,.F.,.F.,.F.)
B_SPLINE_SURFACE_WITH_KNOTS((2,1,2),(3,3),(0.,0.289681084359922,0.311483587082788),
(0.625066077454537,0.642578551421364),.UNSPECIFIED.)
GEOMETRIC_REPRESENTATION_ITEM()
RATIONAL_B_SPLINE_SURFACE(((0.990621203777022,0.993706096834649,0.999805186472059),
(0.990621203777022,0.993706096834649,0.999805186472059),(0.990621203777022,
0.993706096834649,0.999805186472059)))
REPRESENTATION_ITEM('')
SURFACE()
);
#4110=(
BOUNDED_SURFACE()
B_SPLINE_SURFACE(1,2,((#163912,#163913,#163914),(#163915,#163916,#163917),
(#163918,#163919,#163920)),.UNSPECIFIED.,.F.,.F.,.F.)
B_SPLINE_SURFACE_WITH_KNOTS((2,1,2),(3,3),(0.,0.289807040991562,0.311582168075301),
(0.0909109506295932,0.108084585199969),.UNSPECIFIED.)
GEOMETRIC_REPRESENTATION_ITEM()
RATIONAL_B_SPLINE_SURFACE(((0.990053454406147,0.987313720921968,0.987472672298934),
(0.990053454406147,0.987313720921968,0.987472672298934),(0.990053454406147,
0.987313720921968,0.987472672298934)))
REPRESENTATION_ITEM('')
SURFACE()
);
#4111=(
BOUNDED_SURFACE()
B_SPLINE_SURFACE(1,2,((#163961,#163962,#163963),(#163964,#163965,#163966),
(#163967,#163968,#163969)),.UNSPECIFIED.,.F.,.F.,.F.)
B_SPLINE_SURFACE_WITH_KNOTS((2,1,2),(3,3),(0.,0.289681084359918,0.31148358684503),
(0.625066077454536,0.642578551421364),.UNSPECIFIED.)
GEOMETRIC_REPRESENTATION_ITEM()
RATIONAL_B_SPLINE_SURFACE(((0.990621203777022,0.993706096834649,0.999805186472059),
(0.990621203777022,0.993706096834649,0.999805186472059),(0.990621203777022,
0.993706096834649,0.999805186472059)))
REPRESENTATION_ITEM('')
SURFACE()
);
#4112=(
BOUNDED_SURFACE()
B_SPLINE_SURFACE(1,2,((#163971,#163972,#163973),(#163974,#163975,#163976),
(#163977,#163978,#163979)),.UNSPECIFIED.,.F.,.F.,.F.)
B_SPLINE_SURFACE_WITH_KNOTS((2,1,2),(3,3),(0.,0.289807040991558,0.311582167912575),
(0.0909109506295932,0.10808458519997),.UNSPECIFIED.)
GEOMETRIC_REPRESENTATION_ITEM()
RATIONAL_B_SPLINE_SURFACE(((0.990053454406148,0.987313720921968,0.987472672298934),
(0.990053454406148,0.987313720921968,0.987472672298934),(0.990053454406148,
0.987313720921968,0.987472672298934)))
REPRESENTATION_ITEM('')
SURFACE()
);
#4113=(
BOUNDED_SURFACE()
B_SPLINE_SURFACE(1,2,((#164020,#164021,#164022),(#164023,#164024,#164025),
(#164026,#164027,#164028)),.UNSPECIFIED.,.F.,.F.,.F.)
B_SPLINE_SURFACE_WITH_KNOTS((2,1,2),(3,3),(0.,0.289681084359916,0.311483587281286),
(0.625066077454537,0.642578551421364),.UNSPECIFIED.)
GEOMETRIC_REPRESENTATION_ITEM()
RATIONAL_B_SPLINE_SURFACE(((0.990621203777022,0.993706096834649,0.999805186472059),
(0.990621203777022,0.993706096834649,0.999805186472059),(0.990621203777022,
0.993706096834649,0.999805186472059)))
REPRESENTATION_ITEM('')
SURFACE()
);
#4114=(
BOUNDED_SURFACE()
B_SPLINE_SURFACE(1,2,((#164030,#164031,#164032),(#164033,#164034,#164035),
(#164036,#164037,#164038)),.UNSPECIFIED.,.F.,.F.,.F.)
B_SPLINE_SURFACE_WITH_KNOTS((2,1,2),(3,3),(0.,0.28980704099156,0.31158216795133),
(0.0909109506295932,0.10808458519997),.UNSPECIFIED.)
GEOMETRIC_REPRESENTATION_ITEM()
RATIONAL_B_SPLINE_SURFACE(((0.990053454406148,0.987313720921968,0.987472672298934),
(0.990053454406148,0.987313720921968,0.987472672298934),(0.990053454406148,
0.987313720921968,0.987472672298934)))
REPRESENTATION_ITEM('')
SURFACE()
);
#4115=(
BOUNDED_SURFACE()
B_SPLINE_SURFACE(1,2,((#164079,#164080,#164081),(#164082,#164083,#164084),
(#164085,#164086,#164087)),.UNSPECIFIED.,.F.,.F.,.F.)
B_SPLINE_SURFACE_WITH_KNOTS((2,1,2),(3,3),(0.,0.289681084359915,0.31148358716528),
(0.625066077454537,0.642578551421363),.UNSPECIFIED.)
GEOMETRIC_REPRESENTATION_ITEM()
RATIONAL_B_SPLINE_SURFACE(((0.990621203777022,0.993706096834649,0.999805186472059),
(0.990621203777022,0.993706096834649,0.999805186472059),(0.990621203777022,
0.993706096834649,0.999805186472059)))
REPRESENTATION_ITEM('')
SURFACE()
);
#4116=(
BOUNDED_SURFACE()
B_SPLINE_SURFACE(1,2,((#164089,#164090,#164091),(#164092,#164093,#164094),
(#164095,#164096,#164097)),.UNSPECIFIED.,.F.,.F.,.F.)
B_SPLINE_SURFACE_WITH_KNOTS((2,1,2),(3,3),(0.,0.289807040991637,0.311582168368617),
(0.0909109506295941,0.10808458519997),.UNSPECIFIED.)
GEOMETRIC_REPRESENTATION_ITEM()
RATIONAL_B_SPLINE_SURFACE(((0.990053454406147,0.987313720921968,0.987472672298934),
(0.990053454406147,0.987313720921968,0.987472672298934),(0.990053454406147,
0.987313720921968,0.987472672298934)))
REPRESENTATION_ITEM('')
SURFACE()
);
#4117=(
BOUNDED_SURFACE()
B_SPLINE_SURFACE(1,2,((#164138,#164139,#164140),(#164141,#164142,#164143),
(#164144,#164145,#164146)),.UNSPECIFIED.,.F.,.F.,.F.)
B_SPLINE_SURFACE_WITH_KNOTS((2,1,2),(3,3),(0.,0.289681084359918,0.311483587033473),
(0.625066077454535,0.642578551421363),.UNSPECIFIED.)
GEOMETRIC_REPRESENTATION_ITEM()
RATIONAL_B_SPLINE_SURFACE(((0.990621203777021,0.993706096834649,0.999805186472059),
(0.990621203777021,0.993706096834649,0.999805186472059),(0.990621203777021,
0.993706096834649,0.999805186472059)))
REPRESENTATION_ITEM('')
SURFACE()
);
#4118=(
BOUNDED_SURFACE()
B_SPLINE_SURFACE(1,2,((#164148,#164149,#164150),(#164151,#164152,#164153),
(#164154,#164155,#164156)),.UNSPECIFIED.,.F.,.F.,.F.)
B_SPLINE_SURFACE_WITH_KNOTS((2,1,2),(3,3),(0.,0.289807040991563,0.31158216809578),
(0.0909109506295943,0.108084585199971),.UNSPECIFIED.)
GEOMETRIC_REPRESENTATION_ITEM()
RATIONAL_B_SPLINE_SURFACE(((0.990053454406147,0.987313720921968,0.987472672298934),
(0.990053454406147,0.987313720921968,0.987472672298934),(0.990053454406147,
0.987313720921968,0.987472672298934)))
REPRESENTATION_ITEM('')
SURFACE()
);
#4119=(
BOUNDED_SURFACE()
B_SPLINE_SURFACE(1,2,((#164197,#164198,#164199),(#164200,#164201,#164202),
(#164203,#164204,#164205)),.UNSPECIFIED.,.F.,.F.,.F.)
B_SPLINE_SURFACE_WITH_KNOTS((2,1,2),(3,3),(0.,0.289681084359918,0.311483587195346),
(0.625066077454535,0.642578551421363),.UNSPECIFIED.)
GEOMETRIC_REPRESENTATION_ITEM()
RATIONAL_B_SPLINE_SURFACE(((0.990621203777021,0.993706096834649,0.999805186472059),
(0.990621203777021,0.993706096834649,0.999805186472059),(0.990621203777021,
0.993706096834649,0.999805186472059)))
REPRESENTATION_ITEM('')
SURFACE()
);
#4120=(
BOUNDED_SURFACE()
B_SPLINE_SURFACE(1,2,((#164207,#164208,#164209),(#164210,#164211,#164212),
(#164213,#164214,#164215)),.UNSPECIFIED.,.F.,.F.,.F.)
B_SPLINE_SURFACE_WITH_KNOTS((2,1,2),(3,3),(0.,0.289807040991564,0.31158216794018),
(0.0909109506295943,0.108084585199971),.UNSPECIFIED.)
GEOMETRIC_REPRESENTATION_ITEM()
RATIONAL_B_SPLINE_SURFACE(((0.990053454406147,0.987313720921968,0.987472672298934),
(0.990053454406147,0.987313720921968,0.987472672298934),(0.990053454406147,
0.987313720921968,0.987472672298934)))
REPRESENTATION_ITEM('')
SURFACE()
);
#4121=(
BOUNDED_SURFACE()
B_SPLINE_SURFACE(1,2,((#164256,#164257,#164258),(#164259,#164260,#164261),
(#164262,#164263,#164264)),.UNSPECIFIED.,.F.,.F.,.F.)
B_SPLINE_SURFACE_WITH_KNOTS((2,1,2),(3,3),(0.,0.289681084359924,0.311483586863778),
(0.625066077454535,0.642578551421363),.UNSPECIFIED.)
GEOMETRIC_REPRESENTATION_ITEM()
RATIONAL_B_SPLINE_SURFACE(((0.990621203777021,0.993706096834649,0.999805186472059),
(0.990621203777021,0.993706096834649,0.999805186472059),(0.990621203777021,
0.993706096834649,0.999805186472059)))
REPRESENTATION_ITEM('')
SURFACE()
);
#4122=(
BOUNDED_SURFACE()
B_SPLINE_SURFACE(1,2,((#164266,#164267,#164268),(#164269,#164270,#164271),
(#164272,#164273,#164274)),.UNSPECIFIED.,.F.,.F.,.F.)
B_SPLINE_SURFACE_WITH_KNOTS((2,1,2),(3,3),(0.,0.289807040991559,0.311582168493806),
(0.0909109506295943,0.108084585199971),.UNSPECIFIED.)
GEOMETRIC_REPRESENTATION_ITEM()
RATIONAL_B_SPLINE_SURFACE(((0.990053454406147,0.987313720921968,0.987472672298934),
(0.990053454406147,0.987313720921967,0.987472672298933),(0.990053454406147,
0.987313720921967,0.987472672298933)))
REPRESENTATION_ITEM('')
SURFACE()
);
#4123=(
BOUNDED_SURFACE()
B_SPLINE_SURFACE(1,2,((#164282,#164283,#164284),(#164285,#164286,#164287),
(#164288,#164289,#164290)),.UNSPECIFIED.,.F.,.F.,.F.)
B_SPLINE_SURFACE_WITH_KNOTS((2,1,2),(3,3),(0.,0.289681084359921,0.311483587353062),
(0.625066077454535,0.642578551421364),.UNSPECIFIED.)
GEOMETRIC_REPRESENTATION_ITEM()
RATIONAL_B_SPLINE_SURFACE(((0.990621203777021,0.993706096834649,0.999805186472059),
(0.990621203777021,0.993706096834649,0.999805186472059),(0.990621203777021,
0.993706096834649,0.999805186472059)))
REPRESENTATION_ITEM('')
SURFACE()
);
#4124=(
BOUNDED_SURFACE()
B_SPLINE_SURFACE(1,2,((#164292,#164293,#164294),(#164295,#164296,#164297),
(#164298,#164299,#164300)),.UNSPECIFIED.,.F.,.F.,.F.)
B_SPLINE_SURFACE_WITH_KNOTS((2,1,2),(3,3),(0.,0.289807040991592,0.311582168185893),
(0.0909109506295943,0.108084585199971),.UNSPECIFIED.)
GEOMETRIC_REPRESENTATION_ITEM()
RATIONAL_B_SPLINE_SURFACE(((0.990053454406147,0.987313720921968,0.987472672298934),
(0.990053454406147,0.987313720921968,0.987472672298934),(0.990053454406147,
0.987313720921968,0.987472672298934)))
REPRESENTATION_ITEM('')
SURFACE()
);
#4125=(
BOUNDED_SURFACE()
B_SPLINE_SURFACE(1,2,((#164341,#164342,#164343),(#164344,#164345,#164346),
(#164347,#164348,#164349)),.UNSPECIFIED.,.F.,.F.,.F.)
B_SPLINE_SURFACE_WITH_KNOTS((2,1,2),(3,3),(0.,0.28968108435992,0.311483587308824),
(0.625066077454535,0.642578551421363),.UNSPECIFIED.)
GEOMETRIC_REPRESENTATION_ITEM()
RATIONAL_B_SPLINE_SURFACE(((0.990621203777021,0.993706096834649,0.999805186472059),
(0.990621203777021,0.993706096834649,0.999805186472059),(0.990621203777021,
0.993706096834649,0.999805186472059)))
REPRESENTATION_ITEM('')
SURFACE()
);
#4126=(
BOUNDED_SURFACE()
B_SPLINE_SURFACE(1,2,((#164351,#164352,#164353),(#164354,#164355,#164356),
(#164357,#164358,#164359)),.UNSPECIFIED.,.F.,.F.,.F.)
B_SPLINE_SURFACE_WITH_KNOTS((2,1,2),(3,3),(0.,0.289807040991593,0.311582168106922),
(0.0909109506295942,0.10808458519997),.UNSPECIFIED.)
GEOMETRIC_REPRESENTATION_ITEM()
RATIONAL_B_SPLINE_SURFACE(((0.990053454406147,0.987313720921968,0.987472672298934),
(0.990053454406147,0.987313720921968,0.987472672298934),(0.990053454406147,
0.987313720921968,0.987472672298934)))
REPRESENTATION_ITEM('')
SURFACE()
);
#4127=(
BOUNDED_SURFACE()
B_SPLINE_SURFACE(1,2,((#164400,#164401,#164402),(#164403,#164404,#164405),
(#164406,#164407,#164408)),.UNSPECIFIED.,.F.,.F.,.F.)
B_SPLINE_SURFACE_WITH_KNOTS((2,1,2),(3,3),(0.,0.289681084359921,0.31148358700348),
(0.625066077454535,0.642578551421363),.UNSPECIFIED.)
GEOMETRIC_REPRESENTATION_ITEM()
RATIONAL_B_SPLINE_SURFACE(((0.990621203777021,0.993706096834649,0.999805186472059),
(0.990621203777021,0.993706096834649,0.999805186472059),(0.990621203777021,
0.993706096834649,0.999805186472059)))
REPRESENTATION_ITEM('')
SURFACE()
);
#4128=(
BOUNDED_SURFACE()
B_SPLINE_SURFACE(1,2,((#164410,#164411,#164412),(#164413,#164414,#164415),
(#164416,#164417,#164418)),.UNSPECIFIED.,.F.,.F.,.F.)
B_SPLINE_SURFACE_WITH_KNOTS((2,1,2),(3,3),(0.,0.289807040991604,0.311582168205773),
(0.0909109506295943,0.108084585199971),.UNSPECIFIED.)
GEOMETRIC_REPRESENTATION_ITEM()
RATIONAL_B_SPLINE_SURFACE(((0.990053454406147,0.987313720921968,0.987472672298934),
(0.990053454406147,0.987313720921968,0.987472672298934),(0.990053454406147,
0.987313720921968,0.987472672298934)))
REPRESENTATION_ITEM('')
SURFACE()
);
#4129=(
BOUNDED_SURFACE()
B_SPLINE_SURFACE(1,2,((#164459,#164460,#164461),(#164462,#164463,#164464),
(#164465,#164466,#164467)),.UNSPECIFIED.,.F.,.F.,.F.)
B_SPLINE_SURFACE_WITH_KNOTS((2,1,2),(3,3),(0.,0.289681084359918,0.311483587238885),
(0.625066077454535,0.642578551421363),.UNSPECIFIED.)
GEOMETRIC_REPRESENTATION_ITEM()
RATIONAL_B_SPLINE_SURFACE(((0.990621203777021,0.993706096834649,0.999805186472059),
(0.990621203777021,0.993706096834649,0.999805186472059),(0.990621203777021,
0.993706096834649,0.999805186472059)))
REPRESENTATION_ITEM('')
SURFACE()
);
#4130=(
BOUNDED_SURFACE()
B_SPLINE_SURFACE(1,2,((#164469,#164470,#164471),(#164472,#164473,#164474),
(#164475,#164476,#164477)),.UNSPECIFIED.,.F.,.F.,.F.)
B_SPLINE_SURFACE_WITH_KNOTS((2,1,2),(3,3),(0.,0.289807040992979,0.311582168660763),
(0.0909109506295943,0.10808458519997),.UNSPECIFIED.)
GEOMETRIC_REPRESENTATION_ITEM()
RATIONAL_B_SPLINE_SURFACE(((0.990053454406147,0.987313720921968,0.987472672298934),
(0.990053454406147,0.987313720921968,0.987472672298934),(0.990053454406147,
0.987313720921968,0.987472672298934)))
REPRESENTATION_ITEM('')
SURFACE()
);
#4131=(
BOUNDED_SURFACE()
B_SPLINE_SURFACE(1,2,((#164518,#164519,#164520),(#164521,#164522,#164523),
(#164524,#164525,#164526)),.UNSPECIFIED.,.F.,.F.,.F.)
B_SPLINE_SURFACE_WITH_KNOTS((2,1,2),(3,3),(0.,0.289681084360127,0.31148358675689),
(0.625066077454535,0.642578551421363),.UNSPECIFIED.)
GEOMETRIC_REPRESENTATION_ITEM()
RATIONAL_B_SPLINE_SURFACE(((0.990621203777021,0.993706096834649,0.999805186472059),
(0.990621203777021,0.993706096834649,0.999805186472059),(0.990621203777021,
0.993706096834649,0.999805186472059)))
REPRESENTATION_ITEM('')
SURFACE()
);
#4132=(
BOUNDED_SURFACE()
B_SPLINE_SURFACE(1,2,((#164528,#164529,#164530),(#164531,#164532,#164533),
(#164534,#164535,#164536)),.UNSPECIFIED.,.F.,.F.,.F.)
B_SPLINE_SURFACE_WITH_KNOTS((2,1,2),(3,3),(0.,0.289807040991931,0.311582168479859),
(0.0909109506295922,0.108084585199971),.UNSPECIFIED.)
GEOMETRIC_REPRESENTATION_ITEM()
RATIONAL_B_SPLINE_SURFACE(((0.990053454406148,0.987313720921968,0.987472672298933),
(0.990053454406148,0.987313720921968,0.987472672298933),(0.990053454406148,
0.987313720921968,0.987472672298933)))
REPRESENTATION_ITEM('')
SURFACE()
);
#4133=(
BOUNDED_SURFACE()
B_SPLINE_SURFACE(1,2,((#164577,#164578,#164579),(#164580,#164581,#164582),
(#164583,#164584,#164585)),.UNSPECIFIED.,.F.,.F.,.F.)
B_SPLINE_SURFACE_WITH_KNOTS((2,1,2),(3,3),(0.,0.289681084359922,0.311483586918173),
(0.625066077454535,0.642578551421363),.UNSPECIFIED.)
GEOMETRIC_REPRESENTATION_ITEM()
RATIONAL_B_SPLINE_SURFACE(((0.990621203777021,0.993706096834649,0.999805186472059),
(0.990621203777021,0.993706096834649,0.999805186472059),(0.990621203777021,
0.993706096834649,0.999805186472059)))
REPRESENTATION_ITEM('')
SURFACE()
);
#4134=(
BOUNDED_SURFACE()
B_SPLINE_SURFACE(1,2,((#164587,#164588,#164589),(#164590,#164591,#164592),
(#164593,#164594,#164595)),.UNSPECIFIED.,.F.,.F.,.F.)
B_SPLINE_SURFACE_WITH_KNOTS((2,1,2),(3,3),(0.,0.289807040991561,0.311582168314643),
(0.0909109506295943,0.108084585199971),.UNSPECIFIED.)
GEOMETRIC_REPRESENTATION_ITEM()
RATIONAL_B_SPLINE_SURFACE(((0.990053454406147,0.987313720921968,0.987472672298934),
(0.990053454406147,0.987313720921968,0.987472672298934),(0.990053454406147,
0.987313720921968,0.987472672298934)))
REPRESENTATION_ITEM('')
SURFACE()
);
#4135=(
BOUNDED_SURFACE()
B_SPLINE_SURFACE(1,2,((#164636,#164637,#164638),(#164639,#164640,#164641),
(#164642,#164643,#164644)),.UNSPECIFIED.,.F.,.F.,.F.)
B_SPLINE_SURFACE_WITH_KNOTS((2,1,2),(3,3),(0.,0.289681084359922,0.311483586948988),
(0.625066077454535,0.642578551421363),.UNSPECIFIED.)
GEOMETRIC_REPRESENTATION_ITEM()
RATIONAL_B_SPLINE_SURFACE(((0.990621203777021,0.993706096834649,0.999805186472059),
(0.990621203777021,0.993706096834649,0.999805186472059),(0.990621203777021,
0.993706096834649,0.999805186472059)))
REPRESENTATION_ITEM('')
SURFACE()
);
#4136=(
BOUNDED_SURFACE()
B_SPLINE_SURFACE(1,2,((#164646,#164647,#164648),(#164649,#164650,#164651),
(#164652,#164653,#164654)),.UNSPECIFIED.,.F.,.F.,.F.)
B_SPLINE_SURFACE_WITH_KNOTS((2,1,2),(3,3),(0.,0.289807040991561,0.311582167860186),
(0.0909109506295943,0.108084585199971),.UNSPECIFIED.)
GEOMETRIC_REPRESENTATION_ITEM()
RATIONAL_B_SPLINE_SURFACE(((0.990053454406147,0.987313720921968,0.987472672298934),
(0.990053454406147,0.987313720921968,0.987472672298934),(0.990053454406147,
0.987313720921968,0.987472672298934)))
REPRESENTATION_ITEM('')
SURFACE()
);
#4137=(
BOUNDED_SURFACE()
B_SPLINE_SURFACE(1,2,((#164662,#164663,#164664),(#164665,#164666,#164667),
(#164668,#164669,#164670)),.UNSPECIFIED.,.F.,.F.,.F.)
B_SPLINE_SURFACE_WITH_KNOTS((2,1,2),(3,3),(0.,0.289681084359917,0.311483587097765),
(0.625066077454535,0.642578551421363),.UNSPECIFIED.)
GEOMETRIC_REPRESENTATION_ITEM()
RATIONAL_B_SPLINE_SURFACE(((0.990621203777021,0.993706096834649,0.999805186472059),
(0.990621203777021,0.993706096834649,0.999805186472059),(0.990621203777021,
0.993706096834649,0.999805186472059)))
REPRESENTATION_ITEM('')
SURFACE()
);
#4138=(
BOUNDED_SURFACE()
B_SPLINE_SURFACE(1,2,((#164672,#164673,#164674,#164675,#164676,#164677,
#164678),(#164679,#164680,#164681,#164682,#164683,#164684,#164685)),
 .UNSPECIFIED.,.F.,.F.,.F.)
B_SPLINE_SURFACE_WITH_KNOTS((2,2),(3,2,2,3),(0.788462675553386,1.),(0.642404283483305,
0.642578551421363,0.642857142857143,0.660005345227123),.UNSPECIFIED.)
GEOMETRIC_REPRESENTATION_ITEM()
RATIONAL_B_SPLINE_SURFACE(((0.999805186472058,0.999805186472058,0.999805186472058,
0.999902211834794,1.,0.993980822699584,0.990851751371721),(0.999805186472058,
0.999805186472058,0.999805186472058,0.999902211834794,1.,0.993980822699584,
0.990851751371721)))
REPRESENTATION_ITEM('')
SURFACE()
);
#4139=(
BOUNDED_SURFACE()
B_SPLINE_SURFACE(1,2,((#164689,#164690,#164691,#164692,#164693),(#164694,
#164695,#164696,#164697,#164698)),.UNSPECIFIED.,.F.,.F.,.F.)
B_SPLINE_SURFACE_WITH_KNOTS((2,2),(3,2,3),(0.788554614412989,1.),(0.0735508106170104,
0.0909109506295944,0.0910845520297202),.UNSPECIFIED.)
GEOMETRIC_REPRESENTATION_ITEM()
RATIONAL_B_SPLINE_SURFACE(((0.998554414400487,0.992822941359396,0.990053454406147,
0.990053454406147,0.990053454406147),(0.998554414400487,0.992822941359396,
0.990053454406147,0.990053454406147,0.990053454406147)))
REPRESENTATION_ITEM('')
SURFACE()
);
#4140=(
BOUNDED_SURFACE()
B_SPLINE_SURFACE(1,2,((#164700,#164701,#164702,#164703,#164704,#164705,
#164706),(#164707,#164708,#164709,#164710,#164711,#164712,#164713),(#164714,
#164715,#164716,#164717,#164718,#164719,#164720)),.UNSPECIFIED.,.F.,.F.,
 .F.)
B_SPLINE_SURFACE_WITH_KNOTS((2,1,2),(3,2,2,3),(0.788462675553383,1.,1.00211537324447),
(0.642404283483302,0.642578551421363,0.642857142857143,0.660005345227478),
 .UNSPECIFIED.)
GEOMETRIC_REPRESENTATION_ITEM()
RATIONAL_B_SPLINE_SURFACE(((0.999805186472058,0.999805186472058,0.999805186472058,
0.999902211834794,1.,0.993980822699459,0.990851751371591),(0.999805186472058,
0.999805186472058,0.999805186472058,0.999902211834794,1.,0.993980822699459,
0.990851751371591),(0.999805186472058,0.999805186472058,0.999805186472058,
0.999902211834794,1.,0.993980822699459,0.990851751371591)))
REPRESENTATION_ITEM('')
SURFACE()
);
#4141=(
BOUNDED_SURFACE()
B_SPLINE_SURFACE(1,2,((#164727,#164728,#164729,#164730,#164731),(#164732,
#164733,#164734,#164735,#164736)),.UNSPECIFIED.,.F.,.F.,.F.)
B_SPLINE_SURFACE_WITH_KNOTS((2,2),(3,2,3),(0.788554614412989,1.00000106324376),
(0.0735508106169813,0.0909109506295944,0.0910845520297205),
 .UNSPECIFIED.)
GEOMETRIC_REPRESENTATION_ITEM()
RATIONAL_B_SPLINE_SURFACE(((0.998554414400506,0.992822941359401,0.990053454406147,
0.990053454406147,0.990053454406147),(0.998554414400506,0.992822941359401,
0.990053454406147,0.990053454406147,0.990053454406147)))
REPRESENTATION_ITEM('')
SURFACE()
);
#4142=(
BOUNDED_SURFACE()
B_SPLINE_SURFACE(1,2,((#164738,#164739,#164740,#164741,#164742,#164743,
#164744),(#164745,#164746,#164747,#164748,#164749,#164750,#164751)),
 .UNSPECIFIED.,.F.,.F.,.F.)
B_SPLINE_SURFACE_WITH_KNOTS((2,2),(3,2,2,3),(0.78846267555338,1.),(0.642404283483302,
0.642578551421363,0.642857142857143,0.660005345227478),.UNSPECIFIED.)
GEOMETRIC_REPRESENTATION_ITEM()
RATIONAL_B_SPLINE_SURFACE(((0.999805186472058,0.999805186472058,0.999805186472058,
0.999902211834794,1.,0.993980822699459,0.990851751371591),(0.999805186472058,
0.999805186472058,0.999805186472058,0.999902211834794,1.,0.993980822699459,
0.990851751371591)))
REPRESENTATION_ITEM('')
SURFACE()
);
#4143=(
BOUNDED_SURFACE()
B_SPLINE_SURFACE(1,2,((#164755,#164756,#164757,#164758,#164759),(#164760,
#164761,#164762,#164763,#164764)),.UNSPECIFIED.,.F.,.F.,.F.)
B_SPLINE_SURFACE_WITH_KNOTS((2,2),(3,2,3),(0.788554614412984,1.00000106320563),
(0.0735508106171715,0.0909109506295945,0.0910845520297187),
 .UNSPECIFIED.)
GEOMETRIC_REPRESENTATION_ITEM()
RATIONAL_B_SPLINE_SURFACE(((0.99855441440038,0.99282294135937,0.990053454406147,
0.990053454406147,0.990053454406147),(0.99855441440038,0.99282294135937,
0.990053454406147,0.990053454406147,0.990053454406147)))
REPRESENTATION_ITEM('')
SURFACE()
);
#4144=(
BOUNDED_SURFACE()
B_SPLINE_SURFACE(1,2,((#164766,#164767,#164768,#164769,#164770,#164771,
#164772),(#164773,#164774,#164775,#164776,#164777,#164778,#164779)),
 .UNSPECIFIED.,.F.,.F.,.F.)
B_SPLINE_SURFACE_WITH_KNOTS((2,2),(3,2,2,3),(0.788462675553387,1.),(0.642404283483302,
0.642578551421363,0.642857142857143,0.660005345227478),.UNSPECIFIED.)
GEOMETRIC_REPRESENTATION_ITEM()
RATIONAL_B_SPLINE_SURFACE(((0.999805186472058,0.999805186472058,0.999805186472058,
0.999902211834794,1.,0.993980822699459,0.990851751371592),(0.999805186472058,
0.999805186472058,0.999805186472058,0.999902211834794,1.,0.993980822699459,
0.990851751371592)))
REPRESENTATION_ITEM('')
SURFACE()
);
#4145=(
BOUNDED_SURFACE()
B_SPLINE_SURFACE(1,2,((#164783,#164784,#164785,#164786,#164787),(#164788,
#164789,#164790,#164791,#164792)),.UNSPECIFIED.,.F.,.F.,.F.)
B_SPLINE_SURFACE_WITH_KNOTS((2,2),(3,2,3),(0.788554614412988,1.),(0.0735508106173321,
0.0909109506295944,0.091084552029717),.UNSPECIFIED.)
GEOMETRIC_REPRESENTATION_ITEM()
RATIONAL_B_SPLINE_SURFACE(((0.998554414400274,0.992822941359345,0.990053454406147,
0.990053454406147,0.990053454406147),(0.998554414400274,0.992822941359345,
0.990053454406147,0.990053454406147,0.990053454406147)))
REPRESENTATION_ITEM('')
SURFACE()
);
#4146=(
BOUNDED_SURFACE()
B_SPLINE_SURFACE(1,2,((#164794,#164795,#164796,#164797,#164798,#164799,
#164800),(#164801,#164802,#164803,#164804,#164805,#164806,#164807)),
 .UNSPECIFIED.,.F.,.F.,.F.)
B_SPLINE_SURFACE_WITH_KNOTS((2,2),(3,2,2,3),(0.78846267555338,1.),(0.642404283483302,
0.642578551421363,0.642857142857143,0.660005345227478),.UNSPECIFIED.)
GEOMETRIC_REPRESENTATION_ITEM()
RATIONAL_B_SPLINE_SURFACE(((0.999805186472058,0.999805186472058,0.999805186472058,
0.999902211834794,1.,0.993980822699459,0.990851751371591),(0.999805186472058,
0.999805186472058,0.999805186472058,0.999902211834794,1.,0.993980822699459,
0.990851751371591)))
REPRESENTATION_ITEM('')
SURFACE()
);
#4147=(
BOUNDED_SURFACE()
B_SPLINE_SURFACE(1,2,((#164811,#164812,#164813,#164814,#164815),(#164816,
#164817,#164818,#164819,#164820)),.UNSPECIFIED.,.F.,.F.,.F.)
B_SPLINE_SURFACE_WITH_KNOTS((2,2),(3,2,3),(0.788554614412994,1.00000106310531),
(0.073550810617453,0.0909109506295934,0.0910845520297148),.UNSPECIFIED.)
GEOMETRIC_REPRESENTATION_ITEM()
RATIONAL_B_SPLINE_SURFACE(((0.998554414400194,0.992822941359326,0.990053454406148,
0.990053454406148,0.990053454406148),(0.998554414400194,0.992822941359326,
0.990053454406148,0.990053454406148,0.990053454406148)))
REPRESENTATION_ITEM('')
SURFACE()
);
#4148=(
BOUNDED_SURFACE()
B_SPLINE_SURFACE(1,2,((#164822,#164823,#164824,#164825,#164826,#164827,
#164828),(#164829,#164830,#164831,#164832,#164833,#164834,#164835)),
 .UNSPECIFIED.,.F.,.F.,.F.)
B_SPLINE_SURFACE_WITH_KNOTS((2,2),(3,2,2,3),(0.788462675553394,1.),(0.642404283483303,
0.642578551421364,0.642857142857143,0.660005345227479),.UNSPECIFIED.)
GEOMETRIC_REPRESENTATION_ITEM()
RATIONAL_B_SPLINE_SURFACE(((0.999805186472059,0.999805186472059,0.999805186472059,
0.999902211834795,1.,0.993980822699459,0.990851751371591),(0.999805186472059,
0.999805186472059,0.999805186472059,0.999902211834795,1.,0.993980822699459,
0.990851751371591)))
REPRESENTATION_ITEM('')
SURFACE()
);
#4149=(
BOUNDED_SURFACE()
B_SPLINE_SURFACE(1,2,((#164839,#164840,#164841,#164842,#164843),(#164844,
#164845,#164846,#164847,#164848)),.UNSPECIFIED.,.F.,.F.,.F.)
B_SPLINE_SURFACE_WITH_KNOTS((2,2),(3,2,3),(0.788554614412994,1.00000106321494),
(0.0735508106174518,0.0909109506295933,0.0910845520297147),
 .UNSPECIFIED.)
GEOMETRIC_REPRESENTATION_ITEM()
RATIONAL_B_SPLINE_SURFACE(((0.998554414400195,0.992822941359326,0.990053454406148,
0.990053454406148,0.990053454406148),(0.998554414400195,0.992822941359326,
0.990053454406148,0.990053454406148,0.990053454406148)))
REPRESENTATION_ITEM('')
SURFACE()
);
#4150=(
BOUNDED_SURFACE()
B_SPLINE_SURFACE(1,2,((#164850,#164851,#164852,#164853,#164854,#164855,
#164856),(#164857,#164858,#164859,#164860,#164861,#164862,#164863)),
 .UNSPECIFIED.,.F.,.F.,.F.)
B_SPLINE_SURFACE_WITH_KNOTS((2,2),(3,2,2,3),(0.78846267555339,1.),(0.642404283483303,
0.642578551421364,0.642857142857143,0.660005345227479),.UNSPECIFIED.)
GEOMETRIC_REPRESENTATION_ITEM()
RATIONAL_B_SPLINE_SURFACE(((0.999805186472059,0.999805186472059,0.999805186472059,
0.999902211834795,1.,0.993980822699459,0.990851751371591),(0.999805186472059,
0.999805186472059,0.999805186472059,0.999902211834795,1.,0.993980822699459,
0.990851751371591)))
REPRESENTATION_ITEM('')
SURFACE()
);
#4151=(
BOUNDED_SURFACE()
B_SPLINE_SURFACE(1,2,((#164867,#164868,#164869,#164870,#164871),(#164872,
#164873,#164874,#164875,#164876)),.UNSPECIFIED.,.F.,.F.,.F.)
B_SPLINE_SURFACE_WITH_KNOTS((2,2),(3,2,3),(0.788554614412996,1.00000106338885),
(0.0735508106174519,0.0909109506295934,0.0910845520297148),
 .UNSPECIFIED.)
GEOMETRIC_REPRESENTATION_ITEM()
RATIONAL_B_SPLINE_SURFACE(((0.998554414400195,0.992822941359326,0.990053454406148,
0.990053454406148,0.990053454406148),(0.998554414400195,0.992822941359326,
0.990053454406148,0.990053454406148,0.990053454406148)))
REPRESENTATION_ITEM('')
SURFACE()
);
#4152=(
BOUNDED_SURFACE()
B_SPLINE_SURFACE(1,2,((#164878,#164879,#164880,#164881,#164882,#164883,
#164884),(#164885,#164886,#164887,#164888,#164889,#164890,#164891),(#164892,
#164893,#164894,#164895,#164896,#164897,#164898)),.UNSPECIFIED.,.F.,.F.,
 .F.)
B_SPLINE_SURFACE_WITH_KNOTS((2,1,2),(3,2,2,3),(0.788462675553393,1.,1.00211537324447),
(0.642404283483303,0.642578551421364,0.642857142857143,0.660005345227479),
 .UNSPECIFIED.)
GEOMETRIC_REPRESENTATION_ITEM()
RATIONAL_B_SPLINE_SURFACE(((0.999805186472059,0.999805186472059,0.999805186472059,
0.999902211834795,1.,0.993980822699459,0.990851751371591),(0.999805186472059,
0.999805186472059,0.999805186472059,0.999902211834795,1.,0.993980822699459,
0.990851751371591),(0.999805186472059,0.999805186472059,0.999805186472059,
0.999902211834795,1.,0.993980822699459,0.990851751371591)))
REPRESENTATION_ITEM('')
SURFACE()
);
#4153=(
BOUNDED_SURFACE()
B_SPLINE_SURFACE(1,2,((#164905,#164906,#164907,#164908,#164909),(#164910,
#164911,#164912,#164913,#164914)),.UNSPECIFIED.,.F.,.F.,.F.)
B_SPLINE_SURFACE_WITH_KNOTS((2,2),(3,2,3),(0.788554614412992,1.),(0.0735508106174519,
0.0909109506295934,0.0910845520297148),.UNSPECIFIED.)
GEOMETRIC_REPRESENTATION_ITEM()
RATIONAL_B_SPLINE_SURFACE(((0.998554414400195,0.992822941359326,0.990053454406148,
0.990053454406148,0.990053454406148),(0.998554414400195,0.992822941359326,
0.990053454406148,0.990053454406148,0.990053454406148)))
REPRESENTATION_ITEM('')
SURFACE()
);
#4154=(
BOUNDED_SURFACE()
B_SPLINE_SURFACE(1,2,((#164916,#164917,#164918,#164919,#164920,#164921,
#164922),(#164923,#164924,#164925,#164926,#164927,#164928,#164929)),
 .UNSPECIFIED.,.F.,.F.,.F.)
B_SPLINE_SURFACE_WITH_KNOTS((2,2),(3,2,2,3),(0.788462675553392,1.),(0.642404283483303,
0.642578551421364,0.642857142857143,0.660005345227479),.UNSPECIFIED.)
GEOMETRIC_REPRESENTATION_ITEM()
RATIONAL_B_SPLINE_SURFACE(((0.999805186472059,0.999805186472059,0.999805186472059,
0.999902211834795,1.,0.993980822699459,0.990851751371591),(0.999805186472059,
0.999805186472059,0.999805186472059,0.999902211834795,1.,0.993980822699459,
0.990851751371591)))
REPRESENTATION_ITEM('')
SURFACE()
);
#4155=(
BOUNDED_SURFACE()
B_SPLINE_SURFACE(1,2,((#164933,#164934,#164935,#164936,#164937),(#164938,
#164939,#164940,#164941,#164942)),.UNSPECIFIED.,.F.,.F.,.F.)
B_SPLINE_SURFACE_WITH_KNOTS((2,2),(3,2,3),(0.788554614412995,1.00000106564244),
(0.0735508106174519,0.0909109506295934,0.0910845520297148),
 .UNSPECIFIED.)
GEOMETRIC_REPRESENTATION_ITEM()
RATIONAL_B_SPLINE_SURFACE(((0.998554414400195,0.992822941359326,0.990053454406148,
0.990053454406148,0.990053454406148),(0.998554414400195,0.992822941359326,
0.990053454406148,0.990053454406148,0.990053454406148)))
REPRESENTATION_ITEM('')
SURFACE()
);
#4156=(
BOUNDED_SURFACE()
B_SPLINE_SURFACE(1,2,((#164944,#164945,#164946,#164947,#164948,#164949,
#164950),(#164951,#164952,#164953,#164954,#164955,#164956,#164957)),
 .UNSPECIFIED.,.F.,.F.,.F.)
B_SPLINE_SURFACE_WITH_KNOTS((2,2),(3,2,2,3),(0.78846267555339,1.),(0.642404283483303,
0.642578551421364,0.642857142857143,0.660005345227479),.UNSPECIFIED.)
GEOMETRIC_REPRESENTATION_ITEM()
RATIONAL_B_SPLINE_SURFACE(((0.999805186472059,0.999805186472059,0.999805186472059,
0.999902211834795,1.,0.993980822699459,0.990851751371591),(0.999805186472059,
0.999805186472059,0.999805186472059,0.999902211834795,1.,0.993980822699459,
0.990851751371591)))
REPRESENTATION_ITEM('')
SURFACE()
);
#4157=(
BOUNDED_SURFACE()
B_SPLINE_SURFACE(1,2,((#164961,#164962,#164963,#164964,#164965),(#164966,
#164967,#164968,#164969,#164970)),.UNSPECIFIED.,.F.,.F.,.F.)
B_SPLINE_SURFACE_WITH_KNOTS((2,2),(3,2,3),(0.788554614412993,1.00000106557312),
(0.0735508106174519,0.0909109506295933,0.0910845520297147),
 .UNSPECIFIED.)
GEOMETRIC_REPRESENTATION_ITEM()
RATIONAL_B_SPLINE_SURFACE(((0.998554414400195,0.992822941359326,0.990053454406148,
0.990053454406148,0.990053454406148),(0.998554414400195,0.992822941359326,
0.990053454406148,0.990053454406148,0.990053454406148)))
REPRESENTATION_ITEM('')
SURFACE()
);
#4158=(
BOUNDED_SURFACE()
B_SPLINE_SURFACE(1,2,((#164972,#164973,#164974,#164975,#164976,#164977,
#164978),(#164979,#164980,#164981,#164982,#164983,#164984,#164985)),
 .UNSPECIFIED.,.F.,.F.,.F.)
B_SPLINE_SURFACE_WITH_KNOTS((2,2),(3,2,2,3),(0.788462675553395,1.),(0.642404283483303,
0.642578551421364,0.642857142857143,0.660005345227479),.UNSPECIFIED.)
GEOMETRIC_REPRESENTATION_ITEM()
RATIONAL_B_SPLINE_SURFACE(((0.999805186472059,0.999805186472059,0.999805186472059,
0.999902211834795,1.,0.993980822699459,0.990851751371591),(0.999805186472059,
0.999805186472059,0.999805186472059,0.999902211834795,1.,0.993980822699459,
0.990851751371591)))
REPRESENTATION_ITEM('')
SURFACE()
);
#4159=(
BOUNDED_SURFACE()
B_SPLINE_SURFACE(1,2,((#164989,#164990,#164991,#164992,#164993),(#164994,
#164995,#164996,#164997,#164998)),.UNSPECIFIED.,.F.,.F.,.F.)
B_SPLINE_SURFACE_WITH_KNOTS((2,2),(3,2,3),(0.788554614412993,1.),(0.0735508106174519,
0.0909109506295934,0.0910845520297148),.UNSPECIFIED.)
GEOMETRIC_REPRESENTATION_ITEM()
RATIONAL_B_SPLINE_SURFACE(((0.998554414400195,0.992822941359326,0.990053454406147,
0.990053454406147,0.990053454406147),(0.998554414400195,0.992822941359326,
0.990053454406147,0.990053454406147,0.990053454406147)))
REPRESENTATION_ITEM('')
SURFACE()
);
#4160=(
BOUNDED_SURFACE()
B_SPLINE_SURFACE(1,2,((#165000,#165001,#165002,#165003,#165004,#165005,
#165006),(#165007,#165008,#165009,#165010,#165011,#165012,#165013)),
 .UNSPECIFIED.,.F.,.F.,.F.)
B_SPLINE_SURFACE_WITH_KNOTS((2,2),(3,2,2,3),(0.788462675553396,1.),(0.642404283483303,
0.642578551421364,0.642857142857143,0.660005345227478),.UNSPECIFIED.)
GEOMETRIC_REPRESENTATION_ITEM()
RATIONAL_B_SPLINE_SURFACE(((0.999805186472059,0.999805186472059,0.999805186472059,
0.999902211834795,1.,0.993980822699459,0.990851751371591),(0.999805186472059,
0.999805186472059,0.999805186472059,0.999902211834795,1.,0.993980822699459,
0.990851751371591)))
REPRESENTATION_ITEM('')
SURFACE()
);
#4161=(
BOUNDED_SURFACE()
B_SPLINE_SURFACE(1,2,((#165017,#165018,#165019,#165020,#165021),(#165022,
#165023,#165024,#165025,#165026)),.UNSPECIFIED.,.F.,.F.,.F.)
B_SPLINE_SURFACE_WITH_KNOTS((2,2),(3,2,3),(0.788554614412983,1.00000106566568),
(0.0735508106174511,0.0909109506295945,0.0910845520297159),
 .UNSPECIFIED.)
GEOMETRIC_REPRESENTATION_ITEM()
RATIONAL_B_SPLINE_SURFACE(((0.998554414400196,0.992822941359326,0.990053454406147,
0.990053454406147,0.990053454406147),(0.998554414400196,0.992822941359326,
0.990053454406147,0.990053454406147,0.990053454406147)))
REPRESENTATION_ITEM('')
SURFACE()
);
#4162=(
BOUNDED_SURFACE()
B_SPLINE_SURFACE(1,2,((#165028,#165029,#165030,#165031,#165032,#165033,
#165034),(#165035,#165036,#165037,#165038,#165039,#165040,#165041),(#165042,
#165043,#165044,#165045,#165046,#165047,#165048)),.UNSPECIFIED.,.F.,.F.,
 .F.)
B_SPLINE_SURFACE_WITH_KNOTS((2,1,2),(3,2,2,3),(0.788462675553396,1.,1.00211537324447),
(0.642404283483303,0.642578551421364,0.642857142857143,0.660005345227479),
 .UNSPECIFIED.)
GEOMETRIC_REPRESENTATION_ITEM()
RATIONAL_B_SPLINE_SURFACE(((0.999805186472059,0.999805186472059,0.999805186472059,
0.999902211834795,1.,0.993980822699459,0.990851751371591),(0.999805186472059,
0.999805186472059,0.999805186472059,0.999902211834795,1.,0.993980822699459,
0.990851751371591),(0.999805186472059,0.999805186472059,0.999805186472059,
0.999902211834795,1.,0.993980822699459,0.990851751371591)))
REPRESENTATION_ITEM('')
SURFACE()
);
#4163=(
BOUNDED_SURFACE()
B_SPLINE_SURFACE(1,2,((#165055,#165056,#165057,#165058,#165059),(#165060,
#165061,#165062,#165063,#165064)),.UNSPECIFIED.,.F.,.F.,.F.)
B_SPLINE_SURFACE_WITH_KNOTS((2,2),(3,2,3),(0.788554614412996,1.),(0.0735508106174261,
0.0909109506295933,0.091084552029715),.UNSPECIFIED.)
GEOMETRIC_REPRESENTATION_ITEM()
RATIONAL_B_SPLINE_SURFACE(((0.998554414400212,0.99282294135933,0.990053454406147,
0.990053454406147,0.990053454406147),(0.998554414400212,0.99282294135933,
0.990053454406147,0.990053454406147,0.990053454406147)))
REPRESENTATION_ITEM('')
SURFACE()
);
#4164=(
BOUNDED_SURFACE()
B_SPLINE_SURFACE(1,2,((#165066,#165067,#165068,#165069,#165070,#165071,
#165072),(#165073,#165074,#165075,#165076,#165077,#165078,#165079)),
 .UNSPECIFIED.,.F.,.F.,.F.)
B_SPLINE_SURFACE_WITH_KNOTS((2,2),(3,2,2,3),(0.788462675553396,1.),(0.642404283483303,
0.642578551421364,0.642857142857143,0.660005345227479),.UNSPECIFIED.)
GEOMETRIC_REPRESENTATION_ITEM()
RATIONAL_B_SPLINE_SURFACE(((0.999805186472059,0.999805186472059,0.999805186472059,
0.999902211834795,1.,0.993980822699459,0.990851751371591),(0.999805186472059,
0.999805186472059,0.999805186472059,0.999902211834795,1.,0.993980822699459,
0.990851751371591)))
REPRESENTATION_ITEM('')
SURFACE()
);
#4165=(
BOUNDED_SURFACE()
B_SPLINE_SURFACE(1,2,((#165083,#165084,#165085,#165086,#165087),(#165088,
#165089,#165090,#165091,#165092)),.UNSPECIFIED.,.F.,.F.,.F.)
B_SPLINE_SURFACE_WITH_KNOTS((2,2),(3,2,3),(0.788554614412993,1.00000106321825),
(0.0735508106174518,0.0909109506295934,0.0910845520297148),
 .UNSPECIFIED.)
GEOMETRIC_REPRESENTATION_ITEM()
RATIONAL_B_SPLINE_SURFACE(((0.998554414400195,0.992822941359326,0.990053454406148,
0.990053454406148,0.990053454406148),(0.998554414400195,0.992822941359326,
0.990053454406148,0.990053454406148,0.990053454406148)))
REPRESENTATION_ITEM('')
SURFACE()
);
#4166=(
BOUNDED_SURFACE()
B_SPLINE_SURFACE(1,2,((#165094,#165095,#165096,#165097,#165098,#165099,
#165100),(#165101,#165102,#165103,#165104,#165105,#165106,#165107)),
 .UNSPECIFIED.,.F.,.F.,.F.)
B_SPLINE_SURFACE_WITH_KNOTS((2,2),(3,2,2,3),(0.788462675553389,1.),(0.642404283483303,
0.642578551421364,0.642857142857143,0.660005345227479),.UNSPECIFIED.)
GEOMETRIC_REPRESENTATION_ITEM()
RATIONAL_B_SPLINE_SURFACE(((0.999805186472059,0.999805186472059,0.999805186472059,
0.999902211834795,1.,0.993980822699459,0.990851751371591),(0.999805186472059,
0.999805186472059,0.999805186472059,0.999902211834795,1.,0.993980822699459,
0.990851751371591)))
REPRESENTATION_ITEM('')
SURFACE()
);
#4167=(
BOUNDED_SURFACE()
B_SPLINE_SURFACE(1,2,((#165111,#165112,#165113,#165114,#165115),(#165116,
#165117,#165118,#165119,#165120)),.UNSPECIFIED.,.F.,.F.,.F.)
B_SPLINE_SURFACE_WITH_KNOTS((2,2),(3,2,3),(0.788554614412994,1.),(0.0735508106174519,
0.0909109506295933,0.0910845520297147),.UNSPECIFIED.)
GEOMETRIC_REPRESENTATION_ITEM()
RATIONAL_B_SPLINE_SURFACE(((0.998554414400195,0.992822941359326,0.990053454406147,
0.990053454406147,0.990053454406147),(0.998554414400195,0.992822941359326,
0.990053454406147,0.990053454406147,0.990053454406147)))
REPRESENTATION_ITEM('')
SURFACE()
);
#4168=(
BOUNDED_SURFACE()
B_SPLINE_SURFACE(1,2,((#165122,#165123,#165124,#165125,#165126,#165127,
#165128),(#165129,#165130,#165131,#165132,#165133,#165134,#165135),(#165136,
#165137,#165138,#165139,#165140,#165141,#165142)),.UNSPECIFIED.,.F.,.F.,
 .F.)
B_SPLINE_SURFACE_WITH_KNOTS((2,1,2),(3,2,2,3),(0.78846267555339,1.,1.00211537324447),
(0.642404283483303,0.642578551421364,0.642857142857143,0.660005345227479),
 .UNSPECIFIED.)
GEOMETRIC_REPRESENTATION_ITEM()
RATIONAL_B_SPLINE_SURFACE(((0.999805186472059,0.999805186472059,0.999805186472059,
0.999902211834795,1.,0.993980822699459,0.990851751371591),(0.999805186472059,
0.999805186472059,0.999805186472059,0.999902211834795,1.,0.993980822699459,
0.990851751371591),(0.999805186472059,0.999805186472059,0.999805186472059,
0.999902211834795,1.,0.993980822699459,0.990851751371591)))
REPRESENTATION_ITEM('')
SURFACE()
);
#4169=(
BOUNDED_SURFACE()
B_SPLINE_SURFACE(1,2,((#165149,#165150,#165151,#165152,#165153),(#165154,
#165155,#165156,#165157,#165158)),.UNSPECIFIED.,.F.,.F.,.F.)
B_SPLINE_SURFACE_WITH_KNOTS((2,2),(3,2,3),(0.788554614412998,1.),(0.0735508106174519,
0.0909109506295934,0.0910845520297148),.UNSPECIFIED.)
GEOMETRIC_REPRESENTATION_ITEM()
RATIONAL_B_SPLINE_SURFACE(((0.998554414400195,0.992822941359326,0.990053454406148,
0.990053454406148,0.990053454406148),(0.998554414400195,0.992822941359326,
0.990053454406148,0.990053454406148,0.990053454406148)))
REPRESENTATION_ITEM('')
SURFACE()
);
#4170=(
BOUNDED_SURFACE()
B_SPLINE_SURFACE(1,2,((#165160,#165161,#165162,#165163,#165164,#165165,
#165166),(#165167,#165168,#165169,#165170,#165171,#165172,#165173)),
 .UNSPECIFIED.,.F.,.F.,.F.)
B_SPLINE_SURFACE_WITH_KNOTS((2,2),(3,2,2,3),(0.788462675553395,1.),(0.642404283483303,
0.642578551421364,0.642857142857143,0.660005345227479),.UNSPECIFIED.)
GEOMETRIC_REPRESENTATION_ITEM()
RATIONAL_B_SPLINE_SURFACE(((0.999805186472059,0.999805186472059,0.999805186472059,
0.999902211834795,1.,0.993980822699459,0.990851751371591),(0.999805186472059,
0.999805186472059,0.999805186472059,0.999902211834795,1.,0.993980822699459,
0.990851751371591)))
REPRESENTATION_ITEM('')
SURFACE()
);
#4171=(
BOUNDED_SURFACE()
B_SPLINE_SURFACE(1,2,((#165177,#165178,#165179,#165180,#165181),(#165182,
#165183,#165184,#165185,#165186)),.UNSPECIFIED.,.F.,.F.,.F.)
B_SPLINE_SURFACE_WITH_KNOTS((2,2),(3,2,3),(0.78855461441299,1.),(0.0735508106174519,
0.0909109506295936,0.091084552029715),.UNSPECIFIED.)
GEOMETRIC_REPRESENTATION_ITEM()
RATIONAL_B_SPLINE_SURFACE(((0.998554414400195,0.992822941359326,0.990053454406148,
0.990053454406148,0.990053454406148),(0.998554414400195,0.992822941359326,
0.990053454406147,0.990053454406147,0.990053454406147)))
REPRESENTATION_ITEM('')
SURFACE()
);
#4172=(
BOUNDED_SURFACE()
B_SPLINE_SURFACE(1,2,((#165188,#165189,#165190,#165191,#165192,#165193,
#165194),(#165195,#165196,#165197,#165198,#165199,#165200,#165201),(#165202,
#165203,#165204,#165205,#165206,#165207,#165208)),.UNSPECIFIED.,.F.,.F.,
 .F.)
B_SPLINE_SURFACE_WITH_KNOTS((2,1,2),(3,2,2,3),(0.788462675553397,1.,1.00211537324447),
(0.642404283483303,0.642578551421364,0.642857142857143,0.660005345227478),
 .UNSPECIFIED.)
GEOMETRIC_REPRESENTATION_ITEM()
RATIONAL_B_SPLINE_SURFACE(((0.999805186472059,0.999805186472059,0.999805186472059,
0.999902211834795,1.,0.993980822699459,0.990851751371591),(0.999805186472059,
0.999805186472059,0.999805186472059,0.999902211834795,1.,0.993980822699459,
0.990851751371591),(0.999805186472059,0.999805186472059,0.999805186472059,
0.999902211834795,1.,0.993980822699459,0.990851751371591)))
REPRESENTATION_ITEM('')
SURFACE()
);
#4173=(
BOUNDED_SURFACE()
B_SPLINE_SURFACE(1,2,((#165215,#165216,#165217,#165218,#165219),(#165220,
#165221,#165222,#165223,#165224)),.UNSPECIFIED.,.F.,.F.,.F.)
B_SPLINE_SURFACE_WITH_KNOTS((2,2),(3,2,3),(0.788554614412988,1.),(0.0735508106174229,
0.0909109506295945,0.0910845520297162),.UNSPECIFIED.)
GEOMETRIC_REPRESENTATION_ITEM()
RATIONAL_B_SPLINE_SURFACE(((0.998554414400214,0.99282294135933,0.990053454406147,
0.990053454406147,0.990053454406147),(0.998554414400214,0.99282294135933,
0.990053454406147,0.990053454406147,0.990053454406147)))
REPRESENTATION_ITEM('')
SURFACE()
);
#4174=(
BOUNDED_SURFACE()
B_SPLINE_SURFACE(1,2,((#165226,#165227,#165228,#165229,#165230,#165231,
#165232),(#165233,#165234,#165235,#165236,#165237,#165238,#165239)),
 .UNSPECIFIED.,.F.,.F.,.F.)
B_SPLINE_SURFACE_WITH_KNOTS((2,2),(3,2,2,3),(0.788462675553383,1.),(0.642404283483302,
0.642578551421363,0.642857142857143,0.660005345227478),.UNSPECIFIED.)
GEOMETRIC_REPRESENTATION_ITEM()
RATIONAL_B_SPLINE_SURFACE(((0.999805186472058,0.999805186472058,0.999805186472058,
0.999902211834794,1.,0.993980822699459,0.990851751371592),(0.999805186472058,
0.999805186472058,0.999805186472058,0.999902211834794,1.,0.993980822699459,
0.990851751371592)))
REPRESENTATION_ITEM('')
SURFACE()
);
#4175=(
BOUNDED_SURFACE()
B_SPLINE_SURFACE(1,2,((#165243,#165244,#165245,#165246,#165247),(#165248,
#165249,#165250,#165251,#165252)),.UNSPECIFIED.,.F.,.F.,.F.)
B_SPLINE_SURFACE_WITH_KNOTS((2,2),(3,2,3),(0.788554614412982,1.0000010632625),
(0.0735508106174268,0.0909109506295945,0.0910845520297162),
 .UNSPECIFIED.)
GEOMETRIC_REPRESENTATION_ITEM()
RATIONAL_B_SPLINE_SURFACE(((0.998554414400211,0.99282294135933,0.990053454406147,
0.990053454406147,0.990053454406147),(0.998554414400211,0.99282294135933,
0.990053454406147,0.990053454406147,0.990053454406147)))
REPRESENTATION_ITEM('')
SURFACE()
);
#4176=(
BOUNDED_SURFACE()
B_SPLINE_SURFACE(1,2,((#165254,#165255,#165256,#165257,#165258,#165259,
#165260),(#165261,#165262,#165263,#165264,#165265,#165266,#165267)),
 .UNSPECIFIED.,.F.,.F.,.F.)
B_SPLINE_SURFACE_WITH_KNOTS((2,2),(3,2,2,3),(0.788462675553384,1.),(0.642404283483302,
0.642578551421363,0.642857142857143,0.660005345227479),.UNSPECIFIED.)
GEOMETRIC_REPRESENTATION_ITEM()
RATIONAL_B_SPLINE_SURFACE(((0.999805186472058,0.999805186472058,0.999805186472058,
0.999902211834794,1.,0.993980822699459,0.990851751371591),(0.999805186472058,
0.999805186472058,0.999805186472058,0.999902211834794,1.,0.993980822699459,
0.990851751371591)))
REPRESENTATION_ITEM('')
SURFACE()
);
#4177=(
BOUNDED_SURFACE()
B_SPLINE_SURFACE(1,2,((#165271,#165272,#165273,#165274,#165275),(#165276,
#165277,#165278,#165279,#165280)),.UNSPECIFIED.,.F.,.F.,.F.)
B_SPLINE_SURFACE_WITH_KNOTS((2,2),(3,2,3),(0.788554614412984,1.00000106568131),
(0.0735508106174531,0.0909109506295944,0.0910845520297158),
 .UNSPECIFIED.)
GEOMETRIC_REPRESENTATION_ITEM()
RATIONAL_B_SPLINE_SURFACE(((0.998554414400194,0.992822941359325,0.990053454406147,
0.990053454406147,0.990053454406147),(0.998554414400194,0.992822941359325,
0.990053454406147,0.990053454406147,0.990053454406147)))
REPRESENTATION_ITEM('')
SURFACE()
);
#4178=(
BOUNDED_SURFACE()
B_SPLINE_SURFACE(1,2,((#165282,#165283,#165284,#165285,#165286,#165287,
#165288),(#165289,#165290,#165291,#165292,#165293,#165294,#165295),(#165296,
#165297,#165298,#165299,#165300,#165301,#165302)),.UNSPECIFIED.,.F.,.F.,
 .F.)
B_SPLINE_SURFACE_WITH_KNOTS((2,1,2),(3,2,2,3),(0.788462675553387,1.,1.00211537324447),
(0.642404283483302,0.642578551421363,0.642857142857143,0.660005345227478),
 .UNSPECIFIED.)
GEOMETRIC_REPRESENTATION_ITEM()
RATIONAL_B_SPLINE_SURFACE(((0.999805186472058,0.999805186472058,0.999805186472058,
0.999902211834794,1.,0.993980822699459,0.990851751371591),(0.999805186472058,
0.999805186472058,0.999805186472058,0.999902211834794,1.,0.993980822699459,
0.990851751371591),(0.999805186472058,0.999805186472058,0.999805186472058,
0.999902211834794,1.,0.993980822699459,0.990851751371591)))
REPRESENTATION_ITEM('')
SURFACE()
);
#4179=(
BOUNDED_SURFACE()
B_SPLINE_SURFACE(1,2,((#165309,#165310,#165311,#165312,#165313),(#165314,
#165315,#165316,#165317,#165318)),.UNSPECIFIED.,.F.,.F.,.F.)
B_SPLINE_SURFACE_WITH_KNOTS((2,2),(3,2,3),(0.788554614412982,1.),(0.073550810617453,
0.0909109506295945,0.0910845520297159),.UNSPECIFIED.)
GEOMETRIC_REPRESENTATION_ITEM()
RATIONAL_B_SPLINE_SURFACE(((0.998554414400194,0.992822941359326,0.990053454406147,
0.990053454406147,0.990053454406147),(0.998554414400194,0.992822941359326,
0.990053454406147,0.990053454406147,0.990053454406147)))
REPRESENTATION_ITEM('')
SURFACE()
);
#4180=(
BOUNDED_SURFACE()
B_SPLINE_SURFACE(1,2,((#165320,#165321,#165322,#165323,#165324,#165325,
#165326),(#165327,#165328,#165329,#165330,#165331,#165332,#165333),(#165334,
#165335,#165336,#165337,#165338,#165339,#165340)),.UNSPECIFIED.,.F.,.F.,
 .F.)
B_SPLINE_SURFACE_WITH_KNOTS((2,1,2),(3,2,2,3),(0.788462675553383,1.,1.00211537324447),
(0.642404283483302,0.642578551421363,0.642857142857143,0.660005345227478),
 .UNSPECIFIED.)
GEOMETRIC_REPRESENTATION_ITEM()
RATIONAL_B_SPLINE_SURFACE(((0.999805186472058,0.999805186472058,0.999805186472058,
0.999902211834794,1.,0.993980822699459,0.990851751371591),(0.999805186472058,
0.999805186472058,0.999805186472058,0.999902211834794,1.,0.993980822699459,
0.990851751371591),(0.999805186472058,0.999805186472058,0.999805186472058,
0.999902211834794,1.,0.993980822699459,0.990851751371591)))
REPRESENTATION_ITEM('')
SURFACE()
);
#4181=(
BOUNDED_SURFACE()
B_SPLINE_SURFACE(1,2,((#165347,#165348,#165349,#165350,#165351),(#165352,
#165353,#165354,#165355,#165356)),.UNSPECIFIED.,.F.,.F.,.F.)
B_SPLINE_SURFACE_WITH_KNOTS((2,2),(3,2,3),(0.78855461441298,1.),(0.0735508106173347,
0.0909109506295947,0.0910845520297173),.UNSPECIFIED.)
GEOMETRIC_REPRESENTATION_ITEM()
RATIONAL_B_SPLINE_SURFACE(((0.998554414400272,0.992822941359344,0.990053454406147,
0.990053454406147,0.990053454406147),(0.998554414400272,0.992822941359344,
0.990053454406147,0.990053454406147,0.990053454406147)))
REPRESENTATION_ITEM('')
SURFACE()
);
#4182=(
BOUNDED_SURFACE()
B_SPLINE_SURFACE(1,2,((#165358,#165359,#165360,#165361,#165362,#165363,
#165364),(#165365,#165366,#165367,#165368,#165369,#165370,#165371)),
 .UNSPECIFIED.,.F.,.F.,.F.)
B_SPLINE_SURFACE_WITH_KNOTS((2,2),(3,2,2,3),(0.788462675553384,1.),(0.642404283483302,
0.642578551421363,0.642857142857143,0.660005345227478),.UNSPECIFIED.)
GEOMETRIC_REPRESENTATION_ITEM()
RATIONAL_B_SPLINE_SURFACE(((0.999805186472059,0.999805186472059,0.999805186472059,
0.999902211834794,1.,0.993980822699459,0.990851751371591),(0.999805186472059,
0.999805186472059,0.999805186472059,0.999902211834794,1.,0.993980822699459,
0.990851751371591)))
REPRESENTATION_ITEM('')
SURFACE()
);
#4183=(
BOUNDED_SURFACE()
B_SPLINE_SURFACE(1,2,((#165375,#165376,#165377,#165378,#165379),(#165380,
#165381,#165382,#165383,#165384)),.UNSPECIFIED.,.F.,.F.,.F.)
B_SPLINE_SURFACE_WITH_KNOTS((2,2),(3,2,3),(0.788554614412986,1.),(0.073550810617453,
0.0909109506295945,0.0910845520297159),.UNSPECIFIED.)
GEOMETRIC_REPRESENTATION_ITEM()
RATIONAL_B_SPLINE_SURFACE(((0.998554414400194,0.992822941359325,0.990053454406147,
0.990053454406147,0.990053454406147),(0.998554414400194,0.992822941359325,
0.990053454406147,0.990053454406147,0.990053454406147)))
REPRESENTATION_ITEM('')
SURFACE()
);
#4184=(
BOUNDED_SURFACE()
B_SPLINE_SURFACE(1,2,((#165386,#165387,#165388,#165389,#165390,#165391,
#165392),(#165393,#165394,#165395,#165396,#165397,#165398,#165399)),
 .UNSPECIFIED.,.F.,.F.,.F.)
B_SPLINE_SURFACE_WITH_KNOTS((2,2),(3,2,2,3),(0.788462675553381,1.),(0.642404283483302,
0.642578551421363,0.642857142857143,0.660005345227479),.UNSPECIFIED.)
GEOMETRIC_REPRESENTATION_ITEM()
RATIONAL_B_SPLINE_SURFACE(((0.999805186472058,0.999805186472058,0.999805186472058,
0.999902211834794,1.,0.993980822699459,0.990851751371591),(0.999805186472058,
0.999805186472058,0.999805186472058,0.999902211834794,1.,0.993980822699459,
0.990851751371591)))
REPRESENTATION_ITEM('')
SURFACE()
);
#4185=(
BOUNDED_SURFACE()
B_SPLINE_SURFACE(1,2,((#165403,#165404,#165405,#165406,#165407),(#165408,
#165409,#165410,#165411,#165412)),.UNSPECIFIED.,.F.,.F.,.F.)
B_SPLINE_SURFACE_WITH_KNOTS((2,2),(3,2,3),(0.788554614412988,1.00000106334399),
(0.0735508106174531,0.0909109506295945,0.0910845520297159),
 .UNSPECIFIED.)
GEOMETRIC_REPRESENTATION_ITEM()
RATIONAL_B_SPLINE_SURFACE(((0.998554414400194,0.992822941359326,0.990053454406147,
0.990053454406147,0.990053454406147),(0.998554414400194,0.992822941359326,
0.990053454406147,0.990053454406147,0.990053454406147)))
REPRESENTATION_ITEM('')
SURFACE()
);
#4186=(
BOUNDED_SURFACE()
B_SPLINE_SURFACE(1,2,((#165414,#165415,#165416,#165417,#165418,#165419,
#165420),(#165421,#165422,#165423,#165424,#165425,#165426,#165427)),
 .UNSPECIFIED.,.F.,.F.,.F.)
B_SPLINE_SURFACE_WITH_KNOTS((2,2),(3,2,2,3),(0.788462675553238,1.),(0.642404283483285,
0.642578551421346,0.642857142857143,0.660005345227478),.UNSPECIFIED.)
GEOMETRIC_REPRESENTATION_ITEM()
RATIONAL_B_SPLINE_SURFACE(((0.999805186472047,0.999805186472047,0.999805186472047,
0.999902211834788,1.,0.993980822699459,0.990851751371591),(0.999805186472047,
0.999805186472047,0.999805186472047,0.999902211834788,1.,0.993980822699459,
0.990851751371591)))
REPRESENTATION_ITEM('')
SURFACE()
);
#4187=(
BOUNDED_SURFACE()
B_SPLINE_SURFACE(1,2,((#165431,#165432,#165433,#165434,#165435),(#165436,
#165437,#165438,#165439,#165440)),.UNSPECIFIED.,.F.,.F.,.F.)
B_SPLINE_SURFACE_WITH_KNOTS((2,2),(3,2,3),(0.788554614412988,1.00000106562849),
(0.073550810617453,0.0909109506295944,0.0910845520297158),.UNSPECIFIED.)
GEOMETRIC_REPRESENTATION_ITEM()
RATIONAL_B_SPLINE_SURFACE(((0.998554414400194,0.992822941359325,0.990053454406147,
0.990053454406147,0.990053454406147),(0.998554414400194,0.992822941359325,
0.990053454406147,0.990053454406147,0.990053454406147)))
REPRESENTATION_ITEM('')
SURFACE()
);
#4188=(
BOUNDED_SURFACE()
B_SPLINE_SURFACE(1,2,((#165442,#165443,#165444,#165445,#165446,#165447,
#165448),(#165449,#165450,#165451,#165452,#165453,#165454,#165455)),
 .UNSPECIFIED.,.F.,.F.,.F.)
B_SPLINE_SURFACE_WITH_KNOTS((2,2),(3,2,2,3),(0.788462675553159,1.),(0.642404283483276,
0.642578551421337,0.642857142857143,0.660005345227478),.UNSPECIFIED.)
GEOMETRIC_REPRESENTATION_ITEM()
RATIONAL_B_SPLINE_SURFACE(((0.99980518647204,0.99980518647204,0.99980518647204,
0.999902211834785,1.,0.993980822699459,0.990851751371591),(0.99980518647204,
0.99980518647204,0.99980518647204,0.999902211834785,1.,0.993980822699459,
0.990851751371591)))
REPRESENTATION_ITEM('')
SURFACE()
);
#4189=(
BOUNDED_SURFACE()
B_SPLINE_SURFACE(1,2,((#165459,#165460,#165461,#165462,#165463),(#165464,
#165465,#165466,#165467,#165468)),.UNSPECIFIED.,.F.,.F.,.F.)
B_SPLINE_SURFACE_WITH_KNOTS((2,2),(3,2,3),(0.788554614412984,1.00000106325674),
(0.0735508106174531,0.0909109506295946,0.091084552029716),.UNSPECIFIED.)
GEOMETRIC_REPRESENTATION_ITEM()
RATIONAL_B_SPLINE_SURFACE(((0.998554414400194,0.992822941359325,0.990053454406147,
0.990053454406147,0.990053454406147),(0.998554414400194,0.992822941359325,
0.990053454406147,0.990053454406147,0.990053454406147)))
REPRESENTATION_ITEM('')
SURFACE()
);
#4190=(
BOUNDED_SURFACE()
B_SPLINE_SURFACE(1,2,((#165470,#165471,#165472,#165473,#165474,#165475,
#165476),(#165477,#165478,#165479,#165480,#165481,#165482,#165483)),
 .UNSPECIFIED.,.F.,.F.,.F.)
B_SPLINE_SURFACE_WITH_KNOTS((2,2),(3,2,2,3),(0.788462675553045,1.),(0.642404283483262,
0.642578551421323,0.642857142857143,0.660005345227478),.UNSPECIFIED.)
GEOMETRIC_REPRESENTATION_ITEM()
RATIONAL_B_SPLINE_SURFACE(((0.999805186472031,0.999805186472031,0.999805186472031,
0.99990221183478,1.,0.993980822699459,0.990851751371591),(0.999805186472031,
0.999805186472031,0.999805186472031,0.99990221183478,1.,0.993980822699459,
0.990851751371591)))
REPRESENTATION_ITEM('')
SURFACE()
);
#4191=(
BOUNDED_SURFACE()
B_SPLINE_SURFACE(1,2,((#165487,#165488,#165489,#165490,#165491),(#165492,
#165493,#165494,#165495,#165496)),.UNSPECIFIED.,.F.,.F.,.F.)
B_SPLINE_SURFACE_WITH_KNOTS((2,2),(3,2,3),(0.788554614412981,1.00000106317919),
(0.073550810617453,0.0909109506295945,0.0910845520297159),.UNSPECIFIED.)
GEOMETRIC_REPRESENTATION_ITEM()
RATIONAL_B_SPLINE_SURFACE(((0.998554414400194,0.992822941359325,0.990053454406147,
0.990053454406147,0.990053454406147),(0.998554414400194,0.992822941359325,
0.990053454406147,0.990053454406147,0.990053454406147)))
REPRESENTATION_ITEM('')
SURFACE()
);
#4192=(
BOUNDED_SURFACE()
B_SPLINE_SURFACE(1,2,((#165498,#165499,#165500,#165501,#165502,#165503,
#165504),(#165505,#165506,#165507,#165508,#165509,#165510,#165511)),
 .UNSPECIFIED.,.F.,.F.,.F.)
B_SPLINE_SURFACE_WITH_KNOTS((2,2),(3,2,2,3),(0.788462675552883,1.),(0.642404283483242,
0.642578551421304,0.642857142857143,0.660005345227478),.UNSPECIFIED.)
GEOMETRIC_REPRESENTATION_ITEM()
RATIONAL_B_SPLINE_SURFACE(((0.999805186472017,0.999805186472017,0.999805186472017,
0.999902211834774,1.,0.993980822699459,0.990851751371591),(0.999805186472017,
0.999805186472017,0.999805186472017,0.999902211834774,1.,0.993980822699459,
0.990851751371591)))
REPRESENTATION_ITEM('')
SURFACE()
);
#4193=(
BOUNDED_SURFACE()
B_SPLINE_SURFACE(1,2,((#165515,#165516,#165517,#165518,#165519),(#165520,
#165521,#165522,#165523,#165524)),.UNSPECIFIED.,.F.,.F.,.F.)
B_SPLINE_SURFACE_WITH_KNOTS((2,2),(3,2,3),(0.788554614412985,1.00000106576408),
(0.073550810617453,0.0909109506295944,0.0910845520297158),.UNSPECIFIED.)
GEOMETRIC_REPRESENTATION_ITEM()
RATIONAL_B_SPLINE_SURFACE(((0.998554414400194,0.992822941359326,0.990053454406147,
0.990053454406147,0.990053454406147),(0.998554414400194,0.992822941359326,
0.990053454406147,0.990053454406147,0.990053454406147)))
REPRESENTATION_ITEM('')
SURFACE()
);
#4194=(
BOUNDED_SURFACE()
B_SPLINE_SURFACE(1,2,((#165526,#165527,#165528,#165529,#165530,#165531,
#165532),(#165533,#165534,#165535,#165536,#165537,#165538,#165539)),
 .UNSPECIFIED.,.F.,.F.,.F.)
B_SPLINE_SURFACE_WITH_KNOTS((2,2),(3,2,2,3),(0.788462675552653,1.),(0.642404283483215,
0.642578551421277,0.642857142857143,0.660005345227479),.UNSPECIFIED.)
GEOMETRIC_REPRESENTATION_ITEM()
RATIONAL_B_SPLINE_SURFACE(((0.999805186471999,0.999805186471999,0.999805186471999,
0.999902211834764,1.,0.993980822699459,0.990851751371591),(0.999805186471999,
0.999805186471999,0.999805186471999,0.999902211834764,1.,0.993980822699459,
0.990851751371591)))
REPRESENTATION_ITEM('')
SURFACE()
);
#4195=(
BOUNDED_SURFACE()
B_SPLINE_SURFACE(1,2,((#165543,#165544,#165545,#165546,#165547),(#165548,
#165549,#165550,#165551,#165552),(#165553,#165554,#165555,#165556,#165557)),
 .UNSPECIFIED.,.F.,.F.,.F.)
B_SPLINE_SURFACE_WITH_KNOTS((2,1,2),(3,2,3),(0.776713355992017,0.788554614412987,
1.),(0.073550810617453,0.0909109506295944,0.0910845520297158),
 .UNSPECIFIED.)
GEOMETRIC_REPRESENTATION_ITEM()
RATIONAL_B_SPLINE_SURFACE(((0.998554414400194,0.992822941359326,0.990053454406147,
0.990053454406147,0.990053454406147),(0.998554414400194,0.992822941359326,
0.990053454406147,0.990053454406147,0.990053454406147),(0.998554414400194,
0.992822941359326,0.990053454406147,0.990053454406147,0.990053454406147)))
REPRESENTATION_ITEM('')
SURFACE()
);
#4196=(
BOUNDED_SURFACE()
B_SPLINE_SURFACE(1,2,((#165560,#165561,#165562,#165563,#165564),(#165565,
#165566,#165567,#165568,#165569)),.UNSPECIFIED.,.F.,.F.,.F.)
B_SPLINE_SURFACE_WITH_KNOTS((2,2),(3,2,3),(0.,0.182805892339156),(0.642474614281366,
0.642857142857143,0.659901408087481),.UNSPECIFIED.)
GEOMETRIC_REPRESENTATION_ITEM()
RATIONAL_B_SPLINE_SURFACE(((0.999732896029237,0.999865728939372,1.,0.994017305594881,
0.990889788836284),(0.999732896029237,0.999865728939372,1.,0.994017305594881,
0.990889788836284)))
REPRESENTATION_ITEM('')
SURFACE()
);
#4197=(
BOUNDED_SURFACE()
B_SPLINE_SURFACE(1,2,((#165581,#165582,#165583,#165584,#165585),(#165586,
#165587,#165588,#165589,#165590)),.UNSPECIFIED.,.F.,.F.,.F.)
B_SPLINE_SURFACE_WITH_KNOTS((2,2),(3,2,3),(0.938576859128175,1.),(0.0665257254736565,
0.0714285714285714,0.0736543502199111),.UNSPECIFIED.)
GEOMETRIC_REPRESENTATION_ITEM()
RATIONAL_B_SPLINE_SURFACE(((0.996794362316492,0.998279055819231,1.,0.999218731101516,
0.99848615229188),(0.996794362316492,0.998279055819231,1.,0.999218731101516,
0.99848615229188)))
REPRESENTATION_ITEM('')
SURFACE()
);
#4198=(
BOUNDED_SURFACE()
B_SPLINE_SURFACE(1,2,((#165598,#165599,#165600,#165601,#165602),(#165603,
#165604,#165605,#165606,#165607)),.UNSPECIFIED.,.F.,.F.,.F.)
B_SPLINE_SURFACE_WITH_KNOTS((2,2),(3,2,3),(0.,0.0529045403781329),(0.0665257254736577,
0.0714285714285714,0.0736968668682836),.UNSPECIFIED.)
GEOMETRIC_REPRESENTATION_ITEM()
RATIONAL_B_SPLINE_SURFACE(((0.996794362316492,0.998279055819232,1.,0.999203807365532,
0.998458182734476),(0.996794362316492,0.998279055819232,1.,0.999203807365532,
0.998458182734476)))
REPRESENTATION_ITEM('')
SURFACE()
);
#4199=(
BOUNDED_SURFACE()
B_SPLINE_SURFACE(1,2,((#165618,#165619,#165620),(#165621,#165622,#165623)),
 .UNSPECIFIED.,.F.,.F.,.F.)
B_SPLINE_SURFACE_WITH_KNOTS((2,2),(3,3),(0.,0.052881546879832),(0.659860018385301,
0.666841081426899),.UNSPECIFIED.)
GEOMETRIC_REPRESENTATION_ITEM()
RATIONAL_B_SPLINE_SURFACE(((0.990904995179465,0.989621173673398,0.988816334712145),
(0.990904995179465,0.989621173673398,0.988816334712145)))
REPRESENTATION_ITEM('')
SURFACE()
);
#4200=(
BOUNDED_SURFACE()
B_SPLINE_SURFACE(1,2,((#165625,#165626,#165627,#165628,#165629),(#165630,
#165631,#165632,#165633,#165634)),.UNSPECIFIED.,.F.,.F.,.F.)
B_SPLINE_SURFACE_WITH_KNOTS((2,2),(3,2,3),(0.938550151644316,1.0000100824887),
(0.65983201135371,0.659901408087108,0.666841081426899),.UNSPECIFIED.)
GEOMETRIC_REPRESENTATION_ITEM()
RATIONAL_B_SPLINE_SURFACE(((0.990889788836421,0.990889788836421,0.990889788836421,
0.989616401900903,0.988816334712145),(0.990889788836421,0.990889788836421,
0.990889788836421,0.989616401900903,0.988816334712145)))
REPRESENTATION_ITEM('')
SURFACE()
);
#4201=(
BOUNDED_SURFACE()
B_SPLINE_SURFACE(1,2,((#165636,#165637,#165638,#165639,#165640),(#165641,
#165642,#165643,#165644,#165645)),.UNSPECIFIED.,.F.,.F.,.F.)
B_SPLINE_SURFACE_WITH_KNOTS((2,2),(3,2,3),(0.,0.182885378421189),(0.0734807488194108,
0.073654350219536,0.0910144902320546),.UNSPECIFIED.)
GEOMETRIC_REPRESENTATION_ITEM()
RATIONAL_B_SPLINE_SURFACE(((0.998486152292127,0.998486152292127,0.998486152292127,
0.99277234517207,0.990020524139832),(0.998486152292127,0.998486152292127,
0.998486152292127,0.99277234517207,0.990020524139832)))
REPRESENTATION_ITEM('')
SURFACE()
);
#4202=(
BOUNDED_SURFACE()
B_SPLINE_SURFACE(1,2,((#165656,#165657,#165658,#165659,#165660),(#165661,
#165662,#165663,#165664,#165665)),.UNSPECIFIED.,.F.,.F.,.F.)
B_SPLINE_SURFACE_WITH_KNOTS((2,2),(3,2,3),(0.,0.182805892339158),(0.642474614281361,
0.642857142857143,0.659901408087481),.UNSPECIFIED.)
GEOMETRIC_REPRESENTATION_ITEM()
RATIONAL_B_SPLINE_SURFACE(((0.999732896029233,0.99986572893937,1.,0.994017305594881,
0.990889788836284),(0.999732896029233,0.99986572893937,1.,0.994017305594881,
0.990889788836284)))
REPRESENTATION_ITEM('')
SURFACE()
);
#4203=(
BOUNDED_SURFACE()
B_SPLINE_SURFACE(1,2,((#165667,#165668,#165669,#165670,#165671),(#165672,
#165673,#165674,#165675,#165676)),.UNSPECIFIED.,.F.,.F.,.F.)
B_SPLINE_SURFACE_WITH_KNOTS((2,2),(3,2,3),(0.938576859128175,1.),(0.0665257254736565,
0.0714285714285714,0.0736543502199112),.UNSPECIFIED.)
GEOMETRIC_REPRESENTATION_ITEM()
RATIONAL_B_SPLINE_SURFACE(((0.996794362316492,0.998279055819231,1.,0.999218731101516,
0.99848615229188),(0.996794362316492,0.998279055819231,1.,0.999218731101516,
0.99848615229188)))
REPRESENTATION_ITEM('')
SURFACE()
);
#4204=(
BOUNDED_SURFACE()
B_SPLINE_SURFACE(1,2,((#165684,#165685,#165686,#165687,#165688),(#165689,
#165690,#165691,#165692,#165693)),.UNSPECIFIED.,.F.,.F.,.F.)
B_SPLINE_SURFACE_WITH_KNOTS((2,2),(3,2,3),(0.,0.052904540378128),(0.0665257254736564,
0.0714285714285714,0.0736968668684972),.UNSPECIFIED.)
GEOMETRIC_REPRESENTATION_ITEM()
RATIONAL_B_SPLINE_SURFACE(((0.996794362316492,0.998279055819231,1.,0.999203807365457,
0.998458182734336),(0.996794362316492,0.998279055819231,1.,0.999203807365457,
0.998458182734336)))
REPRESENTATION_ITEM('')
SURFACE()
);
#4205=(
BOUNDED_SURFACE()
B_SPLINE_SURFACE(1,2,((#165704,#165705,#165706),(#165707,#165708,#165709)),
 .UNSPECIFIED.,.F.,.F.,.F.)
B_SPLINE_SURFACE_WITH_KNOTS((2,2),(3,3),(0.,0.0528815468798315),(0.659860018385656,
0.666841081426896),.UNSPECIFIED.)
GEOMETRIC_REPRESENTATION_ITEM()
RATIONAL_B_SPLINE_SURFACE(((0.990904995179334,0.989621173673357,0.988816334712145),
(0.990904995179334,0.989621173673357,0.988816334712145)))
REPRESENTATION_ITEM('')
SURFACE()
);
#4206=(
BOUNDED_SURFACE()
B_SPLINE_SURFACE(1,2,((#165711,#165712,#165713,#165714,#165715),(#165716,
#165717,#165718,#165719,#165720)),.UNSPECIFIED.,.F.,.F.,.F.)
B_SPLINE_SURFACE_WITH_KNOTS((2,2),(3,2,3),(0.938550151647612,1.00001008246538),
(0.659832011354087,0.659901408087481,0.666841081426897),.UNSPECIFIED.)
GEOMETRIC_REPRESENTATION_ITEM()
RATIONAL_B_SPLINE_SURFACE(((0.990889788836284,0.990889788836284,0.990889788836284,
0.98961640190086,0.988816334712146),(0.990889788836284,0.990889788836284,
0.990889788836284,0.98961640190086,0.988816334712146)))
REPRESENTATION_ITEM('')
SURFACE()
);
#4207=(
BOUNDED_SURFACE()
B_SPLINE_SURFACE(1,2,((#165722,#165723,#165724,#165725,#165726),(#165727,
#165728,#165729,#165730,#165731)),.UNSPECIFIED.,.F.,.F.,.F.)
B_SPLINE_SURFACE_WITH_KNOTS((2,2),(3,2,3),(-1.0691269832958E-6,0.182885378421193),
(0.0734807488197898,0.0736543502199112,0.0910144902320524),
 .UNSPECIFIED.)
GEOMETRIC_REPRESENTATION_ITEM()
RATIONAL_B_SPLINE_SURFACE(((0.99848615229188,0.99848615229188,0.99848615229188,
0.992772345172011,0.990020524139833),(0.99848615229188,0.99848615229188,
0.99848615229188,0.992772345172011,0.990020524139833)))
REPRESENTATION_ITEM('')
SURFACE()
);
#4208=(
BOUNDED_SURFACE()
B_SPLINE_SURFACE(1,2,((#165742,#165743,#165744,#165745,#165746),(#165747,
#165748,#165749,#165750,#165751)),.UNSPECIFIED.,.F.,.F.,.F.)
B_SPLINE_SURFACE_WITH_KNOTS((2,2),(3,2,3),(0.,0.18280589233916),(0.642474614281366,
0.642857142857143,0.659901408087481),.UNSPECIFIED.)
GEOMETRIC_REPRESENTATION_ITEM()
RATIONAL_B_SPLINE_SURFACE(((0.999732896029237,0.999865728939372,1.,0.994017305594881,
0.990889788836284),(0.999732896029237,0.999865728939372,1.,0.994017305594881,
0.990889788836284)))
REPRESENTATION_ITEM('')
SURFACE()
);
#4209=(
BOUNDED_SURFACE()
B_SPLINE_SURFACE(1,2,((#165753,#165754,#165755,#165756,#165757),(#165758,
#165759,#165760,#165761,#165762)),.UNSPECIFIED.,.F.,.F.,.F.)
B_SPLINE_SURFACE_WITH_KNOTS((2,2),(3,2,3),(0.938576859128171,1.),(0.0665257254736565,
0.0714285714285714,0.0736543502199113),.UNSPECIFIED.)
GEOMETRIC_REPRESENTATION_ITEM()
RATIONAL_B_SPLINE_SURFACE(((0.996794362316492,0.998279055819231,1.,0.999218731101516,
0.99848615229188),(0.996794362316492,0.998279055819231,1.,0.999218731101516,
0.99848615229188)))
REPRESENTATION_ITEM('')
SURFACE()
);
#4210=(
BOUNDED_SURFACE()
B_SPLINE_SURFACE(1,2,((#165770,#165771,#165772,#165773,#165774),(#165775,
#165776,#165777,#165778,#165779)),.UNSPECIFIED.,.F.,.F.,.F.)
B_SPLINE_SURFACE_WITH_KNOTS((2,2),(3,2,3),(0.,0.0529045403781295),(0.0665257254736562,
0.0714285714285714,0.0736968668684972),.UNSPECIFIED.)
GEOMETRIC_REPRESENTATION_ITEM()
RATIONAL_B_SPLINE_SURFACE(((0.996794362316491,0.998279055819231,1.,0.999203807365457,
0.998458182734336),(0.996794362316491,0.998279055819231,1.,0.999203807365457,
0.998458182734336)))
REPRESENTATION_ITEM('')
SURFACE()
);
#4211=(
BOUNDED_SURFACE()
B_SPLINE_SURFACE(1,2,((#165790,#165791,#165792),(#165793,#165794,#165795)),
 .UNSPECIFIED.,.F.,.F.,.F.)
B_SPLINE_SURFACE_WITH_KNOTS((2,2),(3,3),(0.,0.0528815468798302),(0.659860018385514,
0.666841081426898),.UNSPECIFIED.)
GEOMETRIC_REPRESENTATION_ITEM()
RATIONAL_B_SPLINE_SURFACE(((0.990904995179386,0.989621173673374,0.988816334712145),
(0.990904995179386,0.989621173673374,0.988816334712145)))
REPRESENTATION_ITEM('')
SURFACE()
);
#4212=(
BOUNDED_SURFACE()
B_SPLINE_SURFACE(1,2,((#165797,#165798,#165799,#165800,#165801),(#165802,
#165803,#165804,#165805,#165806)),.UNSPECIFIED.,.F.,.F.,.F.)
B_SPLINE_SURFACE_WITH_KNOTS((2,2),(3,2,3),(0.93855015164761,1.00001008255567),
(0.659832011354087,0.659901408087481,0.666841081426897),.UNSPECIFIED.)
GEOMETRIC_REPRESENTATION_ITEM()
RATIONAL_B_SPLINE_SURFACE(((0.990889788836284,0.990889788836284,0.990889788836284,
0.98961640190086,0.988816334712146),(0.990889788836284,0.990889788836284,
0.990889788836284,0.98961640190086,0.988816334712146)))
REPRESENTATION_ITEM('')
SURFACE()
);
#4213=(
BOUNDED_SURFACE()
B_SPLINE_SURFACE(1,2,((#165808,#165809,#165810,#165811,#165812),(#165813,
#165814,#165815,#165816,#165817)),.UNSPECIFIED.,.F.,.F.,.F.)
B_SPLINE_SURFACE_WITH_KNOTS((2,2),(3,2,3),(-1.0690240066242E-6,0.182885378421191),
(0.0734807488197898,0.0736543502199112,0.0910144902320524),
 .UNSPECIFIED.)
GEOMETRIC_REPRESENTATION_ITEM()
RATIONAL_B_SPLINE_SURFACE(((0.99848615229188,0.99848615229188,0.99848615229188,
0.992772345172011,0.990020524139833),(0.99848615229188,0.99848615229188,
0.99848615229188,0.992772345172011,0.990020524139833)))
REPRESENTATION_ITEM('')
SURFACE()
);
#4214=(
BOUNDED_SURFACE()
B_SPLINE_SURFACE(1,2,((#165828,#165829,#165830,#165831,#165832),(#165833,
#165834,#165835,#165836,#165837)),.UNSPECIFIED.,.F.,.F.,.F.)
B_SPLINE_SURFACE_WITH_KNOTS((2,2),(3,2,3),(0.,0.182805892339153),(0.642474614281367,
0.642857142857143,0.659901408087481),.UNSPECIFIED.)
GEOMETRIC_REPRESENTATION_ITEM()
RATIONAL_B_SPLINE_SURFACE(((0.999732896029237,0.999865728939372,1.,0.994017305594881,
0.990889788836284),(0.999732896029237,0.999865728939372,1.,0.994017305594881,
0.990889788836284)))
REPRESENTATION_ITEM('')
SURFACE()
);
#4215=(
BOUNDED_SURFACE()
B_SPLINE_SURFACE(1,2,((#165839,#165840,#165841,#165842,#165843),(#165844,
#165845,#165846,#165847,#165848)),.UNSPECIFIED.,.F.,.F.,.F.)
B_SPLINE_SURFACE_WITH_KNOTS((2,2),(3,2,3),(0.938576859128174,1.),(0.0665257254736565,
0.0714285714285714,0.0736543502199112),.UNSPECIFIED.)
GEOMETRIC_REPRESENTATION_ITEM()
RATIONAL_B_SPLINE_SURFACE(((0.996794362316492,0.998279055819231,1.,0.999218731101516,
0.99848615229188),(0.996794362316492,0.998279055819231,1.,0.999218731101516,
0.99848615229188)))
REPRESENTATION_ITEM('')
SURFACE()
);
#4216=(
BOUNDED_SURFACE()
B_SPLINE_SURFACE(1,2,((#165856,#165857,#165858,#165859,#165860),(#165861,
#165862,#165863,#165864,#165865)),.UNSPECIFIED.,.F.,.F.,.F.)
B_SPLINE_SURFACE_WITH_KNOTS((2,2),(3,2,3),(0.,0.0529045403781288),(0.0665257254736565,
0.0714285714285714,0.0736968668684971),.UNSPECIFIED.)
GEOMETRIC_REPRESENTATION_ITEM()
RATIONAL_B_SPLINE_SURFACE(((0.996794362316492,0.998279055819231,1.,0.999203807365457,
0.998458182734336),(0.996794362316492,0.998279055819231,1.,0.999203807365457,
0.998458182734336)))
REPRESENTATION_ITEM('')
SURFACE()
);
#4217=(
BOUNDED_SURFACE()
B_SPLINE_SURFACE(1,2,((#165876,#165877,#165878),(#165879,#165880,#165881)),
 .UNSPECIFIED.,.F.,.F.,.F.)
B_SPLINE_SURFACE_WITH_KNOTS((2,2),(3,3),(0.,0.0528815468798279),(0.659860018385542,
0.666841081426897),.UNSPECIFIED.)
GEOMETRIC_REPRESENTATION_ITEM()
RATIONAL_B_SPLINE_SURFACE(((0.990904995179376,0.98962117367337,0.988816334712146),
(0.990904995179376,0.98962117367337,0.988816334712146)))
REPRESENTATION_ITEM('')
SURFACE()
);
#4218=(
BOUNDED_SURFACE()
B_SPLINE_SURFACE(1,2,((#165883,#165884,#165885,#165886,#165887),(#165888,
#165889,#165890,#165891,#165892)),.UNSPECIFIED.,.F.,.F.,.F.)
B_SPLINE_SURFACE_WITH_KNOTS((2,2),(3,2,3),(0.93855015164656,1.00001008245209),
(0.659832011353967,0.659901408087362,0.666841081426897),.UNSPECIFIED.)
GEOMETRIC_REPRESENTATION_ITEM()
RATIONAL_B_SPLINE_SURFACE(((0.990889788836328,0.990889788836328,0.990889788836328,
0.989616401900874,0.988816334712145),(0.990889788836328,0.990889788836328,
0.990889788836328,0.989616401900874,0.988816334712145)))
REPRESENTATION_ITEM('')
SURFACE()
);
#4219=(
BOUNDED_SURFACE()
B_SPLINE_SURFACE(1,2,((#165894,#165895,#165896,#165897,#165898),(#165899,
#165900,#165901,#165902,#165903)),.UNSPECIFIED.,.F.,.F.,.F.)
B_SPLINE_SURFACE_WITH_KNOTS((2,2),(3,2,3),(0.,0.182885378421188),(0.0734807488196683,
0.0736543502197909,0.0910144902320531),.UNSPECIFIED.)
GEOMETRIC_REPRESENTATION_ITEM()
RATIONAL_B_SPLINE_SURFACE(((0.998486152291959,0.998486152291959,0.998486152291959,
0.99277234517203,0.990020524139833),(0.998486152291959,0.998486152291959,
0.998486152291959,0.99277234517203,0.990020524139833)))
REPRESENTATION_ITEM('')
SURFACE()
);
#4220=(
BOUNDED_SURFACE()
B_SPLINE_SURFACE(1,2,((#165914,#165915,#165916,#165917,#165918),(#165919,
#165920,#165921,#165922,#165923)),.UNSPECIFIED.,.F.,.F.,.F.)
B_SPLINE_SURFACE_WITH_KNOTS((2,2),(3,2,3),(0.,0.182805892339156),(0.642474614281367,
0.642857142857143,0.659901408087481),.UNSPECIFIED.)
GEOMETRIC_REPRESENTATION_ITEM()
RATIONAL_B_SPLINE_SURFACE(((0.999732896029237,0.999865728939372,1.,0.994017305594881,
0.990889788836284),(0.999732896029237,0.999865728939372,1.,0.994017305594881,
0.990889788836284)))
REPRESENTATION_ITEM('')
SURFACE()
);
#4221=(
BOUNDED_SURFACE()
B_SPLINE_SURFACE(1,2,((#165925,#165926,#165927,#165928,#165929),(#165930,
#165931,#165932,#165933,#165934)),.UNSPECIFIED.,.F.,.F.,.F.)
B_SPLINE_SURFACE_WITH_KNOTS((2,2),(3,2,3),(0.938576859128168,1.),(0.066525725473656,
0.0714285714285714,0.0736543502199112),.UNSPECIFIED.)
GEOMETRIC_REPRESENTATION_ITEM()
RATIONAL_B_SPLINE_SURFACE(((0.996794362316491,0.998279055819231,1.,0.999218731101516,
0.99848615229188),(0.996794362316491,0.998279055819231,1.,0.999218731101516,
0.99848615229188)))
REPRESENTATION_ITEM('')
SURFACE()
);
#4222=(
BOUNDED_SURFACE()
B_SPLINE_SURFACE(1,2,((#165941,#165942,#165943,#165944,#165945),(#165946,
#165947,#165948,#165949,#165950)),.UNSPECIFIED.,.F.,.F.,.F.)
B_SPLINE_SURFACE_WITH_KNOTS((2,2),(3,2,3),(0.,0.0529045403781274),(0.066525725473656,
0.0714285714285714,0.0736968668684972),.UNSPECIFIED.)
GEOMETRIC_REPRESENTATION_ITEM()
RATIONAL_B_SPLINE_SURFACE(((0.996794362316491,0.998279055819231,1.,0.999203807365457,
0.998458182734336),(0.996794362316491,0.998279055819231,1.,0.999203807365457,
0.998458182734336)))
REPRESENTATION_ITEM('')
SURFACE()
);
#4223=(
BOUNDED_SURFACE()
B_SPLINE_SURFACE(1,2,((#165961,#165962,#165963),(#165964,#165965,#165966)),
 .UNSPECIFIED.,.F.,.F.,.F.)
B_SPLINE_SURFACE_WITH_KNOTS((2,2),(3,3),(0.,0.0528815468798305),(0.659860018385656,
0.666841081426897),.UNSPECIFIED.)
GEOMETRIC_REPRESENTATION_ITEM()
RATIONAL_B_SPLINE_SURFACE(((0.990904995179334,0.989621173673357,0.988816334712145),
(0.990904995179334,0.989621173673357,0.988816334712145)))
REPRESENTATION_ITEM('')
SURFACE()
);
#4224=(
BOUNDED_SURFACE()
B_SPLINE_SURFACE(1,2,((#165968,#165969,#165970,#165971,#165972),(#165973,
#165974,#165975,#165976,#165977)),.UNSPECIFIED.,.F.,.F.,.F.)
B_SPLINE_SURFACE_WITH_KNOTS((2,2),(3,2,3),(0.938550151647609,1.00001008248703),
(0.659832011354087,0.659901408087481,0.666841081426897),.UNSPECIFIED.)
GEOMETRIC_REPRESENTATION_ITEM()
RATIONAL_B_SPLINE_SURFACE(((0.990889788836284,0.990889788836284,0.990889788836284,
0.98961640190086,0.988816334712146),(0.990889788836284,0.990889788836284,
0.990889788836284,0.98961640190086,0.988816334712146)))
REPRESENTATION_ITEM('')
SURFACE()
);
#4225=(
BOUNDED_SURFACE()
B_SPLINE_SURFACE(1,2,((#165979,#165980,#165981,#165982,#165983),(#165984,
#165985,#165986,#165987,#165988)),.UNSPECIFIED.,.F.,.F.,.F.)
B_SPLINE_SURFACE_WITH_KNOTS((2,2),(3,2,3),(-1.06890081270921E-6,0.182885378421181),
(0.0734807488197897,0.0736543502199111,0.0910144902320513),
 .UNSPECIFIED.)
GEOMETRIC_REPRESENTATION_ITEM()
RATIONAL_B_SPLINE_SURFACE(((0.99848615229188,0.99848615229188,0.99848615229188,
0.992772345172012,0.990020524139833),(0.99848615229188,0.99848615229188,
0.99848615229188,0.992772345172012,0.990020524139833)))
REPRESENTATION_ITEM('')
SURFACE()
);
#4226=(
BOUNDED_SURFACE()
B_SPLINE_SURFACE(1,2,((#165999,#166000,#166001,#166002,#166003),(#166004,
#166005,#166006,#166007,#166008)),.UNSPECIFIED.,.F.,.F.,.F.)
B_SPLINE_SURFACE_WITH_KNOTS((2,2),(3,2,3),(0.,0.182805892339142),(0.642474614281368,
0.642857142857143,0.659901408087482),.UNSPECIFIED.)
GEOMETRIC_REPRESENTATION_ITEM()
RATIONAL_B_SPLINE_SURFACE(((0.999732896029238,0.999865728939373,1.,0.994017305594881,
0.990889788836284),(0.999732896029238,0.999865728939373,1.,0.994017305594881,
0.990889788836284)))
REPRESENTATION_ITEM('')
SURFACE()
);
#4227=(
BOUNDED_SURFACE()
B_SPLINE_SURFACE(1,2,((#166010,#166011,#166012,#166013,#166014),(#166015,
#166016,#166017,#166018,#166019)),.UNSPECIFIED.,.F.,.F.,.F.)
B_SPLINE_SURFACE_WITH_KNOTS((2,2),(3,2,3),(0.938576859128178,1.),(0.0665257254736559,
0.0714285714285714,0.0736543502199103),.UNSPECIFIED.)
GEOMETRIC_REPRESENTATION_ITEM()
RATIONAL_B_SPLINE_SURFACE(((0.996794362316491,0.998279055819231,1.,0.999218731101516,
0.99848615229188),(0.996794362316491,0.998279055819231,1.,0.999218731101516,
0.99848615229188)))
REPRESENTATION_ITEM('')
SURFACE()
);
#4228=(
BOUNDED_SURFACE()
B_SPLINE_SURFACE(1,2,((#166027,#166028,#166029,#166030,#166031),(#166032,
#166033,#166034,#166035,#166036)),.UNSPECIFIED.,.F.,.F.,.F.)
B_SPLINE_SURFACE_WITH_KNOTS((2,2),(3,2,3),(0.,0.0529045403781231),(0.0665257254736559,
0.0714285714285714,0.0736968668684961),.UNSPECIFIED.)
GEOMETRIC_REPRESENTATION_ITEM()
RATIONAL_B_SPLINE_SURFACE(((0.996794362316491,0.998279055819231,1.,0.999203807365457,
0.998458182734337),(0.996794362316491,0.998279055819231,1.,0.999203807365457,
0.998458182734337)))
REPRESENTATION_ITEM('')
SURFACE()
);
#4229=(
BOUNDED_SURFACE()
B_SPLINE_SURFACE(1,2,((#166047,#166048,#166049),(#166050,#166051,#166052)),
 .UNSPECIFIED.,.F.,.F.,.F.)
B_SPLINE_SURFACE_WITH_KNOTS((2,2),(3,3),(0.,0.0528815468798204),(0.659860018385657,
0.666841081426896),.UNSPECIFIED.)
GEOMETRIC_REPRESENTATION_ITEM()
RATIONAL_B_SPLINE_SURFACE(((0.990904995179334,0.989621173673357,0.988816334712146),
(0.990904995179334,0.989621173673357,0.988816334712146)))
REPRESENTATION_ITEM('')
SURFACE()
);
#4230=(
BOUNDED_SURFACE()
B_SPLINE_SURFACE(1,2,((#166054,#166055,#166056,#166057,#166058),(#166059,
#166060,#166061,#166062,#166063)),.UNSPECIFIED.,.F.,.F.,.F.)
B_SPLINE_SURFACE_WITH_KNOTS((2,2),(3,2,3),(0.938550151647352,1.00001008247331),
(0.659832011354058,0.659901408087452,0.666841081426896),.UNSPECIFIED.)
GEOMETRIC_REPRESENTATION_ITEM()
RATIONAL_B_SPLINE_SURFACE(((0.990889788836295,0.990889788836295,0.990889788836295,
0.989616401900864,0.988816334712146),(0.990889788836295,0.990889788836295,
0.990889788836295,0.989616401900864,0.988816334712146)))
REPRESENTATION_ITEM('')
SURFACE()
);
#4231=(
BOUNDED_SURFACE()
B_SPLINE_SURFACE(1,2,((#166065,#166066,#166067,#166068,#166069),(#166070,
#166071,#166072,#166073,#166074)),.UNSPECIFIED.,.F.,.F.,.F.)
B_SPLINE_SURFACE_WITH_KNOTS((2,2),(3,2,3),(-1.0690222232507E-6,0.182885378421185),
(0.0734807488197886,0.07365435021991,0.0910144902320513),.UNSPECIFIED.)
GEOMETRIC_REPRESENTATION_ITEM()
RATIONAL_B_SPLINE_SURFACE(((0.99848615229188,0.99848615229188,0.99848615229188,
0.992772345172012,0.990020524139833),(0.99848615229188,0.99848615229188,
0.99848615229188,0.992772345172012,0.990020524139833)))
REPRESENTATION_ITEM('')
SURFACE()
);
#4232=(
BOUNDED_SURFACE()
B_SPLINE_SURFACE(1,2,((#166085,#166086,#166087,#166088,#166089),(#166090,
#166091,#166092,#166093,#166094)),.UNSPECIFIED.,.F.,.F.,.F.)
B_SPLINE_SURFACE_WITH_KNOTS((2,2),(3,2,3),(0.,0.182805892339149),(0.642474614281368,
0.642857142857143,0.659901408087483),.UNSPECIFIED.)
GEOMETRIC_REPRESENTATION_ITEM()
RATIONAL_B_SPLINE_SURFACE(((0.999732896029238,0.999865728939373,1.,0.994017305594881,
0.990889788836284),(0.999732896029238,0.999865728939373,1.,0.994017305594881,
0.990889788836284)))
REPRESENTATION_ITEM('')
SURFACE()
);
#4233=(
BOUNDED_SURFACE()
B_SPLINE_SURFACE(1,2,((#166096,#166097,#166098,#166099,#166100),(#166101,
#166102,#166103,#166104,#166105)),.UNSPECIFIED.,.F.,.F.,.F.)
B_SPLINE_SURFACE_WITH_KNOTS((2,2),(3,2,3),(0.93857685912818,1.),(0.0665257254736559,
0.0714285714285714,0.0736543502199101),.UNSPECIFIED.)
GEOMETRIC_REPRESENTATION_ITEM()
RATIONAL_B_SPLINE_SURFACE(((0.996794362316491,0.998279055819231,1.,0.999218731101516,
0.99848615229188),(0.996794362316491,0.998279055819231,1.,0.999218731101516,
0.99848615229188)))
REPRESENTATION_ITEM('')
SURFACE()
);
#4234=(
BOUNDED_SURFACE()
B_SPLINE_SURFACE(1,2,((#166113,#166114,#166115,#166116,#166117),(#166118,
#166119,#166120,#166121,#166122)),.UNSPECIFIED.,.F.,.F.,.F.)
B_SPLINE_SURFACE_WITH_KNOTS((2,2),(3,2,3),(0.,0.0529045403781231),(0.0665257254736559,
0.0714285714285714,0.073696866868496),.UNSPECIFIED.)
GEOMETRIC_REPRESENTATION_ITEM()
RATIONAL_B_SPLINE_SURFACE(((0.996794362316491,0.998279055819231,1.,0.999203807365457,
0.998458182734337),(0.996794362316491,0.998279055819231,1.,0.999203807365457,
0.998458182734337)))
REPRESENTATION_ITEM('')
SURFACE()
);
#4235=(
BOUNDED_SURFACE()
B_SPLINE_SURFACE(1,2,((#166133,#166134,#166135),(#166136,#166137,#166138)),
 .UNSPECIFIED.,.F.,.F.,.F.)
B_SPLINE_SURFACE_WITH_KNOTS((2,2),(3,3),(0.,0.0528815468798243),(0.659860018385657,
0.666841081426897),.UNSPECIFIED.)
GEOMETRIC_REPRESENTATION_ITEM()
RATIONAL_B_SPLINE_SURFACE(((0.990904995179334,0.989621173673357,0.988816334712146),
(0.990904995179334,0.989621173673357,0.988816334712146)))
REPRESENTATION_ITEM('')
SURFACE()
);
#4236=(
BOUNDED_SURFACE()
B_SPLINE_SURFACE(1,2,((#166140,#166141,#166142,#166143,#166144),(#166145,
#166146,#166147,#166148,#166149)),.UNSPECIFIED.,.F.,.F.,.F.)
B_SPLINE_SURFACE_WITH_KNOTS((2,2),(3,2,3),(0.938550151647345,1.00001008244498),
(0.659832011354057,0.659901408087451,0.666841081426897),.UNSPECIFIED.)
GEOMETRIC_REPRESENTATION_ITEM()
RATIONAL_B_SPLINE_SURFACE(((0.990889788836295,0.990889788836295,0.990889788836295,
0.989616401900863,0.988816334712145),(0.990889788836295,0.990889788836295,
0.990889788836295,0.989616401900863,0.988816334712145)))
REPRESENTATION_ITEM('')
SURFACE()
);
#4237=(
BOUNDED_SURFACE()
B_SPLINE_SURFACE(1,2,((#166151,#166152,#166153,#166154,#166155),(#166156,
#166157,#166158,#166159,#166160)),.UNSPECIFIED.,.F.,.F.,.F.)
B_SPLINE_SURFACE_WITH_KNOTS((2,2),(3,2,3),(-1.06898485868802E-6,0.182885378421184),
(0.0734807488197886,0.07365435021991,0.0910144902320514),.UNSPECIFIED.)
GEOMETRIC_REPRESENTATION_ITEM()
RATIONAL_B_SPLINE_SURFACE(((0.998486152291881,0.998486152291881,0.998486152291881,
0.992772345172012,0.990020524139834),(0.998486152291881,0.998486152291881,
0.998486152291881,0.992772345172012,0.990020524139834)))
REPRESENTATION_ITEM('')
SURFACE()
);
#4238=(
BOUNDED_SURFACE()
B_SPLINE_SURFACE(1,2,((#166171,#166172,#166173,#166174,#166175),(#166176,
#166177,#166178,#166179,#166180)),.UNSPECIFIED.,.F.,.F.,.F.)
B_SPLINE_SURFACE_WITH_KNOTS((2,2),(3,2,3),(0.,0.182805892339149),(0.642474614281368,
0.642857142857143,0.659901408087482),.UNSPECIFIED.)
GEOMETRIC_REPRESENTATION_ITEM()
RATIONAL_B_SPLINE_SURFACE(((0.999732896029238,0.999865728939373,1.,0.994017305594881,
0.990889788836284),(0.999732896029238,0.999865728939373,1.,0.994017305594881,
0.990889788836284)))
REPRESENTATION_ITEM('')
SURFACE()
);
#4239=(
BOUNDED_SURFACE()
B_SPLINE_SURFACE(1,2,((#166182,#166183,#166184,#166185,#166186),(#166187,
#166188,#166189,#166190,#166191)),.UNSPECIFIED.,.F.,.F.,.F.)
B_SPLINE_SURFACE_WITH_KNOTS((2,2),(3,2,3),(0.938576859128178,1.),(0.0665257254736558,
0.0714285714285714,0.0736543502199101),.UNSPECIFIED.)
GEOMETRIC_REPRESENTATION_ITEM()
RATIONAL_B_SPLINE_SURFACE(((0.996794362316491,0.998279055819231,1.,0.999218731101516,
0.99848615229188),(0.996794362316491,0.998279055819231,1.,0.999218731101516,
0.99848615229188)))
REPRESENTATION_ITEM('')
SURFACE()
);
#4240=(
BOUNDED_SURFACE()
B_SPLINE_SURFACE(1,2,((#166199,#166200,#166201,#166202,#166203),(#166204,
#166205,#166206,#166207,#166208)),.UNSPECIFIED.,.F.,.F.,.F.)
B_SPLINE_SURFACE_WITH_KNOTS((2,2),(3,2,3),(0.,0.0529045403781231),(0.0665257254736558,
0.0714285714285714,0.073696866868496),.UNSPECIFIED.)
GEOMETRIC_REPRESENTATION_ITEM()
RATIONAL_B_SPLINE_SURFACE(((0.996794362316491,0.998279055819231,1.,0.999203807365457,
0.998458182734336),(0.996794362316491,0.998279055819231,1.,0.999203807365457,
0.998458182734336)))
REPRESENTATION_ITEM('')
SURFACE()
);
#4241=(
BOUNDED_SURFACE()
B_SPLINE_SURFACE(1,2,((#166219,#166220,#166221),(#166222,#166223,#166224)),
 .UNSPECIFIED.,.F.,.F.,.F.)
B_SPLINE_SURFACE_WITH_KNOTS((2,2),(3,3),(0.,0.0528815468798209),(0.659860018385657,
0.666841081426897),.UNSPECIFIED.)
GEOMETRIC_REPRESENTATION_ITEM()
RATIONAL_B_SPLINE_SURFACE(((0.990904995179334,0.989621173673357,0.988816334712146),
(0.990904995179334,0.989621173673357,0.988816334712146)))
REPRESENTATION_ITEM('')
SURFACE()
);
#4242=(
BOUNDED_SURFACE()
B_SPLINE_SURFACE(1,2,((#166226,#166227,#166228,#166229,#166230),(#166231,
#166232,#166233,#166234,#166235)),.UNSPECIFIED.,.F.,.F.,.F.)
B_SPLINE_SURFACE_WITH_KNOTS((2,2),(3,2,3),(0.938550151647348,1.00001008248998),
(0.659832011354058,0.659901408087452,0.666841081426897),.UNSPECIFIED.)
GEOMETRIC_REPRESENTATION_ITEM()
RATIONAL_B_SPLINE_SURFACE(((0.990889788836295,0.990889788836295,0.990889788836295,
0.989616401900863,0.988816334712145),(0.990889788836295,0.990889788836295,
0.990889788836295,0.989616401900863,0.988816334712145)))
REPRESENTATION_ITEM('')
SURFACE()
);
#4243=(
BOUNDED_SURFACE()
B_SPLINE_SURFACE(1,2,((#166237,#166238,#166239,#166240,#166241),(#166242,
#166243,#166244,#166245,#166246)),.UNSPECIFIED.,.F.,.F.,.F.)
B_SPLINE_SURFACE_WITH_KNOTS((2,2),(3,2,3),(0.,0.182885378421184),(0.0734807488197886,
0.07365435021991,0.0910144902320513),.UNSPECIFIED.)
GEOMETRIC_REPRESENTATION_ITEM()
RATIONAL_B_SPLINE_SURFACE(((0.99848615229188,0.99848615229188,0.99848615229188,
0.992772345172012,0.990020524139833),(0.99848615229188,0.99848615229188,
0.99848615229188,0.992772345172012,0.990020524139833)))
REPRESENTATION_ITEM('')
SURFACE()
);
#4244=(
BOUNDED_SURFACE()
B_SPLINE_SURFACE(1,2,((#166257,#166258,#166259,#166260,#166261),(#166262,
#166263,#166264,#166265,#166266)),.UNSPECIFIED.,.F.,.F.,.F.)
B_SPLINE_SURFACE_WITH_KNOTS((2,2),(3,2,3),(0.,0.182805892339146),(0.642474614281368,
0.642857142857143,0.659901408087482),.UNSPECIFIED.)
GEOMETRIC_REPRESENTATION_ITEM()
RATIONAL_B_SPLINE_SURFACE(((0.999732896029238,0.999865728939373,1.,0.994017305594881,
0.990889788836284),(0.999732896029238,0.999865728939373,1.,0.994017305594881,
0.990889788836284)))
REPRESENTATION_ITEM('')
SURFACE()
);
#4245=(
BOUNDED_SURFACE()
B_SPLINE_SURFACE(1,2,((#166268,#166269,#166270,#166271,#166272),(#166273,
#166274,#166275,#166276,#166277)),.UNSPECIFIED.,.F.,.F.,.F.)
B_SPLINE_SURFACE_WITH_KNOTS((2,2),(3,2,3),(0.93857685912818,1.),(0.0665257254736559,
0.0714285714285714,0.07365435021991),.UNSPECIFIED.)
GEOMETRIC_REPRESENTATION_ITEM()
RATIONAL_B_SPLINE_SURFACE(((0.996794362316491,0.998279055819231,1.,0.999218731101516,
0.99848615229188),(0.996794362316491,0.998279055819231,1.,0.999218731101516,
0.99848615229188)))
REPRESENTATION_ITEM('')
SURFACE()
);
#4246=(
BOUNDED_SURFACE()
B_SPLINE_SURFACE(1,2,((#166285,#166286,#166287,#166288,#166289),(#166290,
#166291,#166292,#166293,#166294)),.UNSPECIFIED.,.F.,.F.,.F.)
B_SPLINE_SURFACE_WITH_KNOTS((2,2),(3,2,3),(0.,0.0529045403781213),(0.0665257254736559,
0.0714285714285714,0.073696866868496),.UNSPECIFIED.)
GEOMETRIC_REPRESENTATION_ITEM()
RATIONAL_B_SPLINE_SURFACE(((0.996794362316491,0.998279055819231,1.,0.999203807365457,
0.998458182734337),(0.996794362316491,0.998279055819231,1.,0.999203807365457,
0.998458182734337)))
REPRESENTATION_ITEM('')
SURFACE()
);
#4247=(
BOUNDED_SURFACE()
B_SPLINE_SURFACE(1,2,((#166305,#166306,#166307),(#166308,#166309,#166310)),
 .UNSPECIFIED.,.F.,.F.,.F.)
B_SPLINE_SURFACE_WITH_KNOTS((2,2),(3,3),(0.,0.0528815468798213),(0.659860018385657,
0.666841081426897),.UNSPECIFIED.)
GEOMETRIC_REPRESENTATION_ITEM()
RATIONAL_B_SPLINE_SURFACE(((0.990904995179334,0.989621173673357,0.988816334712145),
(0.990904995179334,0.989621173673357,0.988816334712145)))
REPRESENTATION_ITEM('')
SURFACE()
);
#4248=(
BOUNDED_SURFACE()
B_SPLINE_SURFACE(1,2,((#166312,#166313,#166314,#166315,#166316),(#166317,
#166318,#166319,#166320,#166321)),.UNSPECIFIED.,.F.,.F.,.F.)
B_SPLINE_SURFACE_WITH_KNOTS((2,2),(3,2,3),(0.93855015164735,1.00001008250064),
(0.659832011354058,0.659901408087452,0.666841081426897),.UNSPECIFIED.)
GEOMETRIC_REPRESENTATION_ITEM()
RATIONAL_B_SPLINE_SURFACE(((0.990889788836295,0.990889788836295,0.990889788836295,
0.989616401900864,0.988816334712146),(0.990889788836295,0.990889788836295,
0.990889788836295,0.989616401900864,0.988816334712146)))
REPRESENTATION_ITEM('')
SURFACE()
);
#4249=(
BOUNDED_SURFACE()
B_SPLINE_SURFACE(1,2,((#166323,#166324,#166325,#166326,#166327),(#166328,
#166329,#166330,#166331,#166332)),.UNSPECIFIED.,.F.,.F.,.F.)
B_SPLINE_SURFACE_WITH_KNOTS((2,2),(3,2,3),(-1.07111455693367E-6,0.182885378421183),
(0.0734807488197886,0.07365435021991,0.0910144902320513),.UNSPECIFIED.)
GEOMETRIC_REPRESENTATION_ITEM()
RATIONAL_B_SPLINE_SURFACE(((0.99848615229188,0.99848615229188,0.99848615229188,
0.992772345172012,0.990020524139833),(0.99848615229188,0.99848615229188,
0.99848615229188,0.992772345172012,0.990020524139833)))
REPRESENTATION_ITEM('')
SURFACE()
);
#4250=(
BOUNDED_SURFACE()
B_SPLINE_SURFACE(1,2,((#166343,#166344,#166345,#166346,#166347),(#166348,
#166349,#166350,#166351,#166352)),.UNSPECIFIED.,.F.,.F.,.F.)
B_SPLINE_SURFACE_WITH_KNOTS((2,2),(3,2,3),(0.,0.182805892339148),(0.642474614281367,
0.642857142857143,0.659901408087482),.UNSPECIFIED.)
GEOMETRIC_REPRESENTATION_ITEM()
RATIONAL_B_SPLINE_SURFACE(((0.999732896029238,0.999865728939373,1.,0.994017305594881,
0.990889788836284),(0.999732896029238,0.999865728939373,1.,0.994017305594881,
0.990889788836284)))
REPRESENTATION_ITEM('')
SURFACE()
);
#4251=(
BOUNDED_SURFACE()
B_SPLINE_SURFACE(1,2,((#166354,#166355,#166356,#166357,#166358),(#166359,
#166360,#166361,#166362,#166363)),.UNSPECIFIED.,.F.,.F.,.F.)
B_SPLINE_SURFACE_WITH_KNOTS((2,2),(3,2,3),(0.938576859128178,1.),(0.0665257254736559,
0.0714285714285714,0.0736543502199101),.UNSPECIFIED.)
GEOMETRIC_REPRESENTATION_ITEM()
RATIONAL_B_SPLINE_SURFACE(((0.996794362316491,0.998279055819231,1.,0.999218731101516,
0.99848615229188),(0.996794362316491,0.998279055819231,1.,0.999218731101516,
0.99848615229188)))
REPRESENTATION_ITEM('')
SURFACE()
);
#4252=(
BOUNDED_SURFACE()
B_SPLINE_SURFACE(1,2,((#166370,#166371,#166372,#166373,#166374),(#166375,
#166376,#166377,#166378,#166379)),.UNSPECIFIED.,.F.,.F.,.F.)
B_SPLINE_SURFACE_WITH_KNOTS((2,2),(3,2,3),(0.,0.0529045403781227),(0.0665257254736559,
0.0714285714285714,0.073696866868496),.UNSPECIFIED.)
GEOMETRIC_REPRESENTATION_ITEM()
RATIONAL_B_SPLINE_SURFACE(((0.996794362316491,0.998279055819231,1.,0.999203807365457,
0.998458182734337),(0.996794362316491,0.998279055819231,1.,0.999203807365457,
0.998458182734337)))
REPRESENTATION_ITEM('')
SURFACE()
);
#4253=(
BOUNDED_SURFACE()
B_SPLINE_SURFACE(1,2,((#166390,#166391,#166392),(#166393,#166394,#166395)),
 .UNSPECIFIED.,.F.,.F.,.F.)
B_SPLINE_SURFACE_WITH_KNOTS((2,2),(3,3),(0.,0.0528815468798243),(0.659860018385657,
0.666841081426897),.UNSPECIFIED.)
GEOMETRIC_REPRESENTATION_ITEM()
RATIONAL_B_SPLINE_SURFACE(((0.990904995179334,0.989621173673357,0.988816334712146),
(0.990904995179334,0.989621173673357,0.988816334712145)))
REPRESENTATION_ITEM('')
SURFACE()
);
#4254=(
BOUNDED_SURFACE()
B_SPLINE_SURFACE(1,2,((#166397,#166398,#166399,#166400,#166401),(#166402,
#166403,#166404,#166405,#166406)),.UNSPECIFIED.,.F.,.F.,.F.)
B_SPLINE_SURFACE_WITH_KNOTS((2,2),(3,2,3),(0.938550151647349,1.00001008247581),
(0.659832011354058,0.659901408087452,0.666841081426897),.UNSPECIFIED.)
GEOMETRIC_REPRESENTATION_ITEM()
RATIONAL_B_SPLINE_SURFACE(((0.990889788836295,0.990889788836295,0.990889788836295,
0.989616401900864,0.988816334712146),(0.990889788836295,0.990889788836295,
0.990889788836295,0.989616401900864,0.988816334712146)))
REPRESENTATION_ITEM('')
SURFACE()
);
#4255=(
BOUNDED_SURFACE()
B_SPLINE_SURFACE(1,2,((#166408,#166409,#166410,#166411,#166412),(#166413,
#166414,#166415,#166416,#166417)),.UNSPECIFIED.,.F.,.F.,.F.)
B_SPLINE_SURFACE_WITH_KNOTS((2,2),(3,2,3),(-1.07080442310849E-6,0.182885378421184),
(0.0734807488197886,0.07365435021991,0.0910144902320513),.UNSPECIFIED.)
GEOMETRIC_REPRESENTATION_ITEM()
RATIONAL_B_SPLINE_SURFACE(((0.99848615229188,0.99848615229188,0.99848615229188,
0.992772345172012,0.990020524139833),(0.99848615229188,0.99848615229188,
0.99848615229188,0.992772345172012,0.990020524139833)))
REPRESENTATION_ITEM('')
SURFACE()
);
#4256=(
BOUNDED_SURFACE()
B_SPLINE_SURFACE(1,2,((#166428,#166429,#166430,#166431,#166432),(#166433,
#166434,#166435,#166436,#166437)),.UNSPECIFIED.,.F.,.F.,.F.)
B_SPLINE_SURFACE_WITH_KNOTS((2,2),(3,2,3),(0.,0.182805892339143),(0.642474614281368,
0.642857142857143,0.659901408087482),.UNSPECIFIED.)
GEOMETRIC_REPRESENTATION_ITEM()
RATIONAL_B_SPLINE_SURFACE(((0.999732896029238,0.999865728939373,1.,0.994017305594881,
0.990889788836284),(0.999732896029238,0.999865728939373,1.,0.994017305594881,
0.990889788836284)))
REPRESENTATION_ITEM('')
SURFACE()
);
#4257=(
BOUNDED_SURFACE()
B_SPLINE_SURFACE(1,2,((#166439,#166440,#166441,#166442,#166443),(#166444,
#166445,#166446,#166447,#166448)),.UNSPECIFIED.,.F.,.F.,.F.)
B_SPLINE_SURFACE_WITH_KNOTS((2,2),(3,2,3),(0.938576859128179,1.),(0.0665257254736559,
0.0714285714285714,0.07365435021991),.UNSPECIFIED.)
GEOMETRIC_REPRESENTATION_ITEM()
RATIONAL_B_SPLINE_SURFACE(((0.996794362316491,0.998279055819231,1.,0.999218731101516,
0.99848615229188),(0.996794362316491,0.998279055819231,1.,0.999218731101516,
0.99848615229188)))
REPRESENTATION_ITEM('')
SURFACE()
);
#4258=(
BOUNDED_SURFACE()
B_SPLINE_SURFACE(1,2,((#166456,#166457,#166458,#166459,#166460),(#166461,
#166462,#166463,#166464,#166465)),.UNSPECIFIED.,.F.,.F.,.F.)
B_SPLINE_SURFACE_WITH_KNOTS((2,2),(3,2,3),(0.,0.0529045403781224),(0.066525725473656,
0.0714285714285714,0.073696866868496),.UNSPECIFIED.)
GEOMETRIC_REPRESENTATION_ITEM()
RATIONAL_B_SPLINE_SURFACE(((0.996794362316491,0.998279055819231,1.,0.999203807365457,
0.998458182734337),(0.996794362316491,0.998279055819231,1.,0.999203807365457,
0.998458182734337)))
REPRESENTATION_ITEM('')
SURFACE()
);
#4259=(
BOUNDED_SURFACE()
B_SPLINE_SURFACE(1,2,((#166476,#166477,#166478),(#166479,#166480,#166481)),
 .UNSPECIFIED.,.F.,.F.,.F.)
B_SPLINE_SURFACE_WITH_KNOTS((2,2),(3,3),(0.,0.0528815468798206),(0.659860018385657,
0.666841081426896),.UNSPECIFIED.)
GEOMETRIC_REPRESENTATION_ITEM()
RATIONAL_B_SPLINE_SURFACE(((0.990904995179334,0.989621173673357,0.988816334712146),
(0.990904995179334,0.989621173673357,0.988816334712145)))
REPRESENTATION_ITEM('')
SURFACE()
);
#4260=(
BOUNDED_SURFACE()
B_SPLINE_SURFACE(1,2,((#166483,#166484,#166485,#166486,#166487),(#166488,
#166489,#166490,#166491,#166492)),.UNSPECIFIED.,.F.,.F.,.F.)
B_SPLINE_SURFACE_WITH_KNOTS((2,2),(3,2,3),(0.938550151647356,1.0000100824502),
(0.659832011354058,0.659901408087452,0.666841081426897),.UNSPECIFIED.)
GEOMETRIC_REPRESENTATION_ITEM()
RATIONAL_B_SPLINE_SURFACE(((0.990889788836295,0.990889788836295,0.990889788836295,
0.989616401900864,0.988816334712146),(0.990889788836295,0.990889788836295,
0.990889788836295,0.989616401900864,0.988816334712146)))
REPRESENTATION_ITEM('')
SURFACE()
);
#4261=(
BOUNDED_SURFACE()
B_SPLINE_SURFACE(1,2,((#166494,#166495,#166496,#166497,#166498),(#166499,
#166500,#166501,#166502,#166503)),.UNSPECIFIED.,.F.,.F.,.F.)
B_SPLINE_SURFACE_WITH_KNOTS((2,2),(3,2,3),(0.,0.182885378421178),(0.0734807488197886,
0.07365435021991,0.0910144902320512),.UNSPECIFIED.)
GEOMETRIC_REPRESENTATION_ITEM()
RATIONAL_B_SPLINE_SURFACE(((0.998486152291881,0.998486152291881,0.998486152291881,
0.992772345172012,0.990020524139834),(0.998486152291881,0.998486152291881,
0.998486152291881,0.992772345172012,0.990020524139834)))
REPRESENTATION_ITEM('')
SURFACE()
);
#4262=(
BOUNDED_SURFACE()
B_SPLINE_SURFACE(1,2,((#166514,#166515,#166516,#166517,#166518),(#166519,
#166520,#166521,#166522,#166523)),.UNSPECIFIED.,.F.,.F.,.F.)
B_SPLINE_SURFACE_WITH_KNOTS((2,2),(3,2,3),(0.,0.182805892339139),(0.642474614281368,
0.642857142857143,0.659901408087483),.UNSPECIFIED.)
GEOMETRIC_REPRESENTATION_ITEM()
RATIONAL_B_SPLINE_SURFACE(((0.999732896029238,0.999865728939373,1.,0.994017305594881,
0.990889788836284),(0.999732896029238,0.999865728939373,1.,0.994017305594881,
0.990889788836284)))
REPRESENTATION_ITEM('')
SURFACE()
);
#4263=(
BOUNDED_SURFACE()
B_SPLINE_SURFACE(1,2,((#166525,#166526,#166527,#166528,#166529),(#166530,
#166531,#166532,#166533,#166534)),.UNSPECIFIED.,.F.,.F.,.F.)
B_SPLINE_SURFACE_WITH_KNOTS((2,2),(3,2,3),(0.938576859128171,1.),(0.0665257254736558,
0.0714285714285714,0.0736543502199103),.UNSPECIFIED.)
GEOMETRIC_REPRESENTATION_ITEM()
RATIONAL_B_SPLINE_SURFACE(((0.996794362316491,0.998279055819231,1.,0.999218731101516,
0.99848615229188),(0.996794362316491,0.998279055819231,1.,0.999218731101516,
0.99848615229188)))
REPRESENTATION_ITEM('')
SURFACE()
);
#4264=(
BOUNDED_SURFACE()
B_SPLINE_SURFACE(1,2,((#166541,#166542,#166543,#166544,#166545),(#166546,
#166547,#166548,#166549,#166550)),.UNSPECIFIED.,.F.,.F.,.F.)
B_SPLINE_SURFACE_WITH_KNOTS((2,2),(3,2,3),(0.,0.0529045403781233),(0.0665257254736558,
0.0714285714285714,0.0736968668684958),.UNSPECIFIED.)
GEOMETRIC_REPRESENTATION_ITEM()
RATIONAL_B_SPLINE_SURFACE(((0.996794362316491,0.998279055819231,1.,0.999203807365457,
0.998458182734337),(0.996794362316491,0.998279055819231,1.,0.999203807365457,
0.998458182734337)))
REPRESENTATION_ITEM('')
SURFACE()
);
#4265=(
BOUNDED_SURFACE()
B_SPLINE_SURFACE(1,2,((#166561,#166562,#166563),(#166564,#166565,#166566)),
 .UNSPECIFIED.,.F.,.F.,.F.)
B_SPLINE_SURFACE_WITH_KNOTS((2,2),(3,3),(0.,0.052881546879817),(0.659860018385656,
0.666841081426896),.UNSPECIFIED.)
GEOMETRIC_REPRESENTATION_ITEM()
RATIONAL_B_SPLINE_SURFACE(((0.990904995179334,0.989621173673357,0.988816334712146),
(0.990904995179334,0.989621173673357,0.988816334712146)))
REPRESENTATION_ITEM('')
SURFACE()
);
#4266=(
BOUNDED_SURFACE()
B_SPLINE_SURFACE(1,2,((#166568,#166569,#166570,#166571,#166572),(#166573,
#166574,#166575,#166576,#166577)),.UNSPECIFIED.,.F.,.F.,.F.)
B_SPLINE_SURFACE_WITH_KNOTS((2,2),(3,2,3),(0.938550151647354,1.00001008250033),
(0.659832011354058,0.659901408087452,0.666841081426896),.UNSPECIFIED.)
GEOMETRIC_REPRESENTATION_ITEM()
RATIONAL_B_SPLINE_SURFACE(((0.990889788836295,0.990889788836295,0.990889788836295,
0.989616401900864,0.988816334712146),(0.990889788836295,0.990889788836295,
0.990889788836295,0.989616401900864,0.988816334712146)))
REPRESENTATION_ITEM('')
SURFACE()
);
#4267=(
BOUNDED_SURFACE()
B_SPLINE_SURFACE(1,2,((#166579,#166580,#166581,#166582,#166583),(#166584,
#166585,#166586,#166587,#166588)),.UNSPECIFIED.,.F.,.F.,.F.)
B_SPLINE_SURFACE_WITH_KNOTS((2,2),(3,2,3),(-1.07087661006151E-6,0.182885378421182),
(0.0734807488197878,0.0736543502199092,0.0910144902320526),
 .UNSPECIFIED.)
GEOMETRIC_REPRESENTATION_ITEM()
RATIONAL_B_SPLINE_SURFACE(((0.998486152291881,0.998486152291881,0.998486152291881,
0.992772345172012,0.990020524139833),(0.998486152291881,0.998486152291881,
0.998486152291881,0.992772345172012,0.990020524139833)))
REPRESENTATION_ITEM('')
SURFACE()
);
#4268=(
BOUNDED_SURFACE()
B_SPLINE_SURFACE(1,2,((#166599,#166600,#166601,#166602,#166603),(#166604,
#166605,#166606,#166607,#166608)),.UNSPECIFIED.,.F.,.F.,.F.)
B_SPLINE_SURFACE_WITH_KNOTS((2,2),(3,2,3),(0.,0.182805892339143),(0.642474614281368,
0.642857142857143,0.659901408087483),.UNSPECIFIED.)
GEOMETRIC_REPRESENTATION_ITEM()
RATIONAL_B_SPLINE_SURFACE(((0.999732896029238,0.999865728939373,1.,0.994017305594881,
0.990889788836284),(0.999732896029238,0.999865728939373,1.,0.994017305594881,
0.990889788836284)))
REPRESENTATION_ITEM('')
SURFACE()
);
#4269=(
BOUNDED_SURFACE()
B_SPLINE_SURFACE(1,2,((#166610,#166611,#166612,#166613,#166614),(#166615,
#166616,#166617,#166618,#166619)),.UNSPECIFIED.,.F.,.F.,.F.)
B_SPLINE_SURFACE_WITH_KNOTS((2,2),(3,2,3),(0.938576859128179,1.),(0.066525725473656,
0.0714285714285714,0.0736543502199102),.UNSPECIFIED.)
GEOMETRIC_REPRESENTATION_ITEM()
RATIONAL_B_SPLINE_SURFACE(((0.996794362316491,0.998279055819231,1.,0.999218731101516,
0.99848615229188),(0.996794362316491,0.998279055819231,1.,0.999218731101516,
0.99848615229188)))
REPRESENTATION_ITEM('')
SURFACE()
);
#4270=(
BOUNDED_SURFACE()
B_SPLINE_SURFACE(1,2,((#166626,#166627,#166628,#166629,#166630),(#166631,
#166632,#166633,#166634,#166635)),.UNSPECIFIED.,.F.,.F.,.F.)
B_SPLINE_SURFACE_WITH_KNOTS((2,2),(3,2,3),(0.,0.05290454037812),(0.066525725473656,
0.0714285714285714,0.0736968668684962),.UNSPECIFIED.)
GEOMETRIC_REPRESENTATION_ITEM()
RATIONAL_B_SPLINE_SURFACE(((0.996794362316491,0.998279055819231,1.,0.999203807365457,
0.998458182734337),(0.996794362316491,0.998279055819231,1.,0.999203807365457,
0.998458182734337)))
REPRESENTATION_ITEM('')
SURFACE()
);
#4271=(
BOUNDED_SURFACE()
B_SPLINE_SURFACE(1,2,((#166646,#166647,#166648),(#166649,#166650,#166651)),
 .UNSPECIFIED.,.F.,.F.,.F.)
B_SPLINE_SURFACE_WITH_KNOTS((2,2),(3,3),(0.,0.0528815468798192),(0.659860018385657,
0.666841081426896),.UNSPECIFIED.)
GEOMETRIC_REPRESENTATION_ITEM()
RATIONAL_B_SPLINE_SURFACE(((0.990904995179334,0.989621173673357,0.988816334712146),
(0.990904995179334,0.989621173673357,0.988816334712146)))
REPRESENTATION_ITEM('')
SURFACE()
);
#4272=(
BOUNDED_SURFACE()
B_SPLINE_SURFACE(1,2,((#166653,#166654,#166655,#166656,#166657),(#166658,
#166659,#166660,#166661,#166662)),.UNSPECIFIED.,.F.,.F.,.F.)
B_SPLINE_SURFACE_WITH_KNOTS((2,2),(3,2,3),(0.938550151647622,1.00001008251049),
(0.659832011354088,0.659901408087482,0.666841081426896),.UNSPECIFIED.)
GEOMETRIC_REPRESENTATION_ITEM()
RATIONAL_B_SPLINE_SURFACE(((0.990889788836284,0.990889788836284,0.990889788836284,
0.98961640190086,0.988816334712146),(0.990889788836284,0.990889788836284,
0.990889788836284,0.98961640190086,0.988816334712146)))
REPRESENTATION_ITEM('')
SURFACE()
);
#4273=(
BOUNDED_SURFACE()
B_SPLINE_SURFACE(1,2,((#166664,#166665,#166666,#166667,#166668),(#166669,
#166670,#166671,#166672,#166673)),.UNSPECIFIED.,.F.,.F.,.F.)
B_SPLINE_SURFACE_WITH_KNOTS((2,2),(3,2,3),(0.,0.182885378421183),(0.0734807488197887,
0.0736543502199101,0.0910144902320514),.UNSPECIFIED.)
GEOMETRIC_REPRESENTATION_ITEM()
RATIONAL_B_SPLINE_SURFACE(((0.998486152291881,0.998486152291881,0.998486152291881,
0.992772345172012,0.990020524139833),(0.998486152291881,0.998486152291881,
0.998486152291881,0.992772345172012,0.990020524139833)))
REPRESENTATION_ITEM('')
SURFACE()
);
#4274=(
BOUNDED_SURFACE()
B_SPLINE_SURFACE(1,2,((#166684,#166685,#166686,#166687,#166688),(#166689,
#166690,#166691,#166692,#166693)),.UNSPECIFIED.,.F.,.F.,.F.)
B_SPLINE_SURFACE_WITH_KNOTS((2,2),(3,2,3),(0.,0.182805892339143),(0.642474614281368,
0.642857142857143,0.659901408087483),.UNSPECIFIED.)
GEOMETRIC_REPRESENTATION_ITEM()
RATIONAL_B_SPLINE_SURFACE(((0.999732896029238,0.999865728939373,1.,0.994017305594881,
0.990889788836284),(0.999732896029238,0.999865728939373,1.,0.994017305594881,
0.990889788836284)))
REPRESENTATION_ITEM('')
SURFACE()
);
#4275=(
BOUNDED_SURFACE()
B_SPLINE_SURFACE(1,2,((#166695,#166696,#166697,#166698,#166699),(#166700,
#166701,#166702,#166703,#166704)),.UNSPECIFIED.,.F.,.F.,.F.)
B_SPLINE_SURFACE_WITH_KNOTS((2,2),(3,2,3),(0.938576859128176,1.),(0.0665257254736562,
0.0714285714285714,0.0736543502199103),.UNSPECIFIED.)
GEOMETRIC_REPRESENTATION_ITEM()
RATIONAL_B_SPLINE_SURFACE(((0.996794362316491,0.998279055819231,1.,0.999218731101516,
0.99848615229188),(0.996794362316491,0.998279055819231,1.,0.999218731101516,
0.99848615229188)))
REPRESENTATION_ITEM('')
SURFACE()
);
#4276=(
BOUNDED_SURFACE()
B_SPLINE_SURFACE(1,2,((#166712,#166713,#166714,#166715,#166716),(#166717,
#166718,#166719,#166720,#166721)),.UNSPECIFIED.,.F.,.F.,.F.)
B_SPLINE_SURFACE_WITH_KNOTS((2,2),(3,2,3),(0.,0.0529045403781185),(0.0665257254736562,
0.0714285714285714,0.073696866868496),.UNSPECIFIED.)
GEOMETRIC_REPRESENTATION_ITEM()
RATIONAL_B_SPLINE_SURFACE(((0.996794362316491,0.998279055819231,1.,0.999203807365457,
0.998458182734336),(0.996794362316491,0.998279055819231,1.,0.999203807365457,
0.998458182734336)))
REPRESENTATION_ITEM('')
SURFACE()
);
#4277=(
BOUNDED_SURFACE()
B_SPLINE_SURFACE(1,2,((#166732,#166733,#166734),(#166735,#166736,#166737)),
 .UNSPECIFIED.,.F.,.F.,.F.)
B_SPLINE_SURFACE_WITH_KNOTS((2,2),(3,3),(0.,0.0528815468798166),(0.659860018385657,
0.666841081426896),.UNSPECIFIED.)
GEOMETRIC_REPRESENTATION_ITEM()
RATIONAL_B_SPLINE_SURFACE(((0.990904995179334,0.989621173673357,0.988816334712146),
(0.990904995179334,0.989621173673357,0.988816334712146)))
REPRESENTATION_ITEM('')
SURFACE()
);
#4278=(
BOUNDED_SURFACE()
B_SPLINE_SURFACE(1,2,((#166739,#166740,#166741,#166742,#166743),(#166744,
#166745,#166746,#166747,#166748)),.UNSPECIFIED.,.F.,.F.,.F.)
B_SPLINE_SURFACE_WITH_KNOTS((2,2),(3,2,3),(0.938550151647625,1.00001008244618),
(0.659832011354088,0.659901408087482,0.666841081426896),.UNSPECIFIED.)
GEOMETRIC_REPRESENTATION_ITEM()
RATIONAL_B_SPLINE_SURFACE(((0.990889788836284,0.990889788836284,0.990889788836284,
0.98961640190086,0.988816334712146),(0.990889788836284,0.990889788836284,
0.990889788836284,0.98961640190086,0.988816334712146)))
REPRESENTATION_ITEM('')
SURFACE()
);
#4279=(
BOUNDED_SURFACE()
B_SPLINE_SURFACE(1,2,((#166750,#166751,#166752,#166753,#166754),(#166755,
#166756,#166757,#166758,#166759)),.UNSPECIFIED.,.F.,.F.,.F.)
B_SPLINE_SURFACE_WITH_KNOTS((2,2),(3,2,3),(-1.06918541742082E-6,0.182885378421186),
(0.0734807488197885,0.0736543502199099,0.0910144902320512),
 .UNSPECIFIED.)
GEOMETRIC_REPRESENTATION_ITEM()
RATIONAL_B_SPLINE_SURFACE(((0.99848615229188,0.99848615229188,0.99848615229188,
0.992772345172012,0.990020524139833),(0.99848615229188,0.99848615229188,
0.99848615229188,0.992772345172012,0.990020524139833)))
REPRESENTATION_ITEM('')
SURFACE()
);
#4280=(
BOUNDED_SURFACE()
B_SPLINE_SURFACE(1,2,((#166770,#166771,#166772,#166773,#166774),(#166775,
#166776,#166777,#166778,#166779)),.UNSPECIFIED.,.F.,.F.,.F.)
B_SPLINE_SURFACE_WITH_KNOTS((2,2),(3,2,3),(0.,0.182805892339149),(0.642474614281367,
0.642857142857143,0.659901408087483),.UNSPECIFIED.)
GEOMETRIC_REPRESENTATION_ITEM()
RATIONAL_B_SPLINE_SURFACE(((0.999732896029238,0.999865728939373,1.,0.994017305594881,
0.990889788836284),(0.999732896029238,0.999865728939373,1.,0.994017305594881,
0.990889788836284)))
REPRESENTATION_ITEM('')
SURFACE()
);
#4281=(
BOUNDED_SURFACE()
B_SPLINE_SURFACE(1,2,((#166781,#166782,#166783,#166784,#166785),(#166786,
#166787,#166788,#166789,#166790)),.UNSPECIFIED.,.F.,.F.,.F.)
B_SPLINE_SURFACE_WITH_KNOTS((2,2),(3,2,3),(0.938576859128177,1.),(0.0665257254736559,
0.0714285714285714,0.0736543502199103),.UNSPECIFIED.)
GEOMETRIC_REPRESENTATION_ITEM()
RATIONAL_B_SPLINE_SURFACE(((0.996794362316491,0.998279055819231,1.,0.999218731101516,
0.99848615229188),(0.996794362316491,0.998279055819231,1.,0.999218731101516,
0.99848615229188)))
REPRESENTATION_ITEM('')
SURFACE()
);
#4282=(
BOUNDED_SURFACE()
B_SPLINE_SURFACE(1,2,((#166798,#166799,#166800,#166801,#166802),(#166803,
#166804,#166805,#166806,#166807)),.UNSPECIFIED.,.F.,.F.,.F.)
B_SPLINE_SURFACE_WITH_KNOTS((2,2),(3,2,3),(0.,0.0529045403781202),(0.0665257254736559,
0.0714285714285714,0.0736968668684961),.UNSPECIFIED.)
GEOMETRIC_REPRESENTATION_ITEM()
RATIONAL_B_SPLINE_SURFACE(((0.996794362316491,0.998279055819231,1.,0.999203807365457,
0.998458182734336),(0.996794362316491,0.998279055819231,1.,0.999203807365457,
0.998458182734336)))
REPRESENTATION_ITEM('')
SURFACE()
);
#4283=(
BOUNDED_SURFACE()
B_SPLINE_SURFACE(1,2,((#166818,#166819,#166820),(#166821,#166822,#166823)),
 .UNSPECIFIED.,.F.,.F.,.F.)
B_SPLINE_SURFACE_WITH_KNOTS((2,2),(3,3),(0.,0.052881546879819),(0.659860018385657,
0.666841081426897),.UNSPECIFIED.)
GEOMETRIC_REPRESENTATION_ITEM()
RATIONAL_B_SPLINE_SURFACE(((0.990904995179334,0.989621173673357,0.988816334712145),
(0.990904995179334,0.989621173673357,0.988816334712145)))
REPRESENTATION_ITEM('')
SURFACE()
);
#4284=(
BOUNDED_SURFACE()
B_SPLINE_SURFACE(1,2,((#166825,#166826,#166827,#166828,#166829),(#166830,
#166831,#166832,#166833,#166834)),.UNSPECIFIED.,.F.,.F.,.F.)
B_SPLINE_SURFACE_WITH_KNOTS((2,2),(3,2,3),(0.938550151647619,1.00001008245349),
(0.659832011354088,0.659901408087482,0.666841081426897),.UNSPECIFIED.)
GEOMETRIC_REPRESENTATION_ITEM()
RATIONAL_B_SPLINE_SURFACE(((0.990889788836284,0.990889788836284,0.990889788836284,
0.98961640190086,0.988816334712146),(0.990889788836284,0.990889788836284,
0.990889788836284,0.98961640190086,0.988816334712146)))
REPRESENTATION_ITEM('')
SURFACE()
);
#4285=(
BOUNDED_SURFACE()
B_SPLINE_SURFACE(1,2,((#166836,#166837,#166838,#166839,#166840),(#166841,
#166842,#166843,#166844,#166845)),.UNSPECIFIED.,.F.,.F.,.F.)
B_SPLINE_SURFACE_WITH_KNOTS((2,2),(3,2,3),(0.,0.182885378421186),(0.0734807488197886,
0.07365435021991,0.0910144902320513),.UNSPECIFIED.)
GEOMETRIC_REPRESENTATION_ITEM()
RATIONAL_B_SPLINE_SURFACE(((0.99848615229188,0.99848615229188,0.99848615229188,
0.992772345172012,0.990020524139833),(0.99848615229188,0.99848615229188,
0.99848615229188,0.992772345172012,0.990020524139833)))
REPRESENTATION_ITEM('')
SURFACE()
);
#4286=(
BOUNDED_SURFACE()
B_SPLINE_SURFACE(1,2,((#166856,#166857,#166858,#166859,#166860),(#166861,
#166862,#166863,#166864,#166865)),.UNSPECIFIED.,.F.,.F.,.F.)
B_SPLINE_SURFACE_WITH_KNOTS((2,2),(3,2,3),(0.,0.182805892339151),(0.642474614281368,
0.642857142857143,0.659901408087483),.UNSPECIFIED.)
GEOMETRIC_REPRESENTATION_ITEM()
RATIONAL_B_SPLINE_SURFACE(((0.999732896029238,0.999865728939373,1.,0.994017305594881,
0.990889788836284),(0.999732896029238,0.999865728939373,1.,0.994017305594881,
0.990889788836284)))
REPRESENTATION_ITEM('')
SURFACE()
);
#4287=(
BOUNDED_SURFACE()
B_SPLINE_SURFACE(1,2,((#166867,#166868,#166869,#166870,#166871),(#166872,
#166873,#166874,#166875,#166876)),.UNSPECIFIED.,.F.,.F.,.F.)
B_SPLINE_SURFACE_WITH_KNOTS((2,2),(3,2,3),(0.938576859128184,1.),(0.0665257254736563,
0.0714285714285714,0.07365435021991),.UNSPECIFIED.)
GEOMETRIC_REPRESENTATION_ITEM()
RATIONAL_B_SPLINE_SURFACE(((0.996794362316491,0.998279055819231,1.,0.999218731101516,
0.99848615229188),(0.996794362316491,0.998279055819231,1.,0.999218731101516,
0.99848615229188)))
REPRESENTATION_ITEM('')
SURFACE()
);
#4288=(
BOUNDED_SURFACE()
B_SPLINE_SURFACE(1,2,((#166883,#166884,#166885,#166886,#166887),(#166888,
#166889,#166890,#166891,#166892)),.UNSPECIFIED.,.F.,.F.,.F.)
B_SPLINE_SURFACE_WITH_KNOTS((2,2),(3,2,3),(0.,0.0529045403781217),(0.0665257254736563,
0.0714285714285714,0.073696866868496),.UNSPECIFIED.)
GEOMETRIC_REPRESENTATION_ITEM()
RATIONAL_B_SPLINE_SURFACE(((0.996794362316491,0.998279055819231,1.,0.999203807365457,
0.998458182734337),(0.996794362316491,0.998279055819231,1.,0.999203807365457,
0.998458182734337)))
REPRESENTATION_ITEM('')
SURFACE()
);
#4289=(
BOUNDED_SURFACE()
B_SPLINE_SURFACE(1,2,((#166903,#166904,#166905),(#166906,#166907,#166908)),
 .UNSPECIFIED.,.F.,.F.,.F.)
B_SPLINE_SURFACE_WITH_KNOTS((2,2),(3,3),(0.,0.0528815468798244),(0.659860018385657,
0.666841081426897),.UNSPECIFIED.)
GEOMETRIC_REPRESENTATION_ITEM()
RATIONAL_B_SPLINE_SURFACE(((0.990904995179334,0.989621173673357,0.988816334712146),
(0.990904995179334,0.989621173673357,0.988816334712146)))
REPRESENTATION_ITEM('')
SURFACE()
);
#4290=(
BOUNDED_SURFACE()
B_SPLINE_SURFACE(1,2,((#166910,#166911,#166912,#166913,#166914),(#166915,
#166916,#166917,#166918,#166919)),.UNSPECIFIED.,.F.,.F.,.F.)
B_SPLINE_SURFACE_WITH_KNOTS((2,2),(3,2,3),(0.93855015164762,1.0000100824797),
(0.659832011354088,0.659901408087482,0.666841081426897),.UNSPECIFIED.)
GEOMETRIC_REPRESENTATION_ITEM()
RATIONAL_B_SPLINE_SURFACE(((0.990889788836284,0.990889788836284,0.990889788836284,
0.98961640190086,0.988816334712146),(0.990889788836284,0.990889788836284,
0.990889788836284,0.98961640190086,0.988816334712146)))
REPRESENTATION_ITEM('')
SURFACE()
);
#4291=(
BOUNDED_SURFACE()
B_SPLINE_SURFACE(1,2,((#166921,#166922,#166923,#166924,#166925),(#166926,
#166927,#166928,#166929,#166930)),.UNSPECIFIED.,.F.,.F.,.F.)
B_SPLINE_SURFACE_WITH_KNOTS((2,2),(3,2,3),(0.,0.182885378421181),(0.0734807488197886,
0.07365435021991,0.0910144902320513),.UNSPECIFIED.)
GEOMETRIC_REPRESENTATION_ITEM()
RATIONAL_B_SPLINE_SURFACE(((0.998486152291881,0.998486152291881,0.998486152291881,
0.992772345172012,0.990020524139833),(0.998486152291881,0.998486152291881,
0.998486152291881,0.992772345172012,0.990020524139833)))
REPRESENTATION_ITEM('')
SURFACE()
);
#4292=(
BOUNDED_SURFACE()
B_SPLINE_SURFACE(1,2,((#166941,#166942,#166943,#166944,#166945),(#166946,
#166947,#166948,#166949,#166950)),.UNSPECIFIED.,.F.,.F.,.F.)
B_SPLINE_SURFACE_WITH_KNOTS((2,2),(3,2,3),(0.,0.182805892339142),(0.642474614281368,
0.642857142857143,0.659901408087482),.UNSPECIFIED.)
GEOMETRIC_REPRESENTATION_ITEM()
RATIONAL_B_SPLINE_SURFACE(((0.999732896029238,0.999865728939373,1.,0.994017305594881,
0.990889788836284),(0.999732896029238,0.999865728939373,1.,0.994017305594881,
0.990889788836284)))
REPRESENTATION_ITEM('')
SURFACE()
);
#4293=(
BOUNDED_SURFACE()
B_SPLINE_SURFACE(1,2,((#166952,#166953,#166954,#166955,#166956),(#166957,
#166958,#166959,#166960,#166961)),.UNSPECIFIED.,.F.,.F.,.F.)
B_SPLINE_SURFACE_WITH_KNOTS((2,2),(3,2,3),(0.938576859128179,1.),(0.0665257254736559,
0.0714285714285714,0.0736543502199101),.UNSPECIFIED.)
GEOMETRIC_REPRESENTATION_ITEM()
RATIONAL_B_SPLINE_SURFACE(((0.996794362316491,0.998279055819231,1.,0.999218731101516,
0.99848615229188),(0.996794362316491,0.998279055819231,1.,0.999218731101516,
0.99848615229188)))
REPRESENTATION_ITEM('')
SURFACE()
);
#4294=(
BOUNDED_SURFACE()
B_SPLINE_SURFACE(1,2,((#166968,#166969,#166970,#166971,#166972),(#166973,
#166974,#166975,#166976,#166977)),.UNSPECIFIED.,.F.,.F.,.F.)
B_SPLINE_SURFACE_WITH_KNOTS((2,2),(3,2,3),(0.,0.0529045403781215),(0.0665257254736559,
0.0714285714285714,0.073696866868496),.UNSPECIFIED.)
GEOMETRIC_REPRESENTATION_ITEM()
RATIONAL_B_SPLINE_SURFACE(((0.996794362316491,0.998279055819231,1.,0.999203807365457,
0.998458182734337),(0.996794362316491,0.998279055819231,1.,0.999203807365457,
0.998458182734337)))
REPRESENTATION_ITEM('')
SURFACE()
);
#4295=(
BOUNDED_SURFACE()
B_SPLINE_SURFACE(1,2,((#166988,#166989,#166990),(#166991,#166992,#166993)),
 .UNSPECIFIED.,.F.,.F.,.F.)
B_SPLINE_SURFACE_WITH_KNOTS((2,2),(3,3),(0.,0.0528815468798181),(0.659860018385657,
0.666841081426896),.UNSPECIFIED.)
GEOMETRIC_REPRESENTATION_ITEM()
RATIONAL_B_SPLINE_SURFACE(((0.990904995179334,0.989621173673357,0.988816334712146),
(0.990904995179334,0.989621173673357,0.988816334712146)))
REPRESENTATION_ITEM('')
SURFACE()
);
#4296=(
BOUNDED_SURFACE()
B_SPLINE_SURFACE(1,2,((#166995,#166996,#166997,#166998,#166999),(#167000,
#167001,#167002,#167003,#167004)),.UNSPECIFIED.,.F.,.F.,.F.)
B_SPLINE_SURFACE_WITH_KNOTS((2,2),(3,2,3),(0.938550151647624,1.00001008245332),
(0.659832011354088,0.659901408087482,0.666841081426896),.UNSPECIFIED.)
GEOMETRIC_REPRESENTATION_ITEM()
RATIONAL_B_SPLINE_SURFACE(((0.990889788836284,0.990889788836284,0.990889788836284,
0.98961640190086,0.988816334712146),(0.990889788836284,0.990889788836284,
0.990889788836284,0.98961640190086,0.988816334712146)))
REPRESENTATION_ITEM('')
SURFACE()
);
#4297=(
BOUNDED_SURFACE()
B_SPLINE_SURFACE(1,2,((#167006,#167007,#167008,#167009,#167010),(#167011,
#167012,#167013,#167014,#167015)),.UNSPECIFIED.,.F.,.F.,.F.)
B_SPLINE_SURFACE_WITH_KNOTS((2,2),(3,2,3),(0.,0.182885378421185),(0.0734807488197886,
0.07365435021991,0.0910144902320514),.UNSPECIFIED.)
GEOMETRIC_REPRESENTATION_ITEM()
RATIONAL_B_SPLINE_SURFACE(((0.998486152291881,0.998486152291881,0.998486152291881,
0.992772345172012,0.990020524139834),(0.998486152291881,0.998486152291881,
0.998486152291881,0.992772345172012,0.990020524139834)))
REPRESENTATION_ITEM('')
SURFACE()
);
#4298=(
BOUNDED_SURFACE()
B_SPLINE_SURFACE(1,2,((#167026,#167027,#167028,#167029,#167030),(#167031,
#167032,#167033,#167034,#167035)),.UNSPECIFIED.,.F.,.F.,.F.)
B_SPLINE_SURFACE_WITH_KNOTS((2,2),(3,2,3),(0.,0.182805892339144),(0.642474614281367,
0.642857142857143,0.659901408087591),.UNSPECIFIED.)
GEOMETRIC_REPRESENTATION_ITEM()
RATIONAL_B_SPLINE_SURFACE(((0.999732896029238,0.999865728939373,1.,0.994017305594843,
0.990889788836244),(0.999732896029238,0.999865728939373,1.,0.994017305594843,
0.990889788836244)))
REPRESENTATION_ITEM('')
SURFACE()
);
#4299=(
BOUNDED_SURFACE()
B_SPLINE_SURFACE(1,2,((#167037,#167038,#167039,#167040,#167041),(#167042,
#167043,#167044,#167045,#167046)),.UNSPECIFIED.,.F.,.F.,.F.)
B_SPLINE_SURFACE_WITH_KNOTS((2,2),(3,2,3),(0.938576859127265,1.),(0.0665257254736557,
0.0714285714285714,0.0736543502200163),.UNSPECIFIED.)
GEOMETRIC_REPRESENTATION_ITEM()
RATIONAL_B_SPLINE_SURFACE(((0.996794362316491,0.998279055819231,1.,0.999218731101479,
0.998486152291811),(0.996794362316491,0.998279055819231,1.,0.999218731101479,
0.998486152291811)))
REPRESENTATION_ITEM('')
SURFACE()
);
#4300=(
BOUNDED_SURFACE()
B_SPLINE_SURFACE(1,2,((#167054,#167055,#167056,#167057,#167058),(#167059,
#167060,#167061,#167062,#167063)),.UNSPECIFIED.,.F.,.F.,.F.)
B_SPLINE_SURFACE_WITH_KNOTS((2,2),(3,2,3),(0.,0.0529045403781241),(0.0665257254736563,
0.0714285714285714,0.0736968668684971),.UNSPECIFIED.)
GEOMETRIC_REPRESENTATION_ITEM()
RATIONAL_B_SPLINE_SURFACE(((0.996794362316491,0.998279055819231,1.,0.999203807365457,
0.998458182734336),(0.996794362316491,0.998279055819231,1.,0.999203807365457,
0.998458182734336)))
REPRESENTATION_ITEM('')
SURFACE()
);
#4301=(
BOUNDED_SURFACE()
B_SPLINE_SURFACE(1,2,((#167074,#167075,#167076),(#167077,#167078,#167079)),
 .UNSPECIFIED.,.F.,.F.,.F.)
B_SPLINE_SURFACE_WITH_KNOTS((2,2),(3,3),(0.,0.0528815468798234),(0.65986001838565,
0.666841081426896),.UNSPECIFIED.)
GEOMETRIC_REPRESENTATION_ITEM()
RATIONAL_B_SPLINE_SURFACE(((0.990904995179336,0.989621173673358,0.988816334712146),
(0.990904995179336,0.989621173673358,0.988816334712146)))
REPRESENTATION_ITEM('')
SURFACE()
);
#4302=(
BOUNDED_SURFACE()
B_SPLINE_SURFACE(1,2,((#167081,#167082,#167083,#167084,#167085),(#167086,
#167087,#167088,#167089,#167090)),.UNSPECIFIED.,.F.,.F.,.F.)
B_SPLINE_SURFACE_WITH_KNOTS((2,2),(3,2,3),(0.938550151647616,1.00001008250531),
(0.659832011354087,0.659901408087481,0.666841081426896),.UNSPECIFIED.)
GEOMETRIC_REPRESENTATION_ITEM()
RATIONAL_B_SPLINE_SURFACE(((0.990889788836284,0.990889788836284,0.990889788836284,
0.98961640190086,0.988816334712146),(0.990889788836284,0.990889788836284,
0.990889788836284,0.98961640190086,0.988816334712146)))
REPRESENTATION_ITEM('')
SURFACE()
);
#4303=(
BOUNDED_SURFACE()
B_SPLINE_SURFACE(1,2,((#167092,#167093,#167094,#167095,#167096),(#167097,
#167098,#167099,#167100,#167101)),.UNSPECIFIED.,.F.,.F.,.F.)
B_SPLINE_SURFACE_WITH_KNOTS((2,2),(3,2,3),(0.,0.182885378421189),(0.0734807488197897,
0.0736543502199111,0.0910144902320522),.UNSPECIFIED.)
GEOMETRIC_REPRESENTATION_ITEM()
RATIONAL_B_SPLINE_SURFACE(((0.99848615229188,0.99848615229188,0.99848615229188,
0.992772345172011,0.990020524139833),(0.99848615229188,0.99848615229188,
0.99848615229188,0.992772345172011,0.990020524139833)))
REPRESENTATION_ITEM('')
SURFACE()
);
#4304=(
BOUNDED_SURFACE()
B_SPLINE_SURFACE(1,2,((#167112,#167113,#167114,#167115,#167116),(#167117,
#167118,#167119,#167120,#167121)),.UNSPECIFIED.,.F.,.F.,.F.)
B_SPLINE_SURFACE_WITH_KNOTS((2,2),(3,2,3),(0.,0.182805892339155),(0.642474614281366,
0.642857142857143,0.659901408087481),.UNSPECIFIED.)
GEOMETRIC_REPRESENTATION_ITEM()
RATIONAL_B_SPLINE_SURFACE(((0.999732896029237,0.999865728939372,1.,0.994017305594881,
0.990889788836284),(0.999732896029237,0.999865728939372,1.,0.994017305594881,
0.990889788836284)))
REPRESENTATION_ITEM('')
SURFACE()
);
#4305=(
BOUNDED_SURFACE()
B_SPLINE_SURFACE(1,2,((#167123,#167124,#167125,#167126,#167127),(#167128,
#167129,#167130,#167131,#167132)),.UNSPECIFIED.,.F.,.F.,.F.)
B_SPLINE_SURFACE_WITH_KNOTS((2,2),(3,2,3),(0.938576859128167,1.),(0.0665257254736558,
0.0714285714285714,0.0736543502199113),.UNSPECIFIED.)
GEOMETRIC_REPRESENTATION_ITEM()
RATIONAL_B_SPLINE_SURFACE(((0.996794362316491,0.998279055819231,1.,0.999218731101516,
0.99848615229188),(0.996794362316491,0.998279055819231,1.,0.999218731101516,
0.99848615229188)))
REPRESENTATION_ITEM('')
SURFACE()
);
#4306=(
BOUNDED_SURFACE()
B_SPLINE_SURFACE(1,2,((#167140,#167141,#167142,#167143,#167144),(#167145,
#167146,#167147,#167148,#167149)),.UNSPECIFIED.,.F.,.F.,.F.)
B_SPLINE_SURFACE_WITH_KNOTS((2,2),(3,2,3),(0.,0.0529045403781334),(0.0665257254736558,
0.0714285714285714,0.0736968668684969),.UNSPECIFIED.)
GEOMETRIC_REPRESENTATION_ITEM()
RATIONAL_B_SPLINE_SURFACE(((0.996794362316491,0.998279055819231,1.,0.999203807365457,
0.998458182734336),(0.996794362316491,0.998279055819231,1.,0.999203807365457,
0.998458182734336)))
REPRESENTATION_ITEM('')
SURFACE()
);
#4307=(
BOUNDED_SURFACE()
B_SPLINE_SURFACE(1,2,((#167160,#167161,#167162),(#167163,#167164,#167165)),
 .UNSPECIFIED.,.F.,.F.,.F.)
B_SPLINE_SURFACE_WITH_KNOTS((2,2),(3,3),(0.,0.0528815468798287),(0.659860018385631,
0.666841081426896),.UNSPECIFIED.)
GEOMETRIC_REPRESENTATION_ITEM()
RATIONAL_B_SPLINE_SURFACE(((0.990904995179343,0.98962117367336,0.988816334712146),
(0.990904995179343,0.98962117367336,0.988816334712146)))
REPRESENTATION_ITEM('')
SURFACE()
);
#4308=(
BOUNDED_SURFACE()
B_SPLINE_SURFACE(1,2,((#167167,#167168,#167169,#167170,#167171),(#167172,
#167173,#167174,#167175,#167176)),.UNSPECIFIED.,.F.,.F.,.F.)
B_SPLINE_SURFACE_WITH_KNOTS((2,2),(3,2,3),(0.938550151647388,1.00001008248308),
(0.659832011354062,0.659901408087456,0.666841081426896),.UNSPECIFIED.)
GEOMETRIC_REPRESENTATION_ITEM()
RATIONAL_B_SPLINE_SURFACE(((0.990889788836293,0.990889788836293,0.990889788836293,
0.989616401900863,0.988816334712145),(0.990889788836293,0.990889788836293,
0.990889788836293,0.989616401900863,0.988816334712145)))
REPRESENTATION_ITEM('')
SURFACE()
);
#4309=(
BOUNDED_SURFACE()
B_SPLINE_SURFACE(1,2,((#167178,#167179,#167180,#167181,#167182),(#167183,
#167184,#167185,#167186,#167187)),.UNSPECIFIED.,.F.,.F.,.F.)
B_SPLINE_SURFACE_WITH_KNOTS((2,2),(3,2,3),(-1.06915738063826E-6,0.182885378421192),
(0.0734807488197634,0.0736543502198851,0.0910144902320526),
 .UNSPECIFIED.)
GEOMETRIC_REPRESENTATION_ITEM()
RATIONAL_B_SPLINE_SURFACE(((0.998486152291897,0.998486152291897,0.998486152291897,
0.992772345172015,0.990020524139833),(0.998486152291897,0.998486152291897,
0.998486152291897,0.992772345172015,0.990020524139833)))
REPRESENTATION_ITEM('')
SURFACE()
);
#4310=(
BOUNDED_SURFACE()
B_SPLINE_SURFACE(1,2,((#167198,#167199,#167200,#167201,#167202),(#167203,
#167204,#167205,#167206,#167207)),.UNSPECIFIED.,.F.,.F.,.F.)
B_SPLINE_SURFACE_WITH_KNOTS((2,2),(3,2,3),(0.,0.182805892339151),(0.642474614281366,
0.642857142857143,0.659901408087483),.UNSPECIFIED.)
GEOMETRIC_REPRESENTATION_ITEM()
RATIONAL_B_SPLINE_SURFACE(((0.999732896029237,0.999865728939372,1.,0.994017305594881,
0.990889788836284),(0.999732896029237,0.999865728939372,1.,0.994017305594881,
0.990889788836284)))
REPRESENTATION_ITEM('')
SURFACE()
);
#4311=(
BOUNDED_SURFACE()
B_SPLINE_SURFACE(1,2,((#167209,#167210,#167211,#167212,#167213),(#167214,
#167215,#167216,#167217,#167218)),.UNSPECIFIED.,.F.,.F.,.F.)
B_SPLINE_SURFACE_WITH_KNOTS((2,2),(3,2,3),(0.938576859128156,1.),(0.0665257254736561,
0.0714285714285714,0.0736543502199126),.UNSPECIFIED.)
GEOMETRIC_REPRESENTATION_ITEM()
RATIONAL_B_SPLINE_SURFACE(((0.996794362316491,0.998279055819231,1.,0.999218731101515,
0.998486152291879),(0.996794362316491,0.998279055819231,1.,0.999218731101515,
0.998486152291879)))
REPRESENTATION_ITEM('')
SURFACE()
);
#4312=(
BOUNDED_SURFACE()
B_SPLINE_SURFACE(1,2,((#167226,#167227,#167228,#167229,#167230),(#167231,
#167232,#167233,#167234,#167235)),.UNSPECIFIED.,.F.,.F.,.F.)
B_SPLINE_SURFACE_WITH_KNOTS((2,2),(3,2,3),(0.,0.0529045403781322),(0.066525725473656,
0.0714285714285714,0.0736968668684985),.UNSPECIFIED.)
GEOMETRIC_REPRESENTATION_ITEM()
RATIONAL_B_SPLINE_SURFACE(((0.996794362316491,0.998279055819231,1.,0.999203807365456,
0.998458182734335),(0.996794362316491,0.998279055819231,1.,0.999203807365456,
0.998458182734335)))
REPRESENTATION_ITEM('')
SURFACE()
);
#4313=(
BOUNDED_SURFACE()
B_SPLINE_SURFACE(1,2,((#167246,#167247,#167248),(#167249,#167250,#167251)),
 .UNSPECIFIED.,.F.,.F.,.F.)
B_SPLINE_SURFACE_WITH_KNOTS((2,2),(3,3),(0.,0.0528815468798286),(0.659860018385641,
0.666841081426896),.UNSPECIFIED.)
GEOMETRIC_REPRESENTATION_ITEM()
RATIONAL_B_SPLINE_SURFACE(((0.99090499517934,0.989621173673359,0.988816334712146),
(0.99090499517934,0.989621173673359,0.988816334712146)))
REPRESENTATION_ITEM('')
SURFACE()
);
#4314=(
BOUNDED_SURFACE()
B_SPLINE_SURFACE(1,2,((#167253,#167254,#167255,#167256,#167257),(#167258,
#167259,#167260,#167261,#167262)),.UNSPECIFIED.,.F.,.F.,.F.)
B_SPLINE_SURFACE_WITH_KNOTS((2,2),(3,2,3),(0.938550151647614,1.00001008252413),
(0.659832011354087,0.659901408087481,0.666841081426896),.UNSPECIFIED.)
GEOMETRIC_REPRESENTATION_ITEM()
RATIONAL_B_SPLINE_SURFACE(((0.990889788836284,0.990889788836284,0.990889788836284,
0.98961640190086,0.988816334712146),(0.990889788836284,0.990889788836284,
0.990889788836284,0.98961640190086,0.988816334712146)))
REPRESENTATION_ITEM('')
SURFACE()
);
#4315=(
BOUNDED_SURFACE()
B_SPLINE_SURFACE(1,2,((#167264,#167265,#167266,#167267,#167268),(#167269,
#167270,#167271,#167272,#167273)),.UNSPECIFIED.,.F.,.F.,.F.)
B_SPLINE_SURFACE_WITH_KNOTS((2,2),(3,2,3),(-1.07114226772793E-6,0.18288537842119),
(0.0734807488197897,0.0736543502199111,0.0910144902320524),
 .UNSPECIFIED.)
GEOMETRIC_REPRESENTATION_ITEM()
RATIONAL_B_SPLINE_SURFACE(((0.99848615229188,0.99848615229188,0.99848615229188,
0.992772345172011,0.990020524139833),(0.99848615229188,0.99848615229188,
0.99848615229188,0.992772345172011,0.990020524139833)))
REPRESENTATION_ITEM('')
SURFACE()
);
#4316=(
BOUNDED_SURFACE()
B_SPLINE_SURFACE(1,2,((#167284,#167285,#167286,#167287,#167288),(#167289,
#167290,#167291,#167292,#167293)),.UNSPECIFIED.,.F.,.F.,.F.)
B_SPLINE_SURFACE_WITH_KNOTS((2,2),(3,2,3),(0.,0.18280589233915),(0.642474614281367,
0.642857142857143,0.659901408087481),.UNSPECIFIED.)
GEOMETRIC_REPRESENTATION_ITEM()
RATIONAL_B_SPLINE_SURFACE(((0.999732896029237,0.999865728939372,1.,0.994017305594881,
0.990889788836284),(0.999732896029237,0.999865728939372,1.,0.994017305594881,
0.990889788836284)))
REPRESENTATION_ITEM('')
SURFACE()
);
#4317=(
BOUNDED_SURFACE()
B_SPLINE_SURFACE(1,2,((#167295,#167296,#167297,#167298,#167299),(#167300,
#167301,#167302,#167303,#167304)),.UNSPECIFIED.,.F.,.F.,.F.)
B_SPLINE_SURFACE_WITH_KNOTS((2,2),(3,2,3),(0.938576859128171,1.),(0.0665257254736561,
0.0714285714285714,0.0736543502199112),.UNSPECIFIED.)
GEOMETRIC_REPRESENTATION_ITEM()
RATIONAL_B_SPLINE_SURFACE(((0.996794362316491,0.998279055819231,1.,0.999218731101516,
0.99848615229188),(0.996794362316491,0.998279055819231,1.,0.999218731101516,
0.99848615229188)))
REPRESENTATION_ITEM('')
SURFACE()
);
#4318=(
BOUNDED_SURFACE()
B_SPLINE_SURFACE(1,2,((#167311,#167312,#167313,#167314,#167315),(#167316,
#167317,#167318,#167319,#167320)),.UNSPECIFIED.,.F.,.F.,.F.)
B_SPLINE_SURFACE_WITH_KNOTS((2,2),(3,2,3),(0.,0.0529045403781285),(0.0665257254736561,
0.0714285714285714,0.0736968668684971),.UNSPECIFIED.)
GEOMETRIC_REPRESENTATION_ITEM()
RATIONAL_B_SPLINE_SURFACE(((0.996794362316491,0.998279055819231,1.,0.999203807365457,
0.998458182734336),(0.996794362316491,0.998279055819231,1.,0.999203807365457,
0.998458182734336)))
REPRESENTATION_ITEM('')
SURFACE()
);
#4319=(
BOUNDED_SURFACE()
B_SPLINE_SURFACE(1,2,((#167331,#167332,#167333),(#167334,#167335,#167336)),
 .UNSPECIFIED.,.F.,.F.,.F.)
B_SPLINE_SURFACE_WITH_KNOTS((2,2),(3,3),(0.,0.0528815468798285),(0.659860018385656,
0.666841081426896),.UNSPECIFIED.)
GEOMETRIC_REPRESENTATION_ITEM()
RATIONAL_B_SPLINE_SURFACE(((0.990904995179334,0.989621173673357,0.988816334712145),
(0.990904995179334,0.989621173673357,0.988816334712145)))
REPRESENTATION_ITEM('')
SURFACE()
);
#4320=(
BOUNDED_SURFACE()
B_SPLINE_SURFACE(1,2,((#167338,#167339,#167340,#167341,#167342),(#167343,
#167344,#167345,#167346,#167347)),.UNSPECIFIED.,.F.,.F.,.F.)
B_SPLINE_SURFACE_WITH_KNOTS((2,2),(3,2,3),(0.938550151647616,1.00001008244981),
(0.659832011354087,0.659901408087481,0.666841081426896),.UNSPECIFIED.)
GEOMETRIC_REPRESENTATION_ITEM()
RATIONAL_B_SPLINE_SURFACE(((0.990889788836284,0.990889788836284,0.990889788836284,
0.98961640190086,0.988816334712146),(0.990889788836284,0.990889788836284,
0.990889788836284,0.98961640190086,0.988816334712146)))
REPRESENTATION_ITEM('')
SURFACE()
);
#4321=(
BOUNDED_SURFACE()
B_SPLINE_SURFACE(1,2,((#167349,#167350,#167351,#167352,#167353),(#167354,
#167355,#167356,#167357,#167358)),.UNSPECIFIED.,.F.,.F.,.F.)
B_SPLINE_SURFACE_WITH_KNOTS((2,2),(3,2,3),(0.,0.182885378421189),(0.0734807488197897,
0.0736543502199111,0.0910144902320524),.UNSPECIFIED.)
GEOMETRIC_REPRESENTATION_ITEM()
RATIONAL_B_SPLINE_SURFACE(((0.99848615229188,0.99848615229188,0.99848615229188,
0.992772345172011,0.990020524139833),(0.99848615229188,0.99848615229188,
0.99848615229188,0.992772345172011,0.990020524139833)))
REPRESENTATION_ITEM('')
SURFACE()
);
#4322=(
BOUNDED_SURFACE()
B_SPLINE_SURFACE(1,2,((#167369,#167370,#167371,#167372,#167373),(#167374,
#167375,#167376,#167377,#167378)),.UNSPECIFIED.,.F.,.F.,.F.)
B_SPLINE_SURFACE_WITH_KNOTS((2,2),(3,2,3),(0.,0.182805892339155),(0.642474614281366,
0.642857142857143,0.659901408087482),.UNSPECIFIED.)
GEOMETRIC_REPRESENTATION_ITEM()
RATIONAL_B_SPLINE_SURFACE(((0.999732896029237,0.999865728939372,1.,0.994017305594881,
0.990889788836284),(0.999732896029237,0.999865728939372,1.,0.994017305594881,
0.990889788836284)))
REPRESENTATION_ITEM('')
SURFACE()
);
#4323=(
BOUNDED_SURFACE()
B_SPLINE_SURFACE(1,2,((#167380,#167381,#167382,#167383,#167384),(#167385,
#167386,#167387,#167388,#167389)),.UNSPECIFIED.,.F.,.F.,.F.)
B_SPLINE_SURFACE_WITH_KNOTS((2,2),(3,2,3),(0.938576859128165,1.),(0.0665257254736557,
0.0714285714285714,0.0736543502199114),.UNSPECIFIED.)
GEOMETRIC_REPRESENTATION_ITEM()
RATIONAL_B_SPLINE_SURFACE(((0.996794362316491,0.998279055819231,1.,0.999218731101516,
0.99848615229188),(0.996794362316491,0.998279055819231,1.,0.999218731101516,
0.99848615229188)))
REPRESENTATION_ITEM('')
SURFACE()
);
#4324=(
BOUNDED_SURFACE()
B_SPLINE_SURFACE(1,2,((#167397,#167398,#167399,#167400,#167401),(#167402,
#167403,#167404,#167405,#167406)),.UNSPECIFIED.,.F.,.F.,.F.)
B_SPLINE_SURFACE_WITH_KNOTS((2,2),(3,2,3),(0.,0.0529045403781337),(0.0665257254736557,
0.0714285714285714,0.0736968668684971),.UNSPECIFIED.)
GEOMETRIC_REPRESENTATION_ITEM()
RATIONAL_B_SPLINE_SURFACE(((0.996794362316491,0.998279055819231,1.,0.999203807365457,
0.998458182734336),(0.996794362316491,0.998279055819231,1.,0.999203807365457,
0.998458182734336)))
REPRESENTATION_ITEM('')
SURFACE()
);
#4325=(
BOUNDED_SURFACE()
B_SPLINE_SURFACE(1,2,((#167417,#167418,#167419),(#167420,#167421,#167422)),
 .UNSPECIFIED.,.F.,.F.,.F.)
B_SPLINE_SURFACE_WITH_KNOTS((2,2),(3,3),(0.,0.0528815468798329),(0.659860018385558,
0.666841081426897),.UNSPECIFIED.)
GEOMETRIC_REPRESENTATION_ITEM()
RATIONAL_B_SPLINE_SURFACE(((0.99090499517937,0.989621173673368,0.988816334712145),
(0.99090499517937,0.989621173673368,0.988816334712145)))
REPRESENTATION_ITEM('')
SURFACE()
);
#4326=(
BOUNDED_SURFACE()
B_SPLINE_SURFACE(1,2,((#167424,#167425,#167426,#167427,#167428),(#167429,
#167430,#167431,#167432,#167433)),.UNSPECIFIED.,.F.,.F.,.F.)
B_SPLINE_SURFACE_WITH_KNOTS((2,2),(3,2,3),(0.938550151647612,1.00001008245693),
(0.659832011354087,0.659901408087481,0.666841081426897),.UNSPECIFIED.)
GEOMETRIC_REPRESENTATION_ITEM()
RATIONAL_B_SPLINE_SURFACE(((0.990889788836284,0.990889788836284,0.990889788836284,
0.98961640190086,0.988816334712146),(0.990889788836284,0.990889788836284,
0.990889788836284,0.98961640190086,0.988816334712146)))
REPRESENTATION_ITEM('')
SURFACE()
);
#4327=(
BOUNDED_SURFACE()
B_SPLINE_SURFACE(1,2,((#167435,#167436,#167437,#167438,#167439),(#167440,
#167441,#167442,#167443,#167444)),.UNSPECIFIED.,.F.,.F.,.F.)
B_SPLINE_SURFACE_WITH_KNOTS((2,2),(3,2,3),(0.,0.182885378421192),(0.0734807488197897,
0.0736543502199111,0.0910144902320528),.UNSPECIFIED.)
GEOMETRIC_REPRESENTATION_ITEM()
RATIONAL_B_SPLINE_SURFACE(((0.99848615229188,0.99848615229188,0.99848615229188,
0.992772345172011,0.990020524139833),(0.99848615229188,0.99848615229188,
0.99848615229188,0.992772345172011,0.990020524139833)))
REPRESENTATION_ITEM('')
SURFACE()
);
#4328=(
BOUNDED_SURFACE()
B_SPLINE_SURFACE(1,2,((#167455,#167456,#167457,#167458,#167459),(#167460,
#167461,#167462,#167463,#167464)),.UNSPECIFIED.,.F.,.F.,.F.)
B_SPLINE_SURFACE_WITH_KNOTS((2,2),(3,2,3),(0.,0.182805892339158),(0.642474614281367,
0.642857142857143,0.659901408087481),.UNSPECIFIED.)
GEOMETRIC_REPRESENTATION_ITEM()
RATIONAL_B_SPLINE_SURFACE(((0.999732896029238,0.999865728939373,1.,0.994017305594881,
0.990889788836284),(0.999732896029238,0.999865728939373,1.,0.994017305594881,
0.990889788836284)))
REPRESENTATION_ITEM('')
SURFACE()
);
#4329=(
BOUNDED_SURFACE()
B_SPLINE_SURFACE(1,2,((#167466,#167467,#167468,#167469,#167470),(#167471,
#167472,#167473,#167474,#167475)),.UNSPECIFIED.,.F.,.F.,.F.)
B_SPLINE_SURFACE_WITH_KNOTS((2,2),(3,2,3),(0.938576859128171,1.),(0.0665257254736564,
0.0714285714285714,0.0736543502199112),.UNSPECIFIED.)
GEOMETRIC_REPRESENTATION_ITEM()
RATIONAL_B_SPLINE_SURFACE(((0.996794362316492,0.998279055819231,1.,0.999218731101516,
0.99848615229188),(0.996794362316492,0.998279055819231,1.,0.999218731101516,
0.99848615229188)))
REPRESENTATION_ITEM('')
SURFACE()
);
#4330=(
BOUNDED_SURFACE()
B_SPLINE_SURFACE(1,2,((#167482,#167483,#167484,#167485,#167486),(#167487,
#167488,#167489,#167490,#167491)),.UNSPECIFIED.,.F.,.F.,.F.)
B_SPLINE_SURFACE_WITH_KNOTS((2,2),(3,2,3),(0.,0.052904540378125),(0.0665257254736564,
0.0714285714285714,0.0736968668684972),.UNSPECIFIED.)
GEOMETRIC_REPRESENTATION_ITEM()
RATIONAL_B_SPLINE_SURFACE(((0.996794362316492,0.998279055819231,1.,0.999203807365457,
0.998458182734336),(0.996794362316492,0.998279055819231,1.,0.999203807365457,
0.998458182734336)))
REPRESENTATION_ITEM('')
SURFACE()
);
#4331=(
BOUNDED_SURFACE()
B_SPLINE_SURFACE(1,2,((#167502,#167503,#167504),(#167505,#167506,#167507)),
 .UNSPECIFIED.,.F.,.F.,.F.)
B_SPLINE_SURFACE_WITH_KNOTS((2,2),(3,3),(0.,0.0528815468798311),(0.659860018385656,
0.666841081426897),.UNSPECIFIED.)
GEOMETRIC_REPRESENTATION_ITEM()
RATIONAL_B_SPLINE_SURFACE(((0.990904995179334,0.989621173673357,0.988816334712145),
(0.990904995179334,0.989621173673357,0.988816334712145)))
REPRESENTATION_ITEM('')
SURFACE()
);
#4332=(
BOUNDED_SURFACE()
B_SPLINE_SURFACE(1,2,((#167509,#167510,#167511,#167512,#167513),(#167514,
#167515,#167516,#167517,#167518)),.UNSPECIFIED.,.F.,.F.,.F.)
B_SPLINE_SURFACE_WITH_KNOTS((2,2),(3,2,3),(0.938550151647611,1.00001008249664),
(0.659832011354087,0.659901408087481,0.666841081426897),.UNSPECIFIED.)
GEOMETRIC_REPRESENTATION_ITEM()
RATIONAL_B_SPLINE_SURFACE(((0.990889788836284,0.990889788836284,0.990889788836284,
0.98961640190086,0.988816334712146),(0.990889788836284,0.990889788836284,
0.990889788836284,0.98961640190086,0.988816334712146)))
REPRESENTATION_ITEM('')
SURFACE()
);
#4333=(
BOUNDED_SURFACE()
B_SPLINE_SURFACE(1,2,((#167520,#167521,#167522,#167523,#167524),(#167525,
#167526,#167527,#167528,#167529)),.UNSPECIFIED.,.F.,.F.,.F.)
B_SPLINE_SURFACE_WITH_KNOTS((2,2),(3,2,3),(-1.06908625210514E-6,0.182885378421192),
(0.0734807488197897,0.0736543502199111,0.0910144902320523),
 .UNSPECIFIED.)
GEOMETRIC_REPRESENTATION_ITEM()
RATIONAL_B_SPLINE_SURFACE(((0.99848615229188,0.99848615229188,0.99848615229188,
0.992772345172011,0.990020524139833),(0.99848615229188,0.99848615229188,
0.99848615229188,0.992772345172011,0.990020524139833)))
REPRESENTATION_ITEM('')
SURFACE()
);
#4334=(
BOUNDED_SURFACE()
B_SPLINE_SURFACE(1,2,((#167540,#167541,#167542,#167543,#167544),(#167545,
#167546,#167547,#167548,#167549)),.UNSPECIFIED.,.F.,.F.,.F.)
B_SPLINE_SURFACE_WITH_KNOTS((2,2),(3,2,3),(0.,0.182805892339156),(0.642474614281366,
0.642857142857143,0.659901408087482),.UNSPECIFIED.)
GEOMETRIC_REPRESENTATION_ITEM()
RATIONAL_B_SPLINE_SURFACE(((0.999732896029237,0.999865728939372,1.,0.994017305594881,
0.990889788836284),(0.999732896029237,0.999865728939372,1.,0.994017305594881,
0.990889788836284)))
REPRESENTATION_ITEM('')
SURFACE()
);
#4335=(
BOUNDED_SURFACE()
B_SPLINE_SURFACE(1,2,((#167551,#167552,#167553,#167554,#167555),(#167556,
#167557,#167558,#167559,#167560)),.UNSPECIFIED.,.F.,.F.,.F.)
B_SPLINE_SURFACE_WITH_KNOTS((2,2),(3,2,3),(0.938576859128167,1.),(0.0665257254736567,
0.0714285714285714,0.0736543502199119),.UNSPECIFIED.)
GEOMETRIC_REPRESENTATION_ITEM()
RATIONAL_B_SPLINE_SURFACE(((0.996794362316492,0.998279055819231,1.,0.999218731101515,
0.998486152291879),(0.996794362316492,0.998279055819231,1.,0.999218731101515,
0.998486152291879)))
REPRESENTATION_ITEM('')
SURFACE()
);
#4336=(
BOUNDED_SURFACE()
B_SPLINE_SURFACE(1,2,((#167568,#167569,#167570,#167571,#167572),(#167573,
#167574,#167575,#167576,#167577)),.UNSPECIFIED.,.F.,.F.,.F.)
B_SPLINE_SURFACE_WITH_KNOTS((2,2),(3,2,3),(0.,0.0529045403781293),(0.0665257254736565,
0.0714285714285714,0.0736968668684979),.UNSPECIFIED.)
GEOMETRIC_REPRESENTATION_ITEM()
RATIONAL_B_SPLINE_SURFACE(((0.996794362316492,0.998279055819231,1.,0.999203807365456,
0.998458182734335),(0.996794362316492,0.998279055819231,1.,0.999203807365456,
0.998458182734335)))
REPRESENTATION_ITEM('')
SURFACE()
);
#4337=(
BOUNDED_SURFACE()
B_SPLINE_SURFACE(1,2,((#167588,#167589,#167590),(#167591,#167592,#167593)),
 .UNSPECIFIED.,.F.,.F.,.F.)
B_SPLINE_SURFACE_WITH_KNOTS((2,2),(3,3),(0.,0.0528815468798305),(0.659860018385656,
0.666841081426896),.UNSPECIFIED.)
GEOMETRIC_REPRESENTATION_ITEM()
RATIONAL_B_SPLINE_SURFACE(((0.990904995179334,0.989621173673357,0.988816334712145),
(0.990904995179334,0.989621173673357,0.988816334712145)))
REPRESENTATION_ITEM('')
SURFACE()
);
#4338=(
BOUNDED_SURFACE()
B_SPLINE_SURFACE(1,2,((#167595,#167596,#167597,#167598,#167599),(#167600,
#167601,#167602,#167603,#167604)),.UNSPECIFIED.,.F.,.F.,.F.)
B_SPLINE_SURFACE_WITH_KNOTS((2,2),(3,2,3),(0.938550151643589,1.00001008249256),
(0.659832011353627,0.659901408087026,0.666841081426899),.UNSPECIFIED.)
GEOMETRIC_REPRESENTATION_ITEM()
RATIONAL_B_SPLINE_SURFACE(((0.990889788836451,0.990889788836451,0.990889788836451,
0.989616401900912,0.988816334712145),(0.990889788836451,0.990889788836451,
0.990889788836451,0.989616401900912,0.988816334712145)))
REPRESENTATION_ITEM('')
SURFACE()
);
#4339=(
BOUNDED_SURFACE()
B_SPLINE_SURFACE(1,2,((#167606,#167607,#167608,#167609,#167610),(#167611,
#167612,#167613,#167614,#167615)),.UNSPECIFIED.,.F.,.F.,.F.)
B_SPLINE_SURFACE_WITH_KNOTS((2,2),(3,2,3),(-1.06896686295104E-6,0.18288537842119),
(0.0734807488195811,0.0736543502197046,0.0910144902320537),
 .UNSPECIFIED.)
GEOMETRIC_REPRESENTATION_ITEM()
RATIONAL_B_SPLINE_SURFACE(((0.998486152292016,0.998486152292016,0.998486152292016,
0.992772345172043,0.990020524139833),(0.998486152292016,0.998486152292016,
0.998486152292016,0.992772345172043,0.990020524139833)))
REPRESENTATION_ITEM('')
SURFACE()
);
#4340=(
BOUNDED_SURFACE()
B_SPLINE_SURFACE(1,2,((#167626,#167627,#167628,#167629,#167630),(#167631,
#167632,#167633,#167634,#167635)),.UNSPECIFIED.,.F.,.F.,.F.)
B_SPLINE_SURFACE_WITH_KNOTS((2,2),(3,2,3),(0.,0.182805892339159),(0.642474614281366,
0.642857142857143,0.659901408087481),.UNSPECIFIED.)
GEOMETRIC_REPRESENTATION_ITEM()
RATIONAL_B_SPLINE_SURFACE(((0.999732896029237,0.999865728939372,1.,0.994017305594881,
0.990889788836284),(0.999732896029237,0.999865728939372,1.,0.994017305594881,
0.990889788836284)))
REPRESENTATION_ITEM('')
SURFACE()
);
#4341=(
BOUNDED_SURFACE()
B_SPLINE_SURFACE(1,2,((#167637,#167638,#167639,#167640,#167641),(#167642,
#167643,#167644,#167645,#167646)),.UNSPECIFIED.,.F.,.F.,.F.)
B_SPLINE_SURFACE_WITH_KNOTS((2,2),(3,2,3),(0.938576859128175,1.),(0.0665257254736565,
0.0714285714285714,0.0736543502199112),.UNSPECIFIED.)
GEOMETRIC_REPRESENTATION_ITEM()
RATIONAL_B_SPLINE_SURFACE(((0.996794362316492,0.998279055819231,1.,0.999218731101516,
0.99848615229188),(0.996794362316492,0.998279055819231,1.,0.999218731101516,
0.99848615229188)))
REPRESENTATION_ITEM('')
SURFACE()
);
#4342=(
BOUNDED_SURFACE()
B_SPLINE_SURFACE(1,2,((#167652,#167653,#167654,#167655,#167656),(#167657,
#167658,#167659,#167660,#167661)),.UNSPECIFIED.,.F.,.F.,.F.)
B_SPLINE_SURFACE_WITH_KNOTS((2,2),(3,2,3),(0.,0.0525890063985138),(0.0665682420727563,
0.0714285714285714,0.0736543503731481),.UNSPECIFIED.)
GEOMETRIC_REPRESENTATION_ITEM()
RATIONAL_B_SPLINE_SURFACE(((0.996820130073177,0.99829397953792,1.,0.999218731047729,
0.998486152191009),(0.996820130073177,0.99829397953792,1.,0.999218731047729,
0.998486152191009)))
REPRESENTATION_ITEM('')
SURFACE()
);
#4343=(
BOUNDED_SURFACE()
B_SPLINE_SURFACE(1,2,((#167672,#167673,#167674),(#167675,#167676,#167677)),
 .UNSPECIFIED.,.F.,.F.,.F.)
B_SPLINE_SURFACE_WITH_KNOTS((2,2),(3,3),(0.,0.0528815468798306),(0.659860018385656,
0.666841081426897),.UNSPECIFIED.)
GEOMETRIC_REPRESENTATION_ITEM()
RATIONAL_B_SPLINE_SURFACE(((0.990904995179334,0.989621173673357,0.988816334712145),
(0.990904995179334,0.989621173673357,0.988816334712146)))
REPRESENTATION_ITEM('')
SURFACE()
);
#4344=(
BOUNDED_SURFACE()
B_SPLINE_SURFACE(1,2,((#167679,#167680,#167681,#167682,#167683),(#167684,
#167685,#167686,#167687,#167688)),.UNSPECIFIED.,.F.,.F.,.F.)
B_SPLINE_SURFACE_WITH_KNOTS((2,2),(3,2,3),(0.938550151647611,1.00001008245607),
(0.659832011354087,0.659901408087481,0.666841081426897),.UNSPECIFIED.)
GEOMETRIC_REPRESENTATION_ITEM()
RATIONAL_B_SPLINE_SURFACE(((0.990889788836284,0.990889788836284,0.990889788836284,
0.98961640190086,0.988816334712146),(0.990889788836284,0.990889788836284,
0.990889788836284,0.98961640190086,0.988816334712146)))
REPRESENTATION_ITEM('')
SURFACE()
);
#4345=(
BOUNDED_SURFACE()
B_SPLINE_SURFACE(1,2,((#167690,#167691,#167692,#167693,#167694),(#167695,
#167696,#167697,#167698,#167699)),.UNSPECIFIED.,.F.,.F.,.F.)
B_SPLINE_SURFACE_WITH_KNOTS((2,2),(3,2,3),(-1.07106247283029E-6,0.182885378421187),
(0.0734807488197897,0.0736543502199111,0.0910144902320524),
 .UNSPECIFIED.)
GEOMETRIC_REPRESENTATION_ITEM()
RATIONAL_B_SPLINE_SURFACE(((0.99848615229188,0.99848615229188,0.99848615229188,
0.992772345172011,0.990020524139833),(0.99848615229188,0.99848615229188,
0.99848615229188,0.992772345172011,0.990020524139833)))
REPRESENTATION_ITEM('')
SURFACE()
);
#4346=(
BOUNDED_SURFACE()
B_SPLINE_SURFACE(1,2,((#167710,#167711,#167712,#167713,#167714),(#167715,
#167716,#167717,#167718,#167719)),.UNSPECIFIED.,.F.,.F.,.F.)
B_SPLINE_SURFACE_WITH_KNOTS((2,2),(3,2,3),(0.,0.182805892339153),(0.642474614281367,
0.642857142857143,0.659901408087481),.UNSPECIFIED.)
GEOMETRIC_REPRESENTATION_ITEM()
RATIONAL_B_SPLINE_SURFACE(((0.999732896029237,0.999865728939372,1.,0.994017305594881,
0.990889788836284),(0.999732896029237,0.999865728939372,1.,0.994017305594881,
0.990889788836284)))
REPRESENTATION_ITEM('')
SURFACE()
);
#4347=(
BOUNDED_SURFACE()
B_SPLINE_SURFACE(1,2,((#167721,#167722,#167723,#167724,#167725),(#167726,
#167727,#167728,#167729,#167730)),.UNSPECIFIED.,.F.,.F.,.F.)
B_SPLINE_SURFACE_WITH_KNOTS((2,2),(3,2,3),(0.938576859128174,1.),(0.0665257254736566,
0.0714285714285714,0.0736543502199112),.UNSPECIFIED.)
GEOMETRIC_REPRESENTATION_ITEM()
RATIONAL_B_SPLINE_SURFACE(((0.996794362316492,0.998279055819231,1.,0.999218731101516,
0.99848615229188),(0.996794362316492,0.998279055819231,1.,0.999218731101516,
0.99848615229188)))
REPRESENTATION_ITEM('')
SURFACE()
);
#4348=(
BOUNDED_SURFACE()
B_SPLINE_SURFACE(1,2,((#167738,#167739,#167740,#167741,#167742),(#167743,
#167744,#167745,#167746,#167747)),.UNSPECIFIED.,.F.,.F.,.F.)
B_SPLINE_SURFACE_WITH_KNOTS((2,2),(3,2,3),(0.,0.0529045403781294),(0.0665257254736564,
0.0714285714285714,0.0736968668684973),.UNSPECIFIED.)
GEOMETRIC_REPRESENTATION_ITEM()
RATIONAL_B_SPLINE_SURFACE(((0.996794362316492,0.998279055819231,1.,0.999203807365457,
0.998458182734336),(0.996794362316492,0.998279055819231,1.,0.999203807365457,
0.998458182734336)))
REPRESENTATION_ITEM('')
SURFACE()
);
#4349=(
BOUNDED_SURFACE()
B_SPLINE_SURFACE(1,2,((#167758,#167759,#167760),(#167761,#167762,#167763)),
 .UNSPECIFIED.,.F.,.F.,.F.)
B_SPLINE_SURFACE_WITH_KNOTS((2,2),(3,3),(0.,0.0528815468798319),(0.659860018385656,
0.666841081426897),.UNSPECIFIED.)
GEOMETRIC_REPRESENTATION_ITEM()
RATIONAL_B_SPLINE_SURFACE(((0.990904995179334,0.989621173673357,0.988816334712146),
(0.990904995179334,0.989621173673357,0.988816334712146)))
REPRESENTATION_ITEM('')
SURFACE()
);
#4350=(
BOUNDED_SURFACE()
B_SPLINE_SURFACE(1,2,((#167765,#167766,#167767,#167768,#167769),(#167770,
#167771,#167772,#167773,#167774)),.UNSPECIFIED.,.F.,.F.,.F.)
B_SPLINE_SURFACE_WITH_KNOTS((2,2),(3,2,3),(0.938550151647611,1.00001008245706),
(0.659832011354087,0.659901408087481,0.666841081426897),.UNSPECIFIED.)
GEOMETRIC_REPRESENTATION_ITEM()
RATIONAL_B_SPLINE_SURFACE(((0.990889788836284,0.990889788836284,0.990889788836284,
0.98961640190086,0.988816334712145),(0.990889788836284,0.990889788836284,
0.990889788836284,0.98961640190086,0.988816334712145)))
REPRESENTATION_ITEM('')
SURFACE()
);
#4351=(
BOUNDED_SURFACE()
B_SPLINE_SURFACE(1,2,((#167776,#167777,#167778,#167779,#167780),(#167781,
#167782,#167783,#167784,#167785)),.UNSPECIFIED.,.F.,.F.,.F.)
B_SPLINE_SURFACE_WITH_KNOTS((2,2),(3,2,3),(-1.06904910472764E-6,0.182885378421189),
(0.0734807488197898,0.0736543502199112,0.0910144902320519),
 .UNSPECIFIED.)
GEOMETRIC_REPRESENTATION_ITEM()
RATIONAL_B_SPLINE_SURFACE(((0.99848615229188,0.99848615229188,0.99848615229188,
0.992772345172011,0.990020524139833),(0.99848615229188,0.99848615229188,
0.99848615229188,0.992772345172011,0.990020524139833)))
REPRESENTATION_ITEM('')
SURFACE()
);
#4352=(
BOUNDED_SURFACE()
B_SPLINE_SURFACE(1,2,((#167796,#167797,#167798,#167799,#167800),(#167801,
#167802,#167803,#167804,#167805)),.UNSPECIFIED.,.F.,.F.,.F.)
B_SPLINE_SURFACE_WITH_KNOTS((2,2),(3,2,3),(0.,0.18280589233916),(0.642474614281364,
0.642857142857143,0.659901408087481),.UNSPECIFIED.)
GEOMETRIC_REPRESENTATION_ITEM()
RATIONAL_B_SPLINE_SURFACE(((0.999732896029236,0.999865728939372,1.,0.994017305594881,
0.990889788836284),(0.999732896029236,0.999865728939372,1.,0.994017305594881,
0.990889788836284)))
REPRESENTATION_ITEM('')
SURFACE()
);
#4353=(
BOUNDED_SURFACE()
B_SPLINE_SURFACE(1,2,((#167807,#167808,#167809,#167810,#167811),(#167812,
#167813,#167814,#167815,#167816)),.UNSPECIFIED.,.F.,.F.,.F.)
B_SPLINE_SURFACE_WITH_KNOTS((2,2),(3,2,3),(0.938576859128167,1.),(0.066525725473656,
0.0714285714285714,0.0736543502199112),.UNSPECIFIED.)
GEOMETRIC_REPRESENTATION_ITEM()
RATIONAL_B_SPLINE_SURFACE(((0.996794362316491,0.998279055819231,1.,0.999218731101516,
0.99848615229188),(0.996794362316491,0.998279055819231,1.,0.999218731101516,
0.99848615229188)))
REPRESENTATION_ITEM('')
SURFACE()
);
#4354=(
BOUNDED_SURFACE()
B_SPLINE_SURFACE(1,2,((#167823,#167824,#167825,#167826,#167827),(#167828,
#167829,#167830,#167831,#167832)),.UNSPECIFIED.,.F.,.F.,.F.)
B_SPLINE_SURFACE_WITH_KNOTS((2,2),(3,2,3),(0.,0.0529045403781331),(0.0665257254736559,
0.0714285714285714,0.0736968668684971),.UNSPECIFIED.)
GEOMETRIC_REPRESENTATION_ITEM()
RATIONAL_B_SPLINE_SURFACE(((0.996794362316491,0.998279055819231,1.,0.999203807365457,
0.998458182734336),(0.996794362316491,0.998279055819231,1.,0.999203807365457,
0.998458182734336)))
REPRESENTATION_ITEM('')
SURFACE()
);
#4355=(
BOUNDED_SURFACE()
B_SPLINE_SURFACE(1,2,((#167843,#167844,#167845),(#167846,#167847,#167848)),
 .UNSPECIFIED.,.F.,.F.,.F.)
B_SPLINE_SURFACE_WITH_KNOTS((2,2),(3,3),(0.,0.0528815468798318),(0.659860018385434,
0.666841081426898),.UNSPECIFIED.)
GEOMETRIC_REPRESENTATION_ITEM()
RATIONAL_B_SPLINE_SURFACE(((0.990904995179416,0.989621173673383,0.988816334712145),
(0.990904995179416,0.989621173673383,0.988816334712145)))
REPRESENTATION_ITEM('')
SURFACE()
);
#4356=(
BOUNDED_SURFACE()
B_SPLINE_SURFACE(1,2,((#167850,#167851,#167852,#167853,#167854),(#167855,
#167856,#167857,#167858,#167859)),.UNSPECIFIED.,.F.,.F.,.F.)
B_SPLINE_SURFACE_WITH_KNOTS((2,2),(3,2,3),(0.938550151647612,1.00001008240785),
(0.659832011354087,0.659901408087481,0.666841081426897),.UNSPECIFIED.)
GEOMETRIC_REPRESENTATION_ITEM()
RATIONAL_B_SPLINE_SURFACE(((0.990889788836284,0.990889788836284,0.990889788836284,
0.98961640190086,0.988816334712145),(0.990889788836284,0.990889788836284,
0.990889788836284,0.98961640190086,0.988816334712145)))
REPRESENTATION_ITEM('')
SURFACE()
);
#4357=(
BOUNDED_SURFACE()
B_SPLINE_SURFACE(1,2,((#167861,#167862,#167863,#167864,#167865),(#167866,
#167867,#167868,#167869,#167870)),.UNSPECIFIED.,.F.,.F.,.F.)
B_SPLINE_SURFACE_WITH_KNOTS((2,2),(3,2,3),(-1.06888495707795E-6,0.182885378421191),
(0.0734807488197897,0.0736543502199111,0.0910144902320524),
 .UNSPECIFIED.)
GEOMETRIC_REPRESENTATION_ITEM()
RATIONAL_B_SPLINE_SURFACE(((0.99848615229188,0.99848615229188,0.99848615229188,
0.992772345172011,0.990020524139833),(0.99848615229188,0.99848615229188,
0.99848615229188,0.992772345172011,0.990020524139833)))
REPRESENTATION_ITEM('')
SURFACE()
);
#4358=(
BOUNDED_SURFACE()
B_SPLINE_SURFACE(1,2,((#167881,#167882,#167883,#167884,#167885),(#167886,
#167887,#167888,#167889,#167890)),.UNSPECIFIED.,.F.,.F.,.F.)
B_SPLINE_SURFACE_WITH_KNOTS((2,2),(3,2,3),(0.,0.182805892339158),(0.642474614281364,
0.642857142857143,0.659901408087481),.UNSPECIFIED.)
GEOMETRIC_REPRESENTATION_ITEM()
RATIONAL_B_SPLINE_SURFACE(((0.999732896029236,0.999865728939372,1.,0.994017305594881,
0.990889788836284),(0.999732896029236,0.999865728939372,1.,0.994017305594881,
0.990889788836284)))
REPRESENTATION_ITEM('')
SURFACE()
);
#4359=(
BOUNDED_SURFACE()
B_SPLINE_SURFACE(1,2,((#167892,#167893,#167894,#167895,#167896),(#167897,
#167898,#167899,#167900,#167901)),.UNSPECIFIED.,.F.,.F.,.F.)
B_SPLINE_SURFACE_WITH_KNOTS((2,2),(3,2,3),(0.938576859128169,1.),(0.0665257254736559,
0.0714285714285714,0.0736543502199112),.UNSPECIFIED.)
GEOMETRIC_REPRESENTATION_ITEM()
RATIONAL_B_SPLINE_SURFACE(((0.996794362316491,0.998279055819231,1.,0.999218731101516,
0.99848615229188),(0.996794362316491,0.998279055819231,1.,0.999218731101516,
0.99848615229188)))
REPRESENTATION_ITEM('')
SURFACE()
);
#4360=(
BOUNDED_SURFACE()
B_SPLINE_SURFACE(1,2,((#167909,#167910,#167911,#167912,#167913),(#167914,
#167915,#167916,#167917,#167918)),.UNSPECIFIED.,.F.,.F.,.F.)
B_SPLINE_SURFACE_WITH_KNOTS((2,2),(3,2,3),(0.,0.0529045403781336),(0.0665257254736559,
0.0714285714285714,0.0736968668684972),.UNSPECIFIED.)
GEOMETRIC_REPRESENTATION_ITEM()
RATIONAL_B_SPLINE_SURFACE(((0.996794362316491,0.998279055819231,1.,0.999203807365457,
0.998458182734336),(0.996794362316491,0.998279055819231,1.,0.999203807365457,
0.998458182734336)))
REPRESENTATION_ITEM('')
SURFACE()
);
#4361=(
BOUNDED_SURFACE()
B_SPLINE_SURFACE(1,2,((#167929,#167930,#167931),(#167932,#167933,#167934)),
 .UNSPECIFIED.,.F.,.F.,.F.)
B_SPLINE_SURFACE_WITH_KNOTS((2,2),(3,3),(0.,0.0528815468798333),(0.659860018385656,
0.666841081426897),.UNSPECIFIED.)
GEOMETRIC_REPRESENTATION_ITEM()
RATIONAL_B_SPLINE_SURFACE(((0.990904995179334,0.989621173673357,0.988816334712145),
(0.990904995179334,0.989621173673357,0.988816334712145)))
REPRESENTATION_ITEM('')
SURFACE()
);
#4362=(
BOUNDED_SURFACE()
B_SPLINE_SURFACE(1,2,((#167936,#167937,#167938,#167939,#167940),(#167941,
#167942,#167943,#167944,#167945)),.UNSPECIFIED.,.F.,.F.,.F.)
B_SPLINE_SURFACE_WITH_KNOTS((2,2),(3,2,3),(0.938550151647612,1.00001008244309),
(0.659832011354087,0.659901408087481,0.666841081426897),.UNSPECIFIED.)
GEOMETRIC_REPRESENTATION_ITEM()
RATIONAL_B_SPLINE_SURFACE(((0.990889788836284,0.990889788836284,0.990889788836284,
0.98961640190086,0.988816334712146),(0.990889788836284,0.990889788836284,
0.990889788836284,0.98961640190086,0.988816334712146)))
REPRESENTATION_ITEM('')
SURFACE()
);
#4363=(
BOUNDED_SURFACE()
B_SPLINE_SURFACE(1,2,((#167947,#167948,#167949,#167950,#167951),(#167952,
#167953,#167954,#167955,#167956)),.UNSPECIFIED.,.F.,.F.,.F.)
B_SPLINE_SURFACE_WITH_KNOTS((2,2),(3,2,3),(-1.07113328560007E-6,0.182885378421191),
(0.0734807488197897,0.0736543502199111,0.0910144902320524),
 .UNSPECIFIED.)
GEOMETRIC_REPRESENTATION_ITEM()
RATIONAL_B_SPLINE_SURFACE(((0.99848615229188,0.99848615229188,0.99848615229188,
0.992772345172011,0.990020524139833),(0.99848615229188,0.99848615229188,
0.99848615229188,0.992772345172011,0.990020524139833)))
REPRESENTATION_ITEM('')
SURFACE()
);
#4364=(
BOUNDED_SURFACE()
B_SPLINE_SURFACE(1,2,((#167967,#167968,#167969,#167970,#167971),(#167972,
#167973,#167974,#167975,#167976)),.UNSPECIFIED.,.F.,.F.,.F.)
B_SPLINE_SURFACE_WITH_KNOTS((2,2),(3,2,3),(0.,0.182805892339156),(0.642474614281366,
0.642857142857143,0.659901408087481),.UNSPECIFIED.)
GEOMETRIC_REPRESENTATION_ITEM()
RATIONAL_B_SPLINE_SURFACE(((0.999732896029237,0.999865728939372,1.,0.994017305594881,
0.990889788836284),(0.999732896029237,0.999865728939372,1.,0.994017305594881,
0.990889788836284)))
REPRESENTATION_ITEM('')
SURFACE()
);
#4365=(
BOUNDED_SURFACE()
B_SPLINE_SURFACE(1,2,((#167978,#167979,#167980,#167981,#167982),(#167983,
#167984,#167985,#167986,#167987)),.UNSPECIFIED.,.F.,.F.,.F.)
B_SPLINE_SURFACE_WITH_KNOTS((2,2),(3,2,3),(0.938576859128171,1.),(0.0665257254736565,
0.0714285714285714,0.0736543502199112),.UNSPECIFIED.)
GEOMETRIC_REPRESENTATION_ITEM()
RATIONAL_B_SPLINE_SURFACE(((0.996794362316492,0.998279055819231,1.,0.999218731101516,
0.99848615229188),(0.996794362316492,0.998279055819231,1.,0.999218731101516,
0.99848615229188)))
REPRESENTATION_ITEM('')
SURFACE()
);
#4366=(
BOUNDED_SURFACE()
B_SPLINE_SURFACE(1,2,((#167995,#167996,#167997,#167998,#167999),(#168000,
#168001,#168002,#168003,#168004)),.UNSPECIFIED.,.F.,.F.,.F.)
B_SPLINE_SURFACE_WITH_KNOTS((2,2),(3,2,3),(0.,0.052904540378127),(0.0665257254736564,
0.0714285714285714,0.0736968668684973),.UNSPECIFIED.)
GEOMETRIC_REPRESENTATION_ITEM()
RATIONAL_B_SPLINE_SURFACE(((0.996794362316492,0.998279055819231,1.,0.999203807365457,
0.998458182734336),(0.996794362316492,0.998279055819231,1.,0.999203807365457,
0.998458182734336)))
REPRESENTATION_ITEM('')
SURFACE()
);
#4367=(
BOUNDED_SURFACE()
B_SPLINE_SURFACE(1,2,((#168015,#168016,#168017),(#168018,#168019,#168020)),
 .UNSPECIFIED.,.F.,.F.,.F.)
B_SPLINE_SURFACE_WITH_KNOTS((2,2),(3,3),(0.,0.0528815468798321),(0.659860018385656,
0.666841081426897),.UNSPECIFIED.)
GEOMETRIC_REPRESENTATION_ITEM()
RATIONAL_B_SPLINE_SURFACE(((0.990904995179334,0.989621173673357,0.988816334712145),
(0.990904995179334,0.989621173673357,0.988816334712145)))
REPRESENTATION_ITEM('')
SURFACE()
);
#4368=(
BOUNDED_SURFACE()
B_SPLINE_SURFACE(1,2,((#168022,#168023,#168024,#168025,#168026),(#168027,
#168028,#168029,#168030,#168031)),.UNSPECIFIED.,.F.,.F.,.F.)
B_SPLINE_SURFACE_WITH_KNOTS((2,2),(3,2,3),(0.938550151647611,1.00001008251789),
(0.659832011354087,0.659901408087481,0.666841081426897),.UNSPECIFIED.)
GEOMETRIC_REPRESENTATION_ITEM()
RATIONAL_B_SPLINE_SURFACE(((0.990889788836284,0.990889788836284,0.990889788836284,
0.98961640190086,0.988816334712145),(0.990889788836284,0.990889788836284,
0.990889788836284,0.98961640190086,0.988816334712145)))
REPRESENTATION_ITEM('')
SURFACE()
);
#4369=(
BOUNDED_SURFACE()
B_SPLINE_SURFACE(1,2,((#168033,#168034,#168035,#168036,#168037),(#168038,
#168039,#168040,#168041,#168042)),.UNSPECIFIED.,.F.,.F.,.F.)
B_SPLINE_SURFACE_WITH_KNOTS((2,2),(3,2,3),(0.,0.182885378421188),(0.0734807488197898,
0.0736543502199112,0.0910144902320524),.UNSPECIFIED.)
GEOMETRIC_REPRESENTATION_ITEM()
RATIONAL_B_SPLINE_SURFACE(((0.99848615229188,0.99848615229188,0.99848615229188,
0.992772345172011,0.990020524139833),(0.99848615229188,0.99848615229188,
0.99848615229188,0.992772345172011,0.990020524139833)))
REPRESENTATION_ITEM('')
SURFACE()
);
#4370=(
BOUNDED_SURFACE()
B_SPLINE_SURFACE(3,1,((#168511,#168512),(#168513,#168514),(#168515,#168516),
(#168517,#168518)),.UNSPECIFIED.,.F.,.F.,.F.)
B_SPLINE_SURFACE_WITH_KNOTS((4,4),(2,2),(-8.56707287333166E-8,1.00000008548767),
(0.00592879452423504,0.99406998347921),.UNSPECIFIED.)
GEOMETRIC_REPRESENTATION_ITEM()
RATIONAL_B_SPLINE_SURFACE(((1.00000000253644,1.00000000253644),(0.990131033425531,
0.990131033425531),(0.990131033423724,0.990131033423724),(1.00000000253103,
1.00000000253102)))
REPRESENTATION_ITEM('')
SURFACE()
);
#4371=(
BOUNDED_SURFACE()
B_SPLINE_SURFACE(3,2,((#168680,#168681,#168682),(#168683,#168684,#168685),
(#168686,#168687,#168688),(#168689,#168690,#168691),(#168692,#168693,#168694),
(#168695,#168696,#168697),(#168698,#168699,#168700),(#168701,#168702,#168703),
(#168704,#168705,#168706),(#168707,#168708,#168709),(#168710,#168711,#168712),
(#168713,#168714,#168715),(#168716,#168717,#168718),(#168719,#168720,#168721),
(#168722,#168723,#168724),(#168725,#168726,#168727),(#168728,#168729,#168730),
(#168731,#168732,#168733),(#168734,#168735,#168736),(#168737,#168738,#168739),
(#168740,#168741,#168742),(#168743,#168744,#168745),(#168746,#168747,#168748),
(#168749,#168750,#168751),(#168752,#168753,#168754),(#168755,#168756,#168757),
(#168758,#168759,#168760),(#168761,#168762,#168763),(#168764,#168765,#168766),
(#168767,#168768,#168769),(#168770,#168771,#168772),(#168773,#168774,#168775),
(#168776,#168777,#168778),(#168779,#168780,#168781),(#168782,#168783,#168784),
(#168785,#168786,#168787),(#168788,#168789,#168790),(#168791,#168792,#168793),
(#168794,#168795,#168796),(#168797,#168798,#168799),(#168800,#168801,#168802),
(#168803,#168804,#168805),(#168806,#168807,#168808),(#168809,#168810,#168811),
(#168812,#168813,#168814),(#168815,#168816,#168817),(#168818,#168819,#168820),
(#168821,#168822,#168823),(#168824,#168825,#168826),(#168827,#168828,#168829)),
 .UNSPECIFIED.,.F.,.F.,.F.)
B_SPLINE_SURFACE_WITH_KNOTS((4,2,2,2,2,2,2,2,2,2,2,2,2,2,2,2,2,2,2,2,2,
2,2,2,4),(3,3),(0.00438204809785496,0.00442773757395586,0.00445058231200631,
0.00446200468103154,0.00447342705005676,0.00451911652615766,0.00454196126420811,
0.00456480600225856,0.00474756390666215,0.00511307971546933,0.0058441113330837,
0.00730617456831243,0.0102303010387699,0.0131544275092274,0.0146164907444561,
0.0153475223620705,0.0157130381708776,0.0158957960752812,0.0159186408133317,
0.0159414855513821,0.015987175027483,0.0159985973965083,0.0160100197655335,
0.0160328645035839,0.0160785539796848),(0.,1.),.UNSPECIFIED.)
GEOMETRIC_REPRESENTATION_ITEM()
RATIONAL_B_SPLINE_SURFACE(((1.,0.934218767962417,1.),(1.,0.934219268725543,
1.),(1.,0.934219769475696,1.),(1.,0.934220520581468,1.),(1.,0.934221098516136,
1.),(1.,0.93422098270531,1.),(1.,0.934218146084782,1.),(1.,0.934214890227589,
1.),(1.,0.934213259806577,1.),(1.,0.934205095242336,1.),(1.,0.934198523721367,
1.),(1.,0.934188606688787,1.),(1.,0.934185286091514,1.),(1.,0.934178648365384,
1.),(1.,0.934175336166584,1.),(1.,0.934145586350039,1.),(1.,0.934119568538277,
1.),(1.,0.934042793646304,1.),(1.,0.933993312945644,1.),(1.,0.933849992791617,
1.),(1.,0.933761355730532,1.),(1.,0.93351603018512,1.),(1.,0.933379914807182,
1.),(1.,0.93305317905279,1.),(1.,0.932943966614937,1.),(1.,0.932943963043387,
1.),(1.,0.933053175643618,1.),(1.,0.933379911515294,1.),(1.,0.93351602735766,
1.),(1.,0.933761354538682,1.),(1.,0.933849992301547,1.),(1.,0.933993313783528,
1.),(1.,0.93404279394322,1.),(1.,0.934119568707732,1.),(1.,0.934145586476303,
1.),(1.,0.934175336243606,1.),(1.,0.934178648436936,1.),(1.,0.934185286152106,
1.),(1.,0.934188606743602,1.),(1.,0.934198523759289,1.),(1.,0.9342050952691,
1.),(1.,0.934213259819631,1.),(1.,0.934214890237893,1.),(1.,0.934218146089636,
1.),(1.,0.934220982704232,1.),(1.,0.934221098518431,1.),(1.,0.934220520582345,
1.),(1.,0.934219769477844,1.),(1.,0.934219268728507,1.),(1.,0.934218767966226,
1.)))
REPRESENTATION_ITEM('')
SURFACE()
);
#4372=(
BOUNDED_SURFACE()
B_SPLINE_SURFACE(3,1,((#168914,#168915),(#168916,#168917),(#168918,#168919),
(#168920,#168921)),.UNSPECIFIED.,.F.,.F.,.F.)
B_SPLINE_SURFACE_WITH_KNOTS((4,4),(2,2),(-8.59560614834357E-8,1.00000008613876),
(0.00592875831867496,0.994072405691805),.UNSPECIFIED.)
GEOMETRIC_REPRESENTATION_ITEM()
RATIONAL_B_SPLINE_SURFACE(((1.00000000254489,1.00000000254489),(0.990131033419105,
0.990131033419106),(0.990131033420908,0.990131033420909),(1.0000000025503,
1.0000000025503)))
REPRESENTATION_ITEM('')
SURFACE()
);
#4373=(
BOUNDED_SURFACE()
B_SPLINE_SURFACE(3,2,((#169270,#169271,#169272),(#169273,#169274,#169275),
(#169276,#169277,#169278),(#169279,#169280,#169281),(#169282,#169283,#169284),
(#169285,#169286,#169287),(#169288,#169289,#169290),(#169291,#169292,#169293),
(#169294,#169295,#169296),(#169297,#169298,#169299),(#169300,#169301,#169302),
(#169303,#169304,#169305),(#169306,#169307,#169308),(#169309,#169310,#169311),
(#169312,#169313,#169314),(#169315,#169316,#169317),(#169318,#169319,#169320),
(#169321,#169322,#169323),(#169324,#169325,#169326),(#169327,#169328,#169329),
(#169330,#169331,#169332),(#169333,#169334,#169335),(#169336,#169337,#169338),
(#169339,#169340,#169341),(#169342,#169343,#169344),(#169345,#169346,#169347),
(#169348,#169349,#169350),(#169351,#169352,#169353),(#169354,#169355,#169356),
(#169357,#169358,#169359),(#169360,#169361,#169362),(#169363,#169364,#169365),
(#169366,#169367,#169368),(#169369,#169370,#169371),(#169372,#169373,#169374),
(#169375,#169376,#169377),(#169378,#169379,#169380),(#169381,#169382,#169383),
(#169384,#169385,#169386),(#169387,#169388,#169389),(#169390,#169391,#169392),
(#169393,#169394,#169395),(#169396,#169397,#169398),(#169399,#169400,#169401),
(#169402,#169403,#169404),(#169405,#169406,#169407),(#169408,#169409,#169410),
(#169411,#169412,#169413),(#169414,#169415,#169416),(#169417,#169418,#169419),
(#169420,#169421,#169422),(#169423,#169424,#169425),(#169426,#169427,#169428),
(#169429,#169430,#169431),(#169432,#169433,#169434),(#169435,#169436,#169437),
(#169438,#169439,#169440),(#169441,#169442,#169443),(#169444,#169445,#169446),
(#169447,#169448,#169449),(#169450,#169451,#169452),(#169453,#169454,#169455),
(#169456,#169457,#169458),(#169459,#169460,#169461),(#169462,#169463,#169464),
(#169465,#169466,#169467),(#169468,#169469,#169470),(#169471,#169472,#169473),
(#169474,#169475,#169476),(#169477,#169478,#169479),(#169480,#169481,#169482),
(#169483,#169484,#169485),(#169486,#169487,#169488),(#169489,#169490,#169491)),
 .UNSPECIFIED.,.F.,.F.,.F.)
B_SPLINE_SURFACE_WITH_KNOTS((4,2,2,2,2,2,2,2,2,2,2,2,2,2,2,2,2,2,2,2,2,
2,2,2,2,2,2,2,2,2,2,2,2,2,2,2,4),(3,3),(0.0179612750605611,0.0180038120055911,
0.0180250804781061,0.0180303975962348,0.0180357147143635,0.018046348950621,
0.0181314228406809,0.0182164967307408,0.0182271309669983,0.0182377652032558,
0.0182590336757708,0.0183015706208007,0.0186418661810403,0.0193224573015194,
0.0200030484219985,0.0206836395424776,0.0213642306629567,0.0220448217834359,
0.0234060040243941,0.0247671862653523,0.0254477773858315,0.0261283685063106,
0.0268089596267897,0.0274895507472688,0.0281701418677479,0.0285104374279875,
0.0285529743730174,0.0285742428455324,0.0285848770817899,0.0285955113180474,
0.0286805852081073,0.0287656590981672,0.0287762933344247,0.0287816104525534,
0.0287869275706821,0.0288081960431971,0.0288507329882271),(0.,1.),
 .UNSPECIFIED.)
GEOMETRIC_REPRESENTATION_ITEM()
RATIONAL_B_SPLINE_SURFACE(((1.,0.936904821453696,1.),(1.,0.936904794108661,
1.),(1.,0.936904766764048,1.),(1.,0.936904725747745,1.),(1.,0.936905128260374,
1.),(1.,0.936904590939729,1.),(1.,0.936903346459592,1.),(1.,0.936901627765994,
1.),(1.,0.936900767797278,1.),(1.,0.936898186025644,1.),(1.,0.936896462357224,
1.),(1.,0.936880926961442,1.),(1.,0.936866958574279,1.),(1.,0.936838704163249,
1.),(1.,0.936824418139244,1.),(1.,0.936808168049907,1.),(1.,0.936806360007847,
1.),(1.,0.936802738971814,1.),(1.,0.936800862095946,1.),(1.,0.936795849431034,
1.),(1.,0.936792514575336,1.),(1.,0.936782530740213,1.),(1.,0.936775902492467,
1.),(1.,0.936716496356665,1.),(1.,0.936665452813206,1.),(1.,0.936517538966925,
1.),(1.,0.93642586040289,1.),(1.,0.936256634386565,1.),(1.,0.936179189842934,
1.),(1.,0.936038226722045,1.),(1.,0.935974776717855,1.),(1.,0.935862123528188,
1.),(1.,0.935812981619732,1.),(1.,0.93572859095576,1.),(1.,0.935693341074582,
1.),(1.,0.935608906032864,1.),(1.,0.935580787501173,1.),(1.,0.935580755598083,
1.),(1.,0.935608926183175,1.),(1.,0.935693493416876,1.),(1.,0.935728787043659,
1.),(1.,0.935813225027166,1.),(1.,0.935862370889367,1.),(1.,0.935974951078453,
1.),(1.,0.936038323852223,1.),(1.,0.936179015169328,1.),(1.,0.93625634937854,
1.),(1.,0.936425491452454,1.),(1.,0.936517220625567,1.),(1.,0.936665263045723,
1.),(1.,0.9367163495052,1.),(1.,0.936775803162665,1.),(1.,0.936782436680194,
1.),(1.,0.936792428402367,1.),(1.,0.936795765884152,1.),(1.,0.936800782483542,
1.),(1.,0.936802654166495,1.),(1.,0.936806278312161,1.),(1.,0.936808087904325,
1.),(1.,0.936824351902175,1.),(1.,0.936838649987733,1.),(1.,0.936866927922814,
1.),(1.,0.936880907772467,1.),(1.,0.93689645572885,1.),(1.,0.936898180788246,
1.),(1.,0.936900764639372,1.),(1.,0.936901625300091,1.),(1.,0.936903345375374,
1.),(1.,0.936904591114425,1.),(1.,0.936905127567446,1.),(1.,0.936904725770864,
1.),(1.,0.936904766820085,1.),(1.,0.93690479418665,1.),(1.,0.936904821553629,
1.)))
REPRESENTATION_ITEM('')
SURFACE()
);
#4374=(
BOUNDED_SURFACE()
B_SPLINE_SURFACE(3,2,((#169695,#169696,#169697),(#169698,#169699,#169700),
(#169701,#169702,#169703),(#169704,#169705,#169706),(#169707,#169708,#169709),
(#169710,#169711,#169712),(#169713,#169714,#169715),(#169716,#169717,#169718),
(#169719,#169720,#169721),(#169722,#169723,#169724),(#169725,#169726,#169727),
(#169728,#169729,#169730),(#169731,#169732,#169733),(#169734,#169735,#169736),
(#169737,#169738,#169739),(#169740,#169741,#169742),(#169743,#169744,#169745),
(#169746,#169747,#169748),(#169749,#169750,#169751),(#169752,#169753,#169754),
(#169755,#169756,#169757),(#169758,#169759,#169760),(#169761,#169762,#169763),
(#169764,#169765,#169766),(#169767,#169768,#169769),(#169770,#169771,#169772),
(#169773,#169774,#169775),(#169776,#169777,#169778),(#169779,#169780,#169781),
(#169782,#169783,#169784),(#169785,#169786,#169787),(#169788,#169789,#169790),
(#169791,#169792,#169793),(#169794,#169795,#169796),(#169797,#169798,#169799),
(#169800,#169801,#169802),(#169803,#169804,#169805),(#169806,#169807,#169808),
(#169809,#169810,#169811),(#169812,#169813,#169814),(#169815,#169816,#169817),
(#169818,#169819,#169820),(#169821,#169822,#169823),(#169824,#169825,#169826),
(#169827,#169828,#169829),(#169830,#169831,#169832),(#169833,#169834,#169835),
(#169836,#169837,#169838),(#169839,#169840,#169841),(#169842,#169843,#169844),
(#169845,#169846,#169847),(#169848,#169849,#169850)),.UNSPECIFIED.,.F.,
 .F.,.F.)
B_SPLINE_SURFACE_WITH_KNOTS((4,2,2,2,2,2,2,2,2,2,2,2,2,2,2,2,2,2,2,2,2,
2,2,2,2,4),(3,3),(0.0156015153159842,0.0159832133339201,0.0161740623428881,
0.016269486847372,0.016317199099614,0.016341055225735,0.0163529832887955,
0.016364911351856,0.0171283073877279,0.0186550994594716,0.0194184954953434,
0.0201818915312153,0.021708683602959,0.0224720796388308,0.0232354756747027,
0.0247622677464464,0.0262890598181901,0.0270524558540619,0.0270584198855922,
0.0270643839171224,0.0270763119801829,0.0271001681063039,0.0271478803585459,
0.0272433048630299,0.0274341538719979,0.0278158518899338),(0.,1.),
 .UNSPECIFIED.)
GEOMETRIC_REPRESENTATION_ITEM()
RATIONAL_B_SPLINE_SURFACE(((1.,0.776444097652961,1.),(1.,0.776058926606058,
1.),(1.,0.775673843099958,1.),(1.,0.775096481210286,1.),(1.,0.774904071156476,
1.),(1.,0.774615538680226,1.),(1.,0.774519374957158,1.),(1.,0.774375152135543,
1.),(1.,0.774327081655569,1.),(1.,0.774254981891155,1.),(1.,0.774230949628936,
1.),(1.,0.774194902757698,1.),(1.,0.774182887387605,1.),(1.,0.774158857160334,
1.),(1.,0.774150992177244,1.),(1.,0.773543654478887,1.),(1.,0.77298505575604,
1.),(1.,0.771431978714256,1.),(1.,0.77056039765908,1.),(1.,0.769511352915782,
1.),(1.,0.769204886519117,1.),(1.,0.768679727581747,1.),(1.,0.768460849050857,
1.),(1.,0.767935355999606,1.),(1.,0.767759786976898,1.),(1.,0.767759465570472,
1.),(1.,0.767803217713065,1.),(1.,0.767978602526777,1.),(1.,0.768110252004706,
1.),(1.,0.768636034778269,1.),(1.,0.769161202927011,1.),(1.,0.770557236848331,
1.),(1.,0.771427908462379,1.),(1.,0.772982352753207,1.),(1.,0.773541690771539,
1.),(1.,0.774144848886315,1.),(1.,0.774149526925736,1.),(1.,0.774158887792997,
1.),(1.,0.77416299521755,1.),(1.,0.774181034357718,1.),(1.,0.774193060706593,
1.),(1.,0.774229140511077,1.),(1.,0.774253194724663,1.),(1.,0.774325360330513,
1.),(1.,0.774373474688076,1.),(1.,0.774517829090711,1.),(1.,0.774614080465712,
1.),(1.,0.774902875681382,1.),(1.,0.775095460606343,1.),(1.,0.775673346165181,
1.),(1.,0.776058777525586,1.),(1.,0.776444294966368,1.)))
REPRESENTATION_ITEM('')
SURFACE()
);
#4375=(
BOUNDED_CURVE()
B_SPLINE_CURVE(2,(#95475,#95476,#95477,#95478,#95479),.UNSPECIFIED.,.F.,
 .F.)
B_SPLINE_CURVE_WITH_KNOTS((3,2,3),(0.418312080773434,0.428571428571429,
0.430498434992938),.UNSPECIFIED.)
CURVE()
GEOMETRIC_REPRESENTATION_ITEM()
RATIONAL_B_SPLINE_CURVE((0.99383221411677,0.996398874234721,1.,0.999323602960832,
0.998683701721927))
REPRESENTATION_ITEM('')
);
#4376=(
BOUNDED_CURVE()
B_SPLINE_CURVE(2,(#98022,#98023,#98024,#98025,#98026),.UNSPECIFIED.,.F.,
 .F.)
B_SPLINE_CURVE_WITH_KNOTS((3,2,3),(0.349440546437696,0.359118183105575,
0.366891343982437),.UNSPECIFIED.)
CURVE()
GEOMETRIC_REPRESENTATION_ITEM()
RATIONAL_B_SPLINE_CURVE((0.994126602224873,0.996603060231146,1.,0.997271548790187,
0.995136940905933))
REPRESENTATION_ITEM('')
);
#4377=(
BOUNDED_CURVE()
B_SPLINE_CURVE(2,(#98055,#98056,#98057,#98058,#98059),.UNSPECIFIED.,.F.,
 .F.)
B_SPLINE_CURVE_WITH_KNOTS((3,2,3),(0.349440546446772,0.359118183105576,
0.366891343971801),.UNSPECIFIED.)
CURVE()
GEOMETRIC_REPRESENTATION_ITEM()
RATIONAL_B_SPLINE_CURVE((0.994126602224872,0.996603060231146,1.,0.99727154879392,
0.995136940911775))
REPRESENTATION_ITEM('')
);
#4378=(
BOUNDED_CURVE()
B_SPLINE_CURVE(2,(#98088,#98089,#98090,#98091,#98092),.UNSPECIFIED.,.F.,
 .F.)
B_SPLINE_CURVE_WITH_KNOTS((3,2,3),(0.349440546433574,0.359118183105575,
0.366891343991316),.UNSPECIFIED.)
CURVE()
GEOMETRIC_REPRESENTATION_ITEM()
RATIONAL_B_SPLINE_CURVE((0.994126602224873,0.996603060231146,1.,0.99727154878707,
0.995136940901056))
REPRESENTATION_ITEM('')
);
#4379=(
BOUNDED_CURVE()
B_SPLINE_CURVE(2,(#98121,#98122,#98123,#98124,#98125),.UNSPECIFIED.,.F.,
 .F.)
B_SPLINE_CURVE_WITH_KNOTS((3,2,3),(0.349440546441033,0.359118183105575,
0.36689134396703),.UNSPECIFIED.)
CURVE()
GEOMETRIC_REPRESENTATION_ITEM()
RATIONAL_B_SPLINE_CURVE((0.994126602224873,0.996603060231146,1.,0.997271548795594,
0.995136940914395))
REPRESENTATION_ITEM('')
);
#4380=(
BOUNDED_CURVE()
B_SPLINE_CURVE(2,(#98154,#98155,#98156,#98157,#98158),.UNSPECIFIED.,.F.,
 .F.)
B_SPLINE_CURVE_WITH_KNOTS((3,2,3),(0.349440546416899,0.359118183105575,
0.366891343982081),.UNSPECIFIED.)
CURVE()
GEOMETRIC_REPRESENTATION_ITEM()
RATIONAL_B_SPLINE_CURVE((0.994126602224873,0.996603060231146,1.,0.997271548790312,
0.995136940906129))
REPRESENTATION_ITEM('')
);
#4381=(
BOUNDED_CURVE()
B_SPLINE_CURVE(2,(#98187,#98188,#98189,#98190,#98191),.UNSPECIFIED.,.F.,
 .F.)
B_SPLINE_CURVE_WITH_KNOTS((3,2,3),(0.349440546419126,0.359118183105565,
0.366891343966471),.UNSPECIFIED.)
CURVE()
GEOMETRIC_REPRESENTATION_ITEM()
RATIONAL_B_SPLINE_CURVE((0.994126602224873,0.996603060231146,1.,0.997271548795788,
0.995136940914697))
REPRESENTATION_ITEM('')
);
#4382=(
BOUNDED_CURVE()
B_SPLINE_CURVE(2,(#98220,#98221,#98222,#98223,#98224),.UNSPECIFIED.,.F.,
 .F.)
B_SPLINE_CURVE_WITH_KNOTS((3,2,3),(0.349440546426667,0.359118183105575,
0.366891343970343),.UNSPECIFIED.)
CURVE()
GEOMETRIC_REPRESENTATION_ITEM()
RATIONAL_B_SPLINE_CURVE((0.994126602224873,0.996603060231146,1.,0.997271548794432,
0.995136940912576))
REPRESENTATION_ITEM('')
);
#4383=(
BOUNDED_CURVE()
B_SPLINE_CURVE(2,(#98288,#98289,#98290,#98291,#98292),.UNSPECIFIED.,.F.,
 .F.)
B_SPLINE_CURVE_WITH_KNOTS((3,2,3),(0.349440546445551,0.359118183105575,
0.366891343984427),.UNSPECIFIED.)
CURVE()
GEOMETRIC_REPRESENTATION_ITEM()
RATIONAL_B_SPLINE_CURVE((0.994126602224873,0.996603060231146,1.,0.997271548789488,
0.99513694090484))
REPRESENTATION_ITEM('')
);
#4384=(
BOUNDED_CURVE()
B_SPLINE_CURVE(2,(#98321,#98322,#98323,#98324,#98325),.UNSPECIFIED.,.F.,
 .F.)
B_SPLINE_CURVE_WITH_KNOTS((3,2,3),(0.349440546417489,0.359118183105584,
0.366891343969882),.UNSPECIFIED.)
CURVE()
GEOMETRIC_REPRESENTATION_ITEM()
RATIONAL_B_SPLINE_CURVE((0.994126602224868,0.996603060231143,1.,0.997271548794597,
0.995136940912833))
REPRESENTATION_ITEM('')
);
#4385=(
BOUNDED_CURVE()
B_SPLINE_CURVE(2,(#98354,#98355,#98356,#98357,#98358),.UNSPECIFIED.,.F.,
 .F.)
B_SPLINE_CURVE_WITH_KNOTS((3,2,3),(0.349440546409791,0.359118183105584,
0.366891343977855),.UNSPECIFIED.)
CURVE()
GEOMETRIC_REPRESENTATION_ITEM()
RATIONAL_B_SPLINE_CURVE((0.994126602224868,0.996603060231143,1.,0.997271548791798,
0.995136940908454))
REPRESENTATION_ITEM('')
);
#4386=(
BOUNDED_CURVE()
B_SPLINE_CURVE(2,(#98387,#98388,#98389,#98390,#98391),.UNSPECIFIED.,.F.,
 .F.)
B_SPLINE_CURVE_WITH_KNOTS((3,2,3),(0.349440546428452,0.359118183105584,
0.366891343978224),.UNSPECIFIED.)
CURVE()
GEOMETRIC_REPRESENTATION_ITEM()
RATIONAL_B_SPLINE_CURVE((0.994126602224868,0.996603060231143,1.,0.997271548791668,
0.995136940908252))
REPRESENTATION_ITEM('')
);
#4387=(
BOUNDED_CURVE()
B_SPLINE_CURVE(2,(#98490,#98491,#98492,#98493,#98494),.UNSPECIFIED.,.F.,
 .F.)
B_SPLINE_CURVE_WITH_KNOTS((3,2,3),(0.349440546425061,0.359118183105584,
0.366891343989552),.UNSPECIFIED.)
CURVE()
GEOMETRIC_REPRESENTATION_ITEM()
RATIONAL_B_SPLINE_CURVE((0.994126602224868,0.996603060231143,1.,0.997271548787692,
0.99513694090203))
REPRESENTATION_ITEM('')
);
#4388=(
BOUNDED_CURVE()
B_SPLINE_CURVE(2,(#98523,#98524,#98525,#98526,#98527),.UNSPECIFIED.,.F.,
 .F.)
B_SPLINE_CURVE_WITH_KNOTS((3,2,3),(0.349440546442563,0.359118183105584,
0.366891343973804),.UNSPECIFIED.)
CURVE()
GEOMETRIC_REPRESENTATION_ITEM()
RATIONAL_B_SPLINE_CURVE((0.994126602224868,0.996603060231143,1.,0.99727154879322,
0.995136940910679))
REPRESENTATION_ITEM('')
);
#4389=(
BOUNDED_CURVE()
B_SPLINE_CURVE(2,(#98591,#98592,#98593,#98594,#98595),.UNSPECIFIED.,.F.,
 .F.)
B_SPLINE_CURVE_WITH_KNOTS((3,2,3),(0.349440546416269,0.359118183105584,
0.366891343964705),.UNSPECIFIED.)
CURVE()
GEOMETRIC_REPRESENTATION_ITEM()
RATIONAL_B_SPLINE_CURVE((0.994126602224868,0.996603060231143,1.,0.997271548796414,
0.995136940915677))
REPRESENTATION_ITEM('')
);
#4390=(
BOUNDED_CURVE()
B_SPLINE_CURVE(2,(#98624,#98625,#98626,#98627,#98628),.UNSPECIFIED.,.F.,
 .F.)
B_SPLINE_CURVE_WITH_KNOTS((3,2,3),(0.349440546439546,0.359118183105584,
0.366891343987011),.UNSPECIFIED.)
CURVE()
GEOMETRIC_REPRESENTATION_ITEM()
RATIONAL_B_SPLINE_CURVE((0.994126602224868,0.996603060231143,1.,0.997271548788584,
0.995136940903426))
REPRESENTATION_ITEM('')
);
#4391=(
BOUNDED_CURVE()
B_SPLINE_CURVE(2,(#98657,#98658,#98659,#98660,#98661),.UNSPECIFIED.,.F.,
 .F.)
B_SPLINE_CURVE_WITH_KNOTS((3,2,3),(0.349440546419593,0.359118183105584,
0.366891343980483),.UNSPECIFIED.)
CURVE()
GEOMETRIC_REPRESENTATION_ITEM()
RATIONAL_B_SPLINE_CURVE((0.994126602224868,0.996603060231143,1.,0.997271548790876,
0.995136940907011))
REPRESENTATION_ITEM('')
);
#4392=(
BOUNDED_CURVE()
B_SPLINE_CURVE(2,(#98690,#98691,#98692,#98693,#98694),.UNSPECIFIED.,.F.,
 .F.)
B_SPLINE_CURVE_WITH_KNOTS((3,2,3),(0.349440546448491,0.359118183105584,
0.366891343972737),.UNSPECIFIED.)
CURVE()
GEOMETRIC_REPRESENTATION_ITEM()
RATIONAL_B_SPLINE_CURVE((0.994126602224868,0.996603060231143,1.,0.997271548793594,
0.995136940911266))
REPRESENTATION_ITEM('')
);
#4393=(
BOUNDED_CURVE()
B_SPLINE_CURVE(2,(#98723,#98724,#98725,#98726,#98727),.UNSPECIFIED.,.F.,
 .F.)
B_SPLINE_CURVE_WITH_KNOTS((3,2,3),(0.349440546424786,0.359118183105584,
0.366891343966157),.UNSPECIFIED.)
CURVE()
GEOMETRIC_REPRESENTATION_ITEM()
RATIONAL_B_SPLINE_CURVE((0.994126602224868,0.996603060231143,1.,0.997271548795904,
0.995136940914879))
REPRESENTATION_ITEM('')
);
#4394=(
BOUNDED_CURVE()
B_SPLINE_CURVE(2,(#98861,#98862,#98863,#98864,#98865),.UNSPECIFIED.,.F.,
 .F.)
B_SPLINE_CURVE_WITH_KNOTS((3,2,3),(0.349440546437349,0.359118183105576,
0.366891343969567),.UNSPECIFIED.)
CURVE()
GEOMETRIC_REPRESENTATION_ITEM()
RATIONAL_B_SPLINE_CURVE((0.994126602224873,0.996603060231146,1.,0.997271548794705,
0.995136940913002))
REPRESENTATION_ITEM('')
);
#4395=(
BOUNDED_CURVE()
B_SPLINE_CURVE(2,(#98894,#98895,#98896,#98897,#98898),.UNSPECIFIED.,.F.,
 .F.)
B_SPLINE_CURVE_WITH_KNOTS((3,2,3),(0.349440546418518,0.359118183105575,
0.366891343970643),.UNSPECIFIED.)
CURVE()
GEOMETRIC_REPRESENTATION_ITEM()
RATIONAL_B_SPLINE_CURVE((0.994126602224873,0.996603060231146,1.,0.997271548794326,
0.99513694091241))
REPRESENTATION_ITEM('')
);
#4396=(
BOUNDED_CURVE()
B_SPLINE_CURVE(2,(#98927,#98928,#98929,#98930,#98931),.UNSPECIFIED.,.F.,
 .F.)
B_SPLINE_CURVE_WITH_KNOTS((3,2,3),(0.349440546437857,0.359118183105575,
0.366891343981114),.UNSPECIFIED.)
CURVE()
GEOMETRIC_REPRESENTATION_ITEM()
RATIONAL_B_SPLINE_CURVE((0.994126602224873,0.996603060231146,1.,0.997271548790651,
0.99513694090666))
REPRESENTATION_ITEM('')
);
#4397=(
BOUNDED_CURVE()
B_SPLINE_CURVE(2,(#101127,#101128,#101129,#101130,#101131),
 .UNSPECIFIED.,.F.,.F.)
B_SPLINE_CURVE_WITH_KNOTS((3,2,3),(0.418312080773434,0.428571428571429,
0.430498434990588),.UNSPECIFIED.)
CURVE()
GEOMETRIC_REPRESENTATION_ITEM()
RATIONAL_B_SPLINE_CURVE((0.99383221411677,0.99639887423472,1.,0.999323602961657,
0.998683701723488))
REPRESENTATION_ITEM('')
);
#4398=(
BOUNDED_CURVE()
B_SPLINE_CURVE(2,(#101168,#101169,#101170,#101171,#101172),
 .UNSPECIFIED.,.F.,.F.)
B_SPLINE_CURVE_WITH_KNOTS((3,2,3),(0.418312080773433,0.428571428571429,
0.430498434989605),.UNSPECIFIED.)
CURVE()
GEOMETRIC_REPRESENTATION_ITEM()
RATIONAL_B_SPLINE_CURVE((0.993832214116769,0.99639887423472,1.,0.999323602962002,
0.99868370172414))
REPRESENTATION_ITEM('')
);
#4399=(
BOUNDED_CURVE()
B_SPLINE_CURVE(2,(#101209,#101210,#101211,#101212,#101213),
 .UNSPECIFIED.,.F.,.F.)
B_SPLINE_CURVE_WITH_KNOTS((3,2,3),(0.418312080773433,0.428571428571429,
0.430498434990323),.UNSPECIFIED.)
CURVE()
GEOMETRIC_REPRESENTATION_ITEM()
RATIONAL_B_SPLINE_CURVE((0.993832214116769,0.99639887423472,1.,0.99932360296175,
0.998683701723664))
REPRESENTATION_ITEM('')
);
#4400=(
BOUNDED_CURVE()
B_SPLINE_CURVE(2,(#101250,#101251,#101252,#101253,#101254),
 .UNSPECIFIED.,.F.,.F.)
B_SPLINE_CURVE_WITH_KNOTS((3,2,3),(0.418312080773433,0.428571428571429,
0.430498434985288),.UNSPECIFIED.)
CURVE()
GEOMETRIC_REPRESENTATION_ITEM()
RATIONAL_B_SPLINE_CURVE((0.993832214116769,0.99639887423472,1.,0.999323602963517,
0.998683701727008))
REPRESENTATION_ITEM('')
);
#4401=(
BOUNDED_CURVE()
B_SPLINE_CURVE(2,(#101291,#101292,#101293,#101294,#101295),
 .UNSPECIFIED.,.F.,.F.)
B_SPLINE_CURVE_WITH_KNOTS((3,2,3),(0.418312080773434,0.428571428571429,
0.430498434986539),.UNSPECIFIED.)
CURVE()
GEOMETRIC_REPRESENTATION_ITEM()
RATIONAL_B_SPLINE_CURVE((0.99383221411677,0.99639887423472,1.,0.999323602963078,
0.998683701726177))
REPRESENTATION_ITEM('')
);
#4402=(
BOUNDED_CURVE()
B_SPLINE_CURVE(2,(#101332,#101333,#101334,#101335,#101336),
 .UNSPECIFIED.,.F.,.F.)
B_SPLINE_CURVE_WITH_KNOTS((3,2,3),(0.418312080773434,0.428571428571429,
0.430498434990513),.UNSPECIFIED.)
CURVE()
GEOMETRIC_REPRESENTATION_ITEM()
RATIONAL_B_SPLINE_CURVE((0.99383221411677,0.996398874234721,1.,0.999323602961683,
0.998683701723538))
REPRESENTATION_ITEM('')
);
#4403=(
BOUNDED_CURVE()
B_SPLINE_CURVE(2,(#101373,#101374,#101375,#101376,#101377),
 .UNSPECIFIED.,.F.,.F.)
B_SPLINE_CURVE_WITH_KNOTS((3,2,3),(0.418312080773434,0.428571428571429,
0.430498434985252),.UNSPECIFIED.)
CURVE()
GEOMETRIC_REPRESENTATION_ITEM()
RATIONAL_B_SPLINE_CURVE((0.99383221411677,0.99639887423472,1.,0.99932360296353,
0.998683701727032))
REPRESENTATION_ITEM('')
);
#4404=(
BOUNDED_CURVE()
B_SPLINE_CURVE(2,(#101414,#101415,#101416,#101417,#101418),
 .UNSPECIFIED.,.F.,.F.)
B_SPLINE_CURVE_WITH_KNOTS((3,2,3),(0.418312080773434,0.428571428571429,
0.430498434984252),.UNSPECIFIED.)
CURVE()
GEOMETRIC_REPRESENTATION_ITEM()
RATIONAL_B_SPLINE_CURVE((0.99383221411677,0.996398874234721,1.,0.999323602963881,
0.998683701727696))
REPRESENTATION_ITEM('')
);
#4405=(
BOUNDED_CURVE()
B_SPLINE_CURVE(2,(#101455,#101456,#101457,#101458,#101459),
 .UNSPECIFIED.,.F.,.F.)
B_SPLINE_CURVE_WITH_KNOTS((3,2,3),(0.418312080773434,0.428571428571429,
0.430498434987172),.UNSPECIFIED.)
CURVE()
GEOMETRIC_REPRESENTATION_ITEM()
RATIONAL_B_SPLINE_CURVE((0.99383221411677,0.996398874234721,1.,0.999323602962856,
0.998683701725757))
REPRESENTATION_ITEM('')
);
#4406=(
BOUNDED_CURVE()
B_SPLINE_CURVE(2,(#101496,#101497,#101498,#101499,#101500),
 .UNSPECIFIED.,.F.,.F.)
B_SPLINE_CURVE_WITH_KNOTS((3,2,3),(0.418312080773434,0.428571428571429,
0.43049843498926),.UNSPECIFIED.)
CURVE()
GEOMETRIC_REPRESENTATION_ITEM()
RATIONAL_B_SPLINE_CURVE((0.99383221411677,0.996398874234721,1.,0.999323602962123,
0.99868370172437))
REPRESENTATION_ITEM('')
);
#4407=(
BOUNDED_CURVE()
B_SPLINE_CURVE(2,(#101537,#101538,#101539,#101540,#101541),
 .UNSPECIFIED.,.F.,.F.)
B_SPLINE_CURVE_WITH_KNOTS((3,2,3),(0.418312080773434,0.428571428571429,
0.43049843498763),.UNSPECIFIED.)
CURVE()
GEOMETRIC_REPRESENTATION_ITEM()
RATIONAL_B_SPLINE_CURVE((0.99383221411677,0.99639887423472,1.,0.999323602962695,
0.998683701725452))
REPRESENTATION_ITEM('')
);
#4408=(
BOUNDED_CURVE()
B_SPLINE_CURVE(2,(#101578,#101579,#101580,#101581,#101582),
 .UNSPECIFIED.,.F.,.F.)
B_SPLINE_CURVE_WITH_KNOTS((3,2,3),(0.418312080773434,0.428571428571429,
0.430498434990192),.UNSPECIFIED.)
CURVE()
GEOMETRIC_REPRESENTATION_ITEM()
RATIONAL_B_SPLINE_CURVE((0.99383221411677,0.996398874234721,1.,0.999323602961796,
0.998683701723751))
REPRESENTATION_ITEM('')
);
#4409=(
BOUNDED_CURVE()
B_SPLINE_CURVE(2,(#101619,#101620,#101621,#101622,#101623),
 .UNSPECIFIED.,.F.,.F.)
B_SPLINE_CURVE_WITH_KNOTS((3,2,3),(0.418312080773434,0.428571428571429,
0.430498434989795),.UNSPECIFIED.)
CURVE()
GEOMETRIC_REPRESENTATION_ITEM()
RATIONAL_B_SPLINE_CURVE((0.99383221411677,0.996398874234721,1.,0.999323602961935,
0.998683701724015))
REPRESENTATION_ITEM('')
);
#4410=(
BOUNDED_CURVE()
B_SPLINE_CURVE(2,(#101660,#101661,#101662,#101663,#101664),
 .UNSPECIFIED.,.F.,.F.)
B_SPLINE_CURVE_WITH_KNOTS((3,2,3),(0.418312080773434,0.428571428571429,
0.430498434986927),.UNSPECIFIED.)
CURVE()
GEOMETRIC_REPRESENTATION_ITEM()
RATIONAL_B_SPLINE_CURVE((0.99383221411677,0.99639887423472,1.,0.999323602962942,
0.998683701725919))
REPRESENTATION_ITEM('')
);
#4411=(
BOUNDED_CURVE()
B_SPLINE_CURVE(2,(#101701,#101702,#101703,#101704,#101705),
 .UNSPECIFIED.,.F.,.F.)
B_SPLINE_CURVE_WITH_KNOTS((3,2,3),(0.418312080773433,0.428571428571429,
0.430498434988302),.UNSPECIFIED.)
CURVE()
GEOMETRIC_REPRESENTATION_ITEM()
RATIONAL_B_SPLINE_CURVE((0.99383221411677,0.99639887423472,1.,0.999323602962459,
0.998683701725006))
REPRESENTATION_ITEM('')
);
#4412=(
BOUNDED_CURVE()
B_SPLINE_CURVE(2,(#101742,#101743,#101744,#101745,#101746),
 .UNSPECIFIED.,.F.,.F.)
B_SPLINE_CURVE_WITH_KNOTS((3,2,3),(0.418312080773434,0.428571428571429,
0.430498434993456),.UNSPECIFIED.)
CURVE()
GEOMETRIC_REPRESENTATION_ITEM()
RATIONAL_B_SPLINE_CURVE((0.99383221411677,0.996398874234721,1.,0.99932360296065,
0.998683701721583))
REPRESENTATION_ITEM('')
);
#4413=(
BOUNDED_CURVE()
B_SPLINE_CURVE(2,(#101783,#101784,#101785,#101786,#101787),
 .UNSPECIFIED.,.F.,.F.)
B_SPLINE_CURVE_WITH_KNOTS((3,2,3),(0.418312080773434,0.428571428571429,
0.430498434990347),.UNSPECIFIED.)
CURVE()
GEOMETRIC_REPRESENTATION_ITEM()
RATIONAL_B_SPLINE_CURVE((0.99383221411677,0.996398874234721,1.,0.999323602961742,
0.998683701723649))
REPRESENTATION_ITEM('')
);
#4414=(
BOUNDED_CURVE()
B_SPLINE_CURVE(2,(#101824,#101825,#101826,#101827,#101828),
 .UNSPECIFIED.,.F.,.F.)
B_SPLINE_CURVE_WITH_KNOTS((3,2,3),(0.418312080773434,0.428571428571429,
0.430498434990058),.UNSPECIFIED.)
CURVE()
GEOMETRIC_REPRESENTATION_ITEM()
RATIONAL_B_SPLINE_CURVE((0.99383221411677,0.996398874234721,1.,0.999323602961843,
0.99868370172384))
REPRESENTATION_ITEM('')
);
#4415=(
BOUNDED_CURVE()
B_SPLINE_CURVE(2,(#101865,#101866,#101867,#101868,#101869),
 .UNSPECIFIED.,.F.,.F.)
B_SPLINE_CURVE_WITH_KNOTS((3,2,3),(0.418312080773434,0.428571428571429,
0.43049843498816),.UNSPECIFIED.)
CURVE()
GEOMETRIC_REPRESENTATION_ITEM()
RATIONAL_B_SPLINE_CURVE((0.99383221411677,0.996398874234721,1.,0.999323602962509,
0.998683701725101))
REPRESENTATION_ITEM('')
);
#4416=(
BOUNDED_CURVE()
B_SPLINE_CURVE(2,(#101906,#101907,#101908,#101909,#101910),
 .UNSPECIFIED.,.F.,.F.)
B_SPLINE_CURVE_WITH_KNOTS((3,2,3),(0.418312080773434,0.428571428571429,
0.430498434988028),.UNSPECIFIED.)
CURVE()
GEOMETRIC_REPRESENTATION_ITEM()
RATIONAL_B_SPLINE_CURVE((0.99383221411677,0.996398874234721,1.,0.999323602962556,
0.998683701725188))
REPRESENTATION_ITEM('')
);
#4417=(
BOUNDED_CURVE()
B_SPLINE_CURVE(2,(#101947,#101948,#101949,#101950,#101951),
 .UNSPECIFIED.,.F.,.F.)
B_SPLINE_CURVE_WITH_KNOTS((3,2,3),(0.418312080773434,0.428571428571429,
0.430498434991989),.UNSPECIFIED.)
CURVE()
GEOMETRIC_REPRESENTATION_ITEM()
RATIONAL_B_SPLINE_CURVE((0.99383221411677,0.996398874234721,1.,0.999323602961165,
0.998683701722558))
REPRESENTATION_ITEM('')
);
#4418=(
BOUNDED_CURVE()
B_SPLINE_CURVE(2,(#102016,#102017,#102018,#102019,#102020),
 .UNSPECIFIED.,.F.,.F.)
B_SPLINE_CURVE_WITH_KNOTS((3,2,3),(0.418312080773434,0.428571428571429,
0.430498434989518),.UNSPECIFIED.)
CURVE()
GEOMETRIC_REPRESENTATION_ITEM()
RATIONAL_B_SPLINE_CURVE((0.99383221411677,0.99639887423472,1.,0.999323602962032,
0.998683701724199))
REPRESENTATION_ITEM('')
);
#4419=(
BOUNDED_CURVE()
B_SPLINE_CURVE(2,(#102057,#102058,#102059,#102060,#102061),
 .UNSPECIFIED.,.F.,.F.)
B_SPLINE_CURVE_WITH_KNOTS((3,2,3),(0.418312080773434,0.428571428571429,
0.430498434994573),.UNSPECIFIED.)
CURVE()
GEOMETRIC_REPRESENTATION_ITEM()
RATIONAL_B_SPLINE_CURVE((0.99383221411677,0.996398874234721,1.,0.999323602960258,
0.998683701720842))
REPRESENTATION_ITEM('')
);
#4420=(
BOUNDED_CURVE()
B_SPLINE_CURVE(2,(#102098,#102099,#102100,#102101,#102102),
 .UNSPECIFIED.,.F.,.F.)
B_SPLINE_CURVE_WITH_KNOTS((3,2,3),(0.418312080773434,0.428571428571429,
0.430498434990144),.UNSPECIFIED.)
CURVE()
GEOMETRIC_REPRESENTATION_ITEM()
RATIONAL_B_SPLINE_CURVE((0.99383221411677,0.996398874234721,1.,0.999323602961813,
0.998683701723783))
REPRESENTATION_ITEM('')
);
#4421=(
BOUNDED_CURVE()
B_SPLINE_CURVE(2,(#102139,#102140,#102141,#102142,#102143),
 .UNSPECIFIED.,.F.,.F.)
B_SPLINE_CURVE_WITH_KNOTS((3,2,3),(0.418312080773434,0.428571428571429,
0.430498434989385),.UNSPECIFIED.)
CURVE()
GEOMETRIC_REPRESENTATION_ITEM()
RATIONAL_B_SPLINE_CURVE((0.99383221411677,0.99639887423472,1.,0.999323602962079,
0.998683701724287))
REPRESENTATION_ITEM('')
);
#4422=(
BOUNDED_CURVE()
B_SPLINE_CURVE(2,(#102180,#102181,#102182,#102183,#102184),
 .UNSPECIFIED.,.F.,.F.)
B_SPLINE_CURVE_WITH_KNOTS((3,2,3),(0.418312080773434,0.428571428571429,
0.430498434988894),.UNSPECIFIED.)
CURVE()
GEOMETRIC_REPRESENTATION_ITEM()
RATIONAL_B_SPLINE_CURVE((0.99383221411677,0.996398874234721,1.,0.999323602962252,
0.998683701724613))
REPRESENTATION_ITEM('')
);
#4423=(
BOUNDED_CURVE()
B_SPLINE_CURVE(2,(#102221,#102222,#102223,#102224,#102225),
 .UNSPECIFIED.,.F.,.F.)
B_SPLINE_CURVE_WITH_KNOTS((3,2,3),(0.418312080773434,0.428571428571429,
0.430498434988829),.UNSPECIFIED.)
CURVE()
GEOMETRIC_REPRESENTATION_ITEM()
RATIONAL_B_SPLINE_CURVE((0.99383221411677,0.99639887423472,1.,0.999323602962274,
0.998683701724656))
REPRESENTATION_ITEM('')
);
#4424=(
BOUNDED_CURVE()
B_SPLINE_CURVE(2,(#102262,#102263,#102264,#102265,#102266),
 .UNSPECIFIED.,.F.,.F.)
B_SPLINE_CURVE_WITH_KNOTS((3,2,3),(0.418312080773434,0.428571428571429,
0.430498434986823),.UNSPECIFIED.)
CURVE()
GEOMETRIC_REPRESENTATION_ITEM()
RATIONAL_B_SPLINE_CURVE((0.99383221411677,0.99639887423472,1.,0.999323602962978,
0.998683701725988))
REPRESENTATION_ITEM('')
);
#4425=(
BOUNDED_CURVE()
B_SPLINE_CURVE(2,(#108607,#108608,#108609,#108610,#108611),
 .UNSPECIFIED.,.F.,.F.)
B_SPLINE_CURVE_WITH_KNOTS((3,2,3),(0.280433083113984,0.285714285714286,
0.297856505249078),.UNSPECIFIED.)
CURVE()
GEOMETRIC_REPRESENTATION_ITEM()
RATIONAL_B_SPLINE_CURVE((0.996566619267863,0.998146249162903,1.,0.995737968877225,
0.992924952246043))
REPRESENTATION_ITEM('')
);
#4426=(
BOUNDED_CURVE()
B_SPLINE_CURVE(2,(#123888,#123889,#123890,#123891,#123892),
 .UNSPECIFIED.,.F.,.F.)
B_SPLINE_CURVE_WITH_KNOTS((3,2,3),(0.211502584834065,0.214285714285714,
0.228883374865518),.UNSPECIFIED.)
CURVE()
GEOMETRIC_REPRESENTATION_ITEM()
RATIONAL_B_SPLINE_CURVE((0.998122319569323,0.999023095875705,1.,0.994876086408045,
0.991846493056848))
REPRESENTATION_ITEM('')
);
#4427=(
BOUNDED_CURVE()
B_SPLINE_CURVE(2,(#123929,#123930,#123931,#123932,#123933),
 .UNSPECIFIED.,.F.,.F.)
B_SPLINE_CURVE_WITH_KNOTS((3,2,3),(0.211502584834065,0.214285714285714,
0.228883374853505),.UNSPECIFIED.)
CURVE()
GEOMETRIC_REPRESENTATION_ITEM()
RATIONAL_B_SPLINE_CURVE((0.998122319569323,0.999023095875705,1.,0.994876086412262,
0.991846493061834))
REPRESENTATION_ITEM('')
);
#4428=(
BOUNDED_CURVE()
B_SPLINE_CURVE(2,(#124062,#124063,#124064,#124065,#124066),
 .UNSPECIFIED.,.F.,.F.)
B_SPLINE_CURVE_WITH_KNOTS((3,2,3),(0.211502584834065,0.214285714285714,
0.228883374851655),.UNSPECIFIED.)
CURVE()
GEOMETRIC_REPRESENTATION_ITEM()
RATIONAL_B_SPLINE_CURVE((0.998122319569323,0.999023095875705,1.,0.994876086412911,
0.991846493062601))
REPRESENTATION_ITEM('')
);
#4429=(
BOUNDED_CURVE()
B_SPLINE_CURVE(2,(#124103,#124104,#124105,#124106,#124107),
 .UNSPECIFIED.,.F.,.F.)
B_SPLINE_CURVE_WITH_KNOTS((3,2,3),(0.211502584834065,0.214285714285714,
0.228883374862862),.UNSPECIFIED.)
CURVE()
GEOMETRIC_REPRESENTATION_ITEM()
RATIONAL_B_SPLINE_CURVE((0.998122319569323,0.999023095875705,1.,0.994876086408978,
0.99184649305795))
REPRESENTATION_ITEM('')
);
#4430=(
BOUNDED_CURVE()
B_SPLINE_CURVE(2,(#124144,#124145,#124146,#124147,#124148),
 .UNSPECIFIED.,.F.,.F.)
B_SPLINE_CURVE_WITH_KNOTS((3,2,3),(0.211502584834064,0.214285714285714,
0.228883374863024),.UNSPECIFIED.)
CURVE()
GEOMETRIC_REPRESENTATION_ITEM()
RATIONAL_B_SPLINE_CURVE((0.998122319569322,0.999023095875704,1.,0.994876086408921,
0.991846493057883))
REPRESENTATION_ITEM('')
);
#4431=(
BOUNDED_CURVE()
B_SPLINE_CURVE(2,(#124185,#124186,#124187,#124188,#124189),
 .UNSPECIFIED.,.F.,.F.)
B_SPLINE_CURVE_WITH_KNOTS((3,2,3),(0.211502584834064,0.214285714285714,
0.228883374860444),.UNSPECIFIED.)
CURVE()
GEOMETRIC_REPRESENTATION_ITEM()
RATIONAL_B_SPLINE_CURVE((0.998122319569322,0.999023095875704,1.,0.994876086409827,
0.991846493058953))
REPRESENTATION_ITEM('')
);
#4432=(
BOUNDED_CURVE()
B_SPLINE_CURVE(2,(#124272,#124273,#124274,#124275,#124276),
 .UNSPECIFIED.,.F.,.F.)
B_SPLINE_CURVE_WITH_KNOTS((3,2,3),(0.211502584834064,0.214285714285714,
0.228883374854438),.UNSPECIFIED.)
CURVE()
GEOMETRIC_REPRESENTATION_ITEM()
RATIONAL_B_SPLINE_CURVE((0.998122319569322,0.999023095875704,1.,0.994876086411935,
0.991846493061446))
REPRESENTATION_ITEM('')
);
#4433=(
BOUNDED_CURVE()
B_SPLINE_CURVE(2,(#124313,#124314,#124315,#124316,#124317),
 .UNSPECIFIED.,.F.,.F.)
B_SPLINE_CURVE_WITH_KNOTS((3,2,3),(0.211502584834064,0.214285714285714,
0.228883374860568),.UNSPECIFIED.)
CURVE()
GEOMETRIC_REPRESENTATION_ITEM()
RATIONAL_B_SPLINE_CURVE((0.998122319569322,0.999023095875704,1.,0.994876086409783,
0.991846493058902))
REPRESENTATION_ITEM('')
);
#4434=(
BOUNDED_CURVE()
B_SPLINE_CURVE(2,(#124354,#124355,#124356,#124357,#124358),
 .UNSPECIFIED.,.F.,.F.)
B_SPLINE_CURVE_WITH_KNOTS((3,2,3),(0.211502584834064,0.214285714285714,
0.228883374858422),.UNSPECIFIED.)
CURVE()
GEOMETRIC_REPRESENTATION_ITEM()
RATIONAL_B_SPLINE_CURVE((0.998122319569322,0.999023095875704,1.,0.994876086410537,
0.991846493059793))
REPRESENTATION_ITEM('')
);
#4435=(
BOUNDED_CURVE()
B_SPLINE_CURVE(2,(#124545,#124546,#124547,#124548,#124549),
 .UNSPECIFIED.,.F.,.F.)
B_SPLINE_CURVE_WITH_KNOTS((3,2,3),(0.211502584834062,0.214285714285714,
0.228883374860236),.UNSPECIFIED.)
CURVE()
GEOMETRIC_REPRESENTATION_ITEM()
RATIONAL_B_SPLINE_CURVE((0.998122319569321,0.999023095875703,1.,0.9948760864099,
0.99184649305904))
REPRESENTATION_ITEM('')
);
#4436=(
BOUNDED_CURVE()
B_SPLINE_CURVE(2,(#124586,#124587,#124588,#124589,#124590),
 .UNSPECIFIED.,.F.,.F.)
B_SPLINE_CURVE_WITH_KNOTS((3,2,3),(0.211502584834064,0.214285714285714,
0.228883374861132),.UNSPECIFIED.)
CURVE()
GEOMETRIC_REPRESENTATION_ITEM()
RATIONAL_B_SPLINE_CURVE((0.998122319569322,0.999023095875704,1.,0.994876086409585,
0.991846493058668))
REPRESENTATION_ITEM('')
);
#4437=(
BOUNDED_CURVE()
B_SPLINE_CURVE(2,(#124673,#124674,#124675,#124676,#124677),
 .UNSPECIFIED.,.F.,.F.)
B_SPLINE_CURVE_WITH_KNOTS((3,2,3),(0.211502584834063,0.214285714285714,
0.228883374855239),.UNSPECIFIED.)
CURVE()
GEOMETRIC_REPRESENTATION_ITEM()
RATIONAL_B_SPLINE_CURVE((0.998122319569321,0.999023095875704,1.,0.994876086411653,
0.991846493061113))
REPRESENTATION_ITEM('')
);
#4438=(
BOUNDED_CURVE()
B_SPLINE_CURVE(2,(#124714,#124715,#124716,#124717,#124718),
 .UNSPECIFIED.,.F.,.F.)
B_SPLINE_CURVE_WITH_KNOTS((3,2,3),(0.21150258483406,0.214285714285714,0.228883374855733),
 .UNSPECIFIED.)
CURVE()
GEOMETRIC_REPRESENTATION_ITEM()
RATIONAL_B_SPLINE_CURVE((0.998122319569319,0.999023095875703,1.,0.99487608641148,
0.991846493060909))
REPRESENTATION_ITEM('')
);
#4439=(
BOUNDED_CURVE()
B_SPLINE_CURVE(2,(#124851,#124852,#124853,#124854,#124855),
 .UNSPECIFIED.,.F.,.F.)
B_SPLINE_CURVE_WITH_KNOTS((3,2,3),(0.211502584834064,0.214285714285714,
0.22888337485822),.UNSPECIFIED.)
CURVE()
GEOMETRIC_REPRESENTATION_ITEM()
RATIONAL_B_SPLINE_CURVE((0.998122319569322,0.999023095875704,1.,0.994876086410607,
0.991846493059876))
REPRESENTATION_ITEM('')
);
#4440=(
BOUNDED_CURVE()
B_SPLINE_CURVE(2,(#124892,#124893,#124894,#124895,#124896),
 .UNSPECIFIED.,.F.,.F.)
B_SPLINE_CURVE_WITH_KNOTS((3,2,3),(0.211502584834064,0.214285714285714,
0.22888337485685),.UNSPECIFIED.)
CURVE()
GEOMETRIC_REPRESENTATION_ITEM()
RATIONAL_B_SPLINE_CURVE((0.998122319569322,0.999023095875704,1.,0.994876086411088,
0.991846493060445))
REPRESENTATION_ITEM('')
);
#4441=(
BOUNDED_CURVE()
B_SPLINE_CURVE(2,(#124933,#124934,#124935,#124936,#124937),
 .UNSPECIFIED.,.F.,.F.)
B_SPLINE_CURVE_WITH_KNOTS((3,2,3),(0.211502584834064,0.214285714285714,
0.22888337486731),.UNSPECIFIED.)
CURVE()
GEOMETRIC_REPRESENTATION_ITEM()
RATIONAL_B_SPLINE_CURVE((0.998122319569322,0.999023095875704,1.,0.994876086407416,
0.991846493056104))
REPRESENTATION_ITEM('')
);
#4442=(
BOUNDED_CURVE()
B_SPLINE_CURVE(2,(#132970,#132971,#132972,#132973,#132974),
 .UNSPECIFIED.,.F.,.F.)
B_SPLINE_CURVE_WITH_KNOTS((3,2,3),(0.492524364190421,0.5,0.504719756176228),
 .UNSPECIFIED.)
CURVE()
GEOMETRIC_REPRESENTATION_ITEM()
RATIONAL_B_SPLINE_CURVE((0.995301219176778,0.997375982834797,1.,0.998343322021369,
0.996905579294145))
REPRESENTATION_ITEM('')
);
#4443=(
BOUNDED_CURVE()
B_SPLINE_CURVE(2,(#136465,#136466,#136467,#136468,#136469),
 .UNSPECIFIED.,.F.,.F.)
B_SPLINE_CURVE_WITH_KNOTS((3,2,3),(0.556212823134607,0.571428571428571,
0.573654350147172),.UNSPECIFIED.)
CURVE()
GEOMETRIC_REPRESENTATION_ITEM()
RATIONAL_B_SPLINE_CURVE((0.991593692355873,0.994659131915763,1.,0.999218731127048,
0.998486152339761))
REPRESENTATION_ITEM('')
);
#4444=(
BOUNDED_CURVE()
B_SPLINE_CURVE(2,(#136506,#136507,#136508,#136509,#136510),
 .UNSPECIFIED.,.F.,.F.)
B_SPLINE_CURVE_WITH_KNOTS((3,2,3),(0.556212830495791,0.571428571428571,
0.573654350219911),.UNSPECIFIED.)
CURVE()
GEOMETRIC_REPRESENTATION_ITEM()
RATIONAL_B_SPLINE_CURVE((0.991593695321915,0.994659134499606,1.,0.999218731101516,
0.99848615229188))
REPRESENTATION_ITEM('')
);
#4445=(
BOUNDED_CURVE()
B_SPLINE_CURVE(2,(#136692,#136693,#136694,#136695,#136696),
 .UNSPECIFIED.,.F.,.F.)
B_SPLINE_CURVE_WITH_KNOTS((3,2,3),(0.55621283049301,0.571428571428571,0.573654350219911),
 .UNSPECIFIED.)
CURVE()
GEOMETRIC_REPRESENTATION_ITEM()
RATIONAL_B_SPLINE_CURVE((0.991593695320794,0.99465913449863,1.,0.999218731101516,
0.99848615229188))
REPRESENTATION_ITEM('')
);
#4446=(
BOUNDED_CURVE()
B_SPLINE_CURVE(2,(#136783,#136784,#136785,#136786,#136787),
 .UNSPECIFIED.,.F.,.F.)
B_SPLINE_CURVE_WITH_KNOTS((3,2,3),(0.556212830496133,0.571428571428571,
0.573654350219911),.UNSPECIFIED.)
CURVE()
GEOMETRIC_REPRESENTATION_ITEM()
RATIONAL_B_SPLINE_CURVE((0.991593695322053,0.994659134499726,1.,0.999218731101516,
0.99848615229188))
REPRESENTATION_ITEM('')
);
#4447=(
BOUNDED_CURVE()
B_SPLINE_CURVE(2,(#137072,#137073,#137074,#137075,#137076),
 .UNSPECIFIED.,.F.,.F.)
B_SPLINE_CURVE_WITH_KNOTS((3,2,3),(0.556212830497704,0.571428571428571,
0.573654350219911),.UNSPECIFIED.)
CURVE()
GEOMETRIC_REPRESENTATION_ITEM()
RATIONAL_B_SPLINE_CURVE((0.991593695322685,0.994659134500278,1.,0.999218731101516,
0.99848615229188))
REPRESENTATION_ITEM('')
);
#4448=(
BOUNDED_CURVE()
B_SPLINE_CURVE(2,(#137113,#137114,#137115,#137116,#137117),
 .UNSPECIFIED.,.F.,.F.)
B_SPLINE_CURVE_WITH_KNOTS((3,2,3),(0.556212830496801,0.571428571428571,
0.573654350219911),.UNSPECIFIED.)
CURVE()
GEOMETRIC_REPRESENTATION_ITEM()
RATIONAL_B_SPLINE_CURVE((0.991593695322322,0.994659134499961,1.,0.999218731101516,
0.99848615229188))
REPRESENTATION_ITEM('')
);
#4449=(
BOUNDED_CURVE()
B_SPLINE_CURVE(2,(#137204,#137205,#137206,#137207,#137208),
 .UNSPECIFIED.,.F.,.F.)
B_SPLINE_CURVE_WITH_KNOTS((3,2,3),(0.556212830500266,0.571428571428571,
0.57365435021991),.UNSPECIFIED.)
CURVE()
GEOMETRIC_REPRESENTATION_ITEM()
RATIONAL_B_SPLINE_CURVE((0.991593695323718,0.994659134501177,1.,0.999218731101516,
0.99848615229188))
REPRESENTATION_ITEM('')
);
#4450=(
BOUNDED_CURVE()
B_SPLINE_CURVE(2,(#146696,#146697,#146698,#146699,#146700),
 .UNSPECIFIED.,.F.,.F.)
B_SPLINE_CURVE_WITH_KNOTS((3,2,3),(0.556108173865715,0.558333952657054,
0.573549700888524),.UNSPECIFIED.)
CURVE()
GEOMETRIC_REPRESENTATION_ITEM()
RATIONAL_B_SPLINE_CURVE((0.99848615229188,0.999218731101516,1.,0.994659131937698,
0.991593692381054))
REPRESENTATION_ITEM('')
);
#4451=(
BOUNDED_CURVE()
B_SPLINE_CURVE(2,(#146787,#146788,#146789,#146790,#146791),
 .UNSPECIFIED.,.F.,.F.)
B_SPLINE_CURVE_WITH_KNOTS((3,2,3),(0.556108173865715,0.558333952657055,
0.573549700890172),.UNSPECIFIED.)
CURVE()
GEOMETRIC_REPRESENTATION_ITEM()
RATIONAL_B_SPLINE_CURVE((0.99848615229188,0.999218731101516,1.,0.994659131937121,
0.991593692380391))
REPRESENTATION_ITEM('')
);
#4452=(
BOUNDED_CURVE()
B_SPLINE_CURVE(2,(#146828,#146829,#146830,#146831,#146832),
 .UNSPECIFIED.,.F.,.F.)
B_SPLINE_CURVE_WITH_KNOTS((3,2,3),(0.556108173865716,0.558333952657056,
0.573549700892252),.UNSPECIFIED.)
CURVE()
GEOMETRIC_REPRESENTATION_ITEM()
RATIONAL_B_SPLINE_CURVE((0.99848615229188,0.999218731101516,1.,0.994659131936391,
0.991593692379553))
REPRESENTATION_ITEM('')
);
#4453=(
BOUNDED_CURVE()
B_SPLINE_CURVE(2,(#147117,#147118,#147119,#147120,#147121),
 .UNSPECIFIED.,.F.,.F.)
B_SPLINE_CURVE_WITH_KNOTS((3,2,3),(0.556108173865716,0.558333952657056,
0.57354970089628),.UNSPECIFIED.)
CURVE()
GEOMETRIC_REPRESENTATION_ITEM()
RATIONAL_B_SPLINE_CURVE((0.99848615229188,0.999218731101516,1.,0.994659131934977,
0.99159369237793))
REPRESENTATION_ITEM('')
);
#4454=(
BOUNDED_CURVE()
B_SPLINE_CURVE(2,(#147208,#147209,#147210,#147211,#147212),
 .UNSPECIFIED.,.F.,.F.)
B_SPLINE_CURVE_WITH_KNOTS((3,2,3),(0.556108173865715,0.558333952657055,
0.573549700896557),.UNSPECIFIED.)
CURVE()
GEOMETRIC_REPRESENTATION_ITEM()
RATIONAL_B_SPLINE_CURVE((0.99848615229188,0.999218731101516,1.,0.994659131934879,
0.991593692377818))
REPRESENTATION_ITEM('')
);
#4455=(
BOUNDED_CURVE()
B_SPLINE_CURVE(2,(#147394,#147395,#147396,#147397,#147398),
 .UNSPECIFIED.,.F.,.F.)
B_SPLINE_CURVE_WITH_KNOTS((3,2,3),(0.556108173865716,0.558333952657056,
0.573549700888435),.UNSPECIFIED.)
CURVE()
GEOMETRIC_REPRESENTATION_ITEM()
RATIONAL_B_SPLINE_CURVE((0.99848615229188,0.999218731101516,1.,0.99465913193773,
0.99159369238109))
REPRESENTATION_ITEM('')
);
#4456=(
BOUNDED_CURVE()
B_SPLINE_CURVE(2,(#158499,#158500,#158501,#158502,#158503),
 .UNSPECIFIED.,.F.,.F.)
B_SPLINE_CURVE_WITH_KNOTS((3,2,3),(-0.0736543716039549,-0.0714285714285714,
-0.0665682420727563),.UNSPECIFIED.)
CURVE()
GEOMETRIC_REPRESENTATION_ITEM()
RATIONAL_B_SPLINE_CURVE((0.998486138215465,0.999218723595519,1.,0.99829397953792,
0.996820130073177))
REPRESENTATION_ITEM('')
);
#4457=(
BOUNDED_CURVE()
B_SPLINE_CURVE(2,(#167647,#167648,#167649,#167650,#167651),
 .UNSPECIFIED.,.F.,.F.)
B_SPLINE_CURVE_WITH_KNOTS((3,2,3),(-0.0736543503731481,-0.0714285714285714,
-0.0665682420727563),.UNSPECIFIED.)
CURVE()
GEOMETRIC_REPRESENTATION_ITEM()
RATIONAL_B_SPLINE_CURVE((0.998486152191009,0.999218731047729,1.,0.99829397953792,
0.996820130073177))
REPRESENTATION_ITEM('')
);
#4458=(
BOUNDED_CURVE()
B_SPLINE_CURVE(3,(#168924,#168925,#168926,#168927,#168928,#168929,#168930,
#168931,#168932,#168933,#168934,#168935,#168936,#168937,#168938,#168939,
#168940,#168941,#168942,#168943,#168944,#168945,#168946,#168947,#168948,
#168949,#168950,#168951,#168952,#168953,#168954,#168955,#168956,#168957,
#168958,#168959,#168960,#168961,#168962,#168963,#168964,#168965,#168966,
#168967,#168968,#168969,#168970,#168971,#168972,#168973,#168974,#168975,
#168976,#168977,#168978,#168979,#168980,#168981,#168982,#168983,#168984,
#168985,#168986,#168987,#168988,#168989),.UNSPECIFIED.,.F.,.F.)
B_SPLINE_CURVE_WITH_KNOTS((4,2,2,2,2,2,2,2,2,2,2,2,2,2,2,2,2,2,2,2,2,2,
2,2,2,2,2,2,2,2,2,2,4),(0.,0.000426248299516627,0.000920386532912638,0.00190866299971401,
0.00981487473411692,0.0177210864685195,0.0187093629353212,0.0196976394021223,
0.0216741923357257,0.0256272982029221,0.0572521451405331,0.120501839015745,
0.183751532890957,0.24700122676617,0.310250920641382,0.373500614516604,
0.500000002267029,0.626499390017453,0.689749083892675,0.752998777767887,
0.816248471643099,0.879498165518312,0.942747859393524,0.974372706331135,
0.978325812198331,0.980302365131934,0.981290641598736,0.982278918065537,
0.99018512979994,0.998091341534343,0.999079618001144,0.99957375623454,1.),
 .UNSPECIFIED.)
CURVE()
GEOMETRIC_REPRESENTATION_ITEM()
RATIONAL_B_SPLINE_CURVE((0.999999893495044,0.999999893494474,0.999999893492739,
0.999999893490038,0.999999893488586,0.999999893484228,0.999999893481318,
0.999999893455095,0.999999893431516,0.999999893383822,0.999999893359708,
0.999999893332278,0.999999893329226,0.999999893323113,0.999999893319945,
0.999999893311484,0.999999893305855,0.999999893289002,0.999999893277814,
0.999999893177536,0.999999893091374,0.999999892841696,0.999999892686943,
0.99999989240129,0.999999892270563,0.999999892032618,0.999999891925514,
0.999999891735356,0.999999891652404,0.999999891509953,0.999999891450451,
0.999999891307925,0.999999891260461,0.999999891260407,0.999999891307959,
0.999999891450708,0.999999891510284,0.999999891652815,0.999999891735774,
0.999999891925809,0.999999892032782,0.999999892270268,0.999999892400809,
0.99999989268632,0.999999892841159,0.999999893091054,0.999999893177288,
0.999999893277646,0.999999893288843,0.999999893305709,0.999999893311343,
0.999999893319811,0.99999989332297,0.999999893329088,0.999999893332142,
0.999999893359596,0.999999893383731,0.999999893431464,0.999999893455062,
0.999999893481307,0.999999893484219,0.99999989348858,0.999999893490033,
0.999999893492737,0.999999893494474,0.999999893495044))
REPRESENTATION_ITEM('')
);
#4459=CYLINDRICAL_SURFACE('',#71533,3.25);
#4460=CYLINDRICAL_SURFACE('',#71537,7.);
#4461=CYLINDRICAL_SURFACE('',#71540,6.125);
#4462=CYLINDRICAL_SURFACE('',#71611,7.5000000000019);
#4463=CYLINDRICAL_SURFACE('',#71616,7.50000000000249);
#4464=CYLINDRICAL_SURFACE('',#71623,7.49999999999896);
#4465=CYLINDRICAL_SURFACE('',#71626,7.50000000000045);
#4466=CYLINDRICAL_SURFACE('',#71633,7.49999999999779);
#4467=CYLINDRICAL_SURFACE('',#71635,7.50000000000013);
#4468=CYLINDRICAL_SURFACE('',#71638,7.50000000000107);
#4469=CYLINDRICAL_SURFACE('',#71641,7.5);
#4470=CYLINDRICAL_SURFACE('',#71644,7.50000000000042);
#4471=CYLINDRICAL_SURFACE('',#71647,7.49999999999967);
#4472=CYLINDRICAL_SURFACE('',#71649,7.50000000000012);
#4473=CYLINDRICAL_SURFACE('',#71651,7.49999999999917);
#4474=CYLINDRICAL_SURFACE('',#71653,7.49999999999998);
#4475=CYLINDRICAL_SURFACE('',#71656,7.49999999999897);
#4476=CYLINDRICAL_SURFACE('',#71659,7.50000000000024);
#4477=CYLINDRICAL_SURFACE('',#71661,7.5000000000015);
#4478=CYLINDRICAL_SURFACE('',#71664,7.49999999999738);
#4479=CYLINDRICAL_SURFACE('',#71666,7.50000000000006);
#4480=CYLINDRICAL_SURFACE('',#71668,7.49999999999942);
#4481=CYLINDRICAL_SURFACE('',#71671,7.50000000000151);
#4482=CYLINDRICAL_SURFACE('',#71673,7.50000000000047);
#4483=CYLINDRICAL_SURFACE('',#71676,7.50000000000012);
#4484=CYLINDRICAL_SURFACE('',#71678,7.50000000000129);
#4485=CYLINDRICAL_SURFACE('',#71681,7.49999999999964);
#4486=CYLINDRICAL_SURFACE('',#71683,7.50000000000003);
#4487=CYLINDRICAL_SURFACE('',#71685,7.50000000000029);
#4488=CYLINDRICAL_SURFACE('',#71687,7.50000000000047);
#4489=CYLINDRICAL_SURFACE('',#71688,7.49999999999994);
#4490=CYLINDRICAL_SURFACE('',#71691,7.50000000000153);
#4491=CYLINDRICAL_SURFACE('',#71697,7.49999999999978);
#4492=CYLINDRICAL_SURFACE('',#71703,7.50000000000036);
#4493=CYLINDRICAL_SURFACE('',#71709,7.49999999999827);
#4494=CYLINDRICAL_SURFACE('',#71715,7.50000000000059);
#4495=CYLINDRICAL_SURFACE('',#71721,7.50000000000016);
#4496=CYLINDRICAL_SURFACE('',#71727,7.50000000000111);
#4497=CYLINDRICAL_SURFACE('',#71735,7.50000000000021);
#4498=CYLINDRICAL_SURFACE('',#71741,7.49999999999943);
#4499=CYLINDRICAL_SURFACE('',#71747,7.49999999999932);
#4500=CYLINDRICAL_SURFACE('',#71753,7.50000000000055);
#4501=CYLINDRICAL_SURFACE('',#71759,7.50000000000016);
#4502=CYLINDRICAL_SURFACE('',#71765,7.49999999999825);
#4503=CYLINDRICAL_SURFACE('',#71771,7.49999999999844);
#4504=CYLINDRICAL_SURFACE('',#71777,7.49999999999911);
#4505=CYLINDRICAL_SURFACE('',#71783,7.50000000000129);
#4506=CYLINDRICAL_SURFACE('',#71789,7.49999999999985);
#4507=CYLINDRICAL_SURFACE('',#71795,7.49999999999989);
#4508=CYLINDRICAL_SURFACE('',#71801,7.49999999999936);
#4509=CYLINDRICAL_SURFACE('',#71807,7.5000000000015);
#4510=CYLINDRICAL_SURFACE('',#71813,7.49999999999907);
#4511=CYLINDRICAL_SURFACE('',#71819,7.49999999999943);
#4512=CYLINDRICAL_SURFACE('',#71825,7.49999999999939);
#4513=CYLINDRICAL_SURFACE('',#71831,7.49999999999972);
#4514=CYLINDRICAL_SURFACE('',#71839,7.49999999999887);
#4515=CYLINDRICAL_SURFACE('',#71843,7.50000000000122);
#4516=CYLINDRICAL_SURFACE('',#71849,7.49999999999991);
#4517=CYLINDRICAL_SURFACE('',#71855,7.49999999999911);
#4518=CYLINDRICAL_SURFACE('',#71859,7.49999999999879);
#4519=CYLINDRICAL_SURFACE('',#71866,7.49999999999953);
#4520=CYLINDRICAL_SURFACE('',#71871,7.49999999999775);
#4521=CYLINDRICAL_SURFACE('',#71876,7.50000000000054);
#4522=CYLINDRICAL_SURFACE('',#71881,7.49999999999899);
#4523=CYLINDRICAL_SURFACE('',#71886,7.49999999999925);
#4524=CYLINDRICAL_SURFACE('',#71891,7.49999999999932);
#4525=CYLINDRICAL_SURFACE('',#71896,7.50000000000172);
#4526=CYLINDRICAL_SURFACE('',#71901,7.50000000000026);
#4527=CYLINDRICAL_SURFACE('',#71906,7.50000000000139);
#4528=CYLINDRICAL_SURFACE('',#71911,7.50000000000019);
#4529=CYLINDRICAL_SURFACE('',#71916,7.49999999999962);
#4530=CYLINDRICAL_SURFACE('',#71921,7.49999999999975);
#4531=CYLINDRICAL_SURFACE('',#71926,7.49999999999885);
#4532=CYLINDRICAL_SURFACE('',#71931,7.50000000000064);
#4533=CYLINDRICAL_SURFACE('',#71936,7.49999999999907);
#4534=CYLINDRICAL_SURFACE('',#71941,7.49999999999931);
#4535=CYLINDRICAL_SURFACE('',#71946,7.5000000000005);
#4536=CYLINDRICAL_SURFACE('',#71951,7.50000000000094);
#4537=CYLINDRICAL_SURFACE('',#71956,7.50000000000172);
#4538=CYLINDRICAL_SURFACE('',#71961,7.50000000000123);
#4539=CYLINDRICAL_SURFACE('',#71966,7.50000000000139);
#4540=CYLINDRICAL_SURFACE('',#71971,7.49999999999962);
#4541=CYLINDRICAL_SURFACE('',#71976,7.49999999999967);
#4542=CYLINDRICAL_SURFACE('',#71981,7.50000000000006);
#4543=CYLINDRICAL_SURFACE('',#71986,7.49999999999917);
#4544=CYLINDRICAL_SURFACE('',#71991,7.49999999999949);
#4545=CYLINDRICAL_SURFACE('',#71996,7.49999999999865);
#4546=CYLINDRICAL_SURFACE('',#71999,7.50000000000002);
#4547=CYLINDRICAL_SURFACE('',#72091,7.49999999999856);
#4548=CYLINDRICAL_SURFACE('',#72094,7.49999999999898);
#4549=CYLINDRICAL_SURFACE('',#72097,7.49999999999979);
#4550=CYLINDRICAL_SURFACE('',#72100,7.49999999999998);
#4551=CYLINDRICAL_SURFACE('',#72103,7.49999999999804);
#4552=CYLINDRICAL_SURFACE('',#72106,7.50000000000217);
#4553=CYLINDRICAL_SURFACE('',#72109,7.50000000000047);
#4554=CYLINDRICAL_SURFACE('',#72112,7.49999999999995);
#4555=CYLINDRICAL_SURFACE('',#72115,7.49999999999997);
#4556=CYLINDRICAL_SURFACE('',#72118,7.50000000000076);
#4557=CYLINDRICAL_SURFACE('',#72121,7.50000000000068);
#4558=CYLINDRICAL_SURFACE('',#72124,7.50000000000021);
#4559=CYLINDRICAL_SURFACE('',#72127,7.49999999999918);
#4560=CYLINDRICAL_SURFACE('',#72130,7.50000000000134);
#4561=CYLINDRICAL_SURFACE('',#72133,7.5000000000009);
#4562=CYLINDRICAL_SURFACE('',#72136,7.49999999999987);
#4563=CYLINDRICAL_SURFACE('',#72139,7.49999999999943);
#4564=CYLINDRICAL_SURFACE('',#72142,7.5);
#4565=CYLINDRICAL_SURFACE('',#72145,7.49999999999884);
#4566=CYLINDRICAL_SURFACE('',#72148,7.50000000000024);
#4567=CYLINDRICAL_SURFACE('',#72151,7.50000000000066);
#4568=CYLINDRICAL_SURFACE('',#72154,7.50000000000124);
#4569=CYLINDRICAL_SURFACE('',#72157,7.49999999999855);
#4570=CYLINDRICAL_SURFACE('',#72160,7.50000000000082);
#4571=CYLINDRICAL_SURFACE('',#72163,7.4999999999996);
#4572=CYLINDRICAL_SURFACE('',#72166,7.50000000000008);
#4573=CYLINDRICAL_SURFACE('',#72169,7.50000000000191);
#4574=CYLINDRICAL_SURFACE('',#72172,7.50000000000073);
#4575=CYLINDRICAL_SURFACE('',#72176,7.5000000000004);
#4576=CYLINDRICAL_SURFACE('',#72180,7.49999999999908);
#4577=CYLINDRICAL_SURFACE('',#72184,7.50000000000109);
#4578=CYLINDRICAL_SURFACE('',#72188,7.49999999999915);
#4579=CYLINDRICAL_SURFACE('',#72192,7.49999999999946);
#4580=CYLINDRICAL_SURFACE('',#72196,7.50000000000006);
#4581=CYLINDRICAL_SURFACE('',#72200,7.49999999999995);
#4582=CYLINDRICAL_SURFACE('',#72204,7.49999999999935);
#4583=CYLINDRICAL_SURFACE('',#72208,7.4999999999993);
#4584=CYLINDRICAL_SURFACE('',#72212,7.49999999999968);
#4585=CYLINDRICAL_SURFACE('',#72216,7.50000000000123);
#4586=CYLINDRICAL_SURFACE('',#72220,7.50000000000104);
#4587=CYLINDRICAL_SURFACE('',#72224,7.49999999999961);
#4588=CYLINDRICAL_SURFACE('',#72228,7.50000000000035);
#4589=CYLINDRICAL_SURFACE('',#72232,7.4999999999982);
#4590=CYLINDRICAL_SURFACE('',#72236,7.50000000000075);
#4591=CYLINDRICAL_SURFACE('',#72240,7.50000000000173);
#4592=CYLINDRICAL_SURFACE('',#72244,7.49999999999834);
#4593=CYLINDRICAL_SURFACE('',#72248,7.49999999999941);
#4594=CYLINDRICAL_SURFACE('',#72252,7.49999999999971);
#4595=CYLINDRICAL_SURFACE('',#72256,7.50000000000052);
#4596=CYLINDRICAL_SURFACE('',#72260,7.49999999999878);
#4597=CYLINDRICAL_SURFACE('',#72264,7.50000000000034);
#4598=CYLINDRICAL_SURFACE('',#72268,7.50000000000112);
#4599=CYLINDRICAL_SURFACE('',#72272,7.50000000000131);
#4600=CYLINDRICAL_SURFACE('',#72276,7.49999999999987);
#4601=CYLINDRICAL_SURFACE('',#72280,7.50000000000044);
#4602=CYLINDRICAL_SURFACE('',#72284,7.50000000000073);
#4603=CYLINDRICAL_SURFACE('',#72345,7.5000000000005);
#4604=CYLINDRICAL_SURFACE('',#72349,7.50000000000059);
#4605=CYLINDRICAL_SURFACE('',#72353,7.50000000000095);
#4606=CYLINDRICAL_SURFACE('',#72357,7.49999999999793);
#4607=CYLINDRICAL_SURFACE('',#72361,7.49999999999914);
#4608=CYLINDRICAL_SURFACE('',#72365,7.50000000000072);
#4609=CYLINDRICAL_SURFACE('',#72369,7.49999999999963);
#4610=CYLINDRICAL_SURFACE('',#72373,7.49999999999949);
#4611=CYLINDRICAL_SURFACE('',#72377,7.50000000000053);
#4612=CYLINDRICAL_SURFACE('',#72381,7.50000000000013);
#4613=CYLINDRICAL_SURFACE('',#72385,7.50000000000036);
#4614=CYLINDRICAL_SURFACE('',#72389,7.50000000000167);
#4615=CYLINDRICAL_SURFACE('',#72393,7.49999999999751);
#4616=CYLINDRICAL_SURFACE('',#72397,7.49999999999885);
#4617=CYLINDRICAL_SURFACE('',#72401,7.50000000000097);
#4618=CYLINDRICAL_SURFACE('',#72405,7.49999999999976);
#4619=CYLINDRICAL_SURFACE('',#72409,7.49999999999933);
#4620=CYLINDRICAL_SURFACE('',#72413,7.49999999999933);
#4621=CYLINDRICAL_SURFACE('',#72417,7.49999999999827);
#4622=CYLINDRICAL_SURFACE('',#72421,7.50000000000131);
#4623=CYLINDRICAL_SURFACE('',#72425,7.50000000000009);
#4624=CYLINDRICAL_SURFACE('',#72429,7.50000000000029);
#4625=CYLINDRICAL_SURFACE('',#72434,7.49999999999913);
#4626=CYLINDRICAL_SURFACE('',#72437,7.50000000000064);
#4627=CYLINDRICAL_SURFACE('',#72441,7.50000000000118);
#4628=CYLINDRICAL_SURFACE('',#72445,7.49999999999926);
#4629=CYLINDRICAL_SURFACE('',#72449,7.49999999999923);
#4630=CYLINDRICAL_SURFACE('',#72453,7.50000000000082);
#4631=CYLINDRICAL_SURFACE('',#72458,7.49999999999976);
#4632=CYLINDRICAL_SURFACE('',#72462,7.49999999999993);
#4633=CYLINDRICAL_SURFACE('',#72466,7.50000000000046);
#4634=CYLINDRICAL_SURFACE('',#72470,7.50000000000008);
#4635=CYLINDRICAL_SURFACE('',#72474,7.49999999999994);
#4636=CYLINDRICAL_SURFACE('',#72478,7.50000000000125);
#4637=CYLINDRICAL_SURFACE('',#72482,7.49999999999926);
#4638=CYLINDRICAL_SURFACE('',#72486,7.49999999999853);
#4639=CYLINDRICAL_SURFACE('',#72490,7.49999999999969);
#4640=CYLINDRICAL_SURFACE('',#72494,7.49999999999989);
#4641=CYLINDRICAL_SURFACE('',#72498,7.50000000000173);
#4642=CYLINDRICAL_SURFACE('',#72502,7.4999999999987);
#4643=CYLINDRICAL_SURFACE('',#72506,7.50000000000052);
#4644=CYLINDRICAL_SURFACE('',#72510,7.50000000000042);
#4645=CYLINDRICAL_SURFACE('',#72514,7.5000000000004);
#4646=CYLINDRICAL_SURFACE('',#72518,7.50000000000212);
#4647=CYLINDRICAL_SURFACE('',#72522,7.50000000000009);
#4648=CYLINDRICAL_SURFACE('',#72526,7.50000000000025);
#4649=CYLINDRICAL_SURFACE('',#72530,7.4999999999998);
#4650=CYLINDRICAL_SURFACE('',#72534,7.50000000000038);
#4651=CYLINDRICAL_SURFACE('',#72538,7.49999999999992);
#4652=CYLINDRICAL_SURFACE('',#72542,7.49999999999992);
#4653=CYLINDRICAL_SURFACE('',#72546,7.50000000000101);
#4654=CYLINDRICAL_SURFACE('',#72550,7.49999999999969);
#4655=CYLINDRICAL_SURFACE('',#72554,7.50000000000117);
#4656=CYLINDRICAL_SURFACE('',#72558,7.4999999999993);
#4657=CYLINDRICAL_SURFACE('',#72562,7.49999999999926);
#4658=CYLINDRICAL_SURFACE('',#72565,7.49999999999808);
#4659=CYLINDRICAL_SURFACE('',#72656,7.49999999999972);
#4660=CYLINDRICAL_SURFACE('',#72661,7.49999999999782);
#4661=CYLINDRICAL_SURFACE('',#72666,7.49999999999986);
#4662=CYLINDRICAL_SURFACE('',#72671,7.50000000000091);
#4663=CYLINDRICAL_SURFACE('',#72676,7.49999999999878);
#4664=CYLINDRICAL_SURFACE('',#72681,7.50000000000178);
#4665=CYLINDRICAL_SURFACE('',#72686,7.49999999999909);
#4666=CYLINDRICAL_SURFACE('',#72691,7.5000000000006);
#4667=CYLINDRICAL_SURFACE('',#72696,7.4999999999991);
#4668=CYLINDRICAL_SURFACE('',#72701,7.4999999999995);
#4669=CYLINDRICAL_SURFACE('',#72706,7.49999999999992);
#4670=CYLINDRICAL_SURFACE('',#72711,7.49999999999957);
#4671=CYLINDRICAL_SURFACE('',#72716,7.5000000000003);
#4672=CYLINDRICAL_SURFACE('',#72721,7.49999999999944);
#4673=CYLINDRICAL_SURFACE('',#72726,7.50000000000098);
#4674=CYLINDRICAL_SURFACE('',#72731,7.5000000000002);
#4675=CYLINDRICAL_SURFACE('',#72736,7.50000000000003);
#4676=CYLINDRICAL_SURFACE('',#72741,7.50000000000008);
#4677=CYLINDRICAL_SURFACE('',#72746,7.49999999999799);
#4678=CYLINDRICAL_SURFACE('',#72751,7.49999999999937);
#4679=CYLINDRICAL_SURFACE('',#72756,7.5000000000009);
#4680=CYLINDRICAL_SURFACE('',#72761,7.50000000000057);
#4681=CYLINDRICAL_SURFACE('',#72767,7.49999999999968);
#4682=CYLINDRICAL_SURFACE('',#72771,7.50000000000128);
#4683=CYLINDRICAL_SURFACE('',#72776,7.49999999999952);
#4684=CYLINDRICAL_SURFACE('',#72781,7.5);
#4685=CYLINDRICAL_SURFACE('',#72786,7.50000000000135);
#4686=CYLINDRICAL_SURFACE('',#72791,7.4999999999995);
#4687=CYLINDRICAL_SURFACE('',#72796,7.50000000000061);
#4688=CYLINDRICAL_SURFACE('',#72800,7.4999999999991);
#4689=CYLINDRICAL_SURFACE('',#72804,7.49999999999952);
#4690=CYLINDRICAL_SURFACE('',#72808,7.50000000000152);
#4691=CYLINDRICAL_SURFACE('',#72812,7.49999999999977);
#4692=CYLINDRICAL_SURFACE('',#72816,7.50000000000048);
#4693=CYLINDRICAL_SURFACE('',#72820,7.50000000000133);
#4694=CYLINDRICAL_SURFACE('',#72824,7.49999999999992);
#4695=CYLINDRICAL_SURFACE('',#72828,7.50000000000004);
#4696=CYLINDRICAL_SURFACE('',#72832,7.49999999999888);
#4697=CYLINDRICAL_SURFACE('',#72836,7.49999999999974);
#4698=CYLINDRICAL_SURFACE('',#72840,7.50000000000138);
#4699=CYLINDRICAL_SURFACE('',#72844,7.49999999999858);
#4700=CYLINDRICAL_SURFACE('',#72848,7.5000000000013);
#4701=CYLINDRICAL_SURFACE('',#72852,7.50000000000192);
#4702=CYLINDRICAL_SURFACE('',#72856,7.50000000000123);
#4703=CYLINDRICAL_SURFACE('',#72860,7.50000000000003);
#4704=CYLINDRICAL_SURFACE('',#72864,7.50000000000171);
#4705=CYLINDRICAL_SURFACE('',#72868,7.49999999999925);
#4706=CYLINDRICAL_SURFACE('',#72872,7.49999999999916);
#4707=CYLINDRICAL_SURFACE('',#72876,7.5000000000006);
#4708=CYLINDRICAL_SURFACE('',#72880,7.49999999999937);
#4709=CYLINDRICAL_SURFACE('',#72884,7.49999999999992);
#4710=CYLINDRICAL_SURFACE('',#72888,7.50000000000151);
#4711=CYLINDRICAL_SURFACE('',#72892,7.50000000000037);
#4712=CYLINDRICAL_SURFACE('',#72896,7.50000000000052);
#4713=CYLINDRICAL_SURFACE('',#72900,7.50000000000022);
#4714=CYLINDRICAL_SURFACE('',#72904,7.50000000000124);
#4715=CYLINDRICAL_SURFACE('',#72908,7.49999999999967);
#4716=CYLINDRICAL_SURFACE('',#73029,7.49999999999918);
#4717=CYLINDRICAL_SURFACE('',#73033,7.49999999999899);
#4718=CYLINDRICAL_SURFACE('',#73037,7.49999999999804);
#4719=CYLINDRICAL_SURFACE('',#73041,7.49999999999938);
#4720=CYLINDRICAL_SURFACE('',#73045,7.49999999999996);
#4721=CYLINDRICAL_SURFACE('',#73049,7.50000000000072);
#4722=CYLINDRICAL_SURFACE('',#73053,7.49999999999797);
#4723=CYLINDRICAL_SURFACE('',#73057,7.50000000000107);
#4724=CYLINDRICAL_SURFACE('',#73061,7.49999999999992);
#4725=CYLINDRICAL_SURFACE('',#73065,7.49999999999948);
#4726=CYLINDRICAL_SURFACE('',#73069,7.50000000000065);
#4727=CYLINDRICAL_SURFACE('',#73073,7.500000000001);
#4728=CYLINDRICAL_SURFACE('',#73077,7.50000000000035);
#4729=CYLINDRICAL_SURFACE('',#73081,7.49999999999899);
#4730=CYLINDRICAL_SURFACE('',#73085,7.49999999999896);
#4731=CYLINDRICAL_SURFACE('',#73089,7.49999999999911);
#4732=CYLINDRICAL_SURFACE('',#73093,7.49999999999864);
#4733=CYLINDRICAL_SURFACE('',#73097,7.50000000000138);
#4734=CYLINDRICAL_SURFACE('',#73101,7.50000000000113);
#4735=CYLINDRICAL_SURFACE('',#73105,7.49999999999821);
#4736=CYLINDRICAL_SURFACE('',#73109,7.49999999999997);
#4737=CYLINDRICAL_SURFACE('',#73114,7.50000000000013);
#4738=CYLINDRICAL_SURFACE('',#73117,7.4999999999984);
#4739=CYLINDRICAL_SURFACE('',#73121,7.49999999999845);
#4740=CYLINDRICAL_SURFACE('',#73125,7.49999999999939);
#4741=CYLINDRICAL_SURFACE('',#73129,7.5000000000014);
#4742=CYLINDRICAL_SURFACE('',#73133,7.49999999999944);
#4743=CYLINDRICAL_SURFACE('',#73136,7.50000000000009);
#4744=CYLINDRICAL_SURFACE('',#73142,7.50000000000093);
#4745=CYLINDRICAL_SURFACE('',#73147,7.50000000000101);
#4746=CYLINDRICAL_SURFACE('',#73152,7.50000000000019);
#4747=CYLINDRICAL_SURFACE('',#73157,7.50000000000078);
#4748=CYLINDRICAL_SURFACE('',#73162,7.49999999999956);
#4749=CYLINDRICAL_SURFACE('',#73167,7.49999999999952);
#4750=CYLINDRICAL_SURFACE('',#73172,7.49999999999875);
#4751=CYLINDRICAL_SURFACE('',#73177,7.50000000000101);
#4752=CYLINDRICAL_SURFACE('',#73182,7.49999999999994);
#4753=CYLINDRICAL_SURFACE('',#73187,7.49999999999869);
#4754=CYLINDRICAL_SURFACE('',#73192,7.50000000000083);
#4755=CYLINDRICAL_SURFACE('',#73197,7.50000000000055);
#4756=CYLINDRICAL_SURFACE('',#73202,7.49999999999946);
#4757=CYLINDRICAL_SURFACE('',#73207,7.49999999999996);
#4758=CYLINDRICAL_SURFACE('',#73212,7.49999999999975);
#4759=CYLINDRICAL_SURFACE('',#73217,7.50000000000033);
#4760=CYLINDRICAL_SURFACE('',#73222,7.49999999999967);
#4761=CYLINDRICAL_SURFACE('',#73227,7.49999999999812);
#4762=CYLINDRICAL_SURFACE('',#73232,7.49999999999913);
#4763=CYLINDRICAL_SURFACE('',#73237,7.50000000000017);
#4764=CYLINDRICAL_SURFACE('',#73242,7.49999999999952);
#4765=CYLINDRICAL_SURFACE('',#73247,7.49999999999948);
#4766=CYLINDRICAL_SURFACE('',#73252,7.49999999999999);
#4767=CYLINDRICAL_SURFACE('',#73257,7.50000000000098);
#4768=CYLINDRICAL_SURFACE('',#73262,7.4999999999991);
#4769=CYLINDRICAL_SURFACE('',#73267,7.49999999999897);
#4770=CYLINDRICAL_SURFACE('',#73272,7.5000000000004);
#4771=CYLINDRICAL_SURFACE('',#73275,7.50000000000016);
#4772=CYLINDRICAL_SURFACE('',#73367,7.50000000000024);
#4773=CYLINDRICAL_SURFACE('',#73371,7.49999999999933);
#4774=CYLINDRICAL_SURFACE('',#73375,7.50000000000075);
#4775=CYLINDRICAL_SURFACE('',#73379,7.50000000000048);
#4776=CYLINDRICAL_SURFACE('',#73383,7.49999999999963);
#4777=CYLINDRICAL_SURFACE('',#73387,7.49999999999864);
#4778=CYLINDRICAL_SURFACE('',#73391,7.50000000000096);
#4779=CYLINDRICAL_SURFACE('',#73395,7.50000000000103);
#4780=CYLINDRICAL_SURFACE('',#73399,7.50000000000109);
#4781=CYLINDRICAL_SURFACE('',#73403,7.50000000000174);
#4782=CYLINDRICAL_SURFACE('',#73407,7.50000000000068);
#4783=CYLINDRICAL_SURFACE('',#73411,7.49999999999957);
#4784=CYLINDRICAL_SURFACE('',#73415,7.49999999999931);
#4785=CYLINDRICAL_SURFACE('',#73419,7.49999999999943);
#4786=CYLINDRICAL_SURFACE('',#73423,7.50000000000114);
#4787=CYLINDRICAL_SURFACE('',#73427,7.49999999999958);
#4788=CYLINDRICAL_SURFACE('',#73431,7.50000000000009);
#4789=CYLINDRICAL_SURFACE('',#73435,7.49999999999893);
#4790=CYLINDRICAL_SURFACE('',#73439,7.499999999999);
#4791=CYLINDRICAL_SURFACE('',#73443,7.50000000000161);
#4792=CYLINDRICAL_SURFACE('',#73447,7.50000000000002);
#4793=CYLINDRICAL_SURFACE('',#73451,7.499999999999);
#4794=CYLINDRICAL_SURFACE('',#73455,7.50000000000037);
#4795=CYLINDRICAL_SURFACE('',#73459,7.50000000000065);
#4796=CYLINDRICAL_SURFACE('',#73463,7.50000000000121);
#4797=CYLINDRICAL_SURFACE('',#73467,7.49999999999954);
#4798=CYLINDRICAL_SURFACE('',#73471,7.5000000000004);
#4799=CYLINDRICAL_SURFACE('',#73475,7.49999999999934);
#4800=CYLINDRICAL_SURFACE('',#73480,7.5000000000006);
#4801=CYLINDRICAL_SURFACE('',#73485,7.50000000000082);
#4802=CYLINDRICAL_SURFACE('',#73490,7.5000000000001);
#4803=CYLINDRICAL_SURFACE('',#73495,7.49999999999925);
#4804=CYLINDRICAL_SURFACE('',#73500,7.49999999999948);
#4805=CYLINDRICAL_SURFACE('',#73505,7.50000000000036);
#4806=CYLINDRICAL_SURFACE('',#73510,7.50000000000125);
#4807=CYLINDRICAL_SURFACE('',#73515,7.50000000000139);
#4808=CYLINDRICAL_SURFACE('',#73520,7.49999999999891);
#4809=CYLINDRICAL_SURFACE('',#73525,7.50000000000095);
#4810=CYLINDRICAL_SURFACE('',#73530,7.5000000000018);
#4811=CYLINDRICAL_SURFACE('',#73535,7.50000000000146);
#4812=CYLINDRICAL_SURFACE('',#73540,7.50000000000031);
#4813=CYLINDRICAL_SURFACE('',#73545,7.50000000000054);
#4814=CYLINDRICAL_SURFACE('',#73550,7.49999999999982);
#4815=CYLINDRICAL_SURFACE('',#73555,7.50000000000102);
#4816=CYLINDRICAL_SURFACE('',#73560,7.49999999999954);
#4817=CYLINDRICAL_SURFACE('',#73565,7.50000000000099);
#4818=CYLINDRICAL_SURFACE('',#73570,7.50000000000137);
#4819=CYLINDRICAL_SURFACE('',#73575,7.50000000000115);
#4820=CYLINDRICAL_SURFACE('',#73580,7.49999999999994);
#4821=CYLINDRICAL_SURFACE('',#73585,7.4999999999994);
#4822=CYLINDRICAL_SURFACE('',#73590,7.50000000000148);
#4823=CYLINDRICAL_SURFACE('',#73595,7.49999999999962);
#4824=CYLINDRICAL_SURFACE('',#73600,7.4999999999996);
#4825=CYLINDRICAL_SURFACE('',#73605,7.4999999999989);
#4826=CYLINDRICAL_SURFACE('',#73610,7.49999999999878);
#4827=CYLINDRICAL_SURFACE('',#73615,7.49999999999946);
#4828=CYLINDRICAL_SURFACE('',#73677,7.49999999999873);
#4829=CYLINDRICAL_SURFACE('',#73681,7.4999999999998);
#4830=CYLINDRICAL_SURFACE('',#73685,7.50000000000156);
#4831=CYLINDRICAL_SURFACE('',#73689,7.49999999999997);
#4832=CYLINDRICAL_SURFACE('',#73693,7.50000000000053);
#4833=CYLINDRICAL_SURFACE('',#73697,7.5000000000006);
#4834=CYLINDRICAL_SURFACE('',#73701,7.50000000000044);
#4835=CYLINDRICAL_SURFACE('',#73705,7.50000000000109);
#4836=CYLINDRICAL_SURFACE('',#73709,7.50000000000118);
#4837=CYLINDRICAL_SURFACE('',#73713,7.49999999999971);
#4838=CYLINDRICAL_SURFACE('',#73717,7.49999999999824);
#4839=CYLINDRICAL_SURFACE('',#73721,7.49999999999969);
#4840=CYLINDRICAL_SURFACE('',#73725,7.50000000000001);
#4841=CYLINDRICAL_SURFACE('',#73729,7.50000000000027);
#4842=CYLINDRICAL_SURFACE('',#73733,7.50000000000108);
#4843=CYLINDRICAL_SURFACE('',#73737,7.50000000000155);
#4844=CYLINDRICAL_SURFACE('',#73741,7.49999999999977);
#4845=CYLINDRICAL_SURFACE('',#73745,7.49999999999988);
#4846=CYLINDRICAL_SURFACE('',#73749,7.49999999999933);
#4847=CYLINDRICAL_SURFACE('',#73753,7.49999999999938);
#4848=CYLINDRICAL_SURFACE('',#73758,7.50000000000141);
#4849=CYLINDRICAL_SURFACE('',#73761,7.49999999999987);
#4850=CYLINDRICAL_SURFACE('',#73765,7.49999999999894);
#4851=CYLINDRICAL_SURFACE('',#73769,7.50000000000072);
#4852=CYLINDRICAL_SURFACE('',#73773,7.50000000000035);
#4853=CYLINDRICAL_SURFACE('',#73777,7.50000000000078);
#4854=CYLINDRICAL_SURFACE('',#73781,7.5000000000011);
#4855=CYLINDRICAL_SURFACE('',#73785,7.49999999999968);
#4856=CYLINDRICAL_SURFACE('',#73790,7.50000000000073);
#4857=CYLINDRICAL_SURFACE('',#73794,7.49999999999964);
#4858=CYLINDRICAL_SURFACE('',#73798,7.50000000000016);
#4859=CYLINDRICAL_SURFACE('',#73802,7.50000000000077);
#4860=CYLINDRICAL_SURFACE('',#73806,7.49999999999883);
#4861=CYLINDRICAL_SURFACE('',#73810,7.49999999999898);
#4862=CYLINDRICAL_SURFACE('',#73814,7.50000000000104);
#4863=CYLINDRICAL_SURFACE('',#73818,7.49999999999999);
#4864=CYLINDRICAL_SURFACE('',#73822,7.4999999999997);
#4865=CYLINDRICAL_SURFACE('',#73826,7.50000000000055);
#4866=CYLINDRICAL_SURFACE('',#73830,7.5000000000011);
#4867=CYLINDRICAL_SURFACE('',#73834,7.49999999999919);
#4868=CYLINDRICAL_SURFACE('',#73838,7.50000000000024);
#4869=CYLINDRICAL_SURFACE('',#73842,7.4999999999999);
#4870=CYLINDRICAL_SURFACE('',#73846,7.4999999999998);
#4871=CYLINDRICAL_SURFACE('',#73850,7.50000000000136);
#4872=CYLINDRICAL_SURFACE('',#73854,7.49999999999837);
#4873=CYLINDRICAL_SURFACE('',#73858,7.4999999999993);
#4874=CYLINDRICAL_SURFACE('',#73862,7.50000000000194);
#4875=CYLINDRICAL_SURFACE('',#73866,7.50000000000107);
#4876=CYLINDRICAL_SURFACE('',#73870,7.49999999999828);
#4877=CYLINDRICAL_SURFACE('',#73874,7.50000000000107);
#4878=CYLINDRICAL_SURFACE('',#73878,7.50000000000048);
#4879=CYLINDRICAL_SURFACE('',#73882,7.49999999999992);
#4880=CYLINDRICAL_SURFACE('',#73886,7.49999999999992);
#4881=CYLINDRICAL_SURFACE('',#73890,7.49999999999964);
#4882=CYLINDRICAL_SURFACE('',#73894,7.49999999999907);
#4883=CYLINDRICAL_SURFACE('',#73897,7.49999999999886);
#4884=CYLINDRICAL_SURFACE('',#73988,7.50000000000108);
#4885=CYLINDRICAL_SURFACE('',#73993,7.49999999999884);
#4886=CYLINDRICAL_SURFACE('',#73998,7.50000000000104);
#4887=CYLINDRICAL_SURFACE('',#74003,7.49999999999938);
#4888=CYLINDRICAL_SURFACE('',#74008,7.49999999999986);
#4889=CYLINDRICAL_SURFACE('',#74013,7.5000000000004);
#4890=CYLINDRICAL_SURFACE('',#74018,7.49999999999964);
#4891=CYLINDRICAL_SURFACE('',#74023,7.50000000000035);
#4892=CYLINDRICAL_SURFACE('',#74028,7.50000000000071);
#4893=CYLINDRICAL_SURFACE('',#74033,7.49999999999945);
#4894=CYLINDRICAL_SURFACE('',#74038,7.50000000000004);
#4895=CYLINDRICAL_SURFACE('',#74043,7.49999999999904);
#4896=CYLINDRICAL_SURFACE('',#74048,7.49999999999924);
#4897=CYLINDRICAL_SURFACE('',#74053,7.50000000000149);
#4898=CYLINDRICAL_SURFACE('',#74058,7.49999999999987);
#4899=CYLINDRICAL_SURFACE('',#74063,7.50000000000046);
#4900=CYLINDRICAL_SURFACE('',#74068,7.49999999999963);
#4901=CYLINDRICAL_SURFACE('',#74073,7.49999999999954);
#4902=CYLINDRICAL_SURFACE('',#74078,7.49999999999914);
#4903=CYLINDRICAL_SURFACE('',#74083,7.50000000000008);
#4904=CYLINDRICAL_SURFACE('',#74089,7.50000000000167);
#4905=CYLINDRICAL_SURFACE('',#74093,7.50000000000075);
#4906=CYLINDRICAL_SURFACE('',#74098,7.50000000000071);
#4907=CYLINDRICAL_SURFACE('',#74103,7.5000000000001);
#4908=CYLINDRICAL_SURFACE('',#74108,7.49999999999912);
#4909=CYLINDRICAL_SURFACE('',#74113,7.49999999999949);
#4910=CYLINDRICAL_SURFACE('',#74118,7.49999999999822);
#4911=CYLINDRICAL_SURFACE('',#74123,7.50000000000116);
#4912=CYLINDRICAL_SURFACE('',#74128,7.50000000000107);
#4913=CYLINDRICAL_SURFACE('',#74132,7.500000000001);
#4914=CYLINDRICAL_SURFACE('',#74136,7.49999999999867);
#4915=CYLINDRICAL_SURFACE('',#74140,7.50000000000072);
#4916=CYLINDRICAL_SURFACE('',#74144,7.50000000000002);
#4917=CYLINDRICAL_SURFACE('',#74148,7.50000000000016);
#4918=CYLINDRICAL_SURFACE('',#74152,7.4999999999977);
#4919=CYLINDRICAL_SURFACE('',#74156,7.50000000000075);
#4920=CYLINDRICAL_SURFACE('',#74160,7.50000000000128);
#4921=CYLINDRICAL_SURFACE('',#74164,7.50000000000007);
#4922=CYLINDRICAL_SURFACE('',#74168,7.49999999999968);
#4923=CYLINDRICAL_SURFACE('',#74172,7.49999999999942);
#4924=CYLINDRICAL_SURFACE('',#74176,7.49999999999947);
#4925=CYLINDRICAL_SURFACE('',#74180,7.49999999999886);
#4926=CYLINDRICAL_SURFACE('',#74184,7.49999999999996);
#4927=CYLINDRICAL_SURFACE('',#74188,7.49999999999863);
#4928=CYLINDRICAL_SURFACE('',#74192,7.49999999999905);
#4929=CYLINDRICAL_SURFACE('',#74196,7.49999999999839);
#4930=CYLINDRICAL_SURFACE('',#74200,7.50000000000018);
#4931=CYLINDRICAL_SURFACE('',#74204,7.50000000000139);
#4932=CYLINDRICAL_SURFACE('',#74208,7.50000000000011);
#4933=CYLINDRICAL_SURFACE('',#74212,7.49999999999936);
#4934=CYLINDRICAL_SURFACE('',#74216,7.49999999999924);
#4935=CYLINDRICAL_SURFACE('',#74220,7.49999999999896);
#4936=CYLINDRICAL_SURFACE('',#74224,7.50000000000106);
#4937=CYLINDRICAL_SURFACE('',#74228,7.49999999999841);
#4938=CYLINDRICAL_SURFACE('',#74232,7.5000000000007);
#4939=CYLINDRICAL_SURFACE('',#74236,7.49999999999929);
#4940=CYLINDRICAL_SURFACE('',#74357,7.49999999999838);
#4941=CYLINDRICAL_SURFACE('',#74362,7.49999999999869);
#4942=CYLINDRICAL_SURFACE('',#74367,7.50000000000082);
#4943=CYLINDRICAL_SURFACE('',#74372,7.50000000000171);
#4944=CYLINDRICAL_SURFACE('',#74377,7.49999999999838);
#4945=CYLINDRICAL_SURFACE('',#74382,7.49999999999738);
#4946=CYLINDRICAL_SURFACE('',#74387,7.49999999999968);
#4947=CYLINDRICAL_SURFACE('',#74392,7.49999999999915);
#4948=CYLINDRICAL_SURFACE('',#74397,7.50000000000115);
#4949=CYLINDRICAL_SURFACE('',#74402,7.49999999999923);
#4950=CYLINDRICAL_SURFACE('',#74407,7.49999999999971);
#4951=CYLINDRICAL_SURFACE('',#74412,7.50000000000045);
#4952=CYLINDRICAL_SURFACE('',#74417,7.4999999999983);
#4953=CYLINDRICAL_SURFACE('',#74422,7.49999999999974);
#4954=CYLINDRICAL_SURFACE('',#74427,7.50000000000059);
#4955=CYLINDRICAL_SURFACE('',#74432,7.49999999999865);
#4956=CYLINDRICAL_SURFACE('',#74437,7.5000000000016);
#4957=CYLINDRICAL_SURFACE('',#74442,7.49999999999936);
#4958=CYLINDRICAL_SURFACE('',#74447,7.49999999999902);
#4959=CYLINDRICAL_SURFACE('',#74453,7.5000000000002);
#4960=CYLINDRICAL_SURFACE('',#74457,7.50000000000014);
#4961=CYLINDRICAL_SURFACE('',#74462,7.50000000000037);
#4962=CYLINDRICAL_SURFACE('',#74467,7.5000000000016);
#4963=CYLINDRICAL_SURFACE('',#74472,7.49999999999911);
#4964=CYLINDRICAL_SURFACE('',#74477,7.49999999999995);
#4965=CYLINDRICAL_SURFACE('',#74482,7.50000000000142);
#4966=CYLINDRICAL_SURFACE('',#74487,7.50000000000018);
#4967=CYLINDRICAL_SURFACE('',#74491,7.49999999999995);
#4968=CYLINDRICAL_SURFACE('',#74498,7.49999999999969);
#4969=CYLINDRICAL_SURFACE('',#74503,7.50000000000032);
#4970=CYLINDRICAL_SURFACE('',#74508,7.50000000000134);
#4971=CYLINDRICAL_SURFACE('',#74513,7.50000000000005);
#4972=CYLINDRICAL_SURFACE('',#74518,7.50000000000026);
#4973=CYLINDRICAL_SURFACE('',#74523,7.5000000000011);
#4974=CYLINDRICAL_SURFACE('',#74528,7.50000000000166);
#4975=CYLINDRICAL_SURFACE('',#74533,7.49999999999912);
#4976=CYLINDRICAL_SURFACE('',#74538,7.50000000000039);
#4977=CYLINDRICAL_SURFACE('',#74543,7.49999999999916);
#4978=CYLINDRICAL_SURFACE('',#74548,7.49999999999987);
#4979=CYLINDRICAL_SURFACE('',#74553,7.49999999999992);
#4980=CYLINDRICAL_SURFACE('',#74558,7.49999999999871);
#4981=CYLINDRICAL_SURFACE('',#74563,7.5000000000005);
#4982=CYLINDRICAL_SURFACE('',#74568,7.50000000000091);
#4983=CYLINDRICAL_SURFACE('',#74573,7.50000000000126);
#4984=CYLINDRICAL_SURFACE('',#74578,7.50000000000107);
#4985=CYLINDRICAL_SURFACE('',#74583,7.50000000000023);
#4986=CYLINDRICAL_SURFACE('',#74588,7.49999999999994);
#4987=CYLINDRICAL_SURFACE('',#74593,7.50000000000013);
#4988=CYLINDRICAL_SURFACE('',#74598,7.50000000000086);
#4989=CYLINDRICAL_SURFACE('',#74603,7.50000000000015);
#4990=CYLINDRICAL_SURFACE('',#74608,7.50000000000103);
#4991=CYLINDRICAL_SURFACE('',#74613,7.50000000000045);
#4992=CYLINDRICAL_SURFACE('',#74618,7.50000000000103);
#4993=CYLINDRICAL_SURFACE('',#74623,7.49999999999952);
#4994=CYLINDRICAL_SURFACE('',#74628,7.50000000000068);
#4995=CYLINDRICAL_SURFACE('',#74631,7.49999999999993);
#4996=CYLINDRICAL_SURFACE('',#74723,7.49999999999987);
#4997=CYLINDRICAL_SURFACE('',#74727,7.49999999999988);
#4998=CYLINDRICAL_SURFACE('',#74731,7.49999999999856);
#4999=CYLINDRICAL_SURFACE('',#74735,7.50000000000064);
#5000=CYLINDRICAL_SURFACE('',#74739,7.50000000000078);
#5001=CYLINDRICAL_SURFACE('',#74743,7.50000000000074);
#5002=CYLINDRICAL_SURFACE('',#74747,7.49999999999937);
#5003=CYLINDRICAL_SURFACE('',#74751,7.50000000000038);
#5004=CYLINDRICAL_SURFACE('',#74755,7.50000000000138);
#5005=CYLINDRICAL_SURFACE('',#74759,7.50000000000087);
#5006=CYLINDRICAL_SURFACE('',#74763,7.50000000000108);
#5007=CYLINDRICAL_SURFACE('',#74767,7.49999999999908);
#5008=CYLINDRICAL_SURFACE('',#74771,7.49999999999961);
#5009=CYLINDRICAL_SURFACE('',#74775,7.50000000000016);
#5010=CYLINDRICAL_SURFACE('',#74779,7.4999999999995);
#5011=CYLINDRICAL_SURFACE('',#74783,7.50000000000142);
#5012=CYLINDRICAL_SURFACE('',#74787,7.50000000000107);
#5013=CYLINDRICAL_SURFACE('',#74791,7.50000000000045);
#5014=CYLINDRICAL_SURFACE('',#74795,7.49999999999951);
#5015=CYLINDRICAL_SURFACE('',#74799,7.4999999999989);
#5016=CYLINDRICAL_SURFACE('',#74803,7.49999999999918);
#5017=CYLINDRICAL_SURFACE('',#74807,7.50000000000033);
#5018=CYLINDRICAL_SURFACE('',#74811,7.49999999999982);
#5019=CYLINDRICAL_SURFACE('',#74815,7.49999999999988);
#5020=CYLINDRICAL_SURFACE('',#74819,7.50000000000107);
#5021=CYLINDRICAL_SURFACE('',#74823,7.50000000000036);
#5022=CYLINDRICAL_SURFACE('',#74827,7.50000000000041);
#5023=CYLINDRICAL_SURFACE('',#74831,7.50000000000068);
#5024=CYLINDRICAL_SURFACE('',#74836,7.50000000000055);
#5025=CYLINDRICAL_SURFACE('',#74841,7.49999999999906);
#5026=CYLINDRICAL_SURFACE('',#74846,7.49999999999978);
#5027=CYLINDRICAL_SURFACE('',#74851,7.50000000000051);
#5028=CYLINDRICAL_SURFACE('',#74856,7.50000000000021);
#5029=CYLINDRICAL_SURFACE('',#74861,7.50000000000068);
#5030=CYLINDRICAL_SURFACE('',#74866,7.50000000000086);
#5031=CYLINDRICAL_SURFACE('',#74871,7.50000000000036);
#5032=CYLINDRICAL_SURFACE('',#74876,7.50000000000095);
#5033=CYLINDRICAL_SURFACE('',#74881,7.50000000000105);
#5034=CYLINDRICAL_SURFACE('',#74886,7.50000000000114);
#5035=CYLINDRICAL_SURFACE('',#74891,7.5000000000009);
#5036=CYLINDRICAL_SURFACE('',#74896,7.50000000000006);
#5037=CYLINDRICAL_SURFACE('',#74901,7.49999999999887);
#5038=CYLINDRICAL_SURFACE('',#74906,7.49999999999948);
#5039=CYLINDRICAL_SURFACE('',#74911,7.5000000000009);
#5040=CYLINDRICAL_SURFACE('',#74916,7.49999999999928);
#5041=CYLINDRICAL_SURFACE('',#74921,7.50000000000024);
#5042=CYLINDRICAL_SURFACE('',#74926,7.50000000000052);
#5043=CYLINDRICAL_SURFACE('',#74931,7.49999999999965);
#5044=CYLINDRICAL_SURFACE('',#74936,7.50000000000169);
#5045=CYLINDRICAL_SURFACE('',#74941,7.50000000000101);
#5046=CYLINDRICAL_SURFACE('',#74946,7.49999999999905);
#5047=CYLINDRICAL_SURFACE('',#74951,7.49999999999969);
#5048=CYLINDRICAL_SURFACE('',#74956,7.50000000000003);
#5049=CYLINDRICAL_SURFACE('',#74961,7.49999999999982);
#5050=CYLINDRICAL_SURFACE('',#74966,7.4999999999998);
#5051=CYLINDRICAL_SURFACE('',#74971,7.50000000000035);
#5052=CYLINDRICAL_SURFACE('',#74976,7.4999999999998);
#5053=CYLINDRICAL_SURFACE('',#75038,7.50000000000103);
#5054=CYLINDRICAL_SURFACE('',#75042,7.49999999999921);
#5055=CYLINDRICAL_SURFACE('',#75046,7.50000000000047);
#5056=CYLINDRICAL_SURFACE('',#75050,7.49999999999861);
#5057=CYLINDRICAL_SURFACE('',#75054,7.49999999999951);
#5058=CYLINDRICAL_SURFACE('',#75058,7.4999999999994);
#5059=CYLINDRICAL_SURFACE('',#75062,7.49999999999855);
#5060=CYLINDRICAL_SURFACE('',#75066,7.50000000000025);
#5061=CYLINDRICAL_SURFACE('',#75070,7.50000000000009);
#5062=CYLINDRICAL_SURFACE('',#75074,7.49999999999832);
#5063=CYLINDRICAL_SURFACE('',#75078,7.49999999999923);
#5064=CYLINDRICAL_SURFACE('',#75082,7.49999999999844);
#5065=CYLINDRICAL_SURFACE('',#75086,7.49999999999893);
#5066=CYLINDRICAL_SURFACE('',#75090,7.50000000000281);
#5067=CYLINDRICAL_SURFACE('',#75094,7.50000000000082);
#5068=CYLINDRICAL_SURFACE('',#75098,7.5);
#5069=CYLINDRICAL_SURFACE('',#75102,7.50000000000082);
#5070=CYLINDRICAL_SURFACE('',#75106,7.50000000000095);
#5071=CYLINDRICAL_SURFACE('',#75111,7.50000000000097);
#5072=CYLINDRICAL_SURFACE('',#75114,7.50000000000035);
#5073=CYLINDRICAL_SURFACE('',#75118,7.49999999999909);
#5074=CYLINDRICAL_SURFACE('',#75122,7.5000000000005);
#5075=CYLINDRICAL_SURFACE('',#75126,7.49999999999976);
#5076=CYLINDRICAL_SURFACE('',#75130,7.49999999999953);
#5077=CYLINDRICAL_SURFACE('',#75134,7.49999999999916);
#5078=CYLINDRICAL_SURFACE('',#75138,7.5000000000001);
#5079=CYLINDRICAL_SURFACE('',#75142,7.50000000000193);
#5080=CYLINDRICAL_SURFACE('',#75146,7.49999999999949);
#5081=CYLINDRICAL_SURFACE('',#75151,7.4999999999997);
#5082=CYLINDRICAL_SURFACE('',#75155,7.49999999999984);
#5083=CYLINDRICAL_SURFACE('',#75159,7.50000000000064);
#5084=CYLINDRICAL_SURFACE('',#75163,7.49999999999956);
#5085=CYLINDRICAL_SURFACE('',#75167,7.50000000000121);
#5086=CYLINDRICAL_SURFACE('',#75171,7.49999999999886);
#5087=CYLINDRICAL_SURFACE('',#75175,7.49999999999906);
#5088=CYLINDRICAL_SURFACE('',#75179,7.49999999999926);
#5089=CYLINDRICAL_SURFACE('',#75183,7.49999999999995);
#5090=CYLINDRICAL_SURFACE('',#75187,7.49999999999959);
#5091=CYLINDRICAL_SURFACE('',#75191,7.49999999999962);
#5092=CYLINDRICAL_SURFACE('',#75195,7.50000000000058);
#5093=CYLINDRICAL_SURFACE('',#75199,7.49999999999953);
#5094=CYLINDRICAL_SURFACE('',#75203,7.49999999999982);
#5095=CYLINDRICAL_SURFACE('',#75207,7.49999999999959);
#5096=CYLINDRICAL_SURFACE('',#75211,7.50000000000001);
#5097=CYLINDRICAL_SURFACE('',#75215,7.49999999999972);
#5098=CYLINDRICAL_SURFACE('',#75219,7.50000000000012);
#5099=CYLINDRICAL_SURFACE('',#75223,7.49999999999998);
#5100=CYLINDRICAL_SURFACE('',#75227,7.49999999999767);
#5101=CYLINDRICAL_SURFACE('',#75231,7.50000000000083);
#5102=CYLINDRICAL_SURFACE('',#75235,7.49999999999857);
#5103=CYLINDRICAL_SURFACE('',#75239,7.50000000000065);
#5104=CYLINDRICAL_SURFACE('',#75243,7.49999999999904);
#5105=CYLINDRICAL_SURFACE('',#75247,7.50000000000149);
#5106=CYLINDRICAL_SURFACE('',#75251,7.49999999999998);
#5107=CYLINDRICAL_SURFACE('',#75255,7.50000000000078);
#5108=CYLINDRICAL_SURFACE('',#75258,7.49999999999895);
#5109=CYLINDRICAL_SURFACE('',#75378,7.50000000000086);
#5110=CYLINDRICAL_SURFACE('',#75383,7.50000000000024);
#5111=CYLINDRICAL_SURFACE('',#75388,7.49999999999883);
#5112=CYLINDRICAL_SURFACE('',#75393,7.50000000000074);
#5113=CYLINDRICAL_SURFACE('',#75398,7.49999999999952);
#5114=CYLINDRICAL_SURFACE('',#75403,7.49999999999914);
#5115=CYLINDRICAL_SURFACE('',#75408,7.49999999999965);
#5116=CYLINDRICAL_SURFACE('',#75413,7.50000000000115);
#5117=CYLINDRICAL_SURFACE('',#75418,7.49999999999992);
#5118=CYLINDRICAL_SURFACE('',#75423,7.49999999999906);
#5119=CYLINDRICAL_SURFACE('',#75428,7.50000000000055);
#5120=CYLINDRICAL_SURFACE('',#75433,7.50000000000195);
#5121=CYLINDRICAL_SURFACE('',#75438,7.49999999999956);
#5122=CYLINDRICAL_SURFACE('',#75443,7.49999999999863);
#5123=CYLINDRICAL_SURFACE('',#75448,7.49999999999977);
#5124=CYLINDRICAL_SURFACE('',#75453,7.5000000000016);
#5125=CYLINDRICAL_SURFACE('',#75458,7.50000000000047);
#5126=CYLINDRICAL_SURFACE('',#75463,7.50000000000125);
#5127=CYLINDRICAL_SURFACE('',#75469,7.50000000000031);
#5128=CYLINDRICAL_SURFACE('',#75473,7.50000000000031);
#5129=CYLINDRICAL_SURFACE('',#75478,7.49999999999752);
#5130=CYLINDRICAL_SURFACE('',#75483,7.49999999999966);
#5131=CYLINDRICAL_SURFACE('',#75488,7.50000000000105);
#5132=CYLINDRICAL_SURFACE('',#75493,7.50000000000112);
#5133=CYLINDRICAL_SURFACE('',#75498,7.5000000000005);
#5134=CYLINDRICAL_SURFACE('',#75503,7.49999999999953);
#5135=CYLINDRICAL_SURFACE('',#75508,7.50000000000087);
#5136=CYLINDRICAL_SURFACE('',#75513,7.49999999999993);
#5137=CYLINDRICAL_SURFACE('',#75519,7.5000000000018);
#5138=CYLINDRICAL_SURFACE('',#75524,7.50000000000045);
#5139=CYLINDRICAL_SURFACE('',#75529,7.49999999999987);
#5140=CYLINDRICAL_SURFACE('',#75534,7.5000000000015);
#5141=CYLINDRICAL_SURFACE('',#75539,7.50000000000095);
#5142=CYLINDRICAL_SURFACE('',#75544,7.50000000000098);
#5143=CYLINDRICAL_SURFACE('',#75549,7.50000000000068);
#5144=CYLINDRICAL_SURFACE('',#75554,7.49999999999984);
#5145=CYLINDRICAL_SURFACE('',#75559,7.50000000000035);
#5146=CYLINDRICAL_SURFACE('',#75564,7.49999999999952);
#5147=CYLINDRICAL_SURFACE('',#75569,7.50000000000135);
#5148=CYLINDRICAL_SURFACE('',#75574,7.49999999999964);
#5149=CYLINDRICAL_SURFACE('',#75579,7.50000000000069);
#5150=CYLINDRICAL_SURFACE('',#75584,7.50000000000112);
#5151=CYLINDRICAL_SURFACE('',#75589,7.50000000000045);
#5152=CYLINDRICAL_SURFACE('',#75594,7.500000000003);
#5153=CYLINDRICAL_SURFACE('',#75599,7.50000000000051);
#5154=CYLINDRICAL_SURFACE('',#75604,7.50000000000022);
#5155=CYLINDRICAL_SURFACE('',#75609,7.49999999999907);
#5156=CYLINDRICAL_SURFACE('',#75614,7.49999999999984);
#5157=CYLINDRICAL_SURFACE('',#75619,7.50000000000031);
#5158=CYLINDRICAL_SURFACE('',#75624,7.50000000000036);
#5159=CYLINDRICAL_SURFACE('',#75629,7.49999999999868);
#5160=CYLINDRICAL_SURFACE('',#75634,7.49999999999904);
#5161=CYLINDRICAL_SURFACE('',#75639,7.49999999999943);
#5162=CYLINDRICAL_SURFACE('',#75644,7.49999999999986);
#5163=CYLINDRICAL_SURFACE('',#75649,7.50000000000246);
#5164=CYLINDRICAL_SURFACE('',#75654,7.50000000000062);
#5165=CYLINDRICAL_SURFACE('',#75775,7.49999999999993);
#5166=CYLINDRICAL_SURFACE('',#75780,7.50000000000008);
#5167=CYLINDRICAL_SURFACE('',#75785,7.50000000000149);
#5168=CYLINDRICAL_SURFACE('',#75790,7.50000000000108);
#5169=CYLINDRICAL_SURFACE('',#75795,7.50000000000101);
#5170=CYLINDRICAL_SURFACE('',#75800,7.49999999999874);
#5171=CYLINDRICAL_SURFACE('',#75805,7.50000000000018);
#5172=CYLINDRICAL_SURFACE('',#75810,7.50000000000006);
#5173=CYLINDRICAL_SURFACE('',#75815,7.5000000000002);
#5174=CYLINDRICAL_SURFACE('',#75820,7.50000000000027);
#5175=CYLINDRICAL_SURFACE('',#75825,7.50000000000002);
#5176=CYLINDRICAL_SURFACE('',#75830,7.49999999999989);
#5177=CYLINDRICAL_SURFACE('',#75835,7.50000000000097);
#5178=CYLINDRICAL_SURFACE('',#75840,7.50000000000115);
#5179=CYLINDRICAL_SURFACE('',#75845,7.50000000000046);
#5180=CYLINDRICAL_SURFACE('',#75850,7.49999999999974);
#5181=CYLINDRICAL_SURFACE('',#75855,7.50000000000165);
#5182=CYLINDRICAL_SURFACE('',#75861,7.50000000000142);
#5183=CYLINDRICAL_SURFACE('',#75865,7.50000000000104);
#5184=CYLINDRICAL_SURFACE('',#75870,7.49999999999953);
#5185=CYLINDRICAL_SURFACE('',#75875,7.50000000000099);
#5186=CYLINDRICAL_SURFACE('',#75880,7.50000000000091);
#5187=CYLINDRICAL_SURFACE('',#75885,7.49999999999943);
#5188=CYLINDRICAL_SURFACE('',#75890,7.50000000000072);
#5189=CYLINDRICAL_SURFACE('',#75895,7.49999999999811);
#5190=CYLINDRICAL_SURFACE('',#75900,7.50000000000036);
#5191=CYLINDRICAL_SURFACE('',#75905,7.49999999999855);
#5192=CYLINDRICAL_SURFACE('',#75909,7.49999999999989);
#5193=CYLINDRICAL_SURFACE('',#75916,7.49999999999854);
#5194=CYLINDRICAL_SURFACE('',#75921,7.4999999999983);
#5195=CYLINDRICAL_SURFACE('',#75926,7.49999999999806);
#5196=CYLINDRICAL_SURFACE('',#75931,7.49999999999984);
#5197=CYLINDRICAL_SURFACE('',#75936,7.49999999999986);
#5198=CYLINDRICAL_SURFACE('',#75941,7.50000000000069);
#5199=CYLINDRICAL_SURFACE('',#75946,7.49999999999977);
#5200=CYLINDRICAL_SURFACE('',#75951,7.49999999999974);
#5201=CYLINDRICAL_SURFACE('',#75956,7.49999999999927);
#5202=CYLINDRICAL_SURFACE('',#75961,7.50000000000063);
#5203=CYLINDRICAL_SURFACE('',#75966,7.4999999999996);
#5204=CYLINDRICAL_SURFACE('',#75971,7.49999999999951);
#5205=CYLINDRICAL_SURFACE('',#75976,7.50000000000091);
#5206=CYLINDRICAL_SURFACE('',#75981,7.49999999999948);
#5207=CYLINDRICAL_SURFACE('',#75986,7.49999999999928);
#5208=CYLINDRICAL_SURFACE('',#75991,7.49999999999904);
#5209=CYLINDRICAL_SURFACE('',#75996,7.49999999999936);
#5210=CYLINDRICAL_SURFACE('',#76001,7.50000000000108);
#5211=CYLINDRICAL_SURFACE('',#76006,7.5000000000006);
#5212=CYLINDRICAL_SURFACE('',#76011,7.50000000000072);
#5213=CYLINDRICAL_SURFACE('',#76016,7.49999999999886);
#5214=CYLINDRICAL_SURFACE('',#76021,7.49999999999831);
#5215=CYLINDRICAL_SURFACE('',#76026,7.50000000000101);
#5216=CYLINDRICAL_SURFACE('',#76031,7.49999999999924);
#5217=CYLINDRICAL_SURFACE('',#76036,7.49999999999796);
#5218=CYLINDRICAL_SURFACE('',#76041,7.49999999999881);
#5219=CYLINDRICAL_SURFACE('',#76046,7.49999999999965);
#5220=CYLINDRICAL_SURFACE('',#76049,7.50000000000054);
#5221=CYLINDRICAL_SURFACE('',#76141,7.49999999999829);
#5222=CYLINDRICAL_SURFACE('',#76145,7.50000000000136);
#5223=CYLINDRICAL_SURFACE('',#76149,7.50000000000038);
#5224=CYLINDRICAL_SURFACE('',#76153,7.50000000000154);
#5225=CYLINDRICAL_SURFACE('',#76157,7.50000000000029);
#5226=CYLINDRICAL_SURFACE('',#76161,7.49999999999914);
#5227=CYLINDRICAL_SURFACE('',#76165,7.49999999999986);
#5228=CYLINDRICAL_SURFACE('',#76169,7.5000000000006);
#5229=CYLINDRICAL_SURFACE('',#76173,7.50000000000089);
#5230=CYLINDRICAL_SURFACE('',#76177,7.50000000000173);
#5231=CYLINDRICAL_SURFACE('',#76181,7.49999999999671);
#5232=CYLINDRICAL_SURFACE('',#76185,7.50000000000107);
#5233=CYLINDRICAL_SURFACE('',#76189,7.50000000000124);
#5234=CYLINDRICAL_SURFACE('',#76193,7.4999999999985);
#5235=CYLINDRICAL_SURFACE('',#76197,7.49999999999936);
#5236=CYLINDRICAL_SURFACE('',#76201,7.50000000000132);
#5237=CYLINDRICAL_SURFACE('',#76205,7.50000000000063);
#5238=CYLINDRICAL_SURFACE('',#76209,7.49999999999944);
#5239=CYLINDRICAL_SURFACE('',#76213,7.50000000000154);
#5240=CYLINDRICAL_SURFACE('',#76217,7.49999999999982);
#5241=CYLINDRICAL_SURFACE('',#76221,7.49999999999879);
#5242=CYLINDRICAL_SURFACE('',#76225,7.49999999999893);
#5243=CYLINDRICAL_SURFACE('',#76229,7.49999999999837);
#5244=CYLINDRICAL_SURFACE('',#76233,7.49999999999956);
#5245=CYLINDRICAL_SURFACE('',#76237,7.50000000000076);
#5246=CYLINDRICAL_SURFACE('',#76241,7.49999999999921);
#5247=CYLINDRICAL_SURFACE('',#76245,7.49999999999933);
#5248=CYLINDRICAL_SURFACE('',#76249,7.5000000000015);
#5249=CYLINDRICAL_SURFACE('',#76258,7.50000000000068);
#5250=CYLINDRICAL_SURFACE('',#76267,7.49999999999906);
#5251=CYLINDRICAL_SURFACE('',#76276,7.50000000000119);
#5252=CYLINDRICAL_SURFACE('',#76285,7.50000000000095);
#5253=CYLINDRICAL_SURFACE('',#76294,7.49999999999979);
#5254=CYLINDRICAL_SURFACE('',#76303,7.49999999999866);
#5255=CYLINDRICAL_SURFACE('',#76312,7.50000000000089);
#5256=CYLINDRICAL_SURFACE('',#76321,7.50000000000142);
#5257=CYLINDRICAL_SURFACE('',#76330,7.49999999999948);
#5258=CYLINDRICAL_SURFACE('',#76339,7.49999999999996);
#5259=CYLINDRICAL_SURFACE('',#76348,7.49999999999837);
#5260=CYLINDRICAL_SURFACE('',#76357,7.50000000000016);
#5261=CYLINDRICAL_SURFACE('',#76366,7.5000000000002);
#5262=CYLINDRICAL_SURFACE('',#76375,7.49999999999976);
#5263=CYLINDRICAL_SURFACE('',#76384,7.50000000000073);
#5264=CYLINDRICAL_SURFACE('',#76393,7.50000000000145);
#5265=CYLINDRICAL_SURFACE('',#76402,7.50000000000033);
#5266=CYLINDRICAL_SURFACE('',#76411,7.50000000000189);
#5267=CYLINDRICAL_SURFACE('',#76420,7.50000000000128);
#5268=CYLINDRICAL_SURFACE('',#76429,7.49999999999988);
#5269=CYLINDRICAL_SURFACE('',#76438,7.50000000000037);
#5270=CYLINDRICAL_SURFACE('',#76447,7.49999999999926);
#5271=CYLINDRICAL_SURFACE('',#76456,7.50000000000009);
#5272=CYLINDRICAL_SURFACE('',#76465,7.49999999999888);
#5273=CYLINDRICAL_SURFACE('',#76474,7.5000000000001);
#5274=CYLINDRICAL_SURFACE('',#76483,7.49999999999936);
#5275=CYLINDRICAL_SURFACE('',#76492,7.49999999999966);
#5276=CYLINDRICAL_SURFACE('',#76501,7.49999999999988);
#5277=CYLINDRICAL_SURFACE('',#76651,7.50000000000019);
#5278=CYLINDRICAL_SURFACE('',#76656,7.50000000000089);
#5279=CYLINDRICAL_SURFACE('',#76661,7.500000000001);
#5280=CYLINDRICAL_SURFACE('',#76666,7.50000000000125);
#5281=CYLINDRICAL_SURFACE('',#76671,7.50000000000063);
#5282=CYLINDRICAL_SURFACE('',#76676,7.49999999999918);
#5283=CYLINDRICAL_SURFACE('',#76681,7.50000000000149);
#5284=CYLINDRICAL_SURFACE('',#76686,7.50000000000101);
#5285=CYLINDRICAL_SURFACE('',#76691,7.49999999999985);
#5286=CYLINDRICAL_SURFACE('',#76696,7.50000000000006);
#5287=CYLINDRICAL_SURFACE('',#76701,7.50000000000201);
#5288=CYLINDRICAL_SURFACE('',#76706,7.5000000000003);
#5289=CYLINDRICAL_SURFACE('',#76711,7.50000000000073);
#5290=CYLINDRICAL_SURFACE('',#76716,7.49999999999934);
#5291=CYLINDRICAL_SURFACE('',#76721,7.49999999999874);
#5292=CYLINDRICAL_SURFACE('',#76726,7.50000000000064);
#5293=CYLINDRICAL_SURFACE('',#76732,7.49999999999973);
#5294=CYLINDRICAL_SURFACE('',#76736,7.49999999999924);
#5295=CYLINDRICAL_SURFACE('',#76741,7.50000000000012);
#5296=CYLINDRICAL_SURFACE('',#76746,7.499999999999);
#5297=CYLINDRICAL_SURFACE('',#76751,7.49999999999987);
#5298=CYLINDRICAL_SURFACE('',#76756,7.50000000000125);
#5299=CYLINDRICAL_SURFACE('',#76761,7.50000000000055);
#5300=CYLINDRICAL_SURFACE('',#76766,7.50000000000049);
#5301=CYLINDRICAL_SURFACE('',#76771,7.49999999999952);
#5302=CYLINDRICAL_SURFACE('',#76776,7.50000000000184);
#5303=CYLINDRICAL_SURFACE('',#76781,7.49999999999831);
#5304=CYLINDRICAL_SURFACE('',#76785,7.50000000000028);
#5305=CYLINDRICAL_SURFACE('',#76933,7.50000000000006);
#5306=CYLINDRICAL_SURFACE('',#76938,7.50000000000193);
#5307=CYLINDRICAL_SURFACE('',#76943,7.50000000000066);
#5308=CYLINDRICAL_SURFACE('',#76948,7.50000000000187);
#5309=CYLINDRICAL_SURFACE('',#76953,7.49999999999954);
#5310=CYLINDRICAL_SURFACE('',#76958,7.49999999999832);
#5311=CYLINDRICAL_SURFACE('',#76963,7.49999999999972);
#5312=CYLINDRICAL_SURFACE('',#76968,7.50000000000133);
#5313=CYLINDRICAL_SURFACE('',#76973,7.50000000000065);
#5314=CYLINDRICAL_SURFACE('',#76978,7.50000000000155);
#5315=CYLINDRICAL_SURFACE('',#76983,7.50000000000083);
#5316=CYLINDRICAL_SURFACE('',#76988,7.50000000000002);
#5317=CYLINDRICAL_SURFACE('',#76993,7.49999999999901);
#5318=CYLINDRICAL_SURFACE('',#76998,7.50000000000075);
#5319=CYLINDRICAL_SURFACE('',#77003,7.50000000000107);
#5320=CYLINDRICAL_SURFACE('',#77008,7.49999999999885);
#5321=CYLINDRICAL_SURFACE('',#77014,7.50000000000039);
#5322=CYLINDRICAL_SURFACE('',#77018,7.49999999999898);
#5323=CYLINDRICAL_SURFACE('',#77023,7.49999999999877);
#5324=CYLINDRICAL_SURFACE('',#77028,7.49999999999893);
#5325=CYLINDRICAL_SURFACE('',#77033,7.4999999999999);
#5326=CYLINDRICAL_SURFACE('',#77038,7.49999999999949);
#5327=CYLINDRICAL_SURFACE('',#77043,7.49999999999888);
#5328=CYLINDRICAL_SURFACE('',#77048,7.50000000000012);
#5329=CYLINDRICAL_SURFACE('',#77053,7.49999999999965);
#5330=CYLINDRICAL_SURFACE('',#77058,7.50000000000049);
#5331=CYLINDRICAL_SURFACE('',#77063,7.49999999999969);
#5332=CYLINDRICAL_SURFACE('',#77068,7.50000000000174);
#5333=CYLINDRICAL_SURFACE('',#77166,7.50000000000002);
#5334=CYLINDRICAL_SURFACE('',#77175,7.50000000000086);
#5335=CYLINDRICAL_SURFACE('',#77184,7.49999999999894);
#5336=CYLINDRICAL_SURFACE('',#77193,7.49999999999968);
#5337=CYLINDRICAL_SURFACE('',#77202,7.49999999999949);
#5338=CYLINDRICAL_SURFACE('',#77211,7.50000000000058);
#5339=CYLINDRICAL_SURFACE('',#77223,7.49999999999883);
#5340=CYLINDRICAL_SURFACE('',#77232,7.50000000000146);
#5341=CYLINDRICAL_SURFACE('',#77241,7.49999999999999);
#5342=CYLINDRICAL_SURFACE('',#77250,7.50000000000032);
#5343=CYLINDRICAL_SURFACE('',#77259,7.49999999999892);
#5344=CYLINDRICAL_SURFACE('',#77268,7.50000000000196);
#5345=CYLINDRICAL_SURFACE('',#77277,7.50000000000019);
#5346=CYLINDRICAL_SURFACE('',#77286,7.50000000000041);
#5347=CYLINDRICAL_SURFACE('',#77295,7.50000000000071);
#5348=CYLINDRICAL_SURFACE('',#77304,7.49999999999975);
#5349=CYLINDRICAL_SURFACE('',#77313,7.49999999999947);
#5350=CYLINDRICAL_SURFACE('',#77322,7.5);
#5351=CYLINDRICAL_SURFACE('',#77331,7.49999999999963);
#5352=CYLINDRICAL_SURFACE('',#77340,7.49999999999951);
#5353=CYLINDRICAL_SURFACE('',#77349,7.50000000000136);
#5354=CYLINDRICAL_SURFACE('',#77358,7.49999999999879);
#5355=CYLINDRICAL_SURFACE('',#77367,7.50000000000127);
#5356=CYLINDRICAL_SURFACE('',#77376,7.50000000000044);
#5357=CYLINDRICAL_SURFACE('',#77385,7.49999999999987);
#5358=CYLINDRICAL_SURFACE('',#77394,7.50000000000078);
#5359=CYLINDRICAL_SURFACE('',#77403,7.50000000000087);
#5360=CYLINDRICAL_SURFACE('',#77410,7.50000000000169);
#5361=CYLINDRICAL_SURFACE('',#77642,7.);
#5362=CYLINDRICAL_SURFACE('',#77645,4.5);
#5363=CYLINDRICAL_SURFACE('',#77652,6.5);
#5364=CYLINDRICAL_SURFACE('',#77656,5.99999999999999);
#5365=CYLINDRICAL_SURFACE('',#77663,5.9);
#5366=CYLINDRICAL_SURFACE('',#77669,5.99999999999999);
#5367=CYLINDRICAL_SURFACE('',#77677,6.);
#5368=CYLINDRICAL_SURFACE('',#77679,6.);
#5369=CYLINDRICAL_SURFACE('',#77682,2.5);
#5370=CYLINDRICAL_SURFACE('',#77689,2.5);
#5371=CYLINDRICAL_SURFACE('',#77691,12.9999999996215);
#5372=CYLINDRICAL_SURFACE('',#77694,6.00000000044796);
#5373=CYLINDRICAL_SURFACE('',#77699,2.99999999919632);
#5374=CYLINDRICAL_SURFACE('',#77700,2.99999999919632);
#5375=CYLINDRICAL_SURFACE('',#77709,4.50000000012307);
#5376=CYLINDRICAL_SURFACE('',#77712,2.5);
#5377=CYLINDRICAL_SURFACE('',#77722,4.);
#5378=CYLINDRICAL_SURFACE('',#77732,1.65);
#5379=CYLINDRICAL_SURFACE('',#77736,1.65);
#5380=CYLINDRICAL_SURFACE('',#77740,2.5);
#5381=CYLINDRICAL_SURFACE('',#77750,1.676167978);
#5382=CYLINDRICAL_SURFACE('',#77752,1.65);
#5383=FACE_OUTER_BOUND('',#10648,.T.);
#5384=FACE_OUTER_BOUND('',#10649,.T.);
#5385=FACE_OUTER_BOUND('',#10650,.T.);
#5386=FACE_OUTER_BOUND('',#10651,.T.);
#5387=FACE_OUTER_BOUND('',#10652,.T.);
#5388=FACE_OUTER_BOUND('',#10653,.T.);
#5389=FACE_OUTER_BOUND('',#10654,.T.);
#5390=FACE_OUTER_BOUND('',#10655,.T.);
#5391=FACE_OUTER_BOUND('',#10656,.T.);
#5392=FACE_OUTER_BOUND('',#10657,.T.);
#5393=FACE_OUTER_BOUND('',#10658,.T.);
#5394=FACE_OUTER_BOUND('',#10659,.T.);
#5395=FACE_OUTER_BOUND('',#10660,.T.);
#5396=FACE_OUTER_BOUND('',#10661,.T.);
#5397=FACE_OUTER_BOUND('',#10662,.T.);
#5398=FACE_OUTER_BOUND('',#10663,.T.);
#5399=FACE_OUTER_BOUND('',#10664,.T.);
#5400=FACE_OUTER_BOUND('',#10665,.T.);
#5401=FACE_OUTER_BOUND('',#10666,.T.);
#5402=FACE_OUTER_BOUND('',#10667,.T.);
#5403=FACE_OUTER_BOUND('',#10668,.T.);
#5404=FACE_OUTER_BOUND('',#10669,.T.);
#5405=FACE_OUTER_BOUND('',#10670,.T.);
#5406=FACE_OUTER_BOUND('',#10671,.T.);
#5407=FACE_OUTER_BOUND('',#10672,.T.);
#5408=FACE_OUTER_BOUND('',#10673,.T.);
#5409=FACE_OUTER_BOUND('',#10674,.T.);
#5410=FACE_OUTER_BOUND('',#10675,.T.);
#5411=FACE_OUTER_BOUND('',#10676,.T.);
#5412=FACE_OUTER_BOUND('',#10677,.T.);
#5413=FACE_OUTER_BOUND('',#10678,.T.);
#5414=FACE_OUTER_BOUND('',#10679,.T.);
#5415=FACE_OUTER_BOUND('',#10680,.T.);
#5416=FACE_OUTER_BOUND('',#10681,.T.);
#5417=FACE_OUTER_BOUND('',#10682,.T.);
#5418=FACE_OUTER_BOUND('',#10683,.T.);
#5419=FACE_OUTER_BOUND('',#10684,.T.);
#5420=FACE_OUTER_BOUND('',#10685,.T.);
#5421=FACE_OUTER_BOUND('',#10686,.T.);
#5422=FACE_OUTER_BOUND('',#10687,.T.);
#5423=FACE_OUTER_BOUND('',#10688,.T.);
#5424=FACE_OUTER_BOUND('',#10689,.T.);
#5425=FACE_OUTER_BOUND('',#10690,.T.);
#5426=FACE_OUTER_BOUND('',#10691,.T.);
#5427=FACE_OUTER_BOUND('',#10692,.T.);
#5428=FACE_OUTER_BOUND('',#10693,.T.);
#5429=FACE_OUTER_BOUND('',#10694,.T.);
#5430=FACE_OUTER_BOUND('',#10695,.T.);
#5431=FACE_OUTER_BOUND('',#10696,.T.);
#5432=FACE_OUTER_BOUND('',#10697,.T.);
#5433=FACE_OUTER_BOUND('',#10698,.T.);
#5434=FACE_OUTER_BOUND('',#10699,.T.);
#5435=FACE_OUTER_BOUND('',#10700,.T.);
#5436=FACE_OUTER_BOUND('',#10701,.T.);
#5437=FACE_OUTER_BOUND('',#10702,.T.);
#5438=FACE_OUTER_BOUND('',#10703,.T.);
#5439=FACE_OUTER_BOUND('',#10704,.T.);
#5440=FACE_OUTER_BOUND('',#10705,.T.);
#5441=FACE_OUTER_BOUND('',#10706,.T.);
#5442=FACE_OUTER_BOUND('',#10707,.T.);
#5443=FACE_OUTER_BOUND('',#10708,.T.);
#5444=FACE_OUTER_BOUND('',#10709,.T.);
#5445=FACE_OUTER_BOUND('',#10710,.T.);
#5446=FACE_OUTER_BOUND('',#10711,.T.);
#5447=FACE_OUTER_BOUND('',#10712,.T.);
#5448=FACE_OUTER_BOUND('',#10713,.T.);
#5449=FACE_OUTER_BOUND('',#10714,.T.);
#5450=FACE_OUTER_BOUND('',#10715,.T.);
#5451=FACE_OUTER_BOUND('',#10716,.T.);
#5452=FACE_OUTER_BOUND('',#10717,.T.);
#5453=FACE_OUTER_BOUND('',#10718,.T.);
#5454=FACE_OUTER_BOUND('',#10719,.T.);
#5455=FACE_OUTER_BOUND('',#10720,.T.);
#5456=FACE_OUTER_BOUND('',#10721,.T.);
#5457=FACE_OUTER_BOUND('',#10722,.T.);
#5458=FACE_OUTER_BOUND('',#10723,.T.);
#5459=FACE_OUTER_BOUND('',#10724,.T.);
#5460=FACE_OUTER_BOUND('',#10725,.T.);
#5461=FACE_OUTER_BOUND('',#10726,.T.);
#5462=FACE_OUTER_BOUND('',#10727,.T.);
#5463=FACE_OUTER_BOUND('',#10728,.T.);
#5464=FACE_OUTER_BOUND('',#10729,.T.);
#5465=FACE_OUTER_BOUND('',#10730,.T.);
#5466=FACE_OUTER_BOUND('',#10731,.T.);
#5467=FACE_OUTER_BOUND('',#10732,.T.);
#5468=FACE_OUTER_BOUND('',#10733,.T.);
#5469=FACE_OUTER_BOUND('',#10734,.T.);
#5470=FACE_OUTER_BOUND('',#10735,.T.);
#5471=FACE_OUTER_BOUND('',#10736,.T.);
#5472=FACE_OUTER_BOUND('',#10737,.T.);
#5473=FACE_OUTER_BOUND('',#10738,.T.);
#5474=FACE_OUTER_BOUND('',#10739,.T.);
#5475=FACE_OUTER_BOUND('',#10740,.T.);
#5476=FACE_OUTER_BOUND('',#10741,.T.);
#5477=FACE_OUTER_BOUND('',#10742,.T.);
#5478=FACE_OUTER_BOUND('',#10743,.T.);
#5479=FACE_OUTER_BOUND('',#10744,.T.);
#5480=FACE_OUTER_BOUND('',#10745,.T.);
#5481=FACE_OUTER_BOUND('',#10746,.T.);
#5482=FACE_OUTER_BOUND('',#10747,.T.);
#5483=FACE_OUTER_BOUND('',#10748,.T.);
#5484=FACE_OUTER_BOUND('',#10749,.T.);
#5485=FACE_OUTER_BOUND('',#10750,.T.);
#5486=FACE_OUTER_BOUND('',#10751,.T.);
#5487=FACE_OUTER_BOUND('',#10752,.T.);
#5488=FACE_OUTER_BOUND('',#10753,.T.);
#5489=FACE_OUTER_BOUND('',#10754,.T.);
#5490=FACE_OUTER_BOUND('',#10755,.T.);
#5491=FACE_OUTER_BOUND('',#10756,.T.);
#5492=FACE_OUTER_BOUND('',#10757,.T.);
#5493=FACE_OUTER_BOUND('',#10758,.T.);
#5494=FACE_OUTER_BOUND('',#10759,.T.);
#5495=FACE_OUTER_BOUND('',#10760,.T.);
#5496=FACE_OUTER_BOUND('',#10761,.T.);
#5497=FACE_OUTER_BOUND('',#10762,.T.);
#5498=FACE_OUTER_BOUND('',#10763,.T.);
#5499=FACE_OUTER_BOUND('',#10764,.T.);
#5500=FACE_OUTER_BOUND('',#10765,.T.);
#5501=FACE_OUTER_BOUND('',#10766,.T.);
#5502=FACE_OUTER_BOUND('',#10767,.T.);
#5503=FACE_OUTER_BOUND('',#10768,.T.);
#5504=FACE_OUTER_BOUND('',#10769,.T.);
#5505=FACE_OUTER_BOUND('',#10770,.T.);
#5506=FACE_OUTER_BOUND('',#10771,.T.);
#5507=FACE_OUTER_BOUND('',#10772,.T.);
#5508=FACE_OUTER_BOUND('',#10773,.T.);
#5509=FACE_OUTER_BOUND('',#10774,.T.);
#5510=FACE_OUTER_BOUND('',#10775,.T.);
#5511=FACE_OUTER_BOUND('',#10776,.T.);
#5512=FACE_OUTER_BOUND('',#10777,.T.);
#5513=FACE_OUTER_BOUND('',#10778,.T.);
#5514=FACE_OUTER_BOUND('',#10779,.T.);
#5515=FACE_OUTER_BOUND('',#10780,.T.);
#5516=FACE_OUTER_BOUND('',#10781,.T.);
#5517=FACE_OUTER_BOUND('',#10782,.T.);
#5518=FACE_OUTER_BOUND('',#10783,.T.);
#5519=FACE_OUTER_BOUND('',#10784,.T.);
#5520=FACE_OUTER_BOUND('',#10785,.T.);
#5521=FACE_OUTER_BOUND('',#10786,.T.);
#5522=FACE_OUTER_BOUND('',#10787,.T.);
#5523=FACE_OUTER_BOUND('',#10788,.T.);
#5524=FACE_OUTER_BOUND('',#10789,.T.);
#5525=FACE_OUTER_BOUND('',#10790,.T.);
#5526=FACE_OUTER_BOUND('',#10791,.T.);
#5527=FACE_OUTER_BOUND('',#10792,.T.);
#5528=FACE_OUTER_BOUND('',#10793,.T.);
#5529=FACE_OUTER_BOUND('',#10794,.T.);
#5530=FACE_OUTER_BOUND('',#10795,.T.);
#5531=FACE_OUTER_BOUND('',#10796,.T.);
#5532=FACE_OUTER_BOUND('',#10797,.T.);
#5533=FACE_OUTER_BOUND('',#10798,.T.);
#5534=FACE_OUTER_BOUND('',#10799,.T.);
#5535=FACE_OUTER_BOUND('',#10800,.T.);
#5536=FACE_OUTER_BOUND('',#10801,.T.);
#5537=FACE_OUTER_BOUND('',#10802,.T.);
#5538=FACE_OUTER_BOUND('',#10803,.T.);
#5539=FACE_OUTER_BOUND('',#10804,.T.);
#5540=FACE_OUTER_BOUND('',#10805,.T.);
#5541=FACE_OUTER_BOUND('',#10806,.T.);
#5542=FACE_OUTER_BOUND('',#10807,.T.);
#5543=FACE_OUTER_BOUND('',#10808,.T.);
#5544=FACE_OUTER_BOUND('',#10809,.T.);
#5545=FACE_OUTER_BOUND('',#10810,.T.);
#5546=FACE_OUTER_BOUND('',#10811,.T.);
#5547=FACE_OUTER_BOUND('',#10812,.T.);
#5548=FACE_OUTER_BOUND('',#10813,.T.);
#5549=FACE_OUTER_BOUND('',#10814,.T.);
#5550=FACE_OUTER_BOUND('',#10815,.T.);
#5551=FACE_OUTER_BOUND('',#10816,.T.);
#5552=FACE_OUTER_BOUND('',#10817,.T.);
#5553=FACE_OUTER_BOUND('',#10818,.T.);
#5554=FACE_OUTER_BOUND('',#10819,.T.);
#5555=FACE_OUTER_BOUND('',#10820,.T.);
#5556=FACE_OUTER_BOUND('',#10821,.T.);
#5557=FACE_OUTER_BOUND('',#10822,.T.);
#5558=FACE_OUTER_BOUND('',#10823,.T.);
#5559=FACE_OUTER_BOUND('',#10824,.T.);
#5560=FACE_OUTER_BOUND('',#10825,.T.);
#5561=FACE_OUTER_BOUND('',#10826,.T.);
#5562=FACE_OUTER_BOUND('',#10827,.T.);
#5563=FACE_OUTER_BOUND('',#10828,.T.);
#5564=FACE_OUTER_BOUND('',#10829,.T.);
#5565=FACE_OUTER_BOUND('',#10830,.T.);
#5566=FACE_OUTER_BOUND('',#10831,.T.);
#5567=FACE_OUTER_BOUND('',#10832,.T.);
#5568=FACE_OUTER_BOUND('',#10833,.T.);
#5569=FACE_OUTER_BOUND('',#10834,.T.);
#5570=FACE_OUTER_BOUND('',#10835,.T.);
#5571=FACE_OUTER_BOUND('',#10836,.T.);
#5572=FACE_OUTER_BOUND('',#10837,.T.);
#5573=FACE_OUTER_BOUND('',#10838,.T.);
#5574=FACE_OUTER_BOUND('',#10839,.T.);
#5575=FACE_OUTER_BOUND('',#10840,.T.);
#5576=FACE_OUTER_BOUND('',#10841,.T.);
#5577=FACE_OUTER_BOUND('',#10842,.T.);
#5578=FACE_OUTER_BOUND('',#10843,.T.);
#5579=FACE_OUTER_BOUND('',#10844,.T.);
#5580=FACE_OUTER_BOUND('',#10845,.T.);
#5581=FACE_OUTER_BOUND('',#10846,.T.);
#5582=FACE_OUTER_BOUND('',#10847,.T.);
#5583=FACE_OUTER_BOUND('',#10848,.T.);
#5584=FACE_OUTER_BOUND('',#10849,.T.);
#5585=FACE_OUTER_BOUND('',#10850,.T.);
#5586=FACE_OUTER_BOUND('',#10851,.T.);
#5587=FACE_OUTER_BOUND('',#10852,.T.);
#5588=FACE_OUTER_BOUND('',#10853,.T.);
#5589=FACE_OUTER_BOUND('',#10854,.T.);
#5590=FACE_OUTER_BOUND('',#10855,.T.);
#5591=FACE_OUTER_BOUND('',#10856,.T.);
#5592=FACE_OUTER_BOUND('',#10857,.T.);
#5593=FACE_OUTER_BOUND('',#10858,.T.);
#5594=FACE_OUTER_BOUND('',#10859,.T.);
#5595=FACE_OUTER_BOUND('',#10860,.T.);
#5596=FACE_OUTER_BOUND('',#10861,.T.);
#5597=FACE_OUTER_BOUND('',#10862,.T.);
#5598=FACE_OUTER_BOUND('',#10863,.T.);
#5599=FACE_OUTER_BOUND('',#10864,.T.);
#5600=FACE_OUTER_BOUND('',#10865,.T.);
#5601=FACE_OUTER_BOUND('',#10866,.T.);
#5602=FACE_OUTER_BOUND('',#10867,.T.);
#5603=FACE_OUTER_BOUND('',#10868,.T.);
#5604=FACE_OUTER_BOUND('',#10869,.T.);
#5605=FACE_OUTER_BOUND('',#10870,.T.);
#5606=FACE_OUTER_BOUND('',#10871,.T.);
#5607=FACE_OUTER_BOUND('',#10872,.T.);
#5608=FACE_OUTER_BOUND('',#10873,.T.);
#5609=FACE_OUTER_BOUND('',#10874,.T.);
#5610=FACE_OUTER_BOUND('',#10875,.T.);
#5611=FACE_OUTER_BOUND('',#10876,.T.);
#5612=FACE_OUTER_BOUND('',#10877,.T.);
#5613=FACE_OUTER_BOUND('',#10878,.T.);
#5614=FACE_OUTER_BOUND('',#10879,.T.);
#5615=FACE_OUTER_BOUND('',#10880,.T.);
#5616=FACE_OUTER_BOUND('',#10881,.T.);
#5617=FACE_OUTER_BOUND('',#10882,.T.);
#5618=FACE_OUTER_BOUND('',#10883,.T.);
#5619=FACE_OUTER_BOUND('',#10884,.T.);
#5620=FACE_OUTER_BOUND('',#10885,.T.);
#5621=FACE_OUTER_BOUND('',#10886,.T.);
#5622=FACE_OUTER_BOUND('',#10887,.T.);
#5623=FACE_OUTER_BOUND('',#10888,.T.);
#5624=FACE_OUTER_BOUND('',#10889,.T.);
#5625=FACE_OUTER_BOUND('',#10890,.T.);
#5626=FACE_OUTER_BOUND('',#10891,.T.);
#5627=FACE_OUTER_BOUND('',#10892,.T.);
#5628=FACE_OUTER_BOUND('',#10893,.T.);
#5629=FACE_OUTER_BOUND('',#10894,.T.);
#5630=FACE_OUTER_BOUND('',#10895,.T.);
#5631=FACE_OUTER_BOUND('',#10896,.T.);
#5632=FACE_OUTER_BOUND('',#10897,.T.);
#5633=FACE_OUTER_BOUND('',#10898,.T.);
#5634=FACE_OUTER_BOUND('',#10899,.T.);
#5635=FACE_OUTER_BOUND('',#10900,.T.);
#5636=FACE_OUTER_BOUND('',#10901,.T.);
#5637=FACE_OUTER_BOUND('',#10902,.T.);
#5638=FACE_OUTER_BOUND('',#10903,.T.);
#5639=FACE_OUTER_BOUND('',#10904,.T.);
#5640=FACE_OUTER_BOUND('',#10905,.T.);
#5641=FACE_OUTER_BOUND('',#10906,.T.);
#5642=FACE_OUTER_BOUND('',#10907,.T.);
#5643=FACE_OUTER_BOUND('',#10908,.T.);
#5644=FACE_OUTER_BOUND('',#10909,.T.);
#5645=FACE_OUTER_BOUND('',#10910,.T.);
#5646=FACE_OUTER_BOUND('',#10911,.T.);
#5647=FACE_OUTER_BOUND('',#10912,.T.);
#5648=FACE_OUTER_BOUND('',#10913,.T.);
#5649=FACE_OUTER_BOUND('',#10914,.T.);
#5650=FACE_OUTER_BOUND('',#10915,.T.);
#5651=FACE_OUTER_BOUND('',#10916,.T.);
#5652=FACE_OUTER_BOUND('',#10917,.T.);
#5653=FACE_OUTER_BOUND('',#10918,.T.);
#5654=FACE_OUTER_BOUND('',#10919,.T.);
#5655=FACE_OUTER_BOUND('',#10920,.T.);
#5656=FACE_OUTER_BOUND('',#10921,.T.);
#5657=FACE_OUTER_BOUND('',#10922,.T.);
#5658=FACE_OUTER_BOUND('',#10923,.T.);
#5659=FACE_OUTER_BOUND('',#10924,.T.);
#5660=FACE_OUTER_BOUND('',#10925,.T.);
#5661=FACE_OUTER_BOUND('',#10926,.T.);
#5662=FACE_OUTER_BOUND('',#10927,.T.);
#5663=FACE_OUTER_BOUND('',#10928,.T.);
#5664=FACE_OUTER_BOUND('',#10929,.T.);
#5665=FACE_OUTER_BOUND('',#10930,.T.);
#5666=FACE_OUTER_BOUND('',#10931,.T.);
#5667=FACE_OUTER_BOUND('',#10932,.T.);
#5668=FACE_OUTER_BOUND('',#10933,.T.);
#5669=FACE_OUTER_BOUND('',#10934,.T.);
#5670=FACE_OUTER_BOUND('',#10935,.T.);
#5671=FACE_OUTER_BOUND('',#10936,.T.);
#5672=FACE_OUTER_BOUND('',#10937,.T.);
#5673=FACE_OUTER_BOUND('',#10938,.T.);
#5674=FACE_OUTER_BOUND('',#10939,.T.);
#5675=FACE_OUTER_BOUND('',#10940,.T.);
#5676=FACE_OUTER_BOUND('',#10941,.T.);
#5677=FACE_OUTER_BOUND('',#10942,.T.);
#5678=FACE_OUTER_BOUND('',#10943,.T.);
#5679=FACE_OUTER_BOUND('',#10944,.T.);
#5680=FACE_OUTER_BOUND('',#10945,.T.);
#5681=FACE_OUTER_BOUND('',#10946,.T.);
#5682=FACE_OUTER_BOUND('',#10947,.T.);
#5683=FACE_OUTER_BOUND('',#10948,.T.);
#5684=FACE_OUTER_BOUND('',#10949,.T.);
#5685=FACE_OUTER_BOUND('',#10950,.T.);
#5686=FACE_OUTER_BOUND('',#10951,.T.);
#5687=FACE_OUTER_BOUND('',#10952,.T.);
#5688=FACE_OUTER_BOUND('',#10953,.T.);
#5689=FACE_OUTER_BOUND('',#10954,.T.);
#5690=FACE_OUTER_BOUND('',#10955,.T.);
#5691=FACE_OUTER_BOUND('',#10956,.T.);
#5692=FACE_OUTER_BOUND('',#10957,.T.);
#5693=FACE_OUTER_BOUND('',#10958,.T.);
#5694=FACE_OUTER_BOUND('',#10959,.T.);
#5695=FACE_OUTER_BOUND('',#10960,.T.);
#5696=FACE_OUTER_BOUND('',#10961,.T.);
#5697=FACE_OUTER_BOUND('',#10962,.T.);
#5698=FACE_OUTER_BOUND('',#10963,.T.);
#5699=FACE_OUTER_BOUND('',#10964,.T.);
#5700=FACE_OUTER_BOUND('',#10965,.T.);
#5701=FACE_OUTER_BOUND('',#10966,.T.);
#5702=FACE_OUTER_BOUND('',#10967,.T.);
#5703=FACE_OUTER_BOUND('',#10968,.T.);
#5704=FACE_OUTER_BOUND('',#10969,.T.);
#5705=FACE_OUTER_BOUND('',#10970,.T.);
#5706=FACE_OUTER_BOUND('',#10971,.T.);
#5707=FACE_OUTER_BOUND('',#10972,.T.);
#5708=FACE_OUTER_BOUND('',#10973,.T.);
#5709=FACE_OUTER_BOUND('',#10974,.T.);
#5710=FACE_OUTER_BOUND('',#10975,.T.);
#5711=FACE_OUTER_BOUND('',#10976,.T.);
#5712=FACE_OUTER_BOUND('',#10977,.T.);
#5713=FACE_OUTER_BOUND('',#10978,.T.);
#5714=FACE_OUTER_BOUND('',#10979,.T.);
#5715=FACE_OUTER_BOUND('',#10980,.T.);
#5716=FACE_OUTER_BOUND('',#10981,.T.);
#5717=FACE_OUTER_BOUND('',#10982,.T.);
#5718=FACE_OUTER_BOUND('',#10983,.T.);
#5719=FACE_OUTER_BOUND('',#10984,.T.);
#5720=FACE_OUTER_BOUND('',#10985,.T.);
#5721=FACE_OUTER_BOUND('',#10986,.T.);
#5722=FACE_OUTER_BOUND('',#10987,.T.);
#5723=FACE_OUTER_BOUND('',#10988,.T.);
#5724=FACE_OUTER_BOUND('',#10989,.T.);
#5725=FACE_OUTER_BOUND('',#10990,.T.);
#5726=FACE_OUTER_BOUND('',#10991,.T.);
#5727=FACE_OUTER_BOUND('',#10992,.T.);
#5728=FACE_OUTER_BOUND('',#10993,.T.);
#5729=FACE_OUTER_BOUND('',#10994,.T.);
#5730=FACE_OUTER_BOUND('',#10995,.T.);
#5731=FACE_OUTER_BOUND('',#10996,.T.);
#5732=FACE_OUTER_BOUND('',#10997,.T.);
#5733=FACE_OUTER_BOUND('',#10998,.T.);
#5734=FACE_OUTER_BOUND('',#10999,.T.);
#5735=FACE_OUTER_BOUND('',#11000,.T.);
#5736=FACE_OUTER_BOUND('',#11001,.T.);
#5737=FACE_OUTER_BOUND('',#11002,.T.);
#5738=FACE_OUTER_BOUND('',#11003,.T.);
#5739=FACE_OUTER_BOUND('',#11004,.T.);
#5740=FACE_OUTER_BOUND('',#11005,.T.);
#5741=FACE_OUTER_BOUND('',#11006,.T.);
#5742=FACE_OUTER_BOUND('',#11007,.T.);
#5743=FACE_OUTER_BOUND('',#11008,.T.);
#5744=FACE_OUTER_BOUND('',#11009,.T.);
#5745=FACE_OUTER_BOUND('',#11010,.T.);
#5746=FACE_OUTER_BOUND('',#11011,.T.);
#5747=FACE_OUTER_BOUND('',#11012,.T.);
#5748=FACE_OUTER_BOUND('',#11013,.T.);
#5749=FACE_OUTER_BOUND('',#11014,.T.);
#5750=FACE_OUTER_BOUND('',#11015,.T.);
#5751=FACE_OUTER_BOUND('',#11016,.T.);
#5752=FACE_OUTER_BOUND('',#11017,.T.);
#5753=FACE_OUTER_BOUND('',#11018,.T.);
#5754=FACE_OUTER_BOUND('',#11019,.T.);
#5755=FACE_OUTER_BOUND('',#11020,.T.);
#5756=FACE_OUTER_BOUND('',#11021,.T.);
#5757=FACE_OUTER_BOUND('',#11022,.T.);
#5758=FACE_OUTER_BOUND('',#11023,.T.);
#5759=FACE_OUTER_BOUND('',#11024,.T.);
#5760=FACE_OUTER_BOUND('',#11025,.T.);
#5761=FACE_OUTER_BOUND('',#11026,.T.);
#5762=FACE_OUTER_BOUND('',#11027,.T.);
#5763=FACE_OUTER_BOUND('',#11028,.T.);
#5764=FACE_OUTER_BOUND('',#11029,.T.);
#5765=FACE_OUTER_BOUND('',#11030,.T.);
#5766=FACE_OUTER_BOUND('',#11031,.T.);
#5767=FACE_OUTER_BOUND('',#11032,.T.);
#5768=FACE_OUTER_BOUND('',#11033,.T.);
#5769=FACE_OUTER_BOUND('',#11034,.T.);
#5770=FACE_OUTER_BOUND('',#11035,.T.);
#5771=FACE_OUTER_BOUND('',#11036,.T.);
#5772=FACE_OUTER_BOUND('',#11037,.T.);
#5773=FACE_OUTER_BOUND('',#11038,.T.);
#5774=FACE_OUTER_BOUND('',#11039,.T.);
#5775=FACE_OUTER_BOUND('',#11040,.T.);
#5776=FACE_OUTER_BOUND('',#11041,.T.);
#5777=FACE_OUTER_BOUND('',#11042,.T.);
#5778=FACE_OUTER_BOUND('',#11043,.T.);
#5779=FACE_OUTER_BOUND('',#11044,.T.);
#5780=FACE_OUTER_BOUND('',#11045,.T.);
#5781=FACE_OUTER_BOUND('',#11046,.T.);
#5782=FACE_OUTER_BOUND('',#11047,.T.);
#5783=FACE_OUTER_BOUND('',#11048,.T.);
#5784=FACE_OUTER_BOUND('',#11049,.T.);
#5785=FACE_OUTER_BOUND('',#11050,.T.);
#5786=FACE_OUTER_BOUND('',#11051,.T.);
#5787=FACE_OUTER_BOUND('',#11052,.T.);
#5788=FACE_OUTER_BOUND('',#11053,.T.);
#5789=FACE_OUTER_BOUND('',#11054,.T.);
#5790=FACE_OUTER_BOUND('',#11055,.T.);
#5791=FACE_OUTER_BOUND('',#11056,.T.);
#5792=FACE_OUTER_BOUND('',#11057,.T.);
#5793=FACE_OUTER_BOUND('',#11058,.T.);
#5794=FACE_OUTER_BOUND('',#11059,.T.);
#5795=FACE_OUTER_BOUND('',#11060,.T.);
#5796=FACE_OUTER_BOUND('',#11061,.T.);
#5797=FACE_OUTER_BOUND('',#11062,.T.);
#5798=FACE_OUTER_BOUND('',#11063,.T.);
#5799=FACE_OUTER_BOUND('',#11064,.T.);
#5800=FACE_OUTER_BOUND('',#11065,.T.);
#5801=FACE_OUTER_BOUND('',#11066,.T.);
#5802=FACE_OUTER_BOUND('',#11067,.T.);
#5803=FACE_OUTER_BOUND('',#11068,.T.);
#5804=FACE_OUTER_BOUND('',#11069,.T.);
#5805=FACE_OUTER_BOUND('',#11070,.T.);
#5806=FACE_OUTER_BOUND('',#11071,.T.);
#5807=FACE_OUTER_BOUND('',#11072,.T.);
#5808=FACE_OUTER_BOUND('',#11073,.T.);
#5809=FACE_OUTER_BOUND('',#11074,.T.);
#5810=FACE_OUTER_BOUND('',#11075,.T.);
#5811=FACE_OUTER_BOUND('',#11076,.T.);
#5812=FACE_OUTER_BOUND('',#11077,.T.);
#5813=FACE_OUTER_BOUND('',#11078,.T.);
#5814=FACE_OUTER_BOUND('',#11079,.T.);
#5815=FACE_OUTER_BOUND('',#11080,.T.);
#5816=FACE_OUTER_BOUND('',#11081,.T.);
#5817=FACE_OUTER_BOUND('',#11082,.T.);
#5818=FACE_OUTER_BOUND('',#11083,.T.);
#5819=FACE_OUTER_BOUND('',#11084,.T.);
#5820=FACE_OUTER_BOUND('',#11085,.T.);
#5821=FACE_OUTER_BOUND('',#11086,.T.);
#5822=FACE_OUTER_BOUND('',#11087,.T.);
#5823=FACE_OUTER_BOUND('',#11088,.T.);
#5824=FACE_OUTER_BOUND('',#11089,.T.);
#5825=FACE_OUTER_BOUND('',#11090,.T.);
#5826=FACE_OUTER_BOUND('',#11091,.T.);
#5827=FACE_OUTER_BOUND('',#11092,.T.);
#5828=FACE_OUTER_BOUND('',#11093,.T.);
#5829=FACE_OUTER_BOUND('',#11094,.T.);
#5830=FACE_OUTER_BOUND('',#11095,.T.);
#5831=FACE_OUTER_BOUND('',#11096,.T.);
#5832=FACE_OUTER_BOUND('',#11097,.T.);
#5833=FACE_OUTER_BOUND('',#11098,.T.);
#5834=FACE_OUTER_BOUND('',#11099,.T.);
#5835=FACE_OUTER_BOUND('',#11100,.T.);
#5836=FACE_OUTER_BOUND('',#11101,.T.);
#5837=FACE_OUTER_BOUND('',#11102,.T.);
#5838=FACE_OUTER_BOUND('',#11103,.T.);
#5839=FACE_OUTER_BOUND('',#11104,.T.);
#5840=FACE_OUTER_BOUND('',#11105,.T.);
#5841=FACE_OUTER_BOUND('',#11106,.T.);
#5842=FACE_OUTER_BOUND('',#11107,.T.);
#5843=FACE_OUTER_BOUND('',#11108,.T.);
#5844=FACE_OUTER_BOUND('',#11109,.T.);
#5845=FACE_OUTER_BOUND('',#11110,.T.);
#5846=FACE_OUTER_BOUND('',#11111,.T.);
#5847=FACE_OUTER_BOUND('',#11112,.T.);
#5848=FACE_OUTER_BOUND('',#11113,.T.);
#5849=FACE_OUTER_BOUND('',#11114,.T.);
#5850=FACE_OUTER_BOUND('',#11115,.T.);
#5851=FACE_OUTER_BOUND('',#11116,.T.);
#5852=FACE_OUTER_BOUND('',#11117,.T.);
#5853=FACE_OUTER_BOUND('',#11118,.T.);
#5854=FACE_OUTER_BOUND('',#11119,.T.);
#5855=FACE_OUTER_BOUND('',#11120,.T.);
#5856=FACE_OUTER_BOUND('',#11121,.T.);
#5857=FACE_OUTER_BOUND('',#11122,.T.);
#5858=FACE_OUTER_BOUND('',#11123,.T.);
#5859=FACE_OUTER_BOUND('',#11124,.T.);
#5860=FACE_OUTER_BOUND('',#11125,.T.);
#5861=FACE_OUTER_BOUND('',#11126,.T.);
#5862=FACE_OUTER_BOUND('',#11127,.T.);
#5863=FACE_OUTER_BOUND('',#11128,.T.);
#5864=FACE_OUTER_BOUND('',#11129,.T.);
#5865=FACE_OUTER_BOUND('',#11130,.T.);
#5866=FACE_OUTER_BOUND('',#11131,.T.);
#5867=FACE_OUTER_BOUND('',#11132,.T.);
#5868=FACE_OUTER_BOUND('',#11133,.T.);
#5869=FACE_OUTER_BOUND('',#11134,.T.);
#5870=FACE_OUTER_BOUND('',#11135,.T.);
#5871=FACE_OUTER_BOUND('',#11136,.T.);
#5872=FACE_OUTER_BOUND('',#11137,.T.);
#5873=FACE_OUTER_BOUND('',#11138,.T.);
#5874=FACE_OUTER_BOUND('',#11139,.T.);
#5875=FACE_OUTER_BOUND('',#11140,.T.);
#5876=FACE_OUTER_BOUND('',#11141,.T.);
#5877=FACE_OUTER_BOUND('',#11142,.T.);
#5878=FACE_OUTER_BOUND('',#11143,.T.);
#5879=FACE_OUTER_BOUND('',#11144,.T.);
#5880=FACE_OUTER_BOUND('',#11145,.T.);
#5881=FACE_OUTER_BOUND('',#11146,.T.);
#5882=FACE_OUTER_BOUND('',#11147,.T.);
#5883=FACE_OUTER_BOUND('',#11148,.T.);
#5884=FACE_OUTER_BOUND('',#11149,.T.);
#5885=FACE_OUTER_BOUND('',#11150,.T.);
#5886=FACE_OUTER_BOUND('',#11151,.T.);
#5887=FACE_OUTER_BOUND('',#11152,.T.);
#5888=FACE_OUTER_BOUND('',#11153,.T.);
#5889=FACE_OUTER_BOUND('',#11154,.T.);
#5890=FACE_OUTER_BOUND('',#11155,.T.);
#5891=FACE_OUTER_BOUND('',#11156,.T.);
#5892=FACE_OUTER_BOUND('',#11157,.T.);
#5893=FACE_OUTER_BOUND('',#11158,.T.);
#5894=FACE_OUTER_BOUND('',#11159,.T.);
#5895=FACE_OUTER_BOUND('',#11160,.T.);
#5896=FACE_OUTER_BOUND('',#11161,.T.);
#5897=FACE_OUTER_BOUND('',#11162,.T.);
#5898=FACE_OUTER_BOUND('',#11163,.T.);
#5899=FACE_OUTER_BOUND('',#11164,.T.);
#5900=FACE_OUTER_BOUND('',#11165,.T.);
#5901=FACE_OUTER_BOUND('',#11166,.T.);
#5902=FACE_OUTER_BOUND('',#11167,.T.);
#5903=FACE_OUTER_BOUND('',#11168,.T.);
#5904=FACE_OUTER_BOUND('',#11169,.T.);
#5905=FACE_OUTER_BOUND('',#11170,.T.);
#5906=FACE_OUTER_BOUND('',#11171,.T.);
#5907=FACE_OUTER_BOUND('',#11172,.T.);
#5908=FACE_OUTER_BOUND('',#11173,.T.);
#5909=FACE_OUTER_BOUND('',#11174,.T.);
#5910=FACE_OUTER_BOUND('',#11175,.T.);
#5911=FACE_OUTER_BOUND('',#11176,.T.);
#5912=FACE_OUTER_BOUND('',#11177,.T.);
#5913=FACE_OUTER_BOUND('',#11178,.T.);
#5914=FACE_OUTER_BOUND('',#11179,.T.);
#5915=FACE_OUTER_BOUND('',#11180,.T.);
#5916=FACE_OUTER_BOUND('',#11181,.T.);
#5917=FACE_OUTER_BOUND('',#11182,.T.);
#5918=FACE_OUTER_BOUND('',#11183,.T.);
#5919=FACE_OUTER_BOUND('',#11184,.T.);
#5920=FACE_OUTER_BOUND('',#11185,.T.);
#5921=FACE_OUTER_BOUND('',#11186,.T.);
#5922=FACE_OUTER_BOUND('',#11187,.T.);
#5923=FACE_OUTER_BOUND('',#11188,.T.);
#5924=FACE_OUTER_BOUND('',#11189,.T.);
#5925=FACE_OUTER_BOUND('',#11190,.T.);
#5926=FACE_OUTER_BOUND('',#11191,.T.);
#5927=FACE_OUTER_BOUND('',#11192,.T.);
#5928=FACE_OUTER_BOUND('',#11193,.T.);
#5929=FACE_OUTER_BOUND('',#11194,.T.);
#5930=FACE_OUTER_BOUND('',#11195,.T.);
#5931=FACE_OUTER_BOUND('',#11196,.T.);
#5932=FACE_OUTER_BOUND('',#11197,.T.);
#5933=FACE_OUTER_BOUND('',#11198,.T.);
#5934=FACE_OUTER_BOUND('',#11199,.T.);
#5935=FACE_OUTER_BOUND('',#11200,.T.);
#5936=FACE_OUTER_BOUND('',#11201,.T.);
#5937=FACE_OUTER_BOUND('',#11202,.T.);
#5938=FACE_OUTER_BOUND('',#11203,.T.);
#5939=FACE_OUTER_BOUND('',#11204,.T.);
#5940=FACE_OUTER_BOUND('',#11205,.T.);
#5941=FACE_OUTER_BOUND('',#11206,.T.);
#5942=FACE_OUTER_BOUND('',#11207,.T.);
#5943=FACE_OUTER_BOUND('',#11208,.T.);
#5944=FACE_OUTER_BOUND('',#11209,.T.);
#5945=FACE_OUTER_BOUND('',#11210,.T.);
#5946=FACE_OUTER_BOUND('',#11211,.T.);
#5947=FACE_OUTER_BOUND('',#11212,.T.);
#5948=FACE_OUTER_BOUND('',#11213,.T.);
#5949=FACE_OUTER_BOUND('',#11214,.T.);
#5950=FACE_OUTER_BOUND('',#11215,.T.);
#5951=FACE_OUTER_BOUND('',#11216,.T.);
#5952=FACE_OUTER_BOUND('',#11217,.T.);
#5953=FACE_OUTER_BOUND('',#11218,.T.);
#5954=FACE_OUTER_BOUND('',#11219,.T.);
#5955=FACE_OUTER_BOUND('',#11220,.T.);
#5956=FACE_OUTER_BOUND('',#11221,.T.);
#5957=FACE_OUTER_BOUND('',#11222,.T.);
#5958=FACE_OUTER_BOUND('',#11223,.T.);
#5959=FACE_OUTER_BOUND('',#11224,.T.);
#5960=FACE_OUTER_BOUND('',#11225,.T.);
#5961=FACE_OUTER_BOUND('',#11226,.T.);
#5962=FACE_OUTER_BOUND('',#11227,.T.);
#5963=FACE_OUTER_BOUND('',#11228,.T.);
#5964=FACE_OUTER_BOUND('',#11229,.T.);
#5965=FACE_OUTER_BOUND('',#11230,.T.);
#5966=FACE_OUTER_BOUND('',#11231,.T.);
#5967=FACE_OUTER_BOUND('',#11232,.T.);
#5968=FACE_OUTER_BOUND('',#11233,.T.);
#5969=FACE_OUTER_BOUND('',#11234,.T.);
#5970=FACE_OUTER_BOUND('',#11235,.T.);
#5971=FACE_OUTER_BOUND('',#11236,.T.);
#5972=FACE_OUTER_BOUND('',#11237,.T.);
#5973=FACE_OUTER_BOUND('',#11238,.T.);
#5974=FACE_OUTER_BOUND('',#11239,.T.);
#5975=FACE_OUTER_BOUND('',#11240,.T.);
#5976=FACE_OUTER_BOUND('',#11241,.T.);
#5977=FACE_OUTER_BOUND('',#11242,.T.);
#5978=FACE_OUTER_BOUND('',#11243,.T.);
#5979=FACE_OUTER_BOUND('',#11244,.T.);
#5980=FACE_OUTER_BOUND('',#11245,.T.);
#5981=FACE_OUTER_BOUND('',#11246,.T.);
#5982=FACE_OUTER_BOUND('',#11247,.T.);
#5983=FACE_OUTER_BOUND('',#11248,.T.);
#5984=FACE_OUTER_BOUND('',#11249,.T.);
#5985=FACE_OUTER_BOUND('',#11250,.T.);
#5986=FACE_OUTER_BOUND('',#11251,.T.);
#5987=FACE_OUTER_BOUND('',#11252,.T.);
#5988=FACE_OUTER_BOUND('',#11253,.T.);
#5989=FACE_OUTER_BOUND('',#11254,.T.);
#5990=FACE_OUTER_BOUND('',#11255,.T.);
#5991=FACE_OUTER_BOUND('',#11256,.T.);
#5992=FACE_OUTER_BOUND('',#11257,.T.);
#5993=FACE_OUTER_BOUND('',#11258,.T.);
#5994=FACE_OUTER_BOUND('',#11259,.T.);
#5995=FACE_OUTER_BOUND('',#11260,.T.);
#5996=FACE_OUTER_BOUND('',#11261,.T.);
#5997=FACE_OUTER_BOUND('',#11262,.T.);
#5998=FACE_OUTER_BOUND('',#11263,.T.);
#5999=FACE_OUTER_BOUND('',#11264,.T.);
#6000=FACE_OUTER_BOUND('',#11265,.T.);
#6001=FACE_OUTER_BOUND('',#11266,.T.);
#6002=FACE_OUTER_BOUND('',#11267,.T.);
#6003=FACE_OUTER_BOUND('',#11268,.T.);
#6004=FACE_OUTER_BOUND('',#11269,.T.);
#6005=FACE_OUTER_BOUND('',#11270,.T.);
#6006=FACE_OUTER_BOUND('',#11271,.T.);
#6007=FACE_OUTER_BOUND('',#11272,.T.);
#6008=FACE_OUTER_BOUND('',#11273,.T.);
#6009=FACE_OUTER_BOUND('',#11274,.T.);
#6010=FACE_OUTER_BOUND('',#11275,.T.);
#6011=FACE_OUTER_BOUND('',#11276,.T.);
#6012=FACE_OUTER_BOUND('',#11277,.T.);
#6013=FACE_OUTER_BOUND('',#11278,.T.);
#6014=FACE_OUTER_BOUND('',#11279,.T.);
#6015=FACE_OUTER_BOUND('',#11280,.T.);
#6016=FACE_OUTER_BOUND('',#11281,.T.);
#6017=FACE_OUTER_BOUND('',#11282,.T.);
#6018=FACE_OUTER_BOUND('',#11283,.T.);
#6019=FACE_OUTER_BOUND('',#11284,.T.);
#6020=FACE_OUTER_BOUND('',#11285,.T.);
#6021=FACE_OUTER_BOUND('',#11286,.T.);
#6022=FACE_OUTER_BOUND('',#11287,.T.);
#6023=FACE_OUTER_BOUND('',#11288,.T.);
#6024=FACE_OUTER_BOUND('',#11289,.T.);
#6025=FACE_OUTER_BOUND('',#11290,.T.);
#6026=FACE_OUTER_BOUND('',#11291,.T.);
#6027=FACE_OUTER_BOUND('',#11292,.T.);
#6028=FACE_OUTER_BOUND('',#11293,.T.);
#6029=FACE_OUTER_BOUND('',#11294,.T.);
#6030=FACE_OUTER_BOUND('',#11295,.T.);
#6031=FACE_OUTER_BOUND('',#11296,.T.);
#6032=FACE_OUTER_BOUND('',#11297,.T.);
#6033=FACE_OUTER_BOUND('',#11298,.T.);
#6034=FACE_OUTER_BOUND('',#11299,.T.);
#6035=FACE_OUTER_BOUND('',#11300,.T.);
#6036=FACE_OUTER_BOUND('',#11301,.T.);
#6037=FACE_OUTER_BOUND('',#11302,.T.);
#6038=FACE_OUTER_BOUND('',#11303,.T.);
#6039=FACE_OUTER_BOUND('',#11304,.T.);
#6040=FACE_OUTER_BOUND('',#11305,.T.);
#6041=FACE_OUTER_BOUND('',#11306,.T.);
#6042=FACE_OUTER_BOUND('',#11307,.T.);
#6043=FACE_OUTER_BOUND('',#11308,.T.);
#6044=FACE_OUTER_BOUND('',#11309,.T.);
#6045=FACE_OUTER_BOUND('',#11310,.T.);
#6046=FACE_OUTER_BOUND('',#11311,.T.);
#6047=FACE_OUTER_BOUND('',#11312,.T.);
#6048=FACE_OUTER_BOUND('',#11313,.T.);
#6049=FACE_OUTER_BOUND('',#11314,.T.);
#6050=FACE_OUTER_BOUND('',#11315,.T.);
#6051=FACE_OUTER_BOUND('',#11316,.T.);
#6052=FACE_OUTER_BOUND('',#11317,.T.);
#6053=FACE_OUTER_BOUND('',#11318,.T.);
#6054=FACE_OUTER_BOUND('',#11319,.T.);
#6055=FACE_OUTER_BOUND('',#11320,.T.);
#6056=FACE_OUTER_BOUND('',#11321,.T.);
#6057=FACE_OUTER_BOUND('',#11322,.T.);
#6058=FACE_OUTER_BOUND('',#11323,.T.);
#6059=FACE_OUTER_BOUND('',#11324,.T.);
#6060=FACE_OUTER_BOUND('',#11325,.T.);
#6061=FACE_OUTER_BOUND('',#11326,.T.);
#6062=FACE_OUTER_BOUND('',#11327,.T.);
#6063=FACE_OUTER_BOUND('',#11328,.T.);
#6064=FACE_OUTER_BOUND('',#11329,.T.);
#6065=FACE_OUTER_BOUND('',#11330,.T.);
#6066=FACE_OUTER_BOUND('',#11331,.T.);
#6067=FACE_OUTER_BOUND('',#11332,.T.);
#6068=FACE_OUTER_BOUND('',#11333,.T.);
#6069=FACE_OUTER_BOUND('',#11334,.T.);
#6070=FACE_OUTER_BOUND('',#11335,.T.);
#6071=FACE_OUTER_BOUND('',#11336,.T.);
#6072=FACE_OUTER_BOUND('',#11337,.T.);
#6073=FACE_OUTER_BOUND('',#11338,.T.);
#6074=FACE_OUTER_BOUND('',#11339,.T.);
#6075=FACE_OUTER_BOUND('',#11340,.T.);
#6076=FACE_OUTER_BOUND('',#11341,.T.);
#6077=FACE_OUTER_BOUND('',#11342,.T.);
#6078=FACE_OUTER_BOUND('',#11343,.T.);
#6079=FACE_OUTER_BOUND('',#11344,.T.);
#6080=FACE_OUTER_BOUND('',#11345,.T.);
#6081=FACE_OUTER_BOUND('',#11346,.T.);
#6082=FACE_OUTER_BOUND('',#11347,.T.);
#6083=FACE_OUTER_BOUND('',#11348,.T.);
#6084=FACE_OUTER_BOUND('',#11349,.T.);
#6085=FACE_OUTER_BOUND('',#11350,.T.);
#6086=FACE_OUTER_BOUND('',#11351,.T.);
#6087=FACE_OUTER_BOUND('',#11352,.T.);
#6088=FACE_OUTER_BOUND('',#11353,.T.);
#6089=FACE_OUTER_BOUND('',#11354,.T.);
#6090=FACE_OUTER_BOUND('',#11355,.T.);
#6091=FACE_OUTER_BOUND('',#11356,.T.);
#6092=FACE_OUTER_BOUND('',#11357,.T.);
#6093=FACE_OUTER_BOUND('',#11358,.T.);
#6094=FACE_OUTER_BOUND('',#11359,.T.);
#6095=FACE_OUTER_BOUND('',#11360,.T.);
#6096=FACE_OUTER_BOUND('',#11361,.T.);
#6097=FACE_OUTER_BOUND('',#11362,.T.);
#6098=FACE_OUTER_BOUND('',#11363,.T.);
#6099=FACE_OUTER_BOUND('',#11364,.T.);
#6100=FACE_OUTER_BOUND('',#11365,.T.);
#6101=FACE_OUTER_BOUND('',#11366,.T.);
#6102=FACE_OUTER_BOUND('',#11367,.T.);
#6103=FACE_OUTER_BOUND('',#11368,.T.);
#6104=FACE_OUTER_BOUND('',#11369,.T.);
#6105=FACE_OUTER_BOUND('',#11370,.T.);
#6106=FACE_OUTER_BOUND('',#11371,.T.);
#6107=FACE_OUTER_BOUND('',#11372,.T.);
#6108=FACE_OUTER_BOUND('',#11373,.T.);
#6109=FACE_OUTER_BOUND('',#11374,.T.);
#6110=FACE_OUTER_BOUND('',#11375,.T.);
#6111=FACE_OUTER_BOUND('',#11376,.T.);
#6112=FACE_OUTER_BOUND('',#11377,.T.);
#6113=FACE_OUTER_BOUND('',#11378,.T.);
#6114=FACE_OUTER_BOUND('',#11379,.T.);
#6115=FACE_OUTER_BOUND('',#11380,.T.);
#6116=FACE_OUTER_BOUND('',#11381,.T.);
#6117=FACE_OUTER_BOUND('',#11382,.T.);
#6118=FACE_OUTER_BOUND('',#11383,.T.);
#6119=FACE_OUTER_BOUND('',#11384,.T.);
#6120=FACE_OUTER_BOUND('',#11385,.T.);
#6121=FACE_OUTER_BOUND('',#11386,.T.);
#6122=FACE_OUTER_BOUND('',#11387,.T.);
#6123=FACE_OUTER_BOUND('',#11388,.T.);
#6124=FACE_OUTER_BOUND('',#11389,.T.);
#6125=FACE_OUTER_BOUND('',#11390,.T.);
#6126=FACE_OUTER_BOUND('',#11391,.T.);
#6127=FACE_OUTER_BOUND('',#11392,.T.);
#6128=FACE_OUTER_BOUND('',#11393,.T.);
#6129=FACE_OUTER_BOUND('',#11394,.T.);
#6130=FACE_OUTER_BOUND('',#11395,.T.);
#6131=FACE_OUTER_BOUND('',#11396,.T.);
#6132=FACE_OUTER_BOUND('',#11397,.T.);
#6133=FACE_OUTER_BOUND('',#11398,.T.);
#6134=FACE_OUTER_BOUND('',#11399,.T.);
#6135=FACE_OUTER_BOUND('',#11400,.T.);
#6136=FACE_OUTER_BOUND('',#11401,.T.);
#6137=FACE_OUTER_BOUND('',#11402,.T.);
#6138=FACE_OUTER_BOUND('',#11403,.T.);
#6139=FACE_OUTER_BOUND('',#11404,.T.);
#6140=FACE_OUTER_BOUND('',#11405,.T.);
#6141=FACE_OUTER_BOUND('',#11406,.T.);
#6142=FACE_OUTER_BOUND('',#11407,.T.);
#6143=FACE_OUTER_BOUND('',#11408,.T.);
#6144=FACE_OUTER_BOUND('',#11409,.T.);
#6145=FACE_OUTER_BOUND('',#11410,.T.);
#6146=FACE_OUTER_BOUND('',#11411,.T.);
#6147=FACE_OUTER_BOUND('',#11412,.T.);
#6148=FACE_OUTER_BOUND('',#11413,.T.);
#6149=FACE_OUTER_BOUND('',#11414,.T.);
#6150=FACE_OUTER_BOUND('',#11415,.T.);
#6151=FACE_OUTER_BOUND('',#11416,.T.);
#6152=FACE_OUTER_BOUND('',#11417,.T.);
#6153=FACE_OUTER_BOUND('',#11418,.T.);
#6154=FACE_OUTER_BOUND('',#11419,.T.);
#6155=FACE_OUTER_BOUND('',#11420,.T.);
#6156=FACE_OUTER_BOUND('',#11421,.T.);
#6157=FACE_OUTER_BOUND('',#11422,.T.);
#6158=FACE_OUTER_BOUND('',#11423,.T.);
#6159=FACE_OUTER_BOUND('',#11424,.T.);
#6160=FACE_OUTER_BOUND('',#11425,.T.);
#6161=FACE_OUTER_BOUND('',#11426,.T.);
#6162=FACE_OUTER_BOUND('',#11427,.T.);
#6163=FACE_OUTER_BOUND('',#11428,.T.);
#6164=FACE_OUTER_BOUND('',#11429,.T.);
#6165=FACE_OUTER_BOUND('',#11430,.T.);
#6166=FACE_OUTER_BOUND('',#11431,.T.);
#6167=FACE_OUTER_BOUND('',#11432,.T.);
#6168=FACE_OUTER_BOUND('',#11433,.T.);
#6169=FACE_OUTER_BOUND('',#11434,.T.);
#6170=FACE_OUTER_BOUND('',#11435,.T.);
#6171=FACE_OUTER_BOUND('',#11436,.T.);
#6172=FACE_OUTER_BOUND('',#11437,.T.);
#6173=FACE_OUTER_BOUND('',#11438,.T.);
#6174=FACE_OUTER_BOUND('',#11439,.T.);
#6175=FACE_OUTER_BOUND('',#11440,.T.);
#6176=FACE_OUTER_BOUND('',#11441,.T.);
#6177=FACE_OUTER_BOUND('',#11442,.T.);
#6178=FACE_OUTER_BOUND('',#11443,.T.);
#6179=FACE_OUTER_BOUND('',#11444,.T.);
#6180=FACE_OUTER_BOUND('',#11445,.T.);
#6181=FACE_OUTER_BOUND('',#11446,.T.);
#6182=FACE_OUTER_BOUND('',#11447,.T.);
#6183=FACE_OUTER_BOUND('',#11448,.T.);
#6184=FACE_OUTER_BOUND('',#11449,.T.);
#6185=FACE_OUTER_BOUND('',#11450,.T.);
#6186=FACE_OUTER_BOUND('',#11451,.T.);
#6187=FACE_OUTER_BOUND('',#11452,.T.);
#6188=FACE_OUTER_BOUND('',#11453,.T.);
#6189=FACE_OUTER_BOUND('',#11454,.T.);
#6190=FACE_OUTER_BOUND('',#11455,.T.);
#6191=FACE_OUTER_BOUND('',#11456,.T.);
#6192=FACE_OUTER_BOUND('',#11457,.T.);
#6193=FACE_OUTER_BOUND('',#11458,.T.);
#6194=FACE_OUTER_BOUND('',#11459,.T.);
#6195=FACE_OUTER_BOUND('',#11460,.T.);
#6196=FACE_OUTER_BOUND('',#11461,.T.);
#6197=FACE_OUTER_BOUND('',#11462,.T.);
#6198=FACE_OUTER_BOUND('',#11463,.T.);
#6199=FACE_OUTER_BOUND('',#11464,.T.);
#6200=FACE_OUTER_BOUND('',#11465,.T.);
#6201=FACE_OUTER_BOUND('',#11466,.T.);
#6202=FACE_OUTER_BOUND('',#11467,.T.);
#6203=FACE_OUTER_BOUND('',#11468,.T.);
#6204=FACE_OUTER_BOUND('',#11469,.T.);
#6205=FACE_OUTER_BOUND('',#11470,.T.);
#6206=FACE_OUTER_BOUND('',#11471,.T.);
#6207=FACE_OUTER_BOUND('',#11472,.T.);
#6208=FACE_OUTER_BOUND('',#11473,.T.);
#6209=FACE_OUTER_BOUND('',#11474,.T.);
#6210=FACE_OUTER_BOUND('',#11475,.T.);
#6211=FACE_OUTER_BOUND('',#11476,.T.);
#6212=FACE_OUTER_BOUND('',#11477,.T.);
#6213=FACE_OUTER_BOUND('',#11478,.T.);
#6214=FACE_OUTER_BOUND('',#11479,.T.);
#6215=FACE_OUTER_BOUND('',#11480,.T.);
#6216=FACE_OUTER_BOUND('',#11481,.T.);
#6217=FACE_OUTER_BOUND('',#11482,.T.);
#6218=FACE_OUTER_BOUND('',#11483,.T.);
#6219=FACE_OUTER_BOUND('',#11484,.T.);
#6220=FACE_OUTER_BOUND('',#11485,.T.);
#6221=FACE_OUTER_BOUND('',#11486,.T.);
#6222=FACE_OUTER_BOUND('',#11487,.T.);
#6223=FACE_OUTER_BOUND('',#11488,.T.);
#6224=FACE_OUTER_BOUND('',#11489,.T.);
#6225=FACE_OUTER_BOUND('',#11490,.T.);
#6226=FACE_OUTER_BOUND('',#11491,.T.);
#6227=FACE_OUTER_BOUND('',#11492,.T.);
#6228=FACE_OUTER_BOUND('',#11493,.T.);
#6229=FACE_OUTER_BOUND('',#11494,.T.);
#6230=FACE_OUTER_BOUND('',#11495,.T.);
#6231=FACE_OUTER_BOUND('',#11496,.T.);
#6232=FACE_OUTER_BOUND('',#11497,.T.);
#6233=FACE_OUTER_BOUND('',#11498,.T.);
#6234=FACE_OUTER_BOUND('',#11499,.T.);
#6235=FACE_OUTER_BOUND('',#11500,.T.);
#6236=FACE_OUTER_BOUND('',#11501,.T.);
#6237=FACE_OUTER_BOUND('',#11502,.T.);
#6238=FACE_OUTER_BOUND('',#11503,.T.);
#6239=FACE_OUTER_BOUND('',#11504,.T.);
#6240=FACE_OUTER_BOUND('',#11505,.T.);
#6241=FACE_OUTER_BOUND('',#11506,.T.);
#6242=FACE_OUTER_BOUND('',#11507,.T.);
#6243=FACE_OUTER_BOUND('',#11508,.T.);
#6244=FACE_OUTER_BOUND('',#11509,.T.);
#6245=FACE_OUTER_BOUND('',#11510,.T.);
#6246=FACE_OUTER_BOUND('',#11511,.T.);
#6247=FACE_OUTER_BOUND('',#11512,.T.);
#6248=FACE_OUTER_BOUND('',#11513,.T.);
#6249=FACE_OUTER_BOUND('',#11514,.T.);
#6250=FACE_OUTER_BOUND('',#11515,.T.);
#6251=FACE_OUTER_BOUND('',#11516,.T.);
#6252=FACE_OUTER_BOUND('',#11517,.T.);
#6253=FACE_OUTER_BOUND('',#11518,.T.);
#6254=FACE_OUTER_BOUND('',#11519,.T.);
#6255=FACE_OUTER_BOUND('',#11520,.T.);
#6256=FACE_OUTER_BOUND('',#11521,.T.);
#6257=FACE_OUTER_BOUND('',#11522,.T.);
#6258=FACE_OUTER_BOUND('',#11523,.T.);
#6259=FACE_OUTER_BOUND('',#11524,.T.);
#6260=FACE_OUTER_BOUND('',#11525,.T.);
#6261=FACE_OUTER_BOUND('',#11526,.T.);
#6262=FACE_OUTER_BOUND('',#11527,.T.);
#6263=FACE_OUTER_BOUND('',#11528,.T.);
#6264=FACE_OUTER_BOUND('',#11529,.T.);
#6265=FACE_OUTER_BOUND('',#11530,.T.);
#6266=FACE_OUTER_BOUND('',#11531,.T.);
#6267=FACE_OUTER_BOUND('',#11532,.T.);
#6268=FACE_OUTER_BOUND('',#11533,.T.);
#6269=FACE_OUTER_BOUND('',#11534,.T.);
#6270=FACE_OUTER_BOUND('',#11535,.T.);
#6271=FACE_OUTER_BOUND('',#11536,.T.);
#6272=FACE_OUTER_BOUND('',#11537,.T.);
#6273=FACE_OUTER_BOUND('',#11538,.T.);
#6274=FACE_OUTER_BOUND('',#11539,.T.);
#6275=FACE_OUTER_BOUND('',#11540,.T.);
#6276=FACE_OUTER_BOUND('',#11541,.T.);
#6277=FACE_OUTER_BOUND('',#11542,.T.);
#6278=FACE_OUTER_BOUND('',#11543,.T.);
#6279=FACE_OUTER_BOUND('',#11544,.T.);
#6280=FACE_OUTER_BOUND('',#11545,.T.);
#6281=FACE_OUTER_BOUND('',#11546,.T.);
#6282=FACE_OUTER_BOUND('',#11547,.T.);
#6283=FACE_OUTER_BOUND('',#11548,.T.);
#6284=FACE_OUTER_BOUND('',#11549,.T.);
#6285=FACE_OUTER_BOUND('',#11550,.T.);
#6286=FACE_OUTER_BOUND('',#11551,.T.);
#6287=FACE_OUTER_BOUND('',#11552,.T.);
#6288=FACE_OUTER_BOUND('',#11553,.T.);
#6289=FACE_OUTER_BOUND('',#11554,.T.);
#6290=FACE_OUTER_BOUND('',#11555,.T.);
#6291=FACE_OUTER_BOUND('',#11556,.T.);
#6292=FACE_OUTER_BOUND('',#11557,.T.);
#6293=FACE_OUTER_BOUND('',#11558,.T.);
#6294=FACE_OUTER_BOUND('',#11559,.T.);
#6295=FACE_OUTER_BOUND('',#11560,.T.);
#6296=FACE_OUTER_BOUND('',#11561,.T.);
#6297=FACE_OUTER_BOUND('',#11562,.T.);
#6298=FACE_OUTER_BOUND('',#11563,.T.);
#6299=FACE_OUTER_BOUND('',#11564,.T.);
#6300=FACE_OUTER_BOUND('',#11565,.T.);
#6301=FACE_OUTER_BOUND('',#11566,.T.);
#6302=FACE_OUTER_BOUND('',#11567,.T.);
#6303=FACE_OUTER_BOUND('',#11568,.T.);
#6304=FACE_OUTER_BOUND('',#11569,.T.);
#6305=FACE_OUTER_BOUND('',#11570,.T.);
#6306=FACE_OUTER_BOUND('',#11571,.T.);
#6307=FACE_OUTER_BOUND('',#11572,.T.);
#6308=FACE_OUTER_BOUND('',#11573,.T.);
#6309=FACE_OUTER_BOUND('',#11574,.T.);
#6310=FACE_OUTER_BOUND('',#11575,.T.);
#6311=FACE_OUTER_BOUND('',#11576,.T.);
#6312=FACE_OUTER_BOUND('',#11577,.T.);
#6313=FACE_OUTER_BOUND('',#11578,.T.);
#6314=FACE_OUTER_BOUND('',#11579,.T.);
#6315=FACE_OUTER_BOUND('',#11580,.T.);
#6316=FACE_OUTER_BOUND('',#11581,.T.);
#6317=FACE_OUTER_BOUND('',#11582,.T.);
#6318=FACE_OUTER_BOUND('',#11583,.T.);
#6319=FACE_OUTER_BOUND('',#11584,.T.);
#6320=FACE_OUTER_BOUND('',#11585,.T.);
#6321=FACE_OUTER_BOUND('',#11586,.T.);
#6322=FACE_OUTER_BOUND('',#11587,.T.);
#6323=FACE_OUTER_BOUND('',#11588,.T.);
#6324=FACE_OUTER_BOUND('',#11589,.T.);
#6325=FACE_OUTER_BOUND('',#11590,.T.);
#6326=FACE_OUTER_BOUND('',#11591,.T.);
#6327=FACE_OUTER_BOUND('',#11592,.T.);
#6328=FACE_OUTER_BOUND('',#11593,.T.);
#6329=FACE_OUTER_BOUND('',#11594,.T.);
#6330=FACE_OUTER_BOUND('',#11595,.T.);
#6331=FACE_OUTER_BOUND('',#11596,.T.);
#6332=FACE_OUTER_BOUND('',#11597,.T.);
#6333=FACE_OUTER_BOUND('',#11598,.T.);
#6334=FACE_OUTER_BOUND('',#11599,.T.);
#6335=FACE_OUTER_BOUND('',#11600,.T.);
#6336=FACE_OUTER_BOUND('',#11601,.T.);
#6337=FACE_OUTER_BOUND('',#11602,.T.);
#6338=FACE_OUTER_BOUND('',#11603,.T.);
#6339=FACE_OUTER_BOUND('',#11604,.T.);
#6340=FACE_OUTER_BOUND('',#11605,.T.);
#6341=FACE_OUTER_BOUND('',#11606,.T.);
#6342=FACE_OUTER_BOUND('',#11607,.T.);
#6343=FACE_OUTER_BOUND('',#11608,.T.);
#6344=FACE_OUTER_BOUND('',#11609,.T.);
#6345=FACE_OUTER_BOUND('',#11610,.T.);
#6346=FACE_OUTER_BOUND('',#11611,.T.);
#6347=FACE_OUTER_BOUND('',#11612,.T.);
#6348=FACE_OUTER_BOUND('',#11613,.T.);
#6349=FACE_OUTER_BOUND('',#11614,.T.);
#6350=FACE_OUTER_BOUND('',#11615,.T.);
#6351=FACE_OUTER_BOUND('',#11616,.T.);
#6352=FACE_OUTER_BOUND('',#11617,.T.);
#6353=FACE_OUTER_BOUND('',#11618,.T.);
#6354=FACE_OUTER_BOUND('',#11619,.T.);
#6355=FACE_OUTER_BOUND('',#11620,.T.);
#6356=FACE_OUTER_BOUND('',#11621,.T.);
#6357=FACE_OUTER_BOUND('',#11622,.T.);
#6358=FACE_OUTER_BOUND('',#11623,.T.);
#6359=FACE_OUTER_BOUND('',#11624,.T.);
#6360=FACE_OUTER_BOUND('',#11625,.T.);
#6361=FACE_OUTER_BOUND('',#11626,.T.);
#6362=FACE_OUTER_BOUND('',#11627,.T.);
#6363=FACE_OUTER_BOUND('',#11628,.T.);
#6364=FACE_OUTER_BOUND('',#11629,.T.);
#6365=FACE_OUTER_BOUND('',#11630,.T.);
#6366=FACE_OUTER_BOUND('',#11631,.T.);
#6367=FACE_OUTER_BOUND('',#11632,.T.);
#6368=FACE_OUTER_BOUND('',#11633,.T.);
#6369=FACE_OUTER_BOUND('',#11634,.T.);
#6370=FACE_OUTER_BOUND('',#11635,.T.);
#6371=FACE_OUTER_BOUND('',#11636,.T.);
#6372=FACE_OUTER_BOUND('',#11637,.T.);
#6373=FACE_OUTER_BOUND('',#11638,.T.);
#6374=FACE_OUTER_BOUND('',#11639,.T.);
#6375=FACE_OUTER_BOUND('',#11640,.T.);
#6376=FACE_OUTER_BOUND('',#11641,.T.);
#6377=FACE_OUTER_BOUND('',#11642,.T.);
#6378=FACE_OUTER_BOUND('',#11643,.T.);
#6379=FACE_OUTER_BOUND('',#11644,.T.);
#6380=FACE_OUTER_BOUND('',#11645,.T.);
#6381=FACE_OUTER_BOUND('',#11646,.T.);
#6382=FACE_OUTER_BOUND('',#11647,.T.);
#6383=FACE_OUTER_BOUND('',#11648,.T.);
#6384=FACE_OUTER_BOUND('',#11649,.T.);
#6385=FACE_OUTER_BOUND('',#11650,.T.);
#6386=FACE_OUTER_BOUND('',#11651,.T.);
#6387=FACE_OUTER_BOUND('',#11652,.T.);
#6388=FACE_OUTER_BOUND('',#11653,.T.);
#6389=FACE_OUTER_BOUND('',#11654,.T.);
#6390=FACE_OUTER_BOUND('',#11655,.T.);
#6391=FACE_OUTER_BOUND('',#11656,.T.);
#6392=FACE_OUTER_BOUND('',#11657,.T.);
#6393=FACE_OUTER_BOUND('',#11658,.T.);
#6394=FACE_OUTER_BOUND('',#11659,.T.);
#6395=FACE_OUTER_BOUND('',#11660,.T.);
#6396=FACE_OUTER_BOUND('',#11661,.T.);
#6397=FACE_OUTER_BOUND('',#11662,.T.);
#6398=FACE_OUTER_BOUND('',#11663,.T.);
#6399=FACE_OUTER_BOUND('',#11664,.T.);
#6400=FACE_OUTER_BOUND('',#11665,.T.);
#6401=FACE_OUTER_BOUND('',#11666,.T.);
#6402=FACE_OUTER_BOUND('',#11667,.T.);
#6403=FACE_OUTER_BOUND('',#11668,.T.);
#6404=FACE_OUTER_BOUND('',#11669,.T.);
#6405=FACE_OUTER_BOUND('',#11670,.T.);
#6406=FACE_OUTER_BOUND('',#11671,.T.);
#6407=FACE_OUTER_BOUND('',#11672,.T.);
#6408=FACE_OUTER_BOUND('',#11673,.T.);
#6409=FACE_OUTER_BOUND('',#11674,.T.);
#6410=FACE_OUTER_BOUND('',#11675,.T.);
#6411=FACE_OUTER_BOUND('',#11676,.T.);
#6412=FACE_OUTER_BOUND('',#11677,.T.);
#6413=FACE_OUTER_BOUND('',#11678,.T.);
#6414=FACE_OUTER_BOUND('',#11679,.T.);
#6415=FACE_OUTER_BOUND('',#11680,.T.);
#6416=FACE_OUTER_BOUND('',#11681,.T.);
#6417=FACE_OUTER_BOUND('',#11682,.T.);
#6418=FACE_OUTER_BOUND('',#11683,.T.);
#6419=FACE_OUTER_BOUND('',#11684,.T.);
#6420=FACE_OUTER_BOUND('',#11685,.T.);
#6421=FACE_OUTER_BOUND('',#11686,.T.);
#6422=FACE_OUTER_BOUND('',#11687,.T.);
#6423=FACE_OUTER_BOUND('',#11688,.T.);
#6424=FACE_OUTER_BOUND('',#11689,.T.);
#6425=FACE_OUTER_BOUND('',#11690,.T.);
#6426=FACE_OUTER_BOUND('',#11691,.T.);
#6427=FACE_OUTER_BOUND('',#11692,.T.);
#6428=FACE_OUTER_BOUND('',#11693,.T.);
#6429=FACE_OUTER_BOUND('',#11694,.T.);
#6430=FACE_OUTER_BOUND('',#11695,.T.);
#6431=FACE_OUTER_BOUND('',#11696,.T.);
#6432=FACE_OUTER_BOUND('',#11697,.T.);
#6433=FACE_OUTER_BOUND('',#11698,.T.);
#6434=FACE_OUTER_BOUND('',#11699,.T.);
#6435=FACE_OUTER_BOUND('',#11700,.T.);
#6436=FACE_OUTER_BOUND('',#11701,.T.);
#6437=FACE_OUTER_BOUND('',#11702,.T.);
#6438=FACE_OUTER_BOUND('',#11703,.T.);
#6439=FACE_OUTER_BOUND('',#11704,.T.);
#6440=FACE_OUTER_BOUND('',#11705,.T.);
#6441=FACE_OUTER_BOUND('',#11706,.T.);
#6442=FACE_OUTER_BOUND('',#11707,.T.);
#6443=FACE_OUTER_BOUND('',#11708,.T.);
#6444=FACE_OUTER_BOUND('',#11709,.T.);
#6445=FACE_OUTER_BOUND('',#11710,.T.);
#6446=FACE_OUTER_BOUND('',#11711,.T.);
#6447=FACE_OUTER_BOUND('',#11712,.T.);
#6448=FACE_OUTER_BOUND('',#11713,.T.);
#6449=FACE_OUTER_BOUND('',#11714,.T.);
#6450=FACE_OUTER_BOUND('',#11715,.T.);
#6451=FACE_OUTER_BOUND('',#11716,.T.);
#6452=FACE_OUTER_BOUND('',#11717,.T.);
#6453=FACE_OUTER_BOUND('',#11718,.T.);
#6454=FACE_OUTER_BOUND('',#11719,.T.);
#6455=FACE_OUTER_BOUND('',#11720,.T.);
#6456=FACE_OUTER_BOUND('',#11721,.T.);
#6457=FACE_OUTER_BOUND('',#11722,.T.);
#6458=FACE_OUTER_BOUND('',#11723,.T.);
#6459=FACE_OUTER_BOUND('',#11724,.T.);
#6460=FACE_OUTER_BOUND('',#11725,.T.);
#6461=FACE_OUTER_BOUND('',#11726,.T.);
#6462=FACE_OUTER_BOUND('',#11727,.T.);
#6463=FACE_OUTER_BOUND('',#11728,.T.);
#6464=FACE_OUTER_BOUND('',#11729,.T.);
#6465=FACE_OUTER_BOUND('',#11730,.T.);
#6466=FACE_OUTER_BOUND('',#11731,.T.);
#6467=FACE_OUTER_BOUND('',#11732,.T.);
#6468=FACE_OUTER_BOUND('',#11733,.T.);
#6469=FACE_OUTER_BOUND('',#11734,.T.);
#6470=FACE_OUTER_BOUND('',#11735,.T.);
#6471=FACE_OUTER_BOUND('',#11736,.T.);
#6472=FACE_OUTER_BOUND('',#11737,.T.);
#6473=FACE_OUTER_BOUND('',#11738,.T.);
#6474=FACE_OUTER_BOUND('',#11739,.T.);
#6475=FACE_OUTER_BOUND('',#11740,.T.);
#6476=FACE_OUTER_BOUND('',#11741,.T.);
#6477=FACE_OUTER_BOUND('',#11742,.T.);
#6478=FACE_OUTER_BOUND('',#11743,.T.);
#6479=FACE_OUTER_BOUND('',#11744,.T.);
#6480=FACE_OUTER_BOUND('',#11745,.T.);
#6481=FACE_OUTER_BOUND('',#11746,.T.);
#6482=FACE_OUTER_BOUND('',#11747,.T.);
#6483=FACE_OUTER_BOUND('',#11748,.T.);
#6484=FACE_OUTER_BOUND('',#11749,.T.);
#6485=FACE_OUTER_BOUND('',#11750,.T.);
#6486=FACE_OUTER_BOUND('',#11751,.T.);
#6487=FACE_OUTER_BOUND('',#11752,.T.);
#6488=FACE_OUTER_BOUND('',#11753,.T.);
#6489=FACE_OUTER_BOUND('',#11754,.T.);
#6490=FACE_OUTER_BOUND('',#11755,.T.);
#6491=FACE_OUTER_BOUND('',#11756,.T.);
#6492=FACE_OUTER_BOUND('',#11757,.T.);
#6493=FACE_OUTER_BOUND('',#11758,.T.);
#6494=FACE_OUTER_BOUND('',#11759,.T.);
#6495=FACE_OUTER_BOUND('',#11760,.T.);
#6496=FACE_OUTER_BOUND('',#11761,.T.);
#6497=FACE_OUTER_BOUND('',#11762,.T.);
#6498=FACE_OUTER_BOUND('',#11763,.T.);
#6499=FACE_OUTER_BOUND('',#11764,.T.);
#6500=FACE_OUTER_BOUND('',#11765,.T.);
#6501=FACE_OUTER_BOUND('',#11766,.T.);
#6502=FACE_OUTER_BOUND('',#11767,.T.);
#6503=FACE_OUTER_BOUND('',#11768,.T.);
#6504=FACE_OUTER_BOUND('',#11769,.T.);
#6505=FACE_OUTER_BOUND('',#11770,.T.);
#6506=FACE_OUTER_BOUND('',#11771,.T.);
#6507=FACE_OUTER_BOUND('',#11772,.T.);
#6508=FACE_OUTER_BOUND('',#11773,.T.);
#6509=FACE_OUTER_BOUND('',#11774,.T.);
#6510=FACE_OUTER_BOUND('',#11775,.T.);
#6511=FACE_OUTER_BOUND('',#11776,.T.);
#6512=FACE_OUTER_BOUND('',#11777,.T.);
#6513=FACE_OUTER_BOUND('',#11778,.T.);
#6514=FACE_OUTER_BOUND('',#11779,.T.);
#6515=FACE_OUTER_BOUND('',#11780,.T.);
#6516=FACE_OUTER_BOUND('',#11781,.T.);
#6517=FACE_OUTER_BOUND('',#11782,.T.);
#6518=FACE_OUTER_BOUND('',#11783,.T.);
#6519=FACE_OUTER_BOUND('',#11784,.T.);
#6520=FACE_OUTER_BOUND('',#11785,.T.);
#6521=FACE_OUTER_BOUND('',#11786,.T.);
#6522=FACE_OUTER_BOUND('',#11787,.T.);
#6523=FACE_OUTER_BOUND('',#11788,.T.);
#6524=FACE_OUTER_BOUND('',#11789,.T.);
#6525=FACE_OUTER_BOUND('',#11790,.T.);
#6526=FACE_OUTER_BOUND('',#11791,.T.);
#6527=FACE_OUTER_BOUND('',#11792,.T.);
#6528=FACE_OUTER_BOUND('',#11793,.T.);
#6529=FACE_OUTER_BOUND('',#11794,.T.);
#6530=FACE_OUTER_BOUND('',#11795,.T.);
#6531=FACE_OUTER_BOUND('',#11796,.T.);
#6532=FACE_OUTER_BOUND('',#11797,.T.);
#6533=FACE_OUTER_BOUND('',#11798,.T.);
#6534=FACE_OUTER_BOUND('',#11799,.T.);
#6535=FACE_OUTER_BOUND('',#11800,.T.);
#6536=FACE_OUTER_BOUND('',#11801,.T.);
#6537=FACE_OUTER_BOUND('',#11802,.T.);
#6538=FACE_OUTER_BOUND('',#11803,.T.);
#6539=FACE_OUTER_BOUND('',#11804,.T.);
#6540=FACE_OUTER_BOUND('',#11805,.T.);
#6541=FACE_OUTER_BOUND('',#11806,.T.);
#6542=FACE_OUTER_BOUND('',#11807,.T.);
#6543=FACE_OUTER_BOUND('',#11808,.T.);
#6544=FACE_OUTER_BOUND('',#11809,.T.);
#6545=FACE_OUTER_BOUND('',#11810,.T.);
#6546=FACE_OUTER_BOUND('',#11811,.T.);
#6547=FACE_OUTER_BOUND('',#11812,.T.);
#6548=FACE_OUTER_BOUND('',#11813,.T.);
#6549=FACE_OUTER_BOUND('',#11814,.T.);
#6550=FACE_OUTER_BOUND('',#11815,.T.);
#6551=FACE_OUTER_BOUND('',#11816,.T.);
#6552=FACE_OUTER_BOUND('',#11817,.T.);
#6553=FACE_OUTER_BOUND('',#11818,.T.);
#6554=FACE_OUTER_BOUND('',#11819,.T.);
#6555=FACE_OUTER_BOUND('',#11820,.T.);
#6556=FACE_OUTER_BOUND('',#11821,.T.);
#6557=FACE_OUTER_BOUND('',#11822,.T.);
#6558=FACE_OUTER_BOUND('',#11823,.T.);
#6559=FACE_OUTER_BOUND('',#11824,.T.);
#6560=FACE_OUTER_BOUND('',#11825,.T.);
#6561=FACE_OUTER_BOUND('',#11826,.T.);
#6562=FACE_OUTER_BOUND('',#11827,.T.);
#6563=FACE_OUTER_BOUND('',#11828,.T.);
#6564=FACE_OUTER_BOUND('',#11829,.T.);
#6565=FACE_OUTER_BOUND('',#11830,.T.);
#6566=FACE_OUTER_BOUND('',#11831,.T.);
#6567=FACE_OUTER_BOUND('',#11832,.T.);
#6568=FACE_OUTER_BOUND('',#11833,.T.);
#6569=FACE_OUTER_BOUND('',#11834,.T.);
#6570=FACE_OUTER_BOUND('',#11835,.T.);
#6571=FACE_OUTER_BOUND('',#11836,.T.);
#6572=FACE_OUTER_BOUND('',#11837,.T.);
#6573=FACE_OUTER_BOUND('',#11838,.T.);
#6574=FACE_OUTER_BOUND('',#11839,.T.);
#6575=FACE_OUTER_BOUND('',#11840,.T.);
#6576=FACE_OUTER_BOUND('',#11841,.T.);
#6577=FACE_OUTER_BOUND('',#11842,.T.);
#6578=FACE_OUTER_BOUND('',#11843,.T.);
#6579=FACE_OUTER_BOUND('',#11844,.T.);
#6580=FACE_OUTER_BOUND('',#11845,.T.);
#6581=FACE_OUTER_BOUND('',#11846,.T.);
#6582=FACE_OUTER_BOUND('',#11847,.T.);
#6583=FACE_OUTER_BOUND('',#11848,.T.);
#6584=FACE_OUTER_BOUND('',#11849,.T.);
#6585=FACE_OUTER_BOUND('',#11850,.T.);
#6586=FACE_OUTER_BOUND('',#11851,.T.);
#6587=FACE_OUTER_BOUND('',#11852,.T.);
#6588=FACE_OUTER_BOUND('',#11853,.T.);
#6589=FACE_OUTER_BOUND('',#11854,.T.);
#6590=FACE_OUTER_BOUND('',#11855,.T.);
#6591=FACE_OUTER_BOUND('',#11856,.T.);
#6592=FACE_OUTER_BOUND('',#11857,.T.);
#6593=FACE_OUTER_BOUND('',#11858,.T.);
#6594=FACE_OUTER_BOUND('',#11859,.T.);
#6595=FACE_OUTER_BOUND('',#11860,.T.);
#6596=FACE_OUTER_BOUND('',#11861,.T.);
#6597=FACE_OUTER_BOUND('',#11862,.T.);
#6598=FACE_OUTER_BOUND('',#11863,.T.);
#6599=FACE_OUTER_BOUND('',#11864,.T.);
#6600=FACE_OUTER_BOUND('',#11865,.T.);
#6601=FACE_OUTER_BOUND('',#11866,.T.);
#6602=FACE_OUTER_BOUND('',#11867,.T.);
#6603=FACE_OUTER_BOUND('',#11868,.T.);
#6604=FACE_OUTER_BOUND('',#11869,.T.);
#6605=FACE_OUTER_BOUND('',#11870,.T.);
#6606=FACE_OUTER_BOUND('',#11871,.T.);
#6607=FACE_OUTER_BOUND('',#11872,.T.);
#6608=FACE_OUTER_BOUND('',#11873,.T.);
#6609=FACE_OUTER_BOUND('',#11874,.T.);
#6610=FACE_OUTER_BOUND('',#11875,.T.);
#6611=FACE_OUTER_BOUND('',#11876,.T.);
#6612=FACE_OUTER_BOUND('',#11877,.T.);
#6613=FACE_OUTER_BOUND('',#11878,.T.);
#6614=FACE_OUTER_BOUND('',#11879,.T.);
#6615=FACE_OUTER_BOUND('',#11880,.T.);
#6616=FACE_OUTER_BOUND('',#11881,.T.);
#6617=FACE_OUTER_BOUND('',#11882,.T.);
#6618=FACE_OUTER_BOUND('',#11883,.T.);
#6619=FACE_OUTER_BOUND('',#11884,.T.);
#6620=FACE_OUTER_BOUND('',#11885,.T.);
#6621=FACE_OUTER_BOUND('',#11886,.T.);
#6622=FACE_OUTER_BOUND('',#11887,.T.);
#6623=FACE_OUTER_BOUND('',#11888,.T.);
#6624=FACE_OUTER_BOUND('',#11889,.T.);
#6625=FACE_OUTER_BOUND('',#11890,.T.);
#6626=FACE_OUTER_BOUND('',#11891,.T.);
#6627=FACE_OUTER_BOUND('',#11892,.T.);
#6628=FACE_OUTER_BOUND('',#11893,.T.);
#6629=FACE_OUTER_BOUND('',#11894,.T.);
#6630=FACE_OUTER_BOUND('',#11895,.T.);
#6631=FACE_OUTER_BOUND('',#11896,.T.);
#6632=FACE_OUTER_BOUND('',#11897,.T.);
#6633=FACE_OUTER_BOUND('',#11898,.T.);
#6634=FACE_OUTER_BOUND('',#11899,.T.);
#6635=FACE_OUTER_BOUND('',#11900,.T.);
#6636=FACE_OUTER_BOUND('',#11901,.T.);
#6637=FACE_OUTER_BOUND('',#11902,.T.);
#6638=FACE_OUTER_BOUND('',#11903,.T.);
#6639=FACE_OUTER_BOUND('',#11904,.T.);
#6640=FACE_OUTER_BOUND('',#11905,.T.);
#6641=FACE_OUTER_BOUND('',#11906,.T.);
#6642=FACE_OUTER_BOUND('',#11907,.T.);
#6643=FACE_OUTER_BOUND('',#11908,.T.);
#6644=FACE_OUTER_BOUND('',#11909,.T.);
#6645=FACE_OUTER_BOUND('',#11910,.T.);
#6646=FACE_OUTER_BOUND('',#11911,.T.);
#6647=FACE_OUTER_BOUND('',#11912,.T.);
#6648=FACE_OUTER_BOUND('',#11913,.T.);
#6649=FACE_OUTER_BOUND('',#11914,.T.);
#6650=FACE_OUTER_BOUND('',#11915,.T.);
#6651=FACE_OUTER_BOUND('',#11916,.T.);
#6652=FACE_OUTER_BOUND('',#11917,.T.);
#6653=FACE_OUTER_BOUND('',#11918,.T.);
#6654=FACE_OUTER_BOUND('',#11919,.T.);
#6655=FACE_OUTER_BOUND('',#11920,.T.);
#6656=FACE_OUTER_BOUND('',#11921,.T.);
#6657=FACE_OUTER_BOUND('',#11922,.T.);
#6658=FACE_OUTER_BOUND('',#11923,.T.);
#6659=FACE_OUTER_BOUND('',#11924,.T.);
#6660=FACE_OUTER_BOUND('',#11925,.T.);
#6661=FACE_OUTER_BOUND('',#11926,.T.);
#6662=FACE_OUTER_BOUND('',#11927,.T.);
#6663=FACE_OUTER_BOUND('',#11928,.T.);
#6664=FACE_OUTER_BOUND('',#11929,.T.);
#6665=FACE_OUTER_BOUND('',#11930,.T.);
#6666=FACE_OUTER_BOUND('',#11931,.T.);
#6667=FACE_OUTER_BOUND('',#11932,.T.);
#6668=FACE_OUTER_BOUND('',#11933,.T.);
#6669=FACE_OUTER_BOUND('',#11934,.T.);
#6670=FACE_OUTER_BOUND('',#11935,.T.);
#6671=FACE_OUTER_BOUND('',#11936,.T.);
#6672=FACE_OUTER_BOUND('',#11937,.T.);
#6673=FACE_OUTER_BOUND('',#11938,.T.);
#6674=FACE_OUTER_BOUND('',#11939,.T.);
#6675=FACE_OUTER_BOUND('',#11940,.T.);
#6676=FACE_OUTER_BOUND('',#11941,.T.);
#6677=FACE_OUTER_BOUND('',#11942,.T.);
#6678=FACE_OUTER_BOUND('',#11943,.T.);
#6679=FACE_OUTER_BOUND('',#11944,.T.);
#6680=FACE_OUTER_BOUND('',#11945,.T.);
#6681=FACE_OUTER_BOUND('',#11946,.T.);
#6682=FACE_OUTER_BOUND('',#11947,.T.);
#6683=FACE_OUTER_BOUND('',#11948,.T.);
#6684=FACE_OUTER_BOUND('',#11949,.T.);
#6685=FACE_OUTER_BOUND('',#11950,.T.);
#6686=FACE_OUTER_BOUND('',#11951,.T.);
#6687=FACE_OUTER_BOUND('',#11952,.T.);
#6688=FACE_OUTER_BOUND('',#11953,.T.);
#6689=FACE_OUTER_BOUND('',#11954,.T.);
#6690=FACE_OUTER_BOUND('',#11955,.T.);
#6691=FACE_OUTER_BOUND('',#11956,.T.);
#6692=FACE_OUTER_BOUND('',#11957,.T.);
#6693=FACE_OUTER_BOUND('',#11958,.T.);
#6694=FACE_OUTER_BOUND('',#11959,.T.);
#6695=FACE_OUTER_BOUND('',#11960,.T.);
#6696=FACE_OUTER_BOUND('',#11961,.T.);
#6697=FACE_OUTER_BOUND('',#11962,.T.);
#6698=FACE_OUTER_BOUND('',#11963,.T.);
#6699=FACE_OUTER_BOUND('',#11964,.T.);
#6700=FACE_OUTER_BOUND('',#11965,.T.);
#6701=FACE_OUTER_BOUND('',#11966,.T.);
#6702=FACE_OUTER_BOUND('',#11967,.T.);
#6703=FACE_OUTER_BOUND('',#11968,.T.);
#6704=FACE_OUTER_BOUND('',#11969,.T.);
#6705=FACE_OUTER_BOUND('',#11970,.T.);
#6706=FACE_OUTER_BOUND('',#11971,.T.);
#6707=FACE_OUTER_BOUND('',#11972,.T.);
#6708=FACE_OUTER_BOUND('',#11973,.T.);
#6709=FACE_OUTER_BOUND('',#11974,.T.);
#6710=FACE_OUTER_BOUND('',#11975,.T.);
#6711=FACE_OUTER_BOUND('',#11976,.T.);
#6712=FACE_OUTER_BOUND('',#11977,.T.);
#6713=FACE_OUTER_BOUND('',#11978,.T.);
#6714=FACE_OUTER_BOUND('',#11979,.T.);
#6715=FACE_OUTER_BOUND('',#11980,.T.);
#6716=FACE_OUTER_BOUND('',#11981,.T.);
#6717=FACE_OUTER_BOUND('',#11982,.T.);
#6718=FACE_OUTER_BOUND('',#11983,.T.);
#6719=FACE_OUTER_BOUND('',#11984,.T.);
#6720=FACE_OUTER_BOUND('',#11985,.T.);
#6721=FACE_OUTER_BOUND('',#11986,.T.);
#6722=FACE_OUTER_BOUND('',#11987,.T.);
#6723=FACE_OUTER_BOUND('',#11988,.T.);
#6724=FACE_OUTER_BOUND('',#11989,.T.);
#6725=FACE_OUTER_BOUND('',#11990,.T.);
#6726=FACE_OUTER_BOUND('',#11991,.T.);
#6727=FACE_OUTER_BOUND('',#11992,.T.);
#6728=FACE_OUTER_BOUND('',#11993,.T.);
#6729=FACE_OUTER_BOUND('',#11994,.T.);
#6730=FACE_OUTER_BOUND('',#11995,.T.);
#6731=FACE_OUTER_BOUND('',#11996,.T.);
#6732=FACE_OUTER_BOUND('',#11997,.T.);
#6733=FACE_OUTER_BOUND('',#11998,.T.);
#6734=FACE_OUTER_BOUND('',#11999,.T.);
#6735=FACE_OUTER_BOUND('',#12000,.T.);
#6736=FACE_OUTER_BOUND('',#12001,.T.);
#6737=FACE_OUTER_BOUND('',#12002,.T.);
#6738=FACE_OUTER_BOUND('',#12003,.T.);
#6739=FACE_OUTER_BOUND('',#12004,.T.);
#6740=FACE_OUTER_BOUND('',#12005,.T.);
#6741=FACE_OUTER_BOUND('',#12006,.T.);
#6742=FACE_OUTER_BOUND('',#12007,.T.);
#6743=FACE_OUTER_BOUND('',#12008,.T.);
#6744=FACE_OUTER_BOUND('',#12009,.T.);
#6745=FACE_OUTER_BOUND('',#12010,.T.);
#6746=FACE_OUTER_BOUND('',#12011,.T.);
#6747=FACE_OUTER_BOUND('',#12012,.T.);
#6748=FACE_OUTER_BOUND('',#12013,.T.);
#6749=FACE_OUTER_BOUND('',#12014,.T.);
#6750=FACE_OUTER_BOUND('',#12015,.T.);
#6751=FACE_OUTER_BOUND('',#12016,.T.);
#6752=FACE_OUTER_BOUND('',#12017,.T.);
#6753=FACE_OUTER_BOUND('',#12018,.T.);
#6754=FACE_OUTER_BOUND('',#12019,.T.);
#6755=FACE_OUTER_BOUND('',#12020,.T.);
#6756=FACE_OUTER_BOUND('',#12021,.T.);
#6757=FACE_OUTER_BOUND('',#12022,.T.);
#6758=FACE_OUTER_BOUND('',#12023,.T.);
#6759=FACE_OUTER_BOUND('',#12024,.T.);
#6760=FACE_OUTER_BOUND('',#12025,.T.);
#6761=FACE_OUTER_BOUND('',#12026,.T.);
#6762=FACE_OUTER_BOUND('',#12027,.T.);
#6763=FACE_OUTER_BOUND('',#12028,.T.);
#6764=FACE_OUTER_BOUND('',#12029,.T.);
#6765=FACE_OUTER_BOUND('',#12030,.T.);
#6766=FACE_OUTER_BOUND('',#12031,.T.);
#6767=FACE_OUTER_BOUND('',#12032,.T.);
#6768=FACE_OUTER_BOUND('',#12033,.T.);
#6769=FACE_OUTER_BOUND('',#12034,.T.);
#6770=FACE_OUTER_BOUND('',#12035,.T.);
#6771=FACE_OUTER_BOUND('',#12036,.T.);
#6772=FACE_OUTER_BOUND('',#12037,.T.);
#6773=FACE_OUTER_BOUND('',#12038,.T.);
#6774=FACE_OUTER_BOUND('',#12039,.T.);
#6775=FACE_OUTER_BOUND('',#12040,.T.);
#6776=FACE_OUTER_BOUND('',#12041,.T.);
#6777=FACE_OUTER_BOUND('',#12042,.T.);
#6778=FACE_OUTER_BOUND('',#12043,.T.);
#6779=FACE_OUTER_BOUND('',#12044,.T.);
#6780=FACE_OUTER_BOUND('',#12045,.T.);
#6781=FACE_OUTER_BOUND('',#12046,.T.);
#6782=FACE_OUTER_BOUND('',#12047,.T.);
#6783=FACE_OUTER_BOUND('',#12048,.T.);
#6784=FACE_OUTER_BOUND('',#12049,.T.);
#6785=FACE_OUTER_BOUND('',#12050,.T.);
#6786=FACE_OUTER_BOUND('',#12051,.T.);
#6787=FACE_OUTER_BOUND('',#12052,.T.);
#6788=FACE_OUTER_BOUND('',#12053,.T.);
#6789=FACE_OUTER_BOUND('',#12054,.T.);
#6790=FACE_OUTER_BOUND('',#12055,.T.);
#6791=FACE_OUTER_BOUND('',#12056,.T.);
#6792=FACE_OUTER_BOUND('',#12057,.T.);
#6793=FACE_OUTER_BOUND('',#12058,.T.);
#6794=FACE_OUTER_BOUND('',#12059,.T.);
#6795=FACE_OUTER_BOUND('',#12060,.T.);
#6796=FACE_OUTER_BOUND('',#12061,.T.);
#6797=FACE_OUTER_BOUND('',#12062,.T.);
#6798=FACE_OUTER_BOUND('',#12063,.T.);
#6799=FACE_OUTER_BOUND('',#12064,.T.);
#6800=FACE_OUTER_BOUND('',#12065,.T.);
#6801=FACE_OUTER_BOUND('',#12066,.T.);
#6802=FACE_OUTER_BOUND('',#12067,.T.);
#6803=FACE_OUTER_BOUND('',#12068,.T.);
#6804=FACE_OUTER_BOUND('',#12069,.T.);
#6805=FACE_OUTER_BOUND('',#12070,.T.);
#6806=FACE_OUTER_BOUND('',#12071,.T.);
#6807=FACE_OUTER_BOUND('',#12072,.T.);
#6808=FACE_OUTER_BOUND('',#12073,.T.);
#6809=FACE_OUTER_BOUND('',#12074,.T.);
#6810=FACE_OUTER_BOUND('',#12075,.T.);
#6811=FACE_OUTER_BOUND('',#12076,.T.);
#6812=FACE_OUTER_BOUND('',#12077,.T.);
#6813=FACE_OUTER_BOUND('',#12078,.T.);
#6814=FACE_OUTER_BOUND('',#12079,.T.);
#6815=FACE_OUTER_BOUND('',#12080,.T.);
#6816=FACE_OUTER_BOUND('',#12081,.T.);
#6817=FACE_OUTER_BOUND('',#12082,.T.);
#6818=FACE_OUTER_BOUND('',#12083,.T.);
#6819=FACE_OUTER_BOUND('',#12084,.T.);
#6820=FACE_OUTER_BOUND('',#12085,.T.);
#6821=FACE_OUTER_BOUND('',#12086,.T.);
#6822=FACE_OUTER_BOUND('',#12087,.T.);
#6823=FACE_OUTER_BOUND('',#12088,.T.);
#6824=FACE_OUTER_BOUND('',#12089,.T.);
#6825=FACE_OUTER_BOUND('',#12090,.T.);
#6826=FACE_OUTER_BOUND('',#12091,.T.);
#6827=FACE_OUTER_BOUND('',#12092,.T.);
#6828=FACE_OUTER_BOUND('',#12093,.T.);
#6829=FACE_OUTER_BOUND('',#12094,.T.);
#6830=FACE_OUTER_BOUND('',#12095,.T.);
#6831=FACE_OUTER_BOUND('',#12096,.T.);
#6832=FACE_OUTER_BOUND('',#12097,.T.);
#6833=FACE_OUTER_BOUND('',#12098,.T.);
#6834=FACE_OUTER_BOUND('',#12099,.T.);
#6835=FACE_OUTER_BOUND('',#12100,.T.);
#6836=FACE_OUTER_BOUND('',#12101,.T.);
#6837=FACE_OUTER_BOUND('',#12102,.T.);
#6838=FACE_OUTER_BOUND('',#12103,.T.);
#6839=FACE_OUTER_BOUND('',#12104,.T.);
#6840=FACE_OUTER_BOUND('',#12105,.T.);
#6841=FACE_OUTER_BOUND('',#12106,.T.);
#6842=FACE_OUTER_BOUND('',#12107,.T.);
#6843=FACE_OUTER_BOUND('',#12108,.T.);
#6844=FACE_OUTER_BOUND('',#12109,.T.);
#6845=FACE_OUTER_BOUND('',#12110,.T.);
#6846=FACE_OUTER_BOUND('',#12111,.T.);
#6847=FACE_OUTER_BOUND('',#12112,.T.);
#6848=FACE_OUTER_BOUND('',#12113,.T.);
#6849=FACE_OUTER_BOUND('',#12114,.T.);
#6850=FACE_OUTER_BOUND('',#12115,.T.);
#6851=FACE_OUTER_BOUND('',#12116,.T.);
#6852=FACE_OUTER_BOUND('',#12117,.T.);
#6853=FACE_OUTER_BOUND('',#12118,.T.);
#6854=FACE_OUTER_BOUND('',#12119,.T.);
#6855=FACE_OUTER_BOUND('',#12120,.T.);
#6856=FACE_OUTER_BOUND('',#12121,.T.);
#6857=FACE_OUTER_BOUND('',#12122,.T.);
#6858=FACE_OUTER_BOUND('',#12123,.T.);
#6859=FACE_OUTER_BOUND('',#12124,.T.);
#6860=FACE_OUTER_BOUND('',#12125,.T.);
#6861=FACE_OUTER_BOUND('',#12126,.T.);
#6862=FACE_OUTER_BOUND('',#12127,.T.);
#6863=FACE_OUTER_BOUND('',#12128,.T.);
#6864=FACE_OUTER_BOUND('',#12129,.T.);
#6865=FACE_OUTER_BOUND('',#12130,.T.);
#6866=FACE_OUTER_BOUND('',#12131,.T.);
#6867=FACE_OUTER_BOUND('',#12132,.T.);
#6868=FACE_OUTER_BOUND('',#12133,.T.);
#6869=FACE_OUTER_BOUND('',#12134,.T.);
#6870=FACE_OUTER_BOUND('',#12135,.T.);
#6871=FACE_OUTER_BOUND('',#12136,.T.);
#6872=FACE_OUTER_BOUND('',#12137,.T.);
#6873=FACE_OUTER_BOUND('',#12138,.T.);
#6874=FACE_OUTER_BOUND('',#12139,.T.);
#6875=FACE_OUTER_BOUND('',#12140,.T.);
#6876=FACE_OUTER_BOUND('',#12141,.T.);
#6877=FACE_OUTER_BOUND('',#12142,.T.);
#6878=FACE_OUTER_BOUND('',#12143,.T.);
#6879=FACE_OUTER_BOUND('',#12144,.T.);
#6880=FACE_OUTER_BOUND('',#12145,.T.);
#6881=FACE_OUTER_BOUND('',#12146,.T.);
#6882=FACE_OUTER_BOUND('',#12147,.T.);
#6883=FACE_OUTER_BOUND('',#12148,.T.);
#6884=FACE_OUTER_BOUND('',#12149,.T.);
#6885=FACE_OUTER_BOUND('',#12150,.T.);
#6886=FACE_OUTER_BOUND('',#12151,.T.);
#6887=FACE_OUTER_BOUND('',#12152,.T.);
#6888=FACE_OUTER_BOUND('',#12153,.T.);
#6889=FACE_OUTER_BOUND('',#12154,.T.);
#6890=FACE_OUTER_BOUND('',#12155,.T.);
#6891=FACE_OUTER_BOUND('',#12156,.T.);
#6892=FACE_OUTER_BOUND('',#12157,.T.);
#6893=FACE_OUTER_BOUND('',#12158,.T.);
#6894=FACE_OUTER_BOUND('',#12159,.T.);
#6895=FACE_OUTER_BOUND('',#12160,.T.);
#6896=FACE_OUTER_BOUND('',#12161,.T.);
#6897=FACE_OUTER_BOUND('',#12162,.T.);
#6898=FACE_OUTER_BOUND('',#12163,.T.);
#6899=FACE_OUTER_BOUND('',#12164,.T.);
#6900=FACE_OUTER_BOUND('',#12165,.T.);
#6901=FACE_OUTER_BOUND('',#12166,.T.);
#6902=FACE_OUTER_BOUND('',#12167,.T.);
#6903=FACE_OUTER_BOUND('',#12168,.T.);
#6904=FACE_OUTER_BOUND('',#12169,.T.);
#6905=FACE_OUTER_BOUND('',#12170,.T.);
#6906=FACE_OUTER_BOUND('',#12171,.T.);
#6907=FACE_OUTER_BOUND('',#12172,.T.);
#6908=FACE_OUTER_BOUND('',#12173,.T.);
#6909=FACE_OUTER_BOUND('',#12174,.T.);
#6910=FACE_OUTER_BOUND('',#12175,.T.);
#6911=FACE_OUTER_BOUND('',#12176,.T.);
#6912=FACE_OUTER_BOUND('',#12177,.T.);
#6913=FACE_OUTER_BOUND('',#12178,.T.);
#6914=FACE_OUTER_BOUND('',#12179,.T.);
#6915=FACE_OUTER_BOUND('',#12180,.T.);
#6916=FACE_OUTER_BOUND('',#12181,.T.);
#6917=FACE_OUTER_BOUND('',#12182,.T.);
#6918=FACE_OUTER_BOUND('',#12183,.T.);
#6919=FACE_OUTER_BOUND('',#12184,.T.);
#6920=FACE_OUTER_BOUND('',#12185,.T.);
#6921=FACE_OUTER_BOUND('',#12186,.T.);
#6922=FACE_OUTER_BOUND('',#12187,.T.);
#6923=FACE_OUTER_BOUND('',#12188,.T.);
#6924=FACE_OUTER_BOUND('',#12189,.T.);
#6925=FACE_OUTER_BOUND('',#12190,.T.);
#6926=FACE_OUTER_BOUND('',#12191,.T.);
#6927=FACE_OUTER_BOUND('',#12192,.T.);
#6928=FACE_OUTER_BOUND('',#12193,.T.);
#6929=FACE_OUTER_BOUND('',#12194,.T.);
#6930=FACE_OUTER_BOUND('',#12195,.T.);
#6931=FACE_OUTER_BOUND('',#12196,.T.);
#6932=FACE_OUTER_BOUND('',#12197,.T.);
#6933=FACE_OUTER_BOUND('',#12198,.T.);
#6934=FACE_OUTER_BOUND('',#12199,.T.);
#6935=FACE_OUTER_BOUND('',#12200,.T.);
#6936=FACE_OUTER_BOUND('',#12201,.T.);
#6937=FACE_OUTER_BOUND('',#12202,.T.);
#6938=FACE_OUTER_BOUND('',#12203,.T.);
#6939=FACE_OUTER_BOUND('',#12204,.T.);
#6940=FACE_OUTER_BOUND('',#12205,.T.);
#6941=FACE_OUTER_BOUND('',#12206,.T.);
#6942=FACE_OUTER_BOUND('',#12207,.T.);
#6943=FACE_OUTER_BOUND('',#12208,.T.);
#6944=FACE_OUTER_BOUND('',#12209,.T.);
#6945=FACE_OUTER_BOUND('',#12210,.T.);
#6946=FACE_OUTER_BOUND('',#12211,.T.);
#6947=FACE_OUTER_BOUND('',#12212,.T.);
#6948=FACE_OUTER_BOUND('',#12213,.T.);
#6949=FACE_OUTER_BOUND('',#12214,.T.);
#6950=FACE_OUTER_BOUND('',#12215,.T.);
#6951=FACE_OUTER_BOUND('',#12216,.T.);
#6952=FACE_OUTER_BOUND('',#12217,.T.);
#6953=FACE_OUTER_BOUND('',#12218,.T.);
#6954=FACE_OUTER_BOUND('',#12219,.T.);
#6955=FACE_OUTER_BOUND('',#12220,.T.);
#6956=FACE_OUTER_BOUND('',#12221,.T.);
#6957=FACE_OUTER_BOUND('',#12222,.T.);
#6958=FACE_OUTER_BOUND('',#12223,.T.);
#6959=FACE_OUTER_BOUND('',#12224,.T.);
#6960=FACE_OUTER_BOUND('',#12225,.T.);
#6961=FACE_OUTER_BOUND('',#12226,.T.);
#6962=FACE_OUTER_BOUND('',#12227,.T.);
#6963=FACE_OUTER_BOUND('',#12228,.T.);
#6964=FACE_OUTER_BOUND('',#12229,.T.);
#6965=FACE_OUTER_BOUND('',#12230,.T.);
#6966=FACE_OUTER_BOUND('',#12231,.T.);
#6967=FACE_OUTER_BOUND('',#12232,.T.);
#6968=FACE_OUTER_BOUND('',#12233,.T.);
#6969=FACE_OUTER_BOUND('',#12234,.T.);
#6970=FACE_OUTER_BOUND('',#12235,.T.);
#6971=FACE_OUTER_BOUND('',#12236,.T.);
#6972=FACE_OUTER_BOUND('',#12237,.T.);
#6973=FACE_OUTER_BOUND('',#12238,.T.);
#6974=FACE_OUTER_BOUND('',#12239,.T.);
#6975=FACE_OUTER_BOUND('',#12240,.T.);
#6976=FACE_OUTER_BOUND('',#12241,.T.);
#6977=FACE_OUTER_BOUND('',#12242,.T.);
#6978=FACE_OUTER_BOUND('',#12243,.T.);
#6979=FACE_OUTER_BOUND('',#12244,.T.);
#6980=FACE_OUTER_BOUND('',#12245,.T.);
#6981=FACE_OUTER_BOUND('',#12246,.T.);
#6982=FACE_OUTER_BOUND('',#12247,.T.);
#6983=FACE_OUTER_BOUND('',#12248,.T.);
#6984=FACE_OUTER_BOUND('',#12249,.T.);
#6985=FACE_OUTER_BOUND('',#12250,.T.);
#6986=FACE_OUTER_BOUND('',#12251,.T.);
#6987=FACE_OUTER_BOUND('',#12252,.T.);
#6988=FACE_OUTER_BOUND('',#12253,.T.);
#6989=FACE_OUTER_BOUND('',#12254,.T.);
#6990=FACE_OUTER_BOUND('',#12255,.T.);
#6991=FACE_OUTER_BOUND('',#12256,.T.);
#6992=FACE_OUTER_BOUND('',#12257,.T.);
#6993=FACE_OUTER_BOUND('',#12258,.T.);
#6994=FACE_OUTER_BOUND('',#12259,.T.);
#6995=FACE_OUTER_BOUND('',#12260,.T.);
#6996=FACE_OUTER_BOUND('',#12261,.T.);
#6997=FACE_OUTER_BOUND('',#12262,.T.);
#6998=FACE_OUTER_BOUND('',#12263,.T.);
#6999=FACE_OUTER_BOUND('',#12264,.T.);
#7000=FACE_OUTER_BOUND('',#12265,.T.);
#7001=FACE_OUTER_BOUND('',#12266,.T.);
#7002=FACE_OUTER_BOUND('',#12267,.T.);
#7003=FACE_OUTER_BOUND('',#12268,.T.);
#7004=FACE_OUTER_BOUND('',#12269,.T.);
#7005=FACE_OUTER_BOUND('',#12270,.T.);
#7006=FACE_OUTER_BOUND('',#12271,.T.);
#7007=FACE_OUTER_BOUND('',#12272,.T.);
#7008=FACE_OUTER_BOUND('',#12273,.T.);
#7009=FACE_OUTER_BOUND('',#12274,.T.);
#7010=FACE_OUTER_BOUND('',#12275,.T.);
#7011=FACE_OUTER_BOUND('',#12276,.T.);
#7012=FACE_OUTER_BOUND('',#12277,.T.);
#7013=FACE_OUTER_BOUND('',#12278,.T.);
#7014=FACE_OUTER_BOUND('',#12279,.T.);
#7015=FACE_OUTER_BOUND('',#12280,.T.);
#7016=FACE_OUTER_BOUND('',#12281,.T.);
#7017=FACE_OUTER_BOUND('',#12282,.T.);
#7018=FACE_OUTER_BOUND('',#12283,.T.);
#7019=FACE_OUTER_BOUND('',#12284,.T.);
#7020=FACE_OUTER_BOUND('',#12285,.T.);
#7021=FACE_OUTER_BOUND('',#12286,.T.);
#7022=FACE_OUTER_BOUND('',#12287,.T.);
#7023=FACE_OUTER_BOUND('',#12288,.T.);
#7024=FACE_OUTER_BOUND('',#12289,.T.);
#7025=FACE_OUTER_BOUND('',#12290,.T.);
#7026=FACE_OUTER_BOUND('',#12291,.T.);
#7027=FACE_OUTER_BOUND('',#12292,.T.);
#7028=FACE_OUTER_BOUND('',#12293,.T.);
#7029=FACE_OUTER_BOUND('',#12294,.T.);
#7030=FACE_OUTER_BOUND('',#12295,.T.);
#7031=FACE_OUTER_BOUND('',#12296,.T.);
#7032=FACE_OUTER_BOUND('',#12297,.T.);
#7033=FACE_OUTER_BOUND('',#12298,.T.);
#7034=FACE_OUTER_BOUND('',#12299,.T.);
#7035=FACE_OUTER_BOUND('',#12300,.T.);
#7036=FACE_OUTER_BOUND('',#12301,.T.);
#7037=FACE_OUTER_BOUND('',#12302,.T.);
#7038=FACE_OUTER_BOUND('',#12303,.T.);
#7039=FACE_OUTER_BOUND('',#12304,.T.);
#7040=FACE_OUTER_BOUND('',#12305,.T.);
#7041=FACE_OUTER_BOUND('',#12306,.T.);
#7042=FACE_OUTER_BOUND('',#12307,.T.);
#7043=FACE_OUTER_BOUND('',#12308,.T.);
#7044=FACE_OUTER_BOUND('',#12309,.T.);
#7045=FACE_OUTER_BOUND('',#12310,.T.);
#7046=FACE_OUTER_BOUND('',#12311,.T.);
#7047=FACE_OUTER_BOUND('',#12312,.T.);
#7048=FACE_OUTER_BOUND('',#12313,.T.);
#7049=FACE_OUTER_BOUND('',#12314,.T.);
#7050=FACE_OUTER_BOUND('',#12315,.T.);
#7051=FACE_OUTER_BOUND('',#12316,.T.);
#7052=FACE_OUTER_BOUND('',#12317,.T.);
#7053=FACE_OUTER_BOUND('',#12318,.T.);
#7054=FACE_OUTER_BOUND('',#12319,.T.);
#7055=FACE_OUTER_BOUND('',#12320,.T.);
#7056=FACE_OUTER_BOUND('',#12321,.T.);
#7057=FACE_OUTER_BOUND('',#12322,.T.);
#7058=FACE_OUTER_BOUND('',#12323,.T.);
#7059=FACE_OUTER_BOUND('',#12324,.T.);
#7060=FACE_OUTER_BOUND('',#12325,.T.);
#7061=FACE_OUTER_BOUND('',#12326,.T.);
#7062=FACE_OUTER_BOUND('',#12327,.T.);
#7063=FACE_OUTER_BOUND('',#12328,.T.);
#7064=FACE_OUTER_BOUND('',#12329,.T.);
#7065=FACE_OUTER_BOUND('',#12330,.T.);
#7066=FACE_OUTER_BOUND('',#12331,.T.);
#7067=FACE_OUTER_BOUND('',#12332,.T.);
#7068=FACE_OUTER_BOUND('',#12333,.T.);
#7069=FACE_OUTER_BOUND('',#12334,.T.);
#7070=FACE_OUTER_BOUND('',#12335,.T.);
#7071=FACE_OUTER_BOUND('',#12336,.T.);
#7072=FACE_OUTER_BOUND('',#12337,.T.);
#7073=FACE_OUTER_BOUND('',#12338,.T.);
#7074=FACE_OUTER_BOUND('',#12339,.T.);
#7075=FACE_OUTER_BOUND('',#12340,.T.);
#7076=FACE_OUTER_BOUND('',#12341,.T.);
#7077=FACE_OUTER_BOUND('',#12342,.T.);
#7078=FACE_OUTER_BOUND('',#12343,.T.);
#7079=FACE_OUTER_BOUND('',#12344,.T.);
#7080=FACE_OUTER_BOUND('',#12345,.T.);
#7081=FACE_OUTER_BOUND('',#12346,.T.);
#7082=FACE_OUTER_BOUND('',#12347,.T.);
#7083=FACE_OUTER_BOUND('',#12348,.T.);
#7084=FACE_OUTER_BOUND('',#12349,.T.);
#7085=FACE_OUTER_BOUND('',#12350,.T.);
#7086=FACE_OUTER_BOUND('',#12351,.T.);
#7087=FACE_OUTER_BOUND('',#12352,.T.);
#7088=FACE_OUTER_BOUND('',#12353,.T.);
#7089=FACE_OUTER_BOUND('',#12354,.T.);
#7090=FACE_OUTER_BOUND('',#12355,.T.);
#7091=FACE_OUTER_BOUND('',#12356,.T.);
#7092=FACE_OUTER_BOUND('',#12357,.T.);
#7093=FACE_OUTER_BOUND('',#12358,.T.);
#7094=FACE_OUTER_BOUND('',#12359,.T.);
#7095=FACE_OUTER_BOUND('',#12360,.T.);
#7096=FACE_OUTER_BOUND('',#12361,.T.);
#7097=FACE_OUTER_BOUND('',#12362,.T.);
#7098=FACE_OUTER_BOUND('',#12363,.T.);
#7099=FACE_OUTER_BOUND('',#12364,.T.);
#7100=FACE_OUTER_BOUND('',#12365,.T.);
#7101=FACE_OUTER_BOUND('',#12366,.T.);
#7102=FACE_OUTER_BOUND('',#12367,.T.);
#7103=FACE_OUTER_BOUND('',#12368,.T.);
#7104=FACE_OUTER_BOUND('',#12369,.T.);
#7105=FACE_OUTER_BOUND('',#12370,.T.);
#7106=FACE_OUTER_BOUND('',#12371,.T.);
#7107=FACE_OUTER_BOUND('',#12372,.T.);
#7108=FACE_OUTER_BOUND('',#12373,.T.);
#7109=FACE_OUTER_BOUND('',#12374,.T.);
#7110=FACE_OUTER_BOUND('',#12375,.T.);
#7111=FACE_OUTER_BOUND('',#12376,.T.);
#7112=FACE_OUTER_BOUND('',#12377,.T.);
#7113=FACE_OUTER_BOUND('',#12378,.T.);
#7114=FACE_OUTER_BOUND('',#12379,.T.);
#7115=FACE_OUTER_BOUND('',#12380,.T.);
#7116=FACE_OUTER_BOUND('',#12381,.T.);
#7117=FACE_OUTER_BOUND('',#12382,.T.);
#7118=FACE_OUTER_BOUND('',#12383,.T.);
#7119=FACE_OUTER_BOUND('',#12384,.T.);
#7120=FACE_OUTER_BOUND('',#12385,.T.);
#7121=FACE_OUTER_BOUND('',#12386,.T.);
#7122=FACE_OUTER_BOUND('',#12387,.T.);
#7123=FACE_OUTER_BOUND('',#12388,.T.);
#7124=FACE_OUTER_BOUND('',#12389,.T.);
#7125=FACE_OUTER_BOUND('',#12390,.T.);
#7126=FACE_OUTER_BOUND('',#12391,.T.);
#7127=FACE_OUTER_BOUND('',#12392,.T.);
#7128=FACE_OUTER_BOUND('',#12393,.T.);
#7129=FACE_OUTER_BOUND('',#12394,.T.);
#7130=FACE_OUTER_BOUND('',#12395,.T.);
#7131=FACE_OUTER_BOUND('',#12396,.T.);
#7132=FACE_OUTER_BOUND('',#12397,.T.);
#7133=FACE_OUTER_BOUND('',#12398,.T.);
#7134=FACE_OUTER_BOUND('',#12399,.T.);
#7135=FACE_OUTER_BOUND('',#12400,.T.);
#7136=FACE_OUTER_BOUND('',#12401,.T.);
#7137=FACE_OUTER_BOUND('',#12402,.T.);
#7138=FACE_OUTER_BOUND('',#12403,.T.);
#7139=FACE_OUTER_BOUND('',#12404,.T.);
#7140=FACE_OUTER_BOUND('',#12405,.T.);
#7141=FACE_OUTER_BOUND('',#12406,.T.);
#7142=FACE_OUTER_BOUND('',#12407,.T.);
#7143=FACE_OUTER_BOUND('',#12408,.T.);
#7144=FACE_OUTER_BOUND('',#12409,.T.);
#7145=FACE_OUTER_BOUND('',#12410,.T.);
#7146=FACE_OUTER_BOUND('',#12411,.T.);
#7147=FACE_OUTER_BOUND('',#12412,.T.);
#7148=FACE_OUTER_BOUND('',#12413,.T.);
#7149=FACE_OUTER_BOUND('',#12414,.T.);
#7150=FACE_OUTER_BOUND('',#12415,.T.);
#7151=FACE_OUTER_BOUND('',#12416,.T.);
#7152=FACE_OUTER_BOUND('',#12417,.T.);
#7153=FACE_OUTER_BOUND('',#12418,.T.);
#7154=FACE_OUTER_BOUND('',#12419,.T.);
#7155=FACE_OUTER_BOUND('',#12420,.T.);
#7156=FACE_OUTER_BOUND('',#12421,.T.);
#7157=FACE_OUTER_BOUND('',#12422,.T.);
#7158=FACE_OUTER_BOUND('',#12423,.T.);
#7159=FACE_OUTER_BOUND('',#12424,.T.);
#7160=FACE_OUTER_BOUND('',#12425,.T.);
#7161=FACE_OUTER_BOUND('',#12426,.T.);
#7162=FACE_OUTER_BOUND('',#12427,.T.);
#7163=FACE_OUTER_BOUND('',#12428,.T.);
#7164=FACE_OUTER_BOUND('',#12429,.T.);
#7165=FACE_OUTER_BOUND('',#12430,.T.);
#7166=FACE_OUTER_BOUND('',#12431,.T.);
#7167=FACE_OUTER_BOUND('',#12432,.T.);
#7168=FACE_OUTER_BOUND('',#12433,.T.);
#7169=FACE_OUTER_BOUND('',#12434,.T.);
#7170=FACE_OUTER_BOUND('',#12435,.T.);
#7171=FACE_OUTER_BOUND('',#12436,.T.);
#7172=FACE_OUTER_BOUND('',#12437,.T.);
#7173=FACE_OUTER_BOUND('',#12438,.T.);
#7174=FACE_OUTER_BOUND('',#12439,.T.);
#7175=FACE_OUTER_BOUND('',#12440,.T.);
#7176=FACE_OUTER_BOUND('',#12441,.T.);
#7177=FACE_OUTER_BOUND('',#12442,.T.);
#7178=FACE_OUTER_BOUND('',#12443,.T.);
#7179=FACE_OUTER_BOUND('',#12444,.T.);
#7180=FACE_OUTER_BOUND('',#12445,.T.);
#7181=FACE_OUTER_BOUND('',#12446,.T.);
#7182=FACE_OUTER_BOUND('',#12447,.T.);
#7183=FACE_OUTER_BOUND('',#12448,.T.);
#7184=FACE_OUTER_BOUND('',#12449,.T.);
#7185=FACE_OUTER_BOUND('',#12450,.T.);
#7186=FACE_OUTER_BOUND('',#12451,.T.);
#7187=FACE_OUTER_BOUND('',#12452,.T.);
#7188=FACE_OUTER_BOUND('',#12453,.T.);
#7189=FACE_OUTER_BOUND('',#12454,.T.);
#7190=FACE_OUTER_BOUND('',#12455,.T.);
#7191=FACE_OUTER_BOUND('',#12456,.T.);
#7192=FACE_OUTER_BOUND('',#12457,.T.);
#7193=FACE_OUTER_BOUND('',#12458,.T.);
#7194=FACE_OUTER_BOUND('',#12459,.T.);
#7195=FACE_OUTER_BOUND('',#12460,.T.);
#7196=FACE_OUTER_BOUND('',#12461,.T.);
#7197=FACE_OUTER_BOUND('',#12462,.T.);
#7198=FACE_OUTER_BOUND('',#12463,.T.);
#7199=FACE_OUTER_BOUND('',#12464,.T.);
#7200=FACE_OUTER_BOUND('',#12465,.T.);
#7201=FACE_OUTER_BOUND('',#12466,.T.);
#7202=FACE_OUTER_BOUND('',#12467,.T.);
#7203=FACE_OUTER_BOUND('',#12468,.T.);
#7204=FACE_OUTER_BOUND('',#12469,.T.);
#7205=FACE_OUTER_BOUND('',#12470,.T.);
#7206=FACE_OUTER_BOUND('',#12471,.T.);
#7207=FACE_OUTER_BOUND('',#12472,.T.);
#7208=FACE_OUTER_BOUND('',#12473,.T.);
#7209=FACE_OUTER_BOUND('',#12474,.T.);
#7210=FACE_OUTER_BOUND('',#12475,.T.);
#7211=FACE_OUTER_BOUND('',#12476,.T.);
#7212=FACE_OUTER_BOUND('',#12477,.T.);
#7213=FACE_OUTER_BOUND('',#12478,.T.);
#7214=FACE_OUTER_BOUND('',#12479,.T.);
#7215=FACE_OUTER_BOUND('',#12480,.T.);
#7216=FACE_OUTER_BOUND('',#12481,.T.);
#7217=FACE_OUTER_BOUND('',#12482,.T.);
#7218=FACE_OUTER_BOUND('',#12483,.T.);
#7219=FACE_OUTER_BOUND('',#12484,.T.);
#7220=FACE_OUTER_BOUND('',#12485,.T.);
#7221=FACE_OUTER_BOUND('',#12486,.T.);
#7222=FACE_OUTER_BOUND('',#12487,.T.);
#7223=FACE_OUTER_BOUND('',#12488,.T.);
#7224=FACE_OUTER_BOUND('',#12489,.T.);
#7225=FACE_OUTER_BOUND('',#12490,.T.);
#7226=FACE_OUTER_BOUND('',#12491,.T.);
#7227=FACE_OUTER_BOUND('',#12492,.T.);
#7228=FACE_OUTER_BOUND('',#12493,.T.);
#7229=FACE_OUTER_BOUND('',#12494,.T.);
#7230=FACE_OUTER_BOUND('',#12495,.T.);
#7231=FACE_OUTER_BOUND('',#12496,.T.);
#7232=FACE_OUTER_BOUND('',#12497,.T.);
#7233=FACE_OUTER_BOUND('',#12498,.T.);
#7234=FACE_OUTER_BOUND('',#12499,.T.);
#7235=FACE_OUTER_BOUND('',#12500,.T.);
#7236=FACE_OUTER_BOUND('',#12501,.T.);
#7237=FACE_OUTER_BOUND('',#12502,.T.);
#7238=FACE_OUTER_BOUND('',#12503,.T.);
#7239=FACE_OUTER_BOUND('',#12504,.T.);
#7240=FACE_OUTER_BOUND('',#12505,.T.);
#7241=FACE_OUTER_BOUND('',#12506,.T.);
#7242=FACE_OUTER_BOUND('',#12507,.T.);
#7243=FACE_OUTER_BOUND('',#12508,.T.);
#7244=FACE_OUTER_BOUND('',#12509,.T.);
#7245=FACE_OUTER_BOUND('',#12510,.T.);
#7246=FACE_OUTER_BOUND('',#12511,.T.);
#7247=FACE_OUTER_BOUND('',#12512,.T.);
#7248=FACE_OUTER_BOUND('',#12513,.T.);
#7249=FACE_OUTER_BOUND('',#12514,.T.);
#7250=FACE_OUTER_BOUND('',#12515,.T.);
#7251=FACE_OUTER_BOUND('',#12516,.T.);
#7252=FACE_OUTER_BOUND('',#12517,.T.);
#7253=FACE_OUTER_BOUND('',#12518,.T.);
#7254=FACE_OUTER_BOUND('',#12519,.T.);
#7255=FACE_OUTER_BOUND('',#12520,.T.);
#7256=FACE_OUTER_BOUND('',#12521,.T.);
#7257=FACE_OUTER_BOUND('',#12522,.T.);
#7258=FACE_OUTER_BOUND('',#12523,.T.);
#7259=FACE_OUTER_BOUND('',#12524,.T.);
#7260=FACE_OUTER_BOUND('',#12525,.T.);
#7261=FACE_OUTER_BOUND('',#12526,.T.);
#7262=FACE_OUTER_BOUND('',#12527,.T.);
#7263=FACE_OUTER_BOUND('',#12528,.T.);
#7264=FACE_OUTER_BOUND('',#12529,.T.);
#7265=FACE_OUTER_BOUND('',#12530,.T.);
#7266=FACE_OUTER_BOUND('',#12531,.T.);
#7267=FACE_OUTER_BOUND('',#12532,.T.);
#7268=FACE_OUTER_BOUND('',#12533,.T.);
#7269=FACE_OUTER_BOUND('',#12534,.T.);
#7270=FACE_OUTER_BOUND('',#12535,.T.);
#7271=FACE_OUTER_BOUND('',#12536,.T.);
#7272=FACE_OUTER_BOUND('',#12537,.T.);
#7273=FACE_OUTER_BOUND('',#12538,.T.);
#7274=FACE_OUTER_BOUND('',#12539,.T.);
#7275=FACE_OUTER_BOUND('',#12540,.T.);
#7276=FACE_OUTER_BOUND('',#12541,.T.);
#7277=FACE_OUTER_BOUND('',#12542,.T.);
#7278=FACE_OUTER_BOUND('',#12543,.T.);
#7279=FACE_OUTER_BOUND('',#12544,.T.);
#7280=FACE_OUTER_BOUND('',#12545,.T.);
#7281=FACE_OUTER_BOUND('',#12546,.T.);
#7282=FACE_OUTER_BOUND('',#12547,.T.);
#7283=FACE_OUTER_BOUND('',#12548,.T.);
#7284=FACE_OUTER_BOUND('',#12549,.T.);
#7285=FACE_OUTER_BOUND('',#12550,.T.);
#7286=FACE_OUTER_BOUND('',#12551,.T.);
#7287=FACE_OUTER_BOUND('',#12552,.T.);
#7288=FACE_OUTER_BOUND('',#12553,.T.);
#7289=FACE_OUTER_BOUND('',#12554,.T.);
#7290=FACE_OUTER_BOUND('',#12555,.T.);
#7291=FACE_OUTER_BOUND('',#12556,.T.);
#7292=FACE_OUTER_BOUND('',#12557,.T.);
#7293=FACE_OUTER_BOUND('',#12558,.T.);
#7294=FACE_OUTER_BOUND('',#12559,.T.);
#7295=FACE_OUTER_BOUND('',#12560,.T.);
#7296=FACE_OUTER_BOUND('',#12561,.T.);
#7297=FACE_OUTER_BOUND('',#12562,.T.);
#7298=FACE_OUTER_BOUND('',#12563,.T.);
#7299=FACE_OUTER_BOUND('',#12564,.T.);
#7300=FACE_OUTER_BOUND('',#12565,.T.);
#7301=FACE_OUTER_BOUND('',#12566,.T.);
#7302=FACE_OUTER_BOUND('',#12567,.T.);
#7303=FACE_OUTER_BOUND('',#12568,.T.);
#7304=FACE_OUTER_BOUND('',#12569,.T.);
#7305=FACE_OUTER_BOUND('',#12570,.T.);
#7306=FACE_OUTER_BOUND('',#12571,.T.);
#7307=FACE_OUTER_BOUND('',#12572,.T.);
#7308=FACE_OUTER_BOUND('',#12573,.T.);
#7309=FACE_OUTER_BOUND('',#12574,.T.);
#7310=FACE_OUTER_BOUND('',#12575,.T.);
#7311=FACE_OUTER_BOUND('',#12576,.T.);
#7312=FACE_OUTER_BOUND('',#12577,.T.);
#7313=FACE_OUTER_BOUND('',#12578,.T.);
#7314=FACE_OUTER_BOUND('',#12579,.T.);
#7315=FACE_OUTER_BOUND('',#12580,.T.);
#7316=FACE_OUTER_BOUND('',#12581,.T.);
#7317=FACE_OUTER_BOUND('',#12582,.T.);
#7318=FACE_OUTER_BOUND('',#12583,.T.);
#7319=FACE_OUTER_BOUND('',#12584,.T.);
#7320=FACE_OUTER_BOUND('',#12585,.T.);
#7321=FACE_OUTER_BOUND('',#12586,.T.);
#7322=FACE_OUTER_BOUND('',#12587,.T.);
#7323=FACE_OUTER_BOUND('',#12588,.T.);
#7324=FACE_OUTER_BOUND('',#12589,.T.);
#7325=FACE_OUTER_BOUND('',#12590,.T.);
#7326=FACE_OUTER_BOUND('',#12591,.T.);
#7327=FACE_OUTER_BOUND('',#12592,.T.);
#7328=FACE_OUTER_BOUND('',#12593,.T.);
#7329=FACE_OUTER_BOUND('',#12594,.T.);
#7330=FACE_OUTER_BOUND('',#12595,.T.);
#7331=FACE_OUTER_BOUND('',#12596,.T.);
#7332=FACE_OUTER_BOUND('',#12597,.T.);
#7333=FACE_OUTER_BOUND('',#12598,.T.);
#7334=FACE_OUTER_BOUND('',#12599,.T.);
#7335=FACE_OUTER_BOUND('',#12600,.T.);
#7336=FACE_OUTER_BOUND('',#12601,.T.);
#7337=FACE_OUTER_BOUND('',#12602,.T.);
#7338=FACE_OUTER_BOUND('',#12603,.T.);
#7339=FACE_OUTER_BOUND('',#12604,.T.);
#7340=FACE_OUTER_BOUND('',#12605,.T.);
#7341=FACE_OUTER_BOUND('',#12606,.T.);
#7342=FACE_OUTER_BOUND('',#12607,.T.);
#7343=FACE_OUTER_BOUND('',#12608,.T.);
#7344=FACE_OUTER_BOUND('',#12609,.T.);
#7345=FACE_OUTER_BOUND('',#12610,.T.);
#7346=FACE_OUTER_BOUND('',#12611,.T.);
#7347=FACE_OUTER_BOUND('',#12612,.T.);
#7348=FACE_OUTER_BOUND('',#12613,.T.);
#7349=FACE_OUTER_BOUND('',#12614,.T.);
#7350=FACE_OUTER_BOUND('',#12615,.T.);
#7351=FACE_OUTER_BOUND('',#12616,.T.);
#7352=FACE_OUTER_BOUND('',#12617,.T.);
#7353=FACE_OUTER_BOUND('',#12618,.T.);
#7354=FACE_OUTER_BOUND('',#12619,.T.);
#7355=FACE_OUTER_BOUND('',#12620,.T.);
#7356=FACE_OUTER_BOUND('',#12621,.T.);
#7357=FACE_OUTER_BOUND('',#12622,.T.);
#7358=FACE_OUTER_BOUND('',#12623,.T.);
#7359=FACE_OUTER_BOUND('',#12624,.T.);
#7360=FACE_OUTER_BOUND('',#12625,.T.);
#7361=FACE_OUTER_BOUND('',#12626,.T.);
#7362=FACE_OUTER_BOUND('',#12627,.T.);
#7363=FACE_OUTER_BOUND('',#12628,.T.);
#7364=FACE_OUTER_BOUND('',#12629,.T.);
#7365=FACE_OUTER_BOUND('',#12630,.T.);
#7366=FACE_OUTER_BOUND('',#12631,.T.);
#7367=FACE_OUTER_BOUND('',#12632,.T.);
#7368=FACE_OUTER_BOUND('',#12633,.T.);
#7369=FACE_OUTER_BOUND('',#12634,.T.);
#7370=FACE_OUTER_BOUND('',#12635,.T.);
#7371=FACE_OUTER_BOUND('',#12636,.T.);
#7372=FACE_OUTER_BOUND('',#12637,.T.);
#7373=FACE_OUTER_BOUND('',#12638,.T.);
#7374=FACE_OUTER_BOUND('',#12639,.T.);
#7375=FACE_OUTER_BOUND('',#12640,.T.);
#7376=FACE_OUTER_BOUND('',#12641,.T.);
#7377=FACE_OUTER_BOUND('',#12642,.T.);
#7378=FACE_OUTER_BOUND('',#12643,.T.);
#7379=FACE_OUTER_BOUND('',#12644,.T.);
#7380=FACE_OUTER_BOUND('',#12645,.T.);
#7381=FACE_OUTER_BOUND('',#12646,.T.);
#7382=FACE_OUTER_BOUND('',#12647,.T.);
#7383=FACE_OUTER_BOUND('',#12648,.T.);
#7384=FACE_OUTER_BOUND('',#12649,.T.);
#7385=FACE_OUTER_BOUND('',#12650,.T.);
#7386=FACE_OUTER_BOUND('',#12651,.T.);
#7387=FACE_OUTER_BOUND('',#12652,.T.);
#7388=FACE_OUTER_BOUND('',#12653,.T.);
#7389=FACE_OUTER_BOUND('',#12654,.T.);
#7390=FACE_OUTER_BOUND('',#12655,.T.);
#7391=FACE_OUTER_BOUND('',#12656,.T.);
#7392=FACE_OUTER_BOUND('',#12657,.T.);
#7393=FACE_OUTER_BOUND('',#12658,.T.);
#7394=FACE_OUTER_BOUND('',#12659,.T.);
#7395=FACE_OUTER_BOUND('',#12660,.T.);
#7396=FACE_OUTER_BOUND('',#12661,.T.);
#7397=FACE_OUTER_BOUND('',#12662,.T.);
#7398=FACE_OUTER_BOUND('',#12663,.T.);
#7399=FACE_OUTER_BOUND('',#12664,.T.);
#7400=FACE_OUTER_BOUND('',#12665,.T.);
#7401=FACE_OUTER_BOUND('',#12666,.T.);
#7402=FACE_OUTER_BOUND('',#12667,.T.);
#7403=FACE_OUTER_BOUND('',#12668,.T.);
#7404=FACE_OUTER_BOUND('',#12669,.T.);
#7405=FACE_OUTER_BOUND('',#12670,.T.);
#7406=FACE_OUTER_BOUND('',#12671,.T.);
#7407=FACE_OUTER_BOUND('',#12672,.T.);
#7408=FACE_OUTER_BOUND('',#12673,.T.);
#7409=FACE_OUTER_BOUND('',#12674,.T.);
#7410=FACE_OUTER_BOUND('',#12675,.T.);
#7411=FACE_OUTER_BOUND('',#12676,.T.);
#7412=FACE_OUTER_BOUND('',#12677,.T.);
#7413=FACE_OUTER_BOUND('',#12678,.T.);
#7414=FACE_OUTER_BOUND('',#12679,.T.);
#7415=FACE_OUTER_BOUND('',#12680,.T.);
#7416=FACE_OUTER_BOUND('',#12681,.T.);
#7417=FACE_OUTER_BOUND('',#12682,.T.);
#7418=FACE_OUTER_BOUND('',#12683,.T.);
#7419=FACE_OUTER_BOUND('',#12684,.T.);
#7420=FACE_OUTER_BOUND('',#12685,.T.);
#7421=FACE_OUTER_BOUND('',#12686,.T.);
#7422=FACE_OUTER_BOUND('',#12687,.T.);
#7423=FACE_OUTER_BOUND('',#12688,.T.);
#7424=FACE_OUTER_BOUND('',#12689,.T.);
#7425=FACE_OUTER_BOUND('',#12690,.T.);
#7426=FACE_OUTER_BOUND('',#12691,.T.);
#7427=FACE_OUTER_BOUND('',#12692,.T.);
#7428=FACE_OUTER_BOUND('',#12693,.T.);
#7429=FACE_OUTER_BOUND('',#12694,.T.);
#7430=FACE_OUTER_BOUND('',#12695,.T.);
#7431=FACE_OUTER_BOUND('',#12696,.T.);
#7432=FACE_OUTER_BOUND('',#12697,.T.);
#7433=FACE_OUTER_BOUND('',#12698,.T.);
#7434=FACE_OUTER_BOUND('',#12699,.T.);
#7435=FACE_OUTER_BOUND('',#12700,.T.);
#7436=FACE_OUTER_BOUND('',#12701,.T.);
#7437=FACE_OUTER_BOUND('',#12702,.T.);
#7438=FACE_OUTER_BOUND('',#12703,.T.);
#7439=FACE_OUTER_BOUND('',#12704,.T.);
#7440=FACE_OUTER_BOUND('',#12705,.T.);
#7441=FACE_OUTER_BOUND('',#12706,.T.);
#7442=FACE_OUTER_BOUND('',#12707,.T.);
#7443=FACE_OUTER_BOUND('',#12708,.T.);
#7444=FACE_OUTER_BOUND('',#12709,.T.);
#7445=FACE_OUTER_BOUND('',#12710,.T.);
#7446=FACE_OUTER_BOUND('',#12711,.T.);
#7447=FACE_OUTER_BOUND('',#12712,.T.);
#7448=FACE_OUTER_BOUND('',#12713,.T.);
#7449=FACE_OUTER_BOUND('',#12714,.T.);
#7450=FACE_OUTER_BOUND('',#12715,.T.);
#7451=FACE_OUTER_BOUND('',#12716,.T.);
#7452=FACE_OUTER_BOUND('',#12717,.T.);
#7453=FACE_OUTER_BOUND('',#12718,.T.);
#7454=FACE_OUTER_BOUND('',#12719,.T.);
#7455=FACE_OUTER_BOUND('',#12720,.T.);
#7456=FACE_OUTER_BOUND('',#12721,.T.);
#7457=FACE_OUTER_BOUND('',#12722,.T.);
#7458=FACE_OUTER_BOUND('',#12723,.T.);
#7459=FACE_OUTER_BOUND('',#12724,.T.);
#7460=FACE_OUTER_BOUND('',#12725,.T.);
#7461=FACE_OUTER_BOUND('',#12726,.T.);
#7462=FACE_OUTER_BOUND('',#12727,.T.);
#7463=FACE_OUTER_BOUND('',#12728,.T.);
#7464=FACE_OUTER_BOUND('',#12729,.T.);
#7465=FACE_OUTER_BOUND('',#12730,.T.);
#7466=FACE_OUTER_BOUND('',#12731,.T.);
#7467=FACE_OUTER_BOUND('',#12732,.T.);
#7468=FACE_OUTER_BOUND('',#12733,.T.);
#7469=FACE_OUTER_BOUND('',#12734,.T.);
#7470=FACE_OUTER_BOUND('',#12735,.T.);
#7471=FACE_OUTER_BOUND('',#12736,.T.);
#7472=FACE_OUTER_BOUND('',#12737,.T.);
#7473=FACE_OUTER_BOUND('',#12738,.T.);
#7474=FACE_OUTER_BOUND('',#12739,.T.);
#7475=FACE_OUTER_BOUND('',#12740,.T.);
#7476=FACE_OUTER_BOUND('',#12741,.T.);
#7477=FACE_OUTER_BOUND('',#12742,.T.);
#7478=FACE_OUTER_BOUND('',#12743,.T.);
#7479=FACE_OUTER_BOUND('',#12744,.T.);
#7480=FACE_OUTER_BOUND('',#12745,.T.);
#7481=FACE_OUTER_BOUND('',#12746,.T.);
#7482=FACE_OUTER_BOUND('',#12747,.T.);
#7483=FACE_OUTER_BOUND('',#12748,.T.);
#7484=FACE_OUTER_BOUND('',#12749,.T.);
#7485=FACE_OUTER_BOUND('',#12750,.T.);
#7486=FACE_OUTER_BOUND('',#12751,.T.);
#7487=FACE_OUTER_BOUND('',#12752,.T.);
#7488=FACE_OUTER_BOUND('',#12753,.T.);
#7489=FACE_OUTER_BOUND('',#12754,.T.);
#7490=FACE_OUTER_BOUND('',#12755,.T.);
#7491=FACE_OUTER_BOUND('',#12756,.T.);
#7492=FACE_OUTER_BOUND('',#12757,.T.);
#7493=FACE_OUTER_BOUND('',#12758,.T.);
#7494=FACE_OUTER_BOUND('',#12759,.T.);
#7495=FACE_OUTER_BOUND('',#12760,.T.);
#7496=FACE_OUTER_BOUND('',#12761,.T.);
#7497=FACE_OUTER_BOUND('',#12762,.T.);
#7498=FACE_OUTER_BOUND('',#12763,.T.);
#7499=FACE_OUTER_BOUND('',#12764,.T.);
#7500=FACE_OUTER_BOUND('',#12765,.T.);
#7501=FACE_OUTER_BOUND('',#12766,.T.);
#7502=FACE_OUTER_BOUND('',#12767,.T.);
#7503=FACE_OUTER_BOUND('',#12768,.T.);
#7504=FACE_OUTER_BOUND('',#12769,.T.);
#7505=FACE_OUTER_BOUND('',#12770,.T.);
#7506=FACE_OUTER_BOUND('',#12771,.T.);
#7507=FACE_OUTER_BOUND('',#12772,.T.);
#7508=FACE_OUTER_BOUND('',#12773,.T.);
#7509=FACE_OUTER_BOUND('',#12774,.T.);
#7510=FACE_OUTER_BOUND('',#12775,.T.);
#7511=FACE_OUTER_BOUND('',#12776,.T.);
#7512=FACE_OUTER_BOUND('',#12777,.T.);
#7513=FACE_OUTER_BOUND('',#12778,.T.);
#7514=FACE_OUTER_BOUND('',#12779,.T.);
#7515=FACE_OUTER_BOUND('',#12780,.T.);
#7516=FACE_OUTER_BOUND('',#12781,.T.);
#7517=FACE_OUTER_BOUND('',#12782,.T.);
#7518=FACE_OUTER_BOUND('',#12783,.T.);
#7519=FACE_OUTER_BOUND('',#12784,.T.);
#7520=FACE_OUTER_BOUND('',#12785,.T.);
#7521=FACE_OUTER_BOUND('',#12786,.T.);
#7522=FACE_OUTER_BOUND('',#12787,.T.);
#7523=FACE_OUTER_BOUND('',#12788,.T.);
#7524=FACE_OUTER_BOUND('',#12789,.T.);
#7525=FACE_OUTER_BOUND('',#12790,.T.);
#7526=FACE_OUTER_BOUND('',#12791,.T.);
#7527=FACE_OUTER_BOUND('',#12792,.T.);
#7528=FACE_OUTER_BOUND('',#12793,.T.);
#7529=FACE_OUTER_BOUND('',#12794,.T.);
#7530=FACE_OUTER_BOUND('',#12795,.T.);
#7531=FACE_OUTER_BOUND('',#12796,.T.);
#7532=FACE_OUTER_BOUND('',#12797,.T.);
#7533=FACE_OUTER_BOUND('',#12798,.T.);
#7534=FACE_OUTER_BOUND('',#12799,.T.);
#7535=FACE_OUTER_BOUND('',#12800,.T.);
#7536=FACE_OUTER_BOUND('',#12801,.T.);
#7537=FACE_OUTER_BOUND('',#12802,.T.);
#7538=FACE_OUTER_BOUND('',#12803,.T.);
#7539=FACE_OUTER_BOUND('',#12804,.T.);
#7540=FACE_OUTER_BOUND('',#12805,.T.);
#7541=FACE_OUTER_BOUND('',#12806,.T.);
#7542=FACE_OUTER_BOUND('',#12807,.T.);
#7543=FACE_OUTER_BOUND('',#12808,.T.);
#7544=FACE_OUTER_BOUND('',#12809,.T.);
#7545=FACE_OUTER_BOUND('',#12810,.T.);
#7546=FACE_OUTER_BOUND('',#12811,.T.);
#7547=FACE_OUTER_BOUND('',#12812,.T.);
#7548=FACE_OUTER_BOUND('',#12813,.T.);
#7549=FACE_OUTER_BOUND('',#12814,.T.);
#7550=FACE_OUTER_BOUND('',#12815,.T.);
#7551=FACE_OUTER_BOUND('',#12816,.T.);
#7552=FACE_OUTER_BOUND('',#12817,.T.);
#7553=FACE_OUTER_BOUND('',#12818,.T.);
#7554=FACE_OUTER_BOUND('',#12819,.T.);
#7555=FACE_OUTER_BOUND('',#12820,.T.);
#7556=FACE_OUTER_BOUND('',#12821,.T.);
#7557=FACE_OUTER_BOUND('',#12822,.T.);
#7558=FACE_OUTER_BOUND('',#12823,.T.);
#7559=FACE_OUTER_BOUND('',#12824,.T.);
#7560=FACE_OUTER_BOUND('',#12825,.T.);
#7561=FACE_OUTER_BOUND('',#12826,.T.);
#7562=FACE_OUTER_BOUND('',#12827,.T.);
#7563=FACE_OUTER_BOUND('',#12828,.T.);
#7564=FACE_OUTER_BOUND('',#12829,.T.);
#7565=FACE_OUTER_BOUND('',#12830,.T.);
#7566=FACE_OUTER_BOUND('',#12831,.T.);
#7567=FACE_OUTER_BOUND('',#12832,.T.);
#7568=FACE_OUTER_BOUND('',#12833,.T.);
#7569=FACE_OUTER_BOUND('',#12834,.T.);
#7570=FACE_OUTER_BOUND('',#12835,.T.);
#7571=FACE_OUTER_BOUND('',#12836,.T.);
#7572=FACE_OUTER_BOUND('',#12837,.T.);
#7573=FACE_OUTER_BOUND('',#12838,.T.);
#7574=FACE_OUTER_BOUND('',#12839,.T.);
#7575=FACE_OUTER_BOUND('',#12840,.T.);
#7576=FACE_OUTER_BOUND('',#12841,.T.);
#7577=FACE_OUTER_BOUND('',#12842,.T.);
#7578=FACE_OUTER_BOUND('',#12843,.T.);
#7579=FACE_OUTER_BOUND('',#12844,.T.);
#7580=FACE_OUTER_BOUND('',#12845,.T.);
#7581=FACE_OUTER_BOUND('',#12846,.T.);
#7582=FACE_OUTER_BOUND('',#12847,.T.);
#7583=FACE_OUTER_BOUND('',#12848,.T.);
#7584=FACE_OUTER_BOUND('',#12849,.T.);
#7585=FACE_OUTER_BOUND('',#12850,.T.);
#7586=FACE_OUTER_BOUND('',#12851,.T.);
#7587=FACE_OUTER_BOUND('',#12852,.T.);
#7588=FACE_OUTER_BOUND('',#12853,.T.);
#7589=FACE_OUTER_BOUND('',#12854,.T.);
#7590=FACE_OUTER_BOUND('',#12855,.T.);
#7591=FACE_OUTER_BOUND('',#12856,.T.);
#7592=FACE_OUTER_BOUND('',#12857,.T.);
#7593=FACE_OUTER_BOUND('',#12858,.T.);
#7594=FACE_OUTER_BOUND('',#12859,.T.);
#7595=FACE_OUTER_BOUND('',#12860,.T.);
#7596=FACE_OUTER_BOUND('',#12861,.T.);
#7597=FACE_OUTER_BOUND('',#12862,.T.);
#7598=FACE_OUTER_BOUND('',#12863,.T.);
#7599=FACE_OUTER_BOUND('',#12864,.T.);
#7600=FACE_OUTER_BOUND('',#12865,.T.);
#7601=FACE_OUTER_BOUND('',#12866,.T.);
#7602=FACE_OUTER_BOUND('',#12867,.T.);
#7603=FACE_OUTER_BOUND('',#12868,.T.);
#7604=FACE_OUTER_BOUND('',#12869,.T.);
#7605=FACE_OUTER_BOUND('',#12870,.T.);
#7606=FACE_OUTER_BOUND('',#12871,.T.);
#7607=FACE_OUTER_BOUND('',#12872,.T.);
#7608=FACE_OUTER_BOUND('',#12873,.T.);
#7609=FACE_OUTER_BOUND('',#12874,.T.);
#7610=FACE_OUTER_BOUND('',#12875,.T.);
#7611=FACE_OUTER_BOUND('',#12876,.T.);
#7612=FACE_OUTER_BOUND('',#12877,.T.);
#7613=FACE_OUTER_BOUND('',#12878,.T.);
#7614=FACE_OUTER_BOUND('',#12879,.T.);
#7615=FACE_OUTER_BOUND('',#12880,.T.);
#7616=FACE_OUTER_BOUND('',#12881,.T.);
#7617=FACE_OUTER_BOUND('',#12882,.T.);
#7618=FACE_OUTER_BOUND('',#12883,.T.);
#7619=FACE_OUTER_BOUND('',#12884,.T.);
#7620=FACE_OUTER_BOUND('',#12885,.T.);
#7621=FACE_OUTER_BOUND('',#12886,.T.);
#7622=FACE_OUTER_BOUND('',#12887,.T.);
#7623=FACE_OUTER_BOUND('',#12888,.T.);
#7624=FACE_OUTER_BOUND('',#12889,.T.);
#7625=FACE_OUTER_BOUND('',#12890,.T.);
#7626=FACE_OUTER_BOUND('',#12891,.T.);
#7627=FACE_OUTER_BOUND('',#12892,.T.);
#7628=FACE_OUTER_BOUND('',#12893,.T.);
#7629=FACE_OUTER_BOUND('',#12894,.T.);
#7630=FACE_OUTER_BOUND('',#12895,.T.);
#7631=FACE_OUTER_BOUND('',#12896,.T.);
#7632=FACE_OUTER_BOUND('',#12897,.T.);
#7633=FACE_OUTER_BOUND('',#12898,.T.);
#7634=FACE_OUTER_BOUND('',#12899,.T.);
#7635=FACE_OUTER_BOUND('',#12900,.T.);
#7636=FACE_OUTER_BOUND('',#12901,.T.);
#7637=FACE_OUTER_BOUND('',#12902,.T.);
#7638=FACE_OUTER_BOUND('',#12903,.T.);
#7639=FACE_OUTER_BOUND('',#12904,.T.);
#7640=FACE_OUTER_BOUND('',#12905,.T.);
#7641=FACE_OUTER_BOUND('',#12906,.T.);
#7642=FACE_OUTER_BOUND('',#12907,.T.);
#7643=FACE_OUTER_BOUND('',#12908,.T.);
#7644=FACE_OUTER_BOUND('',#12909,.T.);
#7645=FACE_OUTER_BOUND('',#12910,.T.);
#7646=FACE_OUTER_BOUND('',#12911,.T.);
#7647=FACE_OUTER_BOUND('',#12912,.T.);
#7648=FACE_OUTER_BOUND('',#12913,.T.);
#7649=FACE_OUTER_BOUND('',#12914,.T.);
#7650=FACE_OUTER_BOUND('',#12915,.T.);
#7651=FACE_OUTER_BOUND('',#12916,.T.);
#7652=FACE_OUTER_BOUND('',#12917,.T.);
#7653=FACE_OUTER_BOUND('',#12918,.T.);
#7654=FACE_OUTER_BOUND('',#12919,.T.);
#7655=FACE_OUTER_BOUND('',#12920,.T.);
#7656=FACE_OUTER_BOUND('',#12921,.T.);
#7657=FACE_OUTER_BOUND('',#12922,.T.);
#7658=FACE_OUTER_BOUND('',#12923,.T.);
#7659=FACE_OUTER_BOUND('',#12924,.T.);
#7660=FACE_OUTER_BOUND('',#12925,.T.);
#7661=FACE_OUTER_BOUND('',#12926,.T.);
#7662=FACE_OUTER_BOUND('',#12927,.T.);
#7663=FACE_OUTER_BOUND('',#12928,.T.);
#7664=FACE_OUTER_BOUND('',#12929,.T.);
#7665=FACE_OUTER_BOUND('',#12930,.T.);
#7666=FACE_OUTER_BOUND('',#12931,.T.);
#7667=FACE_OUTER_BOUND('',#12932,.T.);
#7668=FACE_OUTER_BOUND('',#12933,.T.);
#7669=FACE_OUTER_BOUND('',#12934,.T.);
#7670=FACE_OUTER_BOUND('',#12935,.T.);
#7671=FACE_OUTER_BOUND('',#12936,.T.);
#7672=FACE_OUTER_BOUND('',#12937,.T.);
#7673=FACE_OUTER_BOUND('',#12938,.T.);
#7674=FACE_OUTER_BOUND('',#12939,.T.);
#7675=FACE_OUTER_BOUND('',#12940,.T.);
#7676=FACE_OUTER_BOUND('',#12941,.T.);
#7677=FACE_OUTER_BOUND('',#12942,.T.);
#7678=FACE_OUTER_BOUND('',#12943,.T.);
#7679=FACE_OUTER_BOUND('',#12944,.T.);
#7680=FACE_OUTER_BOUND('',#12945,.T.);
#7681=FACE_OUTER_BOUND('',#12946,.T.);
#7682=FACE_OUTER_BOUND('',#12947,.T.);
#7683=FACE_OUTER_BOUND('',#12948,.T.);
#7684=FACE_OUTER_BOUND('',#12949,.T.);
#7685=FACE_OUTER_BOUND('',#12950,.T.);
#7686=FACE_OUTER_BOUND('',#12951,.T.);
#7687=FACE_OUTER_BOUND('',#12952,.T.);
#7688=FACE_OUTER_BOUND('',#12953,.T.);
#7689=FACE_OUTER_BOUND('',#12954,.T.);
#7690=FACE_OUTER_BOUND('',#12955,.T.);
#7691=FACE_OUTER_BOUND('',#12956,.T.);
#7692=FACE_OUTER_BOUND('',#12957,.T.);
#7693=FACE_OUTER_BOUND('',#12958,.T.);
#7694=FACE_OUTER_BOUND('',#12959,.T.);
#7695=FACE_OUTER_BOUND('',#12960,.T.);
#7696=FACE_OUTER_BOUND('',#12961,.T.);
#7697=FACE_OUTER_BOUND('',#12962,.T.);
#7698=FACE_OUTER_BOUND('',#12963,.T.);
#7699=FACE_OUTER_BOUND('',#12964,.T.);
#7700=FACE_OUTER_BOUND('',#12965,.T.);
#7701=FACE_OUTER_BOUND('',#12966,.T.);
#7702=FACE_OUTER_BOUND('',#12967,.T.);
#7703=FACE_OUTER_BOUND('',#12968,.T.);
#7704=FACE_OUTER_BOUND('',#12969,.T.);
#7705=FACE_OUTER_BOUND('',#12970,.T.);
#7706=FACE_OUTER_BOUND('',#12971,.T.);
#7707=FACE_OUTER_BOUND('',#12972,.T.);
#7708=FACE_OUTER_BOUND('',#12973,.T.);
#7709=FACE_OUTER_BOUND('',#12974,.T.);
#7710=FACE_OUTER_BOUND('',#12975,.T.);
#7711=FACE_OUTER_BOUND('',#12976,.T.);
#7712=FACE_OUTER_BOUND('',#12977,.T.);
#7713=FACE_OUTER_BOUND('',#12978,.T.);
#7714=FACE_OUTER_BOUND('',#12979,.T.);
#7715=FACE_OUTER_BOUND('',#12980,.T.);
#7716=FACE_OUTER_BOUND('',#12981,.T.);
#7717=FACE_OUTER_BOUND('',#12982,.T.);
#7718=FACE_OUTER_BOUND('',#12983,.T.);
#7719=FACE_OUTER_BOUND('',#12984,.T.);
#7720=FACE_OUTER_BOUND('',#12985,.T.);
#7721=FACE_OUTER_BOUND('',#12986,.T.);
#7722=FACE_OUTER_BOUND('',#12987,.T.);
#7723=FACE_OUTER_BOUND('',#12988,.T.);
#7724=FACE_OUTER_BOUND('',#12989,.T.);
#7725=FACE_OUTER_BOUND('',#12990,.T.);
#7726=FACE_OUTER_BOUND('',#12991,.T.);
#7727=FACE_OUTER_BOUND('',#12992,.T.);
#7728=FACE_OUTER_BOUND('',#12993,.T.);
#7729=FACE_OUTER_BOUND('',#12994,.T.);
#7730=FACE_OUTER_BOUND('',#12995,.T.);
#7731=FACE_OUTER_BOUND('',#12996,.T.);
#7732=FACE_OUTER_BOUND('',#12997,.T.);
#7733=FACE_OUTER_BOUND('',#12998,.T.);
#7734=FACE_OUTER_BOUND('',#12999,.T.);
#7735=FACE_OUTER_BOUND('',#13000,.T.);
#7736=FACE_OUTER_BOUND('',#13001,.T.);
#7737=FACE_OUTER_BOUND('',#13002,.T.);
#7738=FACE_OUTER_BOUND('',#13003,.T.);
#7739=FACE_OUTER_BOUND('',#13004,.T.);
#7740=FACE_OUTER_BOUND('',#13005,.T.);
#7741=FACE_OUTER_BOUND('',#13006,.T.);
#7742=FACE_OUTER_BOUND('',#13007,.T.);
#7743=FACE_OUTER_BOUND('',#13008,.T.);
#7744=FACE_OUTER_BOUND('',#13009,.T.);
#7745=FACE_OUTER_BOUND('',#13010,.T.);
#7746=FACE_OUTER_BOUND('',#13011,.T.);
#7747=FACE_OUTER_BOUND('',#13012,.T.);
#7748=FACE_OUTER_BOUND('',#13013,.T.);
#7749=FACE_OUTER_BOUND('',#13014,.T.);
#7750=FACE_OUTER_BOUND('',#13015,.T.);
#7751=FACE_OUTER_BOUND('',#13016,.T.);
#7752=FACE_OUTER_BOUND('',#13017,.T.);
#7753=FACE_OUTER_BOUND('',#13018,.T.);
#7754=FACE_OUTER_BOUND('',#13019,.T.);
#7755=FACE_OUTER_BOUND('',#13020,.T.);
#7756=FACE_OUTER_BOUND('',#13021,.T.);
#7757=FACE_OUTER_BOUND('',#13022,.T.);
#7758=FACE_OUTER_BOUND('',#13023,.T.);
#7759=FACE_OUTER_BOUND('',#13024,.T.);
#7760=FACE_OUTER_BOUND('',#13025,.T.);
#7761=FACE_OUTER_BOUND('',#13026,.T.);
#7762=FACE_OUTER_BOUND('',#13027,.T.);
#7763=FACE_OUTER_BOUND('',#13028,.T.);
#7764=FACE_OUTER_BOUND('',#13029,.T.);
#7765=FACE_OUTER_BOUND('',#13030,.T.);
#7766=FACE_OUTER_BOUND('',#13031,.T.);
#7767=FACE_OUTER_BOUND('',#13032,.T.);
#7768=FACE_OUTER_BOUND('',#13033,.T.);
#7769=FACE_OUTER_BOUND('',#13034,.T.);
#7770=FACE_OUTER_BOUND('',#13035,.T.);
#7771=FACE_OUTER_BOUND('',#13036,.T.);
#7772=FACE_OUTER_BOUND('',#13037,.T.);
#7773=FACE_OUTER_BOUND('',#13038,.T.);
#7774=FACE_OUTER_BOUND('',#13039,.T.);
#7775=FACE_OUTER_BOUND('',#13040,.T.);
#7776=FACE_OUTER_BOUND('',#13041,.T.);
#7777=FACE_OUTER_BOUND('',#13042,.T.);
#7778=FACE_OUTER_BOUND('',#13043,.T.);
#7779=FACE_OUTER_BOUND('',#13044,.T.);
#7780=FACE_OUTER_BOUND('',#13045,.T.);
#7781=FACE_OUTER_BOUND('',#13046,.T.);
#7782=FACE_OUTER_BOUND('',#13047,.T.);
#7783=FACE_OUTER_BOUND('',#13048,.T.);
#7784=FACE_OUTER_BOUND('',#13049,.T.);
#7785=FACE_OUTER_BOUND('',#13050,.T.);
#7786=FACE_OUTER_BOUND('',#13051,.T.);
#7787=FACE_OUTER_BOUND('',#13052,.T.);
#7788=FACE_OUTER_BOUND('',#13053,.T.);
#7789=FACE_OUTER_BOUND('',#13054,.T.);
#7790=FACE_OUTER_BOUND('',#13055,.T.);
#7791=FACE_OUTER_BOUND('',#13056,.T.);
#7792=FACE_OUTER_BOUND('',#13057,.T.);
#7793=FACE_OUTER_BOUND('',#13058,.T.);
#7794=FACE_OUTER_BOUND('',#13059,.T.);
#7795=FACE_OUTER_BOUND('',#13060,.T.);
#7796=FACE_OUTER_BOUND('',#13061,.T.);
#7797=FACE_OUTER_BOUND('',#13062,.T.);
#7798=FACE_OUTER_BOUND('',#13063,.T.);
#7799=FACE_OUTER_BOUND('',#13064,.T.);
#7800=FACE_OUTER_BOUND('',#13065,.T.);
#7801=FACE_OUTER_BOUND('',#13066,.T.);
#7802=FACE_OUTER_BOUND('',#13067,.T.);
#7803=FACE_OUTER_BOUND('',#13068,.T.);
#7804=FACE_OUTER_BOUND('',#13069,.T.);
#7805=FACE_OUTER_BOUND('',#13070,.T.);
#7806=FACE_OUTER_BOUND('',#13071,.T.);
#7807=FACE_OUTER_BOUND('',#13072,.T.);
#7808=FACE_OUTER_BOUND('',#13073,.T.);
#7809=FACE_OUTER_BOUND('',#13074,.T.);
#7810=FACE_OUTER_BOUND('',#13075,.T.);
#7811=FACE_OUTER_BOUND('',#13076,.T.);
#7812=FACE_OUTER_BOUND('',#13077,.T.);
#7813=FACE_OUTER_BOUND('',#13078,.T.);
#7814=FACE_OUTER_BOUND('',#13079,.T.);
#7815=FACE_OUTER_BOUND('',#13080,.T.);
#7816=FACE_OUTER_BOUND('',#13081,.T.);
#7817=FACE_OUTER_BOUND('',#13082,.T.);
#7818=FACE_OUTER_BOUND('',#13083,.T.);
#7819=FACE_OUTER_BOUND('',#13084,.T.);
#7820=FACE_OUTER_BOUND('',#13085,.T.);
#7821=FACE_OUTER_BOUND('',#13086,.T.);
#7822=FACE_OUTER_BOUND('',#13087,.T.);
#7823=FACE_OUTER_BOUND('',#13088,.T.);
#7824=FACE_OUTER_BOUND('',#13089,.T.);
#7825=FACE_OUTER_BOUND('',#13090,.T.);
#7826=FACE_OUTER_BOUND('',#13091,.T.);
#7827=FACE_OUTER_BOUND('',#13092,.T.);
#7828=FACE_OUTER_BOUND('',#13093,.T.);
#7829=FACE_OUTER_BOUND('',#13094,.T.);
#7830=FACE_OUTER_BOUND('',#13095,.T.);
#7831=FACE_OUTER_BOUND('',#13096,.T.);
#7832=FACE_OUTER_BOUND('',#13097,.T.);
#7833=FACE_OUTER_BOUND('',#13098,.T.);
#7834=FACE_OUTER_BOUND('',#13099,.T.);
#7835=FACE_OUTER_BOUND('',#13100,.T.);
#7836=FACE_OUTER_BOUND('',#13101,.T.);
#7837=FACE_OUTER_BOUND('',#13102,.T.);
#7838=FACE_OUTER_BOUND('',#13103,.T.);
#7839=FACE_OUTER_BOUND('',#13104,.T.);
#7840=FACE_OUTER_BOUND('',#13105,.T.);
#7841=FACE_OUTER_BOUND('',#13106,.T.);
#7842=FACE_OUTER_BOUND('',#13107,.T.);
#7843=FACE_OUTER_BOUND('',#13108,.T.);
#7844=FACE_OUTER_BOUND('',#13109,.T.);
#7845=FACE_OUTER_BOUND('',#13110,.T.);
#7846=FACE_OUTER_BOUND('',#13111,.T.);
#7847=FACE_OUTER_BOUND('',#13112,.T.);
#7848=FACE_OUTER_BOUND('',#13113,.T.);
#7849=FACE_OUTER_BOUND('',#13114,.T.);
#7850=FACE_OUTER_BOUND('',#13115,.T.);
#7851=FACE_OUTER_BOUND('',#13116,.T.);
#7852=FACE_OUTER_BOUND('',#13117,.T.);
#7853=FACE_OUTER_BOUND('',#13118,.T.);
#7854=FACE_OUTER_BOUND('',#13119,.T.);
#7855=FACE_OUTER_BOUND('',#13120,.T.);
#7856=FACE_OUTER_BOUND('',#13121,.T.);
#7857=FACE_OUTER_BOUND('',#13122,.T.);
#7858=FACE_OUTER_BOUND('',#13123,.T.);
#7859=FACE_OUTER_BOUND('',#13124,.T.);
#7860=FACE_OUTER_BOUND('',#13125,.T.);
#7861=FACE_OUTER_BOUND('',#13126,.T.);
#7862=FACE_OUTER_BOUND('',#13127,.T.);
#7863=FACE_OUTER_BOUND('',#13128,.T.);
#7864=FACE_OUTER_BOUND('',#13129,.T.);
#7865=FACE_OUTER_BOUND('',#13130,.T.);
#7866=FACE_OUTER_BOUND('',#13131,.T.);
#7867=FACE_OUTER_BOUND('',#13132,.T.);
#7868=FACE_OUTER_BOUND('',#13133,.T.);
#7869=FACE_OUTER_BOUND('',#13134,.T.);
#7870=FACE_OUTER_BOUND('',#13135,.T.);
#7871=FACE_OUTER_BOUND('',#13136,.T.);
#7872=FACE_OUTER_BOUND('',#13137,.T.);
#7873=FACE_OUTER_BOUND('',#13138,.T.);
#7874=FACE_OUTER_BOUND('',#13139,.T.);
#7875=FACE_OUTER_BOUND('',#13140,.T.);
#7876=FACE_OUTER_BOUND('',#13141,.T.);
#7877=FACE_OUTER_BOUND('',#13142,.T.);
#7878=FACE_OUTER_BOUND('',#13143,.T.);
#7879=FACE_OUTER_BOUND('',#13144,.T.);
#7880=FACE_OUTER_BOUND('',#13145,.T.);
#7881=FACE_OUTER_BOUND('',#13146,.T.);
#7882=FACE_OUTER_BOUND('',#13147,.T.);
#7883=FACE_OUTER_BOUND('',#13148,.T.);
#7884=FACE_OUTER_BOUND('',#13149,.T.);
#7885=FACE_OUTER_BOUND('',#13150,.T.);
#7886=FACE_OUTER_BOUND('',#13151,.T.);
#7887=FACE_OUTER_BOUND('',#13152,.T.);
#7888=FACE_OUTER_BOUND('',#13153,.T.);
#7889=FACE_OUTER_BOUND('',#13154,.T.);
#7890=FACE_OUTER_BOUND('',#13155,.T.);
#7891=FACE_OUTER_BOUND('',#13156,.T.);
#7892=FACE_OUTER_BOUND('',#13157,.T.);
#7893=FACE_OUTER_BOUND('',#13158,.T.);
#7894=FACE_OUTER_BOUND('',#13159,.T.);
#7895=FACE_OUTER_BOUND('',#13160,.T.);
#7896=FACE_OUTER_BOUND('',#13161,.T.);
#7897=FACE_OUTER_BOUND('',#13162,.T.);
#7898=FACE_OUTER_BOUND('',#13163,.T.);
#7899=FACE_OUTER_BOUND('',#13164,.T.);
#7900=FACE_OUTER_BOUND('',#13165,.T.);
#7901=FACE_OUTER_BOUND('',#13166,.T.);
#7902=FACE_OUTER_BOUND('',#13167,.T.);
#7903=FACE_OUTER_BOUND('',#13168,.T.);
#7904=FACE_OUTER_BOUND('',#13169,.T.);
#7905=FACE_OUTER_BOUND('',#13170,.T.);
#7906=FACE_OUTER_BOUND('',#13171,.T.);
#7907=FACE_OUTER_BOUND('',#13172,.T.);
#7908=FACE_OUTER_BOUND('',#13173,.T.);
#7909=FACE_OUTER_BOUND('',#13174,.T.);
#7910=FACE_OUTER_BOUND('',#13175,.T.);
#7911=FACE_OUTER_BOUND('',#13176,.T.);
#7912=FACE_OUTER_BOUND('',#13177,.T.);
#7913=FACE_OUTER_BOUND('',#13178,.T.);
#7914=FACE_OUTER_BOUND('',#13179,.T.);
#7915=FACE_OUTER_BOUND('',#13180,.T.);
#7916=FACE_OUTER_BOUND('',#13181,.T.);
#7917=FACE_OUTER_BOUND('',#13182,.T.);
#7918=FACE_OUTER_BOUND('',#13183,.T.);
#7919=FACE_OUTER_BOUND('',#13184,.T.);
#7920=FACE_OUTER_BOUND('',#13185,.T.);
#7921=FACE_OUTER_BOUND('',#13186,.T.);
#7922=FACE_OUTER_BOUND('',#13187,.T.);
#7923=FACE_OUTER_BOUND('',#13188,.T.);
#7924=FACE_OUTER_BOUND('',#13189,.T.);
#7925=FACE_OUTER_BOUND('',#13190,.T.);
#7926=FACE_OUTER_BOUND('',#13191,.T.);
#7927=FACE_OUTER_BOUND('',#13192,.T.);
#7928=FACE_OUTER_BOUND('',#13193,.T.);
#7929=FACE_OUTER_BOUND('',#13194,.T.);
#7930=FACE_OUTER_BOUND('',#13195,.T.);
#7931=FACE_OUTER_BOUND('',#13196,.T.);
#7932=FACE_OUTER_BOUND('',#13197,.T.);
#7933=FACE_OUTER_BOUND('',#13198,.T.);
#7934=FACE_OUTER_BOUND('',#13199,.T.);
#7935=FACE_OUTER_BOUND('',#13200,.T.);
#7936=FACE_OUTER_BOUND('',#13201,.T.);
#7937=FACE_OUTER_BOUND('',#13202,.T.);
#7938=FACE_OUTER_BOUND('',#13203,.T.);
#7939=FACE_OUTER_BOUND('',#13204,.T.);
#7940=FACE_OUTER_BOUND('',#13205,.T.);
#7941=FACE_OUTER_BOUND('',#13206,.T.);
#7942=FACE_OUTER_BOUND('',#13207,.T.);
#7943=FACE_OUTER_BOUND('',#13208,.T.);
#7944=FACE_OUTER_BOUND('',#13209,.T.);
#7945=FACE_OUTER_BOUND('',#13210,.T.);
#7946=FACE_OUTER_BOUND('',#13211,.T.);
#7947=FACE_OUTER_BOUND('',#13212,.T.);
#7948=FACE_OUTER_BOUND('',#13213,.T.);
#7949=FACE_OUTER_BOUND('',#13214,.T.);
#7950=FACE_OUTER_BOUND('',#13215,.T.);
#7951=FACE_OUTER_BOUND('',#13216,.T.);
#7952=FACE_OUTER_BOUND('',#13217,.T.);
#7953=FACE_OUTER_BOUND('',#13218,.T.);
#7954=FACE_OUTER_BOUND('',#13219,.T.);
#7955=FACE_OUTER_BOUND('',#13220,.T.);
#7956=FACE_OUTER_BOUND('',#13221,.T.);
#7957=FACE_OUTER_BOUND('',#13222,.T.);
#7958=FACE_OUTER_BOUND('',#13223,.T.);
#7959=FACE_OUTER_BOUND('',#13224,.T.);
#7960=FACE_OUTER_BOUND('',#13225,.T.);
#7961=FACE_OUTER_BOUND('',#13226,.T.);
#7962=FACE_OUTER_BOUND('',#13227,.T.);
#7963=FACE_OUTER_BOUND('',#13228,.T.);
#7964=FACE_OUTER_BOUND('',#13229,.T.);
#7965=FACE_OUTER_BOUND('',#13230,.T.);
#7966=FACE_OUTER_BOUND('',#13231,.T.);
#7967=FACE_OUTER_BOUND('',#13232,.T.);
#7968=FACE_OUTER_BOUND('',#13233,.T.);
#7969=FACE_OUTER_BOUND('',#13234,.T.);
#7970=FACE_OUTER_BOUND('',#13235,.T.);
#7971=FACE_OUTER_BOUND('',#13236,.T.);
#7972=FACE_OUTER_BOUND('',#13237,.T.);
#7973=FACE_OUTER_BOUND('',#13238,.T.);
#7974=FACE_OUTER_BOUND('',#13239,.T.);
#7975=FACE_OUTER_BOUND('',#13240,.T.);
#7976=FACE_OUTER_BOUND('',#13241,.T.);
#7977=FACE_OUTER_BOUND('',#13242,.T.);
#7978=FACE_OUTER_BOUND('',#13243,.T.);
#7979=FACE_OUTER_BOUND('',#13244,.T.);
#7980=FACE_OUTER_BOUND('',#13245,.T.);
#7981=FACE_OUTER_BOUND('',#13246,.T.);
#7982=FACE_OUTER_BOUND('',#13247,.T.);
#7983=FACE_OUTER_BOUND('',#13248,.T.);
#7984=FACE_OUTER_BOUND('',#13249,.T.);
#7985=FACE_OUTER_BOUND('',#13250,.T.);
#7986=FACE_OUTER_BOUND('',#13251,.T.);
#7987=FACE_OUTER_BOUND('',#13252,.T.);
#7988=FACE_OUTER_BOUND('',#13253,.T.);
#7989=FACE_OUTER_BOUND('',#13254,.T.);
#7990=FACE_OUTER_BOUND('',#13255,.T.);
#7991=FACE_OUTER_BOUND('',#13256,.T.);
#7992=FACE_OUTER_BOUND('',#13257,.T.);
#7993=FACE_OUTER_BOUND('',#13258,.T.);
#7994=FACE_OUTER_BOUND('',#13259,.T.);
#7995=FACE_OUTER_BOUND('',#13260,.T.);
#7996=FACE_OUTER_BOUND('',#13261,.T.);
#7997=FACE_OUTER_BOUND('',#13262,.T.);
#7998=FACE_OUTER_BOUND('',#13263,.T.);
#7999=FACE_OUTER_BOUND('',#13264,.T.);
#8000=FACE_OUTER_BOUND('',#13265,.T.);
#8001=FACE_OUTER_BOUND('',#13266,.T.);
#8002=FACE_OUTER_BOUND('',#13267,.T.);
#8003=FACE_OUTER_BOUND('',#13268,.T.);
#8004=FACE_OUTER_BOUND('',#13269,.T.);
#8005=FACE_OUTER_BOUND('',#13270,.T.);
#8006=FACE_OUTER_BOUND('',#13271,.T.);
#8007=FACE_OUTER_BOUND('',#13272,.T.);
#8008=FACE_OUTER_BOUND('',#13273,.T.);
#8009=FACE_OUTER_BOUND('',#13274,.T.);
#8010=FACE_OUTER_BOUND('',#13275,.T.);
#8011=FACE_OUTER_BOUND('',#13276,.T.);
#8012=FACE_OUTER_BOUND('',#13277,.T.);
#8013=FACE_OUTER_BOUND('',#13278,.T.);
#8014=FACE_OUTER_BOUND('',#13279,.T.);
#8015=FACE_OUTER_BOUND('',#13280,.T.);
#8016=FACE_OUTER_BOUND('',#13281,.T.);
#8017=FACE_OUTER_BOUND('',#13282,.T.);
#8018=FACE_OUTER_BOUND('',#13283,.T.);
#8019=FACE_OUTER_BOUND('',#13284,.T.);
#8020=FACE_OUTER_BOUND('',#13285,.T.);
#8021=FACE_OUTER_BOUND('',#13286,.T.);
#8022=FACE_OUTER_BOUND('',#13287,.T.);
#8023=FACE_OUTER_BOUND('',#13288,.T.);
#8024=FACE_OUTER_BOUND('',#13289,.T.);
#8025=FACE_OUTER_BOUND('',#13290,.T.);
#8026=FACE_OUTER_BOUND('',#13291,.T.);
#8027=FACE_OUTER_BOUND('',#13292,.T.);
#8028=FACE_OUTER_BOUND('',#13293,.T.);
#8029=FACE_OUTER_BOUND('',#13294,.T.);
#8030=FACE_OUTER_BOUND('',#13295,.T.);
#8031=FACE_OUTER_BOUND('',#13296,.T.);
#8032=FACE_OUTER_BOUND('',#13297,.T.);
#8033=FACE_OUTER_BOUND('',#13298,.T.);
#8034=FACE_OUTER_BOUND('',#13299,.T.);
#8035=FACE_OUTER_BOUND('',#13300,.T.);
#8036=FACE_OUTER_BOUND('',#13301,.T.);
#8037=FACE_OUTER_BOUND('',#13302,.T.);
#8038=FACE_OUTER_BOUND('',#13303,.T.);
#8039=FACE_OUTER_BOUND('',#13304,.T.);
#8040=FACE_OUTER_BOUND('',#13305,.T.);
#8041=FACE_OUTER_BOUND('',#13306,.T.);
#8042=FACE_OUTER_BOUND('',#13307,.T.);
#8043=FACE_OUTER_BOUND('',#13308,.T.);
#8044=FACE_OUTER_BOUND('',#13309,.T.);
#8045=FACE_OUTER_BOUND('',#13310,.T.);
#8046=FACE_OUTER_BOUND('',#13311,.T.);
#8047=FACE_OUTER_BOUND('',#13312,.T.);
#8048=FACE_OUTER_BOUND('',#13313,.T.);
#8049=FACE_OUTER_BOUND('',#13314,.T.);
#8050=FACE_OUTER_BOUND('',#13315,.T.);
#8051=FACE_OUTER_BOUND('',#13316,.T.);
#8052=FACE_OUTER_BOUND('',#13317,.T.);
#8053=FACE_OUTER_BOUND('',#13318,.T.);
#8054=FACE_OUTER_BOUND('',#13319,.T.);
#8055=FACE_OUTER_BOUND('',#13320,.T.);
#8056=FACE_OUTER_BOUND('',#13321,.T.);
#8057=FACE_OUTER_BOUND('',#13322,.T.);
#8058=FACE_OUTER_BOUND('',#13323,.T.);
#8059=FACE_OUTER_BOUND('',#13324,.T.);
#8060=FACE_OUTER_BOUND('',#13325,.T.);
#8061=FACE_OUTER_BOUND('',#13326,.T.);
#8062=FACE_OUTER_BOUND('',#13327,.T.);
#8063=FACE_OUTER_BOUND('',#13328,.T.);
#8064=FACE_OUTER_BOUND('',#13329,.T.);
#8065=FACE_OUTER_BOUND('',#13330,.T.);
#8066=FACE_OUTER_BOUND('',#13331,.T.);
#8067=FACE_OUTER_BOUND('',#13332,.T.);
#8068=FACE_OUTER_BOUND('',#13333,.T.);
#8069=FACE_OUTER_BOUND('',#13334,.T.);
#8070=FACE_OUTER_BOUND('',#13335,.T.);
#8071=FACE_OUTER_BOUND('',#13336,.T.);
#8072=FACE_OUTER_BOUND('',#13337,.T.);
#8073=FACE_OUTER_BOUND('',#13338,.T.);
#8074=FACE_OUTER_BOUND('',#13339,.T.);
#8075=FACE_OUTER_BOUND('',#13340,.T.);
#8076=FACE_OUTER_BOUND('',#13341,.T.);
#8077=FACE_OUTER_BOUND('',#13342,.T.);
#8078=FACE_OUTER_BOUND('',#13343,.T.);
#8079=FACE_OUTER_BOUND('',#13344,.T.);
#8080=FACE_OUTER_BOUND('',#13345,.T.);
#8081=FACE_OUTER_BOUND('',#13346,.T.);
#8082=FACE_OUTER_BOUND('',#13347,.T.);
#8083=FACE_OUTER_BOUND('',#13348,.T.);
#8084=FACE_OUTER_BOUND('',#13349,.T.);
#8085=FACE_OUTER_BOUND('',#13350,.T.);
#8086=FACE_OUTER_BOUND('',#13351,.T.);
#8087=FACE_OUTER_BOUND('',#13352,.T.);
#8088=FACE_OUTER_BOUND('',#13353,.T.);
#8089=FACE_OUTER_BOUND('',#13354,.T.);
#8090=FACE_OUTER_BOUND('',#13355,.T.);
#8091=FACE_OUTER_BOUND('',#13356,.T.);
#8092=FACE_OUTER_BOUND('',#13357,.T.);
#8093=FACE_OUTER_BOUND('',#13358,.T.);
#8094=FACE_OUTER_BOUND('',#13359,.T.);
#8095=FACE_OUTER_BOUND('',#13360,.T.);
#8096=FACE_OUTER_BOUND('',#13361,.T.);
#8097=FACE_OUTER_BOUND('',#13362,.T.);
#8098=FACE_OUTER_BOUND('',#13363,.T.);
#8099=FACE_OUTER_BOUND('',#13364,.T.);
#8100=FACE_OUTER_BOUND('',#13365,.T.);
#8101=FACE_OUTER_BOUND('',#13366,.T.);
#8102=FACE_OUTER_BOUND('',#13367,.T.);
#8103=FACE_OUTER_BOUND('',#13368,.T.);
#8104=FACE_OUTER_BOUND('',#13369,.T.);
#8105=FACE_OUTER_BOUND('',#13370,.T.);
#8106=FACE_OUTER_BOUND('',#13371,.T.);
#8107=FACE_OUTER_BOUND('',#13372,.T.);
#8108=FACE_OUTER_BOUND('',#13373,.T.);
#8109=FACE_OUTER_BOUND('',#13374,.T.);
#8110=FACE_OUTER_BOUND('',#13375,.T.);
#8111=FACE_OUTER_BOUND('',#13376,.T.);
#8112=FACE_OUTER_BOUND('',#13377,.T.);
#8113=FACE_OUTER_BOUND('',#13378,.T.);
#8114=FACE_OUTER_BOUND('',#13379,.T.);
#8115=FACE_OUTER_BOUND('',#13380,.T.);
#8116=FACE_OUTER_BOUND('',#13381,.T.);
#8117=FACE_OUTER_BOUND('',#13382,.T.);
#8118=FACE_OUTER_BOUND('',#13383,.T.);
#8119=FACE_OUTER_BOUND('',#13384,.T.);
#8120=FACE_OUTER_BOUND('',#13385,.T.);
#8121=FACE_OUTER_BOUND('',#13386,.T.);
#8122=FACE_OUTER_BOUND('',#13387,.T.);
#8123=FACE_OUTER_BOUND('',#13388,.T.);
#8124=FACE_OUTER_BOUND('',#13389,.T.);
#8125=FACE_OUTER_BOUND('',#13390,.T.);
#8126=FACE_OUTER_BOUND('',#13391,.T.);
#8127=FACE_OUTER_BOUND('',#13392,.T.);
#8128=FACE_OUTER_BOUND('',#13393,.T.);
#8129=FACE_OUTER_BOUND('',#13394,.T.);
#8130=FACE_OUTER_BOUND('',#13395,.T.);
#8131=FACE_OUTER_BOUND('',#13396,.T.);
#8132=FACE_OUTER_BOUND('',#13397,.T.);
#8133=FACE_OUTER_BOUND('',#13398,.T.);
#8134=FACE_OUTER_BOUND('',#13399,.T.);
#8135=FACE_OUTER_BOUND('',#13400,.T.);
#8136=FACE_OUTER_BOUND('',#13401,.T.);
#8137=FACE_OUTER_BOUND('',#13402,.T.);
#8138=FACE_OUTER_BOUND('',#13403,.T.);
#8139=FACE_OUTER_BOUND('',#13404,.T.);
#8140=FACE_OUTER_BOUND('',#13405,.T.);
#8141=FACE_OUTER_BOUND('',#13406,.T.);
#8142=FACE_OUTER_BOUND('',#13407,.T.);
#8143=FACE_OUTER_BOUND('',#13408,.T.);
#8144=FACE_OUTER_BOUND('',#13409,.T.);
#8145=FACE_OUTER_BOUND('',#13410,.T.);
#8146=FACE_OUTER_BOUND('',#13411,.T.);
#8147=FACE_OUTER_BOUND('',#13412,.T.);
#8148=FACE_OUTER_BOUND('',#13413,.T.);
#8149=FACE_OUTER_BOUND('',#13414,.T.);
#8150=FACE_OUTER_BOUND('',#13415,.T.);
#8151=FACE_OUTER_BOUND('',#13416,.T.);
#8152=FACE_OUTER_BOUND('',#13417,.T.);
#8153=FACE_OUTER_BOUND('',#13418,.T.);
#8154=FACE_OUTER_BOUND('',#13419,.T.);
#8155=FACE_OUTER_BOUND('',#13420,.T.);
#8156=FACE_OUTER_BOUND('',#13421,.T.);
#8157=FACE_OUTER_BOUND('',#13422,.T.);
#8158=FACE_OUTER_BOUND('',#13423,.T.);
#8159=FACE_OUTER_BOUND('',#13424,.T.);
#8160=FACE_OUTER_BOUND('',#13425,.T.);
#8161=FACE_OUTER_BOUND('',#13426,.T.);
#8162=FACE_OUTER_BOUND('',#13427,.T.);
#8163=FACE_OUTER_BOUND('',#13428,.T.);
#8164=FACE_OUTER_BOUND('',#13429,.T.);
#8165=FACE_OUTER_BOUND('',#13430,.T.);
#8166=FACE_OUTER_BOUND('',#13431,.T.);
#8167=FACE_OUTER_BOUND('',#13432,.T.);
#8168=FACE_OUTER_BOUND('',#13433,.T.);
#8169=FACE_OUTER_BOUND('',#13434,.T.);
#8170=FACE_OUTER_BOUND('',#13435,.T.);
#8171=FACE_OUTER_BOUND('',#13436,.T.);
#8172=FACE_OUTER_BOUND('',#13437,.T.);
#8173=FACE_OUTER_BOUND('',#13438,.T.);
#8174=FACE_OUTER_BOUND('',#13439,.T.);
#8175=FACE_OUTER_BOUND('',#13440,.T.);
#8176=FACE_OUTER_BOUND('',#13441,.T.);
#8177=FACE_OUTER_BOUND('',#13442,.T.);
#8178=FACE_OUTER_BOUND('',#13443,.T.);
#8179=FACE_OUTER_BOUND('',#13444,.T.);
#8180=FACE_OUTER_BOUND('',#13445,.T.);
#8181=FACE_OUTER_BOUND('',#13446,.T.);
#8182=FACE_OUTER_BOUND('',#13447,.T.);
#8183=FACE_OUTER_BOUND('',#13448,.T.);
#8184=FACE_OUTER_BOUND('',#13449,.T.);
#8185=FACE_OUTER_BOUND('',#13450,.T.);
#8186=FACE_OUTER_BOUND('',#13451,.T.);
#8187=FACE_OUTER_BOUND('',#13452,.T.);
#8188=FACE_OUTER_BOUND('',#13453,.T.);
#8189=FACE_OUTER_BOUND('',#13454,.T.);
#8190=FACE_OUTER_BOUND('',#13455,.T.);
#8191=FACE_OUTER_BOUND('',#13456,.T.);
#8192=FACE_OUTER_BOUND('',#13457,.T.);
#8193=FACE_OUTER_BOUND('',#13458,.T.);
#8194=FACE_OUTER_BOUND('',#13459,.T.);
#8195=FACE_OUTER_BOUND('',#13460,.T.);
#8196=FACE_OUTER_BOUND('',#13461,.T.);
#8197=FACE_OUTER_BOUND('',#13462,.T.);
#8198=FACE_OUTER_BOUND('',#13463,.T.);
#8199=FACE_OUTER_BOUND('',#13464,.T.);
#8200=FACE_OUTER_BOUND('',#13465,.T.);
#8201=FACE_OUTER_BOUND('',#13466,.T.);
#8202=FACE_OUTER_BOUND('',#13467,.T.);
#8203=FACE_OUTER_BOUND('',#13468,.T.);
#8204=FACE_OUTER_BOUND('',#13469,.T.);
#8205=FACE_OUTER_BOUND('',#13470,.T.);
#8206=FACE_OUTER_BOUND('',#13471,.T.);
#8207=FACE_OUTER_BOUND('',#13472,.T.);
#8208=FACE_OUTER_BOUND('',#13473,.T.);
#8209=FACE_OUTER_BOUND('',#13474,.T.);
#8210=FACE_OUTER_BOUND('',#13475,.T.);
#8211=FACE_OUTER_BOUND('',#13476,.T.);
#8212=FACE_OUTER_BOUND('',#13477,.T.);
#8213=FACE_OUTER_BOUND('',#13478,.T.);
#8214=FACE_OUTER_BOUND('',#13479,.T.);
#8215=FACE_OUTER_BOUND('',#13480,.T.);
#8216=FACE_OUTER_BOUND('',#13481,.T.);
#8217=FACE_OUTER_BOUND('',#13482,.T.);
#8218=FACE_OUTER_BOUND('',#13483,.T.);
#8219=FACE_OUTER_BOUND('',#13484,.T.);
#8220=FACE_OUTER_BOUND('',#13485,.T.);
#8221=FACE_OUTER_BOUND('',#13486,.T.);
#8222=FACE_OUTER_BOUND('',#13487,.T.);
#8223=FACE_OUTER_BOUND('',#13488,.T.);
#8224=FACE_OUTER_BOUND('',#13489,.T.);
#8225=FACE_OUTER_BOUND('',#13490,.T.);
#8226=FACE_OUTER_BOUND('',#13491,.T.);
#8227=FACE_OUTER_BOUND('',#13492,.T.);
#8228=FACE_OUTER_BOUND('',#13493,.T.);
#8229=FACE_OUTER_BOUND('',#13494,.T.);
#8230=FACE_OUTER_BOUND('',#13495,.T.);
#8231=FACE_OUTER_BOUND('',#13496,.T.);
#8232=FACE_OUTER_BOUND('',#13497,.T.);
#8233=FACE_OUTER_BOUND('',#13498,.T.);
#8234=FACE_OUTER_BOUND('',#13499,.T.);
#8235=FACE_OUTER_BOUND('',#13500,.T.);
#8236=FACE_OUTER_BOUND('',#13501,.T.);
#8237=FACE_OUTER_BOUND('',#13502,.T.);
#8238=FACE_OUTER_BOUND('',#13503,.T.);
#8239=FACE_OUTER_BOUND('',#13504,.T.);
#8240=FACE_OUTER_BOUND('',#13505,.T.);
#8241=FACE_OUTER_BOUND('',#13506,.T.);
#8242=FACE_OUTER_BOUND('',#13507,.T.);
#8243=FACE_OUTER_BOUND('',#13508,.T.);
#8244=FACE_OUTER_BOUND('',#13509,.T.);
#8245=FACE_OUTER_BOUND('',#13510,.T.);
#8246=FACE_OUTER_BOUND('',#13511,.T.);
#8247=FACE_OUTER_BOUND('',#13512,.T.);
#8248=FACE_OUTER_BOUND('',#13513,.T.);
#8249=FACE_OUTER_BOUND('',#13514,.T.);
#8250=FACE_OUTER_BOUND('',#13515,.T.);
#8251=FACE_OUTER_BOUND('',#13516,.T.);
#8252=FACE_OUTER_BOUND('',#13517,.T.);
#8253=FACE_OUTER_BOUND('',#13518,.T.);
#8254=FACE_OUTER_BOUND('',#13519,.T.);
#8255=FACE_OUTER_BOUND('',#13520,.T.);
#8256=FACE_OUTER_BOUND('',#13521,.T.);
#8257=FACE_OUTER_BOUND('',#13522,.T.);
#8258=FACE_OUTER_BOUND('',#13523,.T.);
#8259=FACE_OUTER_BOUND('',#13524,.T.);
#8260=FACE_OUTER_BOUND('',#13525,.T.);
#8261=FACE_OUTER_BOUND('',#13526,.T.);
#8262=FACE_OUTER_BOUND('',#13527,.T.);
#8263=FACE_OUTER_BOUND('',#13528,.T.);
#8264=FACE_OUTER_BOUND('',#13529,.T.);
#8265=FACE_OUTER_BOUND('',#13530,.T.);
#8266=FACE_OUTER_BOUND('',#13531,.T.);
#8267=FACE_OUTER_BOUND('',#13532,.T.);
#8268=FACE_OUTER_BOUND('',#13533,.T.);
#8269=FACE_OUTER_BOUND('',#13534,.T.);
#8270=FACE_OUTER_BOUND('',#13535,.T.);
#8271=FACE_OUTER_BOUND('',#13536,.T.);
#8272=FACE_OUTER_BOUND('',#13537,.T.);
#8273=FACE_OUTER_BOUND('',#13538,.T.);
#8274=FACE_OUTER_BOUND('',#13539,.T.);
#8275=FACE_OUTER_BOUND('',#13540,.T.);
#8276=FACE_OUTER_BOUND('',#13541,.T.);
#8277=FACE_OUTER_BOUND('',#13542,.T.);
#8278=FACE_OUTER_BOUND('',#13543,.T.);
#8279=FACE_OUTER_BOUND('',#13544,.T.);
#8280=FACE_OUTER_BOUND('',#13545,.T.);
#8281=FACE_OUTER_BOUND('',#13546,.T.);
#8282=FACE_OUTER_BOUND('',#13547,.T.);
#8283=FACE_OUTER_BOUND('',#13548,.T.);
#8284=FACE_OUTER_BOUND('',#13549,.T.);
#8285=FACE_OUTER_BOUND('',#13550,.T.);
#8286=FACE_OUTER_BOUND('',#13551,.T.);
#8287=FACE_OUTER_BOUND('',#13552,.T.);
#8288=FACE_OUTER_BOUND('',#13553,.T.);
#8289=FACE_OUTER_BOUND('',#13554,.T.);
#8290=FACE_OUTER_BOUND('',#13555,.T.);
#8291=FACE_OUTER_BOUND('',#13556,.T.);
#8292=FACE_OUTER_BOUND('',#13557,.T.);
#8293=FACE_OUTER_BOUND('',#13558,.T.);
#8294=FACE_OUTER_BOUND('',#13559,.T.);
#8295=FACE_OUTER_BOUND('',#13560,.T.);
#8296=FACE_OUTER_BOUND('',#13561,.T.);
#8297=FACE_OUTER_BOUND('',#13562,.T.);
#8298=FACE_OUTER_BOUND('',#13563,.T.);
#8299=FACE_OUTER_BOUND('',#13564,.T.);
#8300=FACE_OUTER_BOUND('',#13565,.T.);
#8301=FACE_OUTER_BOUND('',#13566,.T.);
#8302=FACE_OUTER_BOUND('',#13567,.T.);
#8303=FACE_OUTER_BOUND('',#13568,.T.);
#8304=FACE_OUTER_BOUND('',#13569,.T.);
#8305=FACE_OUTER_BOUND('',#13570,.T.);
#8306=FACE_OUTER_BOUND('',#13571,.T.);
#8307=FACE_OUTER_BOUND('',#13572,.T.);
#8308=FACE_OUTER_BOUND('',#13573,.T.);
#8309=FACE_OUTER_BOUND('',#13574,.T.);
#8310=FACE_OUTER_BOUND('',#13575,.T.);
#8311=FACE_OUTER_BOUND('',#13576,.T.);
#8312=FACE_OUTER_BOUND('',#13577,.T.);
#8313=FACE_OUTER_BOUND('',#13578,.T.);
#8314=FACE_OUTER_BOUND('',#13579,.T.);
#8315=FACE_OUTER_BOUND('',#13580,.T.);
#8316=FACE_OUTER_BOUND('',#13581,.T.);
#8317=FACE_OUTER_BOUND('',#13582,.T.);
#8318=FACE_OUTER_BOUND('',#13583,.T.);
#8319=FACE_OUTER_BOUND('',#13584,.T.);
#8320=FACE_OUTER_BOUND('',#13585,.T.);
#8321=FACE_OUTER_BOUND('',#13586,.T.);
#8322=FACE_OUTER_BOUND('',#13587,.T.);
#8323=FACE_OUTER_BOUND('',#13588,.T.);
#8324=FACE_OUTER_BOUND('',#13589,.T.);
#8325=FACE_OUTER_BOUND('',#13590,.T.);
#8326=FACE_OUTER_BOUND('',#13591,.T.);
#8327=FACE_OUTER_BOUND('',#13592,.T.);
#8328=FACE_OUTER_BOUND('',#13593,.T.);
#8329=FACE_OUTER_BOUND('',#13594,.T.);
#8330=FACE_OUTER_BOUND('',#13595,.T.);
#8331=FACE_OUTER_BOUND('',#13596,.T.);
#8332=FACE_OUTER_BOUND('',#13597,.T.);
#8333=FACE_OUTER_BOUND('',#13598,.T.);
#8334=FACE_OUTER_BOUND('',#13599,.T.);
#8335=FACE_OUTER_BOUND('',#13600,.T.);
#8336=FACE_OUTER_BOUND('',#13601,.T.);
#8337=FACE_OUTER_BOUND('',#13602,.T.);
#8338=FACE_OUTER_BOUND('',#13603,.T.);
#8339=FACE_OUTER_BOUND('',#13604,.T.);
#8340=FACE_OUTER_BOUND('',#13605,.T.);
#8341=FACE_OUTER_BOUND('',#13606,.T.);
#8342=FACE_OUTER_BOUND('',#13607,.T.);
#8343=FACE_OUTER_BOUND('',#13608,.T.);
#8344=FACE_OUTER_BOUND('',#13609,.T.);
#8345=FACE_OUTER_BOUND('',#13610,.T.);
#8346=FACE_OUTER_BOUND('',#13611,.T.);
#8347=FACE_OUTER_BOUND('',#13612,.T.);
#8348=FACE_OUTER_BOUND('',#13613,.T.);
#8349=FACE_OUTER_BOUND('',#13614,.T.);
#8350=FACE_OUTER_BOUND('',#13615,.T.);
#8351=FACE_OUTER_BOUND('',#13616,.T.);
#8352=FACE_OUTER_BOUND('',#13617,.T.);
#8353=FACE_OUTER_BOUND('',#13618,.T.);
#8354=FACE_OUTER_BOUND('',#13619,.T.);
#8355=FACE_OUTER_BOUND('',#13620,.T.);
#8356=FACE_OUTER_BOUND('',#13621,.T.);
#8357=FACE_OUTER_BOUND('',#13622,.T.);
#8358=FACE_OUTER_BOUND('',#13623,.T.);
#8359=FACE_OUTER_BOUND('',#13624,.T.);
#8360=FACE_OUTER_BOUND('',#13625,.T.);
#8361=FACE_OUTER_BOUND('',#13626,.T.);
#8362=FACE_OUTER_BOUND('',#13627,.T.);
#8363=FACE_OUTER_BOUND('',#13628,.T.);
#8364=FACE_OUTER_BOUND('',#13629,.T.);
#8365=FACE_OUTER_BOUND('',#13630,.T.);
#8366=FACE_OUTER_BOUND('',#13631,.T.);
#8367=FACE_OUTER_BOUND('',#13632,.T.);
#8368=FACE_OUTER_BOUND('',#13633,.T.);
#8369=FACE_OUTER_BOUND('',#13634,.T.);
#8370=FACE_OUTER_BOUND('',#13635,.T.);
#8371=FACE_OUTER_BOUND('',#13636,.T.);
#8372=FACE_OUTER_BOUND('',#13637,.T.);
#8373=FACE_OUTER_BOUND('',#13638,.T.);
#8374=FACE_OUTER_BOUND('',#13639,.T.);
#8375=FACE_OUTER_BOUND('',#13640,.T.);
#8376=FACE_OUTER_BOUND('',#13641,.T.);
#8377=FACE_OUTER_BOUND('',#13642,.T.);
#8378=FACE_OUTER_BOUND('',#13643,.T.);
#8379=FACE_OUTER_BOUND('',#13644,.T.);
#8380=FACE_OUTER_BOUND('',#13645,.T.);
#8381=FACE_OUTER_BOUND('',#13646,.T.);
#8382=FACE_OUTER_BOUND('',#13647,.T.);
#8383=FACE_OUTER_BOUND('',#13648,.T.);
#8384=FACE_OUTER_BOUND('',#13649,.T.);
#8385=FACE_OUTER_BOUND('',#13650,.T.);
#8386=FACE_OUTER_BOUND('',#13651,.T.);
#8387=FACE_OUTER_BOUND('',#13652,.T.);
#8388=FACE_OUTER_BOUND('',#13653,.T.);
#8389=FACE_OUTER_BOUND('',#13654,.T.);
#8390=FACE_OUTER_BOUND('',#13655,.T.);
#8391=FACE_OUTER_BOUND('',#13656,.T.);
#8392=FACE_OUTER_BOUND('',#13657,.T.);
#8393=FACE_OUTER_BOUND('',#13658,.T.);
#8394=FACE_OUTER_BOUND('',#13659,.T.);
#8395=FACE_OUTER_BOUND('',#13660,.T.);
#8396=FACE_OUTER_BOUND('',#13661,.T.);
#8397=FACE_OUTER_BOUND('',#13662,.T.);
#8398=FACE_OUTER_BOUND('',#13663,.T.);
#8399=FACE_OUTER_BOUND('',#13664,.T.);
#8400=FACE_OUTER_BOUND('',#13665,.T.);
#8401=FACE_OUTER_BOUND('',#13666,.T.);
#8402=FACE_OUTER_BOUND('',#13667,.T.);
#8403=FACE_OUTER_BOUND('',#13668,.T.);
#8404=FACE_OUTER_BOUND('',#13669,.T.);
#8405=FACE_OUTER_BOUND('',#13670,.T.);
#8406=FACE_OUTER_BOUND('',#13671,.T.);
#8407=FACE_OUTER_BOUND('',#13672,.T.);
#8408=FACE_OUTER_BOUND('',#13673,.T.);
#8409=FACE_OUTER_BOUND('',#13674,.T.);
#8410=FACE_OUTER_BOUND('',#13675,.T.);
#8411=FACE_OUTER_BOUND('',#13676,.T.);
#8412=FACE_OUTER_BOUND('',#13677,.T.);
#8413=FACE_OUTER_BOUND('',#13678,.T.);
#8414=FACE_OUTER_BOUND('',#13679,.T.);
#8415=FACE_OUTER_BOUND('',#13680,.T.);
#8416=FACE_OUTER_BOUND('',#13681,.T.);
#8417=FACE_OUTER_BOUND('',#13682,.T.);
#8418=FACE_OUTER_BOUND('',#13683,.T.);
#8419=FACE_OUTER_BOUND('',#13684,.T.);
#8420=FACE_OUTER_BOUND('',#13685,.T.);
#8421=FACE_OUTER_BOUND('',#13686,.T.);
#8422=FACE_OUTER_BOUND('',#13687,.T.);
#8423=FACE_OUTER_BOUND('',#13688,.T.);
#8424=FACE_OUTER_BOUND('',#13689,.T.);
#8425=FACE_OUTER_BOUND('',#13690,.T.);
#8426=FACE_OUTER_BOUND('',#13691,.T.);
#8427=FACE_OUTER_BOUND('',#13692,.T.);
#8428=FACE_OUTER_BOUND('',#13693,.T.);
#8429=FACE_OUTER_BOUND('',#13694,.T.);
#8430=FACE_OUTER_BOUND('',#13695,.T.);
#8431=FACE_OUTER_BOUND('',#13696,.T.);
#8432=FACE_OUTER_BOUND('',#13697,.T.);
#8433=FACE_OUTER_BOUND('',#13698,.T.);
#8434=FACE_OUTER_BOUND('',#13699,.T.);
#8435=FACE_OUTER_BOUND('',#13700,.T.);
#8436=FACE_OUTER_BOUND('',#13701,.T.);
#8437=FACE_OUTER_BOUND('',#13702,.T.);
#8438=FACE_OUTER_BOUND('',#13703,.T.);
#8439=FACE_OUTER_BOUND('',#13704,.T.);
#8440=FACE_OUTER_BOUND('',#13705,.T.);
#8441=FACE_OUTER_BOUND('',#13706,.T.);
#8442=FACE_OUTER_BOUND('',#13707,.T.);
#8443=FACE_OUTER_BOUND('',#13708,.T.);
#8444=FACE_OUTER_BOUND('',#13709,.T.);
#8445=FACE_OUTER_BOUND('',#13710,.T.);
#8446=FACE_OUTER_BOUND('',#13711,.T.);
#8447=FACE_OUTER_BOUND('',#13712,.T.);
#8448=FACE_OUTER_BOUND('',#13713,.T.);
#8449=FACE_OUTER_BOUND('',#13714,.T.);
#8450=FACE_OUTER_BOUND('',#13715,.T.);
#8451=FACE_OUTER_BOUND('',#13716,.T.);
#8452=FACE_OUTER_BOUND('',#13717,.T.);
#8453=FACE_OUTER_BOUND('',#13718,.T.);
#8454=FACE_OUTER_BOUND('',#13719,.T.);
#8455=FACE_OUTER_BOUND('',#13720,.T.);
#8456=FACE_OUTER_BOUND('',#13721,.T.);
#8457=FACE_OUTER_BOUND('',#13722,.T.);
#8458=FACE_OUTER_BOUND('',#13723,.T.);
#8459=FACE_OUTER_BOUND('',#13724,.T.);
#8460=FACE_OUTER_BOUND('',#13725,.T.);
#8461=FACE_OUTER_BOUND('',#13726,.T.);
#8462=FACE_OUTER_BOUND('',#13727,.T.);
#8463=FACE_OUTER_BOUND('',#13728,.T.);
#8464=FACE_OUTER_BOUND('',#13729,.T.);
#8465=FACE_OUTER_BOUND('',#13730,.T.);
#8466=FACE_OUTER_BOUND('',#13731,.T.);
#8467=FACE_OUTER_BOUND('',#13732,.T.);
#8468=FACE_OUTER_BOUND('',#13733,.T.);
#8469=FACE_OUTER_BOUND('',#13734,.T.);
#8470=FACE_OUTER_BOUND('',#13735,.T.);
#8471=FACE_OUTER_BOUND('',#13736,.T.);
#8472=FACE_OUTER_BOUND('',#13737,.T.);
#8473=FACE_OUTER_BOUND('',#13738,.T.);
#8474=FACE_OUTER_BOUND('',#13739,.T.);
#8475=FACE_OUTER_BOUND('',#13740,.T.);
#8476=FACE_OUTER_BOUND('',#13741,.T.);
#8477=FACE_OUTER_BOUND('',#13742,.T.);
#8478=FACE_OUTER_BOUND('',#13743,.T.);
#8479=FACE_OUTER_BOUND('',#13744,.T.);
#8480=FACE_OUTER_BOUND('',#13745,.T.);
#8481=FACE_OUTER_BOUND('',#13746,.T.);
#8482=FACE_OUTER_BOUND('',#13747,.T.);
#8483=FACE_OUTER_BOUND('',#13748,.T.);
#8484=FACE_OUTER_BOUND('',#13749,.T.);
#8485=FACE_OUTER_BOUND('',#13750,.T.);
#8486=FACE_OUTER_BOUND('',#13751,.T.);
#8487=FACE_OUTER_BOUND('',#13752,.T.);
#8488=FACE_OUTER_BOUND('',#13753,.T.);
#8489=FACE_OUTER_BOUND('',#13754,.T.);
#8490=FACE_OUTER_BOUND('',#13755,.T.);
#8491=FACE_OUTER_BOUND('',#13756,.T.);
#8492=FACE_OUTER_BOUND('',#13757,.T.);
#8493=FACE_OUTER_BOUND('',#13758,.T.);
#8494=FACE_OUTER_BOUND('',#13759,.T.);
#8495=FACE_OUTER_BOUND('',#13760,.T.);
#8496=FACE_OUTER_BOUND('',#13761,.T.);
#8497=FACE_OUTER_BOUND('',#13762,.T.);
#8498=FACE_OUTER_BOUND('',#13763,.T.);
#8499=FACE_OUTER_BOUND('',#13764,.T.);
#8500=FACE_OUTER_BOUND('',#13765,.T.);
#8501=FACE_OUTER_BOUND('',#13766,.T.);
#8502=FACE_OUTER_BOUND('',#13767,.T.);
#8503=FACE_OUTER_BOUND('',#13768,.T.);
#8504=FACE_OUTER_BOUND('',#13769,.T.);
#8505=FACE_OUTER_BOUND('',#13770,.T.);
#8506=FACE_OUTER_BOUND('',#13771,.T.);
#8507=FACE_OUTER_BOUND('',#13772,.T.);
#8508=FACE_OUTER_BOUND('',#13773,.T.);
#8509=FACE_OUTER_BOUND('',#13774,.T.);
#8510=FACE_OUTER_BOUND('',#13775,.T.);
#8511=FACE_OUTER_BOUND('',#13776,.T.);
#8512=FACE_OUTER_BOUND('',#13777,.T.);
#8513=FACE_OUTER_BOUND('',#13778,.T.);
#8514=FACE_OUTER_BOUND('',#13779,.T.);
#8515=FACE_OUTER_BOUND('',#13780,.T.);
#8516=FACE_OUTER_BOUND('',#13781,.T.);
#8517=FACE_OUTER_BOUND('',#13782,.T.);
#8518=FACE_OUTER_BOUND('',#13783,.T.);
#8519=FACE_OUTER_BOUND('',#13784,.T.);
#8520=FACE_OUTER_BOUND('',#13785,.T.);
#8521=FACE_OUTER_BOUND('',#13786,.T.);
#8522=FACE_OUTER_BOUND('',#13787,.T.);
#8523=FACE_OUTER_BOUND('',#13788,.T.);
#8524=FACE_OUTER_BOUND('',#13789,.T.);
#8525=FACE_OUTER_BOUND('',#13790,.T.);
#8526=FACE_OUTER_BOUND('',#13791,.T.);
#8527=FACE_OUTER_BOUND('',#13792,.T.);
#8528=FACE_OUTER_BOUND('',#13793,.T.);
#8529=FACE_OUTER_BOUND('',#13794,.T.);
#8530=FACE_OUTER_BOUND('',#13795,.T.);
#8531=FACE_OUTER_BOUND('',#13796,.T.);
#8532=FACE_OUTER_BOUND('',#13797,.T.);
#8533=FACE_OUTER_BOUND('',#13798,.T.);
#8534=FACE_OUTER_BOUND('',#13799,.T.);
#8535=FACE_OUTER_BOUND('',#13800,.T.);
#8536=FACE_OUTER_BOUND('',#13801,.T.);
#8537=FACE_OUTER_BOUND('',#13802,.T.);
#8538=FACE_OUTER_BOUND('',#13803,.T.);
#8539=FACE_OUTER_BOUND('',#13804,.T.);
#8540=FACE_OUTER_BOUND('',#13805,.T.);
#8541=FACE_OUTER_BOUND('',#13806,.T.);
#8542=FACE_OUTER_BOUND('',#13807,.T.);
#8543=FACE_OUTER_BOUND('',#13808,.T.);
#8544=FACE_OUTER_BOUND('',#13809,.T.);
#8545=FACE_OUTER_BOUND('',#13810,.T.);
#8546=FACE_OUTER_BOUND('',#13811,.T.);
#8547=FACE_OUTER_BOUND('',#13812,.T.);
#8548=FACE_OUTER_BOUND('',#13813,.T.);
#8549=FACE_OUTER_BOUND('',#13814,.T.);
#8550=FACE_OUTER_BOUND('',#13815,.T.);
#8551=FACE_OUTER_BOUND('',#13816,.T.);
#8552=FACE_OUTER_BOUND('',#13817,.T.);
#8553=FACE_OUTER_BOUND('',#13818,.T.);
#8554=FACE_OUTER_BOUND('',#13819,.T.);
#8555=FACE_OUTER_BOUND('',#13820,.T.);
#8556=FACE_OUTER_BOUND('',#13821,.T.);
#8557=FACE_OUTER_BOUND('',#13822,.T.);
#8558=FACE_OUTER_BOUND('',#13823,.T.);
#8559=FACE_OUTER_BOUND('',#13824,.T.);
#8560=FACE_OUTER_BOUND('',#13825,.T.);
#8561=FACE_OUTER_BOUND('',#13826,.T.);
#8562=FACE_OUTER_BOUND('',#13827,.T.);
#8563=FACE_OUTER_BOUND('',#13828,.T.);
#8564=FACE_OUTER_BOUND('',#13829,.T.);
#8565=FACE_OUTER_BOUND('',#13830,.T.);
#8566=FACE_OUTER_BOUND('',#13831,.T.);
#8567=FACE_OUTER_BOUND('',#13832,.T.);
#8568=FACE_OUTER_BOUND('',#13833,.T.);
#8569=FACE_OUTER_BOUND('',#13834,.T.);
#8570=FACE_OUTER_BOUND('',#13835,.T.);
#8571=FACE_OUTER_BOUND('',#13836,.T.);
#8572=FACE_OUTER_BOUND('',#13837,.T.);
#8573=FACE_OUTER_BOUND('',#13838,.T.);
#8574=FACE_OUTER_BOUND('',#13839,.T.);
#8575=FACE_OUTER_BOUND('',#13840,.T.);
#8576=FACE_OUTER_BOUND('',#13841,.T.);
#8577=FACE_OUTER_BOUND('',#13842,.T.);
#8578=FACE_OUTER_BOUND('',#13843,.T.);
#8579=FACE_OUTER_BOUND('',#13844,.T.);
#8580=FACE_OUTER_BOUND('',#13845,.T.);
#8581=FACE_OUTER_BOUND('',#13846,.T.);
#8582=FACE_OUTER_BOUND('',#13847,.T.);
#8583=FACE_OUTER_BOUND('',#13848,.T.);
#8584=FACE_OUTER_BOUND('',#13849,.T.);
#8585=FACE_OUTER_BOUND('',#13850,.T.);
#8586=FACE_OUTER_BOUND('',#13851,.T.);
#8587=FACE_OUTER_BOUND('',#13852,.T.);
#8588=FACE_OUTER_BOUND('',#13853,.T.);
#8589=FACE_OUTER_BOUND('',#13854,.T.);
#8590=FACE_OUTER_BOUND('',#13855,.T.);
#8591=FACE_OUTER_BOUND('',#13856,.T.);
#8592=FACE_OUTER_BOUND('',#13857,.T.);
#8593=FACE_OUTER_BOUND('',#13858,.T.);
#8594=FACE_OUTER_BOUND('',#13859,.T.);
#8595=FACE_OUTER_BOUND('',#13860,.T.);
#8596=FACE_OUTER_BOUND('',#13861,.T.);
#8597=FACE_OUTER_BOUND('',#13862,.T.);
#8598=FACE_OUTER_BOUND('',#13863,.T.);
#8599=FACE_OUTER_BOUND('',#13864,.T.);
#8600=FACE_OUTER_BOUND('',#13865,.T.);
#8601=FACE_OUTER_BOUND('',#13866,.T.);
#8602=FACE_OUTER_BOUND('',#13867,.T.);
#8603=FACE_OUTER_BOUND('',#13868,.T.);
#8604=FACE_OUTER_BOUND('',#13869,.T.);
#8605=FACE_OUTER_BOUND('',#13870,.T.);
#8606=FACE_OUTER_BOUND('',#13871,.T.);
#8607=FACE_OUTER_BOUND('',#13872,.T.);
#8608=FACE_OUTER_BOUND('',#13873,.T.);
#8609=FACE_OUTER_BOUND('',#13874,.T.);
#8610=FACE_OUTER_BOUND('',#13875,.T.);
#8611=FACE_OUTER_BOUND('',#13876,.T.);
#8612=FACE_OUTER_BOUND('',#13877,.T.);
#8613=FACE_OUTER_BOUND('',#13878,.T.);
#8614=FACE_OUTER_BOUND('',#13879,.T.);
#8615=FACE_OUTER_BOUND('',#13880,.T.);
#8616=FACE_OUTER_BOUND('',#13881,.T.);
#8617=FACE_OUTER_BOUND('',#13882,.T.);
#8618=FACE_OUTER_BOUND('',#13883,.T.);
#8619=FACE_OUTER_BOUND('',#13884,.T.);
#8620=FACE_OUTER_BOUND('',#13885,.T.);
#8621=FACE_OUTER_BOUND('',#13886,.T.);
#8622=FACE_OUTER_BOUND('',#13887,.T.);
#8623=FACE_OUTER_BOUND('',#13888,.T.);
#8624=FACE_OUTER_BOUND('',#13889,.T.);
#8625=FACE_OUTER_BOUND('',#13890,.T.);
#8626=FACE_OUTER_BOUND('',#13891,.T.);
#8627=FACE_OUTER_BOUND('',#13892,.T.);
#8628=FACE_OUTER_BOUND('',#13893,.T.);
#8629=FACE_OUTER_BOUND('',#13894,.T.);
#8630=FACE_OUTER_BOUND('',#13895,.T.);
#8631=FACE_OUTER_BOUND('',#13896,.T.);
#8632=FACE_OUTER_BOUND('',#13897,.T.);
#8633=FACE_OUTER_BOUND('',#13898,.T.);
#8634=FACE_OUTER_BOUND('',#13899,.T.);
#8635=FACE_OUTER_BOUND('',#13900,.T.);
#8636=FACE_OUTER_BOUND('',#13901,.T.);
#8637=FACE_OUTER_BOUND('',#13902,.T.);
#8638=FACE_OUTER_BOUND('',#13903,.T.);
#8639=FACE_OUTER_BOUND('',#13904,.T.);
#8640=FACE_OUTER_BOUND('',#13905,.T.);
#8641=FACE_OUTER_BOUND('',#13906,.T.);
#8642=FACE_OUTER_BOUND('',#13907,.T.);
#8643=FACE_OUTER_BOUND('',#13908,.T.);
#8644=FACE_OUTER_BOUND('',#13909,.T.);
#8645=FACE_OUTER_BOUND('',#13910,.T.);
#8646=FACE_OUTER_BOUND('',#13911,.T.);
#8647=FACE_OUTER_BOUND('',#13912,.T.);
#8648=FACE_OUTER_BOUND('',#13913,.T.);
#8649=FACE_OUTER_BOUND('',#13914,.T.);
#8650=FACE_OUTER_BOUND('',#13915,.T.);
#8651=FACE_OUTER_BOUND('',#13916,.T.);
#8652=FACE_OUTER_BOUND('',#13917,.T.);
#8653=FACE_OUTER_BOUND('',#13918,.T.);
#8654=FACE_OUTER_BOUND('',#13919,.T.);
#8655=FACE_OUTER_BOUND('',#13920,.T.);
#8656=FACE_OUTER_BOUND('',#13921,.T.);
#8657=FACE_OUTER_BOUND('',#13922,.T.);
#8658=FACE_OUTER_BOUND('',#13923,.T.);
#8659=FACE_OUTER_BOUND('',#13924,.T.);
#8660=FACE_OUTER_BOUND('',#13925,.T.);
#8661=FACE_OUTER_BOUND('',#13926,.T.);
#8662=FACE_OUTER_BOUND('',#13927,.T.);
#8663=FACE_OUTER_BOUND('',#13928,.T.);
#8664=FACE_OUTER_BOUND('',#13929,.T.);
#8665=FACE_OUTER_BOUND('',#13930,.T.);
#8666=FACE_OUTER_BOUND('',#13931,.T.);
#8667=FACE_OUTER_BOUND('',#13932,.T.);
#8668=FACE_OUTER_BOUND('',#13933,.T.);
#8669=FACE_OUTER_BOUND('',#13934,.T.);
#8670=FACE_OUTER_BOUND('',#13935,.T.);
#8671=FACE_OUTER_BOUND('',#13936,.T.);
#8672=FACE_OUTER_BOUND('',#13937,.T.);
#8673=FACE_OUTER_BOUND('',#13938,.T.);
#8674=FACE_OUTER_BOUND('',#13939,.T.);
#8675=FACE_OUTER_BOUND('',#13940,.T.);
#8676=FACE_OUTER_BOUND('',#13941,.T.);
#8677=FACE_OUTER_BOUND('',#13942,.T.);
#8678=FACE_OUTER_BOUND('',#13943,.T.);
#8679=FACE_OUTER_BOUND('',#13944,.T.);
#8680=FACE_OUTER_BOUND('',#13945,.T.);
#8681=FACE_OUTER_BOUND('',#13946,.T.);
#8682=FACE_OUTER_BOUND('',#13947,.T.);
#8683=FACE_OUTER_BOUND('',#13948,.T.);
#8684=FACE_OUTER_BOUND('',#13949,.T.);
#8685=FACE_OUTER_BOUND('',#13950,.T.);
#8686=FACE_OUTER_BOUND('',#13951,.T.);
#8687=FACE_OUTER_BOUND('',#13952,.T.);
#8688=FACE_OUTER_BOUND('',#13953,.T.);
#8689=FACE_OUTER_BOUND('',#13954,.T.);
#8690=FACE_OUTER_BOUND('',#13955,.T.);
#8691=FACE_OUTER_BOUND('',#13956,.T.);
#8692=FACE_OUTER_BOUND('',#13957,.T.);
#8693=FACE_OUTER_BOUND('',#13958,.T.);
#8694=FACE_OUTER_BOUND('',#13959,.T.);
#8695=FACE_OUTER_BOUND('',#13960,.T.);
#8696=FACE_OUTER_BOUND('',#13961,.T.);
#8697=FACE_OUTER_BOUND('',#13962,.T.);
#8698=FACE_OUTER_BOUND('',#13963,.T.);
#8699=FACE_OUTER_BOUND('',#13964,.T.);
#8700=FACE_OUTER_BOUND('',#13965,.T.);
#8701=FACE_OUTER_BOUND('',#13966,.T.);
#8702=FACE_OUTER_BOUND('',#13967,.T.);
#8703=FACE_OUTER_BOUND('',#13968,.T.);
#8704=FACE_OUTER_BOUND('',#13969,.T.);
#8705=FACE_OUTER_BOUND('',#13970,.T.);
#8706=FACE_OUTER_BOUND('',#13971,.T.);
#8707=FACE_OUTER_BOUND('',#13972,.T.);
#8708=FACE_OUTER_BOUND('',#13973,.T.);
#8709=FACE_OUTER_BOUND('',#13974,.T.);
#8710=FACE_OUTER_BOUND('',#13975,.T.);
#8711=FACE_OUTER_BOUND('',#13976,.T.);
#8712=FACE_OUTER_BOUND('',#13977,.T.);
#8713=FACE_OUTER_BOUND('',#13978,.T.);
#8714=FACE_OUTER_BOUND('',#13979,.T.);
#8715=FACE_OUTER_BOUND('',#13980,.T.);
#8716=FACE_OUTER_BOUND('',#13981,.T.);
#8717=FACE_OUTER_BOUND('',#13982,.T.);
#8718=FACE_OUTER_BOUND('',#13983,.T.);
#8719=FACE_OUTER_BOUND('',#13984,.T.);
#8720=FACE_OUTER_BOUND('',#13985,.T.);
#8721=FACE_OUTER_BOUND('',#13986,.T.);
#8722=FACE_OUTER_BOUND('',#13987,.T.);
#8723=FACE_OUTER_BOUND('',#13988,.T.);
#8724=FACE_OUTER_BOUND('',#13989,.T.);
#8725=FACE_OUTER_BOUND('',#13990,.T.);
#8726=FACE_OUTER_BOUND('',#13991,.T.);
#8727=FACE_OUTER_BOUND('',#13992,.T.);
#8728=FACE_OUTER_BOUND('',#13993,.T.);
#8729=FACE_OUTER_BOUND('',#13994,.T.);
#8730=FACE_OUTER_BOUND('',#13995,.T.);
#8731=FACE_OUTER_BOUND('',#13996,.T.);
#8732=FACE_OUTER_BOUND('',#13997,.T.);
#8733=FACE_OUTER_BOUND('',#13998,.T.);
#8734=FACE_OUTER_BOUND('',#13999,.T.);
#8735=FACE_OUTER_BOUND('',#14000,.T.);
#8736=FACE_OUTER_BOUND('',#14001,.T.);
#8737=FACE_OUTER_BOUND('',#14002,.T.);
#8738=FACE_OUTER_BOUND('',#14003,.T.);
#8739=FACE_OUTER_BOUND('',#14004,.T.);
#8740=FACE_OUTER_BOUND('',#14005,.T.);
#8741=FACE_OUTER_BOUND('',#14006,.T.);
#8742=FACE_OUTER_BOUND('',#14007,.T.);
#8743=FACE_OUTER_BOUND('',#14008,.T.);
#8744=FACE_OUTER_BOUND('',#14009,.T.);
#8745=FACE_OUTER_BOUND('',#14010,.T.);
#8746=FACE_OUTER_BOUND('',#14011,.T.);
#8747=FACE_OUTER_BOUND('',#14012,.T.);
#8748=FACE_OUTER_BOUND('',#14013,.T.);
#8749=FACE_OUTER_BOUND('',#14014,.T.);
#8750=FACE_OUTER_BOUND('',#14015,.T.);
#8751=FACE_OUTER_BOUND('',#14016,.T.);
#8752=FACE_OUTER_BOUND('',#14017,.T.);
#8753=FACE_OUTER_BOUND('',#14018,.T.);
#8754=FACE_OUTER_BOUND('',#14019,.T.);
#8755=FACE_OUTER_BOUND('',#14020,.T.);
#8756=FACE_OUTER_BOUND('',#14021,.T.);
#8757=FACE_OUTER_BOUND('',#14022,.T.);
#8758=FACE_OUTER_BOUND('',#14023,.T.);
#8759=FACE_OUTER_BOUND('',#14024,.T.);
#8760=FACE_OUTER_BOUND('',#14025,.T.);
#8761=FACE_OUTER_BOUND('',#14026,.T.);
#8762=FACE_OUTER_BOUND('',#14027,.T.);
#8763=FACE_OUTER_BOUND('',#14028,.T.);
#8764=FACE_OUTER_BOUND('',#14029,.T.);
#8765=FACE_OUTER_BOUND('',#14030,.T.);
#8766=FACE_OUTER_BOUND('',#14031,.T.);
#8767=FACE_OUTER_BOUND('',#14032,.T.);
#8768=FACE_OUTER_BOUND('',#14033,.T.);
#8769=FACE_OUTER_BOUND('',#14034,.T.);
#8770=FACE_OUTER_BOUND('',#14035,.T.);
#8771=FACE_OUTER_BOUND('',#14036,.T.);
#8772=FACE_OUTER_BOUND('',#14037,.T.);
#8773=FACE_OUTER_BOUND('',#14038,.T.);
#8774=FACE_OUTER_BOUND('',#14039,.T.);
#8775=FACE_OUTER_BOUND('',#14040,.T.);
#8776=FACE_OUTER_BOUND('',#14041,.T.);
#8777=FACE_OUTER_BOUND('',#14042,.T.);
#8778=FACE_OUTER_BOUND('',#14043,.T.);
#8779=FACE_OUTER_BOUND('',#14044,.T.);
#8780=FACE_OUTER_BOUND('',#14045,.T.);
#8781=FACE_OUTER_BOUND('',#14046,.T.);
#8782=FACE_OUTER_BOUND('',#14047,.T.);
#8783=FACE_OUTER_BOUND('',#14048,.T.);
#8784=FACE_OUTER_BOUND('',#14049,.T.);
#8785=FACE_OUTER_BOUND('',#14050,.T.);
#8786=FACE_OUTER_BOUND('',#14051,.T.);
#8787=FACE_OUTER_BOUND('',#14052,.T.);
#8788=FACE_OUTER_BOUND('',#14053,.T.);
#8789=FACE_OUTER_BOUND('',#14054,.T.);
#8790=FACE_OUTER_BOUND('',#14055,.T.);
#8791=FACE_OUTER_BOUND('',#14056,.T.);
#8792=FACE_OUTER_BOUND('',#14057,.T.);
#8793=FACE_OUTER_BOUND('',#14058,.T.);
#8794=FACE_OUTER_BOUND('',#14059,.T.);
#8795=FACE_OUTER_BOUND('',#14060,.T.);
#8796=FACE_OUTER_BOUND('',#14061,.T.);
#8797=FACE_OUTER_BOUND('',#14062,.T.);
#8798=FACE_OUTER_BOUND('',#14063,.T.);
#8799=FACE_OUTER_BOUND('',#14064,.T.);
#8800=FACE_OUTER_BOUND('',#14065,.T.);
#8801=FACE_OUTER_BOUND('',#14066,.T.);
#8802=FACE_OUTER_BOUND('',#14067,.T.);
#8803=FACE_OUTER_BOUND('',#14068,.T.);
#8804=FACE_OUTER_BOUND('',#14069,.T.);
#8805=FACE_OUTER_BOUND('',#14070,.T.);
#8806=FACE_OUTER_BOUND('',#14071,.T.);
#8807=FACE_OUTER_BOUND('',#14072,.T.);
#8808=FACE_OUTER_BOUND('',#14073,.T.);
#8809=FACE_OUTER_BOUND('',#14074,.T.);
#8810=FACE_OUTER_BOUND('',#14075,.T.);
#8811=FACE_OUTER_BOUND('',#14076,.T.);
#8812=FACE_OUTER_BOUND('',#14077,.T.);
#8813=FACE_OUTER_BOUND('',#14078,.T.);
#8814=FACE_OUTER_BOUND('',#14079,.T.);
#8815=FACE_OUTER_BOUND('',#14080,.T.);
#8816=FACE_OUTER_BOUND('',#14081,.T.);
#8817=FACE_OUTER_BOUND('',#14082,.T.);
#8818=FACE_OUTER_BOUND('',#14083,.T.);
#8819=FACE_OUTER_BOUND('',#14084,.T.);
#8820=FACE_OUTER_BOUND('',#14085,.T.);
#8821=FACE_OUTER_BOUND('',#14086,.T.);
#8822=FACE_OUTER_BOUND('',#14087,.T.);
#8823=FACE_OUTER_BOUND('',#14088,.T.);
#8824=FACE_OUTER_BOUND('',#14089,.T.);
#8825=FACE_OUTER_BOUND('',#14090,.T.);
#8826=FACE_OUTER_BOUND('',#14091,.T.);
#8827=FACE_OUTER_BOUND('',#14092,.T.);
#8828=FACE_OUTER_BOUND('',#14093,.T.);
#8829=FACE_OUTER_BOUND('',#14094,.T.);
#8830=FACE_OUTER_BOUND('',#14095,.T.);
#8831=FACE_OUTER_BOUND('',#14096,.T.);
#8832=FACE_OUTER_BOUND('',#14097,.T.);
#8833=FACE_OUTER_BOUND('',#14098,.T.);
#8834=FACE_OUTER_BOUND('',#14099,.T.);
#8835=FACE_OUTER_BOUND('',#14100,.T.);
#8836=FACE_OUTER_BOUND('',#14101,.T.);
#8837=FACE_OUTER_BOUND('',#14102,.T.);
#8838=FACE_OUTER_BOUND('',#14103,.T.);
#8839=FACE_OUTER_BOUND('',#14104,.T.);
#8840=FACE_OUTER_BOUND('',#14105,.T.);
#8841=FACE_OUTER_BOUND('',#14106,.T.);
#8842=FACE_OUTER_BOUND('',#14107,.T.);
#8843=FACE_OUTER_BOUND('',#14108,.T.);
#8844=FACE_OUTER_BOUND('',#14109,.T.);
#8845=FACE_OUTER_BOUND('',#14110,.T.);
#8846=FACE_OUTER_BOUND('',#14111,.T.);
#8847=FACE_OUTER_BOUND('',#14112,.T.);
#8848=FACE_OUTER_BOUND('',#14113,.T.);
#8849=FACE_OUTER_BOUND('',#14114,.T.);
#8850=FACE_OUTER_BOUND('',#14115,.T.);
#8851=FACE_OUTER_BOUND('',#14116,.T.);
#8852=FACE_OUTER_BOUND('',#14117,.T.);
#8853=FACE_OUTER_BOUND('',#14118,.T.);
#8854=FACE_OUTER_BOUND('',#14119,.T.);
#8855=FACE_OUTER_BOUND('',#14120,.T.);
#8856=FACE_OUTER_BOUND('',#14121,.T.);
#8857=FACE_OUTER_BOUND('',#14122,.T.);
#8858=FACE_OUTER_BOUND('',#14123,.T.);
#8859=FACE_OUTER_BOUND('',#14124,.T.);
#8860=FACE_OUTER_BOUND('',#14125,.T.);
#8861=FACE_OUTER_BOUND('',#14126,.T.);
#8862=FACE_OUTER_BOUND('',#14127,.T.);
#8863=FACE_OUTER_BOUND('',#14128,.T.);
#8864=FACE_OUTER_BOUND('',#14129,.T.);
#8865=FACE_OUTER_BOUND('',#14130,.T.);
#8866=FACE_OUTER_BOUND('',#14131,.T.);
#8867=FACE_OUTER_BOUND('',#14132,.T.);
#8868=FACE_OUTER_BOUND('',#14133,.T.);
#8869=FACE_OUTER_BOUND('',#14134,.T.);
#8870=FACE_OUTER_BOUND('',#14135,.T.);
#8871=FACE_OUTER_BOUND('',#14136,.T.);
#8872=FACE_OUTER_BOUND('',#14137,.T.);
#8873=FACE_OUTER_BOUND('',#14138,.T.);
#8874=FACE_OUTER_BOUND('',#14139,.T.);
#8875=FACE_OUTER_BOUND('',#14140,.T.);
#8876=FACE_OUTER_BOUND('',#14141,.T.);
#8877=FACE_OUTER_BOUND('',#14142,.T.);
#8878=FACE_OUTER_BOUND('',#14143,.T.);
#8879=FACE_OUTER_BOUND('',#14144,.T.);
#8880=FACE_OUTER_BOUND('',#14145,.T.);
#8881=FACE_OUTER_BOUND('',#14146,.T.);
#8882=FACE_OUTER_BOUND('',#14147,.T.);
#8883=FACE_OUTER_BOUND('',#14148,.T.);
#8884=FACE_OUTER_BOUND('',#14149,.T.);
#8885=FACE_OUTER_BOUND('',#14150,.T.);
#8886=FACE_OUTER_BOUND('',#14151,.T.);
#8887=FACE_OUTER_BOUND('',#14152,.T.);
#8888=FACE_OUTER_BOUND('',#14153,.T.);
#8889=FACE_OUTER_BOUND('',#14154,.T.);
#8890=FACE_OUTER_BOUND('',#14155,.T.);
#8891=FACE_OUTER_BOUND('',#14156,.T.);
#8892=FACE_OUTER_BOUND('',#14157,.T.);
#8893=FACE_OUTER_BOUND('',#14158,.T.);
#8894=FACE_OUTER_BOUND('',#14159,.T.);
#8895=FACE_OUTER_BOUND('',#14160,.T.);
#8896=FACE_OUTER_BOUND('',#14161,.T.);
#8897=FACE_OUTER_BOUND('',#14162,.T.);
#8898=FACE_OUTER_BOUND('',#14163,.T.);
#8899=FACE_OUTER_BOUND('',#14164,.T.);
#8900=FACE_OUTER_BOUND('',#14165,.T.);
#8901=FACE_OUTER_BOUND('',#14166,.T.);
#8902=FACE_OUTER_BOUND('',#14167,.T.);
#8903=FACE_OUTER_BOUND('',#14168,.T.);
#8904=FACE_OUTER_BOUND('',#14169,.T.);
#8905=FACE_OUTER_BOUND('',#14170,.T.);
#8906=FACE_OUTER_BOUND('',#14171,.T.);
#8907=FACE_OUTER_BOUND('',#14172,.T.);
#8908=FACE_OUTER_BOUND('',#14173,.T.);
#8909=FACE_OUTER_BOUND('',#14174,.T.);
#8910=FACE_OUTER_BOUND('',#14175,.T.);
#8911=FACE_OUTER_BOUND('',#14176,.T.);
#8912=FACE_OUTER_BOUND('',#14177,.T.);
#8913=FACE_OUTER_BOUND('',#14178,.T.);
#8914=FACE_OUTER_BOUND('',#14179,.T.);
#8915=FACE_OUTER_BOUND('',#14180,.T.);
#8916=FACE_OUTER_BOUND('',#14181,.T.);
#8917=FACE_OUTER_BOUND('',#14182,.T.);
#8918=FACE_OUTER_BOUND('',#14183,.T.);
#8919=FACE_OUTER_BOUND('',#14184,.T.);
#8920=FACE_OUTER_BOUND('',#14185,.T.);
#8921=FACE_OUTER_BOUND('',#14186,.T.);
#8922=FACE_OUTER_BOUND('',#14187,.T.);
#8923=FACE_OUTER_BOUND('',#14188,.T.);
#8924=FACE_OUTER_BOUND('',#14189,.T.);
#8925=FACE_OUTER_BOUND('',#14190,.T.);
#8926=FACE_OUTER_BOUND('',#14191,.T.);
#8927=FACE_OUTER_BOUND('',#14192,.T.);
#8928=FACE_OUTER_BOUND('',#14193,.T.);
#8929=FACE_OUTER_BOUND('',#14194,.T.);
#8930=FACE_OUTER_BOUND('',#14195,.T.);
#8931=FACE_OUTER_BOUND('',#14196,.T.);
#8932=FACE_OUTER_BOUND('',#14197,.T.);
#8933=FACE_OUTER_BOUND('',#14198,.T.);
#8934=FACE_OUTER_BOUND('',#14199,.T.);
#8935=FACE_OUTER_BOUND('',#14200,.T.);
#8936=FACE_OUTER_BOUND('',#14201,.T.);
#8937=FACE_OUTER_BOUND('',#14202,.T.);
#8938=FACE_OUTER_BOUND('',#14203,.T.);
#8939=FACE_OUTER_BOUND('',#14204,.T.);
#8940=FACE_OUTER_BOUND('',#14205,.T.);
#8941=FACE_OUTER_BOUND('',#14206,.T.);
#8942=FACE_OUTER_BOUND('',#14207,.T.);
#8943=FACE_OUTER_BOUND('',#14208,.T.);
#8944=FACE_OUTER_BOUND('',#14209,.T.);
#8945=FACE_OUTER_BOUND('',#14210,.T.);
#8946=FACE_OUTER_BOUND('',#14211,.T.);
#8947=FACE_OUTER_BOUND('',#14212,.T.);
#8948=FACE_OUTER_BOUND('',#14213,.T.);
#8949=FACE_OUTER_BOUND('',#14214,.T.);
#8950=FACE_OUTER_BOUND('',#14215,.T.);
#8951=FACE_OUTER_BOUND('',#14216,.T.);
#8952=FACE_OUTER_BOUND('',#14217,.T.);
#8953=FACE_OUTER_BOUND('',#14218,.T.);
#8954=FACE_OUTER_BOUND('',#14219,.T.);
#8955=FACE_OUTER_BOUND('',#14220,.T.);
#8956=FACE_OUTER_BOUND('',#14221,.T.);
#8957=FACE_OUTER_BOUND('',#14222,.T.);
#8958=FACE_OUTER_BOUND('',#14223,.T.);
#8959=FACE_OUTER_BOUND('',#14224,.T.);
#8960=FACE_OUTER_BOUND('',#14225,.T.);
#8961=FACE_OUTER_BOUND('',#14226,.T.);
#8962=FACE_OUTER_BOUND('',#14227,.T.);
#8963=FACE_OUTER_BOUND('',#14228,.T.);
#8964=FACE_OUTER_BOUND('',#14229,.T.);
#8965=FACE_OUTER_BOUND('',#14230,.T.);
#8966=FACE_OUTER_BOUND('',#14231,.T.);
#8967=FACE_OUTER_BOUND('',#14232,.T.);
#8968=FACE_OUTER_BOUND('',#14233,.T.);
#8969=FACE_OUTER_BOUND('',#14234,.T.);
#8970=FACE_OUTER_BOUND('',#14235,.T.);
#8971=FACE_OUTER_BOUND('',#14236,.T.);
#8972=FACE_OUTER_BOUND('',#14237,.T.);
#8973=FACE_OUTER_BOUND('',#14238,.T.);
#8974=FACE_OUTER_BOUND('',#14239,.T.);
#8975=FACE_OUTER_BOUND('',#14240,.T.);
#8976=FACE_OUTER_BOUND('',#14241,.T.);
#8977=FACE_OUTER_BOUND('',#14242,.T.);
#8978=FACE_OUTER_BOUND('',#14243,.T.);
#8979=FACE_OUTER_BOUND('',#14244,.T.);
#8980=FACE_OUTER_BOUND('',#14245,.T.);
#8981=FACE_OUTER_BOUND('',#14246,.T.);
#8982=FACE_OUTER_BOUND('',#14247,.T.);
#8983=FACE_OUTER_BOUND('',#14248,.T.);
#8984=FACE_OUTER_BOUND('',#14249,.T.);
#8985=FACE_OUTER_BOUND('',#14250,.T.);
#8986=FACE_OUTER_BOUND('',#14251,.T.);
#8987=FACE_OUTER_BOUND('',#14252,.T.);
#8988=FACE_OUTER_BOUND('',#14253,.T.);
#8989=FACE_OUTER_BOUND('',#14254,.T.);
#8990=FACE_OUTER_BOUND('',#14255,.T.);
#8991=FACE_OUTER_BOUND('',#14256,.T.);
#8992=FACE_OUTER_BOUND('',#14257,.T.);
#8993=FACE_OUTER_BOUND('',#14258,.T.);
#8994=FACE_OUTER_BOUND('',#14259,.T.);
#8995=FACE_OUTER_BOUND('',#14260,.T.);
#8996=FACE_OUTER_BOUND('',#14261,.T.);
#8997=FACE_OUTER_BOUND('',#14262,.T.);
#8998=FACE_OUTER_BOUND('',#14263,.T.);
#8999=FACE_OUTER_BOUND('',#14264,.T.);
#9000=FACE_OUTER_BOUND('',#14265,.T.);
#9001=FACE_OUTER_BOUND('',#14266,.T.);
#9002=FACE_OUTER_BOUND('',#14267,.T.);
#9003=FACE_OUTER_BOUND('',#14268,.T.);
#9004=FACE_OUTER_BOUND('',#14269,.T.);
#9005=FACE_OUTER_BOUND('',#14270,.T.);
#9006=FACE_OUTER_BOUND('',#14271,.T.);
#9007=FACE_OUTER_BOUND('',#14272,.T.);
#9008=FACE_OUTER_BOUND('',#14273,.T.);
#9009=FACE_OUTER_BOUND('',#14274,.T.);
#9010=FACE_OUTER_BOUND('',#14275,.T.);
#9011=FACE_OUTER_BOUND('',#14276,.T.);
#9012=FACE_OUTER_BOUND('',#14277,.T.);
#9013=FACE_OUTER_BOUND('',#14278,.T.);
#9014=FACE_OUTER_BOUND('',#14279,.T.);
#9015=FACE_OUTER_BOUND('',#14280,.T.);
#9016=FACE_OUTER_BOUND('',#14281,.T.);
#9017=FACE_OUTER_BOUND('',#14282,.T.);
#9018=FACE_OUTER_BOUND('',#14283,.T.);
#9019=FACE_OUTER_BOUND('',#14284,.T.);
#9020=FACE_OUTER_BOUND('',#14285,.T.);
#9021=FACE_OUTER_BOUND('',#14286,.T.);
#9022=FACE_OUTER_BOUND('',#14287,.T.);
#9023=FACE_OUTER_BOUND('',#14288,.T.);
#9024=FACE_OUTER_BOUND('',#14289,.T.);
#9025=FACE_OUTER_BOUND('',#14290,.T.);
#9026=FACE_OUTER_BOUND('',#14291,.T.);
#9027=FACE_OUTER_BOUND('',#14292,.T.);
#9028=FACE_OUTER_BOUND('',#14293,.T.);
#9029=FACE_OUTER_BOUND('',#14294,.T.);
#9030=FACE_OUTER_BOUND('',#14295,.T.);
#9031=FACE_OUTER_BOUND('',#14296,.T.);
#9032=FACE_OUTER_BOUND('',#14297,.T.);
#9033=FACE_OUTER_BOUND('',#14298,.T.);
#9034=FACE_OUTER_BOUND('',#14299,.T.);
#9035=FACE_OUTER_BOUND('',#14300,.T.);
#9036=FACE_OUTER_BOUND('',#14301,.T.);
#9037=FACE_OUTER_BOUND('',#14302,.T.);
#9038=FACE_OUTER_BOUND('',#14303,.T.);
#9039=FACE_OUTER_BOUND('',#14304,.T.);
#9040=FACE_OUTER_BOUND('',#14305,.T.);
#9041=FACE_OUTER_BOUND('',#14306,.T.);
#9042=FACE_OUTER_BOUND('',#14307,.T.);
#9043=FACE_OUTER_BOUND('',#14308,.T.);
#9044=FACE_OUTER_BOUND('',#14309,.T.);
#9045=FACE_OUTER_BOUND('',#14310,.T.);
#9046=FACE_OUTER_BOUND('',#14311,.T.);
#9047=FACE_OUTER_BOUND('',#14312,.T.);
#9048=FACE_OUTER_BOUND('',#14313,.T.);
#9049=FACE_OUTER_BOUND('',#14314,.T.);
#9050=FACE_OUTER_BOUND('',#14315,.T.);
#9051=FACE_OUTER_BOUND('',#14316,.T.);
#9052=FACE_OUTER_BOUND('',#14317,.T.);
#9053=FACE_OUTER_BOUND('',#14318,.T.);
#9054=FACE_OUTER_BOUND('',#14319,.T.);
#9055=FACE_OUTER_BOUND('',#14320,.T.);
#9056=FACE_OUTER_BOUND('',#14321,.T.);
#9057=FACE_OUTER_BOUND('',#14322,.T.);
#9058=FACE_OUTER_BOUND('',#14323,.T.);
#9059=FACE_OUTER_BOUND('',#14324,.T.);
#9060=FACE_OUTER_BOUND('',#14325,.T.);
#9061=FACE_OUTER_BOUND('',#14326,.T.);
#9062=FACE_OUTER_BOUND('',#14327,.T.);
#9063=FACE_OUTER_BOUND('',#14328,.T.);
#9064=FACE_OUTER_BOUND('',#14329,.T.);
#9065=FACE_OUTER_BOUND('',#14330,.T.);
#9066=FACE_OUTER_BOUND('',#14331,.T.);
#9067=FACE_OUTER_BOUND('',#14332,.T.);
#9068=FACE_OUTER_BOUND('',#14333,.T.);
#9069=FACE_OUTER_BOUND('',#14334,.T.);
#9070=FACE_OUTER_BOUND('',#14335,.T.);
#9071=FACE_OUTER_BOUND('',#14336,.T.);
#9072=FACE_OUTER_BOUND('',#14337,.T.);
#9073=FACE_OUTER_BOUND('',#14338,.T.);
#9074=FACE_OUTER_BOUND('',#14339,.T.);
#9075=FACE_OUTER_BOUND('',#14340,.T.);
#9076=FACE_OUTER_BOUND('',#14341,.T.);
#9077=FACE_OUTER_BOUND('',#14342,.T.);
#9078=FACE_OUTER_BOUND('',#14343,.T.);
#9079=FACE_OUTER_BOUND('',#14344,.T.);
#9080=FACE_OUTER_BOUND('',#14345,.T.);
#9081=FACE_OUTER_BOUND('',#14346,.T.);
#9082=FACE_OUTER_BOUND('',#14347,.T.);
#9083=FACE_OUTER_BOUND('',#14348,.T.);
#9084=FACE_OUTER_BOUND('',#14349,.T.);
#9085=FACE_OUTER_BOUND('',#14350,.T.);
#9086=FACE_OUTER_BOUND('',#14351,.T.);
#9087=FACE_OUTER_BOUND('',#14352,.T.);
#9088=FACE_OUTER_BOUND('',#14353,.T.);
#9089=FACE_OUTER_BOUND('',#14354,.T.);
#9090=FACE_OUTER_BOUND('',#14355,.T.);
#9091=FACE_OUTER_BOUND('',#14356,.T.);
#9092=FACE_OUTER_BOUND('',#14357,.T.);
#9093=FACE_OUTER_BOUND('',#14358,.T.);
#9094=FACE_OUTER_BOUND('',#14359,.T.);
#9095=FACE_OUTER_BOUND('',#14360,.T.);
#9096=FACE_OUTER_BOUND('',#14361,.T.);
#9097=FACE_OUTER_BOUND('',#14362,.T.);
#9098=FACE_OUTER_BOUND('',#14363,.T.);
#9099=FACE_OUTER_BOUND('',#14364,.T.);
#9100=FACE_OUTER_BOUND('',#14365,.T.);
#9101=FACE_OUTER_BOUND('',#14366,.T.);
#9102=FACE_OUTER_BOUND('',#14367,.T.);
#9103=FACE_OUTER_BOUND('',#14368,.T.);
#9104=FACE_OUTER_BOUND('',#14369,.T.);
#9105=FACE_OUTER_BOUND('',#14370,.T.);
#9106=FACE_OUTER_BOUND('',#14371,.T.);
#9107=FACE_OUTER_BOUND('',#14372,.T.);
#9108=FACE_OUTER_BOUND('',#14373,.T.);
#9109=FACE_OUTER_BOUND('',#14374,.T.);
#9110=FACE_OUTER_BOUND('',#14375,.T.);
#9111=FACE_OUTER_BOUND('',#14376,.T.);
#9112=FACE_OUTER_BOUND('',#14377,.T.);
#9113=FACE_OUTER_BOUND('',#14378,.T.);
#9114=FACE_OUTER_BOUND('',#14379,.T.);
#9115=FACE_OUTER_BOUND('',#14380,.T.);
#9116=FACE_OUTER_BOUND('',#14381,.T.);
#9117=FACE_OUTER_BOUND('',#14382,.T.);
#9118=FACE_OUTER_BOUND('',#14383,.T.);
#9119=FACE_OUTER_BOUND('',#14384,.T.);
#9120=FACE_OUTER_BOUND('',#14385,.T.);
#9121=FACE_OUTER_BOUND('',#14386,.T.);
#9122=FACE_OUTER_BOUND('',#14387,.T.);
#9123=FACE_OUTER_BOUND('',#14388,.T.);
#9124=FACE_OUTER_BOUND('',#14389,.T.);
#9125=FACE_OUTER_BOUND('',#14390,.T.);
#9126=FACE_OUTER_BOUND('',#14391,.T.);
#9127=FACE_OUTER_BOUND('',#14392,.T.);
#9128=FACE_OUTER_BOUND('',#14393,.T.);
#9129=FACE_OUTER_BOUND('',#14394,.T.);
#9130=FACE_OUTER_BOUND('',#14395,.T.);
#9131=FACE_OUTER_BOUND('',#14396,.T.);
#9132=FACE_OUTER_BOUND('',#14397,.T.);
#9133=FACE_OUTER_BOUND('',#14398,.T.);
#9134=FACE_OUTER_BOUND('',#14399,.T.);
#9135=FACE_OUTER_BOUND('',#14400,.T.);
#9136=FACE_OUTER_BOUND('',#14401,.T.);
#9137=FACE_OUTER_BOUND('',#14402,.T.);
#9138=FACE_OUTER_BOUND('',#14403,.T.);
#9139=FACE_OUTER_BOUND('',#14404,.T.);
#9140=FACE_OUTER_BOUND('',#14405,.T.);
#9141=FACE_OUTER_BOUND('',#14406,.T.);
#9142=FACE_OUTER_BOUND('',#14407,.T.);
#9143=FACE_OUTER_BOUND('',#14408,.T.);
#9144=FACE_OUTER_BOUND('',#14409,.T.);
#9145=FACE_OUTER_BOUND('',#14410,.T.);
#9146=FACE_OUTER_BOUND('',#14411,.T.);
#9147=FACE_OUTER_BOUND('',#14412,.T.);
#9148=FACE_OUTER_BOUND('',#14413,.T.);
#9149=FACE_OUTER_BOUND('',#14414,.T.);
#9150=FACE_OUTER_BOUND('',#14415,.T.);
#9151=FACE_OUTER_BOUND('',#14416,.T.);
#9152=FACE_OUTER_BOUND('',#14417,.T.);
#9153=FACE_OUTER_BOUND('',#14418,.T.);
#9154=FACE_OUTER_BOUND('',#14419,.T.);
#9155=FACE_OUTER_BOUND('',#14420,.T.);
#9156=FACE_OUTER_BOUND('',#14421,.T.);
#9157=FACE_OUTER_BOUND('',#14422,.T.);
#9158=FACE_OUTER_BOUND('',#14423,.T.);
#9159=FACE_OUTER_BOUND('',#14424,.T.);
#9160=FACE_OUTER_BOUND('',#14425,.T.);
#9161=FACE_OUTER_BOUND('',#14426,.T.);
#9162=FACE_OUTER_BOUND('',#14427,.T.);
#9163=FACE_OUTER_BOUND('',#14428,.T.);
#9164=FACE_OUTER_BOUND('',#14429,.T.);
#9165=FACE_OUTER_BOUND('',#14430,.T.);
#9166=FACE_OUTER_BOUND('',#14431,.T.);
#9167=FACE_OUTER_BOUND('',#14432,.T.);
#9168=FACE_OUTER_BOUND('',#14433,.T.);
#9169=FACE_OUTER_BOUND('',#14434,.T.);
#9170=FACE_OUTER_BOUND('',#14435,.T.);
#9171=FACE_OUTER_BOUND('',#14436,.T.);
#9172=FACE_OUTER_BOUND('',#14437,.T.);
#9173=FACE_OUTER_BOUND('',#14438,.T.);
#9174=FACE_OUTER_BOUND('',#14439,.T.);
#9175=FACE_OUTER_BOUND('',#14440,.T.);
#9176=FACE_OUTER_BOUND('',#14441,.T.);
#9177=FACE_OUTER_BOUND('',#14442,.T.);
#9178=FACE_OUTER_BOUND('',#14443,.T.);
#9179=FACE_OUTER_BOUND('',#14444,.T.);
#9180=FACE_OUTER_BOUND('',#14445,.T.);
#9181=FACE_OUTER_BOUND('',#14446,.T.);
#9182=FACE_OUTER_BOUND('',#14447,.T.);
#9183=FACE_OUTER_BOUND('',#14448,.T.);
#9184=FACE_OUTER_BOUND('',#14449,.T.);
#9185=FACE_OUTER_BOUND('',#14450,.T.);
#9186=FACE_OUTER_BOUND('',#14451,.T.);
#9187=FACE_OUTER_BOUND('',#14452,.T.);
#9188=FACE_OUTER_BOUND('',#14453,.T.);
#9189=FACE_OUTER_BOUND('',#14454,.T.);
#9190=FACE_OUTER_BOUND('',#14455,.T.);
#9191=FACE_OUTER_BOUND('',#14456,.T.);
#9192=FACE_OUTER_BOUND('',#14457,.T.);
#9193=FACE_OUTER_BOUND('',#14458,.T.);
#9194=FACE_OUTER_BOUND('',#14459,.T.);
#9195=FACE_OUTER_BOUND('',#14460,.T.);
#9196=FACE_OUTER_BOUND('',#14461,.T.);
#9197=FACE_OUTER_BOUND('',#14462,.T.);
#9198=FACE_OUTER_BOUND('',#14463,.T.);
#9199=FACE_OUTER_BOUND('',#14464,.T.);
#9200=FACE_OUTER_BOUND('',#14465,.T.);
#9201=FACE_OUTER_BOUND('',#14466,.T.);
#9202=FACE_OUTER_BOUND('',#14467,.T.);
#9203=FACE_OUTER_BOUND('',#14468,.T.);
#9204=FACE_OUTER_BOUND('',#14469,.T.);
#9205=FACE_OUTER_BOUND('',#14470,.T.);
#9206=FACE_OUTER_BOUND('',#14471,.T.);
#9207=FACE_OUTER_BOUND('',#14472,.T.);
#9208=FACE_OUTER_BOUND('',#14473,.T.);
#9209=FACE_OUTER_BOUND('',#14474,.T.);
#9210=FACE_OUTER_BOUND('',#14475,.T.);
#9211=FACE_OUTER_BOUND('',#14476,.T.);
#9212=FACE_OUTER_BOUND('',#14477,.T.);
#9213=FACE_OUTER_BOUND('',#14478,.T.);
#9214=FACE_OUTER_BOUND('',#14479,.T.);
#9215=FACE_OUTER_BOUND('',#14480,.T.);
#9216=FACE_OUTER_BOUND('',#14481,.T.);
#9217=FACE_OUTER_BOUND('',#14482,.T.);
#9218=FACE_OUTER_BOUND('',#14483,.T.);
#9219=FACE_OUTER_BOUND('',#14484,.T.);
#9220=FACE_OUTER_BOUND('',#14485,.T.);
#9221=FACE_OUTER_BOUND('',#14486,.T.);
#9222=FACE_OUTER_BOUND('',#14487,.T.);
#9223=FACE_OUTER_BOUND('',#14488,.T.);
#9224=FACE_OUTER_BOUND('',#14489,.T.);
#9225=FACE_OUTER_BOUND('',#14490,.T.);
#9226=FACE_OUTER_BOUND('',#14491,.T.);
#9227=FACE_OUTER_BOUND('',#14492,.T.);
#9228=FACE_OUTER_BOUND('',#14493,.T.);
#9229=FACE_OUTER_BOUND('',#14494,.T.);
#9230=FACE_OUTER_BOUND('',#14495,.T.);
#9231=FACE_OUTER_BOUND('',#14496,.T.);
#9232=FACE_OUTER_BOUND('',#14497,.T.);
#9233=FACE_OUTER_BOUND('',#14498,.T.);
#9234=FACE_OUTER_BOUND('',#14499,.T.);
#9235=FACE_OUTER_BOUND('',#14500,.T.);
#9236=FACE_OUTER_BOUND('',#14501,.T.);
#9237=FACE_OUTER_BOUND('',#14502,.T.);
#9238=FACE_OUTER_BOUND('',#14503,.T.);
#9239=FACE_OUTER_BOUND('',#14504,.T.);
#9240=FACE_OUTER_BOUND('',#14505,.T.);
#9241=FACE_OUTER_BOUND('',#14506,.T.);
#9242=FACE_OUTER_BOUND('',#14507,.T.);
#9243=FACE_OUTER_BOUND('',#14508,.T.);
#9244=FACE_OUTER_BOUND('',#14509,.T.);
#9245=FACE_OUTER_BOUND('',#14510,.T.);
#9246=FACE_OUTER_BOUND('',#14511,.T.);
#9247=FACE_OUTER_BOUND('',#14512,.T.);
#9248=FACE_OUTER_BOUND('',#14513,.T.);
#9249=FACE_OUTER_BOUND('',#14514,.T.);
#9250=FACE_OUTER_BOUND('',#14515,.T.);
#9251=FACE_OUTER_BOUND('',#14516,.T.);
#9252=FACE_OUTER_BOUND('',#14517,.T.);
#9253=FACE_OUTER_BOUND('',#14518,.T.);
#9254=FACE_OUTER_BOUND('',#14519,.T.);
#9255=FACE_OUTER_BOUND('',#14520,.T.);
#9256=FACE_OUTER_BOUND('',#14521,.T.);
#9257=FACE_OUTER_BOUND('',#14522,.T.);
#9258=FACE_OUTER_BOUND('',#14523,.T.);
#9259=FACE_OUTER_BOUND('',#14524,.T.);
#9260=FACE_OUTER_BOUND('',#14525,.T.);
#9261=FACE_OUTER_BOUND('',#14526,.T.);
#9262=FACE_OUTER_BOUND('',#14527,.T.);
#9263=FACE_OUTER_BOUND('',#14528,.T.);
#9264=FACE_OUTER_BOUND('',#14529,.T.);
#9265=FACE_OUTER_BOUND('',#14530,.T.);
#9266=FACE_OUTER_BOUND('',#14531,.T.);
#9267=FACE_OUTER_BOUND('',#14532,.T.);
#9268=FACE_OUTER_BOUND('',#14533,.T.);
#9269=FACE_OUTER_BOUND('',#14534,.T.);
#9270=FACE_OUTER_BOUND('',#14535,.T.);
#9271=FACE_OUTER_BOUND('',#14536,.T.);
#9272=FACE_OUTER_BOUND('',#14537,.T.);
#9273=FACE_OUTER_BOUND('',#14538,.T.);
#9274=FACE_OUTER_BOUND('',#14539,.T.);
#9275=FACE_OUTER_BOUND('',#14540,.T.);
#9276=FACE_OUTER_BOUND('',#14541,.T.);
#9277=FACE_OUTER_BOUND('',#14542,.T.);
#9278=FACE_OUTER_BOUND('',#14543,.T.);
#9279=FACE_OUTER_BOUND('',#14544,.T.);
#9280=FACE_OUTER_BOUND('',#14545,.T.);
#9281=FACE_OUTER_BOUND('',#14546,.T.);
#9282=FACE_OUTER_BOUND('',#14547,.T.);
#9283=FACE_OUTER_BOUND('',#14548,.T.);
#9284=FACE_OUTER_BOUND('',#14549,.T.);
#9285=FACE_OUTER_BOUND('',#14550,.T.);
#9286=FACE_OUTER_BOUND('',#14551,.T.);
#9287=FACE_OUTER_BOUND('',#14552,.T.);
#9288=FACE_OUTER_BOUND('',#14553,.T.);
#9289=FACE_OUTER_BOUND('',#14554,.T.);
#9290=FACE_OUTER_BOUND('',#14555,.T.);
#9291=FACE_OUTER_BOUND('',#14556,.T.);
#9292=FACE_OUTER_BOUND('',#14557,.T.);
#9293=FACE_OUTER_BOUND('',#14558,.T.);
#9294=FACE_OUTER_BOUND('',#14559,.T.);
#9295=FACE_OUTER_BOUND('',#14560,.T.);
#9296=FACE_OUTER_BOUND('',#14561,.T.);
#9297=FACE_OUTER_BOUND('',#14562,.T.);
#9298=FACE_OUTER_BOUND('',#14563,.T.);
#9299=FACE_OUTER_BOUND('',#14564,.T.);
#9300=FACE_OUTER_BOUND('',#14565,.T.);
#9301=FACE_OUTER_BOUND('',#14566,.T.);
#9302=FACE_OUTER_BOUND('',#14567,.T.);
#9303=FACE_OUTER_BOUND('',#14568,.T.);
#9304=FACE_OUTER_BOUND('',#14569,.T.);
#9305=FACE_OUTER_BOUND('',#14570,.T.);
#9306=FACE_OUTER_BOUND('',#14571,.T.);
#9307=FACE_OUTER_BOUND('',#14572,.T.);
#9308=FACE_OUTER_BOUND('',#14573,.T.);
#9309=FACE_OUTER_BOUND('',#14574,.T.);
#9310=FACE_OUTER_BOUND('',#14575,.T.);
#9311=FACE_OUTER_BOUND('',#14576,.T.);
#9312=FACE_OUTER_BOUND('',#14577,.T.);
#9313=FACE_OUTER_BOUND('',#14578,.T.);
#9314=FACE_OUTER_BOUND('',#14579,.T.);
#9315=FACE_OUTER_BOUND('',#14580,.T.);
#9316=FACE_OUTER_BOUND('',#14581,.T.);
#9317=FACE_OUTER_BOUND('',#14582,.T.);
#9318=FACE_OUTER_BOUND('',#14583,.T.);
#9319=FACE_OUTER_BOUND('',#14584,.T.);
#9320=FACE_OUTER_BOUND('',#14585,.T.);
#9321=FACE_OUTER_BOUND('',#14586,.T.);
#9322=FACE_OUTER_BOUND('',#14587,.T.);
#9323=FACE_OUTER_BOUND('',#14588,.T.);
#9324=FACE_OUTER_BOUND('',#14589,.T.);
#9325=FACE_OUTER_BOUND('',#14590,.T.);
#9326=FACE_OUTER_BOUND('',#14591,.T.);
#9327=FACE_OUTER_BOUND('',#14592,.T.);
#9328=FACE_OUTER_BOUND('',#14593,.T.);
#9329=FACE_OUTER_BOUND('',#14594,.T.);
#9330=FACE_OUTER_BOUND('',#14595,.T.);
#9331=FACE_OUTER_BOUND('',#14596,.T.);
#9332=FACE_OUTER_BOUND('',#14597,.T.);
#9333=FACE_OUTER_BOUND('',#14598,.T.);
#9334=FACE_OUTER_BOUND('',#14599,.T.);
#9335=FACE_OUTER_BOUND('',#14600,.T.);
#9336=FACE_OUTER_BOUND('',#14601,.T.);
#9337=FACE_OUTER_BOUND('',#14602,.T.);
#9338=FACE_OUTER_BOUND('',#14603,.T.);
#9339=FACE_OUTER_BOUND('',#14604,.T.);
#9340=FACE_OUTER_BOUND('',#14605,.T.);
#9341=FACE_OUTER_BOUND('',#14606,.T.);
#9342=FACE_OUTER_BOUND('',#14607,.T.);
#9343=FACE_OUTER_BOUND('',#14608,.T.);
#9344=FACE_OUTER_BOUND('',#14609,.T.);
#9345=FACE_OUTER_BOUND('',#14610,.T.);
#9346=FACE_OUTER_BOUND('',#14611,.T.);
#9347=FACE_OUTER_BOUND('',#14612,.T.);
#9348=FACE_OUTER_BOUND('',#14613,.T.);
#9349=FACE_OUTER_BOUND('',#14614,.T.);
#9350=FACE_OUTER_BOUND('',#14615,.T.);
#9351=FACE_OUTER_BOUND('',#14616,.T.);
#9352=FACE_OUTER_BOUND('',#14617,.T.);
#9353=FACE_OUTER_BOUND('',#14618,.T.);
#9354=FACE_OUTER_BOUND('',#14619,.T.);
#9355=FACE_OUTER_BOUND('',#14620,.T.);
#9356=FACE_OUTER_BOUND('',#14621,.T.);
#9357=FACE_OUTER_BOUND('',#14622,.T.);
#9358=FACE_OUTER_BOUND('',#14623,.T.);
#9359=FACE_OUTER_BOUND('',#14624,.T.);
#9360=FACE_OUTER_BOUND('',#14625,.T.);
#9361=FACE_OUTER_BOUND('',#14626,.T.);
#9362=FACE_OUTER_BOUND('',#14627,.T.);
#9363=FACE_OUTER_BOUND('',#14628,.T.);
#9364=FACE_OUTER_BOUND('',#14629,.T.);
#9365=FACE_OUTER_BOUND('',#14630,.T.);
#9366=FACE_OUTER_BOUND('',#14631,.T.);
#9367=FACE_OUTER_BOUND('',#14632,.T.);
#9368=FACE_OUTER_BOUND('',#14633,.T.);
#9369=FACE_OUTER_BOUND('',#14634,.T.);
#9370=FACE_OUTER_BOUND('',#14635,.T.);
#9371=FACE_OUTER_BOUND('',#14636,.T.);
#9372=FACE_OUTER_BOUND('',#14637,.T.);
#9373=FACE_OUTER_BOUND('',#14638,.T.);
#9374=FACE_OUTER_BOUND('',#14639,.T.);
#9375=FACE_OUTER_BOUND('',#14640,.T.);
#9376=FACE_OUTER_BOUND('',#14641,.T.);
#9377=FACE_OUTER_BOUND('',#14642,.T.);
#9378=FACE_OUTER_BOUND('',#14643,.T.);
#9379=FACE_OUTER_BOUND('',#14644,.T.);
#9380=FACE_OUTER_BOUND('',#14645,.T.);
#9381=FACE_OUTER_BOUND('',#14646,.T.);
#9382=FACE_OUTER_BOUND('',#14647,.T.);
#9383=FACE_OUTER_BOUND('',#14648,.T.);
#9384=FACE_OUTER_BOUND('',#14649,.T.);
#9385=FACE_OUTER_BOUND('',#14650,.T.);
#9386=FACE_OUTER_BOUND('',#14651,.T.);
#9387=FACE_OUTER_BOUND('',#14652,.T.);
#9388=FACE_OUTER_BOUND('',#14653,.T.);
#9389=FACE_OUTER_BOUND('',#14654,.T.);
#9390=FACE_OUTER_BOUND('',#14655,.T.);
#9391=FACE_OUTER_BOUND('',#14656,.T.);
#9392=FACE_OUTER_BOUND('',#14657,.T.);
#9393=FACE_OUTER_BOUND('',#14658,.T.);
#9394=FACE_OUTER_BOUND('',#14659,.T.);
#9395=FACE_OUTER_BOUND('',#14660,.T.);
#9396=FACE_OUTER_BOUND('',#14661,.T.);
#9397=FACE_OUTER_BOUND('',#14662,.T.);
#9398=FACE_OUTER_BOUND('',#14663,.T.);
#9399=FACE_OUTER_BOUND('',#14664,.T.);
#9400=FACE_OUTER_BOUND('',#14665,.T.);
#9401=FACE_OUTER_BOUND('',#14666,.T.);
#9402=FACE_OUTER_BOUND('',#14667,.T.);
#9403=FACE_OUTER_BOUND('',#14668,.T.);
#9404=FACE_OUTER_BOUND('',#14669,.T.);
#9405=FACE_OUTER_BOUND('',#14670,.T.);
#9406=FACE_OUTER_BOUND('',#14671,.T.);
#9407=FACE_OUTER_BOUND('',#14672,.T.);
#9408=FACE_OUTER_BOUND('',#14673,.T.);
#9409=FACE_OUTER_BOUND('',#14674,.T.);
#9410=FACE_OUTER_BOUND('',#14675,.T.);
#9411=FACE_OUTER_BOUND('',#14676,.T.);
#9412=FACE_OUTER_BOUND('',#14677,.T.);
#9413=FACE_OUTER_BOUND('',#14678,.T.);
#9414=FACE_OUTER_BOUND('',#14679,.T.);
#9415=FACE_OUTER_BOUND('',#14680,.T.);
#9416=FACE_OUTER_BOUND('',#14681,.T.);
#9417=FACE_OUTER_BOUND('',#14682,.T.);
#9418=FACE_OUTER_BOUND('',#14683,.T.);
#9419=FACE_OUTER_BOUND('',#14684,.T.);
#9420=FACE_OUTER_BOUND('',#14685,.T.);
#9421=FACE_OUTER_BOUND('',#14686,.T.);
#9422=FACE_OUTER_BOUND('',#14687,.T.);
#9423=FACE_OUTER_BOUND('',#14688,.T.);
#9424=FACE_OUTER_BOUND('',#14689,.T.);
#9425=FACE_OUTER_BOUND('',#14690,.T.);
#9426=FACE_OUTER_BOUND('',#14691,.T.);
#9427=FACE_OUTER_BOUND('',#14692,.T.);
#9428=FACE_OUTER_BOUND('',#14693,.T.);
#9429=FACE_OUTER_BOUND('',#14694,.T.);
#9430=FACE_OUTER_BOUND('',#14695,.T.);
#9431=FACE_OUTER_BOUND('',#14696,.T.);
#9432=FACE_OUTER_BOUND('',#14697,.T.);
#9433=FACE_OUTER_BOUND('',#14698,.T.);
#9434=FACE_OUTER_BOUND('',#14699,.T.);
#9435=FACE_OUTER_BOUND('',#14700,.T.);
#9436=FACE_OUTER_BOUND('',#14701,.T.);
#9437=FACE_OUTER_BOUND('',#14702,.T.);
#9438=FACE_OUTER_BOUND('',#14703,.T.);
#9439=FACE_OUTER_BOUND('',#14704,.T.);
#9440=FACE_OUTER_BOUND('',#14705,.T.);
#9441=FACE_OUTER_BOUND('',#14706,.T.);
#9442=FACE_OUTER_BOUND('',#14707,.T.);
#9443=FACE_OUTER_BOUND('',#14708,.T.);
#9444=FACE_OUTER_BOUND('',#14709,.T.);
#9445=FACE_OUTER_BOUND('',#14710,.T.);
#9446=FACE_OUTER_BOUND('',#14711,.T.);
#9447=FACE_OUTER_BOUND('',#14712,.T.);
#9448=FACE_OUTER_BOUND('',#14713,.T.);
#9449=FACE_OUTER_BOUND('',#14714,.T.);
#9450=FACE_OUTER_BOUND('',#14715,.T.);
#9451=FACE_OUTER_BOUND('',#14716,.T.);
#9452=FACE_OUTER_BOUND('',#14717,.T.);
#9453=FACE_OUTER_BOUND('',#14718,.T.);
#9454=FACE_OUTER_BOUND('',#14719,.T.);
#9455=FACE_OUTER_BOUND('',#14720,.T.);
#9456=FACE_OUTER_BOUND('',#14721,.T.);
#9457=FACE_OUTER_BOUND('',#14722,.T.);
#9458=FACE_OUTER_BOUND('',#14723,.T.);
#9459=FACE_OUTER_BOUND('',#14724,.T.);
#9460=FACE_OUTER_BOUND('',#14725,.T.);
#9461=FACE_OUTER_BOUND('',#14726,.T.);
#9462=FACE_OUTER_BOUND('',#14727,.T.);
#9463=FACE_OUTER_BOUND('',#14728,.T.);
#9464=FACE_OUTER_BOUND('',#14729,.T.);
#9465=FACE_OUTER_BOUND('',#14730,.T.);
#9466=FACE_OUTER_BOUND('',#14731,.T.);
#9467=FACE_OUTER_BOUND('',#14732,.T.);
#9468=FACE_OUTER_BOUND('',#14733,.T.);
#9469=FACE_OUTER_BOUND('',#14734,.T.);
#9470=FACE_OUTER_BOUND('',#14735,.T.);
#9471=FACE_OUTER_BOUND('',#14736,.T.);
#9472=FACE_OUTER_BOUND('',#14737,.T.);
#9473=FACE_OUTER_BOUND('',#14738,.T.);
#9474=FACE_OUTER_BOUND('',#14739,.T.);
#9475=FACE_OUTER_BOUND('',#14740,.T.);
#9476=FACE_OUTER_BOUND('',#14741,.T.);
#9477=FACE_OUTER_BOUND('',#14742,.T.);
#9478=FACE_OUTER_BOUND('',#14743,.T.);
#9479=FACE_OUTER_BOUND('',#14744,.T.);
#9480=FACE_OUTER_BOUND('',#14745,.T.);
#9481=FACE_OUTER_BOUND('',#14746,.T.);
#9482=FACE_OUTER_BOUND('',#14747,.T.);
#9483=FACE_OUTER_BOUND('',#14748,.T.);
#9484=FACE_OUTER_BOUND('',#14749,.T.);
#9485=FACE_OUTER_BOUND('',#14750,.T.);
#9486=FACE_OUTER_BOUND('',#14751,.T.);
#9487=FACE_OUTER_BOUND('',#14752,.T.);
#9488=FACE_OUTER_BOUND('',#14753,.T.);
#9489=FACE_OUTER_BOUND('',#14754,.T.);
#9490=FACE_OUTER_BOUND('',#14755,.T.);
#9491=FACE_OUTER_BOUND('',#14756,.T.);
#9492=FACE_OUTER_BOUND('',#14757,.T.);
#9493=FACE_OUTER_BOUND('',#14758,.T.);
#9494=FACE_OUTER_BOUND('',#14759,.T.);
#9495=FACE_OUTER_BOUND('',#14760,.T.);
#9496=FACE_OUTER_BOUND('',#14761,.T.);
#9497=FACE_OUTER_BOUND('',#14762,.T.);
#9498=FACE_OUTER_BOUND('',#14763,.T.);
#9499=FACE_OUTER_BOUND('',#14764,.T.);
#9500=FACE_OUTER_BOUND('',#14765,.T.);
#9501=FACE_OUTER_BOUND('',#14766,.T.);
#9502=FACE_OUTER_BOUND('',#14767,.T.);
#9503=FACE_OUTER_BOUND('',#14768,.T.);
#9504=FACE_OUTER_BOUND('',#14769,.T.);
#9505=FACE_OUTER_BOUND('',#14770,.T.);
#9506=FACE_OUTER_BOUND('',#14771,.T.);
#9507=FACE_OUTER_BOUND('',#14772,.T.);
#9508=FACE_OUTER_BOUND('',#14773,.T.);
#9509=FACE_OUTER_BOUND('',#14774,.T.);
#9510=FACE_OUTER_BOUND('',#14775,.T.);
#9511=FACE_OUTER_BOUND('',#14776,.T.);
#9512=FACE_OUTER_BOUND('',#14777,.T.);
#9513=FACE_OUTER_BOUND('',#14778,.T.);
#9514=FACE_OUTER_BOUND('',#14779,.T.);
#9515=FACE_OUTER_BOUND('',#14780,.T.);
#9516=FACE_OUTER_BOUND('',#14781,.T.);
#9517=FACE_OUTER_BOUND('',#14782,.T.);
#9518=FACE_OUTER_BOUND('',#14783,.T.);
#9519=FACE_OUTER_BOUND('',#14784,.T.);
#9520=FACE_OUTER_BOUND('',#14785,.T.);
#9521=FACE_OUTER_BOUND('',#14786,.T.);
#9522=FACE_OUTER_BOUND('',#14787,.T.);
#9523=FACE_OUTER_BOUND('',#14788,.T.);
#9524=FACE_OUTER_BOUND('',#14789,.T.);
#9525=FACE_OUTER_BOUND('',#14790,.T.);
#9526=FACE_OUTER_BOUND('',#14791,.T.);
#9527=FACE_OUTER_BOUND('',#14792,.T.);
#9528=FACE_OUTER_BOUND('',#14793,.T.);
#9529=FACE_OUTER_BOUND('',#14794,.T.);
#9530=FACE_OUTER_BOUND('',#14795,.T.);
#9531=FACE_OUTER_BOUND('',#14796,.T.);
#9532=FACE_OUTER_BOUND('',#14797,.T.);
#9533=FACE_OUTER_BOUND('',#14798,.T.);
#9534=FACE_OUTER_BOUND('',#14799,.T.);
#9535=FACE_OUTER_BOUND('',#14800,.T.);
#9536=FACE_OUTER_BOUND('',#14801,.T.);
#9537=FACE_OUTER_BOUND('',#14802,.T.);
#9538=FACE_OUTER_BOUND('',#14803,.T.);
#9539=FACE_OUTER_BOUND('',#14804,.T.);
#9540=FACE_OUTER_BOUND('',#14805,.T.);
#9541=FACE_OUTER_BOUND('',#14806,.T.);
#9542=FACE_OUTER_BOUND('',#14807,.T.);
#9543=FACE_OUTER_BOUND('',#14808,.T.);
#9544=FACE_OUTER_BOUND('',#14809,.T.);
#9545=FACE_OUTER_BOUND('',#14810,.T.);
#9546=FACE_OUTER_BOUND('',#14811,.T.);
#9547=FACE_OUTER_BOUND('',#14812,.T.);
#9548=FACE_OUTER_BOUND('',#14813,.T.);
#9549=FACE_OUTER_BOUND('',#14814,.T.);
#9550=FACE_OUTER_BOUND('',#14815,.T.);
#9551=FACE_OUTER_BOUND('',#14816,.T.);
#9552=FACE_OUTER_BOUND('',#14817,.T.);
#9553=FACE_OUTER_BOUND('',#14818,.T.);
#9554=FACE_OUTER_BOUND('',#14819,.T.);
#9555=FACE_OUTER_BOUND('',#14820,.T.);
#9556=FACE_OUTER_BOUND('',#14821,.T.);
#9557=FACE_OUTER_BOUND('',#14822,.T.);
#9558=FACE_OUTER_BOUND('',#14823,.T.);
#9559=FACE_OUTER_BOUND('',#14824,.T.);
#9560=FACE_OUTER_BOUND('',#14825,.T.);
#9561=FACE_OUTER_BOUND('',#14826,.T.);
#9562=FACE_OUTER_BOUND('',#14827,.T.);
#9563=FACE_OUTER_BOUND('',#14828,.T.);
#9564=FACE_OUTER_BOUND('',#14829,.T.);
#9565=FACE_OUTER_BOUND('',#14830,.T.);
#9566=FACE_OUTER_BOUND('',#14831,.T.);
#9567=FACE_OUTER_BOUND('',#14832,.T.);
#9568=FACE_OUTER_BOUND('',#14833,.T.);
#9569=FACE_OUTER_BOUND('',#14834,.T.);
#9570=FACE_OUTER_BOUND('',#14835,.T.);
#9571=FACE_OUTER_BOUND('',#14836,.T.);
#9572=FACE_OUTER_BOUND('',#14837,.T.);
#9573=FACE_OUTER_BOUND('',#14838,.T.);
#9574=FACE_OUTER_BOUND('',#14839,.T.);
#9575=FACE_OUTER_BOUND('',#14840,.T.);
#9576=FACE_OUTER_BOUND('',#14841,.T.);
#9577=FACE_OUTER_BOUND('',#14842,.T.);
#9578=FACE_OUTER_BOUND('',#14843,.T.);
#9579=FACE_OUTER_BOUND('',#14844,.T.);
#9580=FACE_OUTER_BOUND('',#14845,.T.);
#9581=FACE_OUTER_BOUND('',#14846,.T.);
#9582=FACE_OUTER_BOUND('',#14847,.T.);
#9583=FACE_OUTER_BOUND('',#14848,.T.);
#9584=FACE_OUTER_BOUND('',#14849,.T.);
#9585=FACE_OUTER_BOUND('',#14850,.T.);
#9586=FACE_OUTER_BOUND('',#14851,.T.);
#9587=FACE_OUTER_BOUND('',#14852,.T.);
#9588=FACE_OUTER_BOUND('',#14853,.T.);
#9589=FACE_OUTER_BOUND('',#14854,.T.);
#9590=FACE_OUTER_BOUND('',#14855,.T.);
#9591=FACE_OUTER_BOUND('',#14856,.T.);
#9592=FACE_OUTER_BOUND('',#14857,.T.);
#9593=FACE_OUTER_BOUND('',#14858,.T.);
#9594=FACE_OUTER_BOUND('',#14859,.T.);
#9595=FACE_OUTER_BOUND('',#14860,.T.);
#9596=FACE_OUTER_BOUND('',#14861,.T.);
#9597=FACE_OUTER_BOUND('',#14862,.T.);
#9598=FACE_OUTER_BOUND('',#14863,.T.);
#9599=FACE_OUTER_BOUND('',#14864,.T.);
#9600=FACE_OUTER_BOUND('',#14865,.T.);
#9601=FACE_OUTER_BOUND('',#14866,.T.);
#9602=FACE_OUTER_BOUND('',#14867,.T.);
#9603=FACE_OUTER_BOUND('',#14868,.T.);
#9604=FACE_OUTER_BOUND('',#14869,.T.);
#9605=FACE_OUTER_BOUND('',#14870,.T.);
#9606=FACE_OUTER_BOUND('',#14871,.T.);
#9607=FACE_OUTER_BOUND('',#14872,.T.);
#9608=FACE_OUTER_BOUND('',#14873,.T.);
#9609=FACE_OUTER_BOUND('',#14874,.T.);
#9610=FACE_OUTER_BOUND('',#14875,.T.);
#9611=FACE_OUTER_BOUND('',#14876,.T.);
#9612=FACE_OUTER_BOUND('',#14877,.T.);
#9613=FACE_OUTER_BOUND('',#14878,.T.);
#9614=FACE_OUTER_BOUND('',#14879,.T.);
#9615=FACE_OUTER_BOUND('',#14880,.T.);
#9616=FACE_OUTER_BOUND('',#14881,.T.);
#9617=FACE_OUTER_BOUND('',#14882,.T.);
#9618=FACE_OUTER_BOUND('',#14883,.T.);
#9619=FACE_OUTER_BOUND('',#14884,.T.);
#9620=FACE_OUTER_BOUND('',#14885,.T.);
#9621=FACE_OUTER_BOUND('',#14886,.T.);
#9622=FACE_OUTER_BOUND('',#14887,.T.);
#9623=FACE_OUTER_BOUND('',#14888,.T.);
#9624=FACE_OUTER_BOUND('',#14889,.T.);
#9625=FACE_OUTER_BOUND('',#14890,.T.);
#9626=FACE_OUTER_BOUND('',#14891,.T.);
#9627=FACE_OUTER_BOUND('',#14892,.T.);
#9628=FACE_OUTER_BOUND('',#14893,.T.);
#9629=FACE_OUTER_BOUND('',#14894,.T.);
#9630=FACE_OUTER_BOUND('',#14895,.T.);
#9631=FACE_OUTER_BOUND('',#14896,.T.);
#9632=FACE_OUTER_BOUND('',#14897,.T.);
#9633=FACE_OUTER_BOUND('',#14898,.T.);
#9634=FACE_OUTER_BOUND('',#14899,.T.);
#9635=FACE_OUTER_BOUND('',#14900,.T.);
#9636=FACE_OUTER_BOUND('',#14901,.T.);
#9637=FACE_OUTER_BOUND('',#14902,.T.);
#9638=FACE_OUTER_BOUND('',#14903,.T.);
#9639=FACE_OUTER_BOUND('',#14904,.T.);
#9640=FACE_OUTER_BOUND('',#14905,.T.);
#9641=FACE_OUTER_BOUND('',#14906,.T.);
#9642=FACE_OUTER_BOUND('',#14907,.T.);
#9643=FACE_OUTER_BOUND('',#14908,.T.);
#9644=FACE_OUTER_BOUND('',#14909,.T.);
#9645=FACE_OUTER_BOUND('',#14910,.T.);
#9646=FACE_OUTER_BOUND('',#14911,.T.);
#9647=FACE_OUTER_BOUND('',#14912,.T.);
#9648=FACE_OUTER_BOUND('',#14913,.T.);
#9649=FACE_OUTER_BOUND('',#14914,.T.);
#9650=FACE_OUTER_BOUND('',#14915,.T.);
#9651=FACE_OUTER_BOUND('',#14916,.T.);
#9652=FACE_OUTER_BOUND('',#14917,.T.);
#9653=FACE_OUTER_BOUND('',#14918,.T.);
#9654=FACE_OUTER_BOUND('',#14919,.T.);
#9655=FACE_OUTER_BOUND('',#14920,.T.);
#9656=FACE_OUTER_BOUND('',#14921,.T.);
#9657=FACE_OUTER_BOUND('',#14922,.T.);
#9658=FACE_OUTER_BOUND('',#14923,.T.);
#9659=FACE_OUTER_BOUND('',#14924,.T.);
#9660=FACE_OUTER_BOUND('',#14925,.T.);
#9661=FACE_OUTER_BOUND('',#14926,.T.);
#9662=FACE_OUTER_BOUND('',#14927,.T.);
#9663=FACE_OUTER_BOUND('',#14928,.T.);
#9664=FACE_OUTER_BOUND('',#14929,.T.);
#9665=FACE_OUTER_BOUND('',#14930,.T.);
#9666=FACE_OUTER_BOUND('',#14931,.T.);
#9667=FACE_OUTER_BOUND('',#14932,.T.);
#9668=FACE_OUTER_BOUND('',#14933,.T.);
#9669=FACE_OUTER_BOUND('',#14934,.T.);
#9670=FACE_OUTER_BOUND('',#14935,.T.);
#9671=FACE_OUTER_BOUND('',#14936,.T.);
#9672=FACE_OUTER_BOUND('',#14937,.T.);
#9673=FACE_OUTER_BOUND('',#14938,.T.);
#9674=FACE_OUTER_BOUND('',#14939,.T.);
#9675=FACE_OUTER_BOUND('',#14940,.T.);
#9676=FACE_OUTER_BOUND('',#14941,.T.);
#9677=FACE_OUTER_BOUND('',#14942,.T.);
#9678=FACE_OUTER_BOUND('',#14943,.T.);
#9679=FACE_OUTER_BOUND('',#14944,.T.);
#9680=FACE_OUTER_BOUND('',#14945,.T.);
#9681=FACE_OUTER_BOUND('',#14946,.T.);
#9682=FACE_OUTER_BOUND('',#14947,.T.);
#9683=FACE_OUTER_BOUND('',#14948,.T.);
#9684=FACE_OUTER_BOUND('',#14949,.T.);
#9685=FACE_OUTER_BOUND('',#14950,.T.);
#9686=FACE_OUTER_BOUND('',#14951,.T.);
#9687=FACE_OUTER_BOUND('',#14952,.T.);
#9688=FACE_OUTER_BOUND('',#14953,.T.);
#9689=FACE_OUTER_BOUND('',#14954,.T.);
#9690=FACE_OUTER_BOUND('',#14955,.T.);
#9691=FACE_OUTER_BOUND('',#14956,.T.);
#9692=FACE_OUTER_BOUND('',#14957,.T.);
#9693=FACE_OUTER_BOUND('',#14958,.T.);
#9694=FACE_OUTER_BOUND('',#14959,.T.);
#9695=FACE_OUTER_BOUND('',#14960,.T.);
#9696=FACE_OUTER_BOUND('',#14961,.T.);
#9697=FACE_OUTER_BOUND('',#14962,.T.);
#9698=FACE_OUTER_BOUND('',#14963,.T.);
#9699=FACE_OUTER_BOUND('',#14964,.T.);
#9700=FACE_OUTER_BOUND('',#14965,.T.);
#9701=FACE_OUTER_BOUND('',#14966,.T.);
#9702=FACE_OUTER_BOUND('',#14967,.T.);
#9703=FACE_OUTER_BOUND('',#14968,.T.);
#9704=FACE_OUTER_BOUND('',#14969,.T.);
#9705=FACE_OUTER_BOUND('',#14970,.T.);
#9706=FACE_OUTER_BOUND('',#14971,.T.);
#9707=FACE_OUTER_BOUND('',#14972,.T.);
#9708=FACE_OUTER_BOUND('',#14973,.T.);
#9709=FACE_OUTER_BOUND('',#14974,.T.);
#9710=FACE_OUTER_BOUND('',#14975,.T.);
#9711=FACE_OUTER_BOUND('',#14976,.T.);
#9712=FACE_OUTER_BOUND('',#14977,.T.);
#9713=FACE_OUTER_BOUND('',#14978,.T.);
#9714=FACE_OUTER_BOUND('',#14979,.T.);
#9715=FACE_OUTER_BOUND('',#14980,.T.);
#9716=FACE_OUTER_BOUND('',#14981,.T.);
#9717=FACE_OUTER_BOUND('',#14982,.T.);
#9718=FACE_OUTER_BOUND('',#14983,.T.);
#9719=FACE_OUTER_BOUND('',#14984,.T.);
#9720=FACE_OUTER_BOUND('',#14985,.T.);
#9721=FACE_OUTER_BOUND('',#14986,.T.);
#9722=FACE_OUTER_BOUND('',#14987,.T.);
#9723=FACE_OUTER_BOUND('',#14988,.T.);
#9724=FACE_OUTER_BOUND('',#14989,.T.);
#9725=FACE_OUTER_BOUND('',#14990,.T.);
#9726=FACE_OUTER_BOUND('',#14991,.T.);
#9727=FACE_OUTER_BOUND('',#14992,.T.);
#9728=FACE_OUTER_BOUND('',#14993,.T.);
#9729=FACE_OUTER_BOUND('',#14994,.T.);
#9730=FACE_OUTER_BOUND('',#14995,.T.);
#9731=FACE_OUTER_BOUND('',#14996,.T.);
#9732=FACE_OUTER_BOUND('',#14997,.T.);
#9733=FACE_OUTER_BOUND('',#14998,.T.);
#9734=FACE_OUTER_BOUND('',#14999,.T.);
#9735=FACE_OUTER_BOUND('',#15000,.T.);
#9736=FACE_OUTER_BOUND('',#15001,.T.);
#9737=FACE_OUTER_BOUND('',#15002,.T.);
#9738=FACE_OUTER_BOUND('',#15003,.T.);
#9739=FACE_OUTER_BOUND('',#15004,.T.);
#9740=FACE_OUTER_BOUND('',#15005,.T.);
#9741=FACE_OUTER_BOUND('',#15006,.T.);
#9742=FACE_OUTER_BOUND('',#15007,.T.);
#9743=FACE_OUTER_BOUND('',#15008,.T.);
#9744=FACE_OUTER_BOUND('',#15009,.T.);
#9745=FACE_OUTER_BOUND('',#15010,.T.);
#9746=FACE_OUTER_BOUND('',#15011,.T.);
#9747=FACE_OUTER_BOUND('',#15012,.T.);
#9748=FACE_OUTER_BOUND('',#15013,.T.);
#9749=FACE_OUTER_BOUND('',#15014,.T.);
#9750=FACE_OUTER_BOUND('',#15015,.T.);
#9751=FACE_OUTER_BOUND('',#15016,.T.);
#9752=FACE_OUTER_BOUND('',#15017,.T.);
#9753=FACE_OUTER_BOUND('',#15018,.T.);
#9754=FACE_OUTER_BOUND('',#15019,.T.);
#9755=FACE_OUTER_BOUND('',#15020,.T.);
#9756=FACE_OUTER_BOUND('',#15021,.T.);
#9757=FACE_OUTER_BOUND('',#15022,.T.);
#9758=FACE_OUTER_BOUND('',#15023,.T.);
#9759=FACE_OUTER_BOUND('',#15024,.T.);
#9760=FACE_OUTER_BOUND('',#15025,.T.);
#9761=FACE_OUTER_BOUND('',#15026,.T.);
#9762=FACE_OUTER_BOUND('',#15027,.T.);
#9763=FACE_OUTER_BOUND('',#15028,.T.);
#9764=FACE_OUTER_BOUND('',#15029,.T.);
#9765=FACE_OUTER_BOUND('',#15030,.T.);
#9766=FACE_OUTER_BOUND('',#15031,.T.);
#9767=FACE_OUTER_BOUND('',#15032,.T.);
#9768=FACE_OUTER_BOUND('',#15033,.T.);
#9769=FACE_OUTER_BOUND('',#15034,.T.);
#9770=FACE_OUTER_BOUND('',#15035,.T.);
#9771=FACE_OUTER_BOUND('',#15036,.T.);
#9772=FACE_OUTER_BOUND('',#15037,.T.);
#9773=FACE_OUTER_BOUND('',#15038,.T.);
#9774=FACE_OUTER_BOUND('',#15039,.T.);
#9775=FACE_OUTER_BOUND('',#15040,.T.);
#9776=FACE_OUTER_BOUND('',#15041,.T.);
#9777=FACE_OUTER_BOUND('',#15042,.T.);
#9778=FACE_OUTER_BOUND('',#15043,.T.);
#9779=FACE_OUTER_BOUND('',#15044,.T.);
#9780=FACE_OUTER_BOUND('',#15045,.T.);
#9781=FACE_OUTER_BOUND('',#15046,.T.);
#9782=FACE_OUTER_BOUND('',#15047,.T.);
#9783=FACE_OUTER_BOUND('',#15048,.T.);
#9784=FACE_OUTER_BOUND('',#15049,.T.);
#9785=FACE_OUTER_BOUND('',#15050,.T.);
#9786=FACE_OUTER_BOUND('',#15051,.T.);
#9787=FACE_OUTER_BOUND('',#15052,.T.);
#9788=FACE_OUTER_BOUND('',#15053,.T.);
#9789=FACE_OUTER_BOUND('',#15054,.T.);
#9790=FACE_OUTER_BOUND('',#15055,.T.);
#9791=FACE_OUTER_BOUND('',#15056,.T.);
#9792=FACE_OUTER_BOUND('',#15057,.T.);
#9793=FACE_OUTER_BOUND('',#15058,.T.);
#9794=FACE_OUTER_BOUND('',#15059,.T.);
#9795=FACE_OUTER_BOUND('',#15060,.T.);
#9796=FACE_OUTER_BOUND('',#15061,.T.);
#9797=FACE_OUTER_BOUND('',#15062,.T.);
#9798=FACE_OUTER_BOUND('',#15063,.T.);
#9799=FACE_OUTER_BOUND('',#15064,.T.);
#9800=FACE_OUTER_BOUND('',#15065,.T.);
#9801=FACE_OUTER_BOUND('',#15066,.T.);
#9802=FACE_OUTER_BOUND('',#15067,.T.);
#9803=FACE_OUTER_BOUND('',#15068,.T.);
#9804=FACE_OUTER_BOUND('',#15069,.T.);
#9805=FACE_OUTER_BOUND('',#15070,.T.);
#9806=FACE_OUTER_BOUND('',#15071,.T.);
#9807=FACE_OUTER_BOUND('',#15072,.T.);
#9808=FACE_OUTER_BOUND('',#15073,.T.);
#9809=FACE_OUTER_BOUND('',#15074,.T.);
#9810=FACE_OUTER_BOUND('',#15075,.T.);
#9811=FACE_OUTER_BOUND('',#15076,.T.);
#9812=FACE_OUTER_BOUND('',#15077,.T.);
#9813=FACE_OUTER_BOUND('',#15078,.T.);
#9814=FACE_OUTER_BOUND('',#15079,.T.);
#9815=FACE_OUTER_BOUND('',#15080,.T.);
#9816=FACE_OUTER_BOUND('',#15081,.T.);
#9817=FACE_OUTER_BOUND('',#15082,.T.);
#9818=FACE_OUTER_BOUND('',#15083,.T.);
#9819=FACE_OUTER_BOUND('',#15084,.T.);
#9820=FACE_OUTER_BOUND('',#15085,.T.);
#9821=FACE_OUTER_BOUND('',#15086,.T.);
#9822=FACE_OUTER_BOUND('',#15087,.T.);
#9823=FACE_OUTER_BOUND('',#15088,.T.);
#9824=FACE_OUTER_BOUND('',#15089,.T.);
#9825=FACE_OUTER_BOUND('',#15090,.T.);
#9826=FACE_OUTER_BOUND('',#15091,.T.);
#9827=FACE_OUTER_BOUND('',#15092,.T.);
#9828=FACE_OUTER_BOUND('',#15093,.T.);
#9829=FACE_OUTER_BOUND('',#15094,.T.);
#9830=FACE_OUTER_BOUND('',#15095,.T.);
#9831=FACE_OUTER_BOUND('',#15096,.T.);
#9832=FACE_OUTER_BOUND('',#15097,.T.);
#9833=FACE_OUTER_BOUND('',#15098,.T.);
#9834=FACE_OUTER_BOUND('',#15099,.T.);
#9835=FACE_OUTER_BOUND('',#15100,.T.);
#9836=FACE_OUTER_BOUND('',#15101,.T.);
#9837=FACE_OUTER_BOUND('',#15102,.T.);
#9838=FACE_OUTER_BOUND('',#15103,.T.);
#9839=FACE_OUTER_BOUND('',#15104,.T.);
#9840=FACE_OUTER_BOUND('',#15105,.T.);
#9841=FACE_OUTER_BOUND('',#15106,.T.);
#9842=FACE_OUTER_BOUND('',#15107,.T.);
#9843=FACE_OUTER_BOUND('',#15108,.T.);
#9844=FACE_OUTER_BOUND('',#15109,.T.);
#9845=FACE_OUTER_BOUND('',#15110,.T.);
#9846=FACE_OUTER_BOUND('',#15111,.T.);
#9847=FACE_OUTER_BOUND('',#15112,.T.);
#9848=FACE_OUTER_BOUND('',#15113,.T.);
#9849=FACE_OUTER_BOUND('',#15114,.T.);
#9850=FACE_OUTER_BOUND('',#15115,.T.);
#9851=FACE_OUTER_BOUND('',#15116,.T.);
#9852=FACE_OUTER_BOUND('',#15117,.T.);
#9853=FACE_OUTER_BOUND('',#15118,.T.);
#9854=FACE_OUTER_BOUND('',#15119,.T.);
#9855=FACE_OUTER_BOUND('',#15120,.T.);
#9856=FACE_OUTER_BOUND('',#15121,.T.);
#9857=FACE_OUTER_BOUND('',#15122,.T.);
#9858=FACE_OUTER_BOUND('',#15123,.T.);
#9859=FACE_OUTER_BOUND('',#15124,.T.);
#9860=FACE_OUTER_BOUND('',#15125,.T.);
#9861=FACE_OUTER_BOUND('',#15126,.T.);
#9862=FACE_OUTER_BOUND('',#15127,.T.);
#9863=FACE_OUTER_BOUND('',#15128,.T.);
#9864=FACE_OUTER_BOUND('',#15129,.T.);
#9865=FACE_OUTER_BOUND('',#15130,.T.);
#9866=FACE_OUTER_BOUND('',#15131,.T.);
#9867=FACE_OUTER_BOUND('',#15132,.T.);
#9868=FACE_OUTER_BOUND('',#15133,.T.);
#9869=FACE_OUTER_BOUND('',#15134,.T.);
#9870=FACE_OUTER_BOUND('',#15135,.T.);
#9871=FACE_OUTER_BOUND('',#15136,.T.);
#9872=FACE_OUTER_BOUND('',#15137,.T.);
#9873=FACE_OUTER_BOUND('',#15138,.T.);
#9874=FACE_OUTER_BOUND('',#15139,.T.);
#9875=FACE_OUTER_BOUND('',#15140,.T.);
#9876=FACE_OUTER_BOUND('',#15141,.T.);
#9877=FACE_OUTER_BOUND('',#15142,.T.);
#9878=FACE_OUTER_BOUND('',#15143,.T.);
#9879=FACE_OUTER_BOUND('',#15144,.T.);
#9880=FACE_OUTER_BOUND('',#15145,.T.);
#9881=FACE_OUTER_BOUND('',#15146,.T.);
#9882=FACE_OUTER_BOUND('',#15147,.T.);
#9883=FACE_OUTER_BOUND('',#15148,.T.);
#9884=FACE_OUTER_BOUND('',#15149,.T.);
#9885=FACE_OUTER_BOUND('',#15150,.T.);
#9886=FACE_OUTER_BOUND('',#15151,.T.);
#9887=FACE_OUTER_BOUND('',#15152,.T.);
#9888=FACE_OUTER_BOUND('',#15153,.T.);
#9889=FACE_OUTER_BOUND('',#15154,.T.);
#9890=FACE_OUTER_BOUND('',#15155,.T.);
#9891=FACE_OUTER_BOUND('',#15156,.T.);
#9892=FACE_OUTER_BOUND('',#15157,.T.);
#9893=FACE_OUTER_BOUND('',#15158,.T.);
#9894=FACE_OUTER_BOUND('',#15159,.T.);
#9895=FACE_OUTER_BOUND('',#15160,.T.);
#9896=FACE_OUTER_BOUND('',#15161,.T.);
#9897=FACE_OUTER_BOUND('',#15162,.T.);
#9898=FACE_OUTER_BOUND('',#15163,.T.);
#9899=FACE_OUTER_BOUND('',#15164,.T.);
#9900=FACE_OUTER_BOUND('',#15165,.T.);
#9901=FACE_OUTER_BOUND('',#15166,.T.);
#9902=FACE_OUTER_BOUND('',#15167,.T.);
#9903=FACE_OUTER_BOUND('',#15168,.T.);
#9904=FACE_OUTER_BOUND('',#15169,.T.);
#9905=FACE_OUTER_BOUND('',#15170,.T.);
#9906=FACE_OUTER_BOUND('',#15171,.T.);
#9907=FACE_OUTER_BOUND('',#15172,.T.);
#9908=FACE_OUTER_BOUND('',#15173,.T.);
#9909=FACE_OUTER_BOUND('',#15174,.T.);
#9910=FACE_OUTER_BOUND('',#15175,.T.);
#9911=FACE_OUTER_BOUND('',#15176,.T.);
#9912=FACE_OUTER_BOUND('',#15177,.T.);
#9913=FACE_OUTER_BOUND('',#15178,.T.);
#9914=FACE_OUTER_BOUND('',#15179,.T.);
#9915=FACE_OUTER_BOUND('',#15180,.T.);
#9916=FACE_OUTER_BOUND('',#15181,.T.);
#9917=FACE_OUTER_BOUND('',#15182,.T.);
#9918=FACE_OUTER_BOUND('',#15183,.T.);
#9919=FACE_OUTER_BOUND('',#15184,.T.);
#9920=FACE_OUTER_BOUND('',#15185,.T.);
#9921=FACE_OUTER_BOUND('',#15186,.T.);
#9922=FACE_OUTER_BOUND('',#15187,.T.);
#9923=FACE_OUTER_BOUND('',#15188,.T.);
#9924=FACE_OUTER_BOUND('',#15189,.T.);
#9925=FACE_OUTER_BOUND('',#15190,.T.);
#9926=FACE_OUTER_BOUND('',#15191,.T.);
#9927=FACE_OUTER_BOUND('',#15192,.T.);
#9928=FACE_OUTER_BOUND('',#15193,.T.);
#9929=FACE_OUTER_BOUND('',#15194,.T.);
#9930=FACE_OUTER_BOUND('',#15195,.T.);
#9931=FACE_OUTER_BOUND('',#15196,.T.);
#9932=FACE_OUTER_BOUND('',#15197,.T.);
#9933=FACE_OUTER_BOUND('',#15198,.T.);
#9934=FACE_OUTER_BOUND('',#15199,.T.);
#9935=FACE_OUTER_BOUND('',#15200,.T.);
#9936=FACE_OUTER_BOUND('',#15201,.T.);
#9937=FACE_OUTER_BOUND('',#15202,.T.);
#9938=FACE_OUTER_BOUND('',#15203,.T.);
#9939=FACE_OUTER_BOUND('',#15204,.T.);
#9940=FACE_OUTER_BOUND('',#15205,.T.);
#9941=FACE_OUTER_BOUND('',#15206,.T.);
#9942=FACE_OUTER_BOUND('',#15207,.T.);
#9943=FACE_OUTER_BOUND('',#15208,.T.);
#9944=FACE_OUTER_BOUND('',#15209,.T.);
#9945=FACE_OUTER_BOUND('',#15210,.T.);
#9946=FACE_OUTER_BOUND('',#15211,.T.);
#9947=FACE_OUTER_BOUND('',#15212,.T.);
#9948=FACE_OUTER_BOUND('',#15213,.T.);
#9949=FACE_OUTER_BOUND('',#15214,.T.);
#9950=FACE_OUTER_BOUND('',#15215,.T.);
#9951=FACE_OUTER_BOUND('',#15216,.T.);
#9952=FACE_OUTER_BOUND('',#15217,.T.);
#9953=FACE_OUTER_BOUND('',#15218,.T.);
#9954=FACE_OUTER_BOUND('',#15219,.T.);
#9955=FACE_OUTER_BOUND('',#15220,.T.);
#9956=FACE_OUTER_BOUND('',#15221,.T.);
#9957=FACE_OUTER_BOUND('',#15222,.T.);
#9958=FACE_OUTER_BOUND('',#15223,.T.);
#9959=FACE_OUTER_BOUND('',#15224,.T.);
#9960=FACE_OUTER_BOUND('',#15225,.T.);
#9961=FACE_OUTER_BOUND('',#15226,.T.);
#9962=FACE_OUTER_BOUND('',#15227,.T.);
#9963=FACE_OUTER_BOUND('',#15228,.T.);
#9964=FACE_OUTER_BOUND('',#15229,.T.);
#9965=FACE_OUTER_BOUND('',#15230,.T.);
#9966=FACE_OUTER_BOUND('',#15231,.T.);
#9967=FACE_OUTER_BOUND('',#15232,.T.);
#9968=FACE_OUTER_BOUND('',#15233,.T.);
#9969=FACE_OUTER_BOUND('',#15234,.T.);
#9970=FACE_OUTER_BOUND('',#15235,.T.);
#9971=FACE_OUTER_BOUND('',#15236,.T.);
#9972=FACE_OUTER_BOUND('',#15237,.T.);
#9973=FACE_OUTER_BOUND('',#15238,.T.);
#9974=FACE_OUTER_BOUND('',#15239,.T.);
#9975=FACE_OUTER_BOUND('',#15240,.T.);
#9976=FACE_OUTER_BOUND('',#15241,.T.);
#9977=FACE_OUTER_BOUND('',#15242,.T.);
#9978=FACE_OUTER_BOUND('',#15243,.T.);
#9979=FACE_OUTER_BOUND('',#15244,.T.);
#9980=FACE_OUTER_BOUND('',#15245,.T.);
#9981=FACE_OUTER_BOUND('',#15246,.T.);
#9982=FACE_OUTER_BOUND('',#15247,.T.);
#9983=FACE_OUTER_BOUND('',#15248,.T.);
#9984=FACE_OUTER_BOUND('',#15249,.T.);
#9985=FACE_OUTER_BOUND('',#15250,.T.);
#9986=FACE_OUTER_BOUND('',#15251,.T.);
#9987=FACE_OUTER_BOUND('',#15252,.T.);
#9988=FACE_OUTER_BOUND('',#15253,.T.);
#9989=FACE_OUTER_BOUND('',#15254,.T.);
#9990=FACE_OUTER_BOUND('',#15255,.T.);
#9991=FACE_OUTER_BOUND('',#15256,.T.);
#9992=FACE_OUTER_BOUND('',#15257,.T.);
#9993=FACE_OUTER_BOUND('',#15258,.T.);
#9994=FACE_OUTER_BOUND('',#15259,.T.);
#9995=FACE_OUTER_BOUND('',#15260,.T.);
#9996=FACE_OUTER_BOUND('',#15261,.T.);
#9997=FACE_OUTER_BOUND('',#15262,.T.);
#9998=FACE_OUTER_BOUND('',#15263,.T.);
#9999=FACE_OUTER_BOUND('',#15264,.T.);
#10000=FACE_OUTER_BOUND('',#15265,.T.);
#10001=FACE_OUTER_BOUND('',#15266,.T.);
#10002=FACE_OUTER_BOUND('',#15267,.T.);
#10003=FACE_OUTER_BOUND('',#15268,.T.);
#10004=FACE_OUTER_BOUND('',#15269,.T.);
#10005=FACE_OUTER_BOUND('',#15270,.T.);
#10006=FACE_OUTER_BOUND('',#15271,.T.);
#10007=FACE_OUTER_BOUND('',#15272,.T.);
#10008=FACE_OUTER_BOUND('',#15273,.T.);
#10009=FACE_OUTER_BOUND('',#15274,.T.);
#10010=FACE_OUTER_BOUND('',#15275,.T.);
#10011=FACE_OUTER_BOUND('',#15276,.T.);
#10012=FACE_OUTER_BOUND('',#15277,.T.);
#10013=FACE_OUTER_BOUND('',#15278,.T.);
#10014=FACE_OUTER_BOUND('',#15279,.T.);
#10015=FACE_OUTER_BOUND('',#15280,.T.);
#10016=FACE_OUTER_BOUND('',#15281,.T.);
#10017=FACE_OUTER_BOUND('',#15282,.T.);
#10018=FACE_OUTER_BOUND('',#15283,.T.);
#10019=FACE_OUTER_BOUND('',#15284,.T.);
#10020=FACE_OUTER_BOUND('',#15285,.T.);
#10021=FACE_OUTER_BOUND('',#15286,.T.);
#10022=FACE_OUTER_BOUND('',#15287,.T.);
#10023=FACE_OUTER_BOUND('',#15288,.T.);
#10024=FACE_OUTER_BOUND('',#15289,.T.);
#10025=FACE_OUTER_BOUND('',#15290,.T.);
#10026=FACE_OUTER_BOUND('',#15291,.T.);
#10027=FACE_OUTER_BOUND('',#15292,.T.);
#10028=FACE_OUTER_BOUND('',#15293,.T.);
#10029=FACE_OUTER_BOUND('',#15294,.T.);
#10030=FACE_OUTER_BOUND('',#15295,.T.);
#10031=FACE_OUTER_BOUND('',#15296,.T.);
#10032=FACE_OUTER_BOUND('',#15297,.T.);
#10033=FACE_OUTER_BOUND('',#15298,.T.);
#10034=FACE_OUTER_BOUND('',#15299,.T.);
#10035=FACE_OUTER_BOUND('',#15300,.T.);
#10036=FACE_OUTER_BOUND('',#15301,.T.);
#10037=FACE_OUTER_BOUND('',#15302,.T.);
#10038=FACE_OUTER_BOUND('',#15303,.T.);
#10039=FACE_OUTER_BOUND('',#15304,.T.);
#10040=FACE_OUTER_BOUND('',#15305,.T.);
#10041=FACE_OUTER_BOUND('',#15306,.T.);
#10042=FACE_OUTER_BOUND('',#15307,.T.);
#10043=FACE_OUTER_BOUND('',#15308,.T.);
#10044=FACE_OUTER_BOUND('',#15309,.T.);
#10045=FACE_OUTER_BOUND('',#15310,.T.);
#10046=FACE_OUTER_BOUND('',#15311,.T.);
#10047=FACE_OUTER_BOUND('',#15312,.T.);
#10048=FACE_OUTER_BOUND('',#15313,.T.);
#10049=FACE_OUTER_BOUND('',#15314,.T.);
#10050=FACE_OUTER_BOUND('',#15315,.T.);
#10051=FACE_OUTER_BOUND('',#15316,.T.);
#10052=FACE_OUTER_BOUND('',#15317,.T.);
#10053=FACE_OUTER_BOUND('',#15318,.T.);
#10054=FACE_OUTER_BOUND('',#15319,.T.);
#10055=FACE_OUTER_BOUND('',#15320,.T.);
#10056=FACE_OUTER_BOUND('',#15321,.T.);
#10057=FACE_OUTER_BOUND('',#15322,.T.);
#10058=FACE_OUTER_BOUND('',#15323,.T.);
#10059=FACE_OUTER_BOUND('',#15324,.T.);
#10060=FACE_OUTER_BOUND('',#15325,.T.);
#10061=FACE_OUTER_BOUND('',#15326,.T.);
#10062=FACE_OUTER_BOUND('',#15327,.T.);
#10063=FACE_OUTER_BOUND('',#15328,.T.);
#10064=FACE_OUTER_BOUND('',#15329,.T.);
#10065=FACE_OUTER_BOUND('',#15330,.T.);
#10066=FACE_OUTER_BOUND('',#15331,.T.);
#10067=FACE_OUTER_BOUND('',#15332,.T.);
#10068=FACE_OUTER_BOUND('',#15333,.T.);
#10069=FACE_OUTER_BOUND('',#15334,.T.);
#10070=FACE_OUTER_BOUND('',#15335,.T.);
#10071=FACE_OUTER_BOUND('',#15336,.T.);
#10072=FACE_OUTER_BOUND('',#15337,.T.);
#10073=FACE_OUTER_BOUND('',#15338,.T.);
#10074=FACE_OUTER_BOUND('',#15339,.T.);
#10075=FACE_OUTER_BOUND('',#15340,.T.);
#10076=FACE_OUTER_BOUND('',#15341,.T.);
#10077=FACE_OUTER_BOUND('',#15342,.T.);
#10078=FACE_OUTER_BOUND('',#15343,.T.);
#10079=FACE_OUTER_BOUND('',#15344,.T.);
#10080=FACE_OUTER_BOUND('',#15345,.T.);
#10081=FACE_OUTER_BOUND('',#15346,.T.);
#10082=FACE_OUTER_BOUND('',#15347,.T.);
#10083=FACE_OUTER_BOUND('',#15348,.T.);
#10084=FACE_OUTER_BOUND('',#15349,.T.);
#10085=FACE_OUTER_BOUND('',#15350,.T.);
#10086=FACE_OUTER_BOUND('',#15351,.T.);
#10087=FACE_OUTER_BOUND('',#15352,.T.);
#10088=FACE_OUTER_BOUND('',#15353,.T.);
#10089=FACE_OUTER_BOUND('',#15354,.T.);
#10090=FACE_OUTER_BOUND('',#15355,.T.);
#10091=FACE_OUTER_BOUND('',#15356,.T.);
#10092=FACE_OUTER_BOUND('',#15357,.T.);
#10093=FACE_OUTER_BOUND('',#15358,.T.);
#10094=FACE_OUTER_BOUND('',#15359,.T.);
#10095=FACE_OUTER_BOUND('',#15360,.T.);
#10096=FACE_OUTER_BOUND('',#15361,.T.);
#10097=FACE_OUTER_BOUND('',#15362,.T.);
#10098=FACE_OUTER_BOUND('',#15363,.T.);
#10099=FACE_OUTER_BOUND('',#15364,.T.);
#10100=FACE_OUTER_BOUND('',#15365,.T.);
#10101=FACE_OUTER_BOUND('',#15366,.T.);
#10102=FACE_OUTER_BOUND('',#15367,.T.);
#10103=FACE_OUTER_BOUND('',#15368,.T.);
#10104=FACE_OUTER_BOUND('',#15369,.T.);
#10105=FACE_OUTER_BOUND('',#15370,.T.);
#10106=FACE_OUTER_BOUND('',#15371,.T.);
#10107=FACE_OUTER_BOUND('',#15372,.T.);
#10108=FACE_OUTER_BOUND('',#15373,.T.);
#10109=FACE_OUTER_BOUND('',#15374,.T.);
#10110=FACE_OUTER_BOUND('',#15375,.T.);
#10111=FACE_OUTER_BOUND('',#15376,.T.);
#10112=FACE_OUTER_BOUND('',#15377,.T.);
#10113=FACE_OUTER_BOUND('',#15378,.T.);
#10114=FACE_OUTER_BOUND('',#15379,.T.);
#10115=FACE_OUTER_BOUND('',#15380,.T.);
#10116=FACE_OUTER_BOUND('',#15381,.T.);
#10117=FACE_OUTER_BOUND('',#15382,.T.);
#10118=FACE_OUTER_BOUND('',#15383,.T.);
#10119=FACE_OUTER_BOUND('',#15384,.T.);
#10120=FACE_OUTER_BOUND('',#15385,.T.);
#10121=FACE_OUTER_BOUND('',#15386,.T.);
#10122=FACE_OUTER_BOUND('',#15387,.T.);
#10123=FACE_OUTER_BOUND('',#15388,.T.);
#10124=FACE_OUTER_BOUND('',#15389,.T.);
#10125=FACE_OUTER_BOUND('',#15390,.T.);
#10126=FACE_OUTER_BOUND('',#15391,.T.);
#10127=FACE_OUTER_BOUND('',#15392,.T.);
#10128=FACE_OUTER_BOUND('',#15393,.T.);
#10129=FACE_OUTER_BOUND('',#15394,.T.);
#10130=FACE_OUTER_BOUND('',#15395,.T.);
#10131=FACE_OUTER_BOUND('',#15396,.T.);
#10132=FACE_OUTER_BOUND('',#15397,.T.);
#10133=FACE_OUTER_BOUND('',#15398,.T.);
#10134=FACE_OUTER_BOUND('',#15399,.T.);
#10135=FACE_OUTER_BOUND('',#15400,.T.);
#10136=FACE_OUTER_BOUND('',#15401,.T.);
#10137=FACE_OUTER_BOUND('',#15402,.T.);
#10138=FACE_OUTER_BOUND('',#15403,.T.);
#10139=FACE_OUTER_BOUND('',#15404,.T.);
#10140=FACE_OUTER_BOUND('',#15405,.T.);
#10141=FACE_OUTER_BOUND('',#15406,.T.);
#10142=FACE_OUTER_BOUND('',#15407,.T.);
#10143=FACE_OUTER_BOUND('',#15408,.T.);
#10144=FACE_OUTER_BOUND('',#15409,.T.);
#10145=FACE_OUTER_BOUND('',#15410,.T.);
#10146=FACE_OUTER_BOUND('',#15411,.T.);
#10147=FACE_OUTER_BOUND('',#15412,.T.);
#10148=FACE_OUTER_BOUND('',#15413,.T.);
#10149=FACE_OUTER_BOUND('',#15414,.T.);
#10150=FACE_OUTER_BOUND('',#15415,.T.);
#10151=FACE_OUTER_BOUND('',#15416,.T.);
#10152=FACE_OUTER_BOUND('',#15417,.T.);
#10153=FACE_OUTER_BOUND('',#15418,.T.);
#10154=FACE_OUTER_BOUND('',#15419,.T.);
#10155=FACE_OUTER_BOUND('',#15420,.T.);
#10156=FACE_OUTER_BOUND('',#15421,.T.);
#10157=FACE_OUTER_BOUND('',#15422,.T.);
#10158=FACE_OUTER_BOUND('',#15423,.T.);
#10159=FACE_OUTER_BOUND('',#15424,.T.);
#10160=FACE_OUTER_BOUND('',#15425,.T.);
#10161=FACE_OUTER_BOUND('',#15426,.T.);
#10162=FACE_OUTER_BOUND('',#15427,.T.);
#10163=FACE_OUTER_BOUND('',#15428,.T.);
#10164=FACE_OUTER_BOUND('',#15429,.T.);
#10165=FACE_OUTER_BOUND('',#15430,.T.);
#10166=FACE_OUTER_BOUND('',#15431,.T.);
#10167=FACE_OUTER_BOUND('',#15432,.T.);
#10168=FACE_OUTER_BOUND('',#15433,.T.);
#10169=FACE_OUTER_BOUND('',#15434,.T.);
#10170=FACE_OUTER_BOUND('',#15435,.T.);
#10171=FACE_OUTER_BOUND('',#15436,.T.);
#10172=FACE_OUTER_BOUND('',#15437,.T.);
#10173=FACE_OUTER_BOUND('',#15438,.T.);
#10174=FACE_OUTER_BOUND('',#15439,.T.);
#10175=FACE_OUTER_BOUND('',#15440,.T.);
#10176=FACE_OUTER_BOUND('',#15441,.T.);
#10177=FACE_OUTER_BOUND('',#15442,.T.);
#10178=FACE_OUTER_BOUND('',#15443,.T.);
#10179=FACE_OUTER_BOUND('',#15444,.T.);
#10180=FACE_OUTER_BOUND('',#15445,.T.);
#10181=FACE_OUTER_BOUND('',#15446,.T.);
#10182=FACE_OUTER_BOUND('',#15447,.T.);
#10183=FACE_OUTER_BOUND('',#15448,.T.);
#10184=FACE_OUTER_BOUND('',#15449,.T.);
#10185=FACE_OUTER_BOUND('',#15450,.T.);
#10186=FACE_OUTER_BOUND('',#15451,.T.);
#10187=FACE_OUTER_BOUND('',#15452,.T.);
#10188=FACE_OUTER_BOUND('',#15453,.T.);
#10189=FACE_OUTER_BOUND('',#15454,.T.);
#10190=FACE_OUTER_BOUND('',#15455,.T.);
#10191=FACE_OUTER_BOUND('',#15456,.T.);
#10192=FACE_OUTER_BOUND('',#15457,.T.);
#10193=FACE_OUTER_BOUND('',#15458,.T.);
#10194=FACE_OUTER_BOUND('',#15459,.T.);
#10195=FACE_OUTER_BOUND('',#15460,.T.);
#10196=FACE_OUTER_BOUND('',#15461,.T.);
#10197=FACE_OUTER_BOUND('',#15462,.T.);
#10198=FACE_OUTER_BOUND('',#15463,.T.);
#10199=FACE_OUTER_BOUND('',#15464,.T.);
#10200=FACE_OUTER_BOUND('',#15465,.T.);
#10201=FACE_OUTER_BOUND('',#15466,.T.);
#10202=FACE_OUTER_BOUND('',#15467,.T.);
#10203=FACE_OUTER_BOUND('',#15468,.T.);
#10204=FACE_OUTER_BOUND('',#15469,.T.);
#10205=FACE_OUTER_BOUND('',#15470,.T.);
#10206=FACE_OUTER_BOUND('',#15471,.T.);
#10207=FACE_OUTER_BOUND('',#15473,.T.);
#10208=FACE_OUTER_BOUND('',#15474,.T.);
#10209=FACE_OUTER_BOUND('',#15475,.T.);
#10210=FACE_OUTER_BOUND('',#15476,.T.);
#10211=FACE_OUTER_BOUND('',#15477,.T.);
#10212=FACE_OUTER_BOUND('',#15478,.T.);
#10213=FACE_OUTER_BOUND('',#15479,.T.);
#10214=FACE_OUTER_BOUND('',#15480,.T.);
#10215=FACE_OUTER_BOUND('',#15481,.T.);
#10216=FACE_OUTER_BOUND('',#15482,.T.);
#10217=FACE_OUTER_BOUND('',#15483,.T.);
#10218=FACE_OUTER_BOUND('',#15484,.T.);
#10219=FACE_OUTER_BOUND('',#15485,.T.);
#10220=FACE_OUTER_BOUND('',#15486,.T.);
#10221=FACE_OUTER_BOUND('',#15487,.T.);
#10222=FACE_OUTER_BOUND('',#15488,.T.);
#10223=FACE_OUTER_BOUND('',#15489,.T.);
#10224=FACE_OUTER_BOUND('',#15490,.T.);
#10225=FACE_OUTER_BOUND('',#15491,.T.);
#10226=FACE_OUTER_BOUND('',#15492,.T.);
#10227=FACE_OUTER_BOUND('',#15493,.T.);
#10228=FACE_OUTER_BOUND('',#15494,.T.);
#10229=FACE_OUTER_BOUND('',#15495,.T.);
#10230=FACE_OUTER_BOUND('',#15496,.T.);
#10231=FACE_OUTER_BOUND('',#15497,.T.);
#10232=FACE_OUTER_BOUND('',#15498,.T.);
#10233=FACE_OUTER_BOUND('',#15499,.T.);
#10234=FACE_OUTER_BOUND('',#15500,.T.);
#10235=FACE_OUTER_BOUND('',#15501,.T.);
#10236=FACE_OUTER_BOUND('',#15502,.T.);
#10237=FACE_OUTER_BOUND('',#15503,.T.);
#10238=FACE_OUTER_BOUND('',#15504,.T.);
#10239=FACE_OUTER_BOUND('',#15505,.T.);
#10240=FACE_OUTER_BOUND('',#15506,.T.);
#10241=FACE_OUTER_BOUND('',#15507,.T.);
#10242=FACE_OUTER_BOUND('',#15508,.T.);
#10243=FACE_OUTER_BOUND('',#15509,.T.);
#10244=FACE_OUTER_BOUND('',#15510,.T.);
#10245=FACE_OUTER_BOUND('',#15511,.T.);
#10246=FACE_OUTER_BOUND('',#15512,.T.);
#10247=FACE_OUTER_BOUND('',#15513,.T.);
#10248=FACE_OUTER_BOUND('',#15514,.T.);
#10249=FACE_OUTER_BOUND('',#15515,.T.);
#10250=FACE_OUTER_BOUND('',#15516,.T.);
#10251=FACE_OUTER_BOUND('',#15517,.T.);
#10252=FACE_OUTER_BOUND('',#15518,.T.);
#10253=FACE_OUTER_BOUND('',#15519,.T.);
#10254=FACE_OUTER_BOUND('',#15520,.T.);
#10255=FACE_OUTER_BOUND('',#15521,.T.);
#10256=FACE_OUTER_BOUND('',#15522,.T.);
#10257=FACE_OUTER_BOUND('',#15523,.T.);
#10258=FACE_OUTER_BOUND('',#15524,.T.);
#10259=FACE_OUTER_BOUND('',#15525,.T.);
#10260=FACE_OUTER_BOUND('',#15526,.T.);
#10261=FACE_OUTER_BOUND('',#15527,.T.);
#10262=FACE_OUTER_BOUND('',#15528,.T.);
#10263=FACE_OUTER_BOUND('',#15529,.T.);
#10264=FACE_OUTER_BOUND('',#15530,.T.);
#10265=FACE_OUTER_BOUND('',#15531,.T.);
#10266=FACE_OUTER_BOUND('',#15532,.T.);
#10267=FACE_OUTER_BOUND('',#15533,.T.);
#10268=FACE_OUTER_BOUND('',#15534,.T.);
#10269=FACE_OUTER_BOUND('',#15535,.T.);
#10270=FACE_OUTER_BOUND('',#15536,.T.);
#10271=FACE_OUTER_BOUND('',#15537,.T.);
#10272=FACE_OUTER_BOUND('',#15538,.T.);
#10273=FACE_OUTER_BOUND('',#15539,.T.);
#10274=FACE_OUTER_BOUND('',#15540,.T.);
#10275=FACE_OUTER_BOUND('',#15541,.T.);
#10276=FACE_OUTER_BOUND('',#15542,.T.);
#10277=FACE_OUTER_BOUND('',#15543,.T.);
#10278=FACE_OUTER_BOUND('',#15544,.T.);
#10279=FACE_OUTER_BOUND('',#15545,.T.);
#10280=FACE_OUTER_BOUND('',#15546,.T.);
#10281=FACE_OUTER_BOUND('',#15547,.T.);
#10282=FACE_OUTER_BOUND('',#15548,.T.);
#10283=FACE_OUTER_BOUND('',#15549,.T.);
#10284=FACE_OUTER_BOUND('',#15550,.T.);
#10285=FACE_OUTER_BOUND('',#15551,.T.);
#10286=FACE_OUTER_BOUND('',#15552,.T.);
#10287=FACE_OUTER_BOUND('',#15553,.T.);
#10288=FACE_OUTER_BOUND('',#15554,.T.);
#10289=FACE_OUTER_BOUND('',#15555,.T.);
#10290=FACE_OUTER_BOUND('',#15556,.T.);
#10291=FACE_OUTER_BOUND('',#15557,.T.);
#10292=FACE_OUTER_BOUND('',#15558,.T.);
#10293=FACE_OUTER_BOUND('',#15559,.T.);
#10294=FACE_OUTER_BOUND('',#15560,.T.);
#10295=FACE_OUTER_BOUND('',#15561,.T.);
#10296=FACE_OUTER_BOUND('',#15562,.T.);
#10297=FACE_OUTER_BOUND('',#15563,.T.);
#10298=FACE_OUTER_BOUND('',#15564,.T.);
#10299=FACE_OUTER_BOUND('',#15565,.T.);
#10300=FACE_OUTER_BOUND('',#15566,.T.);
#10301=FACE_OUTER_BOUND('',#15567,.T.);
#10302=FACE_OUTER_BOUND('',#15568,.T.);
#10303=FACE_OUTER_BOUND('',#15569,.T.);
#10304=FACE_OUTER_BOUND('',#15570,.T.);
#10305=FACE_OUTER_BOUND('',#15571,.T.);
#10306=FACE_OUTER_BOUND('',#15572,.T.);
#10307=FACE_OUTER_BOUND('',#15573,.T.);
#10308=FACE_OUTER_BOUND('',#15574,.T.);
#10309=FACE_OUTER_BOUND('',#15575,.T.);
#10310=FACE_OUTER_BOUND('',#15576,.T.);
#10311=FACE_OUTER_BOUND('',#15577,.T.);
#10312=FACE_OUTER_BOUND('',#15578,.T.);
#10313=FACE_OUTER_BOUND('',#15579,.T.);
#10314=FACE_OUTER_BOUND('',#15580,.T.);
#10315=FACE_OUTER_BOUND('',#15581,.T.);
#10316=FACE_OUTER_BOUND('',#15582,.T.);
#10317=FACE_OUTER_BOUND('',#15583,.T.);
#10318=FACE_OUTER_BOUND('',#15584,.T.);
#10319=FACE_OUTER_BOUND('',#15585,.T.);
#10320=FACE_OUTER_BOUND('',#15586,.T.);
#10321=FACE_OUTER_BOUND('',#15587,.T.);
#10322=FACE_OUTER_BOUND('',#15588,.T.);
#10323=FACE_OUTER_BOUND('',#15589,.T.);
#10324=FACE_OUTER_BOUND('',#15590,.T.);
#10325=FACE_OUTER_BOUND('',#15591,.T.);
#10326=FACE_OUTER_BOUND('',#15592,.T.);
#10327=FACE_OUTER_BOUND('',#15593,.T.);
#10328=FACE_OUTER_BOUND('',#15594,.T.);
#10329=FACE_OUTER_BOUND('',#15595,.T.);
#10330=FACE_OUTER_BOUND('',#15596,.T.);
#10331=FACE_OUTER_BOUND('',#15597,.T.);
#10332=FACE_OUTER_BOUND('',#15598,.T.);
#10333=FACE_OUTER_BOUND('',#15599,.T.);
#10334=FACE_OUTER_BOUND('',#15600,.T.);
#10335=FACE_OUTER_BOUND('',#15601,.T.);
#10336=FACE_OUTER_BOUND('',#15602,.T.);
#10337=FACE_OUTER_BOUND('',#15603,.T.);
#10338=FACE_OUTER_BOUND('',#15604,.T.);
#10339=FACE_OUTER_BOUND('',#15605,.T.);
#10340=FACE_OUTER_BOUND('',#15606,.T.);
#10341=FACE_OUTER_BOUND('',#15607,.T.);
#10342=FACE_OUTER_BOUND('',#15608,.T.);
#10343=FACE_OUTER_BOUND('',#15609,.T.);
#10344=FACE_OUTER_BOUND('',#15610,.T.);
#10345=FACE_OUTER_BOUND('',#15611,.T.);
#10346=FACE_OUTER_BOUND('',#15612,.T.);
#10347=FACE_OUTER_BOUND('',#15613,.T.);
#10348=FACE_OUTER_BOUND('',#15614,.T.);
#10349=FACE_OUTER_BOUND('',#15615,.T.);
#10350=FACE_OUTER_BOUND('',#15616,.T.);
#10351=FACE_OUTER_BOUND('',#15617,.T.);
#10352=FACE_OUTER_BOUND('',#15618,.T.);
#10353=FACE_OUTER_BOUND('',#15619,.T.);
#10354=FACE_OUTER_BOUND('',#15620,.T.);
#10355=FACE_OUTER_BOUND('',#15621,.T.);
#10356=FACE_OUTER_BOUND('',#15622,.T.);
#10357=FACE_OUTER_BOUND('',#15623,.T.);
#10358=FACE_OUTER_BOUND('',#15624,.T.);
#10359=FACE_OUTER_BOUND('',#15625,.T.);
#10360=FACE_OUTER_BOUND('',#15626,.T.);
#10361=FACE_OUTER_BOUND('',#15627,.T.);
#10362=FACE_OUTER_BOUND('',#15628,.T.);
#10363=FACE_OUTER_BOUND('',#15629,.T.);
#10364=FACE_OUTER_BOUND('',#15630,.T.);
#10365=FACE_OUTER_BOUND('',#15631,.T.);
#10366=FACE_OUTER_BOUND('',#15632,.T.);
#10367=FACE_OUTER_BOUND('',#15633,.T.);
#10368=FACE_OUTER_BOUND('',#15634,.T.);
#10369=FACE_OUTER_BOUND('',#15635,.T.);
#10370=FACE_OUTER_BOUND('',#15636,.T.);
#10371=FACE_OUTER_BOUND('',#15637,.T.);
#10372=FACE_OUTER_BOUND('',#15638,.T.);
#10373=FACE_OUTER_BOUND('',#15639,.T.);
#10374=FACE_OUTER_BOUND('',#15640,.T.);
#10375=FACE_OUTER_BOUND('',#15641,.T.);
#10376=FACE_OUTER_BOUND('',#15642,.T.);
#10377=FACE_OUTER_BOUND('',#15643,.T.);
#10378=FACE_OUTER_BOUND('',#15644,.T.);
#10379=FACE_OUTER_BOUND('',#15645,.T.);
#10380=FACE_OUTER_BOUND('',#15646,.T.);
#10381=FACE_OUTER_BOUND('',#15647,.T.);
#10382=FACE_OUTER_BOUND('',#15648,.T.);
#10383=FACE_OUTER_BOUND('',#15649,.T.);
#10384=FACE_OUTER_BOUND('',#15650,.T.);
#10385=FACE_OUTER_BOUND('',#15651,.T.);
#10386=FACE_OUTER_BOUND('',#15652,.T.);
#10387=FACE_OUTER_BOUND('',#15653,.T.);
#10388=FACE_OUTER_BOUND('',#15654,.T.);
#10389=FACE_OUTER_BOUND('',#15655,.T.);
#10390=FACE_OUTER_BOUND('',#15656,.T.);
#10391=FACE_OUTER_BOUND('',#15657,.T.);
#10392=FACE_OUTER_BOUND('',#15658,.T.);
#10393=FACE_OUTER_BOUND('',#15659,.T.);
#10394=FACE_OUTER_BOUND('',#15660,.T.);
#10395=FACE_OUTER_BOUND('',#15661,.T.);
#10396=FACE_OUTER_BOUND('',#15662,.T.);
#10397=FACE_OUTER_BOUND('',#15663,.T.);
#10398=FACE_OUTER_BOUND('',#15664,.T.);
#10399=FACE_OUTER_BOUND('',#15665,.T.);
#10400=FACE_OUTER_BOUND('',#15666,.T.);
#10401=FACE_OUTER_BOUND('',#15667,.T.);
#10402=FACE_OUTER_BOUND('',#15668,.T.);
#10403=FACE_OUTER_BOUND('',#15669,.T.);
#10404=FACE_OUTER_BOUND('',#15670,.T.);
#10405=FACE_OUTER_BOUND('',#15671,.T.);
#10406=FACE_OUTER_BOUND('',#15672,.T.);
#10407=FACE_OUTER_BOUND('',#15673,.T.);
#10408=FACE_OUTER_BOUND('',#15674,.T.);
#10409=FACE_OUTER_BOUND('',#15676,.T.);
#10410=FACE_OUTER_BOUND('',#15677,.T.);
#10411=FACE_OUTER_BOUND('',#15678,.T.);
#10412=FACE_OUTER_BOUND('',#15679,.T.);
#10413=FACE_OUTER_BOUND('',#15680,.T.);
#10414=FACE_OUTER_BOUND('',#15681,.T.);
#10415=FACE_OUTER_BOUND('',#15682,.T.);
#10416=FACE_OUTER_BOUND('',#15683,.T.);
#10417=FACE_OUTER_BOUND('',#15684,.T.);
#10418=FACE_OUTER_BOUND('',#15685,.T.);
#10419=FACE_OUTER_BOUND('',#15686,.T.);
#10420=FACE_OUTER_BOUND('',#15687,.T.);
#10421=FACE_OUTER_BOUND('',#15688,.T.);
#10422=FACE_OUTER_BOUND('',#15689,.T.);
#10423=FACE_OUTER_BOUND('',#15690,.T.);
#10424=FACE_OUTER_BOUND('',#15691,.T.);
#10425=FACE_OUTER_BOUND('',#15692,.T.);
#10426=FACE_OUTER_BOUND('',#15693,.T.);
#10427=FACE_OUTER_BOUND('',#15694,.T.);
#10428=FACE_OUTER_BOUND('',#15695,.T.);
#10429=FACE_OUTER_BOUND('',#15696,.T.);
#10430=FACE_OUTER_BOUND('',#15697,.T.);
#10431=FACE_OUTER_BOUND('',#15698,.T.);
#10432=FACE_OUTER_BOUND('',#15699,.T.);
#10433=FACE_OUTER_BOUND('',#15700,.T.);
#10434=FACE_OUTER_BOUND('',#15701,.T.);
#10435=FACE_OUTER_BOUND('',#15702,.T.);
#10436=FACE_OUTER_BOUND('',#15703,.T.);
#10437=FACE_OUTER_BOUND('',#15704,.T.);
#10438=FACE_OUTER_BOUND('',#15705,.T.);
#10439=FACE_OUTER_BOUND('',#15706,.T.);
#10440=FACE_OUTER_BOUND('',#15707,.T.);
#10441=FACE_OUTER_BOUND('',#15708,.T.);
#10442=FACE_OUTER_BOUND('',#15709,.T.);
#10443=FACE_OUTER_BOUND('',#15710,.T.);
#10444=FACE_OUTER_BOUND('',#15711,.T.);
#10445=FACE_OUTER_BOUND('',#15712,.T.);
#10446=FACE_OUTER_BOUND('',#15713,.T.);
#10447=FACE_OUTER_BOUND('',#15714,.T.);
#10448=FACE_OUTER_BOUND('',#15715,.T.);
#10449=FACE_OUTER_BOUND('',#15716,.T.);
#10450=FACE_OUTER_BOUND('',#15717,.T.);
#10451=FACE_OUTER_BOUND('',#15718,.T.);
#10452=FACE_OUTER_BOUND('',#15719,.T.);
#10453=FACE_OUTER_BOUND('',#15720,.T.);
#10454=FACE_OUTER_BOUND('',#15721,.T.);
#10455=FACE_OUTER_BOUND('',#15722,.T.);
#10456=FACE_OUTER_BOUND('',#15723,.T.);
#10457=FACE_OUTER_BOUND('',#15724,.T.);
#10458=FACE_OUTER_BOUND('',#15725,.T.);
#10459=FACE_OUTER_BOUND('',#15726,.T.);
#10460=FACE_OUTER_BOUND('',#15727,.T.);
#10461=FACE_OUTER_BOUND('',#15728,.T.);
#10462=FACE_OUTER_BOUND('',#15729,.T.);
#10463=FACE_OUTER_BOUND('',#15730,.T.);
#10464=FACE_OUTER_BOUND('',#15731,.T.);
#10465=FACE_OUTER_BOUND('',#15732,.T.);
#10466=FACE_OUTER_BOUND('',#15733,.T.);
#10467=FACE_OUTER_BOUND('',#15734,.T.);
#10468=FACE_OUTER_BOUND('',#15735,.T.);
#10469=FACE_OUTER_BOUND('',#15736,.T.);
#10470=FACE_OUTER_BOUND('',#15737,.T.);
#10471=FACE_OUTER_BOUND('',#15738,.T.);
#10472=FACE_OUTER_BOUND('',#15739,.T.);
#10473=FACE_OUTER_BOUND('',#15740,.T.);
#10474=FACE_OUTER_BOUND('',#15741,.T.);
#10475=FACE_OUTER_BOUND('',#15742,.T.);
#10476=FACE_OUTER_BOUND('',#15743,.T.);
#10477=FACE_OUTER_BOUND('',#15744,.T.);
#10478=FACE_OUTER_BOUND('',#15745,.T.);
#10479=FACE_OUTER_BOUND('',#15746,.T.);
#10480=FACE_OUTER_BOUND('',#15747,.T.);
#10481=FACE_OUTER_BOUND('',#15748,.T.);
#10482=FACE_OUTER_BOUND('',#15749,.T.);
#10483=FACE_OUTER_BOUND('',#15750,.T.);
#10484=FACE_OUTER_BOUND('',#15751,.T.);
#10485=FACE_OUTER_BOUND('',#15752,.T.);
#10486=FACE_OUTER_BOUND('',#15753,.T.);
#10487=FACE_OUTER_BOUND('',#15754,.T.);
#10488=FACE_OUTER_BOUND('',#15755,.T.);
#10489=FACE_OUTER_BOUND('',#15756,.T.);
#10490=FACE_OUTER_BOUND('',#15757,.T.);
#10491=FACE_OUTER_BOUND('',#15758,.T.);
#10492=FACE_OUTER_BOUND('',#15759,.T.);
#10493=FACE_OUTER_BOUND('',#15760,.T.);
#10494=FACE_OUTER_BOUND('',#15761,.T.);
#10495=FACE_OUTER_BOUND('',#15762,.T.);
#10496=FACE_OUTER_BOUND('',#15763,.T.);
#10497=FACE_OUTER_BOUND('',#15764,.T.);
#10498=FACE_OUTER_BOUND('',#15765,.T.);
#10499=FACE_OUTER_BOUND('',#15766,.T.);
#10500=FACE_OUTER_BOUND('',#15767,.T.);
#10501=FACE_OUTER_BOUND('',#15768,.T.);
#10502=FACE_OUTER_BOUND('',#15769,.T.);
#10503=FACE_OUTER_BOUND('',#15770,.T.);
#10504=FACE_OUTER_BOUND('',#15771,.T.);
#10505=FACE_OUTER_BOUND('',#15772,.T.);
#10506=FACE_OUTER_BOUND('',#15773,.T.);
#10507=FACE_OUTER_BOUND('',#15774,.T.);
#10508=FACE_OUTER_BOUND('',#15775,.T.);
#10509=FACE_OUTER_BOUND('',#15776,.T.);
#10510=FACE_OUTER_BOUND('',#15777,.T.);
#10511=FACE_OUTER_BOUND('',#15778,.T.);
#10512=FACE_OUTER_BOUND('',#15779,.T.);
#10513=FACE_OUTER_BOUND('',#15780,.T.);
#10514=FACE_OUTER_BOUND('',#15781,.T.);
#10515=FACE_OUTER_BOUND('',#15782,.T.);
#10516=FACE_OUTER_BOUND('',#15783,.T.);
#10517=FACE_OUTER_BOUND('',#15784,.T.);
#10518=FACE_OUTER_BOUND('',#15785,.T.);
#10519=FACE_OUTER_BOUND('',#15786,.T.);
#10520=FACE_OUTER_BOUND('',#15787,.T.);
#10521=FACE_OUTER_BOUND('',#15788,.T.);
#10522=FACE_OUTER_BOUND('',#15789,.T.);
#10523=FACE_OUTER_BOUND('',#15790,.T.);
#10524=FACE_OUTER_BOUND('',#15791,.T.);
#10525=FACE_OUTER_BOUND('',#15792,.T.);
#10526=FACE_OUTER_BOUND('',#15793,.T.);
#10527=FACE_OUTER_BOUND('',#15794,.T.);
#10528=FACE_OUTER_BOUND('',#15795,.T.);
#10529=FACE_OUTER_BOUND('',#15796,.T.);
#10530=FACE_OUTER_BOUND('',#15797,.T.);
#10531=FACE_OUTER_BOUND('',#15798,.T.);
#10532=FACE_OUTER_BOUND('',#15799,.T.);
#10533=FACE_OUTER_BOUND('',#15800,.T.);
#10534=FACE_OUTER_BOUND('',#15801,.T.);
#10535=FACE_OUTER_BOUND('',#15802,.T.);
#10536=FACE_OUTER_BOUND('',#15803,.T.);
#10537=FACE_OUTER_BOUND('',#15804,.T.);
#10538=FACE_OUTER_BOUND('',#15805,.T.);
#10539=FACE_OUTER_BOUND('',#15806,.T.);
#10540=FACE_OUTER_BOUND('',#15807,.T.);
#10541=FACE_OUTER_BOUND('',#15808,.T.);
#10542=FACE_OUTER_BOUND('',#15809,.T.);
#10543=FACE_OUTER_BOUND('',#15810,.T.);
#10544=FACE_OUTER_BOUND('',#15811,.T.);
#10545=FACE_OUTER_BOUND('',#15812,.T.);
#10546=FACE_OUTER_BOUND('',#15813,.T.);
#10547=FACE_OUTER_BOUND('',#15814,.T.);
#10548=FACE_OUTER_BOUND('',#15815,.T.);
#10549=FACE_OUTER_BOUND('',#15816,.T.);
#10550=FACE_OUTER_BOUND('',#15817,.T.);
#10551=FACE_OUTER_BOUND('',#15818,.T.);
#10552=FACE_OUTER_BOUND('',#15819,.T.);
#10553=FACE_OUTER_BOUND('',#15820,.T.);
#10554=FACE_OUTER_BOUND('',#15821,.T.);
#10555=FACE_OUTER_BOUND('',#15822,.T.);
#10556=FACE_OUTER_BOUND('',#15823,.T.);
#10557=FACE_OUTER_BOUND('',#15824,.T.);
#10558=FACE_OUTER_BOUND('',#15825,.T.);
#10559=FACE_OUTER_BOUND('',#15826,.T.);
#10560=FACE_OUTER_BOUND('',#15827,.T.);
#10561=FACE_OUTER_BOUND('',#15828,.T.);
#10562=FACE_OUTER_BOUND('',#15829,.T.);
#10563=FACE_OUTER_BOUND('',#15830,.T.);
#10564=FACE_OUTER_BOUND('',#15831,.T.);
#10565=FACE_OUTER_BOUND('',#15832,.T.);
#10566=FACE_OUTER_BOUND('',#15833,.T.);
#10567=FACE_OUTER_BOUND('',#15834,.T.);
#10568=FACE_OUTER_BOUND('',#15835,.T.);
#10569=FACE_OUTER_BOUND('',#15836,.T.);
#10570=FACE_OUTER_BOUND('',#15837,.T.);
#10571=FACE_OUTER_BOUND('',#15838,.T.);
#10572=FACE_OUTER_BOUND('',#15839,.T.);
#10573=FACE_OUTER_BOUND('',#15840,.T.);
#10574=FACE_OUTER_BOUND('',#15841,.T.);
#10575=FACE_OUTER_BOUND('',#15842,.T.);
#10576=FACE_OUTER_BOUND('',#15843,.T.);
#10577=FACE_OUTER_BOUND('',#15844,.T.);
#10578=FACE_OUTER_BOUND('',#15845,.T.);
#10579=FACE_OUTER_BOUND('',#15846,.T.);
#10580=FACE_OUTER_BOUND('',#15847,.T.);
#10581=FACE_OUTER_BOUND('',#15848,.T.);
#10582=FACE_OUTER_BOUND('',#15849,.T.);
#10583=FACE_OUTER_BOUND('',#15850,.T.);
#10584=FACE_OUTER_BOUND('',#15852,.T.);
#10585=FACE_OUTER_BOUND('',#15854,.T.);
#10586=FACE_OUTER_BOUND('',#15855,.T.);
#10587=FACE_OUTER_BOUND('',#15856,.T.);
#10588=FACE_OUTER_BOUND('',#15857,.T.);
#10589=FACE_OUTER_BOUND('',#15858,.T.);
#10590=FACE_OUTER_BOUND('',#15859,.T.);
#10591=FACE_OUTER_BOUND('',#15860,.T.);
#10592=FACE_OUTER_BOUND('',#15861,.T.);
#10593=FACE_OUTER_BOUND('',#15863,.T.);
#10594=FACE_OUTER_BOUND('',#15865,.T.);
#10595=FACE_OUTER_BOUND('',#15866,.T.);
#10596=FACE_OUTER_BOUND('',#15867,.T.);
#10597=FACE_OUTER_BOUND('',#15868,.T.);
#10598=FACE_OUTER_BOUND('',#15869,.T.);
#10599=FACE_OUTER_BOUND('',#15870,.T.);
#10600=FACE_OUTER_BOUND('',#15871,.T.);
#10601=FACE_OUTER_BOUND('',#15872,.T.);
#10602=FACE_OUTER_BOUND('',#15873,.T.);
#10603=FACE_OUTER_BOUND('',#15874,.T.);
#10604=FACE_OUTER_BOUND('',#15875,.T.);
#10605=FACE_OUTER_BOUND('',#15876,.T.);
#10606=FACE_OUTER_BOUND('',#15877,.T.);
#10607=FACE_OUTER_BOUND('',#15878,.T.);
#10608=FACE_OUTER_BOUND('',#15879,.T.);
#10609=FACE_OUTER_BOUND('',#15880,.T.);
#10610=FACE_OUTER_BOUND('',#15881,.T.);
#10611=FACE_OUTER_BOUND('',#15882,.T.);
#10612=FACE_OUTER_BOUND('',#15883,.T.);
#10613=FACE_OUTER_BOUND('',#15884,.T.);
#10614=FACE_OUTER_BOUND('',#15885,.T.);
#10615=FACE_OUTER_BOUND('',#15886,.T.);
#10616=FACE_OUTER_BOUND('',#15887,.T.);
#10617=FACE_OUTER_BOUND('',#15888,.T.);
#10618=FACE_OUTER_BOUND('',#15889,.T.);
#10619=FACE_OUTER_BOUND('',#15890,.T.);
#10620=FACE_OUTER_BOUND('',#15891,.T.);
#10621=FACE_OUTER_BOUND('',#15892,.T.);
#10622=FACE_OUTER_BOUND('',#15894,.T.);
#10623=FACE_OUTER_BOUND('',#15896,.T.);
#10624=FACE_OUTER_BOUND('',#15898,.T.);
#10625=FACE_OUTER_BOUND('',#15899,.T.);
#10626=FACE_OUTER_BOUND('',#15900,.T.);
#10627=FACE_OUTER_BOUND('',#15902,.T.);
#10628=FACE_OUTER_BOUND('',#15904,.T.);
#10629=FACE_OUTER_BOUND('',#15906,.T.);
#10630=FACE_OUTER_BOUND('',#15907,.T.);
#10631=FACE_OUTER_BOUND('',#15908,.T.);
#10632=FACE_OUTER_BOUND('',#15909,.T.);
#10633=FACE_OUTER_BOUND('',#15910,.T.);
#10634=FACE_OUTER_BOUND('',#15912,.T.);
#10635=FACE_OUTER_BOUND('',#15913,.T.);
#10636=FACE_OUTER_BOUND('',#15914,.T.);
#10637=FACE_OUTER_BOUND('',#15915,.T.);
#10638=FACE_OUTER_BOUND('',#15917,.T.);
#10639=FACE_OUTER_BOUND('',#15919,.T.);
#10640=FACE_OUTER_BOUND('',#15921,.T.);
#10641=FACE_OUTER_BOUND('',#15922,.T.);
#10642=FACE_OUTER_BOUND('',#15923,.T.);
#10643=FACE_OUTER_BOUND('',#15924,.T.);
#10644=FACE_OUTER_BOUND('',#15925,.T.);
#10645=FACE_OUTER_BOUND('',#15926,.T.);
#10646=FACE_OUTER_BOUND('',#15927,.T.);
#10647=FACE_OUTER_BOUND('',#15928,.T.);
#10648=EDGE_LOOP('',(#44646,#44647,#44648,#44649,#44650,#44651,#44652,#44653,
#44654,#44655,#44656,#44657,#44658,#44659,#44660,#44661,#44662,#44663,#44664,
#44665,#44666,#44667,#44668,#44669,#44670,#44671,#44672,#44673,#44674,#44675,
#44676,#44677,#44678,#44679,#44680,#44681,#44682,#44683,#44684,#44685,#44686,
#44687,#44688,#44689,#44690,#44691,#44692,#44693,#44694,#44695,#44696,#44697,
#44698,#44699,#44700,#44701,#44702,#44703,#44704,#44705,#44706,#44707,#44708,
#44709,#44710,#44711,#44712,#44713,#44714,#44715,#44716,#44717,#44718,#44719,
#44720,#44721,#44722,#44723,#44724,#44725,#44726,#44727,#44728,#44729,#44730,
#44731,#44732,#44733,#44734,#44735,#44736,#44737,#44738,#44739,#44740,#44741,
#44742,#44743,#44744,#44745,#44746,#44747,#44748,#44749,#44750,#44751,#44752,
#44753,#44754,#44755,#44756,#44757,#44758,#44759,#44760,#44761,#44762,#44763,
#44764,#44765,#44766,#44767,#44768,#44769,#44770,#44771,#44772,#44773,#44774,
#44775,#44776,#44777,#44778,#44779,#44780,#44781,#44782,#44783,#44784,#44785,
#44786,#44787,#44788,#44789,#44790,#44791,#44792,#44793,#44794,#44795,#44796,
#44797,#44798,#44799,#44800,#44801,#44802,#44803,#44804,#44805,#44806,#44807,
#44808,#44809,#44810,#44811,#44812,#44813,#44814,#44815,#44816,#44817,#44818,
#44819,#44820,#44821,#44822,#44823,#44824));
#10649=EDGE_LOOP('',(#44825,#44826,#44827,#44828));
#10650=EDGE_LOOP('',(#44829,#44830,#44831));
#10651=EDGE_LOOP('',(#44832,#44833,#44834,#44835));
#10652=EDGE_LOOP('',(#44836,#44837,#44838,#44839,#44840));
#10653=EDGE_LOOP('',(#44841,#44842,#44843,#44844,#44845));
#10654=EDGE_LOOP('',(#44846,#44847,#44848,#44849,#44850,#44851,#44852,#44853,
#44854,#44855,#44856,#44857,#44858,#44859,#44860,#44861,#44862,#44863,#44864,
#44865,#44866,#44867,#44868,#44869,#44870,#44871,#44872,#44873,#44874,#44875,
#44876,#44877,#44878,#44879,#44880,#44881,#44882,#44883,#44884,#44885,#44886,
#44887,#44888,#44889,#44890,#44891,#44892,#44893,#44894,#44895,#44896,#44897,
#44898,#44899,#44900,#44901,#44902,#44903,#44904,#44905,#44906,#44907,#44908,
#44909,#44910,#44911,#44912,#44913,#44914,#44915,#44916,#44917,#44918,#44919,
#44920,#44921,#44922,#44923,#44924,#44925,#44926,#44927,#44928,#44929,#44930,
#44931,#44932,#44933,#44934,#44935,#44936,#44937,#44938,#44939,#44940,#44941,
#44942,#44943,#44944,#44945,#44946,#44947,#44948,#44949,#44950,#44951,#44952,
#44953,#44954,#44955,#44956,#44957,#44958,#44959,#44960,#44961,#44962,#44963,
#44964,#44965,#44966,#44967,#44968,#44969,#44970,#44971,#44972,#44973,#44974,
#44975,#44976,#44977,#44978,#44979,#44980,#44981,#44982,#44983,#44984,#44985,
#44986,#44987,#44988,#44989,#44990,#44991,#44992,#44993,#44994,#44995,#44996,
#44997,#44998,#44999,#45000,#45001,#45002,#45003,#45004,#45005,#45006,#45007,
#45008,#45009,#45010,#45011,#45012,#45013,#45014,#45015,#45016,#45017,#45018,
#45019,#45020,#45021,#45022,#45023));
#10655=EDGE_LOOP('',(#45024,#45025,#45026,#45027));
#10656=EDGE_LOOP('',(#45028,#45029,#45030,#45031));
#10657=EDGE_LOOP('',(#45032,#45033,#45034,#45035,#45036));
#10658=EDGE_LOOP('',(#45037,#45038,#45039,#45040));
#10659=EDGE_LOOP('',(#45041,#45042,#45043,#45044));
#10660=EDGE_LOOP('',(#45045,#45046,#45047,#45048));
#10661=EDGE_LOOP('',(#45049,#45050,#45051,#45052));
#10662=EDGE_LOOP('',(#45053,#45054,#45055,#45056,#45057));
#10663=EDGE_LOOP('',(#45058,#45059,#45060));
#10664=EDGE_LOOP('',(#45061,#45062,#45063,#45064));
#10665=EDGE_LOOP('',(#45065,#45066,#45067,#45068));
#10666=EDGE_LOOP('',(#45069,#45070,#45071,#45072));
#10667=EDGE_LOOP('',(#45073,#45074,#45075,#45076));
#10668=EDGE_LOOP('',(#45077,#45078,#45079,#45080));
#10669=EDGE_LOOP('',(#45081,#45082,#45083,#45084));
#10670=EDGE_LOOP('',(#45085,#45086,#45087,#45088));
#10671=EDGE_LOOP('',(#45089,#45090,#45091,#45092));
#10672=EDGE_LOOP('',(#45093,#45094,#45095,#45096));
#10673=EDGE_LOOP('',(#45097,#45098,#45099,#45100));
#10674=EDGE_LOOP('',(#45101,#45102,#45103,#45104));
#10675=EDGE_LOOP('',(#45105,#45106,#45107,#45108));
#10676=EDGE_LOOP('',(#45109,#45110,#45111,#45112));
#10677=EDGE_LOOP('',(#45113,#45114,#45115,#45116));
#10678=EDGE_LOOP('',(#45117,#45118,#45119,#45120));
#10679=EDGE_LOOP('',(#45121,#45122,#45123,#45124));
#10680=EDGE_LOOP('',(#45125,#45126,#45127,#45128));
#10681=EDGE_LOOP('',(#45129,#45130,#45131,#45132));
#10682=EDGE_LOOP('',(#45133,#45134,#45135,#45136));
#10683=EDGE_LOOP('',(#45137,#45138,#45139,#45140));
#10684=EDGE_LOOP('',(#45141,#45142,#45143,#45144));
#10685=EDGE_LOOP('',(#45145,#45146,#45147,#45148));
#10686=EDGE_LOOP('',(#45149,#45150,#45151,#45152));
#10687=EDGE_LOOP('',(#45153,#45154,#45155,#45156));
#10688=EDGE_LOOP('',(#45157,#45158,#45159,#45160));
#10689=EDGE_LOOP('',(#45161,#45162,#45163,#45164));
#10690=EDGE_LOOP('',(#45165,#45166,#45167,#45168));
#10691=EDGE_LOOP('',(#45169,#45170,#45171,#45172));
#10692=EDGE_LOOP('',(#45173,#45174,#45175,#45176));
#10693=EDGE_LOOP('',(#45177,#45178,#45179,#45180));
#10694=EDGE_LOOP('',(#45181,#45182,#45183,#45184));
#10695=EDGE_LOOP('',(#45185,#45186,#45187,#45188));
#10696=EDGE_LOOP('',(#45189,#45190,#45191,#45192));
#10697=EDGE_LOOP('',(#45193,#45194,#45195,#45196));
#10698=EDGE_LOOP('',(#45197,#45198,#45199,#45200));
#10699=EDGE_LOOP('',(#45201,#45202,#45203,#45204));
#10700=EDGE_LOOP('',(#45205,#45206,#45207,#45208));
#10701=EDGE_LOOP('',(#45209,#45210,#45211,#45212));
#10702=EDGE_LOOP('',(#45213,#45214,#45215,#45216));
#10703=EDGE_LOOP('',(#45217,#45218,#45219,#45220));
#10704=EDGE_LOOP('',(#45221,#45222,#45223,#45224));
#10705=EDGE_LOOP('',(#45225,#45226,#45227,#45228));
#10706=EDGE_LOOP('',(#45229,#45230,#45231,#45232));
#10707=EDGE_LOOP('',(#45233,#45234,#45235,#45236));
#10708=EDGE_LOOP('',(#45237,#45238,#45239,#45240));
#10709=EDGE_LOOP('',(#45241,#45242,#45243,#45244));
#10710=EDGE_LOOP('',(#45245,#45246,#45247,#45248));
#10711=EDGE_LOOP('',(#45249,#45250,#45251,#45252));
#10712=EDGE_LOOP('',(#45253,#45254,#45255,#45256));
#10713=EDGE_LOOP('',(#45257,#45258,#45259,#45260));
#10714=EDGE_LOOP('',(#45261,#45262,#45263,#45264));
#10715=EDGE_LOOP('',(#45265,#45266,#45267,#45268));
#10716=EDGE_LOOP('',(#45269,#45270,#45271,#45272));
#10717=EDGE_LOOP('',(#45273,#45274,#45275,#45276));
#10718=EDGE_LOOP('',(#45277,#45278,#45279,#45280));
#10719=EDGE_LOOP('',(#45281,#45282,#45283,#45284));
#10720=EDGE_LOOP('',(#45285,#45286,#45287,#45288));
#10721=EDGE_LOOP('',(#45289,#45290,#45291,#45292));
#10722=EDGE_LOOP('',(#45293,#45294,#45295,#45296));
#10723=EDGE_LOOP('',(#45297,#45298,#45299,#45300));
#10724=EDGE_LOOP('',(#45301,#45302,#45303,#45304));
#10725=EDGE_LOOP('',(#45305,#45306,#45307,#45308));
#10726=EDGE_LOOP('',(#45309,#45310,#45311,#45312));
#10727=EDGE_LOOP('',(#45313,#45314,#45315,#45316));
#10728=EDGE_LOOP('',(#45317,#45318,#45319,#45320));
#10729=EDGE_LOOP('',(#45321,#45322,#45323,#45324));
#10730=EDGE_LOOP('',(#45325,#45326,#45327,#45328));
#10731=EDGE_LOOP('',(#45329,#45330,#45331,#45332));
#10732=EDGE_LOOP('',(#45333,#45334,#45335,#45336));
#10733=EDGE_LOOP('',(#45337,#45338,#45339,#45340));
#10734=EDGE_LOOP('',(#45341,#45342,#45343,#45344));
#10735=EDGE_LOOP('',(#45345,#45346,#45347,#45348));
#10736=EDGE_LOOP('',(#45349,#45350,#45351,#45352));
#10737=EDGE_LOOP('',(#45353,#45354,#45355,#45356));
#10738=EDGE_LOOP('',(#45357,#45358,#45359,#45360));
#10739=EDGE_LOOP('',(#45361,#45362,#45363,#45364));
#10740=EDGE_LOOP('',(#45365,#45366,#45367,#45368));
#10741=EDGE_LOOP('',(#45369,#45370,#45371,#45372));
#10742=EDGE_LOOP('',(#45373,#45374,#45375,#45376));
#10743=EDGE_LOOP('',(#45377,#45378,#45379,#45380));
#10744=EDGE_LOOP('',(#45381,#45382,#45383,#45384));
#10745=EDGE_LOOP('',(#45385,#45386,#45387,#45388));
#10746=EDGE_LOOP('',(#45389,#45390,#45391,#45392));
#10747=EDGE_LOOP('',(#45393,#45394,#45395,#45396));
#10748=EDGE_LOOP('',(#45397,#45398,#45399,#45400));
#10749=EDGE_LOOP('',(#45401,#45402,#45403,#45404));
#10750=EDGE_LOOP('',(#45405,#45406,#45407,#45408));
#10751=EDGE_LOOP('',(#45409,#45410,#45411,#45412));
#10752=EDGE_LOOP('',(#45413,#45414,#45415,#45416));
#10753=EDGE_LOOP('',(#45417,#45418,#45419,#45420));
#10754=EDGE_LOOP('',(#45421,#45422,#45423,#45424));
#10755=EDGE_LOOP('',(#45425,#45426,#45427,#45428));
#10756=EDGE_LOOP('',(#45429,#45430,#45431,#45432));
#10757=EDGE_LOOP('',(#45433,#45434,#45435,#45436));
#10758=EDGE_LOOP('',(#45437,#45438,#45439,#45440));
#10759=EDGE_LOOP('',(#45441,#45442,#45443,#45444));
#10760=EDGE_LOOP('',(#45445,#45446,#45447,#45448));
#10761=EDGE_LOOP('',(#45449,#45450,#45451,#45452));
#10762=EDGE_LOOP('',(#45453,#45454,#45455,#45456));
#10763=EDGE_LOOP('',(#45457,#45458,#45459,#45460));
#10764=EDGE_LOOP('',(#45461,#45462,#45463,#45464));
#10765=EDGE_LOOP('',(#45465,#45466,#45467,#45468));
#10766=EDGE_LOOP('',(#45469,#45470,#45471,#45472));
#10767=EDGE_LOOP('',(#45473,#45474,#45475,#45476));
#10768=EDGE_LOOP('',(#45477,#45478,#45479,#45480));
#10769=EDGE_LOOP('',(#45481,#45482,#45483,#45484));
#10770=EDGE_LOOP('',(#45485,#45486,#45487,#45488));
#10771=EDGE_LOOP('',(#45489,#45490,#45491,#45492));
#10772=EDGE_LOOP('',(#45493,#45494,#45495,#45496));
#10773=EDGE_LOOP('',(#45497,#45498,#45499,#45500));
#10774=EDGE_LOOP('',(#45501,#45502,#45503,#45504));
#10775=EDGE_LOOP('',(#45505,#45506,#45507,#45508));
#10776=EDGE_LOOP('',(#45509,#45510,#45511,#45512));
#10777=EDGE_LOOP('',(#45513,#45514,#45515,#45516));
#10778=EDGE_LOOP('',(#45517,#45518,#45519,#45520));
#10779=EDGE_LOOP('',(#45521,#45522,#45523,#45524));
#10780=EDGE_LOOP('',(#45525,#45526,#45527,#45528));
#10781=EDGE_LOOP('',(#45529,#45530,#45531,#45532));
#10782=EDGE_LOOP('',(#45533,#45534,#45535,#45536));
#10783=EDGE_LOOP('',(#45537,#45538,#45539,#45540));
#10784=EDGE_LOOP('',(#45541,#45542,#45543,#45544));
#10785=EDGE_LOOP('',(#45545,#45546,#45547,#45548));
#10786=EDGE_LOOP('',(#45549,#45550,#45551,#45552));
#10787=EDGE_LOOP('',(#45553,#45554,#45555,#45556));
#10788=EDGE_LOOP('',(#45557,#45558,#45559,#45560));
#10789=EDGE_LOOP('',(#45561,#45562,#45563,#45564));
#10790=EDGE_LOOP('',(#45565,#45566,#45567,#45568));
#10791=EDGE_LOOP('',(#45569,#45570,#45571,#45572));
#10792=EDGE_LOOP('',(#45573,#45574,#45575,#45576));
#10793=EDGE_LOOP('',(#45577,#45578,#45579,#45580));
#10794=EDGE_LOOP('',(#45581,#45582,#45583,#45584));
#10795=EDGE_LOOP('',(#45585,#45586,#45587,#45588));
#10796=EDGE_LOOP('',(#45589,#45590,#45591,#45592));
#10797=EDGE_LOOP('',(#45593,#45594,#45595,#45596));
#10798=EDGE_LOOP('',(#45597,#45598,#45599,#45600));
#10799=EDGE_LOOP('',(#45601,#45602,#45603,#45604));
#10800=EDGE_LOOP('',(#45605,#45606,#45607,#45608));
#10801=EDGE_LOOP('',(#45609,#45610,#45611,#45612));
#10802=EDGE_LOOP('',(#45613,#45614,#45615,#45616));
#10803=EDGE_LOOP('',(#45617,#45618,#45619,#45620));
#10804=EDGE_LOOP('',(#45621,#45622,#45623,#45624));
#10805=EDGE_LOOP('',(#45625,#45626,#45627,#45628));
#10806=EDGE_LOOP('',(#45629,#45630,#45631,#45632));
#10807=EDGE_LOOP('',(#45633,#45634,#45635,#45636));
#10808=EDGE_LOOP('',(#45637,#45638,#45639,#45640));
#10809=EDGE_LOOP('',(#45641,#45642,#45643,#45644));
#10810=EDGE_LOOP('',(#45645,#45646,#45647,#45648));
#10811=EDGE_LOOP('',(#45649,#45650,#45651,#45652));
#10812=EDGE_LOOP('',(#45653,#45654,#45655,#45656));
#10813=EDGE_LOOP('',(#45657,#45658,#45659,#45660));
#10814=EDGE_LOOP('',(#45661,#45662,#45663,#45664));
#10815=EDGE_LOOP('',(#45665,#45666,#45667,#45668));
#10816=EDGE_LOOP('',(#45669,#45670,#45671,#45672));
#10817=EDGE_LOOP('',(#45673,#45674,#45675,#45676));
#10818=EDGE_LOOP('',(#45677,#45678,#45679,#45680));
#10819=EDGE_LOOP('',(#45681,#45682,#45683,#45684));
#10820=EDGE_LOOP('',(#45685,#45686,#45687,#45688));
#10821=EDGE_LOOP('',(#45689,#45690,#45691,#45692));
#10822=EDGE_LOOP('',(#45693,#45694,#45695,#45696));
#10823=EDGE_LOOP('',(#45697,#45698,#45699,#45700));
#10824=EDGE_LOOP('',(#45701,#45702,#45703,#45704));
#10825=EDGE_LOOP('',(#45705,#45706,#45707,#45708));
#10826=EDGE_LOOP('',(#45709,#45710,#45711,#45712));
#10827=EDGE_LOOP('',(#45713,#45714,#45715,#45716));
#10828=EDGE_LOOP('',(#45717,#45718,#45719,#45720));
#10829=EDGE_LOOP('',(#45721,#45722,#45723,#45724));
#10830=EDGE_LOOP('',(#45725,#45726,#45727,#45728));
#10831=EDGE_LOOP('',(#45729,#45730,#45731,#45732));
#10832=EDGE_LOOP('',(#45733,#45734,#45735,#45736));
#10833=EDGE_LOOP('',(#45737,#45738,#45739,#45740));
#10834=EDGE_LOOP('',(#45741,#45742,#45743,#45744));
#10835=EDGE_LOOP('',(#45745,#45746,#45747,#45748));
#10836=EDGE_LOOP('',(#45749,#45750,#45751,#45752));
#10837=EDGE_LOOP('',(#45753,#45754,#45755,#45756));
#10838=EDGE_LOOP('',(#45757,#45758,#45759,#45760));
#10839=EDGE_LOOP('',(#45761,#45762,#45763,#45764));
#10840=EDGE_LOOP('',(#45765,#45766,#45767,#45768));
#10841=EDGE_LOOP('',(#45769,#45770,#45771,#45772));
#10842=EDGE_LOOP('',(#45773,#45774,#45775,#45776));
#10843=EDGE_LOOP('',(#45777,#45778,#45779,#45780));
#10844=EDGE_LOOP('',(#45781,#45782,#45783,#45784));
#10845=EDGE_LOOP('',(#45785,#45786,#45787,#45788));
#10846=EDGE_LOOP('',(#45789,#45790,#45791,#45792));
#10847=EDGE_LOOP('',(#45793,#45794,#45795,#45796));
#10848=EDGE_LOOP('',(#45797,#45798,#45799,#45800));
#10849=EDGE_LOOP('',(#45801,#45802,#45803,#45804));
#10850=EDGE_LOOP('',(#45805,#45806,#45807,#45808));
#10851=EDGE_LOOP('',(#45809,#45810,#45811,#45812));
#10852=EDGE_LOOP('',(#45813,#45814,#45815,#45816));
#10853=EDGE_LOOP('',(#45817,#45818,#45819,#45820));
#10854=EDGE_LOOP('',(#45821,#45822,#45823,#45824));
#10855=EDGE_LOOP('',(#45825,#45826,#45827,#45828));
#10856=EDGE_LOOP('',(#45829,#45830,#45831,#45832));
#10857=EDGE_LOOP('',(#45833,#45834,#45835,#45836));
#10858=EDGE_LOOP('',(#45837,#45838,#45839,#45840));
#10859=EDGE_LOOP('',(#45841,#45842,#45843,#45844));
#10860=EDGE_LOOP('',(#45845,#45846,#45847,#45848));
#10861=EDGE_LOOP('',(#45849,#45850,#45851,#45852));
#10862=EDGE_LOOP('',(#45853,#45854,#45855,#45856));
#10863=EDGE_LOOP('',(#45857,#45858,#45859,#45860));
#10864=EDGE_LOOP('',(#45861,#45862,#45863,#45864));
#10865=EDGE_LOOP('',(#45865,#45866,#45867,#45868));
#10866=EDGE_LOOP('',(#45869,#45870,#45871,#45872));
#10867=EDGE_LOOP('',(#45873,#45874,#45875,#45876));
#10868=EDGE_LOOP('',(#45877,#45878,#45879,#45880));
#10869=EDGE_LOOP('',(#45881,#45882,#45883,#45884));
#10870=EDGE_LOOP('',(#45885,#45886,#45887,#45888));
#10871=EDGE_LOOP('',(#45889,#45890,#45891,#45892));
#10872=EDGE_LOOP('',(#45893,#45894,#45895,#45896));
#10873=EDGE_LOOP('',(#45897,#45898,#45899,#45900));
#10874=EDGE_LOOP('',(#45901,#45902,#45903,#45904));
#10875=EDGE_LOOP('',(#45905,#45906,#45907,#45908));
#10876=EDGE_LOOP('',(#45909,#45910,#45911,#45912));
#10877=EDGE_LOOP('',(#45913,#45914,#45915,#45916));
#10878=EDGE_LOOP('',(#45917,#45918,#45919,#45920));
#10879=EDGE_LOOP('',(#45921,#45922,#45923,#45924));
#10880=EDGE_LOOP('',(#45925,#45926,#45927,#45928));
#10881=EDGE_LOOP('',(#45929,#45930,#45931,#45932));
#10882=EDGE_LOOP('',(#45933,#45934,#45935,#45936));
#10883=EDGE_LOOP('',(#45937,#45938,#45939,#45940));
#10884=EDGE_LOOP('',(#45941,#45942,#45943,#45944));
#10885=EDGE_LOOP('',(#45945,#45946,#45947,#45948));
#10886=EDGE_LOOP('',(#45949,#45950,#45951,#45952));
#10887=EDGE_LOOP('',(#45953,#45954,#45955,#45956));
#10888=EDGE_LOOP('',(#45957,#45958,#45959,#45960));
#10889=EDGE_LOOP('',(#45961,#45962,#45963,#45964));
#10890=EDGE_LOOP('',(#45965,#45966,#45967,#45968));
#10891=EDGE_LOOP('',(#45969,#45970,#45971,#45972));
#10892=EDGE_LOOP('',(#45973,#45974,#45975,#45976));
#10893=EDGE_LOOP('',(#45977,#45978,#45979,#45980));
#10894=EDGE_LOOP('',(#45981,#45982,#45983,#45984));
#10895=EDGE_LOOP('',(#45985,#45986,#45987,#45988));
#10896=EDGE_LOOP('',(#45989,#45990,#45991,#45992));
#10897=EDGE_LOOP('',(#45993,#45994,#45995,#45996));
#10898=EDGE_LOOP('',(#45997,#45998,#45999,#46000));
#10899=EDGE_LOOP('',(#46001,#46002,#46003,#46004));
#10900=EDGE_LOOP('',(#46005,#46006,#46007,#46008));
#10901=EDGE_LOOP('',(#46009,#46010,#46011,#46012));
#10902=EDGE_LOOP('',(#46013,#46014,#46015,#46016));
#10903=EDGE_LOOP('',(#46017,#46018,#46019,#46020));
#10904=EDGE_LOOP('',(#46021,#46022,#46023,#46024));
#10905=EDGE_LOOP('',(#46025,#46026,#46027,#46028));
#10906=EDGE_LOOP('',(#46029,#46030,#46031,#46032));
#10907=EDGE_LOOP('',(#46033,#46034,#46035,#46036));
#10908=EDGE_LOOP('',(#46037,#46038,#46039,#46040));
#10909=EDGE_LOOP('',(#46041,#46042,#46043,#46044));
#10910=EDGE_LOOP('',(#46045,#46046,#46047,#46048));
#10911=EDGE_LOOP('',(#46049,#46050,#46051,#46052));
#10912=EDGE_LOOP('',(#46053,#46054,#46055,#46056));
#10913=EDGE_LOOP('',(#46057,#46058,#46059,#46060));
#10914=EDGE_LOOP('',(#46061,#46062,#46063,#46064));
#10915=EDGE_LOOP('',(#46065,#46066,#46067,#46068));
#10916=EDGE_LOOP('',(#46069,#46070,#46071,#46072));
#10917=EDGE_LOOP('',(#46073,#46074,#46075,#46076));
#10918=EDGE_LOOP('',(#46077,#46078,#46079,#46080));
#10919=EDGE_LOOP('',(#46081,#46082,#46083,#46084));
#10920=EDGE_LOOP('',(#46085,#46086,#46087,#46088));
#10921=EDGE_LOOP('',(#46089,#46090,#46091,#46092));
#10922=EDGE_LOOP('',(#46093,#46094,#46095,#46096));
#10923=EDGE_LOOP('',(#46097,#46098,#46099,#46100));
#10924=EDGE_LOOP('',(#46101,#46102,#46103,#46104));
#10925=EDGE_LOOP('',(#46105,#46106,#46107,#46108));
#10926=EDGE_LOOP('',(#46109,#46110,#46111,#46112));
#10927=EDGE_LOOP('',(#46113,#46114,#46115,#46116));
#10928=EDGE_LOOP('',(#46117,#46118,#46119,#46120));
#10929=EDGE_LOOP('',(#46121,#46122,#46123,#46124));
#10930=EDGE_LOOP('',(#46125,#46126,#46127,#46128));
#10931=EDGE_LOOP('',(#46129,#46130,#46131,#46132));
#10932=EDGE_LOOP('',(#46133,#46134,#46135,#46136));
#10933=EDGE_LOOP('',(#46137,#46138,#46139,#46140));
#10934=EDGE_LOOP('',(#46141,#46142,#46143,#46144));
#10935=EDGE_LOOP('',(#46145,#46146,#46147,#46148));
#10936=EDGE_LOOP('',(#46149,#46150,#46151,#46152));
#10937=EDGE_LOOP('',(#46153,#46154,#46155,#46156));
#10938=EDGE_LOOP('',(#46157,#46158,#46159,#46160));
#10939=EDGE_LOOP('',(#46161,#46162,#46163,#46164));
#10940=EDGE_LOOP('',(#46165,#46166,#46167,#46168));
#10941=EDGE_LOOP('',(#46169,#46170,#46171,#46172));
#10942=EDGE_LOOP('',(#46173,#46174,#46175,#46176));
#10943=EDGE_LOOP('',(#46177,#46178,#46179,#46180));
#10944=EDGE_LOOP('',(#46181,#46182,#46183,#46184));
#10945=EDGE_LOOP('',(#46185,#46186,#46187,#46188));
#10946=EDGE_LOOP('',(#46189,#46190,#46191,#46192));
#10947=EDGE_LOOP('',(#46193,#46194,#46195,#46196));
#10948=EDGE_LOOP('',(#46197,#46198,#46199,#46200));
#10949=EDGE_LOOP('',(#46201,#46202,#46203,#46204));
#10950=EDGE_LOOP('',(#46205,#46206,#46207,#46208));
#10951=EDGE_LOOP('',(#46209,#46210,#46211,#46212));
#10952=EDGE_LOOP('',(#46213,#46214,#46215,#46216));
#10953=EDGE_LOOP('',(#46217,#46218,#46219,#46220));
#10954=EDGE_LOOP('',(#46221,#46222,#46223,#46224));
#10955=EDGE_LOOP('',(#46225,#46226,#46227,#46228));
#10956=EDGE_LOOP('',(#46229,#46230,#46231,#46232));
#10957=EDGE_LOOP('',(#46233,#46234,#46235,#46236));
#10958=EDGE_LOOP('',(#46237,#46238,#46239,#46240));
#10959=EDGE_LOOP('',(#46241,#46242,#46243,#46244));
#10960=EDGE_LOOP('',(#46245,#46246,#46247,#46248));
#10961=EDGE_LOOP('',(#46249,#46250,#46251,#46252));
#10962=EDGE_LOOP('',(#46253,#46254,#46255,#46256));
#10963=EDGE_LOOP('',(#46257,#46258,#46259,#46260));
#10964=EDGE_LOOP('',(#46261,#46262,#46263,#46264));
#10965=EDGE_LOOP('',(#46265,#46266,#46267,#46268));
#10966=EDGE_LOOP('',(#46269,#46270,#46271,#46272));
#10967=EDGE_LOOP('',(#46273,#46274,#46275,#46276));
#10968=EDGE_LOOP('',(#46277,#46278,#46279,#46280));
#10969=EDGE_LOOP('',(#46281,#46282,#46283,#46284));
#10970=EDGE_LOOP('',(#46285,#46286,#46287,#46288));
#10971=EDGE_LOOP('',(#46289,#46290,#46291,#46292));
#10972=EDGE_LOOP('',(#46293,#46294,#46295,#46296));
#10973=EDGE_LOOP('',(#46297,#46298,#46299,#46300));
#10974=EDGE_LOOP('',(#46301,#46302,#46303,#46304));
#10975=EDGE_LOOP('',(#46305,#46306,#46307,#46308));
#10976=EDGE_LOOP('',(#46309,#46310,#46311,#46312));
#10977=EDGE_LOOP('',(#46313,#46314,#46315,#46316));
#10978=EDGE_LOOP('',(#46317,#46318,#46319,#46320));
#10979=EDGE_LOOP('',(#46321,#46322,#46323,#46324));
#10980=EDGE_LOOP('',(#46325,#46326,#46327,#46328));
#10981=EDGE_LOOP('',(#46329,#46330,#46331,#46332));
#10982=EDGE_LOOP('',(#46333,#46334,#46335,#46336));
#10983=EDGE_LOOP('',(#46337,#46338,#46339,#46340));
#10984=EDGE_LOOP('',(#46341,#46342,#46343,#46344));
#10985=EDGE_LOOP('',(#46345,#46346,#46347,#46348));
#10986=EDGE_LOOP('',(#46349,#46350,#46351,#46352));
#10987=EDGE_LOOP('',(#46353,#46354,#46355,#46356));
#10988=EDGE_LOOP('',(#46357,#46358,#46359,#46360));
#10989=EDGE_LOOP('',(#46361,#46362,#46363,#46364));
#10990=EDGE_LOOP('',(#46365,#46366,#46367,#46368));
#10991=EDGE_LOOP('',(#46369,#46370,#46371,#46372));
#10992=EDGE_LOOP('',(#46373,#46374,#46375,#46376));
#10993=EDGE_LOOP('',(#46377,#46378,#46379,#46380));
#10994=EDGE_LOOP('',(#46381,#46382,#46383,#46384));
#10995=EDGE_LOOP('',(#46385,#46386,#46387,#46388));
#10996=EDGE_LOOP('',(#46389,#46390,#46391,#46392));
#10997=EDGE_LOOP('',(#46393,#46394,#46395,#46396));
#10998=EDGE_LOOP('',(#46397,#46398,#46399,#46400));
#10999=EDGE_LOOP('',(#46401,#46402,#46403,#46404));
#11000=EDGE_LOOP('',(#46405,#46406,#46407,#46408));
#11001=EDGE_LOOP('',(#46409,#46410,#46411,#46412));
#11002=EDGE_LOOP('',(#46413,#46414,#46415,#46416));
#11003=EDGE_LOOP('',(#46417,#46418,#46419,#46420));
#11004=EDGE_LOOP('',(#46421,#46422,#46423,#46424));
#11005=EDGE_LOOP('',(#46425,#46426,#46427,#46428));
#11006=EDGE_LOOP('',(#46429,#46430,#46431,#46432));
#11007=EDGE_LOOP('',(#46433,#46434,#46435,#46436));
#11008=EDGE_LOOP('',(#46437,#46438,#46439,#46440));
#11009=EDGE_LOOP('',(#46441,#46442,#46443,#46444));
#11010=EDGE_LOOP('',(#46445,#46446,#46447,#46448));
#11011=EDGE_LOOP('',(#46449,#46450,#46451,#46452));
#11012=EDGE_LOOP('',(#46453,#46454,#46455,#46456));
#11013=EDGE_LOOP('',(#46457,#46458,#46459,#46460));
#11014=EDGE_LOOP('',(#46461,#46462,#46463,#46464));
#11015=EDGE_LOOP('',(#46465,#46466,#46467,#46468));
#11016=EDGE_LOOP('',(#46469,#46470,#46471,#46472));
#11017=EDGE_LOOP('',(#46473,#46474,#46475,#46476));
#11018=EDGE_LOOP('',(#46477,#46478,#46479,#46480));
#11019=EDGE_LOOP('',(#46481,#46482,#46483,#46484));
#11020=EDGE_LOOP('',(#46485,#46486,#46487,#46488));
#11021=EDGE_LOOP('',(#46489,#46490,#46491,#46492));
#11022=EDGE_LOOP('',(#46493,#46494,#46495,#46496));
#11023=EDGE_LOOP('',(#46497,#46498,#46499,#46500));
#11024=EDGE_LOOP('',(#46501,#46502,#46503,#46504));
#11025=EDGE_LOOP('',(#46505,#46506,#46507,#46508));
#11026=EDGE_LOOP('',(#46509,#46510,#46511,#46512));
#11027=EDGE_LOOP('',(#46513,#46514,#46515,#46516));
#11028=EDGE_LOOP('',(#46517,#46518,#46519,#46520));
#11029=EDGE_LOOP('',(#46521,#46522,#46523,#46524));
#11030=EDGE_LOOP('',(#46525,#46526,#46527,#46528));
#11031=EDGE_LOOP('',(#46529,#46530,#46531,#46532));
#11032=EDGE_LOOP('',(#46533,#46534,#46535,#46536));
#11033=EDGE_LOOP('',(#46537,#46538,#46539,#46540));
#11034=EDGE_LOOP('',(#46541,#46542,#46543,#46544));
#11035=EDGE_LOOP('',(#46545,#46546,#46547,#46548));
#11036=EDGE_LOOP('',(#46549,#46550,#46551,#46552));
#11037=EDGE_LOOP('',(#46553,#46554,#46555,#46556));
#11038=EDGE_LOOP('',(#46557,#46558,#46559,#46560));
#11039=EDGE_LOOP('',(#46561,#46562,#46563,#46564));
#11040=EDGE_LOOP('',(#46565,#46566,#46567,#46568));
#11041=EDGE_LOOP('',(#46569,#46570,#46571,#46572));
#11042=EDGE_LOOP('',(#46573,#46574,#46575,#46576));
#11043=EDGE_LOOP('',(#46577,#46578,#46579,#46580));
#11044=EDGE_LOOP('',(#46581,#46582,#46583,#46584));
#11045=EDGE_LOOP('',(#46585,#46586,#46587,#46588));
#11046=EDGE_LOOP('',(#46589,#46590,#46591,#46592));
#11047=EDGE_LOOP('',(#46593,#46594,#46595,#46596));
#11048=EDGE_LOOP('',(#46597,#46598,#46599,#46600));
#11049=EDGE_LOOP('',(#46601,#46602,#46603,#46604));
#11050=EDGE_LOOP('',(#46605,#46606,#46607,#46608));
#11051=EDGE_LOOP('',(#46609,#46610,#46611,#46612));
#11052=EDGE_LOOP('',(#46613,#46614,#46615,#46616));
#11053=EDGE_LOOP('',(#46617,#46618,#46619,#46620));
#11054=EDGE_LOOP('',(#46621,#46622,#46623,#46624));
#11055=EDGE_LOOP('',(#46625,#46626,#46627,#46628));
#11056=EDGE_LOOP('',(#46629,#46630,#46631,#46632));
#11057=EDGE_LOOP('',(#46633,#46634,#46635,#46636));
#11058=EDGE_LOOP('',(#46637,#46638,#46639,#46640));
#11059=EDGE_LOOP('',(#46641,#46642,#46643,#46644));
#11060=EDGE_LOOP('',(#46645,#46646,#46647,#46648));
#11061=EDGE_LOOP('',(#46649,#46650,#46651,#46652));
#11062=EDGE_LOOP('',(#46653,#46654,#46655,#46656));
#11063=EDGE_LOOP('',(#46657,#46658,#46659,#46660));
#11064=EDGE_LOOP('',(#46661,#46662,#46663,#46664));
#11065=EDGE_LOOP('',(#46665,#46666,#46667,#46668));
#11066=EDGE_LOOP('',(#46669,#46670,#46671,#46672));
#11067=EDGE_LOOP('',(#46673,#46674,#46675,#46676));
#11068=EDGE_LOOP('',(#46677,#46678,#46679,#46680));
#11069=EDGE_LOOP('',(#46681,#46682,#46683,#46684));
#11070=EDGE_LOOP('',(#46685,#46686,#46687,#46688));
#11071=EDGE_LOOP('',(#46689,#46690,#46691,#46692));
#11072=EDGE_LOOP('',(#46693,#46694,#46695,#46696));
#11073=EDGE_LOOP('',(#46697,#46698,#46699,#46700));
#11074=EDGE_LOOP('',(#46701,#46702,#46703,#46704));
#11075=EDGE_LOOP('',(#46705,#46706,#46707,#46708));
#11076=EDGE_LOOP('',(#46709,#46710,#46711,#46712));
#11077=EDGE_LOOP('',(#46713,#46714,#46715,#46716));
#11078=EDGE_LOOP('',(#46717,#46718,#46719,#46720));
#11079=EDGE_LOOP('',(#46721,#46722,#46723,#46724));
#11080=EDGE_LOOP('',(#46725,#46726,#46727,#46728));
#11081=EDGE_LOOP('',(#46729,#46730,#46731,#46732));
#11082=EDGE_LOOP('',(#46733,#46734,#46735,#46736));
#11083=EDGE_LOOP('',(#46737,#46738,#46739,#46740));
#11084=EDGE_LOOP('',(#46741,#46742,#46743,#46744));
#11085=EDGE_LOOP('',(#46745,#46746,#46747,#46748));
#11086=EDGE_LOOP('',(#46749,#46750,#46751,#46752));
#11087=EDGE_LOOP('',(#46753,#46754,#46755,#46756));
#11088=EDGE_LOOP('',(#46757,#46758,#46759,#46760));
#11089=EDGE_LOOP('',(#46761,#46762,#46763,#46764));
#11090=EDGE_LOOP('',(#46765,#46766,#46767,#46768));
#11091=EDGE_LOOP('',(#46769,#46770,#46771,#46772));
#11092=EDGE_LOOP('',(#46773,#46774,#46775,#46776));
#11093=EDGE_LOOP('',(#46777,#46778,#46779,#46780));
#11094=EDGE_LOOP('',(#46781,#46782,#46783,#46784));
#11095=EDGE_LOOP('',(#46785,#46786,#46787,#46788));
#11096=EDGE_LOOP('',(#46789,#46790,#46791,#46792));
#11097=EDGE_LOOP('',(#46793,#46794,#46795,#46796));
#11098=EDGE_LOOP('',(#46797,#46798,#46799,#46800));
#11099=EDGE_LOOP('',(#46801,#46802,#46803,#46804));
#11100=EDGE_LOOP('',(#46805,#46806,#46807,#46808));
#11101=EDGE_LOOP('',(#46809,#46810,#46811,#46812));
#11102=EDGE_LOOP('',(#46813,#46814,#46815,#46816));
#11103=EDGE_LOOP('',(#46817,#46818,#46819,#46820));
#11104=EDGE_LOOP('',(#46821,#46822,#46823,#46824));
#11105=EDGE_LOOP('',(#46825,#46826,#46827,#46828));
#11106=EDGE_LOOP('',(#46829,#46830,#46831,#46832));
#11107=EDGE_LOOP('',(#46833,#46834,#46835,#46836));
#11108=EDGE_LOOP('',(#46837,#46838,#46839,#46840));
#11109=EDGE_LOOP('',(#46841,#46842,#46843,#46844));
#11110=EDGE_LOOP('',(#46845,#46846,#46847,#46848));
#11111=EDGE_LOOP('',(#46849,#46850,#46851,#46852));
#11112=EDGE_LOOP('',(#46853,#46854,#46855,#46856));
#11113=EDGE_LOOP('',(#46857,#46858,#46859,#46860));
#11114=EDGE_LOOP('',(#46861,#46862,#46863,#46864));
#11115=EDGE_LOOP('',(#46865,#46866,#46867,#46868));
#11116=EDGE_LOOP('',(#46869,#46870,#46871,#46872));
#11117=EDGE_LOOP('',(#46873,#46874,#46875,#46876));
#11118=EDGE_LOOP('',(#46877,#46878,#46879,#46880));
#11119=EDGE_LOOP('',(#46881,#46882,#46883,#46884));
#11120=EDGE_LOOP('',(#46885,#46886,#46887,#46888));
#11121=EDGE_LOOP('',(#46889,#46890,#46891,#46892));
#11122=EDGE_LOOP('',(#46893,#46894,#46895,#46896));
#11123=EDGE_LOOP('',(#46897,#46898,#46899,#46900));
#11124=EDGE_LOOP('',(#46901,#46902,#46903,#46904));
#11125=EDGE_LOOP('',(#46905,#46906,#46907,#46908));
#11126=EDGE_LOOP('',(#46909,#46910,#46911,#46912));
#11127=EDGE_LOOP('',(#46913,#46914,#46915,#46916));
#11128=EDGE_LOOP('',(#46917,#46918,#46919,#46920));
#11129=EDGE_LOOP('',(#46921,#46922,#46923,#46924));
#11130=EDGE_LOOP('',(#46925,#46926,#46927,#46928));
#11131=EDGE_LOOP('',(#46929,#46930,#46931,#46932));
#11132=EDGE_LOOP('',(#46933,#46934,#46935,#46936));
#11133=EDGE_LOOP('',(#46937,#46938,#46939,#46940));
#11134=EDGE_LOOP('',(#46941,#46942,#46943,#46944));
#11135=EDGE_LOOP('',(#46945,#46946,#46947,#46948));
#11136=EDGE_LOOP('',(#46949,#46950,#46951,#46952));
#11137=EDGE_LOOP('',(#46953,#46954,#46955,#46956));
#11138=EDGE_LOOP('',(#46957,#46958,#46959,#46960));
#11139=EDGE_LOOP('',(#46961,#46962,#46963,#46964));
#11140=EDGE_LOOP('',(#46965,#46966,#46967,#46968));
#11141=EDGE_LOOP('',(#46969,#46970,#46971,#46972));
#11142=EDGE_LOOP('',(#46973,#46974,#46975,#46976));
#11143=EDGE_LOOP('',(#46977,#46978,#46979,#46980));
#11144=EDGE_LOOP('',(#46981,#46982,#46983,#46984));
#11145=EDGE_LOOP('',(#46985,#46986,#46987,#46988));
#11146=EDGE_LOOP('',(#46989,#46990,#46991,#46992));
#11147=EDGE_LOOP('',(#46993,#46994,#46995,#46996));
#11148=EDGE_LOOP('',(#46997,#46998,#46999,#47000));
#11149=EDGE_LOOP('',(#47001,#47002,#47003,#47004));
#11150=EDGE_LOOP('',(#47005,#47006,#47007,#47008));
#11151=EDGE_LOOP('',(#47009,#47010,#47011,#47012));
#11152=EDGE_LOOP('',(#47013,#47014,#47015,#47016));
#11153=EDGE_LOOP('',(#47017,#47018,#47019,#47020));
#11154=EDGE_LOOP('',(#47021,#47022,#47023,#47024));
#11155=EDGE_LOOP('',(#47025,#47026,#47027,#47028));
#11156=EDGE_LOOP('',(#47029,#47030,#47031,#47032));
#11157=EDGE_LOOP('',(#47033,#47034,#47035,#47036));
#11158=EDGE_LOOP('',(#47037,#47038,#47039,#47040));
#11159=EDGE_LOOP('',(#47041,#47042,#47043,#47044));
#11160=EDGE_LOOP('',(#47045,#47046,#47047,#47048));
#11161=EDGE_LOOP('',(#47049,#47050,#47051,#47052));
#11162=EDGE_LOOP('',(#47053,#47054,#47055,#47056));
#11163=EDGE_LOOP('',(#47057,#47058,#47059,#47060));
#11164=EDGE_LOOP('',(#47061,#47062,#47063,#47064));
#11165=EDGE_LOOP('',(#47065,#47066,#47067,#47068));
#11166=EDGE_LOOP('',(#47069,#47070,#47071,#47072));
#11167=EDGE_LOOP('',(#47073,#47074,#47075,#47076));
#11168=EDGE_LOOP('',(#47077,#47078,#47079,#47080));
#11169=EDGE_LOOP('',(#47081,#47082,#47083,#47084));
#11170=EDGE_LOOP('',(#47085,#47086,#47087,#47088));
#11171=EDGE_LOOP('',(#47089,#47090,#47091,#47092));
#11172=EDGE_LOOP('',(#47093,#47094,#47095,#47096));
#11173=EDGE_LOOP('',(#47097,#47098,#47099,#47100));
#11174=EDGE_LOOP('',(#47101,#47102,#47103,#47104));
#11175=EDGE_LOOP('',(#47105,#47106,#47107,#47108));
#11176=EDGE_LOOP('',(#47109,#47110,#47111,#47112));
#11177=EDGE_LOOP('',(#47113,#47114,#47115,#47116));
#11178=EDGE_LOOP('',(#47117,#47118,#47119,#47120));
#11179=EDGE_LOOP('',(#47121,#47122,#47123,#47124));
#11180=EDGE_LOOP('',(#47125,#47126,#47127,#47128));
#11181=EDGE_LOOP('',(#47129,#47130,#47131,#47132));
#11182=EDGE_LOOP('',(#47133,#47134,#47135,#47136));
#11183=EDGE_LOOP('',(#47137,#47138,#47139,#47140));
#11184=EDGE_LOOP('',(#47141,#47142,#47143,#47144));
#11185=EDGE_LOOP('',(#47145,#47146,#47147,#47148));
#11186=EDGE_LOOP('',(#47149,#47150,#47151,#47152));
#11187=EDGE_LOOP('',(#47153,#47154,#47155,#47156));
#11188=EDGE_LOOP('',(#47157,#47158,#47159,#47160));
#11189=EDGE_LOOP('',(#47161,#47162,#47163,#47164));
#11190=EDGE_LOOP('',(#47165,#47166,#47167,#47168));
#11191=EDGE_LOOP('',(#47169,#47170,#47171,#47172));
#11192=EDGE_LOOP('',(#47173,#47174,#47175,#47176));
#11193=EDGE_LOOP('',(#47177,#47178,#47179,#47180));
#11194=EDGE_LOOP('',(#47181,#47182,#47183,#47184));
#11195=EDGE_LOOP('',(#47185,#47186,#47187,#47188));
#11196=EDGE_LOOP('',(#47189,#47190,#47191,#47192));
#11197=EDGE_LOOP('',(#47193,#47194,#47195,#47196));
#11198=EDGE_LOOP('',(#47197,#47198,#47199,#47200));
#11199=EDGE_LOOP('',(#47201,#47202,#47203,#47204));
#11200=EDGE_LOOP('',(#47205,#47206,#47207,#47208));
#11201=EDGE_LOOP('',(#47209,#47210,#47211,#47212));
#11202=EDGE_LOOP('',(#47213,#47214,#47215,#47216));
#11203=EDGE_LOOP('',(#47217,#47218,#47219,#47220));
#11204=EDGE_LOOP('',(#47221,#47222,#47223,#47224));
#11205=EDGE_LOOP('',(#47225,#47226,#47227,#47228));
#11206=EDGE_LOOP('',(#47229,#47230,#47231,#47232));
#11207=EDGE_LOOP('',(#47233,#47234,#47235,#47236));
#11208=EDGE_LOOP('',(#47237,#47238,#47239,#47240));
#11209=EDGE_LOOP('',(#47241,#47242,#47243,#47244));
#11210=EDGE_LOOP('',(#47245,#47246,#47247,#47248));
#11211=EDGE_LOOP('',(#47249,#47250,#47251,#47252));
#11212=EDGE_LOOP('',(#47253,#47254,#47255,#47256));
#11213=EDGE_LOOP('',(#47257,#47258,#47259,#47260));
#11214=EDGE_LOOP('',(#47261,#47262,#47263,#47264));
#11215=EDGE_LOOP('',(#47265,#47266,#47267,#47268));
#11216=EDGE_LOOP('',(#47269,#47270,#47271,#47272));
#11217=EDGE_LOOP('',(#47273,#47274,#47275,#47276));
#11218=EDGE_LOOP('',(#47277,#47278,#47279,#47280));
#11219=EDGE_LOOP('',(#47281,#47282,#47283,#47284));
#11220=EDGE_LOOP('',(#47285,#47286,#47287,#47288));
#11221=EDGE_LOOP('',(#47289,#47290,#47291,#47292));
#11222=EDGE_LOOP('',(#47293,#47294,#47295,#47296));
#11223=EDGE_LOOP('',(#47297,#47298,#47299,#47300));
#11224=EDGE_LOOP('',(#47301,#47302,#47303,#47304));
#11225=EDGE_LOOP('',(#47305,#47306,#47307,#47308));
#11226=EDGE_LOOP('',(#47309,#47310,#47311,#47312));
#11227=EDGE_LOOP('',(#47313,#47314,#47315,#47316));
#11228=EDGE_LOOP('',(#47317,#47318,#47319,#47320));
#11229=EDGE_LOOP('',(#47321,#47322,#47323,#47324));
#11230=EDGE_LOOP('',(#47325,#47326,#47327,#47328));
#11231=EDGE_LOOP('',(#47329,#47330,#47331,#47332));
#11232=EDGE_LOOP('',(#47333,#47334,#47335,#47336));
#11233=EDGE_LOOP('',(#47337,#47338,#47339,#47340));
#11234=EDGE_LOOP('',(#47341,#47342,#47343,#47344));
#11235=EDGE_LOOP('',(#47345,#47346,#47347,#47348));
#11236=EDGE_LOOP('',(#47349,#47350,#47351,#47352));
#11237=EDGE_LOOP('',(#47353,#47354,#47355,#47356));
#11238=EDGE_LOOP('',(#47357,#47358,#47359,#47360));
#11239=EDGE_LOOP('',(#47361,#47362,#47363,#47364));
#11240=EDGE_LOOP('',(#47365,#47366,#47367,#47368));
#11241=EDGE_LOOP('',(#47369,#47370,#47371,#47372));
#11242=EDGE_LOOP('',(#47373,#47374,#47375,#47376));
#11243=EDGE_LOOP('',(#47377,#47378,#47379,#47380));
#11244=EDGE_LOOP('',(#47381,#47382,#47383,#47384));
#11245=EDGE_LOOP('',(#47385,#47386,#47387,#47388));
#11246=EDGE_LOOP('',(#47389,#47390,#47391,#47392));
#11247=EDGE_LOOP('',(#47393,#47394,#47395,#47396));
#11248=EDGE_LOOP('',(#47397,#47398,#47399,#47400));
#11249=EDGE_LOOP('',(#47401,#47402,#47403,#47404));
#11250=EDGE_LOOP('',(#47405,#47406,#47407,#47408));
#11251=EDGE_LOOP('',(#47409,#47410,#47411,#47412));
#11252=EDGE_LOOP('',(#47413,#47414,#47415,#47416));
#11253=EDGE_LOOP('',(#47417,#47418,#47419,#47420));
#11254=EDGE_LOOP('',(#47421,#47422,#47423,#47424));
#11255=EDGE_LOOP('',(#47425,#47426,#47427,#47428));
#11256=EDGE_LOOP('',(#47429,#47430,#47431,#47432));
#11257=EDGE_LOOP('',(#47433,#47434,#47435,#47436));
#11258=EDGE_LOOP('',(#47437,#47438,#47439,#47440));
#11259=EDGE_LOOP('',(#47441,#47442,#47443,#47444));
#11260=EDGE_LOOP('',(#47445,#47446,#47447,#47448));
#11261=EDGE_LOOP('',(#47449,#47450,#47451,#47452));
#11262=EDGE_LOOP('',(#47453,#47454,#47455,#47456));
#11263=EDGE_LOOP('',(#47457,#47458,#47459,#47460));
#11264=EDGE_LOOP('',(#47461,#47462,#47463,#47464));
#11265=EDGE_LOOP('',(#47465,#47466,#47467,#47468));
#11266=EDGE_LOOP('',(#47469,#47470,#47471,#47472));
#11267=EDGE_LOOP('',(#47473,#47474,#47475,#47476));
#11268=EDGE_LOOP('',(#47477,#47478,#47479,#47480));
#11269=EDGE_LOOP('',(#47481,#47482,#47483,#47484));
#11270=EDGE_LOOP('',(#47485,#47486,#47487,#47488));
#11271=EDGE_LOOP('',(#47489,#47490,#47491,#47492));
#11272=EDGE_LOOP('',(#47493,#47494,#47495,#47496));
#11273=EDGE_LOOP('',(#47497,#47498,#47499,#47500));
#11274=EDGE_LOOP('',(#47501,#47502,#47503,#47504));
#11275=EDGE_LOOP('',(#47505,#47506,#47507,#47508));
#11276=EDGE_LOOP('',(#47509,#47510,#47511,#47512));
#11277=EDGE_LOOP('',(#47513,#47514,#47515,#47516));
#11278=EDGE_LOOP('',(#47517,#47518,#47519,#47520));
#11279=EDGE_LOOP('',(#47521,#47522,#47523,#47524));
#11280=EDGE_LOOP('',(#47525,#47526,#47527,#47528));
#11281=EDGE_LOOP('',(#47529,#47530,#47531,#47532));
#11282=EDGE_LOOP('',(#47533,#47534,#47535,#47536));
#11283=EDGE_LOOP('',(#47537,#47538,#47539,#47540));
#11284=EDGE_LOOP('',(#47541,#47542,#47543,#47544));
#11285=EDGE_LOOP('',(#47545,#47546,#47547,#47548));
#11286=EDGE_LOOP('',(#47549,#47550,#47551,#47552));
#11287=EDGE_LOOP('',(#47553,#47554,#47555,#47556));
#11288=EDGE_LOOP('',(#47557,#47558,#47559,#47560));
#11289=EDGE_LOOP('',(#47561,#47562,#47563,#47564));
#11290=EDGE_LOOP('',(#47565,#47566,#47567,#47568));
#11291=EDGE_LOOP('',(#47569,#47570,#47571,#47572));
#11292=EDGE_LOOP('',(#47573,#47574,#47575,#47576));
#11293=EDGE_LOOP('',(#47577,#47578,#47579,#47580));
#11294=EDGE_LOOP('',(#47581,#47582,#47583,#47584));
#11295=EDGE_LOOP('',(#47585,#47586,#47587,#47588));
#11296=EDGE_LOOP('',(#47589,#47590,#47591,#47592));
#11297=EDGE_LOOP('',(#47593,#47594,#47595,#47596));
#11298=EDGE_LOOP('',(#47597,#47598,#47599,#47600));
#11299=EDGE_LOOP('',(#47601,#47602,#47603,#47604));
#11300=EDGE_LOOP('',(#47605,#47606,#47607,#47608));
#11301=EDGE_LOOP('',(#47609,#47610,#47611,#47612));
#11302=EDGE_LOOP('',(#47613,#47614,#47615,#47616));
#11303=EDGE_LOOP('',(#47617,#47618,#47619,#47620));
#11304=EDGE_LOOP('',(#47621,#47622,#47623,#47624));
#11305=EDGE_LOOP('',(#47625,#47626,#47627,#47628));
#11306=EDGE_LOOP('',(#47629,#47630,#47631,#47632));
#11307=EDGE_LOOP('',(#47633,#47634,#47635,#47636));
#11308=EDGE_LOOP('',(#47637,#47638,#47639,#47640));
#11309=EDGE_LOOP('',(#47641,#47642,#47643,#47644));
#11310=EDGE_LOOP('',(#47645,#47646,#47647,#47648));
#11311=EDGE_LOOP('',(#47649,#47650,#47651,#47652));
#11312=EDGE_LOOP('',(#47653,#47654,#47655,#47656));
#11313=EDGE_LOOP('',(#47657,#47658,#47659,#47660));
#11314=EDGE_LOOP('',(#47661,#47662,#47663,#47664));
#11315=EDGE_LOOP('',(#47665,#47666,#47667,#47668));
#11316=EDGE_LOOP('',(#47669,#47670,#47671,#47672));
#11317=EDGE_LOOP('',(#47673,#47674,#47675,#47676));
#11318=EDGE_LOOP('',(#47677,#47678,#47679,#47680));
#11319=EDGE_LOOP('',(#47681,#47682,#47683,#47684));
#11320=EDGE_LOOP('',(#47685,#47686,#47687,#47688));
#11321=EDGE_LOOP('',(#47689,#47690,#47691,#47692));
#11322=EDGE_LOOP('',(#47693,#47694,#47695,#47696));
#11323=EDGE_LOOP('',(#47697,#47698,#47699,#47700));
#11324=EDGE_LOOP('',(#47701,#47702,#47703,#47704));
#11325=EDGE_LOOP('',(#47705,#47706,#47707,#47708));
#11326=EDGE_LOOP('',(#47709,#47710,#47711,#47712));
#11327=EDGE_LOOP('',(#47713,#47714,#47715,#47716));
#11328=EDGE_LOOP('',(#47717,#47718,#47719,#47720));
#11329=EDGE_LOOP('',(#47721,#47722,#47723,#47724));
#11330=EDGE_LOOP('',(#47725,#47726,#47727,#47728));
#11331=EDGE_LOOP('',(#47729,#47730,#47731,#47732));
#11332=EDGE_LOOP('',(#47733,#47734,#47735,#47736));
#11333=EDGE_LOOP('',(#47737,#47738,#47739,#47740));
#11334=EDGE_LOOP('',(#47741,#47742,#47743,#47744));
#11335=EDGE_LOOP('',(#47745,#47746,#47747,#47748));
#11336=EDGE_LOOP('',(#47749,#47750,#47751,#47752));
#11337=EDGE_LOOP('',(#47753,#47754,#47755,#47756));
#11338=EDGE_LOOP('',(#47757,#47758,#47759,#47760));
#11339=EDGE_LOOP('',(#47761,#47762,#47763,#47764));
#11340=EDGE_LOOP('',(#47765,#47766,#47767,#47768));
#11341=EDGE_LOOP('',(#47769,#47770,#47771,#47772));
#11342=EDGE_LOOP('',(#47773,#47774,#47775,#47776));
#11343=EDGE_LOOP('',(#47777,#47778,#47779,#47780));
#11344=EDGE_LOOP('',(#47781,#47782,#47783,#47784));
#11345=EDGE_LOOP('',(#47785,#47786,#47787,#47788));
#11346=EDGE_LOOP('',(#47789,#47790,#47791,#47792));
#11347=EDGE_LOOP('',(#47793,#47794,#47795,#47796));
#11348=EDGE_LOOP('',(#47797,#47798,#47799,#47800));
#11349=EDGE_LOOP('',(#47801,#47802,#47803,#47804));
#11350=EDGE_LOOP('',(#47805,#47806,#47807,#47808));
#11351=EDGE_LOOP('',(#47809,#47810,#47811,#47812));
#11352=EDGE_LOOP('',(#47813,#47814,#47815,#47816));
#11353=EDGE_LOOP('',(#47817,#47818,#47819,#47820));
#11354=EDGE_LOOP('',(#47821,#47822,#47823,#47824));
#11355=EDGE_LOOP('',(#47825,#47826,#47827,#47828));
#11356=EDGE_LOOP('',(#47829,#47830,#47831,#47832));
#11357=EDGE_LOOP('',(#47833,#47834,#47835,#47836));
#11358=EDGE_LOOP('',(#47837,#47838,#47839,#47840));
#11359=EDGE_LOOP('',(#47841,#47842,#47843,#47844));
#11360=EDGE_LOOP('',(#47845,#47846,#47847,#47848));
#11361=EDGE_LOOP('',(#47849,#47850,#47851,#47852));
#11362=EDGE_LOOP('',(#47853,#47854,#47855,#47856));
#11363=EDGE_LOOP('',(#47857,#47858,#47859,#47860));
#11364=EDGE_LOOP('',(#47861,#47862,#47863,#47864));
#11365=EDGE_LOOP('',(#47865,#47866,#47867,#47868));
#11366=EDGE_LOOP('',(#47869,#47870,#47871,#47872));
#11367=EDGE_LOOP('',(#47873,#47874,#47875,#47876));
#11368=EDGE_LOOP('',(#47877,#47878,#47879,#47880));
#11369=EDGE_LOOP('',(#47881,#47882,#47883,#47884));
#11370=EDGE_LOOP('',(#47885,#47886,#47887,#47888));
#11371=EDGE_LOOP('',(#47889,#47890,#47891,#47892));
#11372=EDGE_LOOP('',(#47893,#47894,#47895,#47896));
#11373=EDGE_LOOP('',(#47897,#47898,#47899,#47900));
#11374=EDGE_LOOP('',(#47901,#47902,#47903,#47904));
#11375=EDGE_LOOP('',(#47905,#47906,#47907,#47908));
#11376=EDGE_LOOP('',(#47909,#47910,#47911,#47912));
#11377=EDGE_LOOP('',(#47913,#47914,#47915,#47916));
#11378=EDGE_LOOP('',(#47917,#47918,#47919,#47920));
#11379=EDGE_LOOP('',(#47921,#47922,#47923,#47924));
#11380=EDGE_LOOP('',(#47925,#47926,#47927,#47928));
#11381=EDGE_LOOP('',(#47929,#47930,#47931,#47932));
#11382=EDGE_LOOP('',(#47933,#47934,#47935,#47936));
#11383=EDGE_LOOP('',(#47937,#47938,#47939,#47940));
#11384=EDGE_LOOP('',(#47941,#47942,#47943,#47944));
#11385=EDGE_LOOP('',(#47945,#47946,#47947,#47948));
#11386=EDGE_LOOP('',(#47949,#47950,#47951,#47952));
#11387=EDGE_LOOP('',(#47953,#47954,#47955,#47956));
#11388=EDGE_LOOP('',(#47957,#47958,#47959,#47960));
#11389=EDGE_LOOP('',(#47961,#47962,#47963,#47964));
#11390=EDGE_LOOP('',(#47965,#47966,#47967,#47968));
#11391=EDGE_LOOP('',(#47969,#47970,#47971,#47972));
#11392=EDGE_LOOP('',(#47973,#47974,#47975,#47976));
#11393=EDGE_LOOP('',(#47977,#47978,#47979,#47980));
#11394=EDGE_LOOP('',(#47981,#47982,#47983,#47984));
#11395=EDGE_LOOP('',(#47985,#47986,#47987,#47988));
#11396=EDGE_LOOP('',(#47989,#47990,#47991,#47992));
#11397=EDGE_LOOP('',(#47993,#47994,#47995,#47996));
#11398=EDGE_LOOP('',(#47997,#47998,#47999,#48000));
#11399=EDGE_LOOP('',(#48001,#48002,#48003,#48004));
#11400=EDGE_LOOP('',(#48005,#48006,#48007,#48008));
#11401=EDGE_LOOP('',(#48009,#48010,#48011,#48012));
#11402=EDGE_LOOP('',(#48013,#48014,#48015,#48016));
#11403=EDGE_LOOP('',(#48017,#48018,#48019,#48020));
#11404=EDGE_LOOP('',(#48021,#48022,#48023,#48024));
#11405=EDGE_LOOP('',(#48025,#48026,#48027,#48028));
#11406=EDGE_LOOP('',(#48029,#48030,#48031,#48032));
#11407=EDGE_LOOP('',(#48033,#48034,#48035,#48036));
#11408=EDGE_LOOP('',(#48037,#48038,#48039,#48040));
#11409=EDGE_LOOP('',(#48041,#48042,#48043,#48044));
#11410=EDGE_LOOP('',(#48045,#48046,#48047,#48048));
#11411=EDGE_LOOP('',(#48049,#48050,#48051,#48052));
#11412=EDGE_LOOP('',(#48053,#48054,#48055,#48056));
#11413=EDGE_LOOP('',(#48057,#48058,#48059,#48060));
#11414=EDGE_LOOP('',(#48061,#48062,#48063,#48064));
#11415=EDGE_LOOP('',(#48065,#48066,#48067,#48068));
#11416=EDGE_LOOP('',(#48069,#48070,#48071,#48072));
#11417=EDGE_LOOP('',(#48073,#48074,#48075,#48076));
#11418=EDGE_LOOP('',(#48077,#48078,#48079,#48080));
#11419=EDGE_LOOP('',(#48081,#48082,#48083,#48084));
#11420=EDGE_LOOP('',(#48085,#48086,#48087,#48088));
#11421=EDGE_LOOP('',(#48089,#48090,#48091,#48092));
#11422=EDGE_LOOP('',(#48093,#48094,#48095,#48096));
#11423=EDGE_LOOP('',(#48097,#48098,#48099,#48100));
#11424=EDGE_LOOP('',(#48101,#48102,#48103,#48104));
#11425=EDGE_LOOP('',(#48105,#48106,#48107,#48108));
#11426=EDGE_LOOP('',(#48109,#48110,#48111,#48112));
#11427=EDGE_LOOP('',(#48113,#48114,#48115,#48116));
#11428=EDGE_LOOP('',(#48117,#48118,#48119,#48120));
#11429=EDGE_LOOP('',(#48121,#48122,#48123,#48124));
#11430=EDGE_LOOP('',(#48125,#48126,#48127,#48128));
#11431=EDGE_LOOP('',(#48129,#48130,#48131,#48132));
#11432=EDGE_LOOP('',(#48133,#48134,#48135,#48136));
#11433=EDGE_LOOP('',(#48137,#48138,#48139,#48140));
#11434=EDGE_LOOP('',(#48141,#48142,#48143,#48144));
#11435=EDGE_LOOP('',(#48145,#48146,#48147,#48148));
#11436=EDGE_LOOP('',(#48149,#48150,#48151,#48152));
#11437=EDGE_LOOP('',(#48153,#48154,#48155,#48156));
#11438=EDGE_LOOP('',(#48157,#48158,#48159,#48160));
#11439=EDGE_LOOP('',(#48161,#48162,#48163,#48164));
#11440=EDGE_LOOP('',(#48165,#48166,#48167,#48168));
#11441=EDGE_LOOP('',(#48169,#48170,#48171,#48172));
#11442=EDGE_LOOP('',(#48173,#48174,#48175,#48176));
#11443=EDGE_LOOP('',(#48177,#48178,#48179,#48180));
#11444=EDGE_LOOP('',(#48181,#48182,#48183,#48184));
#11445=EDGE_LOOP('',(#48185,#48186,#48187,#48188));
#11446=EDGE_LOOP('',(#48189,#48190,#48191,#48192));
#11447=EDGE_LOOP('',(#48193,#48194,#48195,#48196));
#11448=EDGE_LOOP('',(#48197,#48198,#48199,#48200));
#11449=EDGE_LOOP('',(#48201,#48202,#48203,#48204));
#11450=EDGE_LOOP('',(#48205,#48206,#48207,#48208));
#11451=EDGE_LOOP('',(#48209,#48210,#48211,#48212));
#11452=EDGE_LOOP('',(#48213,#48214,#48215,#48216));
#11453=EDGE_LOOP('',(#48217,#48218,#48219,#48220));
#11454=EDGE_LOOP('',(#48221,#48222,#48223,#48224));
#11455=EDGE_LOOP('',(#48225,#48226,#48227,#48228));
#11456=EDGE_LOOP('',(#48229,#48230,#48231,#48232));
#11457=EDGE_LOOP('',(#48233,#48234,#48235,#48236));
#11458=EDGE_LOOP('',(#48237,#48238,#48239,#48240));
#11459=EDGE_LOOP('',(#48241,#48242,#48243,#48244));
#11460=EDGE_LOOP('',(#48245,#48246,#48247,#48248));
#11461=EDGE_LOOP('',(#48249,#48250,#48251,#48252));
#11462=EDGE_LOOP('',(#48253,#48254,#48255,#48256));
#11463=EDGE_LOOP('',(#48257,#48258,#48259,#48260));
#11464=EDGE_LOOP('',(#48261,#48262,#48263,#48264));
#11465=EDGE_LOOP('',(#48265,#48266,#48267,#48268));
#11466=EDGE_LOOP('',(#48269,#48270,#48271,#48272));
#11467=EDGE_LOOP('',(#48273,#48274,#48275,#48276));
#11468=EDGE_LOOP('',(#48277,#48278,#48279,#48280));
#11469=EDGE_LOOP('',(#48281,#48282,#48283,#48284));
#11470=EDGE_LOOP('',(#48285,#48286,#48287,#48288));
#11471=EDGE_LOOP('',(#48289,#48290,#48291,#48292));
#11472=EDGE_LOOP('',(#48293,#48294,#48295,#48296));
#11473=EDGE_LOOP('',(#48297,#48298,#48299,#48300));
#11474=EDGE_LOOP('',(#48301,#48302,#48303,#48304));
#11475=EDGE_LOOP('',(#48305,#48306,#48307,#48308));
#11476=EDGE_LOOP('',(#48309,#48310,#48311,#48312));
#11477=EDGE_LOOP('',(#48313,#48314,#48315,#48316));
#11478=EDGE_LOOP('',(#48317,#48318,#48319,#48320));
#11479=EDGE_LOOP('',(#48321,#48322,#48323,#48324));
#11480=EDGE_LOOP('',(#48325,#48326,#48327,#48328));
#11481=EDGE_LOOP('',(#48329,#48330,#48331,#48332));
#11482=EDGE_LOOP('',(#48333,#48334,#48335,#48336));
#11483=EDGE_LOOP('',(#48337,#48338,#48339,#48340));
#11484=EDGE_LOOP('',(#48341,#48342,#48343,#48344));
#11485=EDGE_LOOP('',(#48345,#48346,#48347,#48348));
#11486=EDGE_LOOP('',(#48349,#48350,#48351,#48352));
#11487=EDGE_LOOP('',(#48353,#48354,#48355,#48356));
#11488=EDGE_LOOP('',(#48357,#48358,#48359,#48360));
#11489=EDGE_LOOP('',(#48361,#48362,#48363,#48364));
#11490=EDGE_LOOP('',(#48365,#48366,#48367,#48368));
#11491=EDGE_LOOP('',(#48369,#48370,#48371,#48372));
#11492=EDGE_LOOP('',(#48373,#48374,#48375,#48376));
#11493=EDGE_LOOP('',(#48377,#48378,#48379,#48380));
#11494=EDGE_LOOP('',(#48381,#48382,#48383,#48384));
#11495=EDGE_LOOP('',(#48385,#48386,#48387,#48388));
#11496=EDGE_LOOP('',(#48389,#48390,#48391,#48392));
#11497=EDGE_LOOP('',(#48393,#48394,#48395,#48396));
#11498=EDGE_LOOP('',(#48397,#48398,#48399,#48400));
#11499=EDGE_LOOP('',(#48401,#48402,#48403,#48404));
#11500=EDGE_LOOP('',(#48405,#48406,#48407,#48408));
#11501=EDGE_LOOP('',(#48409,#48410,#48411,#48412));
#11502=EDGE_LOOP('',(#48413,#48414,#48415,#48416));
#11503=EDGE_LOOP('',(#48417,#48418,#48419,#48420));
#11504=EDGE_LOOP('',(#48421,#48422,#48423,#48424));
#11505=EDGE_LOOP('',(#48425,#48426,#48427,#48428));
#11506=EDGE_LOOP('',(#48429,#48430,#48431,#48432));
#11507=EDGE_LOOP('',(#48433,#48434,#48435,#48436));
#11508=EDGE_LOOP('',(#48437,#48438,#48439,#48440));
#11509=EDGE_LOOP('',(#48441,#48442,#48443,#48444));
#11510=EDGE_LOOP('',(#48445,#48446,#48447,#48448));
#11511=EDGE_LOOP('',(#48449,#48450,#48451,#48452));
#11512=EDGE_LOOP('',(#48453,#48454,#48455,#48456));
#11513=EDGE_LOOP('',(#48457,#48458,#48459,#48460));
#11514=EDGE_LOOP('',(#48461,#48462,#48463,#48464));
#11515=EDGE_LOOP('',(#48465,#48466,#48467,#48468));
#11516=EDGE_LOOP('',(#48469,#48470,#48471,#48472));
#11517=EDGE_LOOP('',(#48473,#48474,#48475,#48476));
#11518=EDGE_LOOP('',(#48477,#48478,#48479,#48480));
#11519=EDGE_LOOP('',(#48481,#48482,#48483,#48484));
#11520=EDGE_LOOP('',(#48485,#48486,#48487,#48488));
#11521=EDGE_LOOP('',(#48489,#48490,#48491,#48492));
#11522=EDGE_LOOP('',(#48493,#48494,#48495,#48496));
#11523=EDGE_LOOP('',(#48497,#48498,#48499,#48500));
#11524=EDGE_LOOP('',(#48501,#48502,#48503,#48504));
#11525=EDGE_LOOP('',(#48505,#48506,#48507,#48508));
#11526=EDGE_LOOP('',(#48509,#48510,#48511,#48512));
#11527=EDGE_LOOP('',(#48513,#48514,#48515,#48516));
#11528=EDGE_LOOP('',(#48517,#48518,#48519,#48520));
#11529=EDGE_LOOP('',(#48521,#48522,#48523,#48524));
#11530=EDGE_LOOP('',(#48525,#48526,#48527,#48528));
#11531=EDGE_LOOP('',(#48529,#48530,#48531,#48532));
#11532=EDGE_LOOP('',(#48533,#48534,#48535,#48536));
#11533=EDGE_LOOP('',(#48537,#48538,#48539,#48540));
#11534=EDGE_LOOP('',(#48541,#48542,#48543,#48544));
#11535=EDGE_LOOP('',(#48545,#48546,#48547,#48548));
#11536=EDGE_LOOP('',(#48549,#48550,#48551,#48552));
#11537=EDGE_LOOP('',(#48553,#48554,#48555,#48556));
#11538=EDGE_LOOP('',(#48557,#48558,#48559,#48560));
#11539=EDGE_LOOP('',(#48561,#48562,#48563,#48564));
#11540=EDGE_LOOP('',(#48565,#48566,#48567,#48568));
#11541=EDGE_LOOP('',(#48569,#48570,#48571,#48572));
#11542=EDGE_LOOP('',(#48573,#48574,#48575,#48576));
#11543=EDGE_LOOP('',(#48577,#48578,#48579,#48580));
#11544=EDGE_LOOP('',(#48581,#48582,#48583,#48584));
#11545=EDGE_LOOP('',(#48585,#48586,#48587,#48588));
#11546=EDGE_LOOP('',(#48589,#48590,#48591,#48592));
#11547=EDGE_LOOP('',(#48593,#48594,#48595,#48596));
#11548=EDGE_LOOP('',(#48597,#48598,#48599,#48600));
#11549=EDGE_LOOP('',(#48601,#48602,#48603,#48604));
#11550=EDGE_LOOP('',(#48605,#48606,#48607,#48608));
#11551=EDGE_LOOP('',(#48609,#48610,#48611,#48612));
#11552=EDGE_LOOP('',(#48613,#48614,#48615,#48616));
#11553=EDGE_LOOP('',(#48617,#48618,#48619,#48620));
#11554=EDGE_LOOP('',(#48621,#48622,#48623,#48624));
#11555=EDGE_LOOP('',(#48625,#48626,#48627,#48628));
#11556=EDGE_LOOP('',(#48629,#48630,#48631,#48632));
#11557=EDGE_LOOP('',(#48633,#48634,#48635,#48636));
#11558=EDGE_LOOP('',(#48637,#48638,#48639,#48640));
#11559=EDGE_LOOP('',(#48641,#48642,#48643,#48644));
#11560=EDGE_LOOP('',(#48645,#48646,#48647,#48648));
#11561=EDGE_LOOP('',(#48649,#48650,#48651,#48652));
#11562=EDGE_LOOP('',(#48653,#48654,#48655,#48656));
#11563=EDGE_LOOP('',(#48657,#48658,#48659,#48660));
#11564=EDGE_LOOP('',(#48661,#48662,#48663,#48664));
#11565=EDGE_LOOP('',(#48665,#48666,#48667,#48668));
#11566=EDGE_LOOP('',(#48669,#48670,#48671,#48672));
#11567=EDGE_LOOP('',(#48673,#48674,#48675,#48676));
#11568=EDGE_LOOP('',(#48677,#48678,#48679,#48680));
#11569=EDGE_LOOP('',(#48681,#48682,#48683,#48684));
#11570=EDGE_LOOP('',(#48685,#48686,#48687,#48688));
#11571=EDGE_LOOP('',(#48689,#48690,#48691,#48692));
#11572=EDGE_LOOP('',(#48693,#48694,#48695,#48696));
#11573=EDGE_LOOP('',(#48697,#48698,#48699,#48700));
#11574=EDGE_LOOP('',(#48701,#48702,#48703,#48704));
#11575=EDGE_LOOP('',(#48705,#48706,#48707,#48708));
#11576=EDGE_LOOP('',(#48709,#48710,#48711,#48712));
#11577=EDGE_LOOP('',(#48713,#48714,#48715,#48716));
#11578=EDGE_LOOP('',(#48717,#48718,#48719,#48720));
#11579=EDGE_LOOP('',(#48721,#48722,#48723,#48724));
#11580=EDGE_LOOP('',(#48725,#48726,#48727,#48728));
#11581=EDGE_LOOP('',(#48729,#48730,#48731,#48732));
#11582=EDGE_LOOP('',(#48733,#48734,#48735,#48736));
#11583=EDGE_LOOP('',(#48737,#48738,#48739,#48740));
#11584=EDGE_LOOP('',(#48741,#48742,#48743,#48744));
#11585=EDGE_LOOP('',(#48745,#48746,#48747,#48748));
#11586=EDGE_LOOP('',(#48749,#48750,#48751,#48752));
#11587=EDGE_LOOP('',(#48753,#48754,#48755,#48756));
#11588=EDGE_LOOP('',(#48757,#48758,#48759,#48760));
#11589=EDGE_LOOP('',(#48761,#48762,#48763,#48764));
#11590=EDGE_LOOP('',(#48765,#48766,#48767,#48768));
#11591=EDGE_LOOP('',(#48769,#48770,#48771,#48772));
#11592=EDGE_LOOP('',(#48773,#48774,#48775,#48776));
#11593=EDGE_LOOP('',(#48777,#48778,#48779,#48780));
#11594=EDGE_LOOP('',(#48781,#48782,#48783,#48784));
#11595=EDGE_LOOP('',(#48785,#48786,#48787,#48788));
#11596=EDGE_LOOP('',(#48789,#48790,#48791,#48792));
#11597=EDGE_LOOP('',(#48793,#48794,#48795,#48796));
#11598=EDGE_LOOP('',(#48797,#48798,#48799,#48800));
#11599=EDGE_LOOP('',(#48801,#48802,#48803,#48804));
#11600=EDGE_LOOP('',(#48805,#48806,#48807,#48808));
#11601=EDGE_LOOP('',(#48809,#48810,#48811,#48812));
#11602=EDGE_LOOP('',(#48813,#48814,#48815,#48816));
#11603=EDGE_LOOP('',(#48817,#48818,#48819,#48820));
#11604=EDGE_LOOP('',(#48821,#48822,#48823,#48824));
#11605=EDGE_LOOP('',(#48825,#48826,#48827,#48828));
#11606=EDGE_LOOP('',(#48829,#48830,#48831,#48832));
#11607=EDGE_LOOP('',(#48833,#48834,#48835,#48836));
#11608=EDGE_LOOP('',(#48837,#48838,#48839,#48840));
#11609=EDGE_LOOP('',(#48841,#48842,#48843,#48844));
#11610=EDGE_LOOP('',(#48845,#48846,#48847,#48848));
#11611=EDGE_LOOP('',(#48849,#48850,#48851,#48852));
#11612=EDGE_LOOP('',(#48853,#48854,#48855,#48856));
#11613=EDGE_LOOP('',(#48857,#48858,#48859,#48860));
#11614=EDGE_LOOP('',(#48861,#48862,#48863,#48864));
#11615=EDGE_LOOP('',(#48865,#48866,#48867,#48868));
#11616=EDGE_LOOP('',(#48869,#48870,#48871,#48872));
#11617=EDGE_LOOP('',(#48873,#48874,#48875,#48876));
#11618=EDGE_LOOP('',(#48877,#48878,#48879,#48880));
#11619=EDGE_LOOP('',(#48881,#48882,#48883,#48884));
#11620=EDGE_LOOP('',(#48885,#48886,#48887,#48888));
#11621=EDGE_LOOP('',(#48889,#48890,#48891,#48892));
#11622=EDGE_LOOP('',(#48893,#48894,#48895,#48896));
#11623=EDGE_LOOP('',(#48897,#48898,#48899,#48900));
#11624=EDGE_LOOP('',(#48901,#48902,#48903,#48904));
#11625=EDGE_LOOP('',(#48905,#48906,#48907,#48908));
#11626=EDGE_LOOP('',(#48909,#48910,#48911,#48912));
#11627=EDGE_LOOP('',(#48913,#48914,#48915,#48916));
#11628=EDGE_LOOP('',(#48917,#48918,#48919,#48920));
#11629=EDGE_LOOP('',(#48921,#48922,#48923,#48924));
#11630=EDGE_LOOP('',(#48925,#48926,#48927,#48928));
#11631=EDGE_LOOP('',(#48929,#48930,#48931,#48932));
#11632=EDGE_LOOP('',(#48933,#48934,#48935,#48936));
#11633=EDGE_LOOP('',(#48937,#48938,#48939,#48940));
#11634=EDGE_LOOP('',(#48941,#48942,#48943,#48944));
#11635=EDGE_LOOP('',(#48945,#48946,#48947,#48948));
#11636=EDGE_LOOP('',(#48949,#48950,#48951,#48952));
#11637=EDGE_LOOP('',(#48953,#48954,#48955,#48956));
#11638=EDGE_LOOP('',(#48957,#48958,#48959,#48960));
#11639=EDGE_LOOP('',(#48961,#48962,#48963,#48964));
#11640=EDGE_LOOP('',(#48965,#48966,#48967,#48968));
#11641=EDGE_LOOP('',(#48969,#48970,#48971,#48972));
#11642=EDGE_LOOP('',(#48973,#48974,#48975,#48976));
#11643=EDGE_LOOP('',(#48977,#48978,#48979,#48980));
#11644=EDGE_LOOP('',(#48981,#48982,#48983,#48984));
#11645=EDGE_LOOP('',(#48985,#48986,#48987,#48988));
#11646=EDGE_LOOP('',(#48989,#48990,#48991,#48992));
#11647=EDGE_LOOP('',(#48993,#48994,#48995,#48996));
#11648=EDGE_LOOP('',(#48997,#48998,#48999,#49000));
#11649=EDGE_LOOP('',(#49001,#49002,#49003,#49004));
#11650=EDGE_LOOP('',(#49005,#49006,#49007,#49008));
#11651=EDGE_LOOP('',(#49009,#49010,#49011,#49012));
#11652=EDGE_LOOP('',(#49013,#49014,#49015,#49016));
#11653=EDGE_LOOP('',(#49017,#49018,#49019,#49020));
#11654=EDGE_LOOP('',(#49021,#49022,#49023,#49024));
#11655=EDGE_LOOP('',(#49025,#49026,#49027,#49028));
#11656=EDGE_LOOP('',(#49029,#49030,#49031,#49032));
#11657=EDGE_LOOP('',(#49033,#49034,#49035,#49036));
#11658=EDGE_LOOP('',(#49037,#49038,#49039,#49040));
#11659=EDGE_LOOP('',(#49041,#49042,#49043,#49044));
#11660=EDGE_LOOP('',(#49045,#49046,#49047,#49048));
#11661=EDGE_LOOP('',(#49049,#49050,#49051,#49052));
#11662=EDGE_LOOP('',(#49053,#49054,#49055,#49056));
#11663=EDGE_LOOP('',(#49057,#49058,#49059,#49060));
#11664=EDGE_LOOP('',(#49061,#49062,#49063,#49064));
#11665=EDGE_LOOP('',(#49065,#49066,#49067,#49068));
#11666=EDGE_LOOP('',(#49069,#49070,#49071,#49072));
#11667=EDGE_LOOP('',(#49073,#49074,#49075,#49076));
#11668=EDGE_LOOP('',(#49077,#49078,#49079,#49080));
#11669=EDGE_LOOP('',(#49081,#49082,#49083,#49084));
#11670=EDGE_LOOP('',(#49085,#49086,#49087,#49088));
#11671=EDGE_LOOP('',(#49089,#49090,#49091,#49092));
#11672=EDGE_LOOP('',(#49093,#49094,#49095,#49096));
#11673=EDGE_LOOP('',(#49097,#49098,#49099,#49100));
#11674=EDGE_LOOP('',(#49101,#49102,#49103,#49104));
#11675=EDGE_LOOP('',(#49105,#49106,#49107,#49108));
#11676=EDGE_LOOP('',(#49109,#49110,#49111,#49112));
#11677=EDGE_LOOP('',(#49113,#49114,#49115,#49116));
#11678=EDGE_LOOP('',(#49117,#49118,#49119,#49120));
#11679=EDGE_LOOP('',(#49121,#49122,#49123,#49124));
#11680=EDGE_LOOP('',(#49125,#49126,#49127,#49128));
#11681=EDGE_LOOP('',(#49129,#49130,#49131,#49132));
#11682=EDGE_LOOP('',(#49133,#49134,#49135,#49136));
#11683=EDGE_LOOP('',(#49137,#49138,#49139,#49140));
#11684=EDGE_LOOP('',(#49141,#49142,#49143,#49144));
#11685=EDGE_LOOP('',(#49145,#49146,#49147,#49148));
#11686=EDGE_LOOP('',(#49149,#49150,#49151,#49152));
#11687=EDGE_LOOP('',(#49153,#49154,#49155,#49156));
#11688=EDGE_LOOP('',(#49157,#49158,#49159,#49160));
#11689=EDGE_LOOP('',(#49161,#49162,#49163,#49164));
#11690=EDGE_LOOP('',(#49165,#49166,#49167,#49168));
#11691=EDGE_LOOP('',(#49169,#49170,#49171,#49172));
#11692=EDGE_LOOP('',(#49173,#49174,#49175,#49176));
#11693=EDGE_LOOP('',(#49177,#49178,#49179,#49180));
#11694=EDGE_LOOP('',(#49181,#49182,#49183,#49184));
#11695=EDGE_LOOP('',(#49185,#49186,#49187,#49188));
#11696=EDGE_LOOP('',(#49189,#49190,#49191,#49192));
#11697=EDGE_LOOP('',(#49193,#49194,#49195,#49196));
#11698=EDGE_LOOP('',(#49197,#49198,#49199,#49200));
#11699=EDGE_LOOP('',(#49201,#49202,#49203,#49204));
#11700=EDGE_LOOP('',(#49205,#49206,#49207,#49208));
#11701=EDGE_LOOP('',(#49209,#49210,#49211,#49212));
#11702=EDGE_LOOP('',(#49213,#49214,#49215,#49216));
#11703=EDGE_LOOP('',(#49217,#49218,#49219,#49220));
#11704=EDGE_LOOP('',(#49221,#49222,#49223,#49224));
#11705=EDGE_LOOP('',(#49225,#49226,#49227,#49228));
#11706=EDGE_LOOP('',(#49229,#49230,#49231,#49232));
#11707=EDGE_LOOP('',(#49233,#49234,#49235,#49236));
#11708=EDGE_LOOP('',(#49237,#49238,#49239,#49240));
#11709=EDGE_LOOP('',(#49241,#49242,#49243,#49244));
#11710=EDGE_LOOP('',(#49245,#49246,#49247,#49248));
#11711=EDGE_LOOP('',(#49249,#49250,#49251,#49252));
#11712=EDGE_LOOP('',(#49253,#49254,#49255,#49256));
#11713=EDGE_LOOP('',(#49257,#49258,#49259,#49260));
#11714=EDGE_LOOP('',(#49261,#49262,#49263,#49264));
#11715=EDGE_LOOP('',(#49265,#49266,#49267,#49268));
#11716=EDGE_LOOP('',(#49269,#49270,#49271,#49272));
#11717=EDGE_LOOP('',(#49273,#49274,#49275,#49276));
#11718=EDGE_LOOP('',(#49277,#49278,#49279,#49280));
#11719=EDGE_LOOP('',(#49281,#49282,#49283,#49284));
#11720=EDGE_LOOP('',(#49285,#49286,#49287,#49288));
#11721=EDGE_LOOP('',(#49289,#49290,#49291,#49292));
#11722=EDGE_LOOP('',(#49293,#49294,#49295,#49296));
#11723=EDGE_LOOP('',(#49297,#49298,#49299,#49300));
#11724=EDGE_LOOP('',(#49301,#49302,#49303,#49304));
#11725=EDGE_LOOP('',(#49305,#49306,#49307,#49308));
#11726=EDGE_LOOP('',(#49309,#49310,#49311,#49312));
#11727=EDGE_LOOP('',(#49313,#49314,#49315,#49316));
#11728=EDGE_LOOP('',(#49317,#49318,#49319,#49320));
#11729=EDGE_LOOP('',(#49321,#49322,#49323,#49324));
#11730=EDGE_LOOP('',(#49325,#49326,#49327,#49328));
#11731=EDGE_LOOP('',(#49329,#49330,#49331,#49332));
#11732=EDGE_LOOP('',(#49333,#49334,#49335,#49336));
#11733=EDGE_LOOP('',(#49337,#49338,#49339,#49340));
#11734=EDGE_LOOP('',(#49341,#49342,#49343,#49344));
#11735=EDGE_LOOP('',(#49345,#49346,#49347,#49348));
#11736=EDGE_LOOP('',(#49349,#49350,#49351,#49352));
#11737=EDGE_LOOP('',(#49353,#49354,#49355,#49356));
#11738=EDGE_LOOP('',(#49357,#49358,#49359,#49360));
#11739=EDGE_LOOP('',(#49361,#49362,#49363,#49364));
#11740=EDGE_LOOP('',(#49365,#49366,#49367,#49368));
#11741=EDGE_LOOP('',(#49369,#49370,#49371,#49372));
#11742=EDGE_LOOP('',(#49373,#49374,#49375,#49376));
#11743=EDGE_LOOP('',(#49377,#49378,#49379,#49380));
#11744=EDGE_LOOP('',(#49381,#49382,#49383,#49384));
#11745=EDGE_LOOP('',(#49385,#49386,#49387,#49388));
#11746=EDGE_LOOP('',(#49389,#49390,#49391,#49392));
#11747=EDGE_LOOP('',(#49393,#49394,#49395,#49396));
#11748=EDGE_LOOP('',(#49397,#49398,#49399,#49400));
#11749=EDGE_LOOP('',(#49401,#49402,#49403,#49404));
#11750=EDGE_LOOP('',(#49405,#49406,#49407,#49408));
#11751=EDGE_LOOP('',(#49409,#49410,#49411,#49412));
#11752=EDGE_LOOP('',(#49413,#49414,#49415,#49416));
#11753=EDGE_LOOP('',(#49417,#49418,#49419,#49420));
#11754=EDGE_LOOP('',(#49421,#49422,#49423,#49424));
#11755=EDGE_LOOP('',(#49425,#49426,#49427,#49428));
#11756=EDGE_LOOP('',(#49429,#49430,#49431,#49432));
#11757=EDGE_LOOP('',(#49433,#49434,#49435,#49436));
#11758=EDGE_LOOP('',(#49437,#49438,#49439,#49440));
#11759=EDGE_LOOP('',(#49441,#49442,#49443,#49444));
#11760=EDGE_LOOP('',(#49445,#49446,#49447,#49448));
#11761=EDGE_LOOP('',(#49449,#49450,#49451,#49452));
#11762=EDGE_LOOP('',(#49453,#49454,#49455,#49456));
#11763=EDGE_LOOP('',(#49457,#49458,#49459,#49460));
#11764=EDGE_LOOP('',(#49461,#49462,#49463,#49464));
#11765=EDGE_LOOP('',(#49465,#49466,#49467,#49468));
#11766=EDGE_LOOP('',(#49469,#49470,#49471,#49472));
#11767=EDGE_LOOP('',(#49473,#49474,#49475,#49476));
#11768=EDGE_LOOP('',(#49477,#49478,#49479,#49480));
#11769=EDGE_LOOP('',(#49481,#49482,#49483,#49484));
#11770=EDGE_LOOP('',(#49485,#49486,#49487,#49488));
#11771=EDGE_LOOP('',(#49489,#49490,#49491,#49492));
#11772=EDGE_LOOP('',(#49493,#49494,#49495,#49496));
#11773=EDGE_LOOP('',(#49497,#49498,#49499,#49500));
#11774=EDGE_LOOP('',(#49501,#49502,#49503,#49504));
#11775=EDGE_LOOP('',(#49505,#49506,#49507,#49508));
#11776=EDGE_LOOP('',(#49509,#49510,#49511,#49512));
#11777=EDGE_LOOP('',(#49513,#49514,#49515,#49516));
#11778=EDGE_LOOP('',(#49517,#49518,#49519,#49520));
#11779=EDGE_LOOP('',(#49521,#49522,#49523,#49524));
#11780=EDGE_LOOP('',(#49525,#49526,#49527,#49528));
#11781=EDGE_LOOP('',(#49529,#49530,#49531,#49532));
#11782=EDGE_LOOP('',(#49533,#49534,#49535,#49536));
#11783=EDGE_LOOP('',(#49537,#49538,#49539,#49540));
#11784=EDGE_LOOP('',(#49541,#49542,#49543,#49544));
#11785=EDGE_LOOP('',(#49545,#49546,#49547,#49548));
#11786=EDGE_LOOP('',(#49549,#49550,#49551,#49552));
#11787=EDGE_LOOP('',(#49553,#49554,#49555,#49556));
#11788=EDGE_LOOP('',(#49557,#49558,#49559,#49560));
#11789=EDGE_LOOP('',(#49561,#49562,#49563,#49564));
#11790=EDGE_LOOP('',(#49565,#49566,#49567,#49568));
#11791=EDGE_LOOP('',(#49569,#49570,#49571,#49572));
#11792=EDGE_LOOP('',(#49573,#49574,#49575,#49576));
#11793=EDGE_LOOP('',(#49577,#49578,#49579,#49580));
#11794=EDGE_LOOP('',(#49581,#49582,#49583,#49584));
#11795=EDGE_LOOP('',(#49585,#49586,#49587,#49588));
#11796=EDGE_LOOP('',(#49589,#49590,#49591,#49592));
#11797=EDGE_LOOP('',(#49593,#49594,#49595,#49596));
#11798=EDGE_LOOP('',(#49597,#49598,#49599,#49600));
#11799=EDGE_LOOP('',(#49601,#49602,#49603,#49604));
#11800=EDGE_LOOP('',(#49605,#49606,#49607,#49608));
#11801=EDGE_LOOP('',(#49609,#49610,#49611,#49612));
#11802=EDGE_LOOP('',(#49613,#49614,#49615,#49616));
#11803=EDGE_LOOP('',(#49617,#49618,#49619,#49620));
#11804=EDGE_LOOP('',(#49621,#49622,#49623,#49624));
#11805=EDGE_LOOP('',(#49625,#49626,#49627,#49628));
#11806=EDGE_LOOP('',(#49629,#49630,#49631,#49632));
#11807=EDGE_LOOP('',(#49633,#49634,#49635,#49636));
#11808=EDGE_LOOP('',(#49637,#49638,#49639,#49640));
#11809=EDGE_LOOP('',(#49641,#49642,#49643,#49644));
#11810=EDGE_LOOP('',(#49645,#49646,#49647,#49648));
#11811=EDGE_LOOP('',(#49649,#49650,#49651,#49652));
#11812=EDGE_LOOP('',(#49653,#49654,#49655,#49656));
#11813=EDGE_LOOP('',(#49657,#49658,#49659,#49660));
#11814=EDGE_LOOP('',(#49661,#49662,#49663,#49664));
#11815=EDGE_LOOP('',(#49665,#49666,#49667,#49668));
#11816=EDGE_LOOP('',(#49669,#49670,#49671,#49672));
#11817=EDGE_LOOP('',(#49673,#49674,#49675,#49676));
#11818=EDGE_LOOP('',(#49677,#49678,#49679,#49680));
#11819=EDGE_LOOP('',(#49681,#49682,#49683,#49684));
#11820=EDGE_LOOP('',(#49685,#49686,#49687,#49688));
#11821=EDGE_LOOP('',(#49689,#49690,#49691,#49692));
#11822=EDGE_LOOP('',(#49693,#49694,#49695,#49696));
#11823=EDGE_LOOP('',(#49697,#49698,#49699,#49700));
#11824=EDGE_LOOP('',(#49701,#49702,#49703,#49704));
#11825=EDGE_LOOP('',(#49705,#49706,#49707,#49708));
#11826=EDGE_LOOP('',(#49709,#49710,#49711,#49712));
#11827=EDGE_LOOP('',(#49713,#49714,#49715,#49716));
#11828=EDGE_LOOP('',(#49717,#49718,#49719,#49720));
#11829=EDGE_LOOP('',(#49721,#49722,#49723,#49724));
#11830=EDGE_LOOP('',(#49725,#49726,#49727,#49728));
#11831=EDGE_LOOP('',(#49729,#49730,#49731,#49732));
#11832=EDGE_LOOP('',(#49733,#49734,#49735,#49736));
#11833=EDGE_LOOP('',(#49737,#49738,#49739,#49740));
#11834=EDGE_LOOP('',(#49741,#49742,#49743,#49744));
#11835=EDGE_LOOP('',(#49745,#49746,#49747,#49748));
#11836=EDGE_LOOP('',(#49749,#49750,#49751,#49752));
#11837=EDGE_LOOP('',(#49753,#49754,#49755,#49756));
#11838=EDGE_LOOP('',(#49757,#49758,#49759,#49760));
#11839=EDGE_LOOP('',(#49761,#49762,#49763,#49764));
#11840=EDGE_LOOP('',(#49765,#49766,#49767,#49768));
#11841=EDGE_LOOP('',(#49769,#49770,#49771,#49772));
#11842=EDGE_LOOP('',(#49773,#49774,#49775,#49776));
#11843=EDGE_LOOP('',(#49777,#49778,#49779,#49780));
#11844=EDGE_LOOP('',(#49781,#49782,#49783,#49784));
#11845=EDGE_LOOP('',(#49785,#49786,#49787,#49788));
#11846=EDGE_LOOP('',(#49789,#49790,#49791,#49792));
#11847=EDGE_LOOP('',(#49793,#49794,#49795,#49796));
#11848=EDGE_LOOP('',(#49797,#49798,#49799,#49800));
#11849=EDGE_LOOP('',(#49801,#49802,#49803,#49804));
#11850=EDGE_LOOP('',(#49805,#49806,#49807,#49808));
#11851=EDGE_LOOP('',(#49809,#49810,#49811,#49812));
#11852=EDGE_LOOP('',(#49813,#49814,#49815,#49816));
#11853=EDGE_LOOP('',(#49817,#49818,#49819,#49820));
#11854=EDGE_LOOP('',(#49821,#49822,#49823,#49824));
#11855=EDGE_LOOP('',(#49825,#49826,#49827,#49828));
#11856=EDGE_LOOP('',(#49829,#49830,#49831,#49832));
#11857=EDGE_LOOP('',(#49833,#49834,#49835,#49836));
#11858=EDGE_LOOP('',(#49837,#49838,#49839,#49840));
#11859=EDGE_LOOP('',(#49841,#49842,#49843,#49844));
#11860=EDGE_LOOP('',(#49845,#49846,#49847,#49848));
#11861=EDGE_LOOP('',(#49849,#49850,#49851,#49852));
#11862=EDGE_LOOP('',(#49853,#49854,#49855,#49856));
#11863=EDGE_LOOP('',(#49857,#49858,#49859,#49860));
#11864=EDGE_LOOP('',(#49861,#49862,#49863,#49864));
#11865=EDGE_LOOP('',(#49865,#49866,#49867,#49868));
#11866=EDGE_LOOP('',(#49869,#49870,#49871,#49872));
#11867=EDGE_LOOP('',(#49873,#49874,#49875,#49876));
#11868=EDGE_LOOP('',(#49877,#49878,#49879,#49880));
#11869=EDGE_LOOP('',(#49881,#49882,#49883,#49884));
#11870=EDGE_LOOP('',(#49885,#49886,#49887,#49888));
#11871=EDGE_LOOP('',(#49889,#49890,#49891,#49892));
#11872=EDGE_LOOP('',(#49893,#49894,#49895,#49896));
#11873=EDGE_LOOP('',(#49897,#49898,#49899,#49900));
#11874=EDGE_LOOP('',(#49901,#49902,#49903,#49904));
#11875=EDGE_LOOP('',(#49905,#49906,#49907,#49908));
#11876=EDGE_LOOP('',(#49909,#49910,#49911,#49912));
#11877=EDGE_LOOP('',(#49913,#49914,#49915,#49916));
#11878=EDGE_LOOP('',(#49917,#49918,#49919,#49920));
#11879=EDGE_LOOP('',(#49921,#49922,#49923,#49924));
#11880=EDGE_LOOP('',(#49925,#49926,#49927,#49928));
#11881=EDGE_LOOP('',(#49929,#49930,#49931,#49932));
#11882=EDGE_LOOP('',(#49933,#49934,#49935,#49936));
#11883=EDGE_LOOP('',(#49937,#49938,#49939,#49940));
#11884=EDGE_LOOP('',(#49941,#49942,#49943,#49944));
#11885=EDGE_LOOP('',(#49945,#49946,#49947,#49948));
#11886=EDGE_LOOP('',(#49949,#49950,#49951,#49952));
#11887=EDGE_LOOP('',(#49953,#49954,#49955,#49956));
#11888=EDGE_LOOP('',(#49957,#49958,#49959,#49960));
#11889=EDGE_LOOP('',(#49961,#49962,#49963,#49964));
#11890=EDGE_LOOP('',(#49965,#49966,#49967,#49968));
#11891=EDGE_LOOP('',(#49969,#49970,#49971,#49972));
#11892=EDGE_LOOP('',(#49973,#49974,#49975,#49976));
#11893=EDGE_LOOP('',(#49977,#49978,#49979,#49980));
#11894=EDGE_LOOP('',(#49981,#49982,#49983,#49984));
#11895=EDGE_LOOP('',(#49985,#49986,#49987,#49988));
#11896=EDGE_LOOP('',(#49989,#49990,#49991,#49992));
#11897=EDGE_LOOP('',(#49993,#49994,#49995,#49996));
#11898=EDGE_LOOP('',(#49997,#49998,#49999,#50000));
#11899=EDGE_LOOP('',(#50001,#50002,#50003,#50004));
#11900=EDGE_LOOP('',(#50005,#50006,#50007,#50008));
#11901=EDGE_LOOP('',(#50009,#50010,#50011,#50012));
#11902=EDGE_LOOP('',(#50013,#50014,#50015,#50016));
#11903=EDGE_LOOP('',(#50017,#50018,#50019,#50020));
#11904=EDGE_LOOP('',(#50021,#50022,#50023,#50024));
#11905=EDGE_LOOP('',(#50025,#50026,#50027,#50028));
#11906=EDGE_LOOP('',(#50029,#50030,#50031,#50032));
#11907=EDGE_LOOP('',(#50033,#50034,#50035,#50036));
#11908=EDGE_LOOP('',(#50037,#50038,#50039,#50040));
#11909=EDGE_LOOP('',(#50041,#50042,#50043,#50044));
#11910=EDGE_LOOP('',(#50045,#50046,#50047,#50048));
#11911=EDGE_LOOP('',(#50049,#50050,#50051,#50052));
#11912=EDGE_LOOP('',(#50053,#50054,#50055,#50056));
#11913=EDGE_LOOP('',(#50057,#50058,#50059,#50060));
#11914=EDGE_LOOP('',(#50061,#50062,#50063,#50064));
#11915=EDGE_LOOP('',(#50065,#50066,#50067,#50068));
#11916=EDGE_LOOP('',(#50069,#50070,#50071,#50072));
#11917=EDGE_LOOP('',(#50073,#50074,#50075,#50076));
#11918=EDGE_LOOP('',(#50077,#50078,#50079,#50080));
#11919=EDGE_LOOP('',(#50081,#50082,#50083,#50084));
#11920=EDGE_LOOP('',(#50085,#50086,#50087,#50088));
#11921=EDGE_LOOP('',(#50089,#50090,#50091,#50092));
#11922=EDGE_LOOP('',(#50093,#50094,#50095,#50096));
#11923=EDGE_LOOP('',(#50097,#50098,#50099,#50100));
#11924=EDGE_LOOP('',(#50101,#50102,#50103,#50104));
#11925=EDGE_LOOP('',(#50105,#50106,#50107,#50108));
#11926=EDGE_LOOP('',(#50109,#50110,#50111,#50112));
#11927=EDGE_LOOP('',(#50113,#50114,#50115,#50116));
#11928=EDGE_LOOP('',(#50117,#50118,#50119,#50120));
#11929=EDGE_LOOP('',(#50121,#50122,#50123,#50124));
#11930=EDGE_LOOP('',(#50125,#50126,#50127,#50128));
#11931=EDGE_LOOP('',(#50129,#50130,#50131,#50132));
#11932=EDGE_LOOP('',(#50133,#50134,#50135,#50136));
#11933=EDGE_LOOP('',(#50137,#50138,#50139,#50140));
#11934=EDGE_LOOP('',(#50141,#50142,#50143,#50144));
#11935=EDGE_LOOP('',(#50145,#50146,#50147,#50148));
#11936=EDGE_LOOP('',(#50149,#50150,#50151,#50152));
#11937=EDGE_LOOP('',(#50153,#50154,#50155,#50156));
#11938=EDGE_LOOP('',(#50157,#50158,#50159,#50160));
#11939=EDGE_LOOP('',(#50161,#50162,#50163,#50164));
#11940=EDGE_LOOP('',(#50165,#50166,#50167,#50168));
#11941=EDGE_LOOP('',(#50169,#50170,#50171,#50172));
#11942=EDGE_LOOP('',(#50173,#50174,#50175,#50176));
#11943=EDGE_LOOP('',(#50177,#50178,#50179,#50180));
#11944=EDGE_LOOP('',(#50181,#50182,#50183,#50184));
#11945=EDGE_LOOP('',(#50185,#50186,#50187,#50188));
#11946=EDGE_LOOP('',(#50189,#50190,#50191,#50192));
#11947=EDGE_LOOP('',(#50193,#50194,#50195,#50196));
#11948=EDGE_LOOP('',(#50197,#50198,#50199,#50200));
#11949=EDGE_LOOP('',(#50201,#50202,#50203,#50204));
#11950=EDGE_LOOP('',(#50205,#50206,#50207,#50208));
#11951=EDGE_LOOP('',(#50209,#50210,#50211,#50212));
#11952=EDGE_LOOP('',(#50213,#50214,#50215,#50216));
#11953=EDGE_LOOP('',(#50217,#50218,#50219,#50220));
#11954=EDGE_LOOP('',(#50221,#50222,#50223,#50224));
#11955=EDGE_LOOP('',(#50225,#50226,#50227,#50228));
#11956=EDGE_LOOP('',(#50229,#50230,#50231,#50232));
#11957=EDGE_LOOP('',(#50233,#50234,#50235,#50236));
#11958=EDGE_LOOP('',(#50237,#50238,#50239,#50240));
#11959=EDGE_LOOP('',(#50241,#50242,#50243,#50244));
#11960=EDGE_LOOP('',(#50245,#50246,#50247,#50248));
#11961=EDGE_LOOP('',(#50249,#50250,#50251,#50252));
#11962=EDGE_LOOP('',(#50253,#50254,#50255,#50256));
#11963=EDGE_LOOP('',(#50257,#50258,#50259,#50260));
#11964=EDGE_LOOP('',(#50261,#50262,#50263,#50264));
#11965=EDGE_LOOP('',(#50265,#50266,#50267,#50268));
#11966=EDGE_LOOP('',(#50269,#50270,#50271,#50272));
#11967=EDGE_LOOP('',(#50273,#50274,#50275,#50276));
#11968=EDGE_LOOP('',(#50277,#50278,#50279,#50280));
#11969=EDGE_LOOP('',(#50281,#50282,#50283,#50284));
#11970=EDGE_LOOP('',(#50285,#50286,#50287,#50288));
#11971=EDGE_LOOP('',(#50289,#50290,#50291,#50292));
#11972=EDGE_LOOP('',(#50293,#50294,#50295,#50296));
#11973=EDGE_LOOP('',(#50297,#50298,#50299,#50300));
#11974=EDGE_LOOP('',(#50301,#50302,#50303,#50304));
#11975=EDGE_LOOP('',(#50305,#50306,#50307,#50308));
#11976=EDGE_LOOP('',(#50309,#50310,#50311,#50312));
#11977=EDGE_LOOP('',(#50313,#50314,#50315,#50316));
#11978=EDGE_LOOP('',(#50317,#50318,#50319,#50320));
#11979=EDGE_LOOP('',(#50321,#50322,#50323,#50324));
#11980=EDGE_LOOP('',(#50325,#50326,#50327,#50328));
#11981=EDGE_LOOP('',(#50329,#50330,#50331,#50332));
#11982=EDGE_LOOP('',(#50333,#50334,#50335,#50336));
#11983=EDGE_LOOP('',(#50337,#50338,#50339,#50340));
#11984=EDGE_LOOP('',(#50341,#50342,#50343,#50344));
#11985=EDGE_LOOP('',(#50345,#50346,#50347,#50348));
#11986=EDGE_LOOP('',(#50349,#50350,#50351,#50352));
#11987=EDGE_LOOP('',(#50353,#50354,#50355,#50356));
#11988=EDGE_LOOP('',(#50357,#50358,#50359,#50360));
#11989=EDGE_LOOP('',(#50361,#50362,#50363,#50364));
#11990=EDGE_LOOP('',(#50365,#50366,#50367,#50368));
#11991=EDGE_LOOP('',(#50369,#50370,#50371,#50372));
#11992=EDGE_LOOP('',(#50373,#50374,#50375,#50376));
#11993=EDGE_LOOP('',(#50377,#50378,#50379,#50380));
#11994=EDGE_LOOP('',(#50381,#50382,#50383,#50384));
#11995=EDGE_LOOP('',(#50385,#50386,#50387,#50388));
#11996=EDGE_LOOP('',(#50389,#50390,#50391,#50392));
#11997=EDGE_LOOP('',(#50393,#50394,#50395,#50396));
#11998=EDGE_LOOP('',(#50397,#50398,#50399,#50400));
#11999=EDGE_LOOP('',(#50401,#50402,#50403,#50404));
#12000=EDGE_LOOP('',(#50405,#50406,#50407,#50408));
#12001=EDGE_LOOP('',(#50409,#50410,#50411,#50412));
#12002=EDGE_LOOP('',(#50413,#50414,#50415,#50416));
#12003=EDGE_LOOP('',(#50417,#50418,#50419,#50420));
#12004=EDGE_LOOP('',(#50421,#50422,#50423,#50424));
#12005=EDGE_LOOP('',(#50425,#50426,#50427,#50428));
#12006=EDGE_LOOP('',(#50429,#50430,#50431,#50432));
#12007=EDGE_LOOP('',(#50433,#50434,#50435,#50436));
#12008=EDGE_LOOP('',(#50437,#50438,#50439,#50440));
#12009=EDGE_LOOP('',(#50441,#50442,#50443,#50444));
#12010=EDGE_LOOP('',(#50445,#50446,#50447,#50448));
#12011=EDGE_LOOP('',(#50449,#50450,#50451,#50452));
#12012=EDGE_LOOP('',(#50453,#50454,#50455,#50456));
#12013=EDGE_LOOP('',(#50457,#50458,#50459,#50460));
#12014=EDGE_LOOP('',(#50461,#50462,#50463,#50464));
#12015=EDGE_LOOP('',(#50465,#50466,#50467,#50468));
#12016=EDGE_LOOP('',(#50469,#50470,#50471,#50472));
#12017=EDGE_LOOP('',(#50473,#50474,#50475,#50476));
#12018=EDGE_LOOP('',(#50477,#50478,#50479,#50480));
#12019=EDGE_LOOP('',(#50481,#50482,#50483,#50484));
#12020=EDGE_LOOP('',(#50485,#50486,#50487,#50488));
#12021=EDGE_LOOP('',(#50489,#50490,#50491,#50492));
#12022=EDGE_LOOP('',(#50493,#50494,#50495,#50496));
#12023=EDGE_LOOP('',(#50497,#50498,#50499,#50500));
#12024=EDGE_LOOP('',(#50501,#50502,#50503,#50504));
#12025=EDGE_LOOP('',(#50505,#50506,#50507,#50508));
#12026=EDGE_LOOP('',(#50509,#50510,#50511,#50512));
#12027=EDGE_LOOP('',(#50513,#50514,#50515,#50516));
#12028=EDGE_LOOP('',(#50517,#50518,#50519,#50520));
#12029=EDGE_LOOP('',(#50521,#50522,#50523,#50524));
#12030=EDGE_LOOP('',(#50525,#50526,#50527,#50528));
#12031=EDGE_LOOP('',(#50529,#50530,#50531,#50532));
#12032=EDGE_LOOP('',(#50533,#50534,#50535,#50536));
#12033=EDGE_LOOP('',(#50537,#50538,#50539,#50540));
#12034=EDGE_LOOP('',(#50541,#50542,#50543,#50544));
#12035=EDGE_LOOP('',(#50545,#50546,#50547,#50548));
#12036=EDGE_LOOP('',(#50549,#50550,#50551,#50552));
#12037=EDGE_LOOP('',(#50553,#50554,#50555,#50556));
#12038=EDGE_LOOP('',(#50557,#50558,#50559,#50560));
#12039=EDGE_LOOP('',(#50561,#50562,#50563,#50564));
#12040=EDGE_LOOP('',(#50565,#50566,#50567,#50568));
#12041=EDGE_LOOP('',(#50569,#50570,#50571,#50572));
#12042=EDGE_LOOP('',(#50573,#50574,#50575,#50576));
#12043=EDGE_LOOP('',(#50577,#50578,#50579,#50580));
#12044=EDGE_LOOP('',(#50581,#50582,#50583,#50584));
#12045=EDGE_LOOP('',(#50585,#50586,#50587,#50588));
#12046=EDGE_LOOP('',(#50589,#50590,#50591,#50592));
#12047=EDGE_LOOP('',(#50593,#50594,#50595,#50596));
#12048=EDGE_LOOP('',(#50597,#50598,#50599,#50600));
#12049=EDGE_LOOP('',(#50601,#50602,#50603,#50604));
#12050=EDGE_LOOP('',(#50605,#50606,#50607,#50608));
#12051=EDGE_LOOP('',(#50609,#50610,#50611,#50612));
#12052=EDGE_LOOP('',(#50613,#50614,#50615,#50616));
#12053=EDGE_LOOP('',(#50617,#50618,#50619,#50620));
#12054=EDGE_LOOP('',(#50621,#50622,#50623,#50624));
#12055=EDGE_LOOP('',(#50625,#50626,#50627,#50628));
#12056=EDGE_LOOP('',(#50629,#50630,#50631,#50632));
#12057=EDGE_LOOP('',(#50633,#50634,#50635,#50636));
#12058=EDGE_LOOP('',(#50637,#50638,#50639,#50640));
#12059=EDGE_LOOP('',(#50641,#50642,#50643,#50644));
#12060=EDGE_LOOP('',(#50645,#50646,#50647,#50648));
#12061=EDGE_LOOP('',(#50649,#50650,#50651,#50652));
#12062=EDGE_LOOP('',(#50653,#50654,#50655,#50656));
#12063=EDGE_LOOP('',(#50657,#50658,#50659,#50660));
#12064=EDGE_LOOP('',(#50661,#50662,#50663,#50664));
#12065=EDGE_LOOP('',(#50665,#50666,#50667,#50668));
#12066=EDGE_LOOP('',(#50669,#50670,#50671,#50672));
#12067=EDGE_LOOP('',(#50673,#50674,#50675,#50676));
#12068=EDGE_LOOP('',(#50677,#50678,#50679,#50680));
#12069=EDGE_LOOP('',(#50681,#50682,#50683,#50684));
#12070=EDGE_LOOP('',(#50685,#50686,#50687,#50688));
#12071=EDGE_LOOP('',(#50689,#50690,#50691,#50692));
#12072=EDGE_LOOP('',(#50693,#50694,#50695,#50696));
#12073=EDGE_LOOP('',(#50697,#50698,#50699,#50700));
#12074=EDGE_LOOP('',(#50701,#50702,#50703,#50704));
#12075=EDGE_LOOP('',(#50705,#50706,#50707,#50708));
#12076=EDGE_LOOP('',(#50709,#50710,#50711,#50712));
#12077=EDGE_LOOP('',(#50713,#50714,#50715,#50716));
#12078=EDGE_LOOP('',(#50717,#50718,#50719,#50720));
#12079=EDGE_LOOP('',(#50721,#50722,#50723,#50724));
#12080=EDGE_LOOP('',(#50725,#50726,#50727,#50728));
#12081=EDGE_LOOP('',(#50729,#50730,#50731,#50732));
#12082=EDGE_LOOP('',(#50733,#50734,#50735,#50736));
#12083=EDGE_LOOP('',(#50737,#50738,#50739,#50740));
#12084=EDGE_LOOP('',(#50741,#50742,#50743,#50744));
#12085=EDGE_LOOP('',(#50745,#50746,#50747,#50748));
#12086=EDGE_LOOP('',(#50749,#50750,#50751,#50752));
#12087=EDGE_LOOP('',(#50753,#50754,#50755,#50756));
#12088=EDGE_LOOP('',(#50757,#50758,#50759,#50760));
#12089=EDGE_LOOP('',(#50761,#50762,#50763,#50764));
#12090=EDGE_LOOP('',(#50765,#50766,#50767,#50768));
#12091=EDGE_LOOP('',(#50769,#50770,#50771,#50772));
#12092=EDGE_LOOP('',(#50773,#50774,#50775,#50776));
#12093=EDGE_LOOP('',(#50777,#50778,#50779,#50780));
#12094=EDGE_LOOP('',(#50781,#50782,#50783,#50784));
#12095=EDGE_LOOP('',(#50785,#50786,#50787,#50788));
#12096=EDGE_LOOP('',(#50789,#50790,#50791,#50792));
#12097=EDGE_LOOP('',(#50793,#50794,#50795,#50796));
#12098=EDGE_LOOP('',(#50797,#50798,#50799,#50800));
#12099=EDGE_LOOP('',(#50801,#50802,#50803,#50804));
#12100=EDGE_LOOP('',(#50805,#50806,#50807,#50808));
#12101=EDGE_LOOP('',(#50809,#50810,#50811,#50812));
#12102=EDGE_LOOP('',(#50813,#50814,#50815,#50816));
#12103=EDGE_LOOP('',(#50817,#50818,#50819,#50820));
#12104=EDGE_LOOP('',(#50821,#50822,#50823,#50824));
#12105=EDGE_LOOP('',(#50825,#50826,#50827,#50828));
#12106=EDGE_LOOP('',(#50829,#50830,#50831,#50832));
#12107=EDGE_LOOP('',(#50833,#50834,#50835,#50836));
#12108=EDGE_LOOP('',(#50837,#50838,#50839,#50840));
#12109=EDGE_LOOP('',(#50841,#50842,#50843,#50844));
#12110=EDGE_LOOP('',(#50845,#50846,#50847,#50848));
#12111=EDGE_LOOP('',(#50849,#50850,#50851,#50852));
#12112=EDGE_LOOP('',(#50853,#50854,#50855,#50856));
#12113=EDGE_LOOP('',(#50857,#50858,#50859,#50860));
#12114=EDGE_LOOP('',(#50861,#50862,#50863,#50864));
#12115=EDGE_LOOP('',(#50865,#50866,#50867,#50868));
#12116=EDGE_LOOP('',(#50869,#50870,#50871,#50872));
#12117=EDGE_LOOP('',(#50873,#50874,#50875,#50876));
#12118=EDGE_LOOP('',(#50877,#50878,#50879,#50880));
#12119=EDGE_LOOP('',(#50881,#50882,#50883,#50884));
#12120=EDGE_LOOP('',(#50885,#50886,#50887,#50888));
#12121=EDGE_LOOP('',(#50889,#50890,#50891,#50892));
#12122=EDGE_LOOP('',(#50893,#50894,#50895,#50896));
#12123=EDGE_LOOP('',(#50897,#50898,#50899,#50900));
#12124=EDGE_LOOP('',(#50901,#50902,#50903,#50904));
#12125=EDGE_LOOP('',(#50905,#50906,#50907,#50908));
#12126=EDGE_LOOP('',(#50909,#50910,#50911,#50912));
#12127=EDGE_LOOP('',(#50913,#50914,#50915,#50916));
#12128=EDGE_LOOP('',(#50917,#50918,#50919,#50920));
#12129=EDGE_LOOP('',(#50921,#50922,#50923,#50924));
#12130=EDGE_LOOP('',(#50925,#50926,#50927,#50928));
#12131=EDGE_LOOP('',(#50929,#50930,#50931,#50932));
#12132=EDGE_LOOP('',(#50933,#50934,#50935,#50936));
#12133=EDGE_LOOP('',(#50937,#50938,#50939,#50940));
#12134=EDGE_LOOP('',(#50941,#50942,#50943,#50944));
#12135=EDGE_LOOP('',(#50945,#50946,#50947,#50948));
#12136=EDGE_LOOP('',(#50949,#50950,#50951,#50952));
#12137=EDGE_LOOP('',(#50953,#50954,#50955,#50956));
#12138=EDGE_LOOP('',(#50957,#50958,#50959,#50960));
#12139=EDGE_LOOP('',(#50961,#50962,#50963,#50964));
#12140=EDGE_LOOP('',(#50965,#50966,#50967,#50968));
#12141=EDGE_LOOP('',(#50969,#50970,#50971,#50972));
#12142=EDGE_LOOP('',(#50973,#50974,#50975,#50976));
#12143=EDGE_LOOP('',(#50977,#50978,#50979,#50980));
#12144=EDGE_LOOP('',(#50981,#50982,#50983,#50984));
#12145=EDGE_LOOP('',(#50985,#50986,#50987,#50988));
#12146=EDGE_LOOP('',(#50989,#50990,#50991,#50992));
#12147=EDGE_LOOP('',(#50993,#50994,#50995,#50996));
#12148=EDGE_LOOP('',(#50997,#50998,#50999,#51000));
#12149=EDGE_LOOP('',(#51001,#51002,#51003,#51004));
#12150=EDGE_LOOP('',(#51005,#51006,#51007,#51008));
#12151=EDGE_LOOP('',(#51009,#51010,#51011,#51012));
#12152=EDGE_LOOP('',(#51013,#51014,#51015,#51016));
#12153=EDGE_LOOP('',(#51017,#51018,#51019,#51020));
#12154=EDGE_LOOP('',(#51021,#51022,#51023,#51024));
#12155=EDGE_LOOP('',(#51025,#51026,#51027,#51028));
#12156=EDGE_LOOP('',(#51029,#51030,#51031,#51032));
#12157=EDGE_LOOP('',(#51033,#51034,#51035,#51036));
#12158=EDGE_LOOP('',(#51037,#51038,#51039,#51040));
#12159=EDGE_LOOP('',(#51041,#51042,#51043,#51044));
#12160=EDGE_LOOP('',(#51045,#51046,#51047,#51048));
#12161=EDGE_LOOP('',(#51049,#51050,#51051,#51052));
#12162=EDGE_LOOP('',(#51053,#51054,#51055,#51056));
#12163=EDGE_LOOP('',(#51057,#51058,#51059,#51060));
#12164=EDGE_LOOP('',(#51061,#51062,#51063,#51064));
#12165=EDGE_LOOP('',(#51065,#51066,#51067,#51068));
#12166=EDGE_LOOP('',(#51069,#51070,#51071,#51072));
#12167=EDGE_LOOP('',(#51073,#51074,#51075,#51076));
#12168=EDGE_LOOP('',(#51077,#51078,#51079,#51080));
#12169=EDGE_LOOP('',(#51081,#51082,#51083,#51084));
#12170=EDGE_LOOP('',(#51085,#51086,#51087,#51088));
#12171=EDGE_LOOP('',(#51089,#51090,#51091,#51092));
#12172=EDGE_LOOP('',(#51093,#51094,#51095,#51096));
#12173=EDGE_LOOP('',(#51097,#51098,#51099,#51100));
#12174=EDGE_LOOP('',(#51101,#51102,#51103,#51104));
#12175=EDGE_LOOP('',(#51105,#51106,#51107,#51108));
#12176=EDGE_LOOP('',(#51109,#51110,#51111,#51112));
#12177=EDGE_LOOP('',(#51113,#51114,#51115,#51116));
#12178=EDGE_LOOP('',(#51117,#51118,#51119,#51120));
#12179=EDGE_LOOP('',(#51121,#51122,#51123,#51124));
#12180=EDGE_LOOP('',(#51125,#51126,#51127,#51128));
#12181=EDGE_LOOP('',(#51129,#51130,#51131,#51132));
#12182=EDGE_LOOP('',(#51133,#51134,#51135,#51136));
#12183=EDGE_LOOP('',(#51137,#51138,#51139,#51140));
#12184=EDGE_LOOP('',(#51141,#51142,#51143,#51144));
#12185=EDGE_LOOP('',(#51145,#51146,#51147,#51148));
#12186=EDGE_LOOP('',(#51149,#51150,#51151,#51152));
#12187=EDGE_LOOP('',(#51153,#51154,#51155,#51156));
#12188=EDGE_LOOP('',(#51157,#51158,#51159,#51160));
#12189=EDGE_LOOP('',(#51161,#51162,#51163,#51164));
#12190=EDGE_LOOP('',(#51165,#51166,#51167,#51168));
#12191=EDGE_LOOP('',(#51169,#51170,#51171,#51172));
#12192=EDGE_LOOP('',(#51173,#51174,#51175,#51176));
#12193=EDGE_LOOP('',(#51177,#51178,#51179,#51180));
#12194=EDGE_LOOP('',(#51181,#51182,#51183,#51184));
#12195=EDGE_LOOP('',(#51185,#51186,#51187,#51188));
#12196=EDGE_LOOP('',(#51189,#51190,#51191,#51192));
#12197=EDGE_LOOP('',(#51193,#51194,#51195,#51196));
#12198=EDGE_LOOP('',(#51197,#51198,#51199,#51200));
#12199=EDGE_LOOP('',(#51201,#51202,#51203,#51204));
#12200=EDGE_LOOP('',(#51205,#51206,#51207,#51208));
#12201=EDGE_LOOP('',(#51209,#51210,#51211,#51212));
#12202=EDGE_LOOP('',(#51213,#51214,#51215,#51216));
#12203=EDGE_LOOP('',(#51217,#51218,#51219,#51220));
#12204=EDGE_LOOP('',(#51221,#51222,#51223,#51224));
#12205=EDGE_LOOP('',(#51225,#51226,#51227,#51228));
#12206=EDGE_LOOP('',(#51229,#51230,#51231,#51232));
#12207=EDGE_LOOP('',(#51233,#51234,#51235,#51236));
#12208=EDGE_LOOP('',(#51237,#51238,#51239,#51240));
#12209=EDGE_LOOP('',(#51241,#51242,#51243,#51244));
#12210=EDGE_LOOP('',(#51245,#51246,#51247,#51248));
#12211=EDGE_LOOP('',(#51249,#51250,#51251,#51252));
#12212=EDGE_LOOP('',(#51253,#51254,#51255,#51256));
#12213=EDGE_LOOP('',(#51257,#51258,#51259,#51260));
#12214=EDGE_LOOP('',(#51261,#51262,#51263,#51264));
#12215=EDGE_LOOP('',(#51265,#51266,#51267,#51268));
#12216=EDGE_LOOP('',(#51269,#51270,#51271,#51272));
#12217=EDGE_LOOP('',(#51273,#51274,#51275,#51276));
#12218=EDGE_LOOP('',(#51277,#51278,#51279,#51280));
#12219=EDGE_LOOP('',(#51281,#51282,#51283,#51284));
#12220=EDGE_LOOP('',(#51285,#51286,#51287,#51288));
#12221=EDGE_LOOP('',(#51289,#51290,#51291,#51292));
#12222=EDGE_LOOP('',(#51293,#51294,#51295,#51296));
#12223=EDGE_LOOP('',(#51297,#51298,#51299,#51300));
#12224=EDGE_LOOP('',(#51301,#51302,#51303,#51304));
#12225=EDGE_LOOP('',(#51305,#51306,#51307,#51308));
#12226=EDGE_LOOP('',(#51309,#51310,#51311,#51312));
#12227=EDGE_LOOP('',(#51313,#51314,#51315,#51316));
#12228=EDGE_LOOP('',(#51317,#51318,#51319,#51320));
#12229=EDGE_LOOP('',(#51321,#51322,#51323,#51324));
#12230=EDGE_LOOP('',(#51325,#51326,#51327,#51328));
#12231=EDGE_LOOP('',(#51329,#51330,#51331,#51332));
#12232=EDGE_LOOP('',(#51333,#51334,#51335,#51336));
#12233=EDGE_LOOP('',(#51337,#51338,#51339,#51340));
#12234=EDGE_LOOP('',(#51341,#51342,#51343,#51344));
#12235=EDGE_LOOP('',(#51345,#51346,#51347,#51348));
#12236=EDGE_LOOP('',(#51349,#51350,#51351,#51352));
#12237=EDGE_LOOP('',(#51353,#51354,#51355,#51356));
#12238=EDGE_LOOP('',(#51357,#51358,#51359,#51360));
#12239=EDGE_LOOP('',(#51361,#51362,#51363,#51364));
#12240=EDGE_LOOP('',(#51365,#51366,#51367,#51368));
#12241=EDGE_LOOP('',(#51369,#51370,#51371,#51372));
#12242=EDGE_LOOP('',(#51373,#51374,#51375,#51376));
#12243=EDGE_LOOP('',(#51377,#51378,#51379,#51380));
#12244=EDGE_LOOP('',(#51381,#51382,#51383,#51384));
#12245=EDGE_LOOP('',(#51385,#51386,#51387,#51388));
#12246=EDGE_LOOP('',(#51389,#51390,#51391,#51392));
#12247=EDGE_LOOP('',(#51393,#51394,#51395,#51396));
#12248=EDGE_LOOP('',(#51397,#51398,#51399,#51400));
#12249=EDGE_LOOP('',(#51401,#51402,#51403,#51404));
#12250=EDGE_LOOP('',(#51405,#51406,#51407,#51408));
#12251=EDGE_LOOP('',(#51409,#51410,#51411,#51412));
#12252=EDGE_LOOP('',(#51413,#51414,#51415,#51416));
#12253=EDGE_LOOP('',(#51417,#51418,#51419,#51420));
#12254=EDGE_LOOP('',(#51421,#51422,#51423,#51424));
#12255=EDGE_LOOP('',(#51425,#51426,#51427,#51428));
#12256=EDGE_LOOP('',(#51429,#51430,#51431,#51432));
#12257=EDGE_LOOP('',(#51433,#51434,#51435,#51436));
#12258=EDGE_LOOP('',(#51437,#51438,#51439,#51440));
#12259=EDGE_LOOP('',(#51441,#51442,#51443,#51444));
#12260=EDGE_LOOP('',(#51445,#51446,#51447,#51448));
#12261=EDGE_LOOP('',(#51449,#51450,#51451,#51452));
#12262=EDGE_LOOP('',(#51453,#51454,#51455,#51456));
#12263=EDGE_LOOP('',(#51457,#51458,#51459,#51460));
#12264=EDGE_LOOP('',(#51461,#51462,#51463,#51464));
#12265=EDGE_LOOP('',(#51465,#51466,#51467,#51468));
#12266=EDGE_LOOP('',(#51469,#51470,#51471,#51472));
#12267=EDGE_LOOP('',(#51473,#51474,#51475,#51476));
#12268=EDGE_LOOP('',(#51477,#51478,#51479,#51480));
#12269=EDGE_LOOP('',(#51481,#51482,#51483,#51484));
#12270=EDGE_LOOP('',(#51485,#51486,#51487,#51488));
#12271=EDGE_LOOP('',(#51489,#51490,#51491,#51492));
#12272=EDGE_LOOP('',(#51493,#51494,#51495,#51496));
#12273=EDGE_LOOP('',(#51497,#51498,#51499,#51500));
#12274=EDGE_LOOP('',(#51501,#51502,#51503,#51504));
#12275=EDGE_LOOP('',(#51505,#51506,#51507,#51508));
#12276=EDGE_LOOP('',(#51509,#51510,#51511,#51512));
#12277=EDGE_LOOP('',(#51513,#51514,#51515,#51516));
#12278=EDGE_LOOP('',(#51517,#51518,#51519,#51520));
#12279=EDGE_LOOP('',(#51521,#51522,#51523,#51524));
#12280=EDGE_LOOP('',(#51525,#51526,#51527,#51528));
#12281=EDGE_LOOP('',(#51529,#51530,#51531,#51532));
#12282=EDGE_LOOP('',(#51533,#51534,#51535,#51536));
#12283=EDGE_LOOP('',(#51537,#51538,#51539,#51540));
#12284=EDGE_LOOP('',(#51541,#51542,#51543,#51544));
#12285=EDGE_LOOP('',(#51545,#51546,#51547,#51548));
#12286=EDGE_LOOP('',(#51549,#51550,#51551,#51552));
#12287=EDGE_LOOP('',(#51553,#51554,#51555,#51556));
#12288=EDGE_LOOP('',(#51557,#51558,#51559,#51560));
#12289=EDGE_LOOP('',(#51561,#51562,#51563,#51564));
#12290=EDGE_LOOP('',(#51565,#51566,#51567,#51568));
#12291=EDGE_LOOP('',(#51569,#51570,#51571,#51572));
#12292=EDGE_LOOP('',(#51573,#51574,#51575,#51576));
#12293=EDGE_LOOP('',(#51577,#51578,#51579,#51580));
#12294=EDGE_LOOP('',(#51581,#51582,#51583,#51584));
#12295=EDGE_LOOP('',(#51585,#51586,#51587,#51588));
#12296=EDGE_LOOP('',(#51589,#51590,#51591,#51592));
#12297=EDGE_LOOP('',(#51593,#51594,#51595,#51596));
#12298=EDGE_LOOP('',(#51597,#51598,#51599,#51600));
#12299=EDGE_LOOP('',(#51601,#51602,#51603,#51604));
#12300=EDGE_LOOP('',(#51605,#51606,#51607,#51608));
#12301=EDGE_LOOP('',(#51609,#51610,#51611,#51612));
#12302=EDGE_LOOP('',(#51613,#51614,#51615,#51616));
#12303=EDGE_LOOP('',(#51617,#51618,#51619,#51620));
#12304=EDGE_LOOP('',(#51621,#51622,#51623,#51624));
#12305=EDGE_LOOP('',(#51625,#51626,#51627,#51628));
#12306=EDGE_LOOP('',(#51629,#51630,#51631,#51632));
#12307=EDGE_LOOP('',(#51633,#51634,#51635,#51636));
#12308=EDGE_LOOP('',(#51637,#51638,#51639,#51640));
#12309=EDGE_LOOP('',(#51641,#51642,#51643,#51644));
#12310=EDGE_LOOP('',(#51645,#51646,#51647,#51648));
#12311=EDGE_LOOP('',(#51649,#51650,#51651,#51652));
#12312=EDGE_LOOP('',(#51653,#51654,#51655,#51656));
#12313=EDGE_LOOP('',(#51657,#51658,#51659,#51660));
#12314=EDGE_LOOP('',(#51661,#51662,#51663,#51664));
#12315=EDGE_LOOP('',(#51665,#51666,#51667,#51668));
#12316=EDGE_LOOP('',(#51669,#51670,#51671,#51672));
#12317=EDGE_LOOP('',(#51673,#51674,#51675,#51676));
#12318=EDGE_LOOP('',(#51677,#51678,#51679,#51680));
#12319=EDGE_LOOP('',(#51681,#51682,#51683,#51684));
#12320=EDGE_LOOP('',(#51685,#51686,#51687,#51688));
#12321=EDGE_LOOP('',(#51689,#51690,#51691,#51692));
#12322=EDGE_LOOP('',(#51693,#51694,#51695,#51696));
#12323=EDGE_LOOP('',(#51697,#51698,#51699,#51700));
#12324=EDGE_LOOP('',(#51701,#51702,#51703,#51704));
#12325=EDGE_LOOP('',(#51705,#51706,#51707,#51708));
#12326=EDGE_LOOP('',(#51709,#51710,#51711,#51712));
#12327=EDGE_LOOP('',(#51713,#51714,#51715,#51716));
#12328=EDGE_LOOP('',(#51717,#51718,#51719,#51720));
#12329=EDGE_LOOP('',(#51721,#51722,#51723,#51724));
#12330=EDGE_LOOP('',(#51725,#51726,#51727,#51728));
#12331=EDGE_LOOP('',(#51729,#51730,#51731,#51732));
#12332=EDGE_LOOP('',(#51733,#51734,#51735,#51736));
#12333=EDGE_LOOP('',(#51737,#51738,#51739,#51740));
#12334=EDGE_LOOP('',(#51741,#51742,#51743,#51744));
#12335=EDGE_LOOP('',(#51745,#51746,#51747,#51748));
#12336=EDGE_LOOP('',(#51749,#51750,#51751,#51752));
#12337=EDGE_LOOP('',(#51753,#51754,#51755,#51756));
#12338=EDGE_LOOP('',(#51757,#51758,#51759,#51760));
#12339=EDGE_LOOP('',(#51761,#51762,#51763,#51764));
#12340=EDGE_LOOP('',(#51765,#51766,#51767,#51768));
#12341=EDGE_LOOP('',(#51769,#51770,#51771,#51772));
#12342=EDGE_LOOP('',(#51773,#51774,#51775,#51776));
#12343=EDGE_LOOP('',(#51777,#51778,#51779,#51780));
#12344=EDGE_LOOP('',(#51781,#51782,#51783,#51784));
#12345=EDGE_LOOP('',(#51785,#51786,#51787,#51788));
#12346=EDGE_LOOP('',(#51789,#51790,#51791,#51792));
#12347=EDGE_LOOP('',(#51793,#51794,#51795,#51796));
#12348=EDGE_LOOP('',(#51797,#51798,#51799,#51800));
#12349=EDGE_LOOP('',(#51801,#51802,#51803,#51804));
#12350=EDGE_LOOP('',(#51805,#51806,#51807,#51808));
#12351=EDGE_LOOP('',(#51809,#51810,#51811,#51812));
#12352=EDGE_LOOP('',(#51813,#51814,#51815,#51816));
#12353=EDGE_LOOP('',(#51817,#51818,#51819,#51820));
#12354=EDGE_LOOP('',(#51821,#51822,#51823,#51824));
#12355=EDGE_LOOP('',(#51825,#51826,#51827,#51828));
#12356=EDGE_LOOP('',(#51829,#51830,#51831,#51832));
#12357=EDGE_LOOP('',(#51833,#51834,#51835,#51836));
#12358=EDGE_LOOP('',(#51837,#51838,#51839,#51840));
#12359=EDGE_LOOP('',(#51841,#51842,#51843,#51844));
#12360=EDGE_LOOP('',(#51845,#51846,#51847,#51848));
#12361=EDGE_LOOP('',(#51849,#51850,#51851,#51852));
#12362=EDGE_LOOP('',(#51853,#51854,#51855,#51856));
#12363=EDGE_LOOP('',(#51857,#51858,#51859,#51860));
#12364=EDGE_LOOP('',(#51861,#51862,#51863,#51864));
#12365=EDGE_LOOP('',(#51865,#51866,#51867,#51868));
#12366=EDGE_LOOP('',(#51869,#51870,#51871,#51872));
#12367=EDGE_LOOP('',(#51873,#51874,#51875,#51876));
#12368=EDGE_LOOP('',(#51877,#51878,#51879,#51880));
#12369=EDGE_LOOP('',(#51881,#51882,#51883,#51884));
#12370=EDGE_LOOP('',(#51885,#51886,#51887,#51888));
#12371=EDGE_LOOP('',(#51889,#51890,#51891,#51892));
#12372=EDGE_LOOP('',(#51893,#51894,#51895,#51896));
#12373=EDGE_LOOP('',(#51897,#51898,#51899,#51900));
#12374=EDGE_LOOP('',(#51901,#51902,#51903,#51904));
#12375=EDGE_LOOP('',(#51905,#51906,#51907,#51908));
#12376=EDGE_LOOP('',(#51909,#51910,#51911,#51912));
#12377=EDGE_LOOP('',(#51913,#51914,#51915,#51916));
#12378=EDGE_LOOP('',(#51917,#51918,#51919,#51920));
#12379=EDGE_LOOP('',(#51921,#51922,#51923,#51924));
#12380=EDGE_LOOP('',(#51925,#51926,#51927,#51928));
#12381=EDGE_LOOP('',(#51929,#51930,#51931,#51932));
#12382=EDGE_LOOP('',(#51933,#51934,#51935,#51936));
#12383=EDGE_LOOP('',(#51937,#51938,#51939,#51940));
#12384=EDGE_LOOP('',(#51941,#51942,#51943,#51944));
#12385=EDGE_LOOP('',(#51945,#51946,#51947,#51948));
#12386=EDGE_LOOP('',(#51949,#51950,#51951,#51952));
#12387=EDGE_LOOP('',(#51953,#51954,#51955,#51956));
#12388=EDGE_LOOP('',(#51957,#51958,#51959,#51960));
#12389=EDGE_LOOP('',(#51961,#51962,#51963,#51964));
#12390=EDGE_LOOP('',(#51965,#51966,#51967,#51968));
#12391=EDGE_LOOP('',(#51969,#51970,#51971,#51972));
#12392=EDGE_LOOP('',(#51973,#51974,#51975,#51976));
#12393=EDGE_LOOP('',(#51977,#51978,#51979,#51980));
#12394=EDGE_LOOP('',(#51981,#51982,#51983,#51984));
#12395=EDGE_LOOP('',(#51985,#51986,#51987,#51988));
#12396=EDGE_LOOP('',(#51989,#51990,#51991,#51992));
#12397=EDGE_LOOP('',(#51993,#51994,#51995,#51996));
#12398=EDGE_LOOP('',(#51997,#51998,#51999,#52000));
#12399=EDGE_LOOP('',(#52001,#52002,#52003,#52004));
#12400=EDGE_LOOP('',(#52005,#52006,#52007,#52008));
#12401=EDGE_LOOP('',(#52009,#52010,#52011,#52012));
#12402=EDGE_LOOP('',(#52013,#52014,#52015,#52016));
#12403=EDGE_LOOP('',(#52017,#52018,#52019,#52020));
#12404=EDGE_LOOP('',(#52021,#52022,#52023,#52024));
#12405=EDGE_LOOP('',(#52025,#52026,#52027,#52028));
#12406=EDGE_LOOP('',(#52029,#52030,#52031,#52032));
#12407=EDGE_LOOP('',(#52033,#52034,#52035,#52036));
#12408=EDGE_LOOP('',(#52037,#52038,#52039,#52040));
#12409=EDGE_LOOP('',(#52041,#52042,#52043,#52044));
#12410=EDGE_LOOP('',(#52045,#52046,#52047,#52048));
#12411=EDGE_LOOP('',(#52049,#52050,#52051,#52052));
#12412=EDGE_LOOP('',(#52053,#52054,#52055,#52056));
#12413=EDGE_LOOP('',(#52057,#52058,#52059,#52060));
#12414=EDGE_LOOP('',(#52061,#52062,#52063,#52064));
#12415=EDGE_LOOP('',(#52065,#52066,#52067,#52068));
#12416=EDGE_LOOP('',(#52069,#52070,#52071,#52072));
#12417=EDGE_LOOP('',(#52073,#52074,#52075,#52076));
#12418=EDGE_LOOP('',(#52077,#52078,#52079,#52080));
#12419=EDGE_LOOP('',(#52081,#52082,#52083,#52084));
#12420=EDGE_LOOP('',(#52085,#52086,#52087,#52088));
#12421=EDGE_LOOP('',(#52089,#52090,#52091,#52092));
#12422=EDGE_LOOP('',(#52093,#52094,#52095,#52096));
#12423=EDGE_LOOP('',(#52097,#52098,#52099,#52100));
#12424=EDGE_LOOP('',(#52101,#52102,#52103,#52104));
#12425=EDGE_LOOP('',(#52105,#52106,#52107,#52108));
#12426=EDGE_LOOP('',(#52109,#52110,#52111,#52112));
#12427=EDGE_LOOP('',(#52113,#52114,#52115,#52116));
#12428=EDGE_LOOP('',(#52117,#52118,#52119,#52120));
#12429=EDGE_LOOP('',(#52121,#52122,#52123,#52124));
#12430=EDGE_LOOP('',(#52125,#52126,#52127,#52128));
#12431=EDGE_LOOP('',(#52129,#52130,#52131,#52132));
#12432=EDGE_LOOP('',(#52133,#52134,#52135,#52136));
#12433=EDGE_LOOP('',(#52137,#52138,#52139,#52140));
#12434=EDGE_LOOP('',(#52141,#52142,#52143,#52144));
#12435=EDGE_LOOP('',(#52145,#52146,#52147,#52148));
#12436=EDGE_LOOP('',(#52149,#52150,#52151,#52152));
#12437=EDGE_LOOP('',(#52153,#52154,#52155,#52156));
#12438=EDGE_LOOP('',(#52157,#52158,#52159,#52160));
#12439=EDGE_LOOP('',(#52161,#52162,#52163,#52164));
#12440=EDGE_LOOP('',(#52165,#52166,#52167,#52168));
#12441=EDGE_LOOP('',(#52169,#52170,#52171,#52172));
#12442=EDGE_LOOP('',(#52173,#52174,#52175,#52176));
#12443=EDGE_LOOP('',(#52177,#52178,#52179,#52180));
#12444=EDGE_LOOP('',(#52181,#52182,#52183,#52184));
#12445=EDGE_LOOP('',(#52185,#52186,#52187,#52188));
#12446=EDGE_LOOP('',(#52189,#52190,#52191,#52192));
#12447=EDGE_LOOP('',(#52193,#52194,#52195,#52196));
#12448=EDGE_LOOP('',(#52197,#52198,#52199,#52200));
#12449=EDGE_LOOP('',(#52201,#52202,#52203,#52204));
#12450=EDGE_LOOP('',(#52205,#52206,#52207,#52208));
#12451=EDGE_LOOP('',(#52209,#52210,#52211,#52212));
#12452=EDGE_LOOP('',(#52213,#52214,#52215,#52216));
#12453=EDGE_LOOP('',(#52217,#52218,#52219,#52220));
#12454=EDGE_LOOP('',(#52221,#52222,#52223,#52224));
#12455=EDGE_LOOP('',(#52225,#52226,#52227,#52228));
#12456=EDGE_LOOP('',(#52229,#52230,#52231,#52232));
#12457=EDGE_LOOP('',(#52233,#52234,#52235,#52236));
#12458=EDGE_LOOP('',(#52237,#52238,#52239,#52240));
#12459=EDGE_LOOP('',(#52241,#52242,#52243,#52244));
#12460=EDGE_LOOP('',(#52245,#52246,#52247,#52248));
#12461=EDGE_LOOP('',(#52249,#52250,#52251,#52252));
#12462=EDGE_LOOP('',(#52253,#52254,#52255,#52256));
#12463=EDGE_LOOP('',(#52257,#52258,#52259,#52260));
#12464=EDGE_LOOP('',(#52261,#52262,#52263,#52264));
#12465=EDGE_LOOP('',(#52265,#52266,#52267,#52268));
#12466=EDGE_LOOP('',(#52269,#52270,#52271,#52272));
#12467=EDGE_LOOP('',(#52273,#52274,#52275,#52276));
#12468=EDGE_LOOP('',(#52277,#52278,#52279,#52280));
#12469=EDGE_LOOP('',(#52281,#52282,#52283,#52284));
#12470=EDGE_LOOP('',(#52285,#52286,#52287,#52288));
#12471=EDGE_LOOP('',(#52289,#52290,#52291,#52292));
#12472=EDGE_LOOP('',(#52293,#52294,#52295,#52296));
#12473=EDGE_LOOP('',(#52297,#52298,#52299,#52300));
#12474=EDGE_LOOP('',(#52301,#52302,#52303,#52304));
#12475=EDGE_LOOP('',(#52305,#52306,#52307,#52308));
#12476=EDGE_LOOP('',(#52309,#52310,#52311,#52312));
#12477=EDGE_LOOP('',(#52313,#52314,#52315,#52316));
#12478=EDGE_LOOP('',(#52317,#52318,#52319,#52320));
#12479=EDGE_LOOP('',(#52321,#52322,#52323,#52324));
#12480=EDGE_LOOP('',(#52325,#52326,#52327,#52328));
#12481=EDGE_LOOP('',(#52329,#52330,#52331,#52332));
#12482=EDGE_LOOP('',(#52333,#52334,#52335,#52336));
#12483=EDGE_LOOP('',(#52337,#52338,#52339,#52340));
#12484=EDGE_LOOP('',(#52341,#52342,#52343,#52344));
#12485=EDGE_LOOP('',(#52345,#52346,#52347,#52348));
#12486=EDGE_LOOP('',(#52349,#52350,#52351,#52352));
#12487=EDGE_LOOP('',(#52353,#52354,#52355,#52356));
#12488=EDGE_LOOP('',(#52357,#52358,#52359,#52360));
#12489=EDGE_LOOP('',(#52361,#52362,#52363,#52364));
#12490=EDGE_LOOP('',(#52365,#52366,#52367,#52368));
#12491=EDGE_LOOP('',(#52369,#52370,#52371,#52372));
#12492=EDGE_LOOP('',(#52373,#52374,#52375,#52376));
#12493=EDGE_LOOP('',(#52377,#52378,#52379,#52380));
#12494=EDGE_LOOP('',(#52381,#52382,#52383,#52384));
#12495=EDGE_LOOP('',(#52385,#52386,#52387,#52388));
#12496=EDGE_LOOP('',(#52389,#52390,#52391,#52392));
#12497=EDGE_LOOP('',(#52393,#52394,#52395,#52396));
#12498=EDGE_LOOP('',(#52397,#52398,#52399,#52400));
#12499=EDGE_LOOP('',(#52401,#52402,#52403,#52404));
#12500=EDGE_LOOP('',(#52405,#52406,#52407,#52408));
#12501=EDGE_LOOP('',(#52409,#52410,#52411,#52412));
#12502=EDGE_LOOP('',(#52413,#52414,#52415,#52416));
#12503=EDGE_LOOP('',(#52417,#52418,#52419,#52420));
#12504=EDGE_LOOP('',(#52421,#52422,#52423,#52424));
#12505=EDGE_LOOP('',(#52425,#52426,#52427,#52428));
#12506=EDGE_LOOP('',(#52429,#52430,#52431,#52432));
#12507=EDGE_LOOP('',(#52433,#52434,#52435,#52436));
#12508=EDGE_LOOP('',(#52437,#52438,#52439,#52440));
#12509=EDGE_LOOP('',(#52441,#52442,#52443,#52444));
#12510=EDGE_LOOP('',(#52445,#52446,#52447,#52448));
#12511=EDGE_LOOP('',(#52449,#52450,#52451,#52452));
#12512=EDGE_LOOP('',(#52453,#52454,#52455,#52456));
#12513=EDGE_LOOP('',(#52457,#52458,#52459,#52460));
#12514=EDGE_LOOP('',(#52461,#52462,#52463,#52464));
#12515=EDGE_LOOP('',(#52465,#52466,#52467,#52468));
#12516=EDGE_LOOP('',(#52469,#52470,#52471,#52472));
#12517=EDGE_LOOP('',(#52473,#52474,#52475,#52476));
#12518=EDGE_LOOP('',(#52477,#52478,#52479,#52480));
#12519=EDGE_LOOP('',(#52481,#52482,#52483,#52484));
#12520=EDGE_LOOP('',(#52485,#52486,#52487,#52488));
#12521=EDGE_LOOP('',(#52489,#52490,#52491,#52492));
#12522=EDGE_LOOP('',(#52493,#52494,#52495,#52496));
#12523=EDGE_LOOP('',(#52497,#52498,#52499,#52500));
#12524=EDGE_LOOP('',(#52501,#52502,#52503,#52504));
#12525=EDGE_LOOP('',(#52505,#52506,#52507,#52508));
#12526=EDGE_LOOP('',(#52509,#52510,#52511,#52512));
#12527=EDGE_LOOP('',(#52513,#52514,#52515,#52516));
#12528=EDGE_LOOP('',(#52517,#52518,#52519,#52520));
#12529=EDGE_LOOP('',(#52521,#52522,#52523,#52524));
#12530=EDGE_LOOP('',(#52525,#52526,#52527,#52528));
#12531=EDGE_LOOP('',(#52529,#52530,#52531,#52532));
#12532=EDGE_LOOP('',(#52533,#52534,#52535,#52536));
#12533=EDGE_LOOP('',(#52537,#52538,#52539,#52540));
#12534=EDGE_LOOP('',(#52541,#52542,#52543,#52544));
#12535=EDGE_LOOP('',(#52545,#52546,#52547,#52548));
#12536=EDGE_LOOP('',(#52549,#52550,#52551,#52552));
#12537=EDGE_LOOP('',(#52553,#52554,#52555,#52556));
#12538=EDGE_LOOP('',(#52557,#52558,#52559,#52560));
#12539=EDGE_LOOP('',(#52561,#52562,#52563,#52564));
#12540=EDGE_LOOP('',(#52565,#52566,#52567,#52568));
#12541=EDGE_LOOP('',(#52569,#52570,#52571,#52572));
#12542=EDGE_LOOP('',(#52573,#52574,#52575,#52576));
#12543=EDGE_LOOP('',(#52577,#52578,#52579,#52580));
#12544=EDGE_LOOP('',(#52581,#52582,#52583,#52584));
#12545=EDGE_LOOP('',(#52585,#52586,#52587,#52588));
#12546=EDGE_LOOP('',(#52589,#52590,#52591,#52592));
#12547=EDGE_LOOP('',(#52593,#52594,#52595,#52596));
#12548=EDGE_LOOP('',(#52597,#52598,#52599,#52600));
#12549=EDGE_LOOP('',(#52601,#52602,#52603,#52604));
#12550=EDGE_LOOP('',(#52605,#52606,#52607,#52608));
#12551=EDGE_LOOP('',(#52609,#52610,#52611,#52612));
#12552=EDGE_LOOP('',(#52613,#52614,#52615,#52616));
#12553=EDGE_LOOP('',(#52617,#52618,#52619,#52620));
#12554=EDGE_LOOP('',(#52621,#52622,#52623,#52624));
#12555=EDGE_LOOP('',(#52625,#52626,#52627,#52628));
#12556=EDGE_LOOP('',(#52629,#52630,#52631,#52632));
#12557=EDGE_LOOP('',(#52633,#52634,#52635,#52636));
#12558=EDGE_LOOP('',(#52637,#52638,#52639,#52640));
#12559=EDGE_LOOP('',(#52641,#52642,#52643,#52644));
#12560=EDGE_LOOP('',(#52645,#52646,#52647,#52648));
#12561=EDGE_LOOP('',(#52649,#52650,#52651,#52652));
#12562=EDGE_LOOP('',(#52653,#52654,#52655,#52656));
#12563=EDGE_LOOP('',(#52657,#52658,#52659,#52660));
#12564=EDGE_LOOP('',(#52661,#52662,#52663,#52664));
#12565=EDGE_LOOP('',(#52665,#52666,#52667,#52668));
#12566=EDGE_LOOP('',(#52669,#52670,#52671,#52672));
#12567=EDGE_LOOP('',(#52673,#52674,#52675,#52676));
#12568=EDGE_LOOP('',(#52677,#52678,#52679,#52680));
#12569=EDGE_LOOP('',(#52681,#52682,#52683,#52684));
#12570=EDGE_LOOP('',(#52685,#52686,#52687,#52688));
#12571=EDGE_LOOP('',(#52689,#52690,#52691,#52692));
#12572=EDGE_LOOP('',(#52693,#52694,#52695,#52696));
#12573=EDGE_LOOP('',(#52697,#52698,#52699,#52700));
#12574=EDGE_LOOP('',(#52701,#52702,#52703,#52704));
#12575=EDGE_LOOP('',(#52705,#52706,#52707,#52708));
#12576=EDGE_LOOP('',(#52709,#52710,#52711,#52712));
#12577=EDGE_LOOP('',(#52713,#52714,#52715,#52716));
#12578=EDGE_LOOP('',(#52717,#52718,#52719,#52720));
#12579=EDGE_LOOP('',(#52721,#52722,#52723,#52724));
#12580=EDGE_LOOP('',(#52725,#52726,#52727,#52728));
#12581=EDGE_LOOP('',(#52729,#52730,#52731,#52732));
#12582=EDGE_LOOP('',(#52733,#52734,#52735,#52736));
#12583=EDGE_LOOP('',(#52737,#52738,#52739,#52740));
#12584=EDGE_LOOP('',(#52741,#52742,#52743,#52744));
#12585=EDGE_LOOP('',(#52745,#52746,#52747,#52748));
#12586=EDGE_LOOP('',(#52749,#52750,#52751,#52752));
#12587=EDGE_LOOP('',(#52753,#52754,#52755,#52756));
#12588=EDGE_LOOP('',(#52757,#52758,#52759,#52760));
#12589=EDGE_LOOP('',(#52761,#52762,#52763,#52764));
#12590=EDGE_LOOP('',(#52765,#52766,#52767,#52768));
#12591=EDGE_LOOP('',(#52769,#52770,#52771,#52772));
#12592=EDGE_LOOP('',(#52773,#52774,#52775,#52776));
#12593=EDGE_LOOP('',(#52777,#52778,#52779,#52780));
#12594=EDGE_LOOP('',(#52781,#52782,#52783,#52784));
#12595=EDGE_LOOP('',(#52785,#52786,#52787,#52788));
#12596=EDGE_LOOP('',(#52789,#52790,#52791,#52792));
#12597=EDGE_LOOP('',(#52793,#52794,#52795,#52796));
#12598=EDGE_LOOP('',(#52797,#52798,#52799,#52800));
#12599=EDGE_LOOP('',(#52801,#52802,#52803,#52804));
#12600=EDGE_LOOP('',(#52805,#52806,#52807,#52808));
#12601=EDGE_LOOP('',(#52809,#52810,#52811,#52812));
#12602=EDGE_LOOP('',(#52813,#52814,#52815,#52816));
#12603=EDGE_LOOP('',(#52817,#52818,#52819,#52820));
#12604=EDGE_LOOP('',(#52821,#52822,#52823,#52824));
#12605=EDGE_LOOP('',(#52825,#52826,#52827,#52828));
#12606=EDGE_LOOP('',(#52829,#52830,#52831,#52832));
#12607=EDGE_LOOP('',(#52833,#52834,#52835,#52836));
#12608=EDGE_LOOP('',(#52837,#52838,#52839,#52840));
#12609=EDGE_LOOP('',(#52841,#52842,#52843,#52844));
#12610=EDGE_LOOP('',(#52845,#52846,#52847,#52848));
#12611=EDGE_LOOP('',(#52849,#52850,#52851,#52852));
#12612=EDGE_LOOP('',(#52853,#52854,#52855,#52856));
#12613=EDGE_LOOP('',(#52857,#52858,#52859,#52860));
#12614=EDGE_LOOP('',(#52861,#52862,#52863,#52864));
#12615=EDGE_LOOP('',(#52865,#52866,#52867,#52868));
#12616=EDGE_LOOP('',(#52869,#52870,#52871,#52872));
#12617=EDGE_LOOP('',(#52873,#52874,#52875,#52876));
#12618=EDGE_LOOP('',(#52877,#52878,#52879,#52880));
#12619=EDGE_LOOP('',(#52881,#52882,#52883,#52884));
#12620=EDGE_LOOP('',(#52885,#52886,#52887,#52888));
#12621=EDGE_LOOP('',(#52889,#52890,#52891,#52892));
#12622=EDGE_LOOP('',(#52893,#52894,#52895,#52896));
#12623=EDGE_LOOP('',(#52897,#52898,#52899,#52900));
#12624=EDGE_LOOP('',(#52901,#52902,#52903,#52904));
#12625=EDGE_LOOP('',(#52905,#52906,#52907,#52908));
#12626=EDGE_LOOP('',(#52909,#52910,#52911,#52912));
#12627=EDGE_LOOP('',(#52913,#52914,#52915,#52916));
#12628=EDGE_LOOP('',(#52917,#52918,#52919,#52920));
#12629=EDGE_LOOP('',(#52921,#52922,#52923,#52924));
#12630=EDGE_LOOP('',(#52925,#52926,#52927,#52928));
#12631=EDGE_LOOP('',(#52929,#52930,#52931,#52932));
#12632=EDGE_LOOP('',(#52933,#52934,#52935,#52936));
#12633=EDGE_LOOP('',(#52937,#52938,#52939,#52940));
#12634=EDGE_LOOP('',(#52941,#52942,#52943,#52944));
#12635=EDGE_LOOP('',(#52945,#52946,#52947,#52948));
#12636=EDGE_LOOP('',(#52949,#52950,#52951,#52952));
#12637=EDGE_LOOP('',(#52953,#52954,#52955,#52956));
#12638=EDGE_LOOP('',(#52957,#52958,#52959,#52960));
#12639=EDGE_LOOP('',(#52961,#52962,#52963,#52964));
#12640=EDGE_LOOP('',(#52965,#52966,#52967,#52968));
#12641=EDGE_LOOP('',(#52969,#52970,#52971,#52972));
#12642=EDGE_LOOP('',(#52973,#52974,#52975,#52976));
#12643=EDGE_LOOP('',(#52977,#52978,#52979,#52980));
#12644=EDGE_LOOP('',(#52981,#52982,#52983,#52984));
#12645=EDGE_LOOP('',(#52985,#52986,#52987,#52988));
#12646=EDGE_LOOP('',(#52989,#52990,#52991,#52992));
#12647=EDGE_LOOP('',(#52993,#52994,#52995,#52996));
#12648=EDGE_LOOP('',(#52997,#52998,#52999,#53000));
#12649=EDGE_LOOP('',(#53001,#53002,#53003,#53004));
#12650=EDGE_LOOP('',(#53005,#53006,#53007,#53008));
#12651=EDGE_LOOP('',(#53009,#53010,#53011,#53012));
#12652=EDGE_LOOP('',(#53013,#53014,#53015,#53016));
#12653=EDGE_LOOP('',(#53017,#53018,#53019,#53020));
#12654=EDGE_LOOP('',(#53021,#53022,#53023,#53024));
#12655=EDGE_LOOP('',(#53025,#53026,#53027,#53028));
#12656=EDGE_LOOP('',(#53029,#53030,#53031,#53032));
#12657=EDGE_LOOP('',(#53033,#53034,#53035,#53036));
#12658=EDGE_LOOP('',(#53037,#53038,#53039,#53040));
#12659=EDGE_LOOP('',(#53041,#53042,#53043,#53044));
#12660=EDGE_LOOP('',(#53045,#53046,#53047,#53048));
#12661=EDGE_LOOP('',(#53049,#53050,#53051,#53052));
#12662=EDGE_LOOP('',(#53053,#53054,#53055,#53056));
#12663=EDGE_LOOP('',(#53057,#53058,#53059,#53060));
#12664=EDGE_LOOP('',(#53061,#53062,#53063,#53064));
#12665=EDGE_LOOP('',(#53065,#53066,#53067,#53068));
#12666=EDGE_LOOP('',(#53069,#53070,#53071,#53072));
#12667=EDGE_LOOP('',(#53073,#53074,#53075,#53076));
#12668=EDGE_LOOP('',(#53077,#53078,#53079,#53080));
#12669=EDGE_LOOP('',(#53081,#53082,#53083,#53084));
#12670=EDGE_LOOP('',(#53085,#53086,#53087,#53088));
#12671=EDGE_LOOP('',(#53089,#53090,#53091,#53092));
#12672=EDGE_LOOP('',(#53093,#53094,#53095,#53096));
#12673=EDGE_LOOP('',(#53097,#53098,#53099,#53100));
#12674=EDGE_LOOP('',(#53101,#53102,#53103,#53104));
#12675=EDGE_LOOP('',(#53105,#53106,#53107,#53108));
#12676=EDGE_LOOP('',(#53109,#53110,#53111,#53112));
#12677=EDGE_LOOP('',(#53113,#53114,#53115,#53116));
#12678=EDGE_LOOP('',(#53117,#53118,#53119,#53120));
#12679=EDGE_LOOP('',(#53121,#53122,#53123,#53124));
#12680=EDGE_LOOP('',(#53125,#53126,#53127,#53128));
#12681=EDGE_LOOP('',(#53129,#53130,#53131,#53132));
#12682=EDGE_LOOP('',(#53133,#53134,#53135,#53136));
#12683=EDGE_LOOP('',(#53137,#53138,#53139,#53140));
#12684=EDGE_LOOP('',(#53141,#53142,#53143,#53144));
#12685=EDGE_LOOP('',(#53145,#53146,#53147,#53148));
#12686=EDGE_LOOP('',(#53149,#53150,#53151,#53152));
#12687=EDGE_LOOP('',(#53153,#53154,#53155,#53156));
#12688=EDGE_LOOP('',(#53157,#53158,#53159,#53160));
#12689=EDGE_LOOP('',(#53161,#53162,#53163,#53164));
#12690=EDGE_LOOP('',(#53165,#53166,#53167,#53168));
#12691=EDGE_LOOP('',(#53169,#53170,#53171,#53172));
#12692=EDGE_LOOP('',(#53173,#53174,#53175,#53176));
#12693=EDGE_LOOP('',(#53177,#53178,#53179,#53180));
#12694=EDGE_LOOP('',(#53181,#53182,#53183,#53184));
#12695=EDGE_LOOP('',(#53185,#53186,#53187,#53188));
#12696=EDGE_LOOP('',(#53189,#53190,#53191,#53192));
#12697=EDGE_LOOP('',(#53193,#53194,#53195,#53196));
#12698=EDGE_LOOP('',(#53197,#53198,#53199,#53200));
#12699=EDGE_LOOP('',(#53201,#53202,#53203,#53204));
#12700=EDGE_LOOP('',(#53205,#53206,#53207,#53208));
#12701=EDGE_LOOP('',(#53209,#53210,#53211,#53212));
#12702=EDGE_LOOP('',(#53213,#53214,#53215,#53216));
#12703=EDGE_LOOP('',(#53217,#53218,#53219,#53220));
#12704=EDGE_LOOP('',(#53221,#53222,#53223,#53224));
#12705=EDGE_LOOP('',(#53225,#53226,#53227,#53228));
#12706=EDGE_LOOP('',(#53229,#53230,#53231,#53232));
#12707=EDGE_LOOP('',(#53233,#53234,#53235,#53236));
#12708=EDGE_LOOP('',(#53237,#53238,#53239,#53240));
#12709=EDGE_LOOP('',(#53241,#53242,#53243,#53244));
#12710=EDGE_LOOP('',(#53245,#53246,#53247,#53248));
#12711=EDGE_LOOP('',(#53249,#53250,#53251,#53252));
#12712=EDGE_LOOP('',(#53253,#53254,#53255,#53256));
#12713=EDGE_LOOP('',(#53257,#53258,#53259,#53260));
#12714=EDGE_LOOP('',(#53261,#53262,#53263,#53264));
#12715=EDGE_LOOP('',(#53265,#53266,#53267,#53268));
#12716=EDGE_LOOP('',(#53269,#53270,#53271,#53272));
#12717=EDGE_LOOP('',(#53273,#53274,#53275,#53276));
#12718=EDGE_LOOP('',(#53277,#53278,#53279,#53280));
#12719=EDGE_LOOP('',(#53281,#53282,#53283,#53284));
#12720=EDGE_LOOP('',(#53285,#53286,#53287,#53288));
#12721=EDGE_LOOP('',(#53289,#53290,#53291,#53292));
#12722=EDGE_LOOP('',(#53293,#53294,#53295,#53296));
#12723=EDGE_LOOP('',(#53297,#53298,#53299,#53300));
#12724=EDGE_LOOP('',(#53301,#53302,#53303,#53304));
#12725=EDGE_LOOP('',(#53305,#53306,#53307,#53308));
#12726=EDGE_LOOP('',(#53309,#53310,#53311,#53312));
#12727=EDGE_LOOP('',(#53313,#53314,#53315,#53316));
#12728=EDGE_LOOP('',(#53317,#53318,#53319,#53320));
#12729=EDGE_LOOP('',(#53321,#53322,#53323,#53324));
#12730=EDGE_LOOP('',(#53325,#53326,#53327,#53328));
#12731=EDGE_LOOP('',(#53329,#53330,#53331,#53332));
#12732=EDGE_LOOP('',(#53333,#53334,#53335,#53336));
#12733=EDGE_LOOP('',(#53337,#53338,#53339,#53340));
#12734=EDGE_LOOP('',(#53341,#53342,#53343,#53344));
#12735=EDGE_LOOP('',(#53345,#53346,#53347,#53348));
#12736=EDGE_LOOP('',(#53349,#53350,#53351,#53352));
#12737=EDGE_LOOP('',(#53353,#53354,#53355,#53356));
#12738=EDGE_LOOP('',(#53357,#53358,#53359,#53360));
#12739=EDGE_LOOP('',(#53361,#53362,#53363,#53364));
#12740=EDGE_LOOP('',(#53365,#53366,#53367,#53368));
#12741=EDGE_LOOP('',(#53369,#53370,#53371,#53372));
#12742=EDGE_LOOP('',(#53373,#53374,#53375,#53376));
#12743=EDGE_LOOP('',(#53377,#53378,#53379,#53380));
#12744=EDGE_LOOP('',(#53381,#53382,#53383,#53384));
#12745=EDGE_LOOP('',(#53385,#53386,#53387,#53388));
#12746=EDGE_LOOP('',(#53389,#53390,#53391,#53392));
#12747=EDGE_LOOP('',(#53393,#53394,#53395,#53396));
#12748=EDGE_LOOP('',(#53397,#53398,#53399,#53400));
#12749=EDGE_LOOP('',(#53401,#53402,#53403,#53404));
#12750=EDGE_LOOP('',(#53405,#53406,#53407,#53408));
#12751=EDGE_LOOP('',(#53409,#53410,#53411,#53412));
#12752=EDGE_LOOP('',(#53413,#53414,#53415,#53416));
#12753=EDGE_LOOP('',(#53417,#53418,#53419,#53420));
#12754=EDGE_LOOP('',(#53421,#53422,#53423,#53424));
#12755=EDGE_LOOP('',(#53425,#53426,#53427,#53428));
#12756=EDGE_LOOP('',(#53429,#53430,#53431,#53432));
#12757=EDGE_LOOP('',(#53433,#53434,#53435,#53436));
#12758=EDGE_LOOP('',(#53437,#53438,#53439,#53440));
#12759=EDGE_LOOP('',(#53441,#53442,#53443,#53444));
#12760=EDGE_LOOP('',(#53445,#53446,#53447,#53448));
#12761=EDGE_LOOP('',(#53449,#53450,#53451,#53452));
#12762=EDGE_LOOP('',(#53453,#53454,#53455,#53456));
#12763=EDGE_LOOP('',(#53457,#53458,#53459,#53460));
#12764=EDGE_LOOP('',(#53461,#53462,#53463,#53464));
#12765=EDGE_LOOP('',(#53465,#53466,#53467,#53468));
#12766=EDGE_LOOP('',(#53469,#53470,#53471,#53472));
#12767=EDGE_LOOP('',(#53473,#53474,#53475,#53476));
#12768=EDGE_LOOP('',(#53477,#53478,#53479,#53480));
#12769=EDGE_LOOP('',(#53481,#53482,#53483,#53484));
#12770=EDGE_LOOP('',(#53485,#53486,#53487,#53488));
#12771=EDGE_LOOP('',(#53489,#53490,#53491,#53492));
#12772=EDGE_LOOP('',(#53493,#53494,#53495,#53496));
#12773=EDGE_LOOP('',(#53497,#53498,#53499,#53500));
#12774=EDGE_LOOP('',(#53501,#53502,#53503,#53504));
#12775=EDGE_LOOP('',(#53505,#53506,#53507,#53508));
#12776=EDGE_LOOP('',(#53509,#53510,#53511,#53512));
#12777=EDGE_LOOP('',(#53513,#53514,#53515,#53516));
#12778=EDGE_LOOP('',(#53517,#53518,#53519,#53520));
#12779=EDGE_LOOP('',(#53521,#53522,#53523,#53524));
#12780=EDGE_LOOP('',(#53525,#53526,#53527,#53528));
#12781=EDGE_LOOP('',(#53529,#53530,#53531,#53532));
#12782=EDGE_LOOP('',(#53533,#53534,#53535,#53536));
#12783=EDGE_LOOP('',(#53537,#53538,#53539,#53540));
#12784=EDGE_LOOP('',(#53541,#53542,#53543,#53544));
#12785=EDGE_LOOP('',(#53545,#53546,#53547,#53548));
#12786=EDGE_LOOP('',(#53549,#53550,#53551,#53552));
#12787=EDGE_LOOP('',(#53553,#53554,#53555,#53556));
#12788=EDGE_LOOP('',(#53557,#53558,#53559,#53560));
#12789=EDGE_LOOP('',(#53561,#53562,#53563,#53564));
#12790=EDGE_LOOP('',(#53565,#53566,#53567,#53568));
#12791=EDGE_LOOP('',(#53569,#53570,#53571,#53572));
#12792=EDGE_LOOP('',(#53573,#53574,#53575,#53576));
#12793=EDGE_LOOP('',(#53577,#53578,#53579,#53580));
#12794=EDGE_LOOP('',(#53581,#53582,#53583,#53584));
#12795=EDGE_LOOP('',(#53585,#53586,#53587,#53588));
#12796=EDGE_LOOP('',(#53589,#53590,#53591,#53592));
#12797=EDGE_LOOP('',(#53593,#53594,#53595,#53596));
#12798=EDGE_LOOP('',(#53597,#53598,#53599,#53600));
#12799=EDGE_LOOP('',(#53601,#53602,#53603,#53604));
#12800=EDGE_LOOP('',(#53605,#53606,#53607,#53608));
#12801=EDGE_LOOP('',(#53609,#53610,#53611,#53612));
#12802=EDGE_LOOP('',(#53613,#53614,#53615,#53616));
#12803=EDGE_LOOP('',(#53617,#53618,#53619,#53620));
#12804=EDGE_LOOP('',(#53621,#53622,#53623,#53624));
#12805=EDGE_LOOP('',(#53625,#53626,#53627,#53628));
#12806=EDGE_LOOP('',(#53629,#53630,#53631,#53632));
#12807=EDGE_LOOP('',(#53633,#53634,#53635,#53636));
#12808=EDGE_LOOP('',(#53637,#53638,#53639,#53640));
#12809=EDGE_LOOP('',(#53641,#53642,#53643,#53644));
#12810=EDGE_LOOP('',(#53645,#53646,#53647,#53648));
#12811=EDGE_LOOP('',(#53649,#53650,#53651,#53652));
#12812=EDGE_LOOP('',(#53653,#53654,#53655,#53656));
#12813=EDGE_LOOP('',(#53657,#53658,#53659,#53660));
#12814=EDGE_LOOP('',(#53661,#53662,#53663,#53664));
#12815=EDGE_LOOP('',(#53665,#53666,#53667,#53668));
#12816=EDGE_LOOP('',(#53669,#53670,#53671,#53672));
#12817=EDGE_LOOP('',(#53673,#53674,#53675,#53676));
#12818=EDGE_LOOP('',(#53677,#53678,#53679,#53680));
#12819=EDGE_LOOP('',(#53681,#53682,#53683,#53684));
#12820=EDGE_LOOP('',(#53685,#53686,#53687,#53688));
#12821=EDGE_LOOP('',(#53689,#53690,#53691,#53692));
#12822=EDGE_LOOP('',(#53693,#53694,#53695,#53696));
#12823=EDGE_LOOP('',(#53697,#53698,#53699,#53700));
#12824=EDGE_LOOP('',(#53701,#53702,#53703,#53704));
#12825=EDGE_LOOP('',(#53705,#53706,#53707,#53708));
#12826=EDGE_LOOP('',(#53709,#53710,#53711,#53712));
#12827=EDGE_LOOP('',(#53713,#53714,#53715,#53716));
#12828=EDGE_LOOP('',(#53717,#53718,#53719,#53720));
#12829=EDGE_LOOP('',(#53721,#53722,#53723,#53724));
#12830=EDGE_LOOP('',(#53725,#53726,#53727,#53728));
#12831=EDGE_LOOP('',(#53729,#53730,#53731,#53732));
#12832=EDGE_LOOP('',(#53733,#53734,#53735,#53736));
#12833=EDGE_LOOP('',(#53737,#53738,#53739,#53740));
#12834=EDGE_LOOP('',(#53741,#53742,#53743,#53744));
#12835=EDGE_LOOP('',(#53745,#53746,#53747,#53748));
#12836=EDGE_LOOP('',(#53749,#53750,#53751,#53752));
#12837=EDGE_LOOP('',(#53753,#53754,#53755,#53756));
#12838=EDGE_LOOP('',(#53757,#53758,#53759,#53760));
#12839=EDGE_LOOP('',(#53761,#53762,#53763,#53764));
#12840=EDGE_LOOP('',(#53765,#53766,#53767,#53768));
#12841=EDGE_LOOP('',(#53769,#53770,#53771,#53772));
#12842=EDGE_LOOP('',(#53773,#53774,#53775,#53776));
#12843=EDGE_LOOP('',(#53777,#53778,#53779,#53780));
#12844=EDGE_LOOP('',(#53781,#53782,#53783,#53784));
#12845=EDGE_LOOP('',(#53785,#53786,#53787,#53788));
#12846=EDGE_LOOP('',(#53789,#53790,#53791,#53792));
#12847=EDGE_LOOP('',(#53793,#53794,#53795,#53796));
#12848=EDGE_LOOP('',(#53797,#53798,#53799,#53800));
#12849=EDGE_LOOP('',(#53801,#53802,#53803,#53804));
#12850=EDGE_LOOP('',(#53805,#53806,#53807,#53808));
#12851=EDGE_LOOP('',(#53809,#53810,#53811,#53812));
#12852=EDGE_LOOP('',(#53813,#53814,#53815,#53816));
#12853=EDGE_LOOP('',(#53817,#53818,#53819,#53820));
#12854=EDGE_LOOP('',(#53821,#53822,#53823,#53824));
#12855=EDGE_LOOP('',(#53825,#53826,#53827,#53828));
#12856=EDGE_LOOP('',(#53829,#53830,#53831,#53832));
#12857=EDGE_LOOP('',(#53833,#53834,#53835,#53836));
#12858=EDGE_LOOP('',(#53837,#53838,#53839,#53840));
#12859=EDGE_LOOP('',(#53841,#53842,#53843,#53844));
#12860=EDGE_LOOP('',(#53845,#53846,#53847,#53848));
#12861=EDGE_LOOP('',(#53849,#53850,#53851,#53852));
#12862=EDGE_LOOP('',(#53853,#53854,#53855,#53856));
#12863=EDGE_LOOP('',(#53857,#53858,#53859,#53860));
#12864=EDGE_LOOP('',(#53861,#53862,#53863,#53864));
#12865=EDGE_LOOP('',(#53865,#53866,#53867,#53868));
#12866=EDGE_LOOP('',(#53869,#53870,#53871,#53872));
#12867=EDGE_LOOP('',(#53873,#53874,#53875,#53876));
#12868=EDGE_LOOP('',(#53877,#53878,#53879,#53880));
#12869=EDGE_LOOP('',(#53881,#53882,#53883,#53884));
#12870=EDGE_LOOP('',(#53885,#53886,#53887,#53888));
#12871=EDGE_LOOP('',(#53889,#53890,#53891,#53892));
#12872=EDGE_LOOP('',(#53893,#53894,#53895,#53896));
#12873=EDGE_LOOP('',(#53897,#53898,#53899,#53900));
#12874=EDGE_LOOP('',(#53901,#53902,#53903,#53904));
#12875=EDGE_LOOP('',(#53905,#53906,#53907,#53908));
#12876=EDGE_LOOP('',(#53909,#53910,#53911,#53912));
#12877=EDGE_LOOP('',(#53913,#53914,#53915,#53916));
#12878=EDGE_LOOP('',(#53917,#53918,#53919,#53920));
#12879=EDGE_LOOP('',(#53921,#53922,#53923,#53924));
#12880=EDGE_LOOP('',(#53925,#53926,#53927,#53928));
#12881=EDGE_LOOP('',(#53929,#53930,#53931,#53932));
#12882=EDGE_LOOP('',(#53933,#53934,#53935,#53936));
#12883=EDGE_LOOP('',(#53937,#53938,#53939,#53940));
#12884=EDGE_LOOP('',(#53941,#53942,#53943,#53944));
#12885=EDGE_LOOP('',(#53945,#53946,#53947,#53948));
#12886=EDGE_LOOP('',(#53949,#53950,#53951,#53952));
#12887=EDGE_LOOP('',(#53953,#53954,#53955,#53956));
#12888=EDGE_LOOP('',(#53957,#53958,#53959,#53960));
#12889=EDGE_LOOP('',(#53961,#53962,#53963,#53964));
#12890=EDGE_LOOP('',(#53965,#53966,#53967,#53968));
#12891=EDGE_LOOP('',(#53969,#53970,#53971,#53972));
#12892=EDGE_LOOP('',(#53973,#53974,#53975,#53976));
#12893=EDGE_LOOP('',(#53977,#53978,#53979,#53980));
#12894=EDGE_LOOP('',(#53981,#53982,#53983,#53984));
#12895=EDGE_LOOP('',(#53985,#53986,#53987,#53988));
#12896=EDGE_LOOP('',(#53989,#53990,#53991,#53992));
#12897=EDGE_LOOP('',(#53993,#53994,#53995,#53996));
#12898=EDGE_LOOP('',(#53997,#53998,#53999,#54000));
#12899=EDGE_LOOP('',(#54001,#54002,#54003,#54004));
#12900=EDGE_LOOP('',(#54005,#54006,#54007,#54008));
#12901=EDGE_LOOP('',(#54009,#54010,#54011,#54012));
#12902=EDGE_LOOP('',(#54013,#54014,#54015,#54016));
#12903=EDGE_LOOP('',(#54017,#54018,#54019,#54020));
#12904=EDGE_LOOP('',(#54021,#54022,#54023,#54024));
#12905=EDGE_LOOP('',(#54025,#54026,#54027,#54028));
#12906=EDGE_LOOP('',(#54029,#54030,#54031,#54032));
#12907=EDGE_LOOP('',(#54033,#54034,#54035,#54036));
#12908=EDGE_LOOP('',(#54037,#54038,#54039,#54040));
#12909=EDGE_LOOP('',(#54041,#54042,#54043,#54044));
#12910=EDGE_LOOP('',(#54045,#54046,#54047,#54048));
#12911=EDGE_LOOP('',(#54049,#54050,#54051,#54052));
#12912=EDGE_LOOP('',(#54053,#54054,#54055,#54056));
#12913=EDGE_LOOP('',(#54057,#54058,#54059,#54060));
#12914=EDGE_LOOP('',(#54061,#54062,#54063,#54064));
#12915=EDGE_LOOP('',(#54065,#54066,#54067,#54068));
#12916=EDGE_LOOP('',(#54069,#54070,#54071,#54072));
#12917=EDGE_LOOP('',(#54073,#54074,#54075,#54076));
#12918=EDGE_LOOP('',(#54077,#54078,#54079,#54080));
#12919=EDGE_LOOP('',(#54081,#54082,#54083,#54084));
#12920=EDGE_LOOP('',(#54085,#54086,#54087,#54088));
#12921=EDGE_LOOP('',(#54089,#54090,#54091,#54092));
#12922=EDGE_LOOP('',(#54093,#54094,#54095,#54096));
#12923=EDGE_LOOP('',(#54097,#54098,#54099,#54100));
#12924=EDGE_LOOP('',(#54101,#54102,#54103,#54104));
#12925=EDGE_LOOP('',(#54105,#54106,#54107,#54108));
#12926=EDGE_LOOP('',(#54109,#54110,#54111,#54112));
#12927=EDGE_LOOP('',(#54113,#54114,#54115,#54116));
#12928=EDGE_LOOP('',(#54117,#54118,#54119,#54120));
#12929=EDGE_LOOP('',(#54121,#54122,#54123,#54124));
#12930=EDGE_LOOP('',(#54125,#54126,#54127,#54128));
#12931=EDGE_LOOP('',(#54129,#54130,#54131,#54132));
#12932=EDGE_LOOP('',(#54133,#54134,#54135,#54136));
#12933=EDGE_LOOP('',(#54137,#54138,#54139,#54140));
#12934=EDGE_LOOP('',(#54141,#54142,#54143,#54144));
#12935=EDGE_LOOP('',(#54145,#54146,#54147,#54148));
#12936=EDGE_LOOP('',(#54149,#54150,#54151,#54152));
#12937=EDGE_LOOP('',(#54153,#54154,#54155,#54156));
#12938=EDGE_LOOP('',(#54157,#54158,#54159,#54160));
#12939=EDGE_LOOP('',(#54161,#54162,#54163,#54164));
#12940=EDGE_LOOP('',(#54165,#54166,#54167,#54168));
#12941=EDGE_LOOP('',(#54169,#54170,#54171,#54172));
#12942=EDGE_LOOP('',(#54173,#54174,#54175,#54176));
#12943=EDGE_LOOP('',(#54177,#54178,#54179,#54180));
#12944=EDGE_LOOP('',(#54181,#54182,#54183,#54184));
#12945=EDGE_LOOP('',(#54185,#54186,#54187,#54188));
#12946=EDGE_LOOP('',(#54189,#54190,#54191,#54192));
#12947=EDGE_LOOP('',(#54193,#54194,#54195,#54196));
#12948=EDGE_LOOP('',(#54197,#54198,#54199,#54200));
#12949=EDGE_LOOP('',(#54201,#54202,#54203,#54204));
#12950=EDGE_LOOP('',(#54205,#54206,#54207,#54208));
#12951=EDGE_LOOP('',(#54209,#54210,#54211,#54212));
#12952=EDGE_LOOP('',(#54213,#54214,#54215,#54216));
#12953=EDGE_LOOP('',(#54217,#54218,#54219,#54220));
#12954=EDGE_LOOP('',(#54221,#54222,#54223,#54224));
#12955=EDGE_LOOP('',(#54225,#54226,#54227,#54228));
#12956=EDGE_LOOP('',(#54229,#54230,#54231,#54232));
#12957=EDGE_LOOP('',(#54233,#54234,#54235,#54236));
#12958=EDGE_LOOP('',(#54237,#54238,#54239,#54240));
#12959=EDGE_LOOP('',(#54241,#54242,#54243,#54244));
#12960=EDGE_LOOP('',(#54245,#54246,#54247,#54248));
#12961=EDGE_LOOP('',(#54249,#54250,#54251,#54252));
#12962=EDGE_LOOP('',(#54253,#54254,#54255,#54256));
#12963=EDGE_LOOP('',(#54257,#54258,#54259,#54260));
#12964=EDGE_LOOP('',(#54261,#54262,#54263,#54264));
#12965=EDGE_LOOP('',(#54265,#54266,#54267,#54268));
#12966=EDGE_LOOP('',(#54269,#54270,#54271,#54272));
#12967=EDGE_LOOP('',(#54273,#54274,#54275,#54276));
#12968=EDGE_LOOP('',(#54277,#54278,#54279,#54280));
#12969=EDGE_LOOP('',(#54281,#54282,#54283,#54284));
#12970=EDGE_LOOP('',(#54285,#54286,#54287,#54288));
#12971=EDGE_LOOP('',(#54289,#54290,#54291,#54292));
#12972=EDGE_LOOP('',(#54293,#54294,#54295,#54296));
#12973=EDGE_LOOP('',(#54297,#54298,#54299,#54300));
#12974=EDGE_LOOP('',(#54301,#54302,#54303,#54304));
#12975=EDGE_LOOP('',(#54305,#54306,#54307,#54308));
#12976=EDGE_LOOP('',(#54309,#54310,#54311,#54312));
#12977=EDGE_LOOP('',(#54313,#54314,#54315,#54316));
#12978=EDGE_LOOP('',(#54317,#54318,#54319,#54320));
#12979=EDGE_LOOP('',(#54321,#54322,#54323,#54324));
#12980=EDGE_LOOP('',(#54325,#54326,#54327,#54328));
#12981=EDGE_LOOP('',(#54329,#54330,#54331,#54332));
#12982=EDGE_LOOP('',(#54333,#54334,#54335,#54336));
#12983=EDGE_LOOP('',(#54337,#54338,#54339,#54340));
#12984=EDGE_LOOP('',(#54341,#54342,#54343,#54344));
#12985=EDGE_LOOP('',(#54345,#54346,#54347,#54348));
#12986=EDGE_LOOP('',(#54349,#54350,#54351,#54352));
#12987=EDGE_LOOP('',(#54353,#54354,#54355,#54356));
#12988=EDGE_LOOP('',(#54357,#54358,#54359,#54360));
#12989=EDGE_LOOP('',(#54361,#54362,#54363,#54364));
#12990=EDGE_LOOP('',(#54365,#54366,#54367,#54368));
#12991=EDGE_LOOP('',(#54369,#54370,#54371,#54372));
#12992=EDGE_LOOP('',(#54373,#54374,#54375,#54376));
#12993=EDGE_LOOP('',(#54377,#54378,#54379,#54380));
#12994=EDGE_LOOP('',(#54381,#54382,#54383,#54384));
#12995=EDGE_LOOP('',(#54385,#54386,#54387,#54388));
#12996=EDGE_LOOP('',(#54389,#54390,#54391,#54392));
#12997=EDGE_LOOP('',(#54393,#54394,#54395,#54396));
#12998=EDGE_LOOP('',(#54397,#54398,#54399,#54400));
#12999=EDGE_LOOP('',(#54401,#54402,#54403,#54404));
#13000=EDGE_LOOP('',(#54405,#54406,#54407,#54408));
#13001=EDGE_LOOP('',(#54409,#54410,#54411,#54412));
#13002=EDGE_LOOP('',(#54413,#54414,#54415,#54416));
#13003=EDGE_LOOP('',(#54417,#54418,#54419,#54420));
#13004=EDGE_LOOP('',(#54421,#54422,#54423,#54424));
#13005=EDGE_LOOP('',(#54425,#54426,#54427,#54428));
#13006=EDGE_LOOP('',(#54429,#54430,#54431,#54432));
#13007=EDGE_LOOP('',(#54433,#54434,#54435,#54436));
#13008=EDGE_LOOP('',(#54437,#54438,#54439,#54440));
#13009=EDGE_LOOP('',(#54441,#54442,#54443,#54444));
#13010=EDGE_LOOP('',(#54445,#54446,#54447,#54448));
#13011=EDGE_LOOP('',(#54449,#54450,#54451,#54452));
#13012=EDGE_LOOP('',(#54453,#54454,#54455,#54456));
#13013=EDGE_LOOP('',(#54457,#54458,#54459,#54460));
#13014=EDGE_LOOP('',(#54461,#54462,#54463,#54464));
#13015=EDGE_LOOP('',(#54465,#54466,#54467,#54468));
#13016=EDGE_LOOP('',(#54469,#54470,#54471,#54472));
#13017=EDGE_LOOP('',(#54473,#54474,#54475,#54476));
#13018=EDGE_LOOP('',(#54477,#54478,#54479,#54480));
#13019=EDGE_LOOP('',(#54481,#54482,#54483,#54484));
#13020=EDGE_LOOP('',(#54485,#54486,#54487,#54488));
#13021=EDGE_LOOP('',(#54489,#54490,#54491,#54492));
#13022=EDGE_LOOP('',(#54493,#54494,#54495,#54496));
#13023=EDGE_LOOP('',(#54497,#54498,#54499,#54500));
#13024=EDGE_LOOP('',(#54501,#54502,#54503,#54504));
#13025=EDGE_LOOP('',(#54505,#54506,#54507,#54508));
#13026=EDGE_LOOP('',(#54509,#54510,#54511,#54512));
#13027=EDGE_LOOP('',(#54513,#54514,#54515,#54516));
#13028=EDGE_LOOP('',(#54517,#54518,#54519,#54520));
#13029=EDGE_LOOP('',(#54521,#54522,#54523,#54524));
#13030=EDGE_LOOP('',(#54525,#54526,#54527,#54528));
#13031=EDGE_LOOP('',(#54529,#54530,#54531,#54532));
#13032=EDGE_LOOP('',(#54533,#54534,#54535,#54536));
#13033=EDGE_LOOP('',(#54537,#54538,#54539,#54540));
#13034=EDGE_LOOP('',(#54541,#54542,#54543,#54544));
#13035=EDGE_LOOP('',(#54545,#54546,#54547,#54548));
#13036=EDGE_LOOP('',(#54549,#54550,#54551,#54552));
#13037=EDGE_LOOP('',(#54553,#54554,#54555,#54556));
#13038=EDGE_LOOP('',(#54557,#54558,#54559,#54560));
#13039=EDGE_LOOP('',(#54561,#54562,#54563,#54564));
#13040=EDGE_LOOP('',(#54565,#54566,#54567,#54568));
#13041=EDGE_LOOP('',(#54569,#54570,#54571,#54572));
#13042=EDGE_LOOP('',(#54573,#54574,#54575,#54576));
#13043=EDGE_LOOP('',(#54577,#54578,#54579,#54580));
#13044=EDGE_LOOP('',(#54581,#54582,#54583,#54584));
#13045=EDGE_LOOP('',(#54585,#54586,#54587,#54588));
#13046=EDGE_LOOP('',(#54589,#54590,#54591,#54592));
#13047=EDGE_LOOP('',(#54593,#54594,#54595,#54596));
#13048=EDGE_LOOP('',(#54597,#54598,#54599,#54600));
#13049=EDGE_LOOP('',(#54601,#54602,#54603,#54604));
#13050=EDGE_LOOP('',(#54605,#54606,#54607,#54608));
#13051=EDGE_LOOP('',(#54609,#54610,#54611,#54612));
#13052=EDGE_LOOP('',(#54613,#54614,#54615,#54616));
#13053=EDGE_LOOP('',(#54617,#54618,#54619,#54620));
#13054=EDGE_LOOP('',(#54621,#54622,#54623,#54624));
#13055=EDGE_LOOP('',(#54625,#54626,#54627,#54628));
#13056=EDGE_LOOP('',(#54629,#54630,#54631,#54632));
#13057=EDGE_LOOP('',(#54633,#54634,#54635,#54636));
#13058=EDGE_LOOP('',(#54637,#54638,#54639,#54640));
#13059=EDGE_LOOP('',(#54641,#54642,#54643,#54644));
#13060=EDGE_LOOP('',(#54645,#54646,#54647,#54648));
#13061=EDGE_LOOP('',(#54649,#54650,#54651,#54652));
#13062=EDGE_LOOP('',(#54653,#54654,#54655,#54656));
#13063=EDGE_LOOP('',(#54657,#54658,#54659,#54660));
#13064=EDGE_LOOP('',(#54661,#54662,#54663,#54664));
#13065=EDGE_LOOP('',(#54665,#54666,#54667,#54668));
#13066=EDGE_LOOP('',(#54669,#54670,#54671,#54672));
#13067=EDGE_LOOP('',(#54673,#54674,#54675,#54676));
#13068=EDGE_LOOP('',(#54677,#54678,#54679,#54680));
#13069=EDGE_LOOP('',(#54681,#54682,#54683,#54684));
#13070=EDGE_LOOP('',(#54685,#54686,#54687,#54688));
#13071=EDGE_LOOP('',(#54689,#54690,#54691,#54692));
#13072=EDGE_LOOP('',(#54693,#54694,#54695,#54696));
#13073=EDGE_LOOP('',(#54697,#54698,#54699,#54700));
#13074=EDGE_LOOP('',(#54701,#54702,#54703,#54704));
#13075=EDGE_LOOP('',(#54705,#54706,#54707,#54708));
#13076=EDGE_LOOP('',(#54709,#54710,#54711,#54712));
#13077=EDGE_LOOP('',(#54713,#54714,#54715,#54716));
#13078=EDGE_LOOP('',(#54717,#54718,#54719,#54720));
#13079=EDGE_LOOP('',(#54721,#54722,#54723,#54724));
#13080=EDGE_LOOP('',(#54725,#54726,#54727,#54728));
#13081=EDGE_LOOP('',(#54729,#54730,#54731,#54732));
#13082=EDGE_LOOP('',(#54733,#54734,#54735,#54736));
#13083=EDGE_LOOP('',(#54737,#54738,#54739,#54740));
#13084=EDGE_LOOP('',(#54741,#54742,#54743,#54744));
#13085=EDGE_LOOP('',(#54745,#54746,#54747,#54748));
#13086=EDGE_LOOP('',(#54749,#54750,#54751,#54752));
#13087=EDGE_LOOP('',(#54753,#54754,#54755,#54756));
#13088=EDGE_LOOP('',(#54757,#54758,#54759,#54760));
#13089=EDGE_LOOP('',(#54761,#54762,#54763,#54764));
#13090=EDGE_LOOP('',(#54765,#54766,#54767,#54768));
#13091=EDGE_LOOP('',(#54769,#54770,#54771,#54772));
#13092=EDGE_LOOP('',(#54773,#54774,#54775,#54776));
#13093=EDGE_LOOP('',(#54777,#54778,#54779,#54780));
#13094=EDGE_LOOP('',(#54781,#54782,#54783,#54784));
#13095=EDGE_LOOP('',(#54785,#54786,#54787,#54788));
#13096=EDGE_LOOP('',(#54789,#54790,#54791,#54792));
#13097=EDGE_LOOP('',(#54793,#54794,#54795,#54796));
#13098=EDGE_LOOP('',(#54797,#54798,#54799,#54800));
#13099=EDGE_LOOP('',(#54801,#54802,#54803,#54804));
#13100=EDGE_LOOP('',(#54805,#54806,#54807,#54808));
#13101=EDGE_LOOP('',(#54809,#54810,#54811,#54812));
#13102=EDGE_LOOP('',(#54813,#54814,#54815,#54816));
#13103=EDGE_LOOP('',(#54817,#54818,#54819,#54820));
#13104=EDGE_LOOP('',(#54821,#54822,#54823,#54824));
#13105=EDGE_LOOP('',(#54825,#54826,#54827,#54828));
#13106=EDGE_LOOP('',(#54829,#54830,#54831,#54832));
#13107=EDGE_LOOP('',(#54833,#54834,#54835,#54836));
#13108=EDGE_LOOP('',(#54837,#54838,#54839,#54840));
#13109=EDGE_LOOP('',(#54841,#54842,#54843,#54844));
#13110=EDGE_LOOP('',(#54845,#54846,#54847,#54848));
#13111=EDGE_LOOP('',(#54849,#54850,#54851,#54852));
#13112=EDGE_LOOP('',(#54853,#54854,#54855,#54856));
#13113=EDGE_LOOP('',(#54857,#54858,#54859,#54860));
#13114=EDGE_LOOP('',(#54861,#54862,#54863,#54864));
#13115=EDGE_LOOP('',(#54865,#54866,#54867,#54868));
#13116=EDGE_LOOP('',(#54869,#54870,#54871,#54872));
#13117=EDGE_LOOP('',(#54873,#54874,#54875,#54876));
#13118=EDGE_LOOP('',(#54877,#54878,#54879,#54880));
#13119=EDGE_LOOP('',(#54881,#54882,#54883,#54884));
#13120=EDGE_LOOP('',(#54885,#54886,#54887,#54888));
#13121=EDGE_LOOP('',(#54889,#54890,#54891,#54892));
#13122=EDGE_LOOP('',(#54893,#54894,#54895,#54896));
#13123=EDGE_LOOP('',(#54897,#54898,#54899,#54900));
#13124=EDGE_LOOP('',(#54901,#54902,#54903,#54904));
#13125=EDGE_LOOP('',(#54905,#54906,#54907,#54908));
#13126=EDGE_LOOP('',(#54909,#54910,#54911,#54912));
#13127=EDGE_LOOP('',(#54913,#54914,#54915,#54916));
#13128=EDGE_LOOP('',(#54917,#54918,#54919,#54920));
#13129=EDGE_LOOP('',(#54921,#54922,#54923,#54924));
#13130=EDGE_LOOP('',(#54925,#54926,#54927,#54928));
#13131=EDGE_LOOP('',(#54929,#54930,#54931,#54932));
#13132=EDGE_LOOP('',(#54933,#54934,#54935,#54936));
#13133=EDGE_LOOP('',(#54937,#54938,#54939,#54940));
#13134=EDGE_LOOP('',(#54941,#54942,#54943,#54944));
#13135=EDGE_LOOP('',(#54945,#54946,#54947,#54948));
#13136=EDGE_LOOP('',(#54949,#54950,#54951,#54952));
#13137=EDGE_LOOP('',(#54953,#54954,#54955,#54956));
#13138=EDGE_LOOP('',(#54957,#54958,#54959,#54960));
#13139=EDGE_LOOP('',(#54961,#54962,#54963,#54964));
#13140=EDGE_LOOP('',(#54965,#54966,#54967,#54968));
#13141=EDGE_LOOP('',(#54969,#54970,#54971,#54972));
#13142=EDGE_LOOP('',(#54973,#54974,#54975,#54976));
#13143=EDGE_LOOP('',(#54977,#54978,#54979,#54980));
#13144=EDGE_LOOP('',(#54981,#54982,#54983,#54984));
#13145=EDGE_LOOP('',(#54985,#54986,#54987,#54988));
#13146=EDGE_LOOP('',(#54989,#54990,#54991,#54992));
#13147=EDGE_LOOP('',(#54993,#54994,#54995,#54996));
#13148=EDGE_LOOP('',(#54997,#54998,#54999,#55000));
#13149=EDGE_LOOP('',(#55001,#55002,#55003,#55004));
#13150=EDGE_LOOP('',(#55005,#55006,#55007,#55008));
#13151=EDGE_LOOP('',(#55009,#55010,#55011,#55012));
#13152=EDGE_LOOP('',(#55013,#55014,#55015,#55016));
#13153=EDGE_LOOP('',(#55017,#55018,#55019,#55020));
#13154=EDGE_LOOP('',(#55021,#55022,#55023,#55024));
#13155=EDGE_LOOP('',(#55025,#55026,#55027,#55028));
#13156=EDGE_LOOP('',(#55029,#55030,#55031,#55032));
#13157=EDGE_LOOP('',(#55033,#55034,#55035,#55036));
#13158=EDGE_LOOP('',(#55037,#55038,#55039,#55040));
#13159=EDGE_LOOP('',(#55041,#55042,#55043,#55044));
#13160=EDGE_LOOP('',(#55045,#55046,#55047,#55048));
#13161=EDGE_LOOP('',(#55049,#55050,#55051,#55052));
#13162=EDGE_LOOP('',(#55053,#55054,#55055,#55056));
#13163=EDGE_LOOP('',(#55057,#55058,#55059,#55060));
#13164=EDGE_LOOP('',(#55061,#55062,#55063,#55064));
#13165=EDGE_LOOP('',(#55065,#55066,#55067,#55068));
#13166=EDGE_LOOP('',(#55069,#55070,#55071,#55072));
#13167=EDGE_LOOP('',(#55073,#55074,#55075,#55076));
#13168=EDGE_LOOP('',(#55077,#55078,#55079,#55080));
#13169=EDGE_LOOP('',(#55081,#55082,#55083,#55084));
#13170=EDGE_LOOP('',(#55085,#55086,#55087,#55088));
#13171=EDGE_LOOP('',(#55089,#55090,#55091,#55092));
#13172=EDGE_LOOP('',(#55093,#55094,#55095,#55096));
#13173=EDGE_LOOP('',(#55097,#55098,#55099,#55100));
#13174=EDGE_LOOP('',(#55101,#55102,#55103,#55104));
#13175=EDGE_LOOP('',(#55105,#55106,#55107,#55108));
#13176=EDGE_LOOP('',(#55109,#55110,#55111,#55112));
#13177=EDGE_LOOP('',(#55113,#55114,#55115,#55116));
#13178=EDGE_LOOP('',(#55117,#55118,#55119,#55120));
#13179=EDGE_LOOP('',(#55121,#55122,#55123,#55124));
#13180=EDGE_LOOP('',(#55125,#55126,#55127,#55128));
#13181=EDGE_LOOP('',(#55129,#55130,#55131,#55132));
#13182=EDGE_LOOP('',(#55133,#55134,#55135,#55136));
#13183=EDGE_LOOP('',(#55137,#55138,#55139,#55140));
#13184=EDGE_LOOP('',(#55141,#55142,#55143,#55144));
#13185=EDGE_LOOP('',(#55145,#55146,#55147,#55148));
#13186=EDGE_LOOP('',(#55149,#55150,#55151,#55152));
#13187=EDGE_LOOP('',(#55153,#55154,#55155,#55156));
#13188=EDGE_LOOP('',(#55157,#55158,#55159,#55160));
#13189=EDGE_LOOP('',(#55161,#55162,#55163,#55164));
#13190=EDGE_LOOP('',(#55165,#55166,#55167,#55168));
#13191=EDGE_LOOP('',(#55169,#55170,#55171,#55172));
#13192=EDGE_LOOP('',(#55173,#55174,#55175,#55176));
#13193=EDGE_LOOP('',(#55177,#55178,#55179,#55180));
#13194=EDGE_LOOP('',(#55181,#55182,#55183,#55184));
#13195=EDGE_LOOP('',(#55185,#55186,#55187,#55188));
#13196=EDGE_LOOP('',(#55189,#55190,#55191,#55192));
#13197=EDGE_LOOP('',(#55193,#55194,#55195,#55196));
#13198=EDGE_LOOP('',(#55197,#55198,#55199,#55200));
#13199=EDGE_LOOP('',(#55201,#55202,#55203,#55204));
#13200=EDGE_LOOP('',(#55205,#55206,#55207,#55208));
#13201=EDGE_LOOP('',(#55209,#55210,#55211,#55212));
#13202=EDGE_LOOP('',(#55213,#55214,#55215,#55216));
#13203=EDGE_LOOP('',(#55217,#55218,#55219,#55220));
#13204=EDGE_LOOP('',(#55221,#55222,#55223,#55224));
#13205=EDGE_LOOP('',(#55225,#55226,#55227,#55228));
#13206=EDGE_LOOP('',(#55229,#55230,#55231,#55232));
#13207=EDGE_LOOP('',(#55233,#55234,#55235,#55236));
#13208=EDGE_LOOP('',(#55237,#55238,#55239,#55240));
#13209=EDGE_LOOP('',(#55241,#55242,#55243,#55244));
#13210=EDGE_LOOP('',(#55245,#55246,#55247,#55248));
#13211=EDGE_LOOP('',(#55249,#55250,#55251,#55252));
#13212=EDGE_LOOP('',(#55253,#55254,#55255,#55256));
#13213=EDGE_LOOP('',(#55257,#55258,#55259,#55260));
#13214=EDGE_LOOP('',(#55261,#55262,#55263,#55264));
#13215=EDGE_LOOP('',(#55265,#55266,#55267,#55268));
#13216=EDGE_LOOP('',(#55269,#55270,#55271,#55272));
#13217=EDGE_LOOP('',(#55273,#55274,#55275,#55276));
#13218=EDGE_LOOP('',(#55277,#55278,#55279,#55280));
#13219=EDGE_LOOP('',(#55281,#55282,#55283,#55284));
#13220=EDGE_LOOP('',(#55285,#55286,#55287,#55288));
#13221=EDGE_LOOP('',(#55289,#55290,#55291,#55292));
#13222=EDGE_LOOP('',(#55293,#55294,#55295,#55296));
#13223=EDGE_LOOP('',(#55297,#55298,#55299,#55300));
#13224=EDGE_LOOP('',(#55301,#55302,#55303,#55304));
#13225=EDGE_LOOP('',(#55305,#55306,#55307,#55308));
#13226=EDGE_LOOP('',(#55309,#55310,#55311,#55312));
#13227=EDGE_LOOP('',(#55313,#55314,#55315,#55316));
#13228=EDGE_LOOP('',(#55317,#55318,#55319,#55320));
#13229=EDGE_LOOP('',(#55321,#55322,#55323,#55324));
#13230=EDGE_LOOP('',(#55325,#55326,#55327,#55328));
#13231=EDGE_LOOP('',(#55329,#55330,#55331,#55332));
#13232=EDGE_LOOP('',(#55333,#55334,#55335,#55336));
#13233=EDGE_LOOP('',(#55337,#55338,#55339,#55340));
#13234=EDGE_LOOP('',(#55341,#55342,#55343,#55344));
#13235=EDGE_LOOP('',(#55345,#55346,#55347,#55348));
#13236=EDGE_LOOP('',(#55349,#55350,#55351,#55352));
#13237=EDGE_LOOP('',(#55353,#55354,#55355,#55356));
#13238=EDGE_LOOP('',(#55357,#55358,#55359,#55360));
#13239=EDGE_LOOP('',(#55361,#55362,#55363,#55364));
#13240=EDGE_LOOP('',(#55365,#55366,#55367,#55368));
#13241=EDGE_LOOP('',(#55369,#55370,#55371,#55372));
#13242=EDGE_LOOP('',(#55373,#55374,#55375,#55376));
#13243=EDGE_LOOP('',(#55377,#55378,#55379,#55380));
#13244=EDGE_LOOP('',(#55381,#55382,#55383,#55384));
#13245=EDGE_LOOP('',(#55385,#55386,#55387,#55388));
#13246=EDGE_LOOP('',(#55389,#55390,#55391,#55392));
#13247=EDGE_LOOP('',(#55393,#55394,#55395,#55396));
#13248=EDGE_LOOP('',(#55397,#55398,#55399,#55400));
#13249=EDGE_LOOP('',(#55401,#55402,#55403,#55404));
#13250=EDGE_LOOP('',(#55405,#55406,#55407,#55408));
#13251=EDGE_LOOP('',(#55409,#55410,#55411,#55412));
#13252=EDGE_LOOP('',(#55413,#55414,#55415,#55416));
#13253=EDGE_LOOP('',(#55417,#55418,#55419,#55420));
#13254=EDGE_LOOP('',(#55421,#55422,#55423,#55424));
#13255=EDGE_LOOP('',(#55425,#55426,#55427,#55428));
#13256=EDGE_LOOP('',(#55429,#55430,#55431,#55432));
#13257=EDGE_LOOP('',(#55433,#55434,#55435,#55436));
#13258=EDGE_LOOP('',(#55437,#55438,#55439,#55440));
#13259=EDGE_LOOP('',(#55441,#55442,#55443,#55444));
#13260=EDGE_LOOP('',(#55445,#55446,#55447,#55448));
#13261=EDGE_LOOP('',(#55449,#55450,#55451,#55452));
#13262=EDGE_LOOP('',(#55453,#55454,#55455,#55456));
#13263=EDGE_LOOP('',(#55457,#55458,#55459,#55460));
#13264=EDGE_LOOP('',(#55461,#55462,#55463,#55464));
#13265=EDGE_LOOP('',(#55465,#55466,#55467,#55468));
#13266=EDGE_LOOP('',(#55469,#55470,#55471,#55472));
#13267=EDGE_LOOP('',(#55473,#55474,#55475,#55476));
#13268=EDGE_LOOP('',(#55477,#55478,#55479,#55480));
#13269=EDGE_LOOP('',(#55481,#55482,#55483,#55484));
#13270=EDGE_LOOP('',(#55485,#55486,#55487,#55488));
#13271=EDGE_LOOP('',(#55489,#55490,#55491,#55492));
#13272=EDGE_LOOP('',(#55493,#55494,#55495,#55496));
#13273=EDGE_LOOP('',(#55497,#55498,#55499,#55500));
#13274=EDGE_LOOP('',(#55501,#55502,#55503,#55504));
#13275=EDGE_LOOP('',(#55505,#55506,#55507,#55508));
#13276=EDGE_LOOP('',(#55509,#55510,#55511,#55512));
#13277=EDGE_LOOP('',(#55513,#55514,#55515,#55516));
#13278=EDGE_LOOP('',(#55517,#55518,#55519,#55520));
#13279=EDGE_LOOP('',(#55521,#55522,#55523,#55524));
#13280=EDGE_LOOP('',(#55525,#55526,#55527,#55528));
#13281=EDGE_LOOP('',(#55529,#55530,#55531,#55532));
#13282=EDGE_LOOP('',(#55533,#55534,#55535,#55536));
#13283=EDGE_LOOP('',(#55537,#55538,#55539,#55540));
#13284=EDGE_LOOP('',(#55541,#55542,#55543,#55544));
#13285=EDGE_LOOP('',(#55545,#55546,#55547,#55548));
#13286=EDGE_LOOP('',(#55549,#55550,#55551,#55552));
#13287=EDGE_LOOP('',(#55553,#55554,#55555,#55556));
#13288=EDGE_LOOP('',(#55557,#55558,#55559,#55560));
#13289=EDGE_LOOP('',(#55561,#55562,#55563,#55564));
#13290=EDGE_LOOP('',(#55565,#55566,#55567,#55568));
#13291=EDGE_LOOP('',(#55569,#55570,#55571,#55572));
#13292=EDGE_LOOP('',(#55573,#55574,#55575,#55576));
#13293=EDGE_LOOP('',(#55577,#55578,#55579,#55580));
#13294=EDGE_LOOP('',(#55581,#55582,#55583,#55584));
#13295=EDGE_LOOP('',(#55585,#55586,#55587,#55588));
#13296=EDGE_LOOP('',(#55589,#55590,#55591,#55592));
#13297=EDGE_LOOP('',(#55593,#55594,#55595,#55596));
#13298=EDGE_LOOP('',(#55597,#55598,#55599,#55600));
#13299=EDGE_LOOP('',(#55601,#55602,#55603,#55604));
#13300=EDGE_LOOP('',(#55605,#55606,#55607,#55608));
#13301=EDGE_LOOP('',(#55609,#55610,#55611,#55612));
#13302=EDGE_LOOP('',(#55613,#55614,#55615,#55616));
#13303=EDGE_LOOP('',(#55617,#55618,#55619,#55620));
#13304=EDGE_LOOP('',(#55621,#55622,#55623,#55624));
#13305=EDGE_LOOP('',(#55625,#55626,#55627,#55628));
#13306=EDGE_LOOP('',(#55629,#55630,#55631,#55632));
#13307=EDGE_LOOP('',(#55633,#55634,#55635,#55636));
#13308=EDGE_LOOP('',(#55637,#55638,#55639,#55640));
#13309=EDGE_LOOP('',(#55641,#55642,#55643,#55644));
#13310=EDGE_LOOP('',(#55645,#55646,#55647,#55648));
#13311=EDGE_LOOP('',(#55649,#55650,#55651,#55652));
#13312=EDGE_LOOP('',(#55653,#55654,#55655,#55656));
#13313=EDGE_LOOP('',(#55657,#55658,#55659,#55660));
#13314=EDGE_LOOP('',(#55661,#55662,#55663,#55664));
#13315=EDGE_LOOP('',(#55665,#55666,#55667,#55668));
#13316=EDGE_LOOP('',(#55669,#55670,#55671,#55672));
#13317=EDGE_LOOP('',(#55673,#55674,#55675,#55676));
#13318=EDGE_LOOP('',(#55677,#55678,#55679,#55680));
#13319=EDGE_LOOP('',(#55681,#55682,#55683,#55684));
#13320=EDGE_LOOP('',(#55685,#55686,#55687,#55688));
#13321=EDGE_LOOP('',(#55689,#55690,#55691,#55692));
#13322=EDGE_LOOP('',(#55693,#55694,#55695,#55696));
#13323=EDGE_LOOP('',(#55697,#55698,#55699,#55700));
#13324=EDGE_LOOP('',(#55701,#55702,#55703,#55704));
#13325=EDGE_LOOP('',(#55705,#55706,#55707,#55708));
#13326=EDGE_LOOP('',(#55709,#55710,#55711,#55712));
#13327=EDGE_LOOP('',(#55713,#55714,#55715,#55716));
#13328=EDGE_LOOP('',(#55717,#55718,#55719,#55720));
#13329=EDGE_LOOP('',(#55721,#55722,#55723,#55724));
#13330=EDGE_LOOP('',(#55725,#55726,#55727,#55728));
#13331=EDGE_LOOP('',(#55729,#55730,#55731,#55732));
#13332=EDGE_LOOP('',(#55733,#55734,#55735,#55736));
#13333=EDGE_LOOP('',(#55737,#55738,#55739,#55740));
#13334=EDGE_LOOP('',(#55741,#55742,#55743,#55744));
#13335=EDGE_LOOP('',(#55745,#55746,#55747,#55748));
#13336=EDGE_LOOP('',(#55749,#55750,#55751,#55752));
#13337=EDGE_LOOP('',(#55753,#55754,#55755,#55756));
#13338=EDGE_LOOP('',(#55757,#55758,#55759,#55760));
#13339=EDGE_LOOP('',(#55761,#55762,#55763,#55764));
#13340=EDGE_LOOP('',(#55765,#55766,#55767,#55768));
#13341=EDGE_LOOP('',(#55769,#55770,#55771,#55772));
#13342=EDGE_LOOP('',(#55773,#55774,#55775,#55776));
#13343=EDGE_LOOP('',(#55777,#55778,#55779,#55780));
#13344=EDGE_LOOP('',(#55781,#55782,#55783,#55784));
#13345=EDGE_LOOP('',(#55785,#55786,#55787,#55788));
#13346=EDGE_LOOP('',(#55789,#55790,#55791,#55792));
#13347=EDGE_LOOP('',(#55793,#55794,#55795,#55796));
#13348=EDGE_LOOP('',(#55797,#55798,#55799,#55800));
#13349=EDGE_LOOP('',(#55801,#55802,#55803,#55804));
#13350=EDGE_LOOP('',(#55805,#55806,#55807,#55808));
#13351=EDGE_LOOP('',(#55809,#55810,#55811,#55812));
#13352=EDGE_LOOP('',(#55813,#55814,#55815,#55816));
#13353=EDGE_LOOP('',(#55817,#55818,#55819,#55820));
#13354=EDGE_LOOP('',(#55821,#55822,#55823,#55824));
#13355=EDGE_LOOP('',(#55825,#55826,#55827,#55828));
#13356=EDGE_LOOP('',(#55829,#55830,#55831,#55832));
#13357=EDGE_LOOP('',(#55833,#55834,#55835,#55836));
#13358=EDGE_LOOP('',(#55837,#55838,#55839,#55840));
#13359=EDGE_LOOP('',(#55841,#55842,#55843,#55844));
#13360=EDGE_LOOP('',(#55845,#55846,#55847,#55848));
#13361=EDGE_LOOP('',(#55849,#55850,#55851,#55852));
#13362=EDGE_LOOP('',(#55853,#55854,#55855,#55856));
#13363=EDGE_LOOP('',(#55857,#55858,#55859,#55860));
#13364=EDGE_LOOP('',(#55861,#55862,#55863,#55864));
#13365=EDGE_LOOP('',(#55865,#55866,#55867,#55868));
#13366=EDGE_LOOP('',(#55869,#55870,#55871,#55872));
#13367=EDGE_LOOP('',(#55873,#55874,#55875,#55876));
#13368=EDGE_LOOP('',(#55877,#55878,#55879,#55880));
#13369=EDGE_LOOP('',(#55881,#55882,#55883,#55884));
#13370=EDGE_LOOP('',(#55885,#55886,#55887,#55888));
#13371=EDGE_LOOP('',(#55889,#55890,#55891,#55892));
#13372=EDGE_LOOP('',(#55893,#55894,#55895,#55896));
#13373=EDGE_LOOP('',(#55897,#55898,#55899,#55900));
#13374=EDGE_LOOP('',(#55901,#55902,#55903,#55904));
#13375=EDGE_LOOP('',(#55905,#55906,#55907,#55908));
#13376=EDGE_LOOP('',(#55909,#55910,#55911,#55912));
#13377=EDGE_LOOP('',(#55913,#55914,#55915,#55916));
#13378=EDGE_LOOP('',(#55917,#55918,#55919,#55920));
#13379=EDGE_LOOP('',(#55921,#55922,#55923,#55924));
#13380=EDGE_LOOP('',(#55925,#55926,#55927,#55928));
#13381=EDGE_LOOP('',(#55929,#55930,#55931,#55932));
#13382=EDGE_LOOP('',(#55933,#55934,#55935,#55936));
#13383=EDGE_LOOP('',(#55937,#55938,#55939,#55940));
#13384=EDGE_LOOP('',(#55941,#55942,#55943,#55944));
#13385=EDGE_LOOP('',(#55945,#55946,#55947,#55948));
#13386=EDGE_LOOP('',(#55949,#55950,#55951,#55952));
#13387=EDGE_LOOP('',(#55953,#55954,#55955,#55956));
#13388=EDGE_LOOP('',(#55957,#55958,#55959,#55960));
#13389=EDGE_LOOP('',(#55961,#55962,#55963,#55964));
#13390=EDGE_LOOP('',(#55965,#55966,#55967,#55968));
#13391=EDGE_LOOP('',(#55969,#55970,#55971,#55972));
#13392=EDGE_LOOP('',(#55973,#55974,#55975,#55976));
#13393=EDGE_LOOP('',(#55977,#55978,#55979,#55980));
#13394=EDGE_LOOP('',(#55981,#55982,#55983,#55984));
#13395=EDGE_LOOP('',(#55985,#55986,#55987,#55988));
#13396=EDGE_LOOP('',(#55989,#55990,#55991,#55992));
#13397=EDGE_LOOP('',(#55993,#55994,#55995,#55996));
#13398=EDGE_LOOP('',(#55997,#55998,#55999,#56000));
#13399=EDGE_LOOP('',(#56001,#56002,#56003,#56004));
#13400=EDGE_LOOP('',(#56005,#56006,#56007,#56008));
#13401=EDGE_LOOP('',(#56009,#56010,#56011,#56012));
#13402=EDGE_LOOP('',(#56013,#56014,#56015,#56016));
#13403=EDGE_LOOP('',(#56017,#56018,#56019,#56020));
#13404=EDGE_LOOP('',(#56021,#56022,#56023,#56024));
#13405=EDGE_LOOP('',(#56025,#56026,#56027,#56028));
#13406=EDGE_LOOP('',(#56029,#56030,#56031,#56032));
#13407=EDGE_LOOP('',(#56033,#56034,#56035,#56036));
#13408=EDGE_LOOP('',(#56037,#56038,#56039,#56040));
#13409=EDGE_LOOP('',(#56041,#56042,#56043,#56044));
#13410=EDGE_LOOP('',(#56045,#56046,#56047,#56048));
#13411=EDGE_LOOP('',(#56049,#56050,#56051,#56052));
#13412=EDGE_LOOP('',(#56053,#56054,#56055,#56056));
#13413=EDGE_LOOP('',(#56057,#56058,#56059,#56060));
#13414=EDGE_LOOP('',(#56061,#56062,#56063,#56064));
#13415=EDGE_LOOP('',(#56065,#56066,#56067,#56068));
#13416=EDGE_LOOP('',(#56069,#56070,#56071,#56072));
#13417=EDGE_LOOP('',(#56073,#56074,#56075,#56076));
#13418=EDGE_LOOP('',(#56077,#56078,#56079,#56080));
#13419=EDGE_LOOP('',(#56081,#56082,#56083,#56084));
#13420=EDGE_LOOP('',(#56085,#56086,#56087,#56088));
#13421=EDGE_LOOP('',(#56089,#56090,#56091,#56092));
#13422=EDGE_LOOP('',(#56093,#56094,#56095,#56096));
#13423=EDGE_LOOP('',(#56097,#56098,#56099,#56100));
#13424=EDGE_LOOP('',(#56101,#56102,#56103,#56104));
#13425=EDGE_LOOP('',(#56105,#56106,#56107,#56108));
#13426=EDGE_LOOP('',(#56109,#56110,#56111,#56112));
#13427=EDGE_LOOP('',(#56113,#56114,#56115,#56116));
#13428=EDGE_LOOP('',(#56117,#56118,#56119,#56120));
#13429=EDGE_LOOP('',(#56121,#56122,#56123,#56124));
#13430=EDGE_LOOP('',(#56125,#56126,#56127,#56128));
#13431=EDGE_LOOP('',(#56129,#56130,#56131,#56132));
#13432=EDGE_LOOP('',(#56133,#56134,#56135,#56136));
#13433=EDGE_LOOP('',(#56137,#56138,#56139,#56140));
#13434=EDGE_LOOP('',(#56141,#56142,#56143,#56144));
#13435=EDGE_LOOP('',(#56145,#56146,#56147,#56148));
#13436=EDGE_LOOP('',(#56149,#56150,#56151,#56152));
#13437=EDGE_LOOP('',(#56153,#56154,#56155,#56156));
#13438=EDGE_LOOP('',(#56157,#56158,#56159,#56160));
#13439=EDGE_LOOP('',(#56161,#56162,#56163,#56164));
#13440=EDGE_LOOP('',(#56165,#56166,#56167,#56168));
#13441=EDGE_LOOP('',(#56169,#56170,#56171,#56172));
#13442=EDGE_LOOP('',(#56173,#56174,#56175,#56176));
#13443=EDGE_LOOP('',(#56177,#56178,#56179,#56180));
#13444=EDGE_LOOP('',(#56181,#56182,#56183,#56184));
#13445=EDGE_LOOP('',(#56185,#56186,#56187,#56188));
#13446=EDGE_LOOP('',(#56189,#56190,#56191,#56192));
#13447=EDGE_LOOP('',(#56193,#56194,#56195,#56196));
#13448=EDGE_LOOP('',(#56197,#56198,#56199,#56200));
#13449=EDGE_LOOP('',(#56201,#56202,#56203,#56204));
#13450=EDGE_LOOP('',(#56205,#56206,#56207,#56208));
#13451=EDGE_LOOP('',(#56209,#56210,#56211,#56212));
#13452=EDGE_LOOP('',(#56213,#56214,#56215,#56216));
#13453=EDGE_LOOP('',(#56217,#56218,#56219,#56220));
#13454=EDGE_LOOP('',(#56221,#56222,#56223,#56224));
#13455=EDGE_LOOP('',(#56225,#56226,#56227,#56228));
#13456=EDGE_LOOP('',(#56229,#56230,#56231,#56232));
#13457=EDGE_LOOP('',(#56233,#56234,#56235,#56236));
#13458=EDGE_LOOP('',(#56237,#56238,#56239,#56240));
#13459=EDGE_LOOP('',(#56241,#56242,#56243,#56244));
#13460=EDGE_LOOP('',(#56245,#56246,#56247,#56248));
#13461=EDGE_LOOP('',(#56249,#56250,#56251,#56252));
#13462=EDGE_LOOP('',(#56253,#56254,#56255,#56256));
#13463=EDGE_LOOP('',(#56257,#56258,#56259,#56260));
#13464=EDGE_LOOP('',(#56261,#56262,#56263,#56264));
#13465=EDGE_LOOP('',(#56265,#56266,#56267,#56268));
#13466=EDGE_LOOP('',(#56269,#56270,#56271,#56272));
#13467=EDGE_LOOP('',(#56273,#56274,#56275,#56276));
#13468=EDGE_LOOP('',(#56277,#56278,#56279,#56280));
#13469=EDGE_LOOP('',(#56281,#56282,#56283,#56284));
#13470=EDGE_LOOP('',(#56285,#56286,#56287,#56288));
#13471=EDGE_LOOP('',(#56289,#56290,#56291,#56292));
#13472=EDGE_LOOP('',(#56293,#56294,#56295,#56296));
#13473=EDGE_LOOP('',(#56297,#56298,#56299,#56300));
#13474=EDGE_LOOP('',(#56301,#56302,#56303,#56304));
#13475=EDGE_LOOP('',(#56305,#56306,#56307,#56308));
#13476=EDGE_LOOP('',(#56309,#56310,#56311,#56312));
#13477=EDGE_LOOP('',(#56313,#56314,#56315,#56316));
#13478=EDGE_LOOP('',(#56317,#56318,#56319,#56320));
#13479=EDGE_LOOP('',(#56321,#56322,#56323,#56324));
#13480=EDGE_LOOP('',(#56325,#56326,#56327,#56328));
#13481=EDGE_LOOP('',(#56329,#56330,#56331,#56332));
#13482=EDGE_LOOP('',(#56333,#56334,#56335,#56336));
#13483=EDGE_LOOP('',(#56337,#56338,#56339,#56340));
#13484=EDGE_LOOP('',(#56341,#56342,#56343,#56344));
#13485=EDGE_LOOP('',(#56345,#56346,#56347,#56348));
#13486=EDGE_LOOP('',(#56349,#56350,#56351,#56352));
#13487=EDGE_LOOP('',(#56353,#56354,#56355,#56356));
#13488=EDGE_LOOP('',(#56357,#56358,#56359,#56360));
#13489=EDGE_LOOP('',(#56361,#56362,#56363,#56364));
#13490=EDGE_LOOP('',(#56365,#56366,#56367,#56368));
#13491=EDGE_LOOP('',(#56369,#56370,#56371,#56372));
#13492=EDGE_LOOP('',(#56373,#56374,#56375,#56376));
#13493=EDGE_LOOP('',(#56377,#56378,#56379,#56380));
#13494=EDGE_LOOP('',(#56381,#56382,#56383,#56384));
#13495=EDGE_LOOP('',(#56385,#56386,#56387,#56388));
#13496=EDGE_LOOP('',(#56389,#56390,#56391,#56392));
#13497=EDGE_LOOP('',(#56393,#56394,#56395,#56396));
#13498=EDGE_LOOP('',(#56397,#56398,#56399,#56400));
#13499=EDGE_LOOP('',(#56401,#56402,#56403,#56404));
#13500=EDGE_LOOP('',(#56405,#56406,#56407,#56408));
#13501=EDGE_LOOP('',(#56409,#56410,#56411,#56412));
#13502=EDGE_LOOP('',(#56413,#56414,#56415,#56416));
#13503=EDGE_LOOP('',(#56417,#56418,#56419,#56420));
#13504=EDGE_LOOP('',(#56421,#56422,#56423,#56424));
#13505=EDGE_LOOP('',(#56425,#56426,#56427,#56428));
#13506=EDGE_LOOP('',(#56429,#56430,#56431,#56432));
#13507=EDGE_LOOP('',(#56433,#56434,#56435,#56436));
#13508=EDGE_LOOP('',(#56437,#56438,#56439,#56440));
#13509=EDGE_LOOP('',(#56441,#56442,#56443,#56444));
#13510=EDGE_LOOP('',(#56445,#56446,#56447,#56448));
#13511=EDGE_LOOP('',(#56449,#56450,#56451,#56452));
#13512=EDGE_LOOP('',(#56453,#56454,#56455,#56456));
#13513=EDGE_LOOP('',(#56457,#56458,#56459,#56460));
#13514=EDGE_LOOP('',(#56461,#56462,#56463,#56464));
#13515=EDGE_LOOP('',(#56465,#56466,#56467,#56468));
#13516=EDGE_LOOP('',(#56469,#56470,#56471,#56472));
#13517=EDGE_LOOP('',(#56473,#56474,#56475,#56476));
#13518=EDGE_LOOP('',(#56477,#56478,#56479,#56480));
#13519=EDGE_LOOP('',(#56481,#56482,#56483,#56484));
#13520=EDGE_LOOP('',(#56485,#56486,#56487,#56488));
#13521=EDGE_LOOP('',(#56489,#56490,#56491,#56492));
#13522=EDGE_LOOP('',(#56493,#56494,#56495,#56496));
#13523=EDGE_LOOP('',(#56497,#56498,#56499,#56500));
#13524=EDGE_LOOP('',(#56501,#56502,#56503,#56504));
#13525=EDGE_LOOP('',(#56505,#56506,#56507,#56508));
#13526=EDGE_LOOP('',(#56509,#56510,#56511,#56512));
#13527=EDGE_LOOP('',(#56513,#56514,#56515,#56516));
#13528=EDGE_LOOP('',(#56517,#56518,#56519,#56520));
#13529=EDGE_LOOP('',(#56521,#56522,#56523,#56524));
#13530=EDGE_LOOP('',(#56525,#56526,#56527,#56528));
#13531=EDGE_LOOP('',(#56529,#56530,#56531,#56532));
#13532=EDGE_LOOP('',(#56533,#56534,#56535,#56536));
#13533=EDGE_LOOP('',(#56537,#56538,#56539,#56540));
#13534=EDGE_LOOP('',(#56541,#56542,#56543,#56544));
#13535=EDGE_LOOP('',(#56545,#56546,#56547,#56548));
#13536=EDGE_LOOP('',(#56549,#56550,#56551,#56552));
#13537=EDGE_LOOP('',(#56553,#56554,#56555,#56556));
#13538=EDGE_LOOP('',(#56557,#56558,#56559,#56560));
#13539=EDGE_LOOP('',(#56561,#56562,#56563,#56564));
#13540=EDGE_LOOP('',(#56565,#56566,#56567,#56568));
#13541=EDGE_LOOP('',(#56569,#56570,#56571,#56572));
#13542=EDGE_LOOP('',(#56573,#56574,#56575,#56576));
#13543=EDGE_LOOP('',(#56577,#56578,#56579,#56580));
#13544=EDGE_LOOP('',(#56581,#56582,#56583,#56584));
#13545=EDGE_LOOP('',(#56585,#56586,#56587,#56588));
#13546=EDGE_LOOP('',(#56589,#56590,#56591,#56592));
#13547=EDGE_LOOP('',(#56593,#56594,#56595,#56596));
#13548=EDGE_LOOP('',(#56597,#56598,#56599,#56600));
#13549=EDGE_LOOP('',(#56601,#56602,#56603,#56604));
#13550=EDGE_LOOP('',(#56605,#56606,#56607,#56608));
#13551=EDGE_LOOP('',(#56609,#56610,#56611,#56612));
#13552=EDGE_LOOP('',(#56613,#56614,#56615,#56616));
#13553=EDGE_LOOP('',(#56617,#56618,#56619,#56620));
#13554=EDGE_LOOP('',(#56621,#56622,#56623,#56624));
#13555=EDGE_LOOP('',(#56625,#56626,#56627,#56628));
#13556=EDGE_LOOP('',(#56629,#56630,#56631,#56632));
#13557=EDGE_LOOP('',(#56633,#56634,#56635,#56636));
#13558=EDGE_LOOP('',(#56637,#56638,#56639,#56640));
#13559=EDGE_LOOP('',(#56641,#56642,#56643,#56644));
#13560=EDGE_LOOP('',(#56645,#56646,#56647,#56648));
#13561=EDGE_LOOP('',(#56649,#56650,#56651,#56652));
#13562=EDGE_LOOP('',(#56653,#56654,#56655,#56656));
#13563=EDGE_LOOP('',(#56657,#56658,#56659,#56660));
#13564=EDGE_LOOP('',(#56661,#56662,#56663,#56664));
#13565=EDGE_LOOP('',(#56665,#56666,#56667,#56668));
#13566=EDGE_LOOP('',(#56669,#56670,#56671,#56672));
#13567=EDGE_LOOP('',(#56673,#56674,#56675,#56676));
#13568=EDGE_LOOP('',(#56677,#56678,#56679,#56680));
#13569=EDGE_LOOP('',(#56681,#56682,#56683,#56684));
#13570=EDGE_LOOP('',(#56685,#56686,#56687,#56688));
#13571=EDGE_LOOP('',(#56689,#56690,#56691,#56692));
#13572=EDGE_LOOP('',(#56693,#56694,#56695,#56696));
#13573=EDGE_LOOP('',(#56697,#56698,#56699,#56700));
#13574=EDGE_LOOP('',(#56701,#56702,#56703,#56704));
#13575=EDGE_LOOP('',(#56705,#56706,#56707,#56708));
#13576=EDGE_LOOP('',(#56709,#56710,#56711,#56712));
#13577=EDGE_LOOP('',(#56713,#56714,#56715,#56716));
#13578=EDGE_LOOP('',(#56717,#56718,#56719,#56720));
#13579=EDGE_LOOP('',(#56721,#56722,#56723,#56724));
#13580=EDGE_LOOP('',(#56725,#56726,#56727,#56728));
#13581=EDGE_LOOP('',(#56729,#56730,#56731,#56732));
#13582=EDGE_LOOP('',(#56733,#56734,#56735,#56736));
#13583=EDGE_LOOP('',(#56737,#56738,#56739,#56740));
#13584=EDGE_LOOP('',(#56741,#56742,#56743,#56744));
#13585=EDGE_LOOP('',(#56745,#56746,#56747,#56748));
#13586=EDGE_LOOP('',(#56749,#56750,#56751,#56752));
#13587=EDGE_LOOP('',(#56753,#56754,#56755,#56756));
#13588=EDGE_LOOP('',(#56757,#56758,#56759,#56760));
#13589=EDGE_LOOP('',(#56761,#56762,#56763,#56764));
#13590=EDGE_LOOP('',(#56765,#56766,#56767,#56768));
#13591=EDGE_LOOP('',(#56769,#56770,#56771,#56772));
#13592=EDGE_LOOP('',(#56773,#56774,#56775,#56776));
#13593=EDGE_LOOP('',(#56777,#56778,#56779,#56780));
#13594=EDGE_LOOP('',(#56781,#56782,#56783,#56784));
#13595=EDGE_LOOP('',(#56785,#56786,#56787,#56788));
#13596=EDGE_LOOP('',(#56789,#56790,#56791,#56792));
#13597=EDGE_LOOP('',(#56793,#56794,#56795,#56796));
#13598=EDGE_LOOP('',(#56797,#56798,#56799,#56800));
#13599=EDGE_LOOP('',(#56801,#56802,#56803,#56804));
#13600=EDGE_LOOP('',(#56805,#56806,#56807,#56808));
#13601=EDGE_LOOP('',(#56809,#56810,#56811,#56812));
#13602=EDGE_LOOP('',(#56813,#56814,#56815,#56816));
#13603=EDGE_LOOP('',(#56817,#56818,#56819,#56820));
#13604=EDGE_LOOP('',(#56821,#56822,#56823,#56824));
#13605=EDGE_LOOP('',(#56825,#56826,#56827,#56828));
#13606=EDGE_LOOP('',(#56829,#56830,#56831,#56832));
#13607=EDGE_LOOP('',(#56833,#56834,#56835,#56836));
#13608=EDGE_LOOP('',(#56837,#56838,#56839,#56840));
#13609=EDGE_LOOP('',(#56841,#56842,#56843,#56844));
#13610=EDGE_LOOP('',(#56845,#56846,#56847,#56848));
#13611=EDGE_LOOP('',(#56849,#56850,#56851,#56852));
#13612=EDGE_LOOP('',(#56853,#56854,#56855,#56856));
#13613=EDGE_LOOP('',(#56857,#56858,#56859,#56860));
#13614=EDGE_LOOP('',(#56861,#56862,#56863,#56864));
#13615=EDGE_LOOP('',(#56865,#56866,#56867,#56868));
#13616=EDGE_LOOP('',(#56869,#56870,#56871,#56872));
#13617=EDGE_LOOP('',(#56873,#56874,#56875,#56876));
#13618=EDGE_LOOP('',(#56877,#56878,#56879,#56880));
#13619=EDGE_LOOP('',(#56881,#56882,#56883,#56884));
#13620=EDGE_LOOP('',(#56885,#56886,#56887,#56888));
#13621=EDGE_LOOP('',(#56889,#56890,#56891,#56892));
#13622=EDGE_LOOP('',(#56893,#56894,#56895,#56896));
#13623=EDGE_LOOP('',(#56897,#56898,#56899,#56900));
#13624=EDGE_LOOP('',(#56901,#56902,#56903,#56904));
#13625=EDGE_LOOP('',(#56905,#56906,#56907,#56908));
#13626=EDGE_LOOP('',(#56909,#56910,#56911,#56912));
#13627=EDGE_LOOP('',(#56913,#56914,#56915,#56916));
#13628=EDGE_LOOP('',(#56917,#56918,#56919,#56920));
#13629=EDGE_LOOP('',(#56921,#56922,#56923,#56924));
#13630=EDGE_LOOP('',(#56925,#56926,#56927,#56928));
#13631=EDGE_LOOP('',(#56929,#56930,#56931,#56932));
#13632=EDGE_LOOP('',(#56933,#56934,#56935,#56936));
#13633=EDGE_LOOP('',(#56937,#56938,#56939,#56940));
#13634=EDGE_LOOP('',(#56941,#56942,#56943,#56944));
#13635=EDGE_LOOP('',(#56945,#56946,#56947,#56948));
#13636=EDGE_LOOP('',(#56949,#56950,#56951,#56952));
#13637=EDGE_LOOP('',(#56953,#56954,#56955,#56956));
#13638=EDGE_LOOP('',(#56957,#56958,#56959,#56960));
#13639=EDGE_LOOP('',(#56961,#56962,#56963,#56964));
#13640=EDGE_LOOP('',(#56965,#56966,#56967,#56968));
#13641=EDGE_LOOP('',(#56969,#56970,#56971,#56972));
#13642=EDGE_LOOP('',(#56973,#56974,#56975,#56976));
#13643=EDGE_LOOP('',(#56977,#56978,#56979,#56980));
#13644=EDGE_LOOP('',(#56981,#56982,#56983,#56984));
#13645=EDGE_LOOP('',(#56985,#56986,#56987,#56988));
#13646=EDGE_LOOP('',(#56989,#56990,#56991,#56992));
#13647=EDGE_LOOP('',(#56993,#56994,#56995,#56996));
#13648=EDGE_LOOP('',(#56997,#56998,#56999,#57000));
#13649=EDGE_LOOP('',(#57001,#57002,#57003,#57004));
#13650=EDGE_LOOP('',(#57005,#57006,#57007,#57008));
#13651=EDGE_LOOP('',(#57009,#57010,#57011,#57012));
#13652=EDGE_LOOP('',(#57013,#57014,#57015,#57016));
#13653=EDGE_LOOP('',(#57017,#57018,#57019,#57020));
#13654=EDGE_LOOP('',(#57021,#57022,#57023,#57024));
#13655=EDGE_LOOP('',(#57025,#57026,#57027,#57028));
#13656=EDGE_LOOP('',(#57029,#57030,#57031,#57032));
#13657=EDGE_LOOP('',(#57033,#57034,#57035,#57036));
#13658=EDGE_LOOP('',(#57037,#57038,#57039,#57040));
#13659=EDGE_LOOP('',(#57041,#57042,#57043,#57044));
#13660=EDGE_LOOP('',(#57045,#57046,#57047,#57048));
#13661=EDGE_LOOP('',(#57049,#57050,#57051,#57052));
#13662=EDGE_LOOP('',(#57053,#57054,#57055,#57056));
#13663=EDGE_LOOP('',(#57057,#57058,#57059,#57060));
#13664=EDGE_LOOP('',(#57061,#57062,#57063,#57064));
#13665=EDGE_LOOP('',(#57065,#57066,#57067,#57068));
#13666=EDGE_LOOP('',(#57069,#57070,#57071,#57072));
#13667=EDGE_LOOP('',(#57073,#57074,#57075,#57076));
#13668=EDGE_LOOP('',(#57077,#57078,#57079,#57080));
#13669=EDGE_LOOP('',(#57081,#57082,#57083,#57084));
#13670=EDGE_LOOP('',(#57085,#57086,#57087,#57088));
#13671=EDGE_LOOP('',(#57089,#57090,#57091,#57092));
#13672=EDGE_LOOP('',(#57093,#57094,#57095,#57096));
#13673=EDGE_LOOP('',(#57097,#57098,#57099,#57100));
#13674=EDGE_LOOP('',(#57101,#57102,#57103,#57104));
#13675=EDGE_LOOP('',(#57105,#57106,#57107,#57108));
#13676=EDGE_LOOP('',(#57109,#57110,#57111,#57112));
#13677=EDGE_LOOP('',(#57113,#57114,#57115,#57116));
#13678=EDGE_LOOP('',(#57117,#57118,#57119,#57120));
#13679=EDGE_LOOP('',(#57121,#57122,#57123,#57124));
#13680=EDGE_LOOP('',(#57125,#57126,#57127,#57128));
#13681=EDGE_LOOP('',(#57129,#57130,#57131,#57132));
#13682=EDGE_LOOP('',(#57133,#57134,#57135,#57136));
#13683=EDGE_LOOP('',(#57137,#57138,#57139,#57140));
#13684=EDGE_LOOP('',(#57141,#57142,#57143,#57144));
#13685=EDGE_LOOP('',(#57145,#57146,#57147,#57148));
#13686=EDGE_LOOP('',(#57149,#57150,#57151,#57152));
#13687=EDGE_LOOP('',(#57153,#57154,#57155,#57156));
#13688=EDGE_LOOP('',(#57157,#57158,#57159,#57160));
#13689=EDGE_LOOP('',(#57161,#57162,#57163,#57164));
#13690=EDGE_LOOP('',(#57165,#57166,#57167,#57168));
#13691=EDGE_LOOP('',(#57169,#57170,#57171,#57172));
#13692=EDGE_LOOP('',(#57173,#57174,#57175,#57176));
#13693=EDGE_LOOP('',(#57177,#57178,#57179,#57180));
#13694=EDGE_LOOP('',(#57181,#57182,#57183,#57184));
#13695=EDGE_LOOP('',(#57185,#57186,#57187,#57188));
#13696=EDGE_LOOP('',(#57189,#57190,#57191,#57192));
#13697=EDGE_LOOP('',(#57193,#57194,#57195,#57196));
#13698=EDGE_LOOP('',(#57197,#57198,#57199,#57200));
#13699=EDGE_LOOP('',(#57201,#57202,#57203,#57204));
#13700=EDGE_LOOP('',(#57205,#57206,#57207,#57208));
#13701=EDGE_LOOP('',(#57209,#57210,#57211,#57212));
#13702=EDGE_LOOP('',(#57213,#57214,#57215,#57216));
#13703=EDGE_LOOP('',(#57217,#57218,#57219,#57220));
#13704=EDGE_LOOP('',(#57221,#57222,#57223,#57224));
#13705=EDGE_LOOP('',(#57225,#57226,#57227,#57228));
#13706=EDGE_LOOP('',(#57229,#57230,#57231,#57232));
#13707=EDGE_LOOP('',(#57233,#57234,#57235,#57236));
#13708=EDGE_LOOP('',(#57237,#57238,#57239,#57240));
#13709=EDGE_LOOP('',(#57241,#57242,#57243,#57244));
#13710=EDGE_LOOP('',(#57245,#57246,#57247,#57248));
#13711=EDGE_LOOP('',(#57249,#57250,#57251,#57252));
#13712=EDGE_LOOP('',(#57253,#57254,#57255,#57256));
#13713=EDGE_LOOP('',(#57257,#57258,#57259,#57260));
#13714=EDGE_LOOP('',(#57261,#57262,#57263,#57264));
#13715=EDGE_LOOP('',(#57265,#57266,#57267,#57268));
#13716=EDGE_LOOP('',(#57269,#57270,#57271,#57272));
#13717=EDGE_LOOP('',(#57273,#57274,#57275,#57276));
#13718=EDGE_LOOP('',(#57277,#57278,#57279,#57280));
#13719=EDGE_LOOP('',(#57281,#57282,#57283,#57284));
#13720=EDGE_LOOP('',(#57285,#57286,#57287,#57288));
#13721=EDGE_LOOP('',(#57289,#57290,#57291,#57292));
#13722=EDGE_LOOP('',(#57293,#57294,#57295,#57296));
#13723=EDGE_LOOP('',(#57297,#57298,#57299,#57300));
#13724=EDGE_LOOP('',(#57301,#57302,#57303,#57304));
#13725=EDGE_LOOP('',(#57305,#57306,#57307,#57308));
#13726=EDGE_LOOP('',(#57309,#57310,#57311,#57312));
#13727=EDGE_LOOP('',(#57313,#57314,#57315,#57316));
#13728=EDGE_LOOP('',(#57317,#57318,#57319,#57320));
#13729=EDGE_LOOP('',(#57321,#57322,#57323,#57324));
#13730=EDGE_LOOP('',(#57325,#57326,#57327,#57328));
#13731=EDGE_LOOP('',(#57329,#57330,#57331,#57332));
#13732=EDGE_LOOP('',(#57333,#57334,#57335,#57336));
#13733=EDGE_LOOP('',(#57337,#57338,#57339,#57340));
#13734=EDGE_LOOP('',(#57341,#57342,#57343,#57344));
#13735=EDGE_LOOP('',(#57345,#57346,#57347,#57348));
#13736=EDGE_LOOP('',(#57349,#57350,#57351,#57352));
#13737=EDGE_LOOP('',(#57353,#57354,#57355,#57356));
#13738=EDGE_LOOP('',(#57357,#57358,#57359,#57360));
#13739=EDGE_LOOP('',(#57361,#57362,#57363,#57364));
#13740=EDGE_LOOP('',(#57365,#57366,#57367,#57368));
#13741=EDGE_LOOP('',(#57369,#57370,#57371,#57372));
#13742=EDGE_LOOP('',(#57373,#57374,#57375,#57376));
#13743=EDGE_LOOP('',(#57377,#57378,#57379,#57380));
#13744=EDGE_LOOP('',(#57381,#57382,#57383,#57384));
#13745=EDGE_LOOP('',(#57385,#57386,#57387,#57388));
#13746=EDGE_LOOP('',(#57389,#57390,#57391,#57392));
#13747=EDGE_LOOP('',(#57393,#57394,#57395,#57396));
#13748=EDGE_LOOP('',(#57397,#57398,#57399,#57400));
#13749=EDGE_LOOP('',(#57401,#57402,#57403,#57404));
#13750=EDGE_LOOP('',(#57405,#57406,#57407,#57408));
#13751=EDGE_LOOP('',(#57409,#57410,#57411,#57412));
#13752=EDGE_LOOP('',(#57413,#57414,#57415,#57416));
#13753=EDGE_LOOP('',(#57417,#57418,#57419,#57420));
#13754=EDGE_LOOP('',(#57421,#57422,#57423,#57424));
#13755=EDGE_LOOP('',(#57425,#57426,#57427,#57428));
#13756=EDGE_LOOP('',(#57429,#57430,#57431,#57432));
#13757=EDGE_LOOP('',(#57433,#57434,#57435,#57436));
#13758=EDGE_LOOP('',(#57437,#57438,#57439,#57440));
#13759=EDGE_LOOP('',(#57441,#57442,#57443,#57444));
#13760=EDGE_LOOP('',(#57445,#57446,#57447,#57448));
#13761=EDGE_LOOP('',(#57449,#57450,#57451,#57452));
#13762=EDGE_LOOP('',(#57453,#57454,#57455,#57456));
#13763=EDGE_LOOP('',(#57457,#57458,#57459,#57460));
#13764=EDGE_LOOP('',(#57461,#57462,#57463,#57464));
#13765=EDGE_LOOP('',(#57465,#57466,#57467,#57468));
#13766=EDGE_LOOP('',(#57469,#57470,#57471,#57472));
#13767=EDGE_LOOP('',(#57473,#57474,#57475,#57476));
#13768=EDGE_LOOP('',(#57477,#57478,#57479,#57480));
#13769=EDGE_LOOP('',(#57481,#57482,#57483,#57484));
#13770=EDGE_LOOP('',(#57485,#57486,#57487,#57488));
#13771=EDGE_LOOP('',(#57489,#57490,#57491,#57492));
#13772=EDGE_LOOP('',(#57493,#57494,#57495,#57496));
#13773=EDGE_LOOP('',(#57497,#57498,#57499,#57500));
#13774=EDGE_LOOP('',(#57501,#57502,#57503,#57504));
#13775=EDGE_LOOP('',(#57505,#57506,#57507,#57508));
#13776=EDGE_LOOP('',(#57509,#57510,#57511,#57512));
#13777=EDGE_LOOP('',(#57513,#57514,#57515,#57516));
#13778=EDGE_LOOP('',(#57517,#57518,#57519,#57520));
#13779=EDGE_LOOP('',(#57521,#57522,#57523,#57524));
#13780=EDGE_LOOP('',(#57525,#57526,#57527,#57528));
#13781=EDGE_LOOP('',(#57529,#57530,#57531,#57532));
#13782=EDGE_LOOP('',(#57533,#57534,#57535,#57536));
#13783=EDGE_LOOP('',(#57537,#57538,#57539,#57540));
#13784=EDGE_LOOP('',(#57541,#57542,#57543,#57544));
#13785=EDGE_LOOP('',(#57545,#57546,#57547,#57548));
#13786=EDGE_LOOP('',(#57549,#57550,#57551,#57552));
#13787=EDGE_LOOP('',(#57553,#57554,#57555,#57556));
#13788=EDGE_LOOP('',(#57557,#57558,#57559,#57560));
#13789=EDGE_LOOP('',(#57561,#57562,#57563,#57564));
#13790=EDGE_LOOP('',(#57565,#57566,#57567,#57568));
#13791=EDGE_LOOP('',(#57569,#57570,#57571,#57572));
#13792=EDGE_LOOP('',(#57573,#57574,#57575,#57576));
#13793=EDGE_LOOP('',(#57577,#57578,#57579,#57580));
#13794=EDGE_LOOP('',(#57581,#57582,#57583,#57584));
#13795=EDGE_LOOP('',(#57585,#57586,#57587,#57588));
#13796=EDGE_LOOP('',(#57589,#57590,#57591,#57592));
#13797=EDGE_LOOP('',(#57593,#57594,#57595,#57596));
#13798=EDGE_LOOP('',(#57597,#57598,#57599,#57600));
#13799=EDGE_LOOP('',(#57601,#57602,#57603,#57604));
#13800=EDGE_LOOP('',(#57605,#57606,#57607,#57608));
#13801=EDGE_LOOP('',(#57609,#57610,#57611,#57612));
#13802=EDGE_LOOP('',(#57613,#57614,#57615,#57616));
#13803=EDGE_LOOP('',(#57617,#57618,#57619,#57620));
#13804=EDGE_LOOP('',(#57621,#57622,#57623,#57624));
#13805=EDGE_LOOP('',(#57625,#57626,#57627,#57628));
#13806=EDGE_LOOP('',(#57629,#57630,#57631,#57632));
#13807=EDGE_LOOP('',(#57633,#57634,#57635,#57636));
#13808=EDGE_LOOP('',(#57637,#57638,#57639,#57640));
#13809=EDGE_LOOP('',(#57641,#57642,#57643,#57644));
#13810=EDGE_LOOP('',(#57645,#57646,#57647,#57648));
#13811=EDGE_LOOP('',(#57649,#57650,#57651,#57652));
#13812=EDGE_LOOP('',(#57653,#57654,#57655,#57656));
#13813=EDGE_LOOP('',(#57657,#57658,#57659,#57660));
#13814=EDGE_LOOP('',(#57661,#57662,#57663,#57664));
#13815=EDGE_LOOP('',(#57665,#57666,#57667,#57668));
#13816=EDGE_LOOP('',(#57669,#57670,#57671,#57672));
#13817=EDGE_LOOP('',(#57673,#57674,#57675,#57676));
#13818=EDGE_LOOP('',(#57677,#57678,#57679,#57680));
#13819=EDGE_LOOP('',(#57681,#57682,#57683,#57684));
#13820=EDGE_LOOP('',(#57685,#57686,#57687,#57688));
#13821=EDGE_LOOP('',(#57689,#57690,#57691,#57692));
#13822=EDGE_LOOP('',(#57693,#57694,#57695,#57696));
#13823=EDGE_LOOP('',(#57697,#57698,#57699,#57700));
#13824=EDGE_LOOP('',(#57701,#57702,#57703,#57704));
#13825=EDGE_LOOP('',(#57705,#57706,#57707,#57708));
#13826=EDGE_LOOP('',(#57709,#57710,#57711,#57712));
#13827=EDGE_LOOP('',(#57713,#57714,#57715,#57716));
#13828=EDGE_LOOP('',(#57717,#57718,#57719,#57720));
#13829=EDGE_LOOP('',(#57721,#57722,#57723,#57724));
#13830=EDGE_LOOP('',(#57725,#57726,#57727,#57728));
#13831=EDGE_LOOP('',(#57729,#57730,#57731,#57732));
#13832=EDGE_LOOP('',(#57733,#57734,#57735,#57736));
#13833=EDGE_LOOP('',(#57737,#57738,#57739,#57740));
#13834=EDGE_LOOP('',(#57741,#57742,#57743,#57744));
#13835=EDGE_LOOP('',(#57745,#57746,#57747,#57748));
#13836=EDGE_LOOP('',(#57749,#57750,#57751,#57752));
#13837=EDGE_LOOP('',(#57753,#57754,#57755,#57756));
#13838=EDGE_LOOP('',(#57757,#57758,#57759,#57760));
#13839=EDGE_LOOP('',(#57761,#57762,#57763,#57764));
#13840=EDGE_LOOP('',(#57765,#57766,#57767,#57768));
#13841=EDGE_LOOP('',(#57769,#57770,#57771,#57772));
#13842=EDGE_LOOP('',(#57773,#57774,#57775,#57776));
#13843=EDGE_LOOP('',(#57777,#57778,#57779,#57780));
#13844=EDGE_LOOP('',(#57781,#57782,#57783,#57784));
#13845=EDGE_LOOP('',(#57785,#57786,#57787,#57788));
#13846=EDGE_LOOP('',(#57789,#57790,#57791,#57792));
#13847=EDGE_LOOP('',(#57793,#57794,#57795,#57796));
#13848=EDGE_LOOP('',(#57797,#57798,#57799,#57800));
#13849=EDGE_LOOP('',(#57801,#57802,#57803,#57804));
#13850=EDGE_LOOP('',(#57805,#57806,#57807,#57808));
#13851=EDGE_LOOP('',(#57809,#57810,#57811,#57812));
#13852=EDGE_LOOP('',(#57813,#57814,#57815,#57816));
#13853=EDGE_LOOP('',(#57817,#57818,#57819,#57820));
#13854=EDGE_LOOP('',(#57821,#57822,#57823,#57824));
#13855=EDGE_LOOP('',(#57825,#57826,#57827,#57828));
#13856=EDGE_LOOP('',(#57829,#57830,#57831,#57832));
#13857=EDGE_LOOP('',(#57833,#57834,#57835,#57836));
#13858=EDGE_LOOP('',(#57837,#57838,#57839,#57840));
#13859=EDGE_LOOP('',(#57841,#57842,#57843,#57844));
#13860=EDGE_LOOP('',(#57845,#57846,#57847,#57848));
#13861=EDGE_LOOP('',(#57849,#57850,#57851,#57852));
#13862=EDGE_LOOP('',(#57853,#57854,#57855,#57856));
#13863=EDGE_LOOP('',(#57857,#57858,#57859,#57860));
#13864=EDGE_LOOP('',(#57861,#57862,#57863,#57864));
#13865=EDGE_LOOP('',(#57865,#57866,#57867,#57868));
#13866=EDGE_LOOP('',(#57869,#57870,#57871,#57872));
#13867=EDGE_LOOP('',(#57873,#57874,#57875,#57876));
#13868=EDGE_LOOP('',(#57877,#57878,#57879,#57880));
#13869=EDGE_LOOP('',(#57881,#57882,#57883,#57884));
#13870=EDGE_LOOP('',(#57885,#57886,#57887,#57888));
#13871=EDGE_LOOP('',(#57889,#57890,#57891,#57892));
#13872=EDGE_LOOP('',(#57893,#57894,#57895,#57896));
#13873=EDGE_LOOP('',(#57897,#57898,#57899,#57900));
#13874=EDGE_LOOP('',(#57901,#57902,#57903,#57904));
#13875=EDGE_LOOP('',(#57905,#57906,#57907,#57908));
#13876=EDGE_LOOP('',(#57909,#57910,#57911,#57912));
#13877=EDGE_LOOP('',(#57913,#57914,#57915,#57916));
#13878=EDGE_LOOP('',(#57917,#57918,#57919,#57920));
#13879=EDGE_LOOP('',(#57921,#57922,#57923,#57924));
#13880=EDGE_LOOP('',(#57925,#57926,#57927,#57928));
#13881=EDGE_LOOP('',(#57929,#57930,#57931,#57932));
#13882=EDGE_LOOP('',(#57933,#57934,#57935,#57936));
#13883=EDGE_LOOP('',(#57937,#57938,#57939,#57940));
#13884=EDGE_LOOP('',(#57941,#57942,#57943,#57944));
#13885=EDGE_LOOP('',(#57945,#57946,#57947,#57948));
#13886=EDGE_LOOP('',(#57949,#57950,#57951,#57952));
#13887=EDGE_LOOP('',(#57953,#57954,#57955,#57956));
#13888=EDGE_LOOP('',(#57957,#57958,#57959,#57960));
#13889=EDGE_LOOP('',(#57961,#57962,#57963,#57964));
#13890=EDGE_LOOP('',(#57965,#57966,#57967,#57968));
#13891=EDGE_LOOP('',(#57969,#57970,#57971,#57972));
#13892=EDGE_LOOP('',(#57973,#57974,#57975,#57976));
#13893=EDGE_LOOP('',(#57977,#57978,#57979,#57980));
#13894=EDGE_LOOP('',(#57981,#57982,#57983,#57984));
#13895=EDGE_LOOP('',(#57985,#57986,#57987,#57988));
#13896=EDGE_LOOP('',(#57989,#57990,#57991,#57992));
#13897=EDGE_LOOP('',(#57993,#57994,#57995,#57996));
#13898=EDGE_LOOP('',(#57997,#57998,#57999,#58000));
#13899=EDGE_LOOP('',(#58001,#58002,#58003,#58004));
#13900=EDGE_LOOP('',(#58005,#58006,#58007,#58008));
#13901=EDGE_LOOP('',(#58009,#58010,#58011,#58012));
#13902=EDGE_LOOP('',(#58013,#58014,#58015,#58016));
#13903=EDGE_LOOP('',(#58017,#58018,#58019,#58020));
#13904=EDGE_LOOP('',(#58021,#58022,#58023,#58024));
#13905=EDGE_LOOP('',(#58025,#58026,#58027,#58028));
#13906=EDGE_LOOP('',(#58029,#58030,#58031,#58032));
#13907=EDGE_LOOP('',(#58033,#58034,#58035,#58036));
#13908=EDGE_LOOP('',(#58037,#58038,#58039,#58040));
#13909=EDGE_LOOP('',(#58041,#58042,#58043,#58044));
#13910=EDGE_LOOP('',(#58045,#58046,#58047,#58048));
#13911=EDGE_LOOP('',(#58049,#58050,#58051,#58052));
#13912=EDGE_LOOP('',(#58053,#58054,#58055,#58056));
#13913=EDGE_LOOP('',(#58057,#58058,#58059,#58060));
#13914=EDGE_LOOP('',(#58061,#58062,#58063,#58064));
#13915=EDGE_LOOP('',(#58065,#58066,#58067,#58068));
#13916=EDGE_LOOP('',(#58069,#58070,#58071,#58072));
#13917=EDGE_LOOP('',(#58073,#58074,#58075,#58076));
#13918=EDGE_LOOP('',(#58077,#58078,#58079,#58080));
#13919=EDGE_LOOP('',(#58081,#58082,#58083,#58084));
#13920=EDGE_LOOP('',(#58085,#58086,#58087,#58088));
#13921=EDGE_LOOP('',(#58089,#58090,#58091,#58092));
#13922=EDGE_LOOP('',(#58093,#58094,#58095,#58096));
#13923=EDGE_LOOP('',(#58097,#58098,#58099,#58100));
#13924=EDGE_LOOP('',(#58101,#58102,#58103,#58104));
#13925=EDGE_LOOP('',(#58105,#58106,#58107,#58108));
#13926=EDGE_LOOP('',(#58109,#58110,#58111,#58112));
#13927=EDGE_LOOP('',(#58113,#58114,#58115,#58116));
#13928=EDGE_LOOP('',(#58117,#58118,#58119,#58120));
#13929=EDGE_LOOP('',(#58121,#58122,#58123,#58124));
#13930=EDGE_LOOP('',(#58125,#58126,#58127,#58128));
#13931=EDGE_LOOP('',(#58129,#58130,#58131,#58132));
#13932=EDGE_LOOP('',(#58133,#58134,#58135,#58136));
#13933=EDGE_LOOP('',(#58137,#58138,#58139,#58140));
#13934=EDGE_LOOP('',(#58141,#58142,#58143,#58144));
#13935=EDGE_LOOP('',(#58145,#58146,#58147,#58148));
#13936=EDGE_LOOP('',(#58149,#58150,#58151,#58152));
#13937=EDGE_LOOP('',(#58153,#58154,#58155,#58156));
#13938=EDGE_LOOP('',(#58157,#58158,#58159,#58160));
#13939=EDGE_LOOP('',(#58161,#58162,#58163,#58164));
#13940=EDGE_LOOP('',(#58165,#58166,#58167,#58168));
#13941=EDGE_LOOP('',(#58169,#58170,#58171,#58172));
#13942=EDGE_LOOP('',(#58173,#58174,#58175,#58176));
#13943=EDGE_LOOP('',(#58177,#58178,#58179,#58180));
#13944=EDGE_LOOP('',(#58181,#58182,#58183,#58184));
#13945=EDGE_LOOP('',(#58185,#58186,#58187,#58188));
#13946=EDGE_LOOP('',(#58189,#58190,#58191,#58192));
#13947=EDGE_LOOP('',(#58193,#58194,#58195,#58196));
#13948=EDGE_LOOP('',(#58197,#58198,#58199,#58200));
#13949=EDGE_LOOP('',(#58201,#58202,#58203,#58204));
#13950=EDGE_LOOP('',(#58205,#58206,#58207,#58208));
#13951=EDGE_LOOP('',(#58209,#58210,#58211,#58212));
#13952=EDGE_LOOP('',(#58213,#58214,#58215,#58216));
#13953=EDGE_LOOP('',(#58217,#58218,#58219,#58220));
#13954=EDGE_LOOP('',(#58221,#58222,#58223,#58224));
#13955=EDGE_LOOP('',(#58225,#58226,#58227,#58228));
#13956=EDGE_LOOP('',(#58229,#58230,#58231,#58232));
#13957=EDGE_LOOP('',(#58233,#58234,#58235,#58236));
#13958=EDGE_LOOP('',(#58237,#58238,#58239,#58240));
#13959=EDGE_LOOP('',(#58241,#58242,#58243,#58244));
#13960=EDGE_LOOP('',(#58245,#58246,#58247,#58248));
#13961=EDGE_LOOP('',(#58249,#58250,#58251,#58252));
#13962=EDGE_LOOP('',(#58253,#58254,#58255,#58256));
#13963=EDGE_LOOP('',(#58257,#58258,#58259,#58260));
#13964=EDGE_LOOP('',(#58261,#58262,#58263,#58264));
#13965=EDGE_LOOP('',(#58265,#58266,#58267,#58268));
#13966=EDGE_LOOP('',(#58269,#58270,#58271,#58272));
#13967=EDGE_LOOP('',(#58273,#58274,#58275,#58276));
#13968=EDGE_LOOP('',(#58277,#58278,#58279,#58280));
#13969=EDGE_LOOP('',(#58281,#58282,#58283,#58284));
#13970=EDGE_LOOP('',(#58285,#58286,#58287,#58288));
#13971=EDGE_LOOP('',(#58289,#58290,#58291,#58292));
#13972=EDGE_LOOP('',(#58293,#58294,#58295,#58296));
#13973=EDGE_LOOP('',(#58297,#58298,#58299,#58300));
#13974=EDGE_LOOP('',(#58301,#58302,#58303,#58304));
#13975=EDGE_LOOP('',(#58305,#58306,#58307,#58308));
#13976=EDGE_LOOP('',(#58309,#58310,#58311,#58312));
#13977=EDGE_LOOP('',(#58313,#58314,#58315,#58316));
#13978=EDGE_LOOP('',(#58317,#58318,#58319,#58320));
#13979=EDGE_LOOP('',(#58321,#58322,#58323,#58324));
#13980=EDGE_LOOP('',(#58325,#58326,#58327,#58328));
#13981=EDGE_LOOP('',(#58329,#58330,#58331,#58332));
#13982=EDGE_LOOP('',(#58333,#58334,#58335,#58336));
#13983=EDGE_LOOP('',(#58337,#58338,#58339,#58340));
#13984=EDGE_LOOP('',(#58341,#58342,#58343,#58344));
#13985=EDGE_LOOP('',(#58345,#58346,#58347,#58348));
#13986=EDGE_LOOP('',(#58349,#58350,#58351,#58352));
#13987=EDGE_LOOP('',(#58353,#58354,#58355,#58356));
#13988=EDGE_LOOP('',(#58357,#58358,#58359,#58360));
#13989=EDGE_LOOP('',(#58361,#58362,#58363,#58364));
#13990=EDGE_LOOP('',(#58365,#58366,#58367,#58368));
#13991=EDGE_LOOP('',(#58369,#58370,#58371,#58372));
#13992=EDGE_LOOP('',(#58373,#58374,#58375,#58376));
#13993=EDGE_LOOP('',(#58377,#58378,#58379,#58380));
#13994=EDGE_LOOP('',(#58381,#58382,#58383,#58384));
#13995=EDGE_LOOP('',(#58385,#58386,#58387,#58388));
#13996=EDGE_LOOP('',(#58389,#58390,#58391,#58392));
#13997=EDGE_LOOP('',(#58393,#58394,#58395,#58396));
#13998=EDGE_LOOP('',(#58397,#58398,#58399,#58400));
#13999=EDGE_LOOP('',(#58401,#58402,#58403,#58404));
#14000=EDGE_LOOP('',(#58405,#58406,#58407,#58408));
#14001=EDGE_LOOP('',(#58409,#58410,#58411,#58412));
#14002=EDGE_LOOP('',(#58413,#58414,#58415,#58416));
#14003=EDGE_LOOP('',(#58417,#58418,#58419,#58420));
#14004=EDGE_LOOP('',(#58421,#58422,#58423,#58424));
#14005=EDGE_LOOP('',(#58425,#58426,#58427,#58428));
#14006=EDGE_LOOP('',(#58429,#58430,#58431,#58432));
#14007=EDGE_LOOP('',(#58433,#58434,#58435,#58436));
#14008=EDGE_LOOP('',(#58437,#58438,#58439,#58440));
#14009=EDGE_LOOP('',(#58441,#58442,#58443,#58444));
#14010=EDGE_LOOP('',(#58445,#58446,#58447,#58448));
#14011=EDGE_LOOP('',(#58449,#58450,#58451,#58452));
#14012=EDGE_LOOP('',(#58453,#58454,#58455,#58456));
#14013=EDGE_LOOP('',(#58457,#58458,#58459,#58460));
#14014=EDGE_LOOP('',(#58461,#58462,#58463,#58464));
#14015=EDGE_LOOP('',(#58465,#58466,#58467,#58468));
#14016=EDGE_LOOP('',(#58469,#58470,#58471,#58472));
#14017=EDGE_LOOP('',(#58473,#58474,#58475,#58476));
#14018=EDGE_LOOP('',(#58477,#58478,#58479,#58480));
#14019=EDGE_LOOP('',(#58481,#58482,#58483,#58484));
#14020=EDGE_LOOP('',(#58485,#58486,#58487,#58488));
#14021=EDGE_LOOP('',(#58489,#58490,#58491,#58492));
#14022=EDGE_LOOP('',(#58493,#58494,#58495,#58496));
#14023=EDGE_LOOP('',(#58497,#58498,#58499,#58500));
#14024=EDGE_LOOP('',(#58501,#58502,#58503,#58504));
#14025=EDGE_LOOP('',(#58505,#58506,#58507,#58508));
#14026=EDGE_LOOP('',(#58509,#58510,#58511,#58512));
#14027=EDGE_LOOP('',(#58513,#58514,#58515,#58516));
#14028=EDGE_LOOP('',(#58517,#58518,#58519,#58520));
#14029=EDGE_LOOP('',(#58521,#58522,#58523,#58524));
#14030=EDGE_LOOP('',(#58525,#58526,#58527,#58528));
#14031=EDGE_LOOP('',(#58529,#58530,#58531,#58532));
#14032=EDGE_LOOP('',(#58533,#58534,#58535,#58536));
#14033=EDGE_LOOP('',(#58537,#58538,#58539,#58540));
#14034=EDGE_LOOP('',(#58541,#58542,#58543,#58544));
#14035=EDGE_LOOP('',(#58545,#58546,#58547,#58548));
#14036=EDGE_LOOP('',(#58549,#58550,#58551,#58552));
#14037=EDGE_LOOP('',(#58553,#58554,#58555,#58556));
#14038=EDGE_LOOP('',(#58557,#58558,#58559,#58560));
#14039=EDGE_LOOP('',(#58561,#58562,#58563,#58564));
#14040=EDGE_LOOP('',(#58565,#58566,#58567,#58568));
#14041=EDGE_LOOP('',(#58569,#58570,#58571,#58572));
#14042=EDGE_LOOP('',(#58573,#58574,#58575,#58576));
#14043=EDGE_LOOP('',(#58577,#58578,#58579,#58580));
#14044=EDGE_LOOP('',(#58581,#58582,#58583,#58584));
#14045=EDGE_LOOP('',(#58585,#58586,#58587,#58588));
#14046=EDGE_LOOP('',(#58589,#58590,#58591,#58592));
#14047=EDGE_LOOP('',(#58593,#58594,#58595,#58596));
#14048=EDGE_LOOP('',(#58597,#58598,#58599,#58600));
#14049=EDGE_LOOP('',(#58601,#58602,#58603,#58604));
#14050=EDGE_LOOP('',(#58605,#58606,#58607,#58608));
#14051=EDGE_LOOP('',(#58609,#58610,#58611,#58612));
#14052=EDGE_LOOP('',(#58613,#58614,#58615,#58616));
#14053=EDGE_LOOP('',(#58617,#58618,#58619,#58620));
#14054=EDGE_LOOP('',(#58621,#58622,#58623,#58624));
#14055=EDGE_LOOP('',(#58625,#58626,#58627,#58628));
#14056=EDGE_LOOP('',(#58629,#58630,#58631,#58632));
#14057=EDGE_LOOP('',(#58633,#58634,#58635,#58636));
#14058=EDGE_LOOP('',(#58637,#58638,#58639,#58640));
#14059=EDGE_LOOP('',(#58641,#58642,#58643,#58644));
#14060=EDGE_LOOP('',(#58645,#58646,#58647,#58648));
#14061=EDGE_LOOP('',(#58649,#58650,#58651,#58652));
#14062=EDGE_LOOP('',(#58653,#58654,#58655,#58656));
#14063=EDGE_LOOP('',(#58657,#58658,#58659,#58660));
#14064=EDGE_LOOP('',(#58661,#58662,#58663,#58664));
#14065=EDGE_LOOP('',(#58665,#58666,#58667,#58668));
#14066=EDGE_LOOP('',(#58669,#58670,#58671,#58672));
#14067=EDGE_LOOP('',(#58673,#58674,#58675,#58676));
#14068=EDGE_LOOP('',(#58677,#58678,#58679,#58680));
#14069=EDGE_LOOP('',(#58681,#58682,#58683,#58684));
#14070=EDGE_LOOP('',(#58685,#58686,#58687,#58688));
#14071=EDGE_LOOP('',(#58689,#58690,#58691,#58692));
#14072=EDGE_LOOP('',(#58693,#58694,#58695,#58696));
#14073=EDGE_LOOP('',(#58697,#58698,#58699,#58700));
#14074=EDGE_LOOP('',(#58701,#58702,#58703,#58704));
#14075=EDGE_LOOP('',(#58705,#58706,#58707,#58708));
#14076=EDGE_LOOP('',(#58709,#58710,#58711,#58712));
#14077=EDGE_LOOP('',(#58713,#58714,#58715,#58716));
#14078=EDGE_LOOP('',(#58717,#58718,#58719,#58720));
#14079=EDGE_LOOP('',(#58721,#58722,#58723,#58724));
#14080=EDGE_LOOP('',(#58725,#58726,#58727,#58728));
#14081=EDGE_LOOP('',(#58729,#58730,#58731,#58732));
#14082=EDGE_LOOP('',(#58733,#58734,#58735,#58736));
#14083=EDGE_LOOP('',(#58737,#58738,#58739,#58740));
#14084=EDGE_LOOP('',(#58741,#58742,#58743,#58744));
#14085=EDGE_LOOP('',(#58745,#58746,#58747,#58748));
#14086=EDGE_LOOP('',(#58749,#58750,#58751,#58752));
#14087=EDGE_LOOP('',(#58753,#58754,#58755,#58756));
#14088=EDGE_LOOP('',(#58757,#58758,#58759,#58760));
#14089=EDGE_LOOP('',(#58761,#58762,#58763,#58764));
#14090=EDGE_LOOP('',(#58765,#58766,#58767,#58768));
#14091=EDGE_LOOP('',(#58769,#58770,#58771,#58772));
#14092=EDGE_LOOP('',(#58773,#58774,#58775,#58776));
#14093=EDGE_LOOP('',(#58777,#58778,#58779,#58780));
#14094=EDGE_LOOP('',(#58781,#58782,#58783,#58784));
#14095=EDGE_LOOP('',(#58785,#58786,#58787,#58788));
#14096=EDGE_LOOP('',(#58789,#58790,#58791,#58792));
#14097=EDGE_LOOP('',(#58793,#58794,#58795,#58796));
#14098=EDGE_LOOP('',(#58797,#58798,#58799,#58800));
#14099=EDGE_LOOP('',(#58801,#58802,#58803,#58804));
#14100=EDGE_LOOP('',(#58805,#58806,#58807,#58808));
#14101=EDGE_LOOP('',(#58809,#58810,#58811,#58812));
#14102=EDGE_LOOP('',(#58813,#58814,#58815,#58816));
#14103=EDGE_LOOP('',(#58817,#58818,#58819,#58820));
#14104=EDGE_LOOP('',(#58821,#58822,#58823,#58824));
#14105=EDGE_LOOP('',(#58825,#58826,#58827,#58828));
#14106=EDGE_LOOP('',(#58829,#58830,#58831,#58832));
#14107=EDGE_LOOP('',(#58833,#58834,#58835,#58836));
#14108=EDGE_LOOP('',(#58837,#58838,#58839,#58840));
#14109=EDGE_LOOP('',(#58841,#58842,#58843,#58844));
#14110=EDGE_LOOP('',(#58845,#58846,#58847,#58848));
#14111=EDGE_LOOP('',(#58849,#58850,#58851,#58852));
#14112=EDGE_LOOP('',(#58853,#58854,#58855,#58856));
#14113=EDGE_LOOP('',(#58857,#58858,#58859,#58860));
#14114=EDGE_LOOP('',(#58861,#58862,#58863,#58864));
#14115=EDGE_LOOP('',(#58865,#58866,#58867,#58868));
#14116=EDGE_LOOP('',(#58869,#58870,#58871,#58872));
#14117=EDGE_LOOP('',(#58873,#58874,#58875,#58876));
#14118=EDGE_LOOP('',(#58877,#58878,#58879,#58880));
#14119=EDGE_LOOP('',(#58881,#58882,#58883,#58884));
#14120=EDGE_LOOP('',(#58885,#58886,#58887,#58888));
#14121=EDGE_LOOP('',(#58889,#58890,#58891,#58892));
#14122=EDGE_LOOP('',(#58893,#58894,#58895,#58896));
#14123=EDGE_LOOP('',(#58897,#58898,#58899,#58900));
#14124=EDGE_LOOP('',(#58901,#58902,#58903,#58904));
#14125=EDGE_LOOP('',(#58905,#58906,#58907,#58908));
#14126=EDGE_LOOP('',(#58909,#58910,#58911,#58912));
#14127=EDGE_LOOP('',(#58913,#58914,#58915,#58916));
#14128=EDGE_LOOP('',(#58917,#58918,#58919,#58920));
#14129=EDGE_LOOP('',(#58921,#58922,#58923,#58924));
#14130=EDGE_LOOP('',(#58925,#58926,#58927,#58928));
#14131=EDGE_LOOP('',(#58929,#58930,#58931,#58932));
#14132=EDGE_LOOP('',(#58933,#58934,#58935,#58936));
#14133=EDGE_LOOP('',(#58937,#58938,#58939,#58940));
#14134=EDGE_LOOP('',(#58941,#58942,#58943,#58944));
#14135=EDGE_LOOP('',(#58945,#58946,#58947,#58948));
#14136=EDGE_LOOP('',(#58949,#58950,#58951,#58952));
#14137=EDGE_LOOP('',(#58953,#58954,#58955,#58956));
#14138=EDGE_LOOP('',(#58957,#58958,#58959,#58960));
#14139=EDGE_LOOP('',(#58961,#58962,#58963,#58964));
#14140=EDGE_LOOP('',(#58965,#58966,#58967,#58968));
#14141=EDGE_LOOP('',(#58969,#58970,#58971,#58972));
#14142=EDGE_LOOP('',(#58973,#58974,#58975,#58976));
#14143=EDGE_LOOP('',(#58977,#58978,#58979,#58980));
#14144=EDGE_LOOP('',(#58981,#58982,#58983,#58984));
#14145=EDGE_LOOP('',(#58985,#58986,#58987,#58988));
#14146=EDGE_LOOP('',(#58989,#58990,#58991,#58992));
#14147=EDGE_LOOP('',(#58993,#58994,#58995,#58996));
#14148=EDGE_LOOP('',(#58997,#58998,#58999,#59000));
#14149=EDGE_LOOP('',(#59001,#59002,#59003,#59004));
#14150=EDGE_LOOP('',(#59005,#59006,#59007,#59008));
#14151=EDGE_LOOP('',(#59009,#59010,#59011,#59012));
#14152=EDGE_LOOP('',(#59013,#59014,#59015,#59016));
#14153=EDGE_LOOP('',(#59017,#59018,#59019,#59020));
#14154=EDGE_LOOP('',(#59021,#59022,#59023,#59024));
#14155=EDGE_LOOP('',(#59025,#59026,#59027,#59028));
#14156=EDGE_LOOP('',(#59029,#59030,#59031,#59032));
#14157=EDGE_LOOP('',(#59033,#59034,#59035,#59036));
#14158=EDGE_LOOP('',(#59037,#59038,#59039,#59040));
#14159=EDGE_LOOP('',(#59041,#59042,#59043,#59044));
#14160=EDGE_LOOP('',(#59045,#59046,#59047,#59048));
#14161=EDGE_LOOP('',(#59049,#59050,#59051,#59052));
#14162=EDGE_LOOP('',(#59053,#59054,#59055,#59056));
#14163=EDGE_LOOP('',(#59057,#59058,#59059,#59060));
#14164=EDGE_LOOP('',(#59061,#59062,#59063,#59064));
#14165=EDGE_LOOP('',(#59065,#59066,#59067,#59068));
#14166=EDGE_LOOP('',(#59069,#59070,#59071,#59072));
#14167=EDGE_LOOP('',(#59073,#59074,#59075,#59076));
#14168=EDGE_LOOP('',(#59077,#59078,#59079,#59080));
#14169=EDGE_LOOP('',(#59081,#59082,#59083,#59084));
#14170=EDGE_LOOP('',(#59085,#59086,#59087,#59088));
#14171=EDGE_LOOP('',(#59089,#59090,#59091,#59092));
#14172=EDGE_LOOP('',(#59093,#59094,#59095,#59096));
#14173=EDGE_LOOP('',(#59097,#59098,#59099,#59100));
#14174=EDGE_LOOP('',(#59101,#59102,#59103,#59104));
#14175=EDGE_LOOP('',(#59105,#59106,#59107,#59108));
#14176=EDGE_LOOP('',(#59109,#59110,#59111,#59112));
#14177=EDGE_LOOP('',(#59113,#59114,#59115,#59116));
#14178=EDGE_LOOP('',(#59117,#59118,#59119,#59120));
#14179=EDGE_LOOP('',(#59121,#59122,#59123,#59124));
#14180=EDGE_LOOP('',(#59125,#59126,#59127,#59128));
#14181=EDGE_LOOP('',(#59129,#59130,#59131,#59132));
#14182=EDGE_LOOP('',(#59133,#59134,#59135,#59136));
#14183=EDGE_LOOP('',(#59137,#59138,#59139,#59140));
#14184=EDGE_LOOP('',(#59141,#59142,#59143,#59144));
#14185=EDGE_LOOP('',(#59145,#59146,#59147,#59148));
#14186=EDGE_LOOP('',(#59149,#59150,#59151,#59152));
#14187=EDGE_LOOP('',(#59153,#59154,#59155,#59156));
#14188=EDGE_LOOP('',(#59157,#59158,#59159,#59160));
#14189=EDGE_LOOP('',(#59161,#59162,#59163,#59164));
#14190=EDGE_LOOP('',(#59165,#59166,#59167,#59168));
#14191=EDGE_LOOP('',(#59169,#59170,#59171,#59172));
#14192=EDGE_LOOP('',(#59173,#59174,#59175,#59176));
#14193=EDGE_LOOP('',(#59177,#59178,#59179,#59180));
#14194=EDGE_LOOP('',(#59181,#59182,#59183,#59184));
#14195=EDGE_LOOP('',(#59185,#59186,#59187,#59188));
#14196=EDGE_LOOP('',(#59189,#59190,#59191,#59192));
#14197=EDGE_LOOP('',(#59193,#59194,#59195,#59196));
#14198=EDGE_LOOP('',(#59197,#59198,#59199,#59200));
#14199=EDGE_LOOP('',(#59201,#59202,#59203,#59204));
#14200=EDGE_LOOP('',(#59205,#59206,#59207,#59208));
#14201=EDGE_LOOP('',(#59209,#59210,#59211,#59212));
#14202=EDGE_LOOP('',(#59213,#59214,#59215,#59216));
#14203=EDGE_LOOP('',(#59217,#59218,#59219,#59220));
#14204=EDGE_LOOP('',(#59221,#59222,#59223,#59224));
#14205=EDGE_LOOP('',(#59225,#59226,#59227,#59228));
#14206=EDGE_LOOP('',(#59229,#59230,#59231,#59232));
#14207=EDGE_LOOP('',(#59233,#59234,#59235,#59236));
#14208=EDGE_LOOP('',(#59237,#59238,#59239,#59240));
#14209=EDGE_LOOP('',(#59241,#59242,#59243,#59244));
#14210=EDGE_LOOP('',(#59245,#59246,#59247,#59248));
#14211=EDGE_LOOP('',(#59249,#59250,#59251,#59252));
#14212=EDGE_LOOP('',(#59253,#59254,#59255,#59256));
#14213=EDGE_LOOP('',(#59257,#59258,#59259,#59260));
#14214=EDGE_LOOP('',(#59261,#59262,#59263,#59264));
#14215=EDGE_LOOP('',(#59265,#59266,#59267,#59268));
#14216=EDGE_LOOP('',(#59269,#59270,#59271,#59272));
#14217=EDGE_LOOP('',(#59273,#59274,#59275,#59276));
#14218=EDGE_LOOP('',(#59277,#59278,#59279,#59280));
#14219=EDGE_LOOP('',(#59281,#59282,#59283,#59284));
#14220=EDGE_LOOP('',(#59285,#59286,#59287,#59288));
#14221=EDGE_LOOP('',(#59289,#59290,#59291,#59292));
#14222=EDGE_LOOP('',(#59293,#59294,#59295,#59296));
#14223=EDGE_LOOP('',(#59297,#59298,#59299,#59300));
#14224=EDGE_LOOP('',(#59301,#59302,#59303,#59304));
#14225=EDGE_LOOP('',(#59305,#59306,#59307,#59308));
#14226=EDGE_LOOP('',(#59309,#59310,#59311,#59312));
#14227=EDGE_LOOP('',(#59313,#59314,#59315,#59316));
#14228=EDGE_LOOP('',(#59317,#59318,#59319,#59320));
#14229=EDGE_LOOP('',(#59321,#59322,#59323,#59324));
#14230=EDGE_LOOP('',(#59325,#59326,#59327,#59328));
#14231=EDGE_LOOP('',(#59329,#59330,#59331,#59332));
#14232=EDGE_LOOP('',(#59333,#59334,#59335,#59336));
#14233=EDGE_LOOP('',(#59337,#59338,#59339,#59340));
#14234=EDGE_LOOP('',(#59341,#59342,#59343,#59344));
#14235=EDGE_LOOP('',(#59345,#59346,#59347,#59348));
#14236=EDGE_LOOP('',(#59349,#59350,#59351,#59352));
#14237=EDGE_LOOP('',(#59353,#59354,#59355,#59356));
#14238=EDGE_LOOP('',(#59357,#59358,#59359,#59360));
#14239=EDGE_LOOP('',(#59361,#59362,#59363,#59364));
#14240=EDGE_LOOP('',(#59365,#59366,#59367,#59368));
#14241=EDGE_LOOP('',(#59369,#59370,#59371,#59372));
#14242=EDGE_LOOP('',(#59373,#59374,#59375,#59376));
#14243=EDGE_LOOP('',(#59377,#59378,#59379,#59380));
#14244=EDGE_LOOP('',(#59381,#59382,#59383,#59384));
#14245=EDGE_LOOP('',(#59385,#59386,#59387,#59388));
#14246=EDGE_LOOP('',(#59389,#59390,#59391,#59392));
#14247=EDGE_LOOP('',(#59393,#59394,#59395,#59396));
#14248=EDGE_LOOP('',(#59397,#59398,#59399,#59400));
#14249=EDGE_LOOP('',(#59401,#59402,#59403,#59404));
#14250=EDGE_LOOP('',(#59405,#59406,#59407,#59408));
#14251=EDGE_LOOP('',(#59409,#59410,#59411,#59412));
#14252=EDGE_LOOP('',(#59413,#59414,#59415,#59416));
#14253=EDGE_LOOP('',(#59417,#59418,#59419,#59420));
#14254=EDGE_LOOP('',(#59421,#59422,#59423,#59424));
#14255=EDGE_LOOP('',(#59425,#59426,#59427,#59428));
#14256=EDGE_LOOP('',(#59429,#59430,#59431,#59432));
#14257=EDGE_LOOP('',(#59433,#59434,#59435,#59436));
#14258=EDGE_LOOP('',(#59437,#59438,#59439,#59440));
#14259=EDGE_LOOP('',(#59441,#59442,#59443,#59444));
#14260=EDGE_LOOP('',(#59445,#59446,#59447,#59448));
#14261=EDGE_LOOP('',(#59449,#59450,#59451,#59452));
#14262=EDGE_LOOP('',(#59453,#59454,#59455,#59456));
#14263=EDGE_LOOP('',(#59457,#59458,#59459,#59460));
#14264=EDGE_LOOP('',(#59461,#59462,#59463,#59464));
#14265=EDGE_LOOP('',(#59465,#59466,#59467,#59468));
#14266=EDGE_LOOP('',(#59469,#59470,#59471,#59472));
#14267=EDGE_LOOP('',(#59473,#59474,#59475,#59476));
#14268=EDGE_LOOP('',(#59477,#59478,#59479,#59480));
#14269=EDGE_LOOP('',(#59481,#59482,#59483,#59484));
#14270=EDGE_LOOP('',(#59485,#59486,#59487,#59488));
#14271=EDGE_LOOP('',(#59489,#59490,#59491,#59492));
#14272=EDGE_LOOP('',(#59493,#59494,#59495,#59496));
#14273=EDGE_LOOP('',(#59497,#59498,#59499,#59500));
#14274=EDGE_LOOP('',(#59501,#59502,#59503,#59504));
#14275=EDGE_LOOP('',(#59505,#59506,#59507,#59508));
#14276=EDGE_LOOP('',(#59509,#59510,#59511,#59512));
#14277=EDGE_LOOP('',(#59513,#59514,#59515,#59516));
#14278=EDGE_LOOP('',(#59517,#59518,#59519,#59520));
#14279=EDGE_LOOP('',(#59521,#59522,#59523,#59524));
#14280=EDGE_LOOP('',(#59525,#59526,#59527,#59528));
#14281=EDGE_LOOP('',(#59529,#59530,#59531,#59532));
#14282=EDGE_LOOP('',(#59533,#59534,#59535,#59536));
#14283=EDGE_LOOP('',(#59537,#59538,#59539,#59540));
#14284=EDGE_LOOP('',(#59541,#59542,#59543,#59544));
#14285=EDGE_LOOP('',(#59545,#59546,#59547,#59548));
#14286=EDGE_LOOP('',(#59549,#59550,#59551,#59552));
#14287=EDGE_LOOP('',(#59553,#59554,#59555,#59556));
#14288=EDGE_LOOP('',(#59557,#59558,#59559,#59560));
#14289=EDGE_LOOP('',(#59561,#59562,#59563,#59564));
#14290=EDGE_LOOP('',(#59565,#59566,#59567,#59568));
#14291=EDGE_LOOP('',(#59569,#59570,#59571,#59572));
#14292=EDGE_LOOP('',(#59573,#59574,#59575,#59576));
#14293=EDGE_LOOP('',(#59577,#59578,#59579,#59580));
#14294=EDGE_LOOP('',(#59581,#59582,#59583,#59584));
#14295=EDGE_LOOP('',(#59585,#59586,#59587,#59588));
#14296=EDGE_LOOP('',(#59589,#59590,#59591,#59592));
#14297=EDGE_LOOP('',(#59593,#59594,#59595,#59596));
#14298=EDGE_LOOP('',(#59597,#59598,#59599,#59600));
#14299=EDGE_LOOP('',(#59601,#59602,#59603,#59604));
#14300=EDGE_LOOP('',(#59605,#59606,#59607,#59608));
#14301=EDGE_LOOP('',(#59609,#59610,#59611,#59612));
#14302=EDGE_LOOP('',(#59613,#59614,#59615,#59616));
#14303=EDGE_LOOP('',(#59617,#59618,#59619,#59620));
#14304=EDGE_LOOP('',(#59621,#59622,#59623,#59624));
#14305=EDGE_LOOP('',(#59625,#59626,#59627,#59628));
#14306=EDGE_LOOP('',(#59629,#59630,#59631,#59632));
#14307=EDGE_LOOP('',(#59633,#59634,#59635,#59636));
#14308=EDGE_LOOP('',(#59637,#59638,#59639,#59640));
#14309=EDGE_LOOP('',(#59641,#59642,#59643,#59644));
#14310=EDGE_LOOP('',(#59645,#59646,#59647,#59648));
#14311=EDGE_LOOP('',(#59649,#59650,#59651,#59652));
#14312=EDGE_LOOP('',(#59653,#59654,#59655,#59656));
#14313=EDGE_LOOP('',(#59657,#59658,#59659,#59660));
#14314=EDGE_LOOP('',(#59661,#59662,#59663,#59664));
#14315=EDGE_LOOP('',(#59665,#59666,#59667,#59668));
#14316=EDGE_LOOP('',(#59669,#59670,#59671,#59672));
#14317=EDGE_LOOP('',(#59673,#59674,#59675,#59676));
#14318=EDGE_LOOP('',(#59677,#59678,#59679,#59680));
#14319=EDGE_LOOP('',(#59681,#59682,#59683,#59684));
#14320=EDGE_LOOP('',(#59685,#59686,#59687,#59688));
#14321=EDGE_LOOP('',(#59689,#59690,#59691,#59692));
#14322=EDGE_LOOP('',(#59693,#59694,#59695,#59696));
#14323=EDGE_LOOP('',(#59697,#59698,#59699,#59700));
#14324=EDGE_LOOP('',(#59701,#59702,#59703,#59704));
#14325=EDGE_LOOP('',(#59705,#59706,#59707,#59708));
#14326=EDGE_LOOP('',(#59709,#59710,#59711,#59712));
#14327=EDGE_LOOP('',(#59713,#59714,#59715,#59716));
#14328=EDGE_LOOP('',(#59717,#59718,#59719,#59720));
#14329=EDGE_LOOP('',(#59721,#59722,#59723,#59724));
#14330=EDGE_LOOP('',(#59725,#59726,#59727,#59728));
#14331=EDGE_LOOP('',(#59729,#59730,#59731,#59732));
#14332=EDGE_LOOP('',(#59733,#59734,#59735,#59736));
#14333=EDGE_LOOP('',(#59737,#59738,#59739,#59740));
#14334=EDGE_LOOP('',(#59741,#59742,#59743,#59744));
#14335=EDGE_LOOP('',(#59745,#59746,#59747,#59748));
#14336=EDGE_LOOP('',(#59749,#59750,#59751,#59752));
#14337=EDGE_LOOP('',(#59753,#59754,#59755,#59756));
#14338=EDGE_LOOP('',(#59757,#59758,#59759,#59760));
#14339=EDGE_LOOP('',(#59761,#59762,#59763,#59764));
#14340=EDGE_LOOP('',(#59765,#59766,#59767,#59768));
#14341=EDGE_LOOP('',(#59769,#59770,#59771,#59772));
#14342=EDGE_LOOP('',(#59773,#59774,#59775,#59776));
#14343=EDGE_LOOP('',(#59777,#59778,#59779,#59780));
#14344=EDGE_LOOP('',(#59781,#59782,#59783,#59784));
#14345=EDGE_LOOP('',(#59785,#59786,#59787,#59788));
#14346=EDGE_LOOP('',(#59789,#59790,#59791,#59792));
#14347=EDGE_LOOP('',(#59793,#59794,#59795,#59796));
#14348=EDGE_LOOP('',(#59797,#59798,#59799,#59800));
#14349=EDGE_LOOP('',(#59801,#59802,#59803,#59804));
#14350=EDGE_LOOP('',(#59805,#59806,#59807,#59808));
#14351=EDGE_LOOP('',(#59809,#59810,#59811,#59812));
#14352=EDGE_LOOP('',(#59813,#59814,#59815,#59816));
#14353=EDGE_LOOP('',(#59817,#59818,#59819,#59820));
#14354=EDGE_LOOP('',(#59821,#59822,#59823,#59824));
#14355=EDGE_LOOP('',(#59825,#59826,#59827,#59828));
#14356=EDGE_LOOP('',(#59829,#59830,#59831,#59832));
#14357=EDGE_LOOP('',(#59833,#59834,#59835,#59836));
#14358=EDGE_LOOP('',(#59837,#59838,#59839,#59840));
#14359=EDGE_LOOP('',(#59841,#59842,#59843,#59844));
#14360=EDGE_LOOP('',(#59845,#59846,#59847,#59848));
#14361=EDGE_LOOP('',(#59849,#59850,#59851,#59852));
#14362=EDGE_LOOP('',(#59853,#59854,#59855,#59856));
#14363=EDGE_LOOP('',(#59857,#59858,#59859,#59860));
#14364=EDGE_LOOP('',(#59861,#59862,#59863,#59864));
#14365=EDGE_LOOP('',(#59865,#59866,#59867,#59868));
#14366=EDGE_LOOP('',(#59869,#59870,#59871,#59872));
#14367=EDGE_LOOP('',(#59873,#59874,#59875,#59876));
#14368=EDGE_LOOP('',(#59877,#59878,#59879,#59880));
#14369=EDGE_LOOP('',(#59881,#59882,#59883,#59884));
#14370=EDGE_LOOP('',(#59885,#59886,#59887,#59888));
#14371=EDGE_LOOP('',(#59889,#59890,#59891,#59892));
#14372=EDGE_LOOP('',(#59893,#59894,#59895,#59896));
#14373=EDGE_LOOP('',(#59897,#59898,#59899,#59900));
#14374=EDGE_LOOP('',(#59901,#59902,#59903,#59904));
#14375=EDGE_LOOP('',(#59905,#59906,#59907,#59908));
#14376=EDGE_LOOP('',(#59909,#59910,#59911,#59912));
#14377=EDGE_LOOP('',(#59913,#59914,#59915,#59916));
#14378=EDGE_LOOP('',(#59917,#59918,#59919,#59920));
#14379=EDGE_LOOP('',(#59921,#59922,#59923,#59924));
#14380=EDGE_LOOP('',(#59925,#59926,#59927,#59928));
#14381=EDGE_LOOP('',(#59929,#59930,#59931,#59932));
#14382=EDGE_LOOP('',(#59933,#59934,#59935,#59936));
#14383=EDGE_LOOP('',(#59937,#59938,#59939,#59940));
#14384=EDGE_LOOP('',(#59941,#59942,#59943,#59944));
#14385=EDGE_LOOP('',(#59945,#59946,#59947,#59948));
#14386=EDGE_LOOP('',(#59949,#59950,#59951,#59952));
#14387=EDGE_LOOP('',(#59953,#59954,#59955,#59956));
#14388=EDGE_LOOP('',(#59957,#59958,#59959,#59960));
#14389=EDGE_LOOP('',(#59961,#59962,#59963,#59964));
#14390=EDGE_LOOP('',(#59965,#59966,#59967,#59968));
#14391=EDGE_LOOP('',(#59969,#59970,#59971,#59972));
#14392=EDGE_LOOP('',(#59973,#59974,#59975,#59976));
#14393=EDGE_LOOP('',(#59977,#59978,#59979,#59980));
#14394=EDGE_LOOP('',(#59981,#59982,#59983,#59984));
#14395=EDGE_LOOP('',(#59985,#59986,#59987,#59988));
#14396=EDGE_LOOP('',(#59989,#59990,#59991,#59992));
#14397=EDGE_LOOP('',(#59993,#59994,#59995,#59996));
#14398=EDGE_LOOP('',(#59997,#59998,#59999,#60000));
#14399=EDGE_LOOP('',(#60001,#60002,#60003,#60004));
#14400=EDGE_LOOP('',(#60005,#60006,#60007,#60008));
#14401=EDGE_LOOP('',(#60009,#60010,#60011,#60012));
#14402=EDGE_LOOP('',(#60013,#60014,#60015,#60016));
#14403=EDGE_LOOP('',(#60017,#60018,#60019,#60020));
#14404=EDGE_LOOP('',(#60021,#60022,#60023,#60024));
#14405=EDGE_LOOP('',(#60025,#60026,#60027,#60028));
#14406=EDGE_LOOP('',(#60029,#60030,#60031,#60032));
#14407=EDGE_LOOP('',(#60033,#60034,#60035,#60036));
#14408=EDGE_LOOP('',(#60037,#60038,#60039,#60040));
#14409=EDGE_LOOP('',(#60041,#60042,#60043,#60044));
#14410=EDGE_LOOP('',(#60045,#60046,#60047,#60048));
#14411=EDGE_LOOP('',(#60049,#60050,#60051,#60052));
#14412=EDGE_LOOP('',(#60053,#60054,#60055,#60056));
#14413=EDGE_LOOP('',(#60057,#60058,#60059,#60060));
#14414=EDGE_LOOP('',(#60061,#60062,#60063,#60064));
#14415=EDGE_LOOP('',(#60065,#60066,#60067,#60068));
#14416=EDGE_LOOP('',(#60069,#60070,#60071,#60072));
#14417=EDGE_LOOP('',(#60073,#60074,#60075,#60076));
#14418=EDGE_LOOP('',(#60077,#60078,#60079,#60080));
#14419=EDGE_LOOP('',(#60081,#60082,#60083,#60084));
#14420=EDGE_LOOP('',(#60085,#60086,#60087,#60088));
#14421=EDGE_LOOP('',(#60089,#60090,#60091,#60092));
#14422=EDGE_LOOP('',(#60093,#60094,#60095,#60096));
#14423=EDGE_LOOP('',(#60097,#60098,#60099,#60100));
#14424=EDGE_LOOP('',(#60101,#60102,#60103,#60104));
#14425=EDGE_LOOP('',(#60105,#60106,#60107,#60108));
#14426=EDGE_LOOP('',(#60109,#60110,#60111,#60112));
#14427=EDGE_LOOP('',(#60113,#60114,#60115,#60116));
#14428=EDGE_LOOP('',(#60117,#60118,#60119,#60120));
#14429=EDGE_LOOP('',(#60121,#60122,#60123,#60124));
#14430=EDGE_LOOP('',(#60125,#60126,#60127,#60128));
#14431=EDGE_LOOP('',(#60129,#60130,#60131,#60132));
#14432=EDGE_LOOP('',(#60133,#60134,#60135,#60136));
#14433=EDGE_LOOP('',(#60137,#60138,#60139,#60140));
#14434=EDGE_LOOP('',(#60141,#60142,#60143,#60144));
#14435=EDGE_LOOP('',(#60145,#60146,#60147,#60148));
#14436=EDGE_LOOP('',(#60149,#60150,#60151,#60152));
#14437=EDGE_LOOP('',(#60153,#60154,#60155,#60156));
#14438=EDGE_LOOP('',(#60157,#60158,#60159,#60160));
#14439=EDGE_LOOP('',(#60161,#60162,#60163,#60164));
#14440=EDGE_LOOP('',(#60165,#60166,#60167,#60168));
#14441=EDGE_LOOP('',(#60169,#60170,#60171,#60172));
#14442=EDGE_LOOP('',(#60173,#60174,#60175,#60176));
#14443=EDGE_LOOP('',(#60177,#60178,#60179,#60180));
#14444=EDGE_LOOP('',(#60181,#60182,#60183,#60184));
#14445=EDGE_LOOP('',(#60185,#60186,#60187,#60188));
#14446=EDGE_LOOP('',(#60189,#60190,#60191,#60192));
#14447=EDGE_LOOP('',(#60193,#60194,#60195,#60196));
#14448=EDGE_LOOP('',(#60197,#60198,#60199,#60200));
#14449=EDGE_LOOP('',(#60201,#60202,#60203,#60204));
#14450=EDGE_LOOP('',(#60205,#60206,#60207,#60208));
#14451=EDGE_LOOP('',(#60209,#60210,#60211,#60212));
#14452=EDGE_LOOP('',(#60213,#60214,#60215,#60216));
#14453=EDGE_LOOP('',(#60217,#60218,#60219,#60220));
#14454=EDGE_LOOP('',(#60221,#60222,#60223,#60224));
#14455=EDGE_LOOP('',(#60225,#60226,#60227,#60228));
#14456=EDGE_LOOP('',(#60229,#60230,#60231,#60232));
#14457=EDGE_LOOP('',(#60233,#60234,#60235,#60236));
#14458=EDGE_LOOP('',(#60237,#60238,#60239,#60240));
#14459=EDGE_LOOP('',(#60241,#60242,#60243,#60244));
#14460=EDGE_LOOP('',(#60245,#60246,#60247,#60248));
#14461=EDGE_LOOP('',(#60249,#60250,#60251,#60252));
#14462=EDGE_LOOP('',(#60253,#60254,#60255,#60256));
#14463=EDGE_LOOP('',(#60257,#60258,#60259,#60260));
#14464=EDGE_LOOP('',(#60261,#60262,#60263,#60264));
#14465=EDGE_LOOP('',(#60265,#60266,#60267,#60268));
#14466=EDGE_LOOP('',(#60269,#60270,#60271,#60272));
#14467=EDGE_LOOP('',(#60273,#60274,#60275,#60276));
#14468=EDGE_LOOP('',(#60277,#60278,#60279,#60280));
#14469=EDGE_LOOP('',(#60281,#60282,#60283,#60284));
#14470=EDGE_LOOP('',(#60285,#60286,#60287,#60288));
#14471=EDGE_LOOP('',(#60289,#60290,#60291,#60292));
#14472=EDGE_LOOP('',(#60293,#60294,#60295,#60296));
#14473=EDGE_LOOP('',(#60297,#60298,#60299,#60300));
#14474=EDGE_LOOP('',(#60301,#60302,#60303,#60304));
#14475=EDGE_LOOP('',(#60305,#60306,#60307,#60308));
#14476=EDGE_LOOP('',(#60309,#60310,#60311,#60312));
#14477=EDGE_LOOP('',(#60313,#60314,#60315,#60316));
#14478=EDGE_LOOP('',(#60317,#60318,#60319,#60320));
#14479=EDGE_LOOP('',(#60321,#60322,#60323,#60324));
#14480=EDGE_LOOP('',(#60325,#60326,#60327,#60328));
#14481=EDGE_LOOP('',(#60329,#60330,#60331,#60332));
#14482=EDGE_LOOP('',(#60333,#60334,#60335,#60336));
#14483=EDGE_LOOP('',(#60337,#60338,#60339,#60340));
#14484=EDGE_LOOP('',(#60341,#60342,#60343,#60344));
#14485=EDGE_LOOP('',(#60345,#60346,#60347,#60348));
#14486=EDGE_LOOP('',(#60349,#60350,#60351,#60352));
#14487=EDGE_LOOP('',(#60353,#60354,#60355,#60356));
#14488=EDGE_LOOP('',(#60357,#60358,#60359,#60360));
#14489=EDGE_LOOP('',(#60361,#60362,#60363,#60364));
#14490=EDGE_LOOP('',(#60365,#60366,#60367,#60368));
#14491=EDGE_LOOP('',(#60369,#60370,#60371,#60372));
#14492=EDGE_LOOP('',(#60373,#60374,#60375,#60376));
#14493=EDGE_LOOP('',(#60377,#60378,#60379,#60380));
#14494=EDGE_LOOP('',(#60381,#60382,#60383,#60384));
#14495=EDGE_LOOP('',(#60385,#60386,#60387,#60388));
#14496=EDGE_LOOP('',(#60389,#60390,#60391,#60392));
#14497=EDGE_LOOP('',(#60393,#60394,#60395,#60396));
#14498=EDGE_LOOP('',(#60397,#60398,#60399,#60400));
#14499=EDGE_LOOP('',(#60401,#60402,#60403,#60404));
#14500=EDGE_LOOP('',(#60405,#60406,#60407,#60408));
#14501=EDGE_LOOP('',(#60409,#60410,#60411,#60412));
#14502=EDGE_LOOP('',(#60413,#60414,#60415,#60416));
#14503=EDGE_LOOP('',(#60417,#60418,#60419,#60420));
#14504=EDGE_LOOP('',(#60421,#60422,#60423,#60424));
#14505=EDGE_LOOP('',(#60425,#60426,#60427,#60428));
#14506=EDGE_LOOP('',(#60429,#60430,#60431,#60432));
#14507=EDGE_LOOP('',(#60433,#60434,#60435,#60436));
#14508=EDGE_LOOP('',(#60437,#60438,#60439,#60440));
#14509=EDGE_LOOP('',(#60441,#60442,#60443,#60444));
#14510=EDGE_LOOP('',(#60445,#60446,#60447,#60448));
#14511=EDGE_LOOP('',(#60449,#60450,#60451,#60452));
#14512=EDGE_LOOP('',(#60453,#60454,#60455,#60456));
#14513=EDGE_LOOP('',(#60457,#60458,#60459,#60460));
#14514=EDGE_LOOP('',(#60461,#60462,#60463,#60464));
#14515=EDGE_LOOP('',(#60465,#60466,#60467,#60468));
#14516=EDGE_LOOP('',(#60469,#60470,#60471,#60472));
#14517=EDGE_LOOP('',(#60473,#60474,#60475,#60476));
#14518=EDGE_LOOP('',(#60477,#60478,#60479,#60480));
#14519=EDGE_LOOP('',(#60481,#60482,#60483,#60484));
#14520=EDGE_LOOP('',(#60485,#60486,#60487,#60488));
#14521=EDGE_LOOP('',(#60489,#60490,#60491,#60492));
#14522=EDGE_LOOP('',(#60493,#60494,#60495));
#14523=EDGE_LOOP('',(#60496,#60497,#60498,#60499));
#14524=EDGE_LOOP('',(#60500,#60501,#60502,#60503,#60504));
#14525=EDGE_LOOP('',(#60505,#60506,#60507,#60508));
#14526=EDGE_LOOP('',(#60509,#60510,#60511));
#14527=EDGE_LOOP('',(#60512,#60513,#60514,#60515));
#14528=EDGE_LOOP('',(#60516,#60517,#60518,#60519,#60520));
#14529=EDGE_LOOP('',(#60521,#60522,#60523,#60524));
#14530=EDGE_LOOP('',(#60525,#60526,#60527));
#14531=EDGE_LOOP('',(#60528,#60529,#60530,#60531));
#14532=EDGE_LOOP('',(#60532,#60533,#60534,#60535,#60536));
#14533=EDGE_LOOP('',(#60537,#60538,#60539,#60540));
#14534=EDGE_LOOP('',(#60541,#60542,#60543));
#14535=EDGE_LOOP('',(#60544,#60545,#60546,#60547));
#14536=EDGE_LOOP('',(#60548,#60549,#60550,#60551,#60552));
#14537=EDGE_LOOP('',(#60553,#60554,#60555,#60556));
#14538=EDGE_LOOP('',(#60557,#60558,#60559));
#14539=EDGE_LOOP('',(#60560,#60561,#60562,#60563));
#14540=EDGE_LOOP('',(#60564,#60565,#60566,#60567,#60568));
#14541=EDGE_LOOP('',(#60569,#60570,#60571,#60572));
#14542=EDGE_LOOP('',(#60573,#60574,#60575));
#14543=EDGE_LOOP('',(#60576,#60577,#60578,#60579));
#14544=EDGE_LOOP('',(#60580,#60581,#60582,#60583,#60584));
#14545=EDGE_LOOP('',(#60585,#60586,#60587,#60588));
#14546=EDGE_LOOP('',(#60589,#60590,#60591));
#14547=EDGE_LOOP('',(#60592,#60593,#60594,#60595));
#14548=EDGE_LOOP('',(#60596,#60597,#60598,#60599,#60600));
#14549=EDGE_LOOP('',(#60601,#60602,#60603,#60604));
#14550=EDGE_LOOP('',(#60605,#60606,#60607));
#14551=EDGE_LOOP('',(#60608,#60609,#60610,#60611));
#14552=EDGE_LOOP('',(#60612,#60613,#60614,#60615,#60616));
#14553=EDGE_LOOP('',(#60617,#60618,#60619,#60620));
#14554=EDGE_LOOP('',(#60621,#60622,#60623));
#14555=EDGE_LOOP('',(#60624,#60625,#60626,#60627));
#14556=EDGE_LOOP('',(#60628,#60629,#60630,#60631,#60632));
#14557=EDGE_LOOP('',(#60633,#60634,#60635,#60636));
#14558=EDGE_LOOP('',(#60637,#60638,#60639));
#14559=EDGE_LOOP('',(#60640,#60641,#60642,#60643));
#14560=EDGE_LOOP('',(#60644,#60645,#60646,#60647,#60648));
#14561=EDGE_LOOP('',(#60649,#60650,#60651,#60652));
#14562=EDGE_LOOP('',(#60653,#60654,#60655));
#14563=EDGE_LOOP('',(#60656,#60657,#60658,#60659));
#14564=EDGE_LOOP('',(#60660,#60661,#60662,#60663,#60664));
#14565=EDGE_LOOP('',(#60665,#60666,#60667,#60668));
#14566=EDGE_LOOP('',(#60669,#60670,#60671));
#14567=EDGE_LOOP('',(#60672,#60673,#60674,#60675));
#14568=EDGE_LOOP('',(#60676,#60677,#60678,#60679,#60680));
#14569=EDGE_LOOP('',(#60681,#60682,#60683,#60684));
#14570=EDGE_LOOP('',(#60685,#60686,#60687));
#14571=EDGE_LOOP('',(#60688,#60689,#60690,#60691));
#14572=EDGE_LOOP('',(#60692,#60693,#60694,#60695,#60696));
#14573=EDGE_LOOP('',(#60697,#60698,#60699,#60700));
#14574=EDGE_LOOP('',(#60701,#60702,#60703));
#14575=EDGE_LOOP('',(#60704,#60705,#60706,#60707));
#14576=EDGE_LOOP('',(#60708,#60709,#60710,#60711,#60712));
#14577=EDGE_LOOP('',(#60713,#60714,#60715,#60716));
#14578=EDGE_LOOP('',(#60717,#60718,#60719));
#14579=EDGE_LOOP('',(#60720,#60721,#60722,#60723));
#14580=EDGE_LOOP('',(#60724,#60725,#60726,#60727,#60728));
#14581=EDGE_LOOP('',(#60729,#60730,#60731,#60732));
#14582=EDGE_LOOP('',(#60733,#60734,#60735));
#14583=EDGE_LOOP('',(#60736,#60737,#60738,#60739));
#14584=EDGE_LOOP('',(#60740,#60741,#60742,#60743,#60744));
#14585=EDGE_LOOP('',(#60745,#60746,#60747,#60748));
#14586=EDGE_LOOP('',(#60749,#60750,#60751));
#14587=EDGE_LOOP('',(#60752,#60753,#60754,#60755));
#14588=EDGE_LOOP('',(#60756,#60757,#60758,#60759,#60760));
#14589=EDGE_LOOP('',(#60761,#60762,#60763,#60764));
#14590=EDGE_LOOP('',(#60765,#60766,#60767));
#14591=EDGE_LOOP('',(#60768,#60769,#60770,#60771));
#14592=EDGE_LOOP('',(#60772,#60773,#60774,#60775,#60776));
#14593=EDGE_LOOP('',(#60777,#60778,#60779,#60780));
#14594=EDGE_LOOP('',(#60781,#60782,#60783));
#14595=EDGE_LOOP('',(#60784,#60785,#60786,#60787));
#14596=EDGE_LOOP('',(#60788,#60789,#60790,#60791,#60792));
#14597=EDGE_LOOP('',(#60793,#60794,#60795,#60796));
#14598=EDGE_LOOP('',(#60797,#60798,#60799));
#14599=EDGE_LOOP('',(#60800,#60801,#60802,#60803));
#14600=EDGE_LOOP('',(#60804,#60805,#60806,#60807,#60808));
#14601=EDGE_LOOP('',(#60809,#60810,#60811,#60812));
#14602=EDGE_LOOP('',(#60813,#60814,#60815));
#14603=EDGE_LOOP('',(#60816,#60817,#60818,#60819));
#14604=EDGE_LOOP('',(#60820,#60821,#60822,#60823,#60824));
#14605=EDGE_LOOP('',(#60825,#60826,#60827,#60828));
#14606=EDGE_LOOP('',(#60829,#60830,#60831,#60832));
#14607=EDGE_LOOP('',(#60833,#60834,#60835,#60836));
#14608=EDGE_LOOP('',(#60837,#60838,#60839));
#14609=EDGE_LOOP('',(#60840,#60841,#60842,#60843));
#14610=EDGE_LOOP('',(#60844,#60845,#60846,#60847,#60848));
#14611=EDGE_LOOP('',(#60849,#60850,#60851,#60852));
#14612=EDGE_LOOP('',(#60853,#60854,#60855));
#14613=EDGE_LOOP('',(#60856,#60857,#60858,#60859));
#14614=EDGE_LOOP('',(#60860,#60861,#60862,#60863,#60864));
#14615=EDGE_LOOP('',(#60865,#60866,#60867,#60868));
#14616=EDGE_LOOP('',(#60869,#60870,#60871));
#14617=EDGE_LOOP('',(#60872,#60873,#60874,#60875));
#14618=EDGE_LOOP('',(#60876,#60877,#60878,#60879,#60880));
#14619=EDGE_LOOP('',(#60881,#60882,#60883,#60884));
#14620=EDGE_LOOP('',(#60885,#60886,#60887));
#14621=EDGE_LOOP('',(#60888,#60889,#60890,#60891));
#14622=EDGE_LOOP('',(#60892,#60893,#60894,#60895,#60896));
#14623=EDGE_LOOP('',(#60897,#60898,#60899,#60900));
#14624=EDGE_LOOP('',(#60901,#60902,#60903));
#14625=EDGE_LOOP('',(#60904,#60905,#60906,#60907));
#14626=EDGE_LOOP('',(#60908,#60909,#60910,#60911,#60912));
#14627=EDGE_LOOP('',(#60913,#60914,#60915,#60916));
#14628=EDGE_LOOP('',(#60917,#60918,#60919));
#14629=EDGE_LOOP('',(#60920,#60921,#60922,#60923));
#14630=EDGE_LOOP('',(#60924,#60925,#60926,#60927,#60928));
#14631=EDGE_LOOP('',(#60929,#60930,#60931,#60932));
#14632=EDGE_LOOP('',(#60933,#60934,#60935));
#14633=EDGE_LOOP('',(#60936,#60937,#60938,#60939));
#14634=EDGE_LOOP('',(#60940,#60941,#60942,#60943,#60944));
#14635=EDGE_LOOP('',(#60945,#60946,#60947,#60948));
#14636=EDGE_LOOP('',(#60949,#60950,#60951,#60952));
#14637=EDGE_LOOP('',(#60953,#60954,#60955,#60956));
#14638=EDGE_LOOP('',(#60957,#60958,#60959,#60960));
#14639=EDGE_LOOP('',(#60961,#60962,#60963,#60964));
#14640=EDGE_LOOP('',(#60965,#60966,#60967,#60968));
#14641=EDGE_LOOP('',(#60969,#60970,#60971,#60972));
#14642=EDGE_LOOP('',(#60973,#60974,#60975,#60976));
#14643=EDGE_LOOP('',(#60977,#60978,#60979,#60980));
#14644=EDGE_LOOP('',(#60981,#60982,#60983,#60984));
#14645=EDGE_LOOP('',(#60985,#60986,#60987,#60988));
#14646=EDGE_LOOP('',(#60989,#60990,#60991,#60992));
#14647=EDGE_LOOP('',(#60993,#60994,#60995,#60996));
#14648=EDGE_LOOP('',(#60997,#60998,#60999,#61000));
#14649=EDGE_LOOP('',(#61001,#61002,#61003,#61004));
#14650=EDGE_LOOP('',(#61005,#61006,#61007,#61008));
#14651=EDGE_LOOP('',(#61009,#61010,#61011,#61012));
#14652=EDGE_LOOP('',(#61013,#61014,#61015,#61016));
#14653=EDGE_LOOP('',(#61017,#61018,#61019,#61020));
#14654=EDGE_LOOP('',(#61021,#61022,#61023,#61024));
#14655=EDGE_LOOP('',(#61025,#61026,#61027,#61028));
#14656=EDGE_LOOP('',(#61029,#61030,#61031,#61032));
#14657=EDGE_LOOP('',(#61033,#61034,#61035,#61036));
#14658=EDGE_LOOP('',(#61037,#61038,#61039,#61040));
#14659=EDGE_LOOP('',(#61041,#61042,#61043,#61044));
#14660=EDGE_LOOP('',(#61045,#61046,#61047,#61048));
#14661=EDGE_LOOP('',(#61049,#61050,#61051,#61052));
#14662=EDGE_LOOP('',(#61053,#61054,#61055,#61056));
#14663=EDGE_LOOP('',(#61057,#61058,#61059,#61060));
#14664=EDGE_LOOP('',(#61061,#61062,#61063,#61064));
#14665=EDGE_LOOP('',(#61065,#61066,#61067,#61068));
#14666=EDGE_LOOP('',(#61069,#61070,#61071,#61072));
#14667=EDGE_LOOP('',(#61073,#61074,#61075,#61076));
#14668=EDGE_LOOP('',(#61077,#61078,#61079,#61080));
#14669=EDGE_LOOP('',(#61081,#61082,#61083,#61084));
#14670=EDGE_LOOP('',(#61085,#61086,#61087,#61088));
#14671=EDGE_LOOP('',(#61089,#61090,#61091,#61092));
#14672=EDGE_LOOP('',(#61093,#61094,#61095,#61096));
#14673=EDGE_LOOP('',(#61097,#61098,#61099,#61100));
#14674=EDGE_LOOP('',(#61101,#61102,#61103,#61104));
#14675=EDGE_LOOP('',(#61105,#61106,#61107,#61108));
#14676=EDGE_LOOP('',(#61109,#61110,#61111,#61112));
#14677=EDGE_LOOP('',(#61113,#61114,#61115,#61116));
#14678=EDGE_LOOP('',(#61117,#61118,#61119,#61120));
#14679=EDGE_LOOP('',(#61121,#61122,#61123,#61124));
#14680=EDGE_LOOP('',(#61125,#61126,#61127,#61128));
#14681=EDGE_LOOP('',(#61129,#61130,#61131,#61132));
#14682=EDGE_LOOP('',(#61133,#61134,#61135,#61136));
#14683=EDGE_LOOP('',(#61137,#61138,#61139,#61140));
#14684=EDGE_LOOP('',(#61141,#61142,#61143,#61144));
#14685=EDGE_LOOP('',(#61145,#61146,#61147,#61148));
#14686=EDGE_LOOP('',(#61149,#61150,#61151,#61152));
#14687=EDGE_LOOP('',(#61153,#61154,#61155,#61156));
#14688=EDGE_LOOP('',(#61157,#61158,#61159,#61160));
#14689=EDGE_LOOP('',(#61161,#61162,#61163,#61164));
#14690=EDGE_LOOP('',(#61165,#61166,#61167,#61168));
#14691=EDGE_LOOP('',(#61169,#61170,#61171,#61172));
#14692=EDGE_LOOP('',(#61173,#61174,#61175,#61176));
#14693=EDGE_LOOP('',(#61177,#61178,#61179,#61180,#61181));
#14694=EDGE_LOOP('',(#61182,#61183,#61184,#61185,#61186));
#14695=EDGE_LOOP('',(#61187,#61188,#61189,#61190,#61191));
#14696=EDGE_LOOP('',(#61192,#61193,#61194,#61195,#61196));
#14697=EDGE_LOOP('',(#61197,#61198,#61199,#61200,#61201));
#14698=EDGE_LOOP('',(#61202,#61203,#61204,#61205,#61206));
#14699=EDGE_LOOP('',(#61207,#61208,#61209,#61210,#61211));
#14700=EDGE_LOOP('',(#61212,#61213,#61214,#61215,#61216));
#14701=EDGE_LOOP('',(#61217,#61218,#61219,#61220,#61221));
#14702=EDGE_LOOP('',(#61222,#61223,#61224,#61225,#61226));
#14703=EDGE_LOOP('',(#61227,#61228,#61229,#61230,#61231));
#14704=EDGE_LOOP('',(#61232,#61233,#61234,#61235,#61236));
#14705=EDGE_LOOP('',(#61237,#61238,#61239,#61240,#61241));
#14706=EDGE_LOOP('',(#61242,#61243,#61244,#61245,#61246));
#14707=EDGE_LOOP('',(#61247,#61248,#61249,#61250,#61251));
#14708=EDGE_LOOP('',(#61252,#61253,#61254,#61255,#61256));
#14709=EDGE_LOOP('',(#61257,#61258,#61259,#61260,#61261));
#14710=EDGE_LOOP('',(#61262,#61263,#61264,#61265,#61266));
#14711=EDGE_LOOP('',(#61267,#61268,#61269,#61270,#61271));
#14712=EDGE_LOOP('',(#61272,#61273,#61274,#61275,#61276));
#14713=EDGE_LOOP('',(#61277,#61278,#61279,#61280,#61281));
#14714=EDGE_LOOP('',(#61282,#61283,#61284,#61285,#61286));
#14715=EDGE_LOOP('',(#61287,#61288,#61289,#61290,#61291));
#14716=EDGE_LOOP('',(#61292,#61293,#61294,#61295,#61296));
#14717=EDGE_LOOP('',(#61297,#61298,#61299,#61300,#61301));
#14718=EDGE_LOOP('',(#61302,#61303,#61304,#61305,#61306));
#14719=EDGE_LOOP('',(#61307,#61308,#61309,#61310,#61311));
#14720=EDGE_LOOP('',(#61312,#61313,#61314,#61315,#61316));
#14721=EDGE_LOOP('',(#61317,#61318,#61319,#61320,#61321));
#14722=EDGE_LOOP('',(#61322,#61323,#61324,#61325,#61326));
#14723=EDGE_LOOP('',(#61327,#61328,#61329,#61330,#61331));
#14724=EDGE_LOOP('',(#61332,#61333,#61334,#61335,#61336));
#14725=EDGE_LOOP('',(#61337,#61338,#61339,#61340,#61341));
#14726=EDGE_LOOP('',(#61342,#61343,#61344,#61345,#61346));
#14727=EDGE_LOOP('',(#61347,#61348,#61349,#61350,#61351));
#14728=EDGE_LOOP('',(#61352,#61353,#61354,#61355,#61356));
#14729=EDGE_LOOP('',(#61357,#61358,#61359,#61360,#61361));
#14730=EDGE_LOOP('',(#61362,#61363,#61364,#61365,#61366));
#14731=EDGE_LOOP('',(#61367,#61368,#61369,#61370,#61371));
#14732=EDGE_LOOP('',(#61372,#61373,#61374,#61375,#61376));
#14733=EDGE_LOOP('',(#61377,#61378,#61379,#61380,#61381));
#14734=EDGE_LOOP('',(#61382,#61383,#61384,#61385,#61386));
#14735=EDGE_LOOP('',(#61387,#61388,#61389,#61390,#61391));
#14736=EDGE_LOOP('',(#61392,#61393,#61394,#61395,#61396));
#14737=EDGE_LOOP('',(#61397,#61398,#61399,#61400,#61401));
#14738=EDGE_LOOP('',(#61402,#61403,#61404,#61405,#61406));
#14739=EDGE_LOOP('',(#61407,#61408,#61409,#61410,#61411));
#14740=EDGE_LOOP('',(#61412,#61413,#61414,#61415,#61416));
#14741=EDGE_LOOP('',(#61417,#61418,#61419,#61420,#61421));
#14742=EDGE_LOOP('',(#61422,#61423,#61424,#61425,#61426));
#14743=EDGE_LOOP('',(#61427,#61428,#61429,#61430,#61431));
#14744=EDGE_LOOP('',(#61432,#61433,#61434,#61435,#61436));
#14745=EDGE_LOOP('',(#61437,#61438,#61439,#61440,#61441));
#14746=EDGE_LOOP('',(#61442,#61443,#61444,#61445,#61446));
#14747=EDGE_LOOP('',(#61447,#61448,#61449,#61450,#61451));
#14748=EDGE_LOOP('',(#61452,#61453,#61454,#61455,#61456));
#14749=EDGE_LOOP('',(#61457,#61458,#61459,#61460,#61461));
#14750=EDGE_LOOP('',(#61462,#61463,#61464,#61465,#61466));
#14751=EDGE_LOOP('',(#61467,#61468,#61469,#61470));
#14752=EDGE_LOOP('',(#61471,#61472,#61473,#61474));
#14753=EDGE_LOOP('',(#61475,#61476,#61477,#61478));
#14754=EDGE_LOOP('',(#61479,#61480,#61481,#61482));
#14755=EDGE_LOOP('',(#61483,#61484,#61485,#61486));
#14756=EDGE_LOOP('',(#61487,#61488,#61489,#61490));
#14757=EDGE_LOOP('',(#61491,#61492,#61493,#61494));
#14758=EDGE_LOOP('',(#61495,#61496,#61497,#61498));
#14759=EDGE_LOOP('',(#61499,#61500,#61501,#61502));
#14760=EDGE_LOOP('',(#61503,#61504,#61505,#61506));
#14761=EDGE_LOOP('',(#61507,#61508,#61509,#61510));
#14762=EDGE_LOOP('',(#61511,#61512,#61513,#61514));
#14763=EDGE_LOOP('',(#61515,#61516,#61517,#61518));
#14764=EDGE_LOOP('',(#61519,#61520,#61521,#61522));
#14765=EDGE_LOOP('',(#61523,#61524,#61525,#61526));
#14766=EDGE_LOOP('',(#61527,#61528,#61529,#61530));
#14767=EDGE_LOOP('',(#61531,#61532,#61533,#61534));
#14768=EDGE_LOOP('',(#61535,#61536,#61537,#61538));
#14769=EDGE_LOOP('',(#61539,#61540,#61541,#61542));
#14770=EDGE_LOOP('',(#61543,#61544,#61545,#61546));
#14771=EDGE_LOOP('',(#61547,#61548,#61549,#61550));
#14772=EDGE_LOOP('',(#61551,#61552,#61553,#61554));
#14773=EDGE_LOOP('',(#61555,#61556,#61557,#61558));
#14774=EDGE_LOOP('',(#61559,#61560,#61561,#61562));
#14775=EDGE_LOOP('',(#61563,#61564,#61565,#61566));
#14776=EDGE_LOOP('',(#61567,#61568,#61569,#61570));
#14777=EDGE_LOOP('',(#61571,#61572,#61573,#61574));
#14778=EDGE_LOOP('',(#61575,#61576,#61577,#61578));
#14779=EDGE_LOOP('',(#61579,#61580,#61581,#61582));
#14780=EDGE_LOOP('',(#61583,#61584,#61585,#61586));
#14781=EDGE_LOOP('',(#61587,#61588,#61589,#61590));
#14782=EDGE_LOOP('',(#61591,#61592,#61593,#61594));
#14783=EDGE_LOOP('',(#61595,#61596,#61597,#61598));
#14784=EDGE_LOOP('',(#61599,#61600,#61601,#61602));
#14785=EDGE_LOOP('',(#61603,#61604,#61605,#61606));
#14786=EDGE_LOOP('',(#61607,#61608,#61609,#61610));
#14787=EDGE_LOOP('',(#61611,#61612,#61613,#61614));
#14788=EDGE_LOOP('',(#61615,#61616,#61617,#61618));
#14789=EDGE_LOOP('',(#61619,#61620,#61621,#61622));
#14790=EDGE_LOOP('',(#61623,#61624,#61625,#61626));
#14791=EDGE_LOOP('',(#61627,#61628,#61629,#61630));
#14792=EDGE_LOOP('',(#61631,#61632,#61633,#61634));
#14793=EDGE_LOOP('',(#61635,#61636,#61637,#61638));
#14794=EDGE_LOOP('',(#61639,#61640,#61641,#61642));
#14795=EDGE_LOOP('',(#61643,#61644,#61645,#61646));
#14796=EDGE_LOOP('',(#61647,#61648,#61649,#61650));
#14797=EDGE_LOOP('',(#61651,#61652,#61653,#61654));
#14798=EDGE_LOOP('',(#61655,#61656,#61657,#61658));
#14799=EDGE_LOOP('',(#61659,#61660,#61661,#61662));
#14800=EDGE_LOOP('',(#61663,#61664,#61665,#61666));
#14801=EDGE_LOOP('',(#61667,#61668,#61669,#61670));
#14802=EDGE_LOOP('',(#61671,#61672,#61673,#61674));
#14803=EDGE_LOOP('',(#61675,#61676,#61677,#61678));
#14804=EDGE_LOOP('',(#61679,#61680,#61681,#61682));
#14805=EDGE_LOOP('',(#61683,#61684,#61685,#61686));
#14806=EDGE_LOOP('',(#61687,#61688,#61689,#61690));
#14807=EDGE_LOOP('',(#61691,#61692,#61693,#61694));
#14808=EDGE_LOOP('',(#61695,#61696,#61697,#61698));
#14809=EDGE_LOOP('',(#61699,#61700,#61701,#61702));
#14810=EDGE_LOOP('',(#61703,#61704,#61705,#61706));
#14811=EDGE_LOOP('',(#61707,#61708,#61709,#61710));
#14812=EDGE_LOOP('',(#61711,#61712,#61713,#61714));
#14813=EDGE_LOOP('',(#61715,#61716,#61717,#61718));
#14814=EDGE_LOOP('',(#61719,#61720,#61721,#61722));
#14815=EDGE_LOOP('',(#61723,#61724,#61725,#61726));
#14816=EDGE_LOOP('',(#61727,#61728,#61729,#61730));
#14817=EDGE_LOOP('',(#61731,#61732,#61733,#61734));
#14818=EDGE_LOOP('',(#61735,#61736,#61737,#61738));
#14819=EDGE_LOOP('',(#61739,#61740,#61741,#61742));
#14820=EDGE_LOOP('',(#61743,#61744,#61745,#61746));
#14821=EDGE_LOOP('',(#61747,#61748,#61749,#61750));
#14822=EDGE_LOOP('',(#61751,#61752,#61753,#61754));
#14823=EDGE_LOOP('',(#61755,#61756,#61757,#61758));
#14824=EDGE_LOOP('',(#61759,#61760,#61761,#61762));
#14825=EDGE_LOOP('',(#61763,#61764,#61765,#61766));
#14826=EDGE_LOOP('',(#61767,#61768,#61769,#61770));
#14827=EDGE_LOOP('',(#61771,#61772,#61773,#61774));
#14828=EDGE_LOOP('',(#61775,#61776,#61777,#61778));
#14829=EDGE_LOOP('',(#61779,#61780,#61781,#61782));
#14830=EDGE_LOOP('',(#61783,#61784,#61785,#61786));
#14831=EDGE_LOOP('',(#61787,#61788,#61789,#61790));
#14832=EDGE_LOOP('',(#61791,#61792,#61793,#61794));
#14833=EDGE_LOOP('',(#61795,#61796,#61797,#61798));
#14834=EDGE_LOOP('',(#61799,#61800,#61801,#61802));
#14835=EDGE_LOOP('',(#61803,#61804,#61805,#61806));
#14836=EDGE_LOOP('',(#61807,#61808,#61809,#61810));
#14837=EDGE_LOOP('',(#61811,#61812,#61813,#61814));
#14838=EDGE_LOOP('',(#61815,#61816,#61817,#61818));
#14839=EDGE_LOOP('',(#61819,#61820,#61821,#61822));
#14840=EDGE_LOOP('',(#61823,#61824,#61825,#61826));
#14841=EDGE_LOOP('',(#61827,#61828,#61829,#61830));
#14842=EDGE_LOOP('',(#61831,#61832,#61833,#61834));
#14843=EDGE_LOOP('',(#61835,#61836,#61837,#61838));
#14844=EDGE_LOOP('',(#61839,#61840,#61841,#61842));
#14845=EDGE_LOOP('',(#61843,#61844,#61845,#61846));
#14846=EDGE_LOOP('',(#61847,#61848,#61849,#61850));
#14847=EDGE_LOOP('',(#61851,#61852,#61853,#61854));
#14848=EDGE_LOOP('',(#61855,#61856,#61857,#61858));
#14849=EDGE_LOOP('',(#61859,#61860,#61861,#61862));
#14850=EDGE_LOOP('',(#61863,#61864,#61865,#61866));
#14851=EDGE_LOOP('',(#61867,#61868,#61869,#61870));
#14852=EDGE_LOOP('',(#61871,#61872,#61873,#61874));
#14853=EDGE_LOOP('',(#61875,#61876,#61877,#61878));
#14854=EDGE_LOOP('',(#61879,#61880,#61881,#61882));
#14855=EDGE_LOOP('',(#61883,#61884,#61885,#61886));
#14856=EDGE_LOOP('',(#61887,#61888,#61889,#61890));
#14857=EDGE_LOOP('',(#61891,#61892,#61893,#61894));
#14858=EDGE_LOOP('',(#61895,#61896,#61897,#61898));
#14859=EDGE_LOOP('',(#61899,#61900,#61901,#61902));
#14860=EDGE_LOOP('',(#61903,#61904,#61905,#61906));
#14861=EDGE_LOOP('',(#61907,#61908,#61909,#61910));
#14862=EDGE_LOOP('',(#61911,#61912,#61913,#61914));
#14863=EDGE_LOOP('',(#61915,#61916,#61917,#61918));
#14864=EDGE_LOOP('',(#61919,#61920,#61921,#61922));
#14865=EDGE_LOOP('',(#61923,#61924,#61925,#61926));
#14866=EDGE_LOOP('',(#61927,#61928,#61929,#61930));
#14867=EDGE_LOOP('',(#61931,#61932,#61933,#61934));
#14868=EDGE_LOOP('',(#61935,#61936,#61937,#61938));
#14869=EDGE_LOOP('',(#61939,#61940,#61941,#61942));
#14870=EDGE_LOOP('',(#61943,#61944,#61945,#61946));
#14871=EDGE_LOOP('',(#61947,#61948,#61949,#61950));
#14872=EDGE_LOOP('',(#61951,#61952,#61953,#61954));
#14873=EDGE_LOOP('',(#61955,#61956,#61957,#61958));
#14874=EDGE_LOOP('',(#61959,#61960,#61961,#61962));
#14875=EDGE_LOOP('',(#61963,#61964,#61965,#61966));
#14876=EDGE_LOOP('',(#61967,#61968,#61969,#61970));
#14877=EDGE_LOOP('',(#61971,#61972,#61973,#61974));
#14878=EDGE_LOOP('',(#61975,#61976,#61977,#61978));
#14879=EDGE_LOOP('',(#61979,#61980,#61981,#61982));
#14880=EDGE_LOOP('',(#61983,#61984,#61985,#61986));
#14881=EDGE_LOOP('',(#61987,#61988,#61989,#61990));
#14882=EDGE_LOOP('',(#61991,#61992,#61993,#61994));
#14883=EDGE_LOOP('',(#61995,#61996,#61997,#61998));
#14884=EDGE_LOOP('',(#61999,#62000,#62001,#62002));
#14885=EDGE_LOOP('',(#62003,#62004,#62005,#62006));
#14886=EDGE_LOOP('',(#62007,#62008,#62009,#62010));
#14887=EDGE_LOOP('',(#62011,#62012,#62013,#62014));
#14888=EDGE_LOOP('',(#62015,#62016,#62017,#62018));
#14889=EDGE_LOOP('',(#62019,#62020,#62021,#62022));
#14890=EDGE_LOOP('',(#62023,#62024,#62025,#62026));
#14891=EDGE_LOOP('',(#62027,#62028,#62029,#62030));
#14892=EDGE_LOOP('',(#62031,#62032,#62033,#62034));
#14893=EDGE_LOOP('',(#62035,#62036,#62037,#62038));
#14894=EDGE_LOOP('',(#62039,#62040,#62041,#62042));
#14895=EDGE_LOOP('',(#62043,#62044,#62045,#62046));
#14896=EDGE_LOOP('',(#62047,#62048,#62049,#62050));
#14897=EDGE_LOOP('',(#62051,#62052,#62053,#62054));
#14898=EDGE_LOOP('',(#62055,#62056,#62057,#62058));
#14899=EDGE_LOOP('',(#62059,#62060,#62061,#62062));
#14900=EDGE_LOOP('',(#62063,#62064,#62065,#62066));
#14901=EDGE_LOOP('',(#62067,#62068,#62069,#62070));
#14902=EDGE_LOOP('',(#62071,#62072,#62073,#62074));
#14903=EDGE_LOOP('',(#62075,#62076,#62077,#62078));
#14904=EDGE_LOOP('',(#62079,#62080,#62081,#62082));
#14905=EDGE_LOOP('',(#62083,#62084,#62085,#62086));
#14906=EDGE_LOOP('',(#62087,#62088,#62089,#62090));
#14907=EDGE_LOOP('',(#62091,#62092,#62093,#62094));
#14908=EDGE_LOOP('',(#62095,#62096,#62097,#62098));
#14909=EDGE_LOOP('',(#62099,#62100,#62101,#62102));
#14910=EDGE_LOOP('',(#62103,#62104,#62105,#62106));
#14911=EDGE_LOOP('',(#62107,#62108,#62109,#62110));
#14912=EDGE_LOOP('',(#62111,#62112,#62113,#62114));
#14913=EDGE_LOOP('',(#62115,#62116,#62117,#62118));
#14914=EDGE_LOOP('',(#62119,#62120,#62121,#62122));
#14915=EDGE_LOOP('',(#62123,#62124,#62125,#62126));
#14916=EDGE_LOOP('',(#62127,#62128,#62129,#62130));
#14917=EDGE_LOOP('',(#62131,#62132,#62133,#62134));
#14918=EDGE_LOOP('',(#62135,#62136,#62137,#62138));
#14919=EDGE_LOOP('',(#62139,#62140,#62141,#62142));
#14920=EDGE_LOOP('',(#62143,#62144,#62145,#62146));
#14921=EDGE_LOOP('',(#62147,#62148,#62149,#62150));
#14922=EDGE_LOOP('',(#62151,#62152,#62153,#62154));
#14923=EDGE_LOOP('',(#62155,#62156,#62157,#62158));
#14924=EDGE_LOOP('',(#62159,#62160,#62161,#62162));
#14925=EDGE_LOOP('',(#62163,#62164,#62165,#62166));
#14926=EDGE_LOOP('',(#62167,#62168,#62169,#62170));
#14927=EDGE_LOOP('',(#62171,#62172,#62173,#62174));
#14928=EDGE_LOOP('',(#62175,#62176,#62177,#62178));
#14929=EDGE_LOOP('',(#62179,#62180,#62181,#62182));
#14930=EDGE_LOOP('',(#62183,#62184,#62185,#62186));
#14931=EDGE_LOOP('',(#62187,#62188,#62189,#62190));
#14932=EDGE_LOOP('',(#62191,#62192,#62193,#62194));
#14933=EDGE_LOOP('',(#62195,#62196,#62197,#62198));
#14934=EDGE_LOOP('',(#62199,#62200,#62201,#62202));
#14935=EDGE_LOOP('',(#62203,#62204,#62205,#62206));
#14936=EDGE_LOOP('',(#62207,#62208,#62209,#62210));
#14937=EDGE_LOOP('',(#62211,#62212,#62213,#62214));
#14938=EDGE_LOOP('',(#62215,#62216,#62217,#62218));
#14939=EDGE_LOOP('',(#62219,#62220,#62221,#62222));
#14940=EDGE_LOOP('',(#62223,#62224,#62225,#62226));
#14941=EDGE_LOOP('',(#62227,#62228,#62229,#62230));
#14942=EDGE_LOOP('',(#62231,#62232,#62233,#62234));
#14943=EDGE_LOOP('',(#62235,#62236,#62237,#62238));
#14944=EDGE_LOOP('',(#62239,#62240,#62241,#62242));
#14945=EDGE_LOOP('',(#62243,#62244,#62245,#62246));
#14946=EDGE_LOOP('',(#62247,#62248,#62249,#62250));
#14947=EDGE_LOOP('',(#62251,#62252,#62253,#62254));
#14948=EDGE_LOOP('',(#62255,#62256,#62257,#62258));
#14949=EDGE_LOOP('',(#62259,#62260,#62261,#62262));
#14950=EDGE_LOOP('',(#62263,#62264,#62265,#62266));
#14951=EDGE_LOOP('',(#62267,#62268,#62269,#62270));
#14952=EDGE_LOOP('',(#62271,#62272,#62273,#62274));
#14953=EDGE_LOOP('',(#62275,#62276,#62277,#62278));
#14954=EDGE_LOOP('',(#62279,#62280,#62281,#62282));
#14955=EDGE_LOOP('',(#62283,#62284,#62285,#62286));
#14956=EDGE_LOOP('',(#62287,#62288,#62289,#62290));
#14957=EDGE_LOOP('',(#62291,#62292,#62293,#62294));
#14958=EDGE_LOOP('',(#62295,#62296,#62297,#62298));
#14959=EDGE_LOOP('',(#62299,#62300,#62301,#62302));
#14960=EDGE_LOOP('',(#62303,#62304,#62305,#62306));
#14961=EDGE_LOOP('',(#62307,#62308,#62309,#62310));
#14962=EDGE_LOOP('',(#62311,#62312,#62313,#62314));
#14963=EDGE_LOOP('',(#62315,#62316,#62317,#62318));
#14964=EDGE_LOOP('',(#62319,#62320,#62321,#62322));
#14965=EDGE_LOOP('',(#62323,#62324,#62325,#62326));
#14966=EDGE_LOOP('',(#62327,#62328,#62329,#62330));
#14967=EDGE_LOOP('',(#62331,#62332,#62333,#62334));
#14968=EDGE_LOOP('',(#62335,#62336,#62337,#62338));
#14969=EDGE_LOOP('',(#62339,#62340,#62341,#62342));
#14970=EDGE_LOOP('',(#62343,#62344,#62345,#62346));
#14971=EDGE_LOOP('',(#62347,#62348,#62349,#62350));
#14972=EDGE_LOOP('',(#62351,#62352,#62353,#62354));
#14973=EDGE_LOOP('',(#62355,#62356,#62357,#62358));
#14974=EDGE_LOOP('',(#62359,#62360,#62361,#62362));
#14975=EDGE_LOOP('',(#62363,#62364,#62365,#62366));
#14976=EDGE_LOOP('',(#62367,#62368,#62369,#62370));
#14977=EDGE_LOOP('',(#62371,#62372,#62373,#62374));
#14978=EDGE_LOOP('',(#62375,#62376,#62377,#62378));
#14979=EDGE_LOOP('',(#62379,#62380,#62381,#62382));
#14980=EDGE_LOOP('',(#62383,#62384,#62385,#62386));
#14981=EDGE_LOOP('',(#62387,#62388,#62389,#62390));
#14982=EDGE_LOOP('',(#62391,#62392,#62393,#62394));
#14983=EDGE_LOOP('',(#62395,#62396,#62397,#62398));
#14984=EDGE_LOOP('',(#62399,#62400,#62401,#62402));
#14985=EDGE_LOOP('',(#62403,#62404,#62405,#62406));
#14986=EDGE_LOOP('',(#62407,#62408,#62409,#62410));
#14987=EDGE_LOOP('',(#62411,#62412,#62413,#62414));
#14988=EDGE_LOOP('',(#62415,#62416,#62417,#62418));
#14989=EDGE_LOOP('',(#62419,#62420,#62421,#62422));
#14990=EDGE_LOOP('',(#62423,#62424,#62425,#62426));
#14991=EDGE_LOOP('',(#62427,#62428,#62429,#62430));
#14992=EDGE_LOOP('',(#62431,#62432,#62433,#62434));
#14993=EDGE_LOOP('',(#62435,#62436,#62437,#62438));
#14994=EDGE_LOOP('',(#62439,#62440,#62441,#62442));
#14995=EDGE_LOOP('',(#62443,#62444,#62445,#62446));
#14996=EDGE_LOOP('',(#62447,#62448,#62449,#62450));
#14997=EDGE_LOOP('',(#62451,#62452,#62453,#62454));
#14998=EDGE_LOOP('',(#62455,#62456,#62457,#62458));
#14999=EDGE_LOOP('',(#62459,#62460,#62461,#62462));
#15000=EDGE_LOOP('',(#62463,#62464,#62465,#62466));
#15001=EDGE_LOOP('',(#62467,#62468,#62469,#62470));
#15002=EDGE_LOOP('',(#62471,#62472,#62473,#62474));
#15003=EDGE_LOOP('',(#62475,#62476,#62477,#62478));
#15004=EDGE_LOOP('',(#62479,#62480,#62481,#62482));
#15005=EDGE_LOOP('',(#62483,#62484,#62485,#62486));
#15006=EDGE_LOOP('',(#62487,#62488,#62489,#62490));
#15007=EDGE_LOOP('',(#62491,#62492,#62493,#62494));
#15008=EDGE_LOOP('',(#62495,#62496,#62497,#62498));
#15009=EDGE_LOOP('',(#62499,#62500,#62501,#62502));
#15010=EDGE_LOOP('',(#62503,#62504,#62505,#62506));
#15011=EDGE_LOOP('',(#62507,#62508,#62509,#62510));
#15012=EDGE_LOOP('',(#62511,#62512,#62513,#62514));
#15013=EDGE_LOOP('',(#62515,#62516,#62517,#62518));
#15014=EDGE_LOOP('',(#62519,#62520,#62521,#62522));
#15015=EDGE_LOOP('',(#62523,#62524,#62525,#62526));
#15016=EDGE_LOOP('',(#62527,#62528,#62529,#62530));
#15017=EDGE_LOOP('',(#62531,#62532,#62533,#62534));
#15018=EDGE_LOOP('',(#62535,#62536,#62537,#62538));
#15019=EDGE_LOOP('',(#62539,#62540,#62541,#62542));
#15020=EDGE_LOOP('',(#62543,#62544,#62545,#62546));
#15021=EDGE_LOOP('',(#62547,#62548,#62549,#62550));
#15022=EDGE_LOOP('',(#62551,#62552,#62553,#62554));
#15023=EDGE_LOOP('',(#62555,#62556,#62557,#62558));
#15024=EDGE_LOOP('',(#62559,#62560,#62561,#62562));
#15025=EDGE_LOOP('',(#62563,#62564,#62565,#62566));
#15026=EDGE_LOOP('',(#62567,#62568,#62569,#62570));
#15027=EDGE_LOOP('',(#62571,#62572,#62573,#62574));
#15028=EDGE_LOOP('',(#62575,#62576,#62577,#62578));
#15029=EDGE_LOOP('',(#62579,#62580,#62581,#62582));
#15030=EDGE_LOOP('',(#62583,#62584,#62585,#62586));
#15031=EDGE_LOOP('',(#62587,#62588,#62589,#62590));
#15032=EDGE_LOOP('',(#62591,#62592,#62593,#62594));
#15033=EDGE_LOOP('',(#62595,#62596,#62597,#62598));
#15034=EDGE_LOOP('',(#62599,#62600,#62601,#62602));
#15035=EDGE_LOOP('',(#62603,#62604,#62605,#62606));
#15036=EDGE_LOOP('',(#62607,#62608,#62609,#62610));
#15037=EDGE_LOOP('',(#62611,#62612,#62613,#62614));
#15038=EDGE_LOOP('',(#62615,#62616,#62617,#62618));
#15039=EDGE_LOOP('',(#62619,#62620,#62621,#62622));
#15040=EDGE_LOOP('',(#62623,#62624,#62625,#62626));
#15041=EDGE_LOOP('',(#62627,#62628,#62629,#62630));
#15042=EDGE_LOOP('',(#62631,#62632,#62633,#62634));
#15043=EDGE_LOOP('',(#62635,#62636,#62637,#62638));
#15044=EDGE_LOOP('',(#62639,#62640,#62641,#62642));
#15045=EDGE_LOOP('',(#62643,#62644,#62645,#62646));
#15046=EDGE_LOOP('',(#62647,#62648,#62649,#62650));
#15047=EDGE_LOOP('',(#62651,#62652,#62653,#62654));
#15048=EDGE_LOOP('',(#62655,#62656,#62657,#62658));
#15049=EDGE_LOOP('',(#62659,#62660,#62661,#62662));
#15050=EDGE_LOOP('',(#62663,#62664,#62665,#62666));
#15051=EDGE_LOOP('',(#62667,#62668,#62669,#62670));
#15052=EDGE_LOOP('',(#62671,#62672,#62673,#62674));
#15053=EDGE_LOOP('',(#62675,#62676,#62677,#62678));
#15054=EDGE_LOOP('',(#62679,#62680,#62681,#62682));
#15055=EDGE_LOOP('',(#62683,#62684,#62685,#62686));
#15056=EDGE_LOOP('',(#62687,#62688,#62689,#62690));
#15057=EDGE_LOOP('',(#62691,#62692,#62693,#62694));
#15058=EDGE_LOOP('',(#62695,#62696,#62697,#62698));
#15059=EDGE_LOOP('',(#62699,#62700,#62701,#62702));
#15060=EDGE_LOOP('',(#62703,#62704,#62705,#62706));
#15061=EDGE_LOOP('',(#62707,#62708,#62709,#62710));
#15062=EDGE_LOOP('',(#62711,#62712,#62713,#62714));
#15063=EDGE_LOOP('',(#62715,#62716,#62717,#62718));
#15064=EDGE_LOOP('',(#62719,#62720,#62721,#62722));
#15065=EDGE_LOOP('',(#62723,#62724,#62725,#62726));
#15066=EDGE_LOOP('',(#62727,#62728,#62729,#62730));
#15067=EDGE_LOOP('',(#62731,#62732,#62733,#62734));
#15068=EDGE_LOOP('',(#62735,#62736,#62737,#62738));
#15069=EDGE_LOOP('',(#62739,#62740,#62741,#62742));
#15070=EDGE_LOOP('',(#62743,#62744,#62745,#62746));
#15071=EDGE_LOOP('',(#62747,#62748,#62749,#62750));
#15072=EDGE_LOOP('',(#62751,#62752,#62753,#62754));
#15073=EDGE_LOOP('',(#62755,#62756,#62757,#62758));
#15074=EDGE_LOOP('',(#62759,#62760,#62761,#62762));
#15075=EDGE_LOOP('',(#62763,#62764,#62765,#62766));
#15076=EDGE_LOOP('',(#62767,#62768,#62769,#62770));
#15077=EDGE_LOOP('',(#62771,#62772,#62773,#62774));
#15078=EDGE_LOOP('',(#62775,#62776,#62777,#62778));
#15079=EDGE_LOOP('',(#62779,#62780,#62781,#62782));
#15080=EDGE_LOOP('',(#62783,#62784,#62785,#62786));
#15081=EDGE_LOOP('',(#62787,#62788,#62789,#62790));
#15082=EDGE_LOOP('',(#62791,#62792,#62793,#62794));
#15083=EDGE_LOOP('',(#62795,#62796,#62797,#62798));
#15084=EDGE_LOOP('',(#62799,#62800,#62801,#62802));
#15085=EDGE_LOOP('',(#62803,#62804,#62805,#62806));
#15086=EDGE_LOOP('',(#62807,#62808,#62809,#62810));
#15087=EDGE_LOOP('',(#62811,#62812,#62813,#62814));
#15088=EDGE_LOOP('',(#62815,#62816,#62817,#62818));
#15089=EDGE_LOOP('',(#62819,#62820,#62821,#62822));
#15090=EDGE_LOOP('',(#62823,#62824,#62825,#62826));
#15091=EDGE_LOOP('',(#62827,#62828,#62829,#62830));
#15092=EDGE_LOOP('',(#62831,#62832,#62833,#62834));
#15093=EDGE_LOOP('',(#62835,#62836,#62837,#62838));
#15094=EDGE_LOOP('',(#62839,#62840,#62841,#62842));
#15095=EDGE_LOOP('',(#62843,#62844,#62845,#62846));
#15096=EDGE_LOOP('',(#62847,#62848,#62849,#62850));
#15097=EDGE_LOOP('',(#62851,#62852,#62853,#62854));
#15098=EDGE_LOOP('',(#62855,#62856,#62857,#62858));
#15099=EDGE_LOOP('',(#62859,#62860,#62861,#62862));
#15100=EDGE_LOOP('',(#62863,#62864,#62865,#62866));
#15101=EDGE_LOOP('',(#62867,#62868,#62869,#62870));
#15102=EDGE_LOOP('',(#62871,#62872,#62873,#62874));
#15103=EDGE_LOOP('',(#62875,#62876,#62877,#62878));
#15104=EDGE_LOOP('',(#62879,#62880,#62881,#62882));
#15105=EDGE_LOOP('',(#62883,#62884,#62885,#62886));
#15106=EDGE_LOOP('',(#62887,#62888,#62889,#62890));
#15107=EDGE_LOOP('',(#62891,#62892,#62893,#62894));
#15108=EDGE_LOOP('',(#62895,#62896,#62897,#62898));
#15109=EDGE_LOOP('',(#62899,#62900,#62901,#62902));
#15110=EDGE_LOOP('',(#62903,#62904,#62905,#62906));
#15111=EDGE_LOOP('',(#62907,#62908,#62909,#62910));
#15112=EDGE_LOOP('',(#62911,#62912,#62913,#62914));
#15113=EDGE_LOOP('',(#62915,#62916,#62917,#62918));
#15114=EDGE_LOOP('',(#62919,#62920,#62921,#62922));
#15115=EDGE_LOOP('',(#62923,#62924,#62925,#62926));
#15116=EDGE_LOOP('',(#62927,#62928,#62929,#62930));
#15117=EDGE_LOOP('',(#62931,#62932,#62933,#62934));
#15118=EDGE_LOOP('',(#62935,#62936,#62937,#62938));
#15119=EDGE_LOOP('',(#62939,#62940,#62941,#62942));
#15120=EDGE_LOOP('',(#62943,#62944,#62945,#62946));
#15121=EDGE_LOOP('',(#62947,#62948,#62949,#62950));
#15122=EDGE_LOOP('',(#62951,#62952,#62953,#62954));
#15123=EDGE_LOOP('',(#62955,#62956,#62957,#62958));
#15124=EDGE_LOOP('',(#62959,#62960,#62961));
#15125=EDGE_LOOP('',(#62962,#62963,#62964));
#15126=EDGE_LOOP('',(#62965,#62966,#62967));
#15127=EDGE_LOOP('',(#62968,#62969,#62970));
#15128=EDGE_LOOP('',(#62971,#62972,#62973,#62974));
#15129=EDGE_LOOP('',(#62975,#62976,#62977,#62978));
#15130=EDGE_LOOP('',(#62979,#62980,#62981));
#15131=EDGE_LOOP('',(#62982,#62983,#62984));
#15132=EDGE_LOOP('',(#62985,#62986,#62987));
#15133=EDGE_LOOP('',(#62988,#62989,#62990));
#15134=EDGE_LOOP('',(#62991,#62992,#62993,#62994));
#15135=EDGE_LOOP('',(#62995,#62996,#62997,#62998));
#15136=EDGE_LOOP('',(#62999,#63000,#63001));
#15137=EDGE_LOOP('',(#63002,#63003,#63004));
#15138=EDGE_LOOP('',(#63005,#63006,#63007));
#15139=EDGE_LOOP('',(#63008,#63009,#63010));
#15140=EDGE_LOOP('',(#63011,#63012,#63013,#63014));
#15141=EDGE_LOOP('',(#63015,#63016,#63017,#63018));
#15142=EDGE_LOOP('',(#63019,#63020,#63021));
#15143=EDGE_LOOP('',(#63022,#63023,#63024));
#15144=EDGE_LOOP('',(#63025,#63026,#63027));
#15145=EDGE_LOOP('',(#63028,#63029,#63030));
#15146=EDGE_LOOP('',(#63031,#63032,#63033,#63034));
#15147=EDGE_LOOP('',(#63035,#63036,#63037,#63038));
#15148=EDGE_LOOP('',(#63039,#63040,#63041));
#15149=EDGE_LOOP('',(#63042,#63043,#63044));
#15150=EDGE_LOOP('',(#63045,#63046,#63047));
#15151=EDGE_LOOP('',(#63048,#63049,#63050));
#15152=EDGE_LOOP('',(#63051,#63052,#63053,#63054));
#15153=EDGE_LOOP('',(#63055,#63056,#63057,#63058));
#15154=EDGE_LOOP('',(#63059,#63060,#63061));
#15155=EDGE_LOOP('',(#63062,#63063,#63064));
#15156=EDGE_LOOP('',(#63065,#63066,#63067));
#15157=EDGE_LOOP('',(#63068,#63069,#63070));
#15158=EDGE_LOOP('',(#63071,#63072,#63073,#63074));
#15159=EDGE_LOOP('',(#63075,#63076,#63077,#63078));
#15160=EDGE_LOOP('',(#63079,#63080,#63081));
#15161=EDGE_LOOP('',(#63082,#63083,#63084));
#15162=EDGE_LOOP('',(#63085,#63086,#63087));
#15163=EDGE_LOOP('',(#63088,#63089,#63090));
#15164=EDGE_LOOP('',(#63091,#63092,#63093,#63094));
#15165=EDGE_LOOP('',(#63095,#63096,#63097,#63098));
#15166=EDGE_LOOP('',(#63099,#63100,#63101));
#15167=EDGE_LOOP('',(#63102,#63103,#63104));
#15168=EDGE_LOOP('',(#63105,#63106,#63107));
#15169=EDGE_LOOP('',(#63108,#63109,#63110));
#15170=EDGE_LOOP('',(#63111,#63112,#63113,#63114));
#15171=EDGE_LOOP('',(#63115,#63116,#63117,#63118));
#15172=EDGE_LOOP('',(#63119,#63120,#63121));
#15173=EDGE_LOOP('',(#63122,#63123,#63124));
#15174=EDGE_LOOP('',(#63125,#63126,#63127));
#15175=EDGE_LOOP('',(#63128,#63129,#63130));
#15176=EDGE_LOOP('',(#63131,#63132,#63133,#63134));
#15177=EDGE_LOOP('',(#63135,#63136,#63137,#63138));
#15178=EDGE_LOOP('',(#63139,#63140,#63141));
#15179=EDGE_LOOP('',(#63142,#63143,#63144));
#15180=EDGE_LOOP('',(#63145,#63146,#63147));
#15181=EDGE_LOOP('',(#63148,#63149,#63150));
#15182=EDGE_LOOP('',(#63151,#63152,#63153,#63154));
#15183=EDGE_LOOP('',(#63155,#63156,#63157,#63158));
#15184=EDGE_LOOP('',(#63159,#63160,#63161));
#15185=EDGE_LOOP('',(#63162,#63163,#63164));
#15186=EDGE_LOOP('',(#63165,#63166,#63167));
#15187=EDGE_LOOP('',(#63168,#63169,#63170));
#15188=EDGE_LOOP('',(#63171,#63172,#63173,#63174));
#15189=EDGE_LOOP('',(#63175,#63176,#63177,#63178));
#15190=EDGE_LOOP('',(#63179,#63180,#63181));
#15191=EDGE_LOOP('',(#63182,#63183,#63184));
#15192=EDGE_LOOP('',(#63185,#63186,#63187));
#15193=EDGE_LOOP('',(#63188,#63189,#63190));
#15194=EDGE_LOOP('',(#63191,#63192,#63193,#63194));
#15195=EDGE_LOOP('',(#63195,#63196,#63197,#63198));
#15196=EDGE_LOOP('',(#63199,#63200,#63201));
#15197=EDGE_LOOP('',(#63202,#63203,#63204));
#15198=EDGE_LOOP('',(#63205,#63206,#63207));
#15199=EDGE_LOOP('',(#63208,#63209,#63210));
#15200=EDGE_LOOP('',(#63211,#63212,#63213,#63214));
#15201=EDGE_LOOP('',(#63215,#63216,#63217,#63218));
#15202=EDGE_LOOP('',(#63219,#63220,#63221));
#15203=EDGE_LOOP('',(#63222,#63223,#63224));
#15204=EDGE_LOOP('',(#63225,#63226,#63227));
#15205=EDGE_LOOP('',(#63228,#63229,#63230));
#15206=EDGE_LOOP('',(#63231,#63232,#63233,#63234));
#15207=EDGE_LOOP('',(#63235,#63236,#63237,#63238));
#15208=EDGE_LOOP('',(#63239,#63240,#63241));
#15209=EDGE_LOOP('',(#63242,#63243,#63244));
#15210=EDGE_LOOP('',(#63245,#63246,#63247));
#15211=EDGE_LOOP('',(#63248,#63249,#63250));
#15212=EDGE_LOOP('',(#63251,#63252,#63253,#63254));
#15213=EDGE_LOOP('',(#63255,#63256,#63257,#63258));
#15214=EDGE_LOOP('',(#63259,#63260,#63261));
#15215=EDGE_LOOP('',(#63262,#63263,#63264));
#15216=EDGE_LOOP('',(#63265,#63266,#63267));
#15217=EDGE_LOOP('',(#63268,#63269,#63270));
#15218=EDGE_LOOP('',(#63271,#63272,#63273,#63274));
#15219=EDGE_LOOP('',(#63275,#63276,#63277,#63278));
#15220=EDGE_LOOP('',(#63279,#63280,#63281));
#15221=EDGE_LOOP('',(#63282,#63283,#63284));
#15222=EDGE_LOOP('',(#63285,#63286,#63287));
#15223=EDGE_LOOP('',(#63288,#63289,#63290));
#15224=EDGE_LOOP('',(#63291,#63292,#63293,#63294));
#15225=EDGE_LOOP('',(#63295,#63296,#63297,#63298));
#15226=EDGE_LOOP('',(#63299,#63300,#63301));
#15227=EDGE_LOOP('',(#63302,#63303,#63304));
#15228=EDGE_LOOP('',(#63305,#63306,#63307));
#15229=EDGE_LOOP('',(#63308,#63309,#63310));
#15230=EDGE_LOOP('',(#63311,#63312,#63313,#63314));
#15231=EDGE_LOOP('',(#63315,#63316,#63317,#63318));
#15232=EDGE_LOOP('',(#63319,#63320,#63321));
#15233=EDGE_LOOP('',(#63322,#63323,#63324));
#15234=EDGE_LOOP('',(#63325,#63326,#63327));
#15235=EDGE_LOOP('',(#63328,#63329,#63330));
#15236=EDGE_LOOP('',(#63331,#63332,#63333,#63334));
#15237=EDGE_LOOP('',(#63335,#63336,#63337,#63338));
#15238=EDGE_LOOP('',(#63339,#63340,#63341));
#15239=EDGE_LOOP('',(#63342,#63343,#63344));
#15240=EDGE_LOOP('',(#63345,#63346,#63347));
#15241=EDGE_LOOP('',(#63348,#63349,#63350));
#15242=EDGE_LOOP('',(#63351,#63352,#63353,#63354));
#15243=EDGE_LOOP('',(#63355,#63356,#63357,#63358));
#15244=EDGE_LOOP('',(#63359,#63360,#63361));
#15245=EDGE_LOOP('',(#63362,#63363,#63364));
#15246=EDGE_LOOP('',(#63365,#63366,#63367));
#15247=EDGE_LOOP('',(#63368,#63369,#63370));
#15248=EDGE_LOOP('',(#63371,#63372,#63373,#63374));
#15249=EDGE_LOOP('',(#63375,#63376,#63377,#63378));
#15250=EDGE_LOOP('',(#63379,#63380,#63381));
#15251=EDGE_LOOP('',(#63382,#63383,#63384));
#15252=EDGE_LOOP('',(#63385,#63386,#63387));
#15253=EDGE_LOOP('',(#63388,#63389,#63390));
#15254=EDGE_LOOP('',(#63391,#63392,#63393,#63394));
#15255=EDGE_LOOP('',(#63395,#63396,#63397,#63398));
#15256=EDGE_LOOP('',(#63399,#63400,#63401));
#15257=EDGE_LOOP('',(#63402,#63403,#63404));
#15258=EDGE_LOOP('',(#63405,#63406,#63407));
#15259=EDGE_LOOP('',(#63408,#63409,#63410));
#15260=EDGE_LOOP('',(#63411,#63412,#63413,#63414));
#15261=EDGE_LOOP('',(#63415,#63416,#63417,#63418));
#15262=EDGE_LOOP('',(#63419,#63420,#63421));
#15263=EDGE_LOOP('',(#63422,#63423,#63424));
#15264=EDGE_LOOP('',(#63425,#63426,#63427));
#15265=EDGE_LOOP('',(#63428,#63429,#63430));
#15266=EDGE_LOOP('',(#63431,#63432,#63433,#63434));
#15267=EDGE_LOOP('',(#63435,#63436,#63437,#63438));
#15268=EDGE_LOOP('',(#63439,#63440,#63441));
#15269=EDGE_LOOP('',(#63442,#63443,#63444));
#15270=EDGE_LOOP('',(#63445,#63446,#63447));
#15271=EDGE_LOOP('',(#63448,#63449,#63450));
#15272=EDGE_LOOP('',(#63451,#63452,#63453,#63454));
#15273=EDGE_LOOP('',(#63455,#63456,#63457,#63458));
#15274=EDGE_LOOP('',(#63459,#63460,#63461));
#15275=EDGE_LOOP('',(#63462,#63463,#63464));
#15276=EDGE_LOOP('',(#63465,#63466,#63467));
#15277=EDGE_LOOP('',(#63468,#63469,#63470));
#15278=EDGE_LOOP('',(#63471,#63472,#63473,#63474));
#15279=EDGE_LOOP('',(#63475,#63476,#63477,#63478));
#15280=EDGE_LOOP('',(#63479,#63480,#63481));
#15281=EDGE_LOOP('',(#63482,#63483,#63484));
#15282=EDGE_LOOP('',(#63485,#63486,#63487));
#15283=EDGE_LOOP('',(#63488,#63489,#63490));
#15284=EDGE_LOOP('',(#63491,#63492,#63493,#63494));
#15285=EDGE_LOOP('',(#63495,#63496,#63497,#63498));
#15286=EDGE_LOOP('',(#63499,#63500,#63501));
#15287=EDGE_LOOP('',(#63502,#63503,#63504));
#15288=EDGE_LOOP('',(#63505,#63506,#63507));
#15289=EDGE_LOOP('',(#63508,#63509,#63510));
#15290=EDGE_LOOP('',(#63511,#63512,#63513,#63514));
#15291=EDGE_LOOP('',(#63515,#63516,#63517,#63518));
#15292=EDGE_LOOP('',(#63519,#63520,#63521));
#15293=EDGE_LOOP('',(#63522,#63523,#63524));
#15294=EDGE_LOOP('',(#63525,#63526,#63527));
#15295=EDGE_LOOP('',(#63528,#63529,#63530));
#15296=EDGE_LOOP('',(#63531,#63532,#63533,#63534));
#15297=EDGE_LOOP('',(#63535,#63536,#63537,#63538,#63539));
#15298=EDGE_LOOP('',(#63540,#63541,#63542,#63543));
#15299=EDGE_LOOP('',(#63544,#63545,#63546,#63547));
#15300=EDGE_LOOP('',(#63548,#63549,#63550,#63551));
#15301=EDGE_LOOP('',(#63552,#63553,#63554,#63555));
#15302=EDGE_LOOP('',(#63556,#63557,#63558,#63559));
#15303=EDGE_LOOP('',(#63560,#63561,#63562,#63563));
#15304=EDGE_LOOP('',(#63564,#63565,#63566,#63567));
#15305=EDGE_LOOP('',(#63568,#63569,#63570,#63571));
#15306=EDGE_LOOP('',(#63572,#63573,#63574,#63575));
#15307=EDGE_LOOP('',(#63576,#63577,#63578,#63579));
#15308=EDGE_LOOP('',(#63580,#63581,#63582,#63583));
#15309=EDGE_LOOP('',(#63584,#63585,#63586,#63587));
#15310=EDGE_LOOP('',(#63588,#63589,#63590,#63591));
#15311=EDGE_LOOP('',(#63592,#63593,#63594,#63595));
#15312=EDGE_LOOP('',(#63596,#63597,#63598,#63599));
#15313=EDGE_LOOP('',(#63600,#63601,#63602,#63603));
#15314=EDGE_LOOP('',(#63604,#63605,#63606,#63607));
#15315=EDGE_LOOP('',(#63608,#63609,#63610,#63611));
#15316=EDGE_LOOP('',(#63612,#63613,#63614,#63615));
#15317=EDGE_LOOP('',(#63616,#63617,#63618,#63619));
#15318=EDGE_LOOP('',(#63620,#63621,#63622,#63623));
#15319=EDGE_LOOP('',(#63624,#63625,#63626,#63627));
#15320=EDGE_LOOP('',(#63628,#63629,#63630,#63631));
#15321=EDGE_LOOP('',(#63632,#63633,#63634,#63635));
#15322=EDGE_LOOP('',(#63636,#63637,#63638,#63639));
#15323=EDGE_LOOP('',(#63640,#63641,#63642,#63643));
#15324=EDGE_LOOP('',(#63644,#63645,#63646,#63647));
#15325=EDGE_LOOP('',(#63648,#63649,#63650,#63651));
#15326=EDGE_LOOP('',(#63652,#63653,#63654,#63655));
#15327=EDGE_LOOP('',(#63656,#63657,#63658,#63659));
#15328=EDGE_LOOP('',(#63660,#63661,#63662,#63663));
#15329=EDGE_LOOP('',(#63664,#63665,#63666,#63667));
#15330=EDGE_LOOP('',(#63668,#63669,#63670,#63671));
#15331=EDGE_LOOP('',(#63672,#63673,#63674,#63675));
#15332=EDGE_LOOP('',(#63676,#63677,#63678,#63679));
#15333=EDGE_LOOP('',(#63680,#63681,#63682,#63683));
#15334=EDGE_LOOP('',(#63684,#63685,#63686,#63687));
#15335=EDGE_LOOP('',(#63688,#63689,#63690,#63691));
#15336=EDGE_LOOP('',(#63692,#63693,#63694,#63695));
#15337=EDGE_LOOP('',(#63696,#63697,#63698,#63699));
#15338=EDGE_LOOP('',(#63700,#63701,#63702,#63703));
#15339=EDGE_LOOP('',(#63704,#63705,#63706,#63707));
#15340=EDGE_LOOP('',(#63708,#63709,#63710,#63711));
#15341=EDGE_LOOP('',(#63712,#63713,#63714,#63715));
#15342=EDGE_LOOP('',(#63716,#63717,#63718,#63719));
#15343=EDGE_LOOP('',(#63720,#63721,#63722,#63723));
#15344=EDGE_LOOP('',(#63724,#63725,#63726,#63727));
#15345=EDGE_LOOP('',(#63728,#63729,#63730,#63731));
#15346=EDGE_LOOP('',(#63732,#63733,#63734,#63735));
#15347=EDGE_LOOP('',(#63736,#63737,#63738,#63739));
#15348=EDGE_LOOP('',(#63740,#63741,#63742,#63743));
#15349=EDGE_LOOP('',(#63744,#63745,#63746,#63747));
#15350=EDGE_LOOP('',(#63748,#63749,#63750,#63751));
#15351=EDGE_LOOP('',(#63752,#63753,#63754,#63755));
#15352=EDGE_LOOP('',(#63756,#63757,#63758,#63759));
#15353=EDGE_LOOP('',(#63760,#63761,#63762,#63763));
#15354=EDGE_LOOP('',(#63764,#63765,#63766,#63767));
#15355=EDGE_LOOP('',(#63768,#63769,#63770,#63771));
#15356=EDGE_LOOP('',(#63772,#63773,#63774,#63775));
#15357=EDGE_LOOP('',(#63776,#63777,#63778,#63779));
#15358=EDGE_LOOP('',(#63780,#63781,#63782));
#15359=EDGE_LOOP('',(#63783,#63784,#63785,#63786));
#15360=EDGE_LOOP('',(#63787,#63788,#63789,#63790,#63791));
#15361=EDGE_LOOP('',(#63792,#63793,#63794,#63795));
#15362=EDGE_LOOP('',(#63796,#63797,#63798));
#15363=EDGE_LOOP('',(#63799,#63800,#63801,#63802));
#15364=EDGE_LOOP('',(#63803,#63804,#63805,#63806,#63807));
#15365=EDGE_LOOP('',(#63808,#63809,#63810,#63811));
#15366=EDGE_LOOP('',(#63812,#63813,#63814));
#15367=EDGE_LOOP('',(#63815,#63816,#63817,#63818));
#15368=EDGE_LOOP('',(#63819,#63820,#63821,#63822,#63823));
#15369=EDGE_LOOP('',(#63824,#63825,#63826,#63827));
#15370=EDGE_LOOP('',(#63828,#63829,#63830));
#15371=EDGE_LOOP('',(#63831,#63832,#63833,#63834));
#15372=EDGE_LOOP('',(#63835,#63836,#63837,#63838,#63839));
#15373=EDGE_LOOP('',(#63840,#63841,#63842,#63843));
#15374=EDGE_LOOP('',(#63844,#63845,#63846));
#15375=EDGE_LOOP('',(#63847,#63848,#63849,#63850));
#15376=EDGE_LOOP('',(#63851,#63852,#63853,#63854,#63855));
#15377=EDGE_LOOP('',(#63856,#63857,#63858,#63859));
#15378=EDGE_LOOP('',(#63860,#63861,#63862));
#15379=EDGE_LOOP('',(#63863,#63864,#63865,#63866));
#15380=EDGE_LOOP('',(#63867,#63868,#63869,#63870,#63871));
#15381=EDGE_LOOP('',(#63872,#63873,#63874,#63875));
#15382=EDGE_LOOP('',(#63876,#63877,#63878));
#15383=EDGE_LOOP('',(#63879,#63880,#63881,#63882));
#15384=EDGE_LOOP('',(#63883,#63884,#63885,#63886));
#15385=EDGE_LOOP('',(#63887,#63888,#63889));
#15386=EDGE_LOOP('',(#63890,#63891,#63892,#63893));
#15387=EDGE_LOOP('',(#63894,#63895,#63896,#63897,#63898));
#15388=EDGE_LOOP('',(#63899,#63900,#63901,#63902));
#15389=EDGE_LOOP('',(#63903,#63904,#63905));
#15390=EDGE_LOOP('',(#63906,#63907,#63908,#63909));
#15391=EDGE_LOOP('',(#63910,#63911,#63912,#63913,#63914));
#15392=EDGE_LOOP('',(#63915,#63916,#63917,#63918));
#15393=EDGE_LOOP('',(#63919,#63920,#63921));
#15394=EDGE_LOOP('',(#63922,#63923,#63924,#63925));
#15395=EDGE_LOOP('',(#63926,#63927,#63928,#63929,#63930));
#15396=EDGE_LOOP('',(#63931,#63932,#63933,#63934));
#15397=EDGE_LOOP('',(#63935,#63936,#63937));
#15398=EDGE_LOOP('',(#63938,#63939,#63940,#63941));
#15399=EDGE_LOOP('',(#63942,#63943,#63944,#63945,#63946));
#15400=EDGE_LOOP('',(#63947,#63948,#63949,#63950));
#15401=EDGE_LOOP('',(#63951,#63952,#63953));
#15402=EDGE_LOOP('',(#63954,#63955,#63956,#63957));
#15403=EDGE_LOOP('',(#63958,#63959,#63960,#63961,#63962));
#15404=EDGE_LOOP('',(#63963,#63964,#63965,#63966));
#15405=EDGE_LOOP('',(#63967,#63968,#63969));
#15406=EDGE_LOOP('',(#63970,#63971,#63972,#63973));
#15407=EDGE_LOOP('',(#63974,#63975,#63976,#63977,#63978));
#15408=EDGE_LOOP('',(#63979,#63980,#63981,#63982));
#15409=EDGE_LOOP('',(#63983,#63984,#63985));
#15410=EDGE_LOOP('',(#63986,#63987,#63988,#63989));
#15411=EDGE_LOOP('',(#63990,#63991,#63992,#63993,#63994));
#15412=EDGE_LOOP('',(#63995,#63996,#63997,#63998));
#15413=EDGE_LOOP('',(#63999,#64000,#64001));
#15414=EDGE_LOOP('',(#64002,#64003,#64004,#64005));
#15415=EDGE_LOOP('',(#64006,#64007,#64008,#64009,#64010));
#15416=EDGE_LOOP('',(#64011,#64012,#64013,#64014));
#15417=EDGE_LOOP('',(#64015,#64016,#64017));
#15418=EDGE_LOOP('',(#64018,#64019,#64020,#64021));
#15419=EDGE_LOOP('',(#64022,#64023,#64024,#64025,#64026));
#15420=EDGE_LOOP('',(#64027,#64028,#64029,#64030));
#15421=EDGE_LOOP('',(#64031,#64032,#64033));
#15422=EDGE_LOOP('',(#64034,#64035,#64036,#64037));
#15423=EDGE_LOOP('',(#64038,#64039,#64040,#64041,#64042));
#15424=EDGE_LOOP('',(#64043,#64044,#64045,#64046));
#15425=EDGE_LOOP('',(#64047,#64048,#64049));
#15426=EDGE_LOOP('',(#64050,#64051,#64052,#64053));
#15427=EDGE_LOOP('',(#64054,#64055,#64056,#64057,#64058));
#15428=EDGE_LOOP('',(#64059,#64060,#64061,#64062));
#15429=EDGE_LOOP('',(#64063,#64064,#64065));
#15430=EDGE_LOOP('',(#64066,#64067,#64068,#64069));
#15431=EDGE_LOOP('',(#64070,#64071,#64072,#64073,#64074));
#15432=EDGE_LOOP('',(#64075,#64076,#64077,#64078));
#15433=EDGE_LOOP('',(#64079,#64080,#64081));
#15434=EDGE_LOOP('',(#64082,#64083,#64084,#64085));
#15435=EDGE_LOOP('',(#64086,#64087,#64088,#64089,#64090));
#15436=EDGE_LOOP('',(#64091,#64092,#64093,#64094));
#15437=EDGE_LOOP('',(#64095,#64096,#64097));
#15438=EDGE_LOOP('',(#64098,#64099,#64100,#64101));
#15439=EDGE_LOOP('',(#64102,#64103,#64104,#64105,#64106));
#15440=EDGE_LOOP('',(#64107,#64108,#64109,#64110));
#15441=EDGE_LOOP('',(#64111,#64112,#64113));
#15442=EDGE_LOOP('',(#64114,#64115,#64116,#64117));
#15443=EDGE_LOOP('',(#64118,#64119,#64120,#64121,#64122));
#15444=EDGE_LOOP('',(#64123,#64124,#64125,#64126));
#15445=EDGE_LOOP('',(#64127,#64128,#64129));
#15446=EDGE_LOOP('',(#64130,#64131,#64132,#64133));
#15447=EDGE_LOOP('',(#64134,#64135,#64136,#64137,#64138));
#15448=EDGE_LOOP('',(#64139,#64140,#64141,#64142));
#15449=EDGE_LOOP('',(#64143,#64144,#64145));
#15450=EDGE_LOOP('',(#64146,#64147,#64148,#64149));
#15451=EDGE_LOOP('',(#64150,#64151,#64152,#64153,#64154));
#15452=EDGE_LOOP('',(#64155,#64156,#64157,#64158));
#15453=EDGE_LOOP('',(#64159,#64160,#64161));
#15454=EDGE_LOOP('',(#64162,#64163,#64164,#64165));
#15455=EDGE_LOOP('',(#64166,#64167,#64168,#64169,#64170));
#15456=EDGE_LOOP('',(#64171,#64172,#64173,#64174));
#15457=EDGE_LOOP('',(#64175,#64176,#64177));
#15458=EDGE_LOOP('',(#64178,#64179,#64180,#64181));
#15459=EDGE_LOOP('',(#64182,#64183,#64184,#64185,#64186));
#15460=EDGE_LOOP('',(#64187,#64188,#64189,#64190));
#15461=EDGE_LOOP('',(#64191,#64192,#64193));
#15462=EDGE_LOOP('',(#64194,#64195,#64196,#64197));
#15463=EDGE_LOOP('',(#64198,#64199,#64200,#64201,#64202));
#15464=EDGE_LOOP('',(#64203,#64204,#64205,#64206));
#15465=EDGE_LOOP('',(#64207,#64208,#64209));
#15466=EDGE_LOOP('',(#64210,#64211,#64212,#64213));
#15467=EDGE_LOOP('',(#64214,#64215,#64216,#64217,#64218));
#15468=EDGE_LOOP('',(#64219,#64220,#64221));
#15469=EDGE_LOOP('',(#64222,#64223,#64224,#64225,#64226));
#15470=EDGE_LOOP('',(#64227,#64228,#64229,#64230));
#15471=EDGE_LOOP('',(#64231));
#15472=EDGE_LOOP('',(#64232));
#15473=EDGE_LOOP('',(#64233,#64234,#64235,#64236,#64237));
#15474=EDGE_LOOP('',(#64238,#64239,#64240,#64241,#64242));
#15475=EDGE_LOOP('',(#64243,#64244,#64245,#64246,#64247));
#15476=EDGE_LOOP('',(#64248,#64249,#64250,#64251,#64252));
#15477=EDGE_LOOP('',(#64253,#64254,#64255,#64256,#64257));
#15478=EDGE_LOOP('',(#64258,#64259,#64260,#64261,#64262));
#15479=EDGE_LOOP('',(#64263,#64264,#64265,#64266,#64267));
#15480=EDGE_LOOP('',(#64268,#64269,#64270,#64271,#64272));
#15481=EDGE_LOOP('',(#64273,#64274,#64275,#64276,#64277));
#15482=EDGE_LOOP('',(#64278,#64279,#64280,#64281,#64282));
#15483=EDGE_LOOP('',(#64283,#64284,#64285,#64286,#64287));
#15484=EDGE_LOOP('',(#64288,#64289,#64290,#64291,#64292));
#15485=EDGE_LOOP('',(#64293,#64294,#64295,#64296,#64297));
#15486=EDGE_LOOP('',(#64298,#64299,#64300,#64301,#64302));
#15487=EDGE_LOOP('',(#64303,#64304,#64305,#64306,#64307));
#15488=EDGE_LOOP('',(#64308,#64309,#64310,#64311,#64312));
#15489=EDGE_LOOP('',(#64313,#64314,#64315,#64316,#64317));
#15490=EDGE_LOOP('',(#64318,#64319,#64320,#64321,#64322));
#15491=EDGE_LOOP('',(#64323,#64324,#64325,#64326,#64327));
#15492=EDGE_LOOP('',(#64328,#64329,#64330,#64331,#64332));
#15493=EDGE_LOOP('',(#64333,#64334,#64335,#64336,#64337));
#15494=EDGE_LOOP('',(#64338,#64339,#64340,#64341,#64342));
#15495=EDGE_LOOP('',(#64343,#64344,#64345,#64346,#64347));
#15496=EDGE_LOOP('',(#64348,#64349,#64350,#64351,#64352));
#15497=EDGE_LOOP('',(#64353,#64354,#64355,#64356,#64357));
#15498=EDGE_LOOP('',(#64358,#64359,#64360,#64361,#64362));
#15499=EDGE_LOOP('',(#64363,#64364,#64365,#64366,#64367));
#15500=EDGE_LOOP('',(#64368,#64369,#64370,#64371,#64372));
#15501=EDGE_LOOP('',(#64373,#64374,#64375,#64376,#64377));
#15502=EDGE_LOOP('',(#64378,#64379,#64380,#64381,#64382));
#15503=EDGE_LOOP('',(#64383,#64384,#64385,#64386,#64387));
#15504=EDGE_LOOP('',(#64388,#64389,#64390,#64391,#64392));
#15505=EDGE_LOOP('',(#64393,#64394,#64395,#64396,#64397));
#15506=EDGE_LOOP('',(#64398,#64399,#64400,#64401,#64402));
#15507=EDGE_LOOP('',(#64403,#64404,#64405,#64406,#64407));
#15508=EDGE_LOOP('',(#64408,#64409,#64410,#64411,#64412));
#15509=EDGE_LOOP('',(#64413,#64414,#64415,#64416,#64417));
#15510=EDGE_LOOP('',(#64418,#64419,#64420,#64421,#64422));
#15511=EDGE_LOOP('',(#64423,#64424,#64425,#64426,#64427));
#15512=EDGE_LOOP('',(#64428,#64429,#64430,#64431,#64432));
#15513=EDGE_LOOP('',(#64433,#64434,#64435,#64436,#64437));
#15514=EDGE_LOOP('',(#64438,#64439,#64440,#64441,#64442));
#15515=EDGE_LOOP('',(#64443,#64444,#64445,#64446,#64447));
#15516=EDGE_LOOP('',(#64448,#64449,#64450,#64451,#64452));
#15517=EDGE_LOOP('',(#64453,#64454,#64455,#64456,#64457));
#15518=EDGE_LOOP('',(#64458,#64459,#64460,#64461,#64462));
#15519=EDGE_LOOP('',(#64463,#64464,#64465,#64466,#64467));
#15520=EDGE_LOOP('',(#64468,#64469,#64470,#64471,#64472));
#15521=EDGE_LOOP('',(#64473,#64474,#64475,#64476,#64477));
#15522=EDGE_LOOP('',(#64478,#64479,#64480,#64481,#64482));
#15523=EDGE_LOOP('',(#64483,#64484,#64485,#64486,#64487));
#15524=EDGE_LOOP('',(#64488,#64489,#64490,#64491,#64492));
#15525=EDGE_LOOP('',(#64493,#64494,#64495,#64496,#64497));
#15526=EDGE_LOOP('',(#64498,#64499,#64500,#64501,#64502));
#15527=EDGE_LOOP('',(#64503,#64504,#64505,#64506,#64507));
#15528=EDGE_LOOP('',(#64508,#64509,#64510,#64511,#64512));
#15529=EDGE_LOOP('',(#64513,#64514,#64515,#64516,#64517));
#15530=EDGE_LOOP('',(#64518,#64519,#64520,#64521,#64522));
#15531=EDGE_LOOP('',(#64523,#64524,#64525,#64526));
#15532=EDGE_LOOP('',(#64527,#64528,#64529,#64530));
#15533=EDGE_LOOP('',(#64531,#64532,#64533,#64534));
#15534=EDGE_LOOP('',(#64535,#64536,#64537,#64538));
#15535=EDGE_LOOP('',(#64539,#64540,#64541,#64542));
#15536=EDGE_LOOP('',(#64543,#64544,#64545,#64546));
#15537=EDGE_LOOP('',(#64547,#64548,#64549,#64550));
#15538=EDGE_LOOP('',(#64551,#64552,#64553,#64554));
#15539=EDGE_LOOP('',(#64555,#64556,#64557,#64558));
#15540=EDGE_LOOP('',(#64559,#64560,#64561,#64562));
#15541=EDGE_LOOP('',(#64563,#64564,#64565,#64566));
#15542=EDGE_LOOP('',(#64567,#64568,#64569,#64570));
#15543=EDGE_LOOP('',(#64571,#64572,#64573,#64574));
#15544=EDGE_LOOP('',(#64575,#64576,#64577,#64578));
#15545=EDGE_LOOP('',(#64579,#64580,#64581,#64582));
#15546=EDGE_LOOP('',(#64583,#64584,#64585,#64586));
#15547=EDGE_LOOP('',(#64587,#64588,#64589,#64590));
#15548=EDGE_LOOP('',(#64591,#64592,#64593,#64594));
#15549=EDGE_LOOP('',(#64595,#64596,#64597,#64598));
#15550=EDGE_LOOP('',(#64599,#64600,#64601,#64602));
#15551=EDGE_LOOP('',(#64603,#64604,#64605,#64606));
#15552=EDGE_LOOP('',(#64607,#64608,#64609,#64610));
#15553=EDGE_LOOP('',(#64611,#64612,#64613,#64614));
#15554=EDGE_LOOP('',(#64615,#64616,#64617,#64618));
#15555=EDGE_LOOP('',(#64619,#64620,#64621,#64622));
#15556=EDGE_LOOP('',(#64623,#64624,#64625,#64626));
#15557=EDGE_LOOP('',(#64627,#64628,#64629,#64630));
#15558=EDGE_LOOP('',(#64631,#64632,#64633,#64634));
#15559=EDGE_LOOP('',(#64635,#64636,#64637,#64638));
#15560=EDGE_LOOP('',(#64639,#64640,#64641,#64642));
#15561=EDGE_LOOP('',(#64643,#64644,#64645,#64646));
#15562=EDGE_LOOP('',(#64647,#64648,#64649,#64650));
#15563=EDGE_LOOP('',(#64651,#64652,#64653,#64654));
#15564=EDGE_LOOP('',(#64655,#64656,#64657,#64658));
#15565=EDGE_LOOP('',(#64659,#64660,#64661,#64662));
#15566=EDGE_LOOP('',(#64663,#64664,#64665,#64666));
#15567=EDGE_LOOP('',(#64667,#64668,#64669,#64670));
#15568=EDGE_LOOP('',(#64671,#64672,#64673,#64674));
#15569=EDGE_LOOP('',(#64675,#64676,#64677,#64678));
#15570=EDGE_LOOP('',(#64679,#64680,#64681,#64682));
#15571=EDGE_LOOP('',(#64683,#64684,#64685,#64686));
#15572=EDGE_LOOP('',(#64687,#64688,#64689,#64690));
#15573=EDGE_LOOP('',(#64691,#64692,#64693,#64694));
#15574=EDGE_LOOP('',(#64695,#64696,#64697,#64698));
#15575=EDGE_LOOP('',(#64699,#64700,#64701,#64702));
#15576=EDGE_LOOP('',(#64703,#64704,#64705,#64706));
#15577=EDGE_LOOP('',(#64707,#64708,#64709,#64710));
#15578=EDGE_LOOP('',(#64711,#64712,#64713,#64714));
#15579=EDGE_LOOP('',(#64715,#64716,#64717,#64718));
#15580=EDGE_LOOP('',(#64719,#64720,#64721,#64722));
#15581=EDGE_LOOP('',(#64723,#64724,#64725,#64726));
#15582=EDGE_LOOP('',(#64727,#64728,#64729,#64730));
#15583=EDGE_LOOP('',(#64731,#64732,#64733,#64734));
#15584=EDGE_LOOP('',(#64735,#64736,#64737,#64738));
#15585=EDGE_LOOP('',(#64739,#64740,#64741,#64742));
#15586=EDGE_LOOP('',(#64743,#64744,#64745,#64746));
#15587=EDGE_LOOP('',(#64747,#64748,#64749,#64750));
#15588=EDGE_LOOP('',(#64751,#64752,#64753,#64754));
#15589=EDGE_LOOP('',(#64755,#64756,#64757,#64758));
#15590=EDGE_LOOP('',(#64759,#64760,#64761,#64762));
#15591=EDGE_LOOP('',(#64763,#64764,#64765,#64766));
#15592=EDGE_LOOP('',(#64767,#64768,#64769,#64770));
#15593=EDGE_LOOP('',(#64771,#64772,#64773,#64774));
#15594=EDGE_LOOP('',(#64775,#64776,#64777,#64778));
#15595=EDGE_LOOP('',(#64779,#64780,#64781,#64782));
#15596=EDGE_LOOP('',(#64783,#64784,#64785,#64786));
#15597=EDGE_LOOP('',(#64787,#64788,#64789,#64790));
#15598=EDGE_LOOP('',(#64791,#64792,#64793,#64794));
#15599=EDGE_LOOP('',(#64795,#64796,#64797,#64798));
#15600=EDGE_LOOP('',(#64799,#64800,#64801,#64802));
#15601=EDGE_LOOP('',(#64803,#64804,#64805,#64806));
#15602=EDGE_LOOP('',(#64807,#64808,#64809,#64810));
#15603=EDGE_LOOP('',(#64811,#64812,#64813,#64814));
#15604=EDGE_LOOP('',(#64815,#64816,#64817,#64818));
#15605=EDGE_LOOP('',(#64819,#64820,#64821,#64822));
#15606=EDGE_LOOP('',(#64823,#64824,#64825,#64826));
#15607=EDGE_LOOP('',(#64827,#64828,#64829,#64830));
#15608=EDGE_LOOP('',(#64831,#64832,#64833,#64834));
#15609=EDGE_LOOP('',(#64835,#64836,#64837,#64838));
#15610=EDGE_LOOP('',(#64839,#64840,#64841,#64842));
#15611=EDGE_LOOP('',(#64843,#64844,#64845,#64846));
#15612=EDGE_LOOP('',(#64847,#64848,#64849,#64850));
#15613=EDGE_LOOP('',(#64851,#64852,#64853,#64854));
#15614=EDGE_LOOP('',(#64855,#64856,#64857,#64858));
#15615=EDGE_LOOP('',(#64859,#64860,#64861,#64862));
#15616=EDGE_LOOP('',(#64863,#64864,#64865,#64866));
#15617=EDGE_LOOP('',(#64867,#64868,#64869,#64870));
#15618=EDGE_LOOP('',(#64871,#64872,#64873,#64874));
#15619=EDGE_LOOP('',(#64875,#64876,#64877,#64878));
#15620=EDGE_LOOP('',(#64879,#64880,#64881,#64882));
#15621=EDGE_LOOP('',(#64883,#64884,#64885,#64886));
#15622=EDGE_LOOP('',(#64887,#64888,#64889,#64890));
#15623=EDGE_LOOP('',(#64891,#64892,#64893,#64894));
#15624=EDGE_LOOP('',(#64895,#64896,#64897,#64898));
#15625=EDGE_LOOP('',(#64899,#64900,#64901,#64902));
#15626=EDGE_LOOP('',(#64903,#64904,#64905,#64906));
#15627=EDGE_LOOP('',(#64907,#64908,#64909,#64910));
#15628=EDGE_LOOP('',(#64911,#64912,#64913,#64914));
#15629=EDGE_LOOP('',(#64915,#64916,#64917,#64918));
#15630=EDGE_LOOP('',(#64919,#64920,#64921,#64922));
#15631=EDGE_LOOP('',(#64923,#64924,#64925,#64926));
#15632=EDGE_LOOP('',(#64927,#64928,#64929,#64930));
#15633=EDGE_LOOP('',(#64931,#64932,#64933,#64934));
#15634=EDGE_LOOP('',(#64935,#64936,#64937,#64938));
#15635=EDGE_LOOP('',(#64939,#64940,#64941,#64942));
#15636=EDGE_LOOP('',(#64943,#64944,#64945,#64946));
#15637=EDGE_LOOP('',(#64947,#64948,#64949,#64950));
#15638=EDGE_LOOP('',(#64951,#64952,#64953,#64954));
#15639=EDGE_LOOP('',(#64955,#64956,#64957,#64958));
#15640=EDGE_LOOP('',(#64959,#64960,#64961,#64962));
#15641=EDGE_LOOP('',(#64963,#64964,#64965,#64966));
#15642=EDGE_LOOP('',(#64967,#64968,#64969,#64970));
#15643=EDGE_LOOP('',(#64971,#64972,#64973,#64974));
#15644=EDGE_LOOP('',(#64975,#64976,#64977,#64978));
#15645=EDGE_LOOP('',(#64979,#64980,#64981,#64982));
#15646=EDGE_LOOP('',(#64983,#64984,#64985,#64986));
#15647=EDGE_LOOP('',(#64987,#64988,#64989,#64990));
#15648=EDGE_LOOP('',(#64991,#64992,#64993,#64994));
#15649=EDGE_LOOP('',(#64995,#64996,#64997,#64998));
#15650=EDGE_LOOP('',(#64999,#65000,#65001,#65002));
#15651=EDGE_LOOP('',(#65003,#65004,#65005,#65006));
#15652=EDGE_LOOP('',(#65007,#65008,#65009,#65010));
#15653=EDGE_LOOP('',(#65011,#65012,#65013,#65014));
#15654=EDGE_LOOP('',(#65015,#65016,#65017,#65018));
#15655=EDGE_LOOP('',(#65019,#65020,#65021,#65022));
#15656=EDGE_LOOP('',(#65023,#65024,#65025,#65026));
#15657=EDGE_LOOP('',(#65027,#65028,#65029,#65030));
#15658=EDGE_LOOP('',(#65031,#65032,#65033,#65034));
#15659=EDGE_LOOP('',(#65035,#65036,#65037,#65038));
#15660=EDGE_LOOP('',(#65039,#65040,#65041,#65042));
#15661=EDGE_LOOP('',(#65043,#65044,#65045,#65046));
#15662=EDGE_LOOP('',(#65047,#65048,#65049,#65050));
#15663=EDGE_LOOP('',(#65051,#65052,#65053,#65054));
#15664=EDGE_LOOP('',(#65055,#65056,#65057,#65058));
#15665=EDGE_LOOP('',(#65059,#65060,#65061,#65062));
#15666=EDGE_LOOP('',(#65063,#65064,#65065,#65066));
#15667=EDGE_LOOP('',(#65067,#65068,#65069,#65070));
#15668=EDGE_LOOP('',(#65071,#65072,#65073,#65074));
#15669=EDGE_LOOP('',(#65075,#65076,#65077,#65078));
#15670=EDGE_LOOP('',(#65079,#65080,#65081,#65082));
#15671=EDGE_LOOP('',(#65083,#65084,#65085,#65086));
#15672=EDGE_LOOP('',(#65087,#65088,#65089,#65090));
#15673=EDGE_LOOP('',(#65091,#65092,#65093,#65094));
#15674=EDGE_LOOP('',(#65095));
#15675=EDGE_LOOP('',(#65096));
#15676=EDGE_LOOP('',(#65097,#65098,#65099,#65100));
#15677=EDGE_LOOP('',(#65101,#65102,#65103));
#15678=EDGE_LOOP('',(#65104,#65105,#65106));
#15679=EDGE_LOOP('',(#65107,#65108,#65109));
#15680=EDGE_LOOP('',(#65110,#65111,#65112));
#15681=EDGE_LOOP('',(#65113,#65114,#65115,#65116));
#15682=EDGE_LOOP('',(#65117,#65118,#65119,#65120));
#15683=EDGE_LOOP('',(#65121,#65122,#65123));
#15684=EDGE_LOOP('',(#65124,#65125,#65126));
#15685=EDGE_LOOP('',(#65127,#65128,#65129));
#15686=EDGE_LOOP('',(#65130,#65131,#65132));
#15687=EDGE_LOOP('',(#65133,#65134,#65135,#65136));
#15688=EDGE_LOOP('',(#65137,#65138,#65139,#65140));
#15689=EDGE_LOOP('',(#65141,#65142,#65143));
#15690=EDGE_LOOP('',(#65144,#65145,#65146));
#15691=EDGE_LOOP('',(#65147,#65148,#65149));
#15692=EDGE_LOOP('',(#65150,#65151,#65152));
#15693=EDGE_LOOP('',(#65153,#65154,#65155,#65156));
#15694=EDGE_LOOP('',(#65157,#65158,#65159,#65160));
#15695=EDGE_LOOP('',(#65161,#65162,#65163));
#15696=EDGE_LOOP('',(#65164,#65165,#65166));
#15697=EDGE_LOOP('',(#65167,#65168,#65169));
#15698=EDGE_LOOP('',(#65170,#65171,#65172));
#15699=EDGE_LOOP('',(#65173,#65174,#65175,#65176));
#15700=EDGE_LOOP('',(#65177,#65178,#65179,#65180));
#15701=EDGE_LOOP('',(#65181,#65182,#65183));
#15702=EDGE_LOOP('',(#65184,#65185,#65186));
#15703=EDGE_LOOP('',(#65187,#65188,#65189));
#15704=EDGE_LOOP('',(#65190,#65191,#65192));
#15705=EDGE_LOOP('',(#65193,#65194,#65195,#65196));
#15706=EDGE_LOOP('',(#65197,#65198,#65199,#65200));
#15707=EDGE_LOOP('',(#65201,#65202,#65203));
#15708=EDGE_LOOP('',(#65204,#65205,#65206));
#15709=EDGE_LOOP('',(#65207,#65208,#65209));
#15710=EDGE_LOOP('',(#65210,#65211,#65212));
#15711=EDGE_LOOP('',(#65213,#65214,#65215,#65216));
#15712=EDGE_LOOP('',(#65217,#65218,#65219,#65220));
#15713=EDGE_LOOP('',(#65221,#65222,#65223));
#15714=EDGE_LOOP('',(#65224,#65225,#65226));
#15715=EDGE_LOOP('',(#65227,#65228,#65229));
#15716=EDGE_LOOP('',(#65230,#65231,#65232));
#15717=EDGE_LOOP('',(#65233,#65234,#65235,#65236));
#15718=EDGE_LOOP('',(#65237,#65238,#65239,#65240));
#15719=EDGE_LOOP('',(#65241,#65242,#65243));
#15720=EDGE_LOOP('',(#65244,#65245,#65246));
#15721=EDGE_LOOP('',(#65247,#65248,#65249));
#15722=EDGE_LOOP('',(#65250,#65251,#65252));
#15723=EDGE_LOOP('',(#65253,#65254,#65255,#65256));
#15724=EDGE_LOOP('',(#65257,#65258,#65259,#65260));
#15725=EDGE_LOOP('',(#65261,#65262,#65263));
#15726=EDGE_LOOP('',(#65264,#65265,#65266));
#15727=EDGE_LOOP('',(#65267,#65268,#65269));
#15728=EDGE_LOOP('',(#65270,#65271,#65272));
#15729=EDGE_LOOP('',(#65273,#65274,#65275,#65276));
#15730=EDGE_LOOP('',(#65277,#65278,#65279,#65280));
#15731=EDGE_LOOP('',(#65281,#65282,#65283));
#15732=EDGE_LOOP('',(#65284,#65285,#65286));
#15733=EDGE_LOOP('',(#65287,#65288,#65289));
#15734=EDGE_LOOP('',(#65290,#65291,#65292));
#15735=EDGE_LOOP('',(#65293,#65294,#65295,#65296));
#15736=EDGE_LOOP('',(#65297,#65298,#65299,#65300));
#15737=EDGE_LOOP('',(#65301,#65302,#65303));
#15738=EDGE_LOOP('',(#65304,#65305,#65306));
#15739=EDGE_LOOP('',(#65307,#65308,#65309));
#15740=EDGE_LOOP('',(#65310,#65311,#65312));
#15741=EDGE_LOOP('',(#65313,#65314,#65315,#65316));
#15742=EDGE_LOOP('',(#65317,#65318,#65319,#65320));
#15743=EDGE_LOOP('',(#65321,#65322,#65323));
#15744=EDGE_LOOP('',(#65324,#65325,#65326));
#15745=EDGE_LOOP('',(#65327,#65328,#65329));
#15746=EDGE_LOOP('',(#65330,#65331,#65332));
#15747=EDGE_LOOP('',(#65333,#65334,#65335,#65336));
#15748=EDGE_LOOP('',(#65337,#65338,#65339,#65340));
#15749=EDGE_LOOP('',(#65341,#65342,#65343));
#15750=EDGE_LOOP('',(#65344,#65345,#65346));
#15751=EDGE_LOOP('',(#65347,#65348,#65349));
#15752=EDGE_LOOP('',(#65350,#65351,#65352));
#15753=EDGE_LOOP('',(#65353,#65354,#65355,#65356));
#15754=EDGE_LOOP('',(#65357,#65358,#65359,#65360));
#15755=EDGE_LOOP('',(#65361,#65362,#65363));
#15756=EDGE_LOOP('',(#65364,#65365,#65366));
#15757=EDGE_LOOP('',(#65367,#65368,#65369));
#15758=EDGE_LOOP('',(#65370,#65371,#65372));
#15759=EDGE_LOOP('',(#65373,#65374,#65375,#65376));
#15760=EDGE_LOOP('',(#65377,#65378,#65379,#65380,#65381));
#15761=EDGE_LOOP('',(#65382,#65383,#65384,#65385));
#15762=EDGE_LOOP('',(#65386,#65387,#65388,#65389));
#15763=EDGE_LOOP('',(#65390,#65391,#65392));
#15764=EDGE_LOOP('',(#65393,#65394,#65395));
#15765=EDGE_LOOP('',(#65396,#65397,#65398,#65399));
#15766=EDGE_LOOP('',(#65400,#65401,#65402,#65403));
#15767=EDGE_LOOP('',(#65404,#65405,#65406));
#15768=EDGE_LOOP('',(#65407,#65408,#65409));
#15769=EDGE_LOOP('',(#65410,#65411,#65412));
#15770=EDGE_LOOP('',(#65413,#65414,#65415));
#15771=EDGE_LOOP('',(#65416,#65417,#65418,#65419));
#15772=EDGE_LOOP('',(#65420,#65421,#65422,#65423));
#15773=EDGE_LOOP('',(#65424,#65425,#65426));
#15774=EDGE_LOOP('',(#65427,#65428,#65429));
#15775=EDGE_LOOP('',(#65430,#65431,#65432));
#15776=EDGE_LOOP('',(#65433,#65434,#65435));
#15777=EDGE_LOOP('',(#65436,#65437,#65438,#65439));
#15778=EDGE_LOOP('',(#65440,#65441,#65442,#65443));
#15779=EDGE_LOOP('',(#65444,#65445,#65446));
#15780=EDGE_LOOP('',(#65447,#65448,#65449));
#15781=EDGE_LOOP('',(#65450,#65451,#65452));
#15782=EDGE_LOOP('',(#65453,#65454,#65455));
#15783=EDGE_LOOP('',(#65456,#65457,#65458,#65459));
#15784=EDGE_LOOP('',(#65460,#65461,#65462,#65463));
#15785=EDGE_LOOP('',(#65464,#65465,#65466));
#15786=EDGE_LOOP('',(#65467,#65468,#65469));
#15787=EDGE_LOOP('',(#65470,#65471,#65472));
#15788=EDGE_LOOP('',(#65473,#65474,#65475));
#15789=EDGE_LOOP('',(#65476,#65477,#65478,#65479));
#15790=EDGE_LOOP('',(#65480,#65481,#65482,#65483));
#15791=EDGE_LOOP('',(#65484,#65485,#65486));
#15792=EDGE_LOOP('',(#65487,#65488,#65489));
#15793=EDGE_LOOP('',(#65490,#65491,#65492));
#15794=EDGE_LOOP('',(#65493,#65494,#65495));
#15795=EDGE_LOOP('',(#65496,#65497,#65498,#65499));
#15796=EDGE_LOOP('',(#65500,#65501,#65502,#65503));
#15797=EDGE_LOOP('',(#65504,#65505,#65506));
#15798=EDGE_LOOP('',(#65507,#65508,#65509));
#15799=EDGE_LOOP('',(#65510,#65511,#65512));
#15800=EDGE_LOOP('',(#65513,#65514,#65515));
#15801=EDGE_LOOP('',(#65516,#65517,#65518,#65519));
#15802=EDGE_LOOP('',(#65520,#65521,#65522,#65523));
#15803=EDGE_LOOP('',(#65524,#65525,#65526));
#15804=EDGE_LOOP('',(#65527,#65528,#65529));
#15805=EDGE_LOOP('',(#65530,#65531,#65532));
#15806=EDGE_LOOP('',(#65533,#65534,#65535));
#15807=EDGE_LOOP('',(#65536,#65537,#65538,#65539));
#15808=EDGE_LOOP('',(#65540,#65541,#65542,#65543));
#15809=EDGE_LOOP('',(#65544,#65545,#65546));
#15810=EDGE_LOOP('',(#65547,#65548,#65549));
#15811=EDGE_LOOP('',(#65550,#65551,#65552));
#15812=EDGE_LOOP('',(#65553,#65554,#65555));
#15813=EDGE_LOOP('',(#65556,#65557,#65558,#65559));
#15814=EDGE_LOOP('',(#65560,#65561,#65562,#65563));
#15815=EDGE_LOOP('',(#65564,#65565,#65566));
#15816=EDGE_LOOP('',(#65567,#65568,#65569));
#15817=EDGE_LOOP('',(#65570,#65571,#65572));
#15818=EDGE_LOOP('',(#65573,#65574,#65575));
#15819=EDGE_LOOP('',(#65576,#65577,#65578,#65579));
#15820=EDGE_LOOP('',(#65580,#65581,#65582,#65583));
#15821=EDGE_LOOP('',(#65584,#65585,#65586));
#15822=EDGE_LOOP('',(#65587,#65588,#65589));
#15823=EDGE_LOOP('',(#65590,#65591,#65592));
#15824=EDGE_LOOP('',(#65593,#65594,#65595));
#15825=EDGE_LOOP('',(#65596,#65597,#65598,#65599));
#15826=EDGE_LOOP('',(#65600,#65601,#65602,#65603));
#15827=EDGE_LOOP('',(#65604,#65605,#65606));
#15828=EDGE_LOOP('',(#65607,#65608,#65609));
#15829=EDGE_LOOP('',(#65610,#65611,#65612));
#15830=EDGE_LOOP('',(#65613,#65614,#65615));
#15831=EDGE_LOOP('',(#65616,#65617,#65618,#65619));
#15832=EDGE_LOOP('',(#65620,#65621,#65622,#65623));
#15833=EDGE_LOOP('',(#65624,#65625,#65626));
#15834=EDGE_LOOP('',(#65627,#65628,#65629));
#15835=EDGE_LOOP('',(#65630,#65631,#65632));
#15836=EDGE_LOOP('',(#65633,#65634,#65635));
#15837=EDGE_LOOP('',(#65636,#65637,#65638,#65639));
#15838=EDGE_LOOP('',(#65640,#65641,#65642,#65643));
#15839=EDGE_LOOP('',(#65644,#65645,#65646));
#15840=EDGE_LOOP('',(#65647,#65648,#65649));
#15841=EDGE_LOOP('',(#65650,#65651,#65652));
#15842=EDGE_LOOP('',(#65653,#65654,#65655));
#15843=EDGE_LOOP('',(#65656,#65657,#65658,#65659));
#15844=EDGE_LOOP('',(#65660,#65661,#65662,#65663));
#15845=EDGE_LOOP('',(#65664,#65665,#65666));
#15846=EDGE_LOOP('',(#65667,#65668,#65669));
#15847=EDGE_LOOP('',(#65670,#65671,#65672));
#15848=EDGE_LOOP('',(#65673,#65674,#65675));
#15849=EDGE_LOOP('',(#65676,#65677,#65678,#65679));
#15850=EDGE_LOOP('',(#65680));
#15851=EDGE_LOOP('',(#65681));
#15852=EDGE_LOOP('',(#65682));
#15853=EDGE_LOOP('',(#65683));
#15854=EDGE_LOOP('',(#65684,#65685,#65686,#65687));
#15855=EDGE_LOOP('',(#65688,#65689,#65690,#65691,#65692,#65693,#65694,#65695,
#65696,#65697,#65698,#65699,#65700,#65701,#65702,#65703));
#15856=EDGE_LOOP('',(#65704,#65705,#65706,#65707,#65708));
#15857=EDGE_LOOP('',(#65709,#65710,#65711,#65712,#65713,#65714,#65715,#65716));
#15858=EDGE_LOOP('',(#65717,#65718,#65719,#65720,#65721));
#15859=EDGE_LOOP('',(#65722,#65723,#65724,#65725));
#15860=EDGE_LOOP('',(#65726,#65727,#65728,#65729,#65730,#65731,#65732,#65733));
#15861=EDGE_LOOP('',(#65734));
#15862=EDGE_LOOP('',(#65735));
#15863=EDGE_LOOP('',(#65736));
#15864=EDGE_LOOP('',(#65737));
#15865=EDGE_LOOP('',(#65738,#65739,#65740,#65741));
#15866=EDGE_LOOP('',(#65742,#65743,#65744,#65745,#65746,#65747,#65748,#65749,
#65750));
#15867=EDGE_LOOP('',(#65751,#65752,#65753,#65754));
#15868=EDGE_LOOP('',(#65755,#65756,#65757,#65758));
#15869=EDGE_LOOP('',(#65759,#65760));
#15870=EDGE_LOOP('',(#65761,#65762,#65763));
#15871=EDGE_LOOP('',(#65764,#65765,#65766,#65767));
#15872=EDGE_LOOP('',(#65768,#65769,#65770,#65771));
#15873=EDGE_LOOP('',(#65772,#65773,#65774));
#15874=EDGE_LOOP('',(#65775,#65776,#65777));
#15875=EDGE_LOOP('',(#65778,#65779,#65780,#65781,#65782));
#15876=EDGE_LOOP('',(#65783,#65784,#65785,#65786));
#15877=EDGE_LOOP('',(#65787,#65788,#65789,#65790));
#15878=EDGE_LOOP('',(#65791,#65792,#65793,#65794));
#15879=EDGE_LOOP('',(#65795,#65796,#65797,#65798,#65799));
#15880=EDGE_LOOP('',(#65800,#65801,#65802,#65803,#65804,#65805,#65806,#65807));
#15881=EDGE_LOOP('',(#65808,#65809,#65810,#65811,#65812,#65813));
#15882=EDGE_LOOP('',(#65814,#65815,#65816,#65817));
#15883=EDGE_LOOP('',(#65818,#65819,#65820,#65821));
#15884=EDGE_LOOP('',(#65822,#65823,#65824,#65825));
#15885=EDGE_LOOP('',(#65826,#65827,#65828,#65829,#65830,#65831));
#15886=EDGE_LOOP('',(#65832,#65833,#65834,#65835));
#15887=EDGE_LOOP('',(#65836,#65837,#65838,#65839));
#15888=EDGE_LOOP('',(#65840,#65841,#65842,#65843));
#15889=EDGE_LOOP('',(#65844,#65845,#65846,#65847));
#15890=EDGE_LOOP('',(#65848,#65849,#65850,#65851));
#15891=EDGE_LOOP('',(#65852,#65853,#65854,#65855));
#15892=EDGE_LOOP('',(#65856,#65857,#65858,#65859));
#15893=EDGE_LOOP('',(#65860));
#15894=EDGE_LOOP('',(#65861,#65862,#65863,#65864,#65865,#65866,#65867,#65868,
#65869,#65870,#65871));
#15895=EDGE_LOOP('',(#65872));
#15896=EDGE_LOOP('',(#65873,#65874,#65875,#65876,#65877,#65878,#65879,#65880,
#65881,#65882,#65883));
#15897=EDGE_LOOP('',(#65884));
#15898=EDGE_LOOP('',(#65885,#65886,#65887,#65888,#65889,#65890,#65891,#65892));
#15899=EDGE_LOOP('',(#65893,#65894,#65895,#65896));
#15900=EDGE_LOOP('',(#65897,#65898,#65899,#65900));
#15901=EDGE_LOOP('',(#65901));
#15902=EDGE_LOOP('',(#65902,#65903,#65904,#65905,#65906,#65907,#65908,#65909,
#65910));
#15903=EDGE_LOOP('',(#65911,#65912));
#15904=EDGE_LOOP('',(#65913,#65914,#65915,#65916,#65917));
#15905=EDGE_LOOP('',(#65918));
#15906=EDGE_LOOP('',(#65919,#65920,#65921,#65922,#65923,#65924,#65925,#65926,
#65927,#65928,#65929,#65930,#65931));
#15907=EDGE_LOOP('',(#65932,#65933,#65934,#65935));
#15908=EDGE_LOOP('',(#65936,#65937,#65938,#65939,#65940));
#15909=EDGE_LOOP('',(#65941,#65942,#65943,#65944,#65945));
#15910=EDGE_LOOP('',(#65946));
#15911=EDGE_LOOP('',(#65947));
#15912=EDGE_LOOP('',(#65948,#65949));
#15913=EDGE_LOOP('',(#65950,#65951));
#15914=EDGE_LOOP('',(#65952,#65953,#65954,#65955,#65956,#65957));
#15915=EDGE_LOOP('',(#65958,#65959,#65960,#65961));
#15916=EDGE_LOOP('',(#65962));
#15917=EDGE_LOOP('',(#65963,#65964,#65965,#65966));
#15918=EDGE_LOOP('',(#65967));
#15919=EDGE_LOOP('',(#65968,#65969,#65970,#65971,#65972,#65973,#65974,#65975,
#65976,#65977));
#15920=EDGE_LOOP('',(#65978,#65979));
#15921=EDGE_LOOP('',(#65980,#65981,#65982,#65983));
#15922=EDGE_LOOP('',(#65984,#65985,#65986,#65987,#65988));
#15923=EDGE_LOOP('',(#65989));
#15924=EDGE_LOOP('',(#65990));
#15925=EDGE_LOOP('',(#65991,#65992,#65993,#65994,#65995,#65996,#65997));
#15926=EDGE_LOOP('',(#65998,#65999,#66000,#66001));
#15927=EDGE_LOOP('',(#66002));
#15928=EDGE_LOOP('',(#66003));
#15929=CIRCLE('',#71474,7.06860568617886);
#15930=CIRCLE('',#71475,7.33422742101415);
#15931=CIRCLE('',#71476,7.06860448235925);
#15932=CIRCLE('',#71477,7.33422663168221);
#15933=CIRCLE('',#71478,7.06860281197277);
#15934=CIRCLE('',#71479,7.3342250351839);
#15935=CIRCLE('',#71480,7.06860459613159);
#15936=CIRCLE('',#71481,7.33422732999641);
#15937=CIRCLE('',#71482,7.06860394071194);
#15938=CIRCLE('',#71483,7.33422671536983);
#15939=CIRCLE('',#71484,7.0686060491576);
#15940=CIRCLE('',#71485,7.33422717282189);
#15941=CIRCLE('',#71486,7.06860489976384);
#15942=CIRCLE('',#71487,7.33422669740432);
#15943=CIRCLE('',#71488,7.06860638429797);
#15944=CIRCLE('',#71489,7.33422795178459);
#15945=CIRCLE('',#71490,7.06860552820924);
#15946=CIRCLE('',#71491,7.33422734233105);
#15947=CIRCLE('',#71492,7.06860556698004);
#15948=CIRCLE('',#71493,7.3342273785942);
#15949=CIRCLE('',#71494,7.06860632435079);
#15950=CIRCLE('',#71495,7.33422770117462);
#15951=CIRCLE('',#71496,7.06860456983854);
#15952=CIRCLE('',#71497,7.33422661758376);
#15953=CIRCLE('',#71498,7.06860572631863);
#15954=CIRCLE('',#71499,7.33422765525036);
#15955=CIRCLE('',#71500,7.06860502971023);
#15956=CIRCLE('',#71501,7.33422693890404);
#15957=CIRCLE('',#71502,7.06860404038351);
#15958=CIRCLE('',#71503,7.33422645405152);
#15959=CIRCLE('',#71504,7.06860678325798);
#15960=CIRCLE('',#71505,7.33422776502736);
#15961=CIRCLE('',#71506,7.0686056226588);
#15962=CIRCLE('',#71507,7.33422778643665);
#15963=CIRCLE('',#71508,7.0686072750088);
#15964=CIRCLE('',#71509,7.33422787644434);
#15965=CIRCLE('',#71510,7.06860627067123);
#15966=CIRCLE('',#71511,7.3342277579675);
#15967=CIRCLE('',#71512,7.06860326789228);
#15968=CIRCLE('',#71513,7.33422642819733);
#15969=CIRCLE('',#71514,7.0686053869475);
#15970=CIRCLE('',#71515,7.33422736323035);
#15971=CIRCLE('',#71516,7.06860674407459);
#15972=CIRCLE('',#71517,7.33422795034231);
#15973=CIRCLE('',#71518,7.06860600194252);
#15974=CIRCLE('',#71519,7.33422781452826);
#15975=CIRCLE('',#71520,7.06860366903633);
#15976=CIRCLE('',#71521,7.33422629778949);
#15977=CIRCLE('',#71522,7.06860610926342);
#15978=CIRCLE('',#71523,7.33422735913368);
#15979=CIRCLE('',#71524,7.06860368230427);
#15980=CIRCLE('',#71525,7.33422671614766);
#15981=CIRCLE('',#71526,7.06860444583504);
#15982=CIRCLE('',#71527,7.33422706459965);
#15983=CIRCLE('',#71528,7.06860456725667);
#15984=CIRCLE('',#71529,7.33422708330648);
#15985=CIRCLE('',#71530,7.06860367611818);
#15986=CIRCLE('',#71531,7.33422714254166);
#15987=CIRCLE('',#71532,6.75);
#15988=CIRCLE('',#71534,3.25);
#15989=CIRCLE('',#71535,3.25);
#15990=CIRCLE('',#71538,7.);
#15991=CIRCLE('',#71539,7.);
#15992=CIRCLE('',#71541,6.125);
#15993=CIRCLE('',#71542,6.125);
#15994=CIRCLE('',#71543,6.125);
#15995=CIRCLE('',#71545,6.425);
#15996=CIRCLE('',#71547,7.33422710637909);
#15997=CIRCLE('',#71548,7.06860836336948);
#15998=CIRCLE('',#71549,7.33422732564574);
#15999=CIRCLE('',#71550,7.06860903695343);
#16000=CIRCLE('',#71551,7.33422702882346);
#16001=CIRCLE('',#71552,7.06860901744208);
#16002=CIRCLE('',#71553,7.3342266652849);
#16003=CIRCLE('',#71554,7.06860850262219);
#16004=CIRCLE('',#71555,7.33422732891954);
#16005=CIRCLE('',#71556,7.06860961375978);
#16006=CIRCLE('',#71557,7.33422624237877);
#16007=CIRCLE('',#71558,7.06860708111272);
#16008=CIRCLE('',#71559,7.33422780073948);
#16009=CIRCLE('',#71560,7.06861064290494);
#16010=CIRCLE('',#71561,7.33422793495388);
#16011=CIRCLE('',#71562,7.0686098556057);
#16012=CIRCLE('',#71563,7.33422761064981);
#16013=CIRCLE('',#71564,7.06861003408136);
#16014=CIRCLE('',#71565,7.33422637344204);
#16015=CIRCLE('',#71566,7.06860802586876);
#16016=CIRCLE('',#71567,7.33422773665016);
#16017=CIRCLE('',#71568,7.06861056875248);
#16018=CIRCLE('',#71569,7.3342281502456);
#16019=CIRCLE('',#71570,7.06861172275373);
#16020=CIRCLE('',#71571,7.33422777311646);
#16021=CIRCLE('',#71572,7.06861072746278);
#16022=CIRCLE('',#71573,7.33422774759614);
#16023=CIRCLE('',#71574,7.06861069549746);
#16024=CIRCLE('',#71575,7.33422668479825);
#16025=CIRCLE('',#71576,7.06860648295125);
#16026=CIRCLE('',#71577,6.75);
#16027=CIRCLE('',#71578,7.33422546202569);
#16028=CIRCLE('',#71579,7.06860901630615);
#16029=CIRCLE('',#71580,7.33422758661738);
#16030=CIRCLE('',#71581,7.06860917719902);
#16031=CIRCLE('',#71582,7.33422552125982);
#16032=CIRCLE('',#71583,7.06860817918064);
#16033=CIRCLE('',#71584,7.33422791354406);
#16034=CIRCLE('',#71585,7.06861114651049);
#16035=CIRCLE('',#71586,7.33422729522531);
#16036=CIRCLE('',#71587,7.06860906896761);
#16037=CIRCLE('',#71588,7.33422754578351);
#16038=CIRCLE('',#71589,7.06860992934319);
#16039=CIRCLE('',#71590,7.33422816391154);
#16040=CIRCLE('',#71591,7.06861129437419);
#16041=CIRCLE('',#71592,7.33422524915925);
#16042=CIRCLE('',#71593,7.06860889389819);
#16043=CIRCLE('',#71594,7.33422708826522);
#16044=CIRCLE('',#71595,7.06860930316695);
#16045=CIRCLE('',#71596,7.33422690268295);
#16046=CIRCLE('',#71597,7.06860890902957);
#16047=CIRCLE('',#71598,7.33422725159127);
#16048=CIRCLE('',#71599,7.06860891185296);
#16049=CIRCLE('',#71600,7.33422516944886);
#16050=CIRCLE('',#71601,7.06860779698365);
#16051=CIRCLE('',#71602,7.33422681347524);
#16052=CIRCLE('',#71603,7.06860860032496);
#16053=CIRCLE('',#71604,7.33422734754571);
#16054=CIRCLE('',#71605,7.06861007792251);
#16055=CIRCLE('',#71607,7.65641797830405);
#16056=CIRCLE('',#71608,7.74391301990334);
#16057=CIRCLE('',#71610,7.74376760109424);
#16058=CIRCLE('',#71612,7.69259377819036);
#16059=CIRCLE('',#71613,7.68762408392115);
#16060=CIRCLE('',#71614,7.50000000109902);
#16061=CIRCLE('',#71615,7.69302971312151);
#16062=CIRCLE('',#71617,7.69146686117127);
#16063=CIRCLE('',#71618,7.69282866600189);
#16064=CIRCLE('',#71620,7.65227963154115);
#16065=CIRCLE('',#71622,7.65227968597654);
#16066=CIRCLE('',#71624,7.68301219447606);
#16067=CIRCLE('',#71625,7.69191399109765);
#16068=CIRCLE('',#71627,7.4999999993286);
#16069=CIRCLE('',#71628,7.6876252604557);
#16070=CIRCLE('',#71629,7.6925870430687);
#16071=CIRCLE('',#71630,7.6930268168054);
#16072=CIRCLE('',#71632,7.82251869020954);
#16073=CIRCLE('',#71634,7.68619221526501);
#16074=CIRCLE('',#71636,7.69282870015808);
#16075=CIRCLE('',#71637,7.69146686065975);
#16076=CIRCLE('',#71639,7.6929092573408);
#16077=CIRCLE('',#71640,7.6851083393197);
#16078=CIRCLE('',#71642,7.69191399110767);
#16079=CIRCLE('',#71643,7.68301221228793);
#16080=CIRCLE('',#71645,7.69207568232512);
#16081=CIRCLE('',#71646,7.69297980315297);
#16082=CIRCLE('',#71648,7.68619221509267);
#16083=CIRCLE('',#71650,7.69242170452788);
#16084=CIRCLE('',#71652,7.68475592667959);
#16085=CIRCLE('',#71654,7.69297983680142);
#16086=CIRCLE('',#71655,7.6920756821004);
#16087=CIRCLE('',#71657,7.69301888945012);
#16088=CIRCLE('',#71658,7.68356129670636);
#16089=CIRCLE('',#71660,7.69242170506121);
#16090=CIRCLE('',#71662,7.69254650683266);
#16091=CIRCLE('',#71663,7.69306084204855);
#16092=CIRCLE('',#71665,7.68475592668143);
#16093=CIRCLE('',#71667,7.69279341210589);
#16094=CIRCLE('',#71669,7.68355912148237);
#16095=CIRCLE('',#71670,7.69301686910343);
#16096=CIRCLE('',#71672,7.68318440412029);
#16097=CIRCLE('',#71674,7.69306086163512);
#16098=CIRCLE('',#71675,7.69254650650468);
#16099=CIRCLE('',#71677,7.6930586350727);
#16100=CIRCLE('',#71679,7.69287888052477);
#16101=CIRCLE('',#71680,7.69291157795238);
#16102=CIRCLE('',#71682,7.68318440411841);
#16103=CIRCLE('',#71684,7.69302871560608);
#16104=CIRCLE('',#71686,7.69305436245181);
#16105=CIRCLE('',#71689,7.69291157795224);
#16106=CIRCLE('',#71690,7.69287888052691);
#16107=CIRCLE('',#71692,7.69302871457533);
#16108=CIRCLE('',#71693,7.6876542201912);
#16109=CIRCLE('',#71694,7.44531753045275);
#16110=CIRCLE('',#71695,7.69302855940779);
#16111=CIRCLE('',#71696,7.44956381440377);
#16112=CIRCLE('',#71698,7.69059190152309);
#16113=CIRCLE('',#71699,7.68765459393669);
#16114=CIRCLE('',#71700,7.44531744983399);
#16115=CIRCLE('',#71701,7.69302885642449);
#16116=CIRCLE('',#71702,7.44956398909122);
#16117=CIRCLE('',#71704,7.69059185498203);
#16118=CIRCLE('',#71705,7.68765421571228);
#16119=CIRCLE('',#71706,7.44531728606217);
#16120=CIRCLE('',#71707,7.69302869881902);
#16121=CIRCLE('',#71708,7.44956390637391);
#16122=CIRCLE('',#71710,7.69059194313262);
#16123=CIRCLE('',#71711,7.68765427778048);
#16124=CIRCLE('',#71712,7.44531736610272);
#16125=CIRCLE('',#71713,7.69302857882909);
#16126=CIRCLE('',#71714,7.44956382734777);
#16127=CIRCLE('',#71716,7.69059182512427);
#16128=CIRCLE('',#71717,7.68765420156565);
#16129=CIRCLE('',#71718,7.44531757419449);
#16130=CIRCLE('',#71719,7.69302854010545);
#16131=CIRCLE('',#71720,7.449564220458);
#16132=CIRCLE('',#71722,7.69059201621511);
#16133=CIRCLE('',#71723,7.68765429038083);
#16134=CIRCLE('',#71724,7.44531728849294);
#16135=CIRCLE('',#71725,7.69302868404055);
#16136=CIRCLE('',#71726,7.44956402238821);
#16137=CIRCLE('',#71728,7.69059208059763);
#16138=CIRCLE('',#71729,7.68765413677979);
#16139=CIRCLE('',#71730,7.44531741562678);
#16140=CIRCLE('',#71731,7.44956416165948);
#16141=CIRCLE('',#71732,7.4453174835798);
#16142=CIRCLE('',#71733,7.69302857388115);
#16143=CIRCLE('',#71734,7.44956389304265);
#16144=CIRCLE('',#71736,7.69059204207201);
#16145=CIRCLE('',#71737,7.6876544760258);
#16146=CIRCLE('',#71738,7.44531737564562);
#16147=CIRCLE('',#71739,7.69302857633999);
#16148=CIRCLE('',#71740,7.44956413304808);
#16149=CIRCLE('',#71742,7.69059201870121);
#16150=CIRCLE('',#71743,7.68765433896887);
#16151=CIRCLE('',#71744,7.4453173960003);
#16152=CIRCLE('',#71745,7.6930287505808);
#16153=CIRCLE('',#71746,7.44956385182571);
#16154=CIRCLE('',#71748,7.690591959103);
#16155=CIRCLE('',#71749,7.68765455691847);
#16156=CIRCLE('',#71750,7.44531750464958);
#16157=CIRCLE('',#71751,7.69302872583272);
#16158=CIRCLE('',#71752,7.44956399165334);
#16159=CIRCLE('',#71754,7.69059185749854);
#16160=CIRCLE('',#71755,7.68765412355323);
#16161=CIRCLE('',#71756,7.44531742994769);
#16162=CIRCLE('',#71757,7.69302859365467);
#16163=CIRCLE('',#71758,7.4495641794038);
#16164=CIRCLE('',#71760,7.69059223800863);
#16165=CIRCLE('',#71761,7.68765432051477);
#16166=CIRCLE('',#71762,7.44531749413859);
#16167=CIRCLE('',#71763,7.69302870979168);
#16168=CIRCLE('',#71764,7.44956417574996);
#16169=CIRCLE('',#71766,7.69059211381182);
#16170=CIRCLE('',#71767,7.68765415326971);
#16171=CIRCLE('',#71768,7.4453174810649);
#16172=CIRCLE('',#71769,7.69302883594045);
#16173=CIRCLE('',#71770,7.44956398258887);
#16174=CIRCLE('',#71772,7.69059215577665);
#16175=CIRCLE('',#71773,7.68765415092922);
#16176=CIRCLE('',#71774,7.44531730976456);
#16177=CIRCLE('',#71775,7.69302855372752);
#16178=CIRCLE('',#71776,7.44956411333289);
#16179=CIRCLE('',#71778,7.69059175946082);
#16180=CIRCLE('',#71779,7.68765427356153);
#16181=CIRCLE('',#71780,7.44531745154568);
#16182=CIRCLE('',#71781,7.6930287837275);
#16183=CIRCLE('',#71782,7.44956391452336);
#16184=CIRCLE('',#71784,7.69059176728946);
#16185=CIRCLE('',#71785,7.68765435654041);
#16186=CIRCLE('',#71786,7.44531756343616);
#16187=CIRCLE('',#71787,7.69302889099309);
#16188=CIRCLE('',#71788,7.44956401906168);
#16189=CIRCLE('',#71790,7.69059179330732);
#16190=CIRCLE('',#71791,7.68765408720567);
#16191=CIRCLE('',#71792,7.44531755818733);
#16192=CIRCLE('',#71793,7.69302850275609);
#16193=CIRCLE('',#71794,7.44956393089751);
#16194=CIRCLE('',#71796,7.69059188019343);
#16195=CIRCLE('',#71797,7.68765433601994);
#16196=CIRCLE('',#71798,7.44531736902152);
#16197=CIRCLE('',#71799,7.69302878495204);
#16198=CIRCLE('',#71800,7.4495640374712);
#16199=CIRCLE('',#71802,7.69059212825047);
#16200=CIRCLE('',#71803,7.68765443964002);
#16201=CIRCLE('',#71804,7.44531739629565);
#16202=CIRCLE('',#71805,7.69302875141739);
#16203=CIRCLE('',#71806,7.44956382538056);
#16204=CIRCLE('',#71808,7.69059171696194);
#16205=CIRCLE('',#71809,7.68765428236649);
#16206=CIRCLE('',#71810,7.44531717926382);
#16207=CIRCLE('',#71811,7.69302889308604);
#16208=CIRCLE('',#71812,7.44956403577385);
#16209=CIRCLE('',#71814,7.69059180814142);
#16210=CIRCLE('',#71815,7.68765408817977);
#16211=CIRCLE('',#71816,7.44531754817613);
#16212=CIRCLE('',#71817,7.69302862085918);
#16213=CIRCLE('',#71818,7.44956414197099);
#16214=CIRCLE('',#71820,7.69059184122841);
#16215=CIRCLE('',#71821,7.68765444403783);
#16216=CIRCLE('',#71822,7.44531741523388);
#16217=CIRCLE('',#71823,7.6930286242407);
#16218=CIRCLE('',#71824,7.4495640397283);
#16219=CIRCLE('',#71826,7.69059178463958);
#16220=CIRCLE('',#71827,7.68765415898238);
#16221=CIRCLE('',#71828,7.44531739985699);
#16222=CIRCLE('',#71829,7.6930286520143);
#16223=CIRCLE('',#71830,7.44956409048606);
#16224=CIRCLE('',#71832,7.69059177271397);
#16225=CIRCLE('',#71833,7.68765414461077);
#16226=CIRCLE('',#71834,7.44531743415826);
#16227=CIRCLE('',#71835,7.69302855341372);
#16228=CIRCLE('',#71836,7.44956396224489);
#16229=CIRCLE('',#71837,7.68765176778231);
#16230=CIRCLE('',#71838,7.44531744815501);
#16231=CIRCLE('',#71840,7.69058939824306);
#16232=CIRCLE('',#71841,7.69302853509787);
#16233=CIRCLE('',#71842,7.44956392538232);
#16234=CIRCLE('',#71844,7.68765433956961);
#16235=CIRCLE('',#71845,7.69059203749584);
#16236=CIRCLE('',#71846,7.44531750825384);
#16237=CIRCLE('',#71847,7.69302869291321);
#16238=CIRCLE('',#71848,7.44956384698696);
#16239=CIRCLE('',#71850,7.69059210187196);
#16240=CIRCLE('',#71851,7.68765420261813);
#16241=CIRCLE('',#71852,7.44531758073562);
#16242=CIRCLE('',#71853,7.69302875800088);
#16243=CIRCLE('',#71854,7.44956383396013);
#16244=CIRCLE('',#71856,7.69059192649959);
#16245=CIRCLE('',#71857,7.68765418531522);
#16246=CIRCLE('',#71858,7.44531752816521);
#16247=CIRCLE('',#71860,7.69059202624217);
#16248=CIRCLE('',#71861,7.69302857898078);
#16249=CIRCLE('',#71862,7.44956388529172);
#16250=CIRCLE('',#71863,7.68994784729622);
#16251=CIRCLE('',#71864,7.69291176352318);
#16252=CIRCLE('',#71865,7.68994816169627);
#16253=CIRCLE('',#71867,7.69287916191551);
#16254=CIRCLE('',#71868,7.6908160876836);
#16255=CIRCLE('',#71869,7.69291193954018);
#16256=CIRCLE('',#71870,7.68994804701675);
#16257=CIRCLE('',#71872,7.6928791090222);
#16258=CIRCLE('',#71873,7.69081611331132);
#16259=CIRCLE('',#71874,7.69291178900954);
#16260=CIRCLE('',#71875,7.68994811657411);
#16261=CIRCLE('',#71877,7.69287932800169);
#16262=CIRCLE('',#71878,7.69081621527755);
#16263=CIRCLE('',#71879,7.6929116428541);
#16264=CIRCLE('',#71880,7.68994801473022);
#16265=CIRCLE('',#71882,7.6928789811809);
#16266=CIRCLE('',#71883,7.69081626752787);
#16267=CIRCLE('',#71884,7.69291192595448);
#16268=CIRCLE('',#71885,7.68994801135637);
#16269=CIRCLE('',#71887,7.69287905800627);
#16270=CIRCLE('',#71888,7.69081623259295);
#16271=CIRCLE('',#71889,7.69291165110062);
#16272=CIRCLE('',#71890,7.68994773730798);
#16273=CIRCLE('',#71892,7.6928792873396);
#16274=CIRCLE('',#71893,7.69081618096169);
#16275=CIRCLE('',#71894,7.69291179086277);
#16276=CIRCLE('',#71895,7.68994794565019);
#16277=CIRCLE('',#71897,7.69287917492001);
#16278=CIRCLE('',#71898,7.69081634191757);
#16279=CIRCLE('',#71899,7.69291211427012);
#16280=CIRCLE('',#71900,7.68994805258136);
#16281=CIRCLE('',#71902,7.69287935101192);
#16282=CIRCLE('',#71903,7.69081651118216);
#16283=CIRCLE('',#71904,7.69291165495763);
#16284=CIRCLE('',#71905,7.68994777136307);
#16285=CIRCLE('',#71907,7.69287897129759);
#16286=CIRCLE('',#71908,7.69081622705858);
#16287=CIRCLE('',#71909,7.69291174915485);
#16288=CIRCLE('',#71910,7.68994804232604);
#16289=CIRCLE('',#71912,7.692879343557);
#16290=CIRCLE('',#71913,7.69081608567409);
#16291=CIRCLE('',#71914,7.69291185563374);
#16292=CIRCLE('',#71915,7.6899479663059);
#16293=CIRCLE('',#71917,7.69287915934469);
#16294=CIRCLE('',#71918,7.69081633928341);
#16295=CIRCLE('',#71919,7.69291176261412);
#16296=CIRCLE('',#71920,7.68994794141999);
#16297=CIRCLE('',#71922,7.69287899177592);
#16298=CIRCLE('',#71923,7.6908164149815);
#16299=CIRCLE('',#71924,7.69291196007127);
#16300=CIRCLE('',#71925,7.68994808931707);
#16301=CIRCLE('',#71927,7.69287910182314);
#16302=CIRCLE('',#71928,7.69081639280079);
#16303=CIRCLE('',#71929,7.69291189125349);
#16304=CIRCLE('',#71930,7.68994771203019);
#16305=CIRCLE('',#71932,7.6928791573007);
#16306=CIRCLE('',#71933,7.69081611679542);
#16307=CIRCLE('',#71934,7.69291202082821);
#16308=CIRCLE('',#71935,7.68994808377934);
#16309=CIRCLE('',#71937,7.69287910535088);
#16310=CIRCLE('',#71938,7.69081634517804);
#16311=CIRCLE('',#71939,7.69291175642132);
#16312=CIRCLE('',#71940,7.68994812033888);
#16313=CIRCLE('',#71942,7.69287902700107);
#16314=CIRCLE('',#71943,7.69081646367517);
#16315=CIRCLE('',#71944,7.69291180726244);
#16316=CIRCLE('',#71945,7.68994797217316);
#16317=CIRCLE('',#71947,7.69287923229888);
#16318=CIRCLE('',#71948,7.69081620173846);
#16319=CIRCLE('',#71949,7.69291195486759);
#16320=CIRCLE('',#71950,7.68994791200507);
#16321=CIRCLE('',#71952,7.69287901866562);
#16322=CIRCLE('',#71953,7.6908162110816);
#16323=CIRCLE('',#71954,7.69291190742198);
#16324=CIRCLE('',#71955,7.68994789696625);
#16325=CIRCLE('',#71957,7.69287911479319);
#16326=CIRCLE('',#71958,7.69081629142424);
#16327=CIRCLE('',#71959,7.69291178333012);
#16328=CIRCLE('',#71960,7.68994811317839);
#16329=CIRCLE('',#71962,7.69287918394);
#16330=CIRCLE('',#71963,7.69081642538975);
#16331=CIRCLE('',#71964,7.69291204322326);
#16332=CIRCLE('',#71965,7.68994813733287);
#16333=CIRCLE('',#71967,7.69287899878939);
#16334=CIRCLE('',#71968,7.69081618466236);
#16335=CIRCLE('',#71969,7.69291183628174);
#16336=CIRCLE('',#71970,7.68994796202815);
#16337=CIRCLE('',#71972,7.69287933504919);
#16338=CIRCLE('',#71973,7.69081628474869);
#16339=CIRCLE('',#71974,7.69291197483368);
#16340=CIRCLE('',#71975,7.68994786758217);
#16341=CIRCLE('',#71977,7.69287921910946);
#16342=CIRCLE('',#71978,7.69081621348498);
#16343=CIRCLE('',#71979,7.69291174121852);
#16344=CIRCLE('',#71980,7.68994793911777);
#16345=CIRCLE('',#71982,7.69287914100389);
#16346=CIRCLE('',#71983,7.69081625308633);
#16347=CIRCLE('',#71984,7.69291162670279);
#16348=CIRCLE('',#71985,7.68994817762516);
#16349=CIRCLE('',#71987,7.69287912011789);
#16350=CIRCLE('',#71988,7.69081627762047);
#16351=CIRCLE('',#71989,7.69291180931249);
#16352=CIRCLE('',#71990,7.68994787650908);
#16353=CIRCLE('',#71992,7.69287925074076);
#16354=CIRCLE('',#71993,7.69081632400146);
#16355=CIRCLE('',#71994,7.69291183764281);
#16356=CIRCLE('',#71995,7.68994780337762);
#16357=CIRCLE('',#71997,7.69287902948873);
#16358=CIRCLE('',#71998,7.690816416425);
#16359=CIRCLE('',#72000,7.69291178964756);
#16360=CIRCLE('',#72001,7.69287934994747);
#16361=CIRCLE('',#72002,7.69081607066127);
#16362=CIRCLE('',#72003,7.44610039872259);
#16363=CIRCLE('',#72004,7.44610202947899);
#16364=CIRCLE('',#72005,7.44610171256494);
#16365=CIRCLE('',#72006,7.44610190544556);
#16366=CIRCLE('',#72007,7.44610194146778);
#16367=CIRCLE('',#72008,7.44610192630802);
#16368=CIRCLE('',#72009,7.44610186558304);
#16369=CIRCLE('',#72010,7.44610174233441);
#16370=CIRCLE('',#72011,7.446101890378);
#16371=CIRCLE('',#72012,7.4461017456576);
#16372=CIRCLE('',#72013,7.44610210531308);
#16373=CIRCLE('',#72014,7.4461020734202);
#16374=CIRCLE('',#72015,7.4461016563064);
#16375=CIRCLE('',#72016,7.44610189129619);
#16376=CIRCLE('',#72017,7.44610194481567);
#16377=CIRCLE('',#72018,7.44610180901079);
#16378=CIRCLE('',#72019,7.44610197957406);
#16379=CIRCLE('',#72020,7.44610171930393);
#16380=CIRCLE('',#72021,7.446101819203);
#16381=CIRCLE('',#72022,7.44610201214073);
#16382=CIRCLE('',#72023,7.44610203318976);
#16383=CIRCLE('',#72024,7.446102073294);
#16384=CIRCLE('',#72025,7.44610208015893);
#16385=CIRCLE('',#72026,7.44610205614831);
#16386=CIRCLE('',#72027,7.44610194233016);
#16387=CIRCLE('',#72028,7.44610181860739);
#16388=CIRCLE('',#72029,7.44610173753958);
#16389=CIRCLE('',#72030,7.44610226722038);
#16390=CIRCLE('',#72031,7.44610178954819);
#16391=CIRCLE('',#72032,7.44636428442216);
#16392=CIRCLE('',#72033,7.44966336559066);
#16393=CIRCLE('',#72034,7.4463619325723);
#16394=CIRCLE('',#72035,7.4496658498726);
#16395=CIRCLE('',#72036,7.4463620247186);
#16396=CIRCLE('',#72037,7.44966320020384);
#16397=CIRCLE('',#72038,7.44636200075496);
#16398=CIRCLE('',#72039,7.44966333026173);
#16399=CIRCLE('',#72040,7.44636191238419);
#16400=CIRCLE('',#72041,7.44966333924492);
#16401=CIRCLE('',#72042,7.44636196252416);
#16402=CIRCLE('',#72043,7.4496632872419);
#16403=CIRCLE('',#72044,7.44636196485215);
#16404=CIRCLE('',#72045,7.44966313666938);
#16405=CIRCLE('',#72046,7.44636197685158);
#16406=CIRCLE('',#72047,7.44966574562592);
#16407=CIRCLE('',#72048,7.44636166648237);
#16408=CIRCLE('',#72049,7.44966570381846);
#16409=CIRCLE('',#72050,7.44636196987988);
#16410=CIRCLE('',#72051,7.44966318966342);
#16411=CIRCLE('',#72052,7.44636215724432);
#16412=CIRCLE('',#72053,7.44966321197049);
#16413=CIRCLE('',#72054,7.44636200455026);
#16414=CIRCLE('',#72055,7.44966307490526);
#16415=CIRCLE('',#72056,7.44636191277395);
#16416=CIRCLE('',#72057,7.44966334625715);
#16417=CIRCLE('',#72058,7.44636197765117);
#16418=CIRCLE('',#72059,7.44966578539828);
#16419=CIRCLE('',#72060,7.44636171142628);
#16420=CIRCLE('',#72061,7.44966318204415);
#16421=CIRCLE('',#72062,7.4463619250286);
#16422=CIRCLE('',#72063,7.44966329395594);
#16423=CIRCLE('',#72064,7.44636184648991);
#16424=CIRCLE('',#72065,7.44966299354813);
#16425=CIRCLE('',#72066,7.44636186285757);
#16426=CIRCLE('',#72067,7.44966326944477);
#16427=CIRCLE('',#72068,7.44636419296111);
#16428=CIRCLE('',#72069,7.44966326236774);
#16429=CIRCLE('',#72070,7.44636197667011);
#16430=CIRCLE('',#72071,7.44966331460107);
#16431=CIRCLE('',#72072,7.44636210971674);
#16432=CIRCLE('',#72073,7.44966336557813);
#16433=CIRCLE('',#72074,7.44636219915216);
#16434=CIRCLE('',#72075,7.44966325286483);
#16435=CIRCLE('',#72076,7.4463620609399);
#16436=CIRCLE('',#72077,7.44966341877736);
#16437=CIRCLE('',#72078,7.44636193742211);
#16438=CIRCLE('',#72079,7.44966321797681);
#16439=CIRCLE('',#72080,7.44636182606499);
#16440=CIRCLE('',#72081,7.44966335654635);
#16441=CIRCLE('',#72082,7.44636204558943);
#16442=CIRCLE('',#72083,7.44966309407696);
#16443=CIRCLE('',#72084,7.44636178384992);
#16444=CIRCLE('',#72085,7.44966347089608);
#16445=CIRCLE('',#72086,7.446361748607);
#16446=CIRCLE('',#72087,7.44966325127484);
#16447=CIRCLE('',#72088,7.44636423009231);
#16448=CIRCLE('',#72089,7.44966580117451);
#16449=CIRCLE('',#72090,7.68852788878312);
#16450=CIRCLE('',#72092,7.68852788871217);
#16451=CIRCLE('',#72093,7.68852808094441);
#16452=CIRCLE('',#72095,7.68852808077644);
#16453=CIRCLE('',#72096,7.68852810841195);
#16454=CIRCLE('',#72098,7.68852810831765);
#16455=CIRCLE('',#72099,7.68852802787468);
#16456=CIRCLE('',#72101,7.68852802770763);
#16457=CIRCLE('',#72102,7.68852784840945);
#16458=CIRCLE('',#72104,7.68852784822142);
#16459=CIRCLE('',#72105,7.68852798010456);
#16460=CIRCLE('',#72107,7.68852798008635);
#16461=CIRCLE('',#72108,7.68852791683948);
#16462=CIRCLE('',#72110,7.6885279167122);
#16463=CIRCLE('',#72111,7.68852821066941);
#16464=CIRCLE('',#72113,7.68852821049969);
#16465=CIRCLE('',#72114,7.68852792917552);
#16466=CIRCLE('',#72116,7.68852792897721);
#16467=CIRCLE('',#72117,7.6885281434879);
#16468=CIRCLE('',#72119,7.68852814345323);
#16469=CIRCLE('',#72120,7.6885279546106);
#16470=CIRCLE('',#72122,7.68852795458423);
#16471=CIRCLE('',#72123,7.68852820378617);
#16472=CIRCLE('',#72125,7.68852820377537);
#16473=CIRCLE('',#72126,7.68852816718055);
#16474=CIRCLE('',#72128,7.68852816717759);
#16475=CIRCLE('',#72129,7.68852828726958);
#16476=CIRCLE('',#72131,7.68852828726758);
#16477=CIRCLE('',#72132,7.68852819473631);
#16478=CIRCLE('',#72134,7.68852819473974);
#16479=CIRCLE('',#72135,7.68852826003133);
#16480=CIRCLE('',#72137,7.68852826001605);
#16481=CIRCLE('',#72138,7.68852802375798);
#16482=CIRCLE('',#72140,7.68852802354785);
#16483=CIRCLE('',#72141,7.68852798333981);
#16484=CIRCLE('',#72143,7.6885279833);
#16485=CIRCLE('',#72144,7.68852790420368);
#16486=CIRCLE('',#72146,7.68852790420423);
#16487=CIRCLE('',#72147,7.68852797344957);
#16488=CIRCLE('',#72149,7.68852797345006);
#16489=CIRCLE('',#72150,7.68852812311045);
#16490=CIRCLE('',#72152,7.68852812311494);
#16491=CIRCLE('',#72153,7.6885280418327);
#16492=CIRCLE('',#72155,7.68852804183216);
#16493=CIRCLE('',#72156,7.68852794146179);
#16494=CIRCLE('',#72158,7.6885279414636);
#16495=CIRCLE('',#72159,7.68852772382627);
#16496=CIRCLE('',#72161,7.68852798822317);
#16497=CIRCLE('',#72162,7.68852794982855);
#16498=CIRCLE('',#72164,7.68852794991581);
#16499=CIRCLE('',#72165,7.68852776699871);
#16500=CIRCLE('',#72167,7.68852776692866);
#16501=CIRCLE('',#72168,7.68852774428418);
#16502=CIRCLE('',#72170,7.68852774423606);
#16503=CIRCLE('',#72171,7.68852783383721);
#16504=CIRCLE('',#72173,7.68852783378586);
#16505=CIRCLE('',#72174,7.68881294990728);
#16506=CIRCLE('',#72175,7.69305416871896);
#16507=CIRCLE('',#72177,7.6913546432824);
#16508=CIRCLE('',#72178,7.68881279059509);
#16509=CIRCLE('',#72179,7.69305425122366);
#16510=CIRCLE('',#72181,7.6913547410763);
#16511=CIRCLE('',#72182,7.68881286886724);
#16512=CIRCLE('',#72183,7.69305407050621);
#16513=CIRCLE('',#72185,7.6913548164225);
#16514=CIRCLE('',#72186,7.68881281359015);
#16515=CIRCLE('',#72187,7.69305419630861);
#16516=CIRCLE('',#72189,7.69135444944937);
#16517=CIRCLE('',#72190,7.68881291627626);
#16518=CIRCLE('',#72191,7.69305434953605);
#16519=CIRCLE('',#72193,7.69135469952928);
#16520=CIRCLE('',#72194,7.68881295725583);
#16521=CIRCLE('',#72195,7.6930541867945);
#16522=CIRCLE('',#72197,7.69135471403681);
#16523=CIRCLE('',#72198,7.68881304041654);
#16524=CIRCLE('',#72199,7.69305427557526);
#16525=CIRCLE('',#72201,7.6913545848261);
#16526=CIRCLE('',#72202,7.68881310970619);
#16527=CIRCLE('',#72203,7.69305424819788);
#16528=CIRCLE('',#72205,7.69135474309964);
#16529=CIRCLE('',#72206,7.6888131572352);
#16530=CIRCLE('',#72207,7.69305440873283);
#16531=CIRCLE('',#72209,7.6913547760876);
#16532=CIRCLE('',#72210,7.68881286389501);
#16533=CIRCLE('',#72211,7.6930543592403);
#16534=CIRCLE('',#72213,7.69135446595711);
#16535=CIRCLE('',#72214,7.68881294817899);
#16536=CIRCLE('',#72215,7.69305419837545);
#16537=CIRCLE('',#72217,7.69135491750166);
#16538=CIRCLE('',#72218,7.68881291089276);
#16539=CIRCLE('',#72219,7.69305429863986);
#16540=CIRCLE('',#72221,7.69135473804577);
#16541=CIRCLE('',#72222,7.6888130380488);
#16542=CIRCLE('',#72223,7.69305440505359);
#16543=CIRCLE('',#72225,7.69135457467);
#16544=CIRCLE('',#72226,7.68881275452481);
#16545=CIRCLE('',#72227,7.69305399990696);
#16546=CIRCLE('',#72229,7.69135445363969);
#16547=CIRCLE('',#72230,7.68881300384858);
#16548=CIRCLE('',#72231,7.69305432864807);
#16549=CIRCLE('',#72233,7.6913547228451);
#16550=CIRCLE('',#72234,7.68881285338845);
#16551=CIRCLE('',#72235,7.69305403777903);
#16552=CIRCLE('',#72237,7.69135477789989);
#16553=CIRCLE('',#72238,7.68881325214323);
#16554=CIRCLE('',#72239,7.69305437016307);
#16555=CIRCLE('',#72241,7.69135463961681);
#16556=CIRCLE('',#72242,7.68881274595675);
#16557=CIRCLE('',#72243,7.69305424024155);
#16558=CIRCLE('',#72245,7.691354591453);
#16559=CIRCLE('',#72246,7.68881313601843);
#16560=CIRCLE('',#72247,7.69305423658223);
#16561=CIRCLE('',#72249,7.69135483048538);
#16562=CIRCLE('',#72250,7.68881313175157);
#16563=CIRCLE('',#72251,7.69305421496098);
#16564=CIRCLE('',#72253,7.69135483246873);
#16565=CIRCLE('',#72254,7.68881287351973);
#16566=CIRCLE('',#72255,7.69305415299332);
#16567=CIRCLE('',#72257,7.69135468194924);
#16568=CIRCLE('',#72258,7.68881305745295);
#16569=CIRCLE('',#72259,7.69305441708648);
#16570=CIRCLE('',#72261,7.69135467139016);
#16571=CIRCLE('',#72262,7.6888130343247);
#16572=CIRCLE('',#72263,7.69305425088512);
#16573=CIRCLE('',#72265,7.69135479635185);
#16574=CIRCLE('',#72266,7.68881329210462);
#16575=CIRCLE('',#72267,7.69305436804117);
#16576=CIRCLE('',#72269,7.6913544468307);
#16577=CIRCLE('',#72270,7.68881306344792);
#16578=CIRCLE('',#72271,7.69305414738288);
#16579=CIRCLE('',#72273,7.69135456385503);
#16580=CIRCLE('',#72274,7.68881318269362);
#16581=CIRCLE('',#72275,7.69305422279801);
#16582=CIRCLE('',#72277,7.69135469458882);
#16583=CIRCLE('',#72278,7.68881305420038);
#16584=CIRCLE('',#72279,7.6930542709141);
#16585=CIRCLE('',#72281,7.69135459595344);
#16586=CIRCLE('',#72282,7.68881312219884);
#16587=CIRCLE('',#72283,7.69305435220014);
#16588=CIRCLE('',#72285,7.69135478455061);
#16589=CIRCLE('',#72286,7.44609831292764);
#16590=CIRCLE('',#72287,7.44609962301868);
#16591=CIRCLE('',#72288,7.44609935175357);
#16592=CIRCLE('',#72289,7.44609956374778);
#16593=CIRCLE('',#72290,7.44609960110811);
#16594=CIRCLE('',#72291,7.44609976907078);
#16595=CIRCLE('',#72292,7.44609970176048);
#16596=CIRCLE('',#72293,7.4460998316161);
#16597=CIRCLE('',#72294,7.44609995608563);
#16598=CIRCLE('',#72295,7.44609954146893);
#16599=CIRCLE('',#72296,7.44610000859957);
#16600=CIRCLE('',#72297,7.44609964341751);
#16601=CIRCLE('',#72298,7.44609943228571);
#16602=CIRCLE('',#72299,7.44609967299467);
#16603=CIRCLE('',#72300,7.4460995580868);
#16604=CIRCLE('',#72301,7.44609952767346);
#16605=CIRCLE('',#72302,7.44609942719343);
#16606=CIRCLE('',#72303,7.44609953709856);
#16607=CIRCLE('',#72304,7.44609964556177);
#16608=CIRCLE('',#72305,7.4460996868155);
#16609=CIRCLE('',#72306,7.44609954955322);
#16610=CIRCLE('',#72307,7.44609968798886);
#16611=CIRCLE('',#72308,7.44609966377836);
#16612=CIRCLE('',#72309,7.44609989884677);
#16613=CIRCLE('',#72310,7.44609968307516);
#16614=CIRCLE('',#72311,7.44609972796809);
#16615=CIRCLE('',#72312,7.44609940228724);
#16616=CIRCLE('',#72313,7.44609997449684);
#16617=CIRCLE('',#72314,7.44609986988839);
#16618=CIRCLE('',#72315,7.44703765958231);
#16619=CIRCLE('',#72316,7.44703740592205);
#16620=CIRCLE('',#72317,7.44703728970287);
#16621=CIRCLE('',#72318,7.44703734046266);
#16622=CIRCLE('',#72319,7.44703750753235);
#16623=CIRCLE('',#72320,7.44703765689882);
#16624=CIRCLE('',#72321,7.44703757846929);
#16625=CIRCLE('',#72322,7.4470374290604);
#16626=CIRCLE('',#72323,7.44703734393595);
#16627=CIRCLE('',#72324,7.44703746303222);
#16628=CIRCLE('',#72325,7.44703758748381);
#16629=CIRCLE('',#72326,7.44703737549802);
#16630=CIRCLE('',#72327,7.44703743508742);
#16631=CIRCLE('',#72328,7.44703765138706);
#16632=CIRCLE('',#72329,7.44703743978475);
#16633=CIRCLE('',#72330,7.44703751052387);
#16634=CIRCLE('',#72331,7.44703748822274);
#16635=CIRCLE('',#72332,7.44703753018844);
#16636=CIRCLE('',#72333,7.447037332229);
#16637=CIRCLE('',#72334,7.44703755755212);
#16638=CIRCLE('',#72335,7.44703741504868);
#16639=CIRCLE('',#72336,7.44703762292078);
#16640=CIRCLE('',#72337,7.44703724464123);
#16641=CIRCLE('',#72338,7.44703743114767);
#16642=CIRCLE('',#72339,7.44703751909643);
#16643=CIRCLE('',#72340,7.44703753083635);
#16644=CIRCLE('',#72341,7.44703745309058);
#16645=CIRCLE('',#72342,7.44703746637215);
#16646=CIRCLE('',#72343,7.44703740586822);
#16647=CIRCLE('',#72344,7.69059202594198);
#16648=CIRCLE('',#72346,7.69302856000655);
#16649=CIRCLE('',#72347,7.68765459426427);
#16650=CIRCLE('',#72348,7.690591902328);
#16651=CIRCLE('',#72350,7.69302885754567);
#16652=CIRCLE('',#72351,7.68765421623993);
#16653=CIRCLE('',#72352,7.69059185365515);
#16654=CIRCLE('',#72354,7.69302869987157);
#16655=CIRCLE('',#72355,7.68765427825275);
#16656=CIRCLE('',#72356,7.69059194180294);
#16657=CIRCLE('',#72358,7.69302857976961);
#16658=CIRCLE('',#72359,7.68765420205096);
#16659=CIRCLE('',#72360,7.6905918237196);
#16660=CIRCLE('',#72362,7.69302854134258);
#16661=CIRCLE('',#72363,7.6876542908369);
#16662=CIRCLE('',#72364,7.69059201504414);
#16663=CIRCLE('',#72366,7.69302868508283);
#16664=CIRCLE('',#72367,7.68765413714181);
#16665=CIRCLE('',#72368,7.69059207938841);
#16666=CIRCLE('',#72370,7.69302857487276);
#16667=CIRCLE('',#72371,7.68765447657531);
#16668=CIRCLE('',#72372,7.6905920405608);
#16669=CIRCLE('',#72374,7.69302857789015);
#16670=CIRCLE('',#72375,7.68765433942058);
#16671=CIRCLE('',#72376,7.69059201956098);
#16672=CIRCLE('',#72378,7.6930287518199);
#16673=CIRCLE('',#72379,7.68765455699274);
#16674=CIRCLE('',#72380,7.69059196034469);
#16675=CIRCLE('',#72382,7.69302872710911);
#16676=CIRCLE('',#72383,7.68765412359293);
#16677=CIRCLE('',#72384,7.69059185681044);
#16678=CIRCLE('',#72386,7.6930285949259);
#16679=CIRCLE('',#72387,7.68765432051234);
#16680=CIRCLE('',#72388,7.69059223732896);
#16681=CIRCLE('',#72390,7.69302871106017);
#16682=CIRCLE('',#72391,7.6876541532703);
#16683=CIRCLE('',#72392,7.69059211516317);
#16684=CIRCLE('',#72394,7.69302883712055);
#16685=CIRCLE('',#72395,7.68765415096754);
#16686=CIRCLE('',#72396,7.69059215704542);
#16687=CIRCLE('',#72398,7.69302855499968);
#16688=CIRCLE('',#72399,7.68765427356152);
#16689=CIRCLE('',#72400,7.69059175878684);
#16690=CIRCLE('',#72402,7.69302878492282);
#16691=CIRCLE('',#72403,7.68765435655919);
#16692=CIRCLE('',#72404,7.69059176654608);
#16693=CIRCLE('',#72406,7.69302889183546);
#16694=CIRCLE('',#72407,7.68765408745106);
#16695=CIRCLE('',#72408,7.69059179184688);
#16696=CIRCLE('',#72410,7.69302850426747);
#16697=CIRCLE('',#72411,7.68765433650955);
#16698=CIRCLE('',#72412,7.69059187920957);
#16699=CIRCLE('',#72414,7.693028786307);
#16700=CIRCLE('',#72415,7.6876544397187);
#16701=CIRCLE('',#72416,7.6905921275555);
#16702=CIRCLE('',#72418,7.69302875264593);
#16703=CIRCLE('',#72419,7.68765428237974);
#16704=CIRCLE('',#72420,7.69059171827927);
#16705=CIRCLE('',#72422,7.69302889434345);
#16706=CIRCLE('',#72423,7.6876540881813);
#16707=CIRCLE('',#72424,7.69059180948577);
#16708=CIRCLE('',#72426,7.69302862207645);
#16709=CIRCLE('',#72427,7.68765444403721);
#16710=CIRCLE('',#72428,7.69059184049164);
#16711=CIRCLE('',#72430,7.69302862547662);
#16712=CIRCLE('',#72431,7.68765415899986);
#16713=CIRCLE('',#72432,7.69059178595574);
#16714=CIRCLE('',#72433,7.69058741691256);
#16715=CIRCLE('',#72435,7.69302865324643);
#16716=CIRCLE('',#72436,7.68764993425013);
#16717=CIRCLE('',#72438,7.69059194581034);
#16718=CIRCLE('',#72439,7.69302855474821);
#16719=CIRCLE('',#72440,7.68765409297156);
#16720=CIRCLE('',#72442,7.69302853646235);
#16721=CIRCLE('',#72443,7.68765433980124);
#16722=CIRCLE('',#72444,7.6905920362682);
#16723=CIRCLE('',#72446,7.69302869406925);
#16724=CIRCLE('',#72447,7.6876542028167);
#16725=CIRCLE('',#72448,7.69059210092743);
#16726=CIRCLE('',#72450,7.69302875921919);
#16727=CIRCLE('',#72451,7.68765418549446);
#16728=CIRCLE('',#72452,7.69059192762103);
#16729=CIRCLE('',#72454,7.69302857768801);
#16730=CIRCLE('',#72455,7.68765422035337);
#16731=CIRCLE('',#72456,7.6895705373055);
#16732=CIRCLE('',#72457,7.68957071702817);
#16733=CIRCLE('',#72459,7.68318431078712);
#16734=CIRCLE('',#72460,7.68733814977416);
#16735=CIRCLE('',#72461,7.68957062858146);
#16736=CIRCLE('',#72463,7.68318471226888);
#16737=CIRCLE('',#72464,7.68733847129689);
#16738=CIRCLE('',#72465,7.68957064027973);
#16739=CIRCLE('',#72467,7.68318447973371);
#16740=CIRCLE('',#72468,7.68733822094465);
#16741=CIRCLE('',#72469,7.68957077150367);
#16742=CIRCLE('',#72471,7.68318420940126);
#16743=CIRCLE('',#72472,7.68733824007977);
#16744=CIRCLE('',#72473,7.6895707292031);
#16745=CIRCLE('',#72475,7.68318447990023);
#16746=CIRCLE('',#72476,7.68733833121305);
#16747=CIRCLE('',#72477,7.68957051214316);
#16748=CIRCLE('',#72479,7.68318398809391);
#16749=CIRCLE('',#72480,7.68733834665324);
#16750=CIRCLE('',#72481,7.68957088611825);
#16751=CIRCLE('',#72483,7.68318408620415);
#16752=CIRCLE('',#72484,7.68733822732077);
#16753=CIRCLE('',#72485,7.68957065040893);
#16754=CIRCLE('',#72487,7.68318452630675);
#16755=CIRCLE('',#72488,7.68733802736002);
#16756=CIRCLE('',#72489,7.68957094261063);
#16757=CIRCLE('',#72491,7.68318482090721);
#16758=CIRCLE('',#72492,7.68733816294838);
#16759=CIRCLE('',#72493,7.68957064665883);
#16760=CIRCLE('',#72495,7.68318426666719);
#16761=CIRCLE('',#72496,7.68733828478715);
#16762=CIRCLE('',#72497,7.68957074083717);
#16763=CIRCLE('',#72499,7.6831839731994);
#16764=CIRCLE('',#72500,7.68733823353924);
#16765=CIRCLE('',#72501,7.68957060360401);
#16766=CIRCLE('',#72503,7.68318443244907);
#16767=CIRCLE('',#72504,7.68733826168596);
#16768=CIRCLE('',#72505,7.68957074524144);
#16769=CIRCLE('',#72507,7.68318434353364);
#16770=CIRCLE('',#72508,7.68733841485494);
#16771=CIRCLE('',#72509,7.68957093395326);
#16772=CIRCLE('',#72511,7.68318462758714);
#16773=CIRCLE('',#72512,7.68733828523044);
#16774=CIRCLE('',#72513,7.68957078939204);
#16775=CIRCLE('',#72515,7.6831848112711);
#16776=CIRCLE('',#72516,7.68733844594019);
#16777=CIRCLE('',#72517,7.68957087822363);
#16778=CIRCLE('',#72519,7.68318425943269);
#16779=CIRCLE('',#72520,7.68733803337296);
#16780=CIRCLE('',#72521,7.68957040880922);
#16781=CIRCLE('',#72523,7.68318448193786);
#16782=CIRCLE('',#72524,7.68733838938515);
#16783=CIRCLE('',#72525,7.68957082558246);
#16784=CIRCLE('',#72527,7.68318409703543);
#16785=CIRCLE('',#72528,7.68733811369692);
#16786=CIRCLE('',#72529,7.68957078793141);
#16787=CIRCLE('',#72531,7.68318432153085);
#16788=CIRCLE('',#72532,7.6873382577664);
#16789=CIRCLE('',#72533,7.68957090366153);
#16790=CIRCLE('',#72535,7.68318447137218);
#16791=CIRCLE('',#72536,7.68733847367282);
#16792=CIRCLE('',#72537,7.68957060775697);
#16793=CIRCLE('',#72539,7.68318416167432);
#16794=CIRCLE('',#72540,7.68733827550981);
#16795=CIRCLE('',#72541,7.68957085438422);
#16796=CIRCLE('',#72543,7.68318476711715);
#16797=CIRCLE('',#72544,7.68733832707878);
#16798=CIRCLE('',#72545,7.68957080161283);
#16799=CIRCLE('',#72547,7.6831845569757);
#16800=CIRCLE('',#72548,7.68733833084729);
#16801=CIRCLE('',#72549,7.68957079004739);
#16802=CIRCLE('',#72551,7.68318419339156);
#16803=CIRCLE('',#72552,7.68733810715353);
#16804=CIRCLE('',#72553,7.68957079118119);
#16805=CIRCLE('',#72555,7.6831845910336);
#16806=CIRCLE('',#72556,7.68733835573841);
#16807=CIRCLE('',#72557,7.68957083928288);
#16808=CIRCLE('',#72559,7.68318437103514);
#16809=CIRCLE('',#72560,7.68733808432302);
#16810=CIRCLE('',#72561,7.68957083624163);
#16811=CIRCLE('',#72563,7.6831840524939);
#16812=CIRCLE('',#72564,7.68733811585128);
#16813=CIRCLE('',#72566,7.68318490909919);
#16814=CIRCLE('',#72567,7.68733853056307);
#16815=CIRCLE('',#72568,7.44531538645819);
#16816=CIRCLE('',#72569,7.44956381440597);
#16817=CIRCLE('',#72570,7.44531525600097);
#16818=CIRCLE('',#72571,7.44956398909259);
#16819=CIRCLE('',#72572,7.44531519228589);
#16820=CIRCLE('',#72573,7.44956390637326);
#16821=CIRCLE('',#72574,7.44531530198313);
#16822=CIRCLE('',#72575,7.44956382734727);
#16823=CIRCLE('',#72576,7.44531538463241);
#16824=CIRCLE('',#72577,7.44956422045783);
#16825=CIRCLE('',#72578,7.44531524460531);
#16826=CIRCLE('',#72579,7.44956402238707);
#16827=CIRCLE('',#72580,7.44531535871156);
#16828=CIRCLE('',#72581,7.44956416166019);
#16829=CIRCLE('',#72582,7.44531527750566);
#16830=CIRCLE('',#72583,7.44956389304393);
#16831=CIRCLE('',#72584,7.44531529542168);
#16832=CIRCLE('',#72585,7.44956413304856);
#16833=CIRCLE('',#72586,7.4453153154805);
#16834=CIRCLE('',#72587,7.44956385182501);
#16835=CIRCLE('',#72588,7.44531529811139);
#16836=CIRCLE('',#72589,7.44956399165328);
#16837=CIRCLE('',#72590,7.44531535591968);
#16838=CIRCLE('',#72591,7.44956417940239);
#16839=CIRCLE('',#72592,7.44531536039092);
#16840=CIRCLE('',#72593,7.44956417574995);
#16841=CIRCLE('',#72594,7.44531533180438);
#16842=CIRCLE('',#72595,7.44956398258933);
#16843=CIRCLE('',#72596,7.44531507760606);
#16844=CIRCLE('',#72597,7.44956411333289);
#16845=CIRCLE('',#72598,7.44531530812124);
#16846=CIRCLE('',#72599,7.44956391452336);
#16847=CIRCLE('',#72600,7.44531533056805);
#16848=CIRCLE('',#72601,7.44956401906169);
#16849=CIRCLE('',#72602,7.44531538142944);
#16850=CIRCLE('',#72603,7.44956393089749);
#16851=CIRCLE('',#72604,7.44531515711117);
#16852=CIRCLE('',#72605,7.4495640374712);
#16853=CIRCLE('',#72606,7.44531526111994);
#16854=CIRCLE('',#72607,7.4495638253791);
#16855=CIRCLE('',#72608,7.44531512832504);
#16856=CIRCLE('',#72609,7.4495640357743);
#16857=CIRCLE('',#72610,7.44531536062869);
#16858=CIRCLE('',#72611,7.44956414197099);
#16859=CIRCLE('',#72612,7.44531540976715);
#16860=CIRCLE('',#72613,7.4495640397269);
#16861=CIRCLE('',#72614,7.44531524242191);
#16862=CIRCLE('',#72615,7.44956409048664);
#16863=CIRCLE('',#72616,7.44531544260196);
#16864=CIRCLE('',#72617,7.44956396224621);
#16865=CIRCLE('',#72618,7.44531525344054);
#16866=CIRCLE('',#72619,7.4495639253832);
#16867=CIRCLE('',#72620,7.44531531942668);
#16868=CIRCLE('',#72621,7.44956384698854);
#16869=CIRCLE('',#72622,7.44531551160301);
#16870=CIRCLE('',#72623,7.4495640070332);
#16871=CIRCLE('',#72624,7.44531539934746);
#16872=CIRCLE('',#72625,7.44956388528947);
#16873=CIRCLE('',#72626,7.44501798128672);
#16874=CIRCLE('',#72627,7.44501863613543);
#16875=CIRCLE('',#72628,7.44501880349459);
#16876=CIRCLE('',#72629,7.44501892336087);
#16877=CIRCLE('',#72630,7.44501873113526);
#16878=CIRCLE('',#72631,7.44501877734031);
#16879=CIRCLE('',#72632,7.44501879135829);
#16880=CIRCLE('',#72633,7.44501889805359);
#16881=CIRCLE('',#72634,7.44501868281248);
#16882=CIRCLE('',#72635,7.44501877144378);
#16883=CIRCLE('',#72636,7.4450186464062);
#16884=CIRCLE('',#72637,7.44501897930043);
#16885=CIRCLE('',#72638,7.44501872350213);
#16886=CIRCLE('',#72639,7.44501872218195);
#16887=CIRCLE('',#72640,7.4450187414317);
#16888=CIRCLE('',#72641,7.44501896740992);
#16889=CIRCLE('',#72642,7.4450189666943);
#16890=CIRCLE('',#72643,7.44501886990939);
#16891=CIRCLE('',#72644,7.44501870710545);
#16892=CIRCLE('',#72645,7.44501889130117);
#16893=CIRCLE('',#72646,7.44501895300577);
#16894=CIRCLE('',#72647,7.44501885439827);
#16895=CIRCLE('',#72648,7.44501873231066);
#16896=CIRCLE('',#72649,7.44501863965835);
#16897=CIRCLE('',#72650,7.44501881787528);
#16898=CIRCLE('',#72651,7.44501870219928);
#16899=CIRCLE('',#72652,7.44501879756191);
#16900=CIRCLE('',#72653,7.44501886683483);
#16901=CIRCLE('',#72654,7.44501879564492);
#16902=CIRCLE('',#72655,7.68994768850121);
#16903=CIRCLE('',#72657,7.69081639039695);
#16904=CIRCLE('',#72658,7.69287902948567);
#16905=CIRCLE('',#72659,7.69291183764604);
#16906=CIRCLE('',#72660,7.68994776176434);
#16907=CIRCLE('',#72662,7.69081629816903);
#16908=CIRCLE('',#72663,7.69287925074);
#16909=CIRCLE('',#72664,7.69291180931347);
#16910=CIRCLE('',#72665,7.68994806307652);
#16911=CIRCLE('',#72667,7.69081625244724);
#16912=CIRCLE('',#72668,7.69287912011643);
#16913=CIRCLE('',#72669,7.69291162670421);
#16914=CIRCLE('',#72670,7.68994782425453);
#16915=CIRCLE('',#72672,7.69081622752238);
#16916=CIRCLE('',#72673,7.69287914100277);
#16917=CIRCLE('',#72674,7.69291174121858);
#16918=CIRCLE('',#72675,7.68994775281266);
#16919=CIRCLE('',#72677,7.69081618799205);
#16920=CIRCLE('',#72678,7.69287921910763);
#16921=CIRCLE('',#72679,7.69291197483402);
#16922=CIRCLE('',#72680,7.68994784764813);
#16923=CIRCLE('',#72682,7.69081625930234);
#16924=CIRCLE('',#72683,7.69287933505147);
#16925=CIRCLE('',#72684,7.69291183628208);
#16926=CIRCLE('',#72685,7.68994802235942);
#16927=CIRCLE('',#72687,7.69081615857865);
#16928=CIRCLE('',#72688,7.69287899879009);
#16929=CIRCLE('',#72689,7.6929120432216);
#16930=CIRCLE('',#72690,7.68994799837717);
#16931=CIRCLE('',#72692,7.69081639968424);
#16932=CIRCLE('',#72693,7.69287918394263);
#16933=CIRCLE('',#72694,7.6929117833322);
#16934=CIRCLE('',#72695,7.68994777527193);
#16935=CIRCLE('',#72697,7.69081626579946);
#16936=CIRCLE('',#72698,7.69287911479038);
#16937=CIRCLE('',#72699,7.69291190741967);
#16938=CIRCLE('',#72700,7.68994779714343);
#16939=CIRCLE('',#72702,7.69081618537138);
#16940=CIRCLE('',#72703,7.6928790186626);
#16941=CIRCLE('',#72704,7.69291195486959);
#16942=CIRCLE('',#72705,7.68994785743113);
#16943=CIRCLE('',#72707,7.69081617604151);
#16944=CIRCLE('',#72708,7.69287923229911);
#16945=CIRCLE('',#72709,7.69291180726217);
#16946=CIRCLE('',#72710,7.68994800537629);
#16947=CIRCLE('',#72712,7.69081643790944);
#16948=CIRCLE('',#72713,7.69287902700114);
#16949=CIRCLE('',#72714,7.69291175642132);
#16950=CIRCLE('',#72715,7.68994796871448);
#16951=CIRCLE('',#72717,7.6908163194903);
#16952=CIRCLE('',#72718,7.69287910534962);
#16953=CIRCLE('',#72719,7.69291202082806);
#16954=CIRCLE('',#72720,7.6899475970862);
#16955=CIRCLE('',#72722,7.6908162053019);
#16956=CIRCLE('',#72723,7.69287915730047);
#16957=CIRCLE('',#72724,7.6929118912537);
#16958=CIRCLE('',#72725,7.68994797437207);
#16959=CIRCLE('',#72727,7.69081636705849);
#16960=CIRCLE('',#72728,7.69287910182044);
#16961=CIRCLE('',#72729,7.69291196007138);
#16962=CIRCLE('',#72730,7.68994782657826);
#16963=CIRCLE('',#72732,7.69081638893993);
#16964=CIRCLE('',#72733,7.69287899177703);
#16965=CIRCLE('',#72734,7.69291176261553);
#16966=CIRCLE('',#72735,7.68994785039263);
#16967=CIRCLE('',#72737,7.69081631363439);
#16968=CIRCLE('',#72738,7.69287915934317);
#16969=CIRCLE('',#72739,7.69291185563463);
#16970=CIRCLE('',#72740,7.68994792779107);
#16971=CIRCLE('',#72742,7.69081611198666);
#16972=CIRCLE('',#72743,7.69287945730006);
#16973=CIRCLE('',#72744,7.69291174915492);
#16974=CIRCLE('',#72745,7.68994765651948);
#16975=CIRCLE('',#72747,7.69081620155709);
#16976=CIRCLE('',#72748,7.6928789712968);
#16977=CIRCLE('',#72749,7.69291165495841);
#16978=CIRCLE('',#72750,7.68994793766104);
#16979=CIRCLE('',#72752,7.69081648538269);
#16980=CIRCLE('',#72753,7.69287935101016);
#16981=CIRCLE('',#72754,7.69291211427012);
#16982=CIRCLE('',#72755,7.68994783081566);
#16983=CIRCLE('',#72757,7.69081631618511);
#16984=CIRCLE('',#72758,7.69287917491714);
#16985=CIRCLE('',#72759,7.69291179086216);
#16986=CIRCLE('',#72760,7.68994762249597);
#16987=CIRCLE('',#72762,7.69081615538454);
#16988=CIRCLE('',#72763,7.69287928734082);
#16989=CIRCLE('',#72764,7.69291165110122);
#16990=CIRCLE('',#72765,7.68994789648978);
#16991=CIRCLE('',#72766,7.69291192595375);
#16992=CIRCLE('',#72768,7.69081620706134);
#16993=CIRCLE('',#72769,7.69287911855576);
#16994=CIRCLE('',#72770,7.68994789980955);
#16995=CIRCLE('',#72772,7.69291164285274);
#16996=CIRCLE('',#72773,7.69081624184935);
#16997=CIRCLE('',#72774,7.69287898118367);
#16998=CIRCLE('',#72775,7.68994800192127);
#16999=CIRCLE('',#72777,7.69081618985827);
#17000=CIRCLE('',#72778,7.69287932799914);
#17001=CIRCLE('',#72779,7.69291178900987);
#17002=CIRCLE('',#72780,7.68994793193109);
#17003=CIRCLE('',#72782,7.69081608773444);
#17004=CIRCLE('',#72783,7.69287910901963);
#17005=CIRCLE('',#72784,7.69291193953742);
#17006=CIRCLE('',#72785,7.68994804678886);
#17007=CIRCLE('',#72787,7.69081606230325);
#17008=CIRCLE('',#72788,7.69287916191094);
#17009=CIRCLE('',#72789,7.69291176352222);
#17010=CIRCLE('',#72790,7.6899477324061);
#17011=CIRCLE('',#72792,7.6908160448308);
#17012=CIRCLE('',#72793,7.69287928896208);
#17013=CIRCLE('',#72794,7.69291178964863);
#17014=CIRCLE('',#72795,7.68969379605931);
#17015=CIRCLE('',#72797,7.68635993537705);
#17016=CIRCLE('',#72798,7.69279340224594);
#17017=CIRCLE('',#72799,7.68969366433993);
#17018=CIRCLE('',#72801,7.68635964596802);
#17019=CIRCLE('',#72802,7.69279317570462);
#17020=CIRCLE('',#72803,7.68969389957442);
#17021=CIRCLE('',#72805,7.68636012101837);
#17022=CIRCLE('',#72806,7.69279321981756);
#17023=CIRCLE('',#72807,7.68969357082102);
#17024=CIRCLE('',#72809,7.68635971152984);
#17025=CIRCLE('',#72810,7.69279330277333);
#17026=CIRCLE('',#72811,7.68969356005781);
#17027=CIRCLE('',#72813,7.68635984569196);
#17028=CIRCLE('',#72814,7.69279339299752);
#17029=CIRCLE('',#72815,7.68969378432535);
#17030=CIRCLE('',#72817,7.68636009876598);
#17031=CIRCLE('',#72818,7.69279319574932);
#17032=CIRCLE('',#72819,7.68969354635827);
#17033=CIRCLE('',#72821,7.68635984983445);
#17034=CIRCLE('',#72822,7.69279329838833);
#17035=CIRCLE('',#72823,7.68969384772044);
#17036=CIRCLE('',#72825,7.68635987722991);
#17037=CIRCLE('',#72826,7.69279306777004);
#17038=CIRCLE('',#72827,7.68969379587333);
#17039=CIRCLE('',#72829,7.68636009200399);
#17040=CIRCLE('',#72830,7.69279307273185);
#17041=CIRCLE('',#72831,7.68969360005298);
#17042=CIRCLE('',#72833,7.68636010647129);
#17043=CIRCLE('',#72834,7.69279313806582);
#17044=CIRCLE('',#72835,7.68969367951995);
#17045=CIRCLE('',#72837,7.6863598904456);
#17046=CIRCLE('',#72838,7.69279352359976);
#17047=CIRCLE('',#72839,7.68969372147397);
#17048=CIRCLE('',#72841,7.68635974611356);
#17049=CIRCLE('',#72842,7.69279344881826);
#17050=CIRCLE('',#72843,7.68969343633667);
#17051=CIRCLE('',#72845,7.68635971737299);
#17052=CIRCLE('',#72846,7.69279338068447);
#17053=CIRCLE('',#72847,7.68969375791827);
#17054=CIRCLE('',#72849,7.68635998328794);
#17055=CIRCLE('',#72850,7.69279332422182);
#17056=CIRCLE('',#72851,7.68969363714325);
#17057=CIRCLE('',#72853,7.68635991849997);
#17058=CIRCLE('',#72854,7.69279311575017);
#17059=CIRCLE('',#72855,7.68969369394559);
#17060=CIRCLE('',#72857,7.68635983689677);
#17061=CIRCLE('',#72858,7.69279334009542);
#17062=CIRCLE('',#72859,7.68969364964678);
#17063=CIRCLE('',#72861,7.68636005130882);
#17064=CIRCLE('',#72862,7.69279299577899);
#17065=CIRCLE('',#72863,7.68969389920012);
#17066=CIRCLE('',#72865,7.68635990825161);
#17067=CIRCLE('',#72866,7.69279308680408);
#17068=CIRCLE('',#72867,7.68969379341059);
#17069=CIRCLE('',#72869,7.6863602299655);
#17070=CIRCLE('',#72870,7.69279310613291);
#17071=CIRCLE('',#72871,7.68969380669233);
#17072=CIRCLE('',#72873,7.68635982548127);
#17073=CIRCLE('',#72874,7.69279340053383);
#17074=CIRCLE('',#72875,7.68969366719949);
#17075=CIRCLE('',#72877,7.68636003695748);
#17076=CIRCLE('',#72878,7.69279333592378);
#17077=CIRCLE('',#72879,7.68969377855696);
#17078=CIRCLE('',#72881,7.68635979155829);
#17079=CIRCLE('',#72882,7.69279341300475);
#17080=CIRCLE('',#72883,7.6896937574551);
#17081=CIRCLE('',#72885,7.68635978467662);
#17082=CIRCLE('',#72886,7.69279336051956);
#17083=CIRCLE('',#72887,7.68969364519625);
#17084=CIRCLE('',#72889,7.68636002417854);
#17085=CIRCLE('',#72890,7.69279335544202);
#17086=CIRCLE('',#72891,7.68969359825938);
#17087=CIRCLE('',#72893,7.68635983159926);
#17088=CIRCLE('',#72894,7.6927933468798);
#17089=CIRCLE('',#72895,7.6896938024155);
#17090=CIRCLE('',#72897,7.68635976539525);
#17091=CIRCLE('',#72898,7.69279326968129);
#17092=CIRCLE('',#72899,7.68969370355732);
#17093=CIRCLE('',#72901,7.68635995743284);
#17094=CIRCLE('',#72902,7.69279303053349);
#17095=CIRCLE('',#72903,7.68969378343039);
#17096=CIRCLE('',#72905,7.68635996847948);
#17097=CIRCLE('',#72906,7.69279317991971);
#17098=CIRCLE('',#72907,7.68969357197823);
#17099=CIRCLE('',#72909,7.68635979354931);
#17100=CIRCLE('',#72910,7.69279316452614);
#17101=CIRCLE('',#72911,7.44636423010508);
#17102=CIRCLE('',#72912,7.44966325127302);
#17103=CIRCLE('',#72913,7.44636174860661);
#17104=CIRCLE('',#72914,7.44966347089591);
#17105=CIRCLE('',#72915,7.44636178384942);
#17106=CIRCLE('',#72916,7.44966309407636);
#17107=CIRCLE('',#72917,7.44636204559121);
#17108=CIRCLE('',#72918,7.44966335654733);
#17109=CIRCLE('',#72919,7.44636182606712);
#17110=CIRCLE('',#72920,7.44966321797586);
#17111=CIRCLE('',#72921,7.44636193742149);
#17112=CIRCLE('',#72922,7.44966341877709);
#17113=CIRCLE('',#72923,7.44636206094047);
#17114=CIRCLE('',#72924,7.44966325286485);
#17115=CIRCLE('',#72925,7.44636219915386);
#17116=CIRCLE('',#72926,7.44966336557642);
#17117=CIRCLE('',#72927,7.44636210971655);
#17118=CIRCLE('',#72928,7.44966331459993);
#17119=CIRCLE('',#72929,7.44636197667186);
#17120=CIRCLE('',#72930,7.44966326236817);
#17121=CIRCLE('',#72931,7.44636419295865);
#17122=CIRCLE('',#72932,7.44966326944475);
#17123=CIRCLE('',#72933,7.44636186285971);
#17124=CIRCLE('',#72934,7.44966299354956);
#17125=CIRCLE('',#72935,7.44636184648999);
#17126=CIRCLE('',#72936,7.44966329395538);
#17127=CIRCLE('',#72937,7.44636192502926);
#17128=CIRCLE('',#72938,7.44966318204452);
#17129=CIRCLE('',#72939,7.44636171142564);
#17130=CIRCLE('',#72940,7.44966578527346);
#17131=CIRCLE('',#72941,7.44636197765164);
#17132=CIRCLE('',#72942,7.44966334625654);
#17133=CIRCLE('',#72943,7.44636191277442);
#17134=CIRCLE('',#72944,7.44966307490312);
#17135=CIRCLE('',#72945,7.44636200455071);
#17136=CIRCLE('',#72946,7.44966321197009);
#17137=CIRCLE('',#72947,7.44636215724628);
#17138=CIRCLE('',#72948,7.44966318966319);
#17139=CIRCLE('',#72949,7.44636196988074);
#17140=CIRCLE('',#72950,7.44966570382605);
#17141=CIRCLE('',#72951,7.44636166648058);
#17142=CIRCLE('',#72952,7.44966574550693);
#17143=CIRCLE('',#72953,7.44636197685232);
#17144=CIRCLE('',#72954,7.4496631366682);
#17145=CIRCLE('',#72955,7.44636196485188);
#17146=CIRCLE('',#72956,7.44966328724103);
#17147=CIRCLE('',#72957,7.44636196252542);
#17148=CIRCLE('',#72958,7.44966333924468);
#17149=CIRCLE('',#72959,7.44636191238592);
#17150=CIRCLE('',#72960,7.44966333026025);
#17151=CIRCLE('',#72961,7.44636200075493);
#17152=CIRCLE('',#72962,7.44966320020436);
#17153=CIRCLE('',#72963,7.44636202472126);
#17154=CIRCLE('',#72964,7.44966584986547);
#17155=CIRCLE('',#72965,7.44636193257106);
#17156=CIRCLE('',#72966,7.44966353760313);
#17157=CIRCLE('',#72967,7.44636196148033);
#17158=CIRCLE('',#72968,7.44966316450105);
#17159=CIRCLE('',#72969,7.44412064297541);
#17160=CIRCLE('',#72970,7.44962090241967);
#17161=CIRCLE('',#72971,7.4441215350551);
#17162=CIRCLE('',#72972,7.44962092331308);
#17163=CIRCLE('',#72973,7.44412171359309);
#17164=CIRCLE('',#72974,7.44962088978136);
#17165=CIRCLE('',#72975,7.44412165693904);
#17166=CIRCLE('',#72976,7.44962101012671);
#17167=CIRCLE('',#72977,7.4441216951693);
#17168=CIRCLE('',#72978,7.44962106412852);
#17169=CIRCLE('',#72979,7.44412170714691);
#17170=CIRCLE('',#72980,7.44962091777948);
#17171=CIRCLE('',#72981,7.44412154598296);
#17172=CIRCLE('',#72982,7.44962075048608);
#17173=CIRCLE('',#72983,7.44412169947591);
#17174=CIRCLE('',#72984,7.44962100045847);
#17175=CIRCLE('',#72985,7.44412167599847);
#17176=CIRCLE('',#72986,7.44962064288898);
#17177=CIRCLE('',#72987,7.44412165364346);
#17178=CIRCLE('',#72988,7.44962107754941);
#17179=CIRCLE('',#72989,7.44412166787335);
#17180=CIRCLE('',#72990,7.44962103513019);
#17181=CIRCLE('',#72991,7.44412183980246);
#17182=CIRCLE('',#72992,7.44962107444732);
#17183=CIRCLE('',#72993,7.44412153534108);
#17184=CIRCLE('',#72994,7.44962093878989);
#17185=CIRCLE('',#72995,7.44412162026275);
#17186=CIRCLE('',#72996,7.44962091020999);
#17187=CIRCLE('',#72997,7.44412164711026);
#17188=CIRCLE('',#72998,7.44962099065294);
#17189=CIRCLE('',#72999,7.44412173822533);
#17190=CIRCLE('',#73000,7.44962082298734);
#17191=CIRCLE('',#73001,7.44412191483093);
#17192=CIRCLE('',#73002,7.44962083948565);
#17193=CIRCLE('',#73003,7.44412154563418);
#17194=CIRCLE('',#73004,7.44962079753425);
#17195=CIRCLE('',#73005,7.44412180227944);
#17196=CIRCLE('',#73006,7.44962074392226);
#17197=CIRCLE('',#73007,7.4441217413041);
#17198=CIRCLE('',#73008,7.44962098648014);
#17199=CIRCLE('',#73009,7.4441217944993);
#17200=CIRCLE('',#73010,7.44962123096037);
#17201=CIRCLE('',#73011,7.44412161325592);
#17202=CIRCLE('',#73012,7.44962082725039);
#17203=CIRCLE('',#73013,7.44412158112357);
#17204=CIRCLE('',#73014,7.44962082581323);
#17205=CIRCLE('',#73015,7.44412158351607);
#17206=CIRCLE('',#73016,7.44962097025443);
#17207=CIRCLE('',#73017,7.44412174516809);
#17208=CIRCLE('',#73018,7.449620984779);
#17209=CIRCLE('',#73019,7.44412175042324);
#17210=CIRCLE('',#73020,7.44962076526355);
#17211=CIRCLE('',#73021,7.44412154988149);
#17212=CIRCLE('',#73022,7.44962082790196);
#17213=CIRCLE('',#73023,7.44412180935468);
#17214=CIRCLE('',#73024,7.44962098873196);
#17215=CIRCLE('',#73025,7.44412180009209);
#17216=CIRCLE('',#73026,7.44962076564967);
#17217=CIRCLE('',#73027,7.68881312209984);
#17218=CIRCLE('',#73028,7.69305842670495);
#17219=CIRCLE('',#73030,7.69135459595439);
#17220=CIRCLE('',#73031,7.68881305425059);
#17221=CIRCLE('',#73032,7.69305851563742);
#17222=CIRCLE('',#73034,7.69135469458866);
#17223=CIRCLE('',#73035,7.68881318241118);
#17224=CIRCLE('',#73036,7.69305837521999);
#17225=CIRCLE('',#73038,7.6913545638551);
#17226=CIRCLE('',#73039,7.68881306332511);
#17227=CIRCLE('',#73040,7.69305860510658);
#17228=CIRCLE('',#73042,7.69135444682733);
#17229=CIRCLE('',#73043,7.6888132919626);
#17230=CIRCLE('',#73044,7.69305837123098);
#17231=CIRCLE('',#73046,7.6913547963529);
#17232=CIRCLE('',#73047,7.68881303446479);
#17233=CIRCLE('',#73048,7.69305857205603);
#17234=CIRCLE('',#73050,7.69135467139072);
#17235=CIRCLE('',#73051,7.68881305751141);
#17236=CIRCLE('',#73052,7.6930583711798);
#17237=CIRCLE('',#73054,7.6913546819479);
#17238=CIRCLE('',#73055,7.68881287342277);
#17239=CIRCLE('',#73056,7.69305844639685);
#17240=CIRCLE('',#73058,7.691354832468);
#17241=CIRCLE('',#73059,7.68881313161581);
#17242=CIRCLE('',#73060,7.69305848534483);
#17243=CIRCLE('',#73062,7.69135483048795);
#17244=CIRCLE('',#73063,7.68881313584477);
#17245=CIRCLE('',#73064,7.69305850720062);
#17246=CIRCLE('',#73066,7.69135459145652);
#17247=CIRCLE('',#73067,7.68881274573051);
#17248=CIRCLE('',#73068,7.69305864966813);
#17249=CIRCLE('',#73070,7.69135463961226);
#17250=CIRCLE('',#73071,7.68881325189327);
#17251=CIRCLE('',#73072,7.69305821213215);
#17252=CIRCLE('',#73074,7.69135477789806);
#17253=CIRCLE('',#73075,7.68881285340086);
#17254=CIRCLE('',#73076,7.69305846026459);
#17255=CIRCLE('',#73078,7.69135472284591);
#17256=CIRCLE('',#73079,7.68881300396549);
#17257=CIRCLE('',#73080,7.69305817498246);
#17258=CIRCLE('',#73082,7.69135445363307);
#17259=CIRCLE('',#73083,7.68881275452915);
#17260=CIRCLE('',#73084,7.69305861452194);
#17261=CIRCLE('',#73086,7.69135457467286);
#17262=CIRCLE('',#73087,7.68881303796674);
#17263=CIRCLE('',#73088,7.69305858517097);
#17264=CIRCLE('',#73090,7.69135473804609);
#17265=CIRCLE('',#73091,7.68881291061956);
#17266=CIRCLE('',#73092,7.69305851660632);
#17267=CIRCLE('',#73094,7.69135491750274);
#17268=CIRCLE('',#73095,7.68881294783481);
#17269=CIRCLE('',#73096,7.69305865774133);
#17270=CIRCLE('',#73098,7.69135446595735);
#17271=CIRCLE('',#73099,7.68881286359618);
#17272=CIRCLE('',#73100,7.69305865167506);
#17273=CIRCLE('',#73102,7.69135477608768);
#17274=CIRCLE('',#73103,7.6888131570718);
#17275=CIRCLE('',#73104,7.69305841221193);
#17276=CIRCLE('',#73106,7.69135474309799);
#17277=CIRCLE('',#73107,7.68881310973368);
#17278=CIRCLE('',#73108,7.693058486018);
#17279=CIRCLE('',#73110,7.69135458482537);
#17280=CIRCLE('',#73111,7.68881304034411);
#17281=CIRCLE('',#73112,7.69305845743024);
#17282=CIRCLE('',#73113,7.68880897371152);
#17283=CIRCLE('',#73115,7.69135060068296);
#17284=CIRCLE('',#73116,7.69305863217014);
#17285=CIRCLE('',#73118,7.68881291601433);
#17286=CIRCLE('',#73119,7.69135469952759);
#17287=CIRCLE('',#73120,7.6930583361325);
#17288=CIRCLE('',#73122,7.69135444944665);
#17289=CIRCLE('',#73123,7.68881281368828);
#17290=CIRCLE('',#73124,7.69305827499903);
#17291=CIRCLE('',#73126,7.69135481642152);
#17292=CIRCLE('',#73127,7.68881286880164);
#17293=CIRCLE('',#73128,7.69305845317125);
#17294=CIRCLE('',#73130,7.69135474107584);
#17295=CIRCLE('',#73131,7.68881279052987);
#17296=CIRCLE('',#73132,7.69305840144874);
#17297=CIRCLE('',#73134,7.69135464328283);
#17298=CIRCLE('',#73135,7.68881294976904);
#17299=CIRCLE('',#73137,7.69135478455158);
#17300=CIRCLE('',#73138,7.6930585711826);
#17301=CIRCLE('',#73139,7.68894221452859);
#17302=CIRCLE('',#73140,7.69306082816528);
#17303=CIRCLE('',#73141,7.68894221816495);
#17304=CIRCLE('',#73143,7.69254652221787);
#17305=CIRCLE('',#73144,7.69154668134093);
#17306=CIRCLE('',#73145,7.69306103162729);
#17307=CIRCLE('',#73146,7.6889420578582);
#17308=CIRCLE('',#73148,7.69254632751691);
#17309=CIRCLE('',#73149,7.69154676522241);
#17310=CIRCLE('',#73150,7.69306084786072);
#17311=CIRCLE('',#73151,7.68894212344255);
#17312=CIRCLE('',#73153,7.69254629177713);
#17313=CIRCLE('',#73154,7.69154659721445);
#17314=CIRCLE('',#73155,7.69306125634641);
#17315=CIRCLE('',#73156,7.68894230414718);
#17316=CIRCLE('',#73158,7.69254630396056);
#17317=CIRCLE('',#73159,7.69154657372904);
#17318=CIRCLE('',#73160,7.6930610465379);
#17319=CIRCLE('',#73161,7.68894215940438);
#17320=CIRCLE('',#73163,7.69254651455718);
#17321=CIRCLE('',#73164,7.69154664597915);
#17322=CIRCLE('',#73165,7.6930611839578);
#17323=CIRCLE('',#73166,7.68894243281189);
#17324=CIRCLE('',#73168,7.69254635990402);
#17325=CIRCLE('',#73169,7.69154701073923);
#17326=CIRCLE('',#73170,7.69306102466985);
#17327=CIRCLE('',#73171,7.68894235114808);
#17328=CIRCLE('',#73173,7.69254624235975);
#17329=CIRCLE('',#73174,7.69154685393794);
#17330=CIRCLE('',#73175,7.69306122370397);
#17331=CIRCLE('',#73176,7.68894225719054);
#17332=CIRCLE('',#73178,7.69254660064401);
#17333=CIRCLE('',#73179,7.69154666639614);
#17334=CIRCLE('',#73180,7.69306112112687);
#17335=CIRCLE('',#73181,7.68894206668824);
#17336=CIRCLE('',#73183,7.69254659939187);
#17337=CIRCLE('',#73184,7.69154686958469);
#17338=CIRCLE('',#73185,7.69306098589994);
#17339=CIRCLE('',#73186,7.68894212480211);
#17340=CIRCLE('',#73188,7.69254664269419);
#17341=CIRCLE('',#73189,7.6915468406462);
#17342=CIRCLE('',#73190,7.69306087910567);
#17343=CIRCLE('',#73191,7.68894223701859);
#17344=CIRCLE('',#73193,7.6925462252469);
#17345=CIRCLE('',#73194,7.69154650914596);
#17346=CIRCLE('',#73195,7.6930609492561);
#17347=CIRCLE('',#73196,7.68894231759131);
#17348=CIRCLE('',#73198,7.69254645363533);
#17349=CIRCLE('',#73199,7.69154672029993);
#17350=CIRCLE('',#73200,7.69306078197452);
#17351=CIRCLE('',#73201,7.68894223814822);
#17352=CIRCLE('',#73203,7.69254661875416);
#17353=CIRCLE('',#73204,7.69154666835679);
#17354=CIRCLE('',#73205,7.69306108280045);
#17355=CIRCLE('',#73206,7.68894225175114);
#17356=CIRCLE('',#73208,7.69254659523722);
#17357=CIRCLE('',#73209,7.69154671923709);
#17358=CIRCLE('',#73210,7.69306124540043);
#17359=CIRCLE('',#73211,7.68894227989443);
#17360=CIRCLE('',#73213,7.69254654866584);
#17361=CIRCLE('',#73214,7.69154673015789);
#17362=CIRCLE('',#73215,7.69306085198288);
#17363=CIRCLE('',#73216,7.68894237178344);
#17364=CIRCLE('',#73218,7.69254635163619);
#17365=CIRCLE('',#73219,7.69154667037883);
#17366=CIRCLE('',#73220,7.6930607036298);
#17367=CIRCLE('',#73221,7.68894226104312);
#17368=CIRCLE('',#73223,7.6925464256185);
#17369=CIRCLE('',#73224,7.69154653529051);
#17370=CIRCLE('',#73225,7.69306131397639);
#17371=CIRCLE('',#73226,7.68894236076532);
#17372=CIRCLE('',#73228,7.69254629704884);
#17373=CIRCLE('',#73229,7.69154704329205);
#17374=CIRCLE('',#73230,7.69306084621818);
#17375=CIRCLE('',#73231,7.68894221484235);
#17376=CIRCLE('',#73233,7.69254616738453);
#17377=CIRCLE('',#73234,7.69154684700041);
#17378=CIRCLE('',#73235,7.69306089555524);
#17379=CIRCLE('',#73236,7.68894233735332);
#17380=CIRCLE('',#73238,7.69254632399395);
#17381=CIRCLE('',#73239,7.69154679094549);
#17382=CIRCLE('',#73240,7.69306100859483);
#17383=CIRCLE('',#73241,7.688942330024);
#17384=CIRCLE('',#73243,7.69254642332663);
#17385=CIRCLE('',#73244,7.69154660688702);
#17386=CIRCLE('',#73245,7.69306118917124);
#17387=CIRCLE('',#73246,7.68894225546997);
#17388=CIRCLE('',#73248,7.69254635523657);
#17389=CIRCLE('',#73249,7.69154694744465);
#17390=CIRCLE('',#73250,7.69306111921035);
#17391=CIRCLE('',#73251,7.68894236019955);
#17392=CIRCLE('',#73253,7.69254652854155);
#17393=CIRCLE('',#73254,7.69154674961277);
#17394=CIRCLE('',#73255,7.69306115184591);
#17395=CIRCLE('',#73256,7.68894222237977);
#17396=CIRCLE('',#73258,7.69254640727368);
#17397=CIRCLE('',#73259,7.69154705511724);
#17398=CIRCLE('',#73260,7.69306111025);
#17399=CIRCLE('',#73261,7.68894239205181);
#17400=CIRCLE('',#73263,7.69254643702591);
#17401=CIRCLE('',#73264,7.69154660575477);
#17402=CIRCLE('',#73265,7.6930610882171);
#17403=CIRCLE('',#73266,7.68894240872928);
#17404=CIRCLE('',#73268,7.69254646618558);
#17405=CIRCLE('',#73269,7.69154672452396);
#17406=CIRCLE('',#73270,7.69306091823566);
#17407=CIRCLE('',#73271,7.68894250390556);
#17408=CIRCLE('',#73273,7.69254667871653);
#17409=CIRCLE('',#73274,7.69154653598979);
#17410=CIRCLE('',#73276,7.69254664694874);
#17411=CIRCLE('',#73277,7.69154682436781);
#17412=CIRCLE('',#73278,7.69306105800644);
#17413=CIRCLE('',#73279,7.44703740601364);
#17414=CIRCLE('',#73280,7.4470374662542);
#17415=CIRCLE('',#73281,7.44703745308987);
#17416=CIRCLE('',#73282,7.44703753082965);
#17417=CIRCLE('',#73283,7.4470375186082);
#17418=CIRCLE('',#73284,7.44703758994448);
#17419=CIRCLE('',#73285,7.4470372444609);
#17420=CIRCLE('',#73286,7.44703762283394);
#17421=CIRCLE('',#73287,7.44703741449571);
#17422=CIRCLE('',#73288,7.44703755754407);
#17423=CIRCLE('',#73289,7.447037331955);
#17424=CIRCLE('',#73290,7.44703753013713);
#17425=CIRCLE('',#73291,7.44703748809038);
#17426=CIRCLE('',#73292,7.44703751023184);
#17427=CIRCLE('',#73293,7.44703743975908);
#17428=CIRCLE('',#73294,7.44703768317363);
#17429=CIRCLE('',#73295,7.44703743497953);
#17430=CIRCLE('',#73296,7.44703737548807);
#17431=CIRCLE('',#73297,7.44703772608559);
#17432=CIRCLE('',#73298,7.44703746302606);
#17433=CIRCLE('',#73299,7.44703734354391);
#17434=CIRCLE('',#73300,7.44703742894028);
#17435=CIRCLE('',#73301,7.44703756648655);
#17436=CIRCLE('',#73302,7.44703765672143);
#17437=CIRCLE('',#73303,7.44703750735441);
#17438=CIRCLE('',#73304,7.44703734033849);
#17439=CIRCLE('',#73305,7.44703728947688);
#17440=CIRCLE('',#73306,7.4470374059196);
#17441=CIRCLE('',#73307,7.44703765920018);
#17442=CIRCLE('',#73308,7.44726855569365);
#17443=CIRCLE('',#73309,7.44947025413789);
#17444=CIRCLE('',#73310,7.44726912411424);
#17445=CIRCLE('',#73311,7.44947031904609);
#17446=CIRCLE('',#73312,7.44726886787919);
#17447=CIRCLE('',#73313,7.4494704190352);
#17448=CIRCLE('',#73314,7.44726899435415);
#17449=CIRCLE('',#73315,7.44947048644738);
#17450=CIRCLE('',#73316,7.44726892731604);
#17451=CIRCLE('',#73317,7.44947035672239);
#17452=CIRCLE('',#73318,7.44726884235559);
#17453=CIRCLE('',#73319,7.44947051052393);
#17454=CIRCLE('',#73320,7.4472689609866);
#17455=CIRCLE('',#73321,7.44947032882476);
#17456=CIRCLE('',#73322,7.44726899765268);
#17457=CIRCLE('',#73323,7.44947053089078);
#17458=CIRCLE('',#73324,7.44726900882362);
#17459=CIRCLE('',#73325,7.44947043308556);
#17460=CIRCLE('',#73326,7.447269063795);
#17461=CIRCLE('',#73327,7.44947037014586);
#17462=CIRCLE('',#73328,7.44726913176407);
#17463=CIRCLE('',#73329,7.44947038677827);
#17464=CIRCLE('',#73330,7.44726899307883);
#17465=CIRCLE('',#73331,7.44947034090865);
#17466=CIRCLE('',#73332,7.44726925582051);
#17467=CIRCLE('',#73333,7.4494704560085);
#17468=CIRCLE('',#73334,7.44726916809589);
#17469=CIRCLE('',#73335,7.44947023321686);
#17470=CIRCLE('',#73336,7.44726899142159);
#17471=CIRCLE('',#73337,7.44947051639951);
#17472=CIRCLE('',#73338,7.44726916275001);
#17473=CIRCLE('',#73339,7.44947054644409);
#17474=CIRCLE('',#73340,7.44726926857587);
#17475=CIRCLE('',#73341,7.44947038945824);
#17476=CIRCLE('',#73342,7.44726894258526);
#17477=CIRCLE('',#73343,7.44947028478043);
#17478=CIRCLE('',#73344,7.44726903924242);
#17479=CIRCLE('',#73345,7.44947057242217);
#17480=CIRCLE('',#73346,7.44726901770602);
#17481=CIRCLE('',#73347,7.44947031239464);
#17482=CIRCLE('',#73348,7.4472693195082);
#17483=CIRCLE('',#73349,7.44947052977426);
#17484=CIRCLE('',#73350,7.44726918026073);
#17485=CIRCLE('',#73351,7.44947047782821);
#17486=CIRCLE('',#73352,7.44726905731159);
#17487=CIRCLE('',#73353,7.44947040140385);
#17488=CIRCLE('',#73354,7.44726922475979);
#17489=CIRCLE('',#73355,7.44947025629113);
#17490=CIRCLE('',#73356,7.44726901139042);
#17491=CIRCLE('',#73357,7.4494704667677);
#17492=CIRCLE('',#73358,7.44726890407121);
#17493=CIRCLE('',#73359,7.44947024139069);
#17494=CIRCLE('',#73360,7.44726911447529);
#17495=CIRCLE('',#73361,7.44947035700436);
#17496=CIRCLE('',#73362,7.44726922435685);
#17497=CIRCLE('',#73363,7.44947055337701);
#17498=CIRCLE('',#73364,7.44726892731434);
#17499=CIRCLE('',#73365,7.44947046068327);
#17500=CIRCLE('',#73366,7.68957748773136);
#17501=CIRCLE('',#73368,7.68734493565065);
#17502=CIRCLE('',#73369,7.68318405249157);
#17503=CIRCLE('',#73370,7.68957748458392);
#17504=CIRCLE('',#73372,7.68734489624771);
#17505=CIRCLE('',#73373,7.68318437103348);
#17506=CIRCLE('',#73374,7.68957744086419);
#17507=CIRCLE('',#73376,7.68734517552602);
#17508=CIRCLE('',#73377,7.68318459103349);
#17509=CIRCLE('',#73378,7.68957743242436);
#17510=CIRCLE('',#73380,7.68734491438801);
#17511=CIRCLE('',#73381,7.68318419339124);
#17512=CIRCLE('',#73382,7.68957745052179);
#17513=CIRCLE('',#73384,7.68734521661807);
#17514=CIRCLE('',#73385,7.68318455697533);
#17515=CIRCLE('',#73386,7.68957749671537);
#17516=CIRCLE('',#73388,7.68734510049166);
#17517=CIRCLE('',#73389,7.68318476711861);
#17518=CIRCLE('',#73390,7.68957725009669);
#17519=CIRCLE('',#73392,7.68734508539297);
#17520=CIRCLE('',#73393,7.68318416167277);
#17521=CIRCLE('',#73394,7.68957754605477);
#17522=CIRCLE('',#73396,7.68734531279094);
#17523=CIRCLE('',#73397,7.68318447137342);
#17524=CIRCLE('',#73398,7.68957743776089);
#17525=CIRCLE('',#73400,7.68734503598025);
#17526=CIRCLE('',#73401,7.68318432152863);
#17527=CIRCLE('',#73402,7.68957747820737);
#17528=CIRCLE('',#73404,7.68734493513009);
#17529=CIRCLE('',#73405,7.68318409703447);
#17530=CIRCLE('',#73406,7.68957705118966);
#17531=CIRCLE('',#73408,7.68734522406006);
#17532=CIRCLE('',#73409,7.6831844819381);
#17533=CIRCLE('',#73410,7.68957752053836);
#17534=CIRCLE('',#73412,7.68734483074303);
#17535=CIRCLE('',#73413,7.68318425943268);
#17536=CIRCLE('',#73414,7.6895774318264);
#17537=CIRCLE('',#73416,7.68734525206946);
#17538=CIRCLE('',#73417,7.68318481127215);
#17539=CIRCLE('',#73418,7.6895775763399);
#17540=CIRCLE('',#73420,7.68734508461849);
#17541=CIRCLE('',#73421,7.68318462759078);
#17542=CIRCLE('',#73422,7.68957738759692);
#17543=CIRCLE('',#73424,7.68734522525487);
#17544=CIRCLE('',#73425,7.68318434353235);
#17545=CIRCLE('',#73426,7.68957724595044);
#17546=CIRCLE('',#73428,7.68734506964628);
#17547=CIRCLE('',#73429,7.68318443245175);
#17548=CIRCLE('',#73430,7.68957738309765);
#17549=CIRCLE('',#73432,7.68734504312503);
#17550=CIRCLE('',#73433,7.68318397319927);
#17551=CIRCLE('',#73434,7.68957728912674);
#17552=CIRCLE('',#73436,7.68734509419147);
#17553=CIRCLE('',#73437,7.68318426666675);
#17554=CIRCLE('',#73438,7.68957758500744);
#17555=CIRCLE('',#73440,7.68734497218318);
#17556=CIRCLE('',#73441,7.68318482091028);
#17557=CIRCLE('',#73442,7.68957729276197);
#17558=CIRCLE('',#73444,7.6873448380935);
#17559=CIRCLE('',#73445,7.68318452630792);
#17560=CIRCLE('',#73446,7.68957752851105);
#17561=CIRCLE('',#73448,7.68734510837944);
#17562=CIRCLE('',#73449,7.68318408620418);
#17563=CIRCLE('',#73450,7.68957715464276);
#17564=CIRCLE('',#73452,7.68734514858287);
#17565=CIRCLE('',#73453,7.68318398809372);
#17566=CIRCLE('',#73454,7.68957737159601);
#17567=CIRCLE('',#73456,7.68734517557214);
#17568=CIRCLE('',#73457,7.68318447990036);
#17569=CIRCLE('',#73458,7.68957741388642);
#17570=CIRCLE('',#73460,7.68734505044421);
#17571=CIRCLE('',#73461,7.68318420939938);
#17572=CIRCLE('',#73462,7.68957728276303);
#17573=CIRCLE('',#73464,7.68734508066004);
#17574=CIRCLE('',#73465,7.68318447973266);
#17575=CIRCLE('',#73466,7.68957727092898);
#17576=CIRCLE('',#73468,7.6873452387982);
#17577=CIRCLE('',#73469,7.68318471227011);
#17578=CIRCLE('',#73470,7.68957735899398);
#17579=CIRCLE('',#73472,7.68734495766267);
#17580=CIRCLE('',#73473,7.68318431078746);
#17581=CIRCLE('',#73474,7.68957718057119);
#17582=CIRCLE('',#73476,7.68734532714596);
#17583=CIRCLE('',#73477,7.68318490909885);
#17584=CIRCLE('',#73478,7.68983489396897);
#17585=CIRCLE('',#73479,7.69301696143299);
#17586=CIRCLE('',#73481,7.69198148285114);
#17587=CIRCLE('',#73482,7.6835593980278);
#17588=CIRCLE('',#73483,7.68983488140878);
#17589=CIRCLE('',#73484,7.6930165800384);
#17590=CIRCLE('',#73486,7.69198186433056);
#17591=CIRCLE('',#73487,7.68355933601086);
#17592=CIRCLE('',#73488,7.6898349856185);
#17593=CIRCLE('',#73489,7.69301671090392);
#17594=CIRCLE('',#73491,7.69198175834686);
#17595=CIRCLE('',#73492,7.6835588366298);
#17596=CIRCLE('',#73493,7.68983478878477);
#17597=CIRCLE('',#73494,7.69301677755821);
#17598=CIRCLE('',#73496,7.6919818100264);
#17599=CIRCLE('',#73497,7.68355962336939);
#17600=CIRCLE('',#73498,7.68983500365314);
#17601=CIRCLE('',#73499,7.69301670443458);
#17602=CIRCLE('',#73501,7.69198173167657);
#17603=CIRCLE('',#73502,7.68355934414267);
#17604=CIRCLE('',#73503,7.68983492418413);
#17605=CIRCLE('',#73504,7.69301683580422);
#17606=CIRCLE('',#73506,7.69198163514051);
#17607=CIRCLE('',#73507,7.6835589110352);
#17608=CIRCLE('',#73508,7.68983487983782);
#17609=CIRCLE('',#73509,7.69301657714507);
#17610=CIRCLE('',#73511,7.69198183398963);
#17611=CIRCLE('',#73512,7.68355883494166);
#17612=CIRCLE('',#73513,7.68983489291763);
#17613=CIRCLE('',#73514,7.6930169715151);
#17614=CIRCLE('',#73516,7.69198147194979);
#17615=CIRCLE('',#73517,7.68355917426551);
#17616=CIRCLE('',#73518,7.68983510882082);
#17617=CIRCLE('',#73519,7.69301663246352);
#17618=CIRCLE('',#73521,7.69198163455624);
#17619=CIRCLE('',#73522,7.68355943924273);
#17620=CIRCLE('',#73523,7.68983479825435);
#17621=CIRCLE('',#73524,7.69301681989919);
#17622=CIRCLE('',#73526,7.6919815043616);
#17623=CIRCLE('',#73527,7.68355894458752);
#17624=CIRCLE('',#73528,7.6898351140751);
#17625=CIRCLE('',#73529,7.69301671501356);
#17626=CIRCLE('',#73531,7.69198167371706);
#17627=CIRCLE('',#73532,7.68355932858418);
#17628=CIRCLE('',#73533,7.68983517939378);
#17629=CIRCLE('',#73534,7.69301664922328);
#17630=CIRCLE('',#73536,7.69198155170029);
#17631=CIRCLE('',#73537,7.68355932581089);
#17632=CIRCLE('',#73538,7.68983489071601);
#17633=CIRCLE('',#73539,7.69301679907012);
#17634=CIRCLE('',#73541,7.69198165345984);
#17635=CIRCLE('',#73542,7.68355935171591);
#17636=CIRCLE('',#73543,7.68983486491984);
#17637=CIRCLE('',#73544,7.6930167136401);
#17638=CIRCLE('',#73546,7.69198156882893);
#17639=CIRCLE('',#73547,7.68355931944083);
#17640=CIRCLE('',#73548,7.6898350257074);
#17641=CIRCLE('',#73549,7.69301667356443);
#17642=CIRCLE('',#73551,7.69198166635035);
#17643=CIRCLE('',#73552,7.68355902854595);
#17644=CIRCLE('',#73553,7.68983514730196);
#17645=CIRCLE('',#73554,7.69301661826608);
#17646=CIRCLE('',#73556,7.69198176951274);
#17647=CIRCLE('',#73557,7.68355940594295);
#17648=CIRCLE('',#73558,7.6898350638292);
#17649=CIRCLE('',#73559,7.69301659660404);
#17650=CIRCLE('',#73561,7.69198160962702);
#17651=CIRCLE('',#73562,7.68355913972534);
#17652=CIRCLE('',#73563,7.68983478759058);
#17653=CIRCLE('',#73564,7.69301692248647);
#17654=CIRCLE('',#73566,7.6919815430316);
#17655=CIRCLE('',#73567,7.68355907541356);
#17656=CIRCLE('',#73568,7.68983480591283);
#17657=CIRCLE('',#73569,7.6930166833839);
#17658=CIRCLE('',#73571,7.69198180730898);
#17659=CIRCLE('',#73572,7.68355879276394);
#17660=CIRCLE('',#73573,7.68983495333692);
#17661=CIRCLE('',#73574,7.69301663935876);
#17662=CIRCLE('',#73576,7.69198160697219);
#17663=CIRCLE('',#73577,7.68355894623691);
#17664=CIRCLE('',#73578,7.68983489183394);
#17665=CIRCLE('',#73579,7.69301656700983);
#17666=CIRCLE('',#73581,7.69198148895534);
#17667=CIRCLE('',#73582,7.68355875344865);
#17668=CIRCLE('',#73583,7.68983508864516);
#17669=CIRCLE('',#73584,7.69301691731102);
#17670=CIRCLE('',#73586,7.69198162591986);
#17671=CIRCLE('',#73587,7.68355909405863);
#17672=CIRCLE('',#73588,7.68983508237929);
#17673=CIRCLE('',#73589,7.69301673454273);
#17674=CIRCLE('',#73591,7.69198177259239);
#17675=CIRCLE('',#73592,7.68355939897891);
#17676=CIRCLE('',#73593,7.68983525272473);
#17677=CIRCLE('',#73594,7.69301685764793);
#17678=CIRCLE('',#73596,7.69198163217241);
#17679=CIRCLE('',#73597,7.68355943041218);
#17680=CIRCLE('',#73598,7.68983498373113);
#17681=CIRCLE('',#73599,7.69301670508415);
#17682=CIRCLE('',#73601,7.69198185871811);
#17683=CIRCLE('',#73602,7.68355915919088);
#17684=CIRCLE('',#73603,7.6898348611317);
#17685=CIRCLE('',#73604,7.69301693833565);
#17686=CIRCLE('',#73606,7.69198149127824);
#17687=CIRCLE('',#73607,7.68355944766628);
#17688=CIRCLE('',#73608,7.68983495953567);
#17689=CIRCLE('',#73609,7.69301672696527);
#17690=CIRCLE('',#73611,7.69198153689078);
#17691=CIRCLE('',#73612,7.68355905642999);
#17692=CIRCLE('',#73613,7.68983511208836);
#17693=CIRCLE('',#73614,7.69301685417526);
#17694=CIRCLE('',#73616,7.69198149366435);
#17695=CIRCLE('',#73617,7.68355961099684);
#17696=CIRCLE('',#73618,7.4450188933114);
#17697=CIRCLE('',#73619,7.44501890449599);
#17698=CIRCLE('',#73620,7.44501879756203);
#17699=CIRCLE('',#73621,7.44501861859603);
#17700=CIRCLE('',#73622,7.44501870669753);
#17701=CIRCLE('',#73623,7.44501871524855);
#17702=CIRCLE('',#73624,7.44501858121209);
#17703=CIRCLE('',#73625,7.44501866536265);
#17704=CIRCLE('',#73626,7.44501872599696);
#17705=CIRCLE('',#73627,7.44501856118857);
#17706=CIRCLE('',#73628,7.44501846236666);
#17707=CIRCLE('',#73629,7.445018651669);
#17708=CIRCLE('',#73630,7.44501885804999);
#17709=CIRCLE('',#73631,7.44501884348547);
#17710=CIRCLE('',#73632,7.44501853237831);
#17711=CIRCLE('',#73633,7.44501869383856);
#17712=CIRCLE('',#73634,7.44501879936885);
#17713=CIRCLE('',#73635,7.44501890514634);
#17714=CIRCLE('',#73636,7.44501858495637);
#17715=CIRCLE('',#73637,7.4450186247389);
#17716=CIRCLE('',#73638,7.44501880900192);
#17717=CIRCLE('',#73639,7.44501880897738);
#17718=CIRCLE('',#73640,7.44501868801496);
#17719=CIRCLE('',#73641,7.44501845999727);
#17720=CIRCLE('',#73642,7.44501866742756);
#17721=CIRCLE('',#73643,7.44501869596626);
#17722=CIRCLE('',#73644,7.44501881893982);
#17723=CIRCLE('',#73645,7.44501863612009);
#17724=CIRCLE('',#73646,7.44501877643286);
#17725=CIRCLE('',#73647,7.44783687688711);
#17726=CIRCLE('',#73648,7.44783621953896);
#17727=CIRCLE('',#73649,7.44783669832343);
#17728=CIRCLE('',#73650,7.44783643383807);
#17729=CIRCLE('',#73651,7.44783642389326);
#17730=CIRCLE('',#73652,7.44783654872719);
#17731=CIRCLE('',#73653,7.44783637644797);
#17732=CIRCLE('',#73654,7.44783635948184);
#17733=CIRCLE('',#73655,7.4478365441613);
#17734=CIRCLE('',#73656,7.44783669119075);
#17735=CIRCLE('',#73657,7.44783686377082);
#17736=CIRCLE('',#73658,7.44783656581571);
#17737=CIRCLE('',#73659,7.44783643994268);
#17738=CIRCLE('',#73660,7.44783624491067);
#17739=CIRCLE('',#73661,7.44783654854467);
#17740=CIRCLE('',#73662,7.44783673428636);
#17741=CIRCLE('',#73663,7.44783662736838);
#17742=CIRCLE('',#73664,7.44783654086163);
#17743=CIRCLE('',#73665,7.44783627414982);
#17744=CIRCLE('',#73666,7.44783632320642);
#17745=CIRCLE('',#73667,7.4478366598755);
#17746=CIRCLE('',#73668,7.4478368763373);
#17747=CIRCLE('',#73669,7.44783643817806);
#17748=CIRCLE('',#73670,7.44783634404276);
#17749=CIRCLE('',#73671,7.44783650547921);
#17750=CIRCLE('',#73672,7.44783628390043);
#17751=CIRCLE('',#73673,7.44783629608604);
#17752=CIRCLE('',#73674,7.44783649178178);
#17753=CIRCLE('',#73675,7.44783649132846);
#17754=CIRCLE('',#73676,7.68969363660472);
#17755=CIRCLE('',#73678,7.69279317840802);
#17756=CIRCLE('',#73679,7.68635996865851);
#17757=CIRCLE('',#73680,7.68969386660789);
#17758=CIRCLE('',#73682,7.69279302868398);
#17759=CIRCLE('',#73683,7.68635995762749);
#17760=CIRCLE('',#73684,7.6896936900641);
#17761=CIRCLE('',#73686,7.69279326824012);
#17762=CIRCLE('',#73687,7.68635976553776);
#17763=CIRCLE('',#73688,7.68969386253329);
#17764=CIRCLE('',#73690,7.69279334574968);
#17765=CIRCLE('',#73691,7.68635983205112);
#17766=CIRCLE('',#73692,7.68969375114687);
#17767=CIRCLE('',#73694,7.69279335413577);
#17768=CIRCLE('',#73695,7.68636002466187);
#17769=CIRCLE('',#73696,7.68969359649545);
#17770=CIRCLE('',#73698,7.69279335917638);
#17771=CIRCLE('',#73699,7.68635978519035);
#17772=CIRCLE('',#73700,7.68969373989023);
#17773=CIRCLE('',#73702,7.69279333421998);
#17774=CIRCLE('',#73703,7.68636003724103);
#17775=CIRCLE('',#73704,7.68969374098561);
#17776=CIRCLE('',#73706,7.69279339904735);
#17777=CIRCLE('',#73707,7.68635982561929);
#17778=CIRCLE('',#73708,7.68969385681376);
#17779=CIRCLE('',#73710,7.69279310456421);
#17780=CIRCLE('',#73711,7.68636023014239);
#17781=CIRCLE('',#73712,7.68969387721714);
#17782=CIRCLE('',#73714,7.69279308553252);
#17783=CIRCLE('',#73715,7.68635990825226);
#17784=CIRCLE('',#73716,7.68969389757644);
#17785=CIRCLE('',#73718,7.69279299440528);
#17786=CIRCLE('',#73719,7.68636005141107);
#17787=CIRCLE('',#73720,7.68969366115901);
#17788=CIRCLE('',#73722,7.69279333913911);
#17789=CIRCLE('',#73723,7.68635983689438);
#17790=CIRCLE('',#73724,7.6896937696048);
#17791=CIRCLE('',#73726,7.69279311454176);
#17792=CIRCLE('',#73727,7.68635991851817);
#17793=CIRCLE('',#73728,7.68969363397531);
#17794=CIRCLE('',#73730,7.69279332251533);
#17795=CIRCLE('',#73731,7.68635998349788);
#17796=CIRCLE('',#73732,7.68969374897493);
#17797=CIRCLE('',#73734,7.69279337928139);
#17798=CIRCLE('',#73735,7.68635971742891);
#17799=CIRCLE('',#73736,7.6896937771446);
#17800=CIRCLE('',#73738,7.69279344747408);
#17801=CIRCLE('',#73739,7.68635974620921);
#17802=CIRCLE('',#73740,7.68969377094987);
#17803=CIRCLE('',#73742,7.692793522416);
#17804=CIRCLE('',#73743,7.6863598904576);
#17805=CIRCLE('',#73744,7.68969376075281);
#17806=CIRCLE('',#73746,7.6927931364953);
#17807=CIRCLE('',#73747,7.68636010655716);
#17808=CIRCLE('',#73748,7.68969359457469);
#17809=CIRCLE('',#73750,7.69279307209504);
#17810=CIRCLE('',#73751,7.6863600924503);
#17811=CIRCLE('',#73752,7.68969379778712);
#17812=CIRCLE('',#73754,7.6927930664211);
#17813=CIRCLE('',#73755,7.68635987732735);
#17814=CIRCLE('',#73756,7.68969392003808);
#17815=CIRCLE('',#73757,7.6896908311552);
#17816=CIRCLE('',#73759,7.69279329720953);
#17817=CIRCLE('',#73760,7.68635720976654);
#17818=CIRCLE('',#73762,7.68969386605261);
#17819=CIRCLE('',#73763,7.69279319432287);
#17820=CIRCLE('',#73764,7.68636009881248);
#17821=CIRCLE('',#73766,7.6927933916593);
#17822=CIRCLE('',#73767,7.68635984579723);
#17823=CIRCLE('',#73768,7.68969363382393);
#17824=CIRCLE('',#73770,7.69279330196327);
#17825=CIRCLE('',#73771,7.68635971171485);
#17826=CIRCLE('',#73772,7.68969361013494);
#17827=CIRCLE('',#73774,7.69279321901403);
#17828=CIRCLE('',#73775,7.68636012112819);
#17829=CIRCLE('',#73776,7.68969391216473);
#17830=CIRCLE('',#73778,7.69279317458319);
#17831=CIRCLE('',#73779,7.68635964597867);
#17832=CIRCLE('',#73780,7.68969355089801);
#17833=CIRCLE('',#73782,7.69279340184492);
#17834=CIRCLE('',#73783,7.68635993568266);
#17835=CIRCLE('',#73784,7.68969386466671);
#17836=CIRCLE('',#73786,7.6927931617596);
#17837=CIRCLE('',#73787,7.68635979372616);
#17838=CIRCLE('',#73788,7.69049143301784);
#17839=CIRCLE('',#73789,7.69049161415286);
#17840=CIRCLE('',#73791,7.68475569860886);
#17841=CIRCLE('',#73792,7.68602741023802);
#17842=CIRCLE('',#73793,7.69049152140508);
#17843=CIRCLE('',#73795,7.68475572981308);
#17844=CIRCLE('',#73796,7.68602772638459);
#17845=CIRCLE('',#73797,7.69049160139286);
#17846=CIRCLE('',#73799,7.6847557150075);
#17847=CIRCLE('',#73800,7.68602747013878);
#17848=CIRCLE('',#73801,7.69049165362067);
#17849=CIRCLE('',#73803,7.68475539161247);
#17850=CIRCLE('',#73804,7.68602763473392);
#17851=CIRCLE('',#73805,7.69049185324544);
#17852=CIRCLE('',#73807,7.68475566956591);
#17853=CIRCLE('',#73808,7.68602761290782);
#17854=CIRCLE('',#73809,7.69049145761145);
#17855=CIRCLE('',#73811,7.68475571189761);
#17856=CIRCLE('',#73812,7.68602760007439);
#17857=CIRCLE('',#73813,7.6904916485909);
#17858=CIRCLE('',#73815,7.68475573508915);
#17859=CIRCLE('',#73816,7.68602771007527);
#17860=CIRCLE('',#73817,7.69049150126655);
#17861=CIRCLE('',#73819,7.68475566164297);
#17862=CIRCLE('',#73820,7.68602755871313);
#17863=CIRCLE('',#73821,7.69049174527211);
#17864=CIRCLE('',#73823,7.68475596896526);
#17865=CIRCLE('',#73824,7.6860273611231);
#17866=CIRCLE('',#73825,7.69049164220205);
#17867=CIRCLE('',#73827,7.68475546250515);
#17868=CIRCLE('',#73828,7.68602787972657);
#17869=CIRCLE('',#73829,7.69049163629909);
#17870=CIRCLE('',#73831,7.68475572461334);
#17871=CIRCLE('',#73832,7.68602754757312);
#17872=CIRCLE('',#73833,7.69049166028763);
#17873=CIRCLE('',#73835,7.68475597486026);
#17874=CIRCLE('',#73836,7.68602729094763);
#17875=CIRCLE('',#73837,7.69049160408503);
#17876=CIRCLE('',#73839,7.68475528721708);
#17877=CIRCLE('',#73840,7.68602767517274);
#17878=CIRCLE('',#73841,7.69049163940496);
#17879=CIRCLE('',#73843,7.68475561008966);
#17880=CIRCLE('',#73844,7.68602753984931);
#17881=CIRCLE('',#73845,7.69049167756843);
#17882=CIRCLE('',#73847,7.68475597255132);
#17883=CIRCLE('',#73848,7.68602762271067);
#17884=CIRCLE('',#73849,7.69049159845339);
#17885=CIRCLE('',#73851,7.68475551206392);
#17886=CIRCLE('',#73852,7.68602756172998);
#17887=CIRCLE('',#73853,7.69049166255934);
#17888=CIRCLE('',#73855,7.68475579404613);
#17889=CIRCLE('',#73856,7.68602756269892);
#17890=CIRCLE('',#73857,7.69049166895877);
#17891=CIRCLE('',#73859,7.68475564415784);
#17892=CIRCLE('',#73860,7.6860273428279);
#17893=CIRCLE('',#73861,7.69049150448244);
#17894=CIRCLE('',#73863,7.68475576796664);
#17895=CIRCLE('',#73864,7.68602744803473);
#17896=CIRCLE('',#73865,7.69049144400215);
#17897=CIRCLE('',#73867,7.68475559032282);
#17898=CIRCLE('',#73868,7.68602747872486);
#17899=CIRCLE('',#73869,7.69049170918301);
#17900=CIRCLE('',#73871,7.68475579599015);
#17901=CIRCLE('',#73872,7.6860277113899);
#17902=CIRCLE('',#73873,7.69049155823195);
#17903=CIRCLE('',#73875,7.68475544644147);
#17904=CIRCLE('',#73876,7.68602747845228);
#17905=CIRCLE('',#73877,7.69049157336687);
#17906=CIRCLE('',#73879,7.68475573644825);
#17907=CIRCLE('',#73880,7.68602731299916);
#17908=CIRCLE('',#73881,7.69049175407852);
#17909=CIRCLE('',#73883,7.68475567017514);
#17910=CIRCLE('',#73884,7.68602748502965);
#17911=CIRCLE('',#73885,7.69049145574597);
#17912=CIRCLE('',#73887,7.6847555902511);
#17913=CIRCLE('',#73888,7.68602772472989);
#17914=CIRCLE('',#73889,7.69049164589603);
#17915=CIRCLE('',#73891,7.68475556041525);
#17916=CIRCLE('',#73892,7.68602739672098);
#17917=CIRCLE('',#73893,7.69049151223703);
#17918=CIRCLE('',#73895,7.68475595845802);
#17919=CIRCLE('',#73896,7.68602760723119);
#17920=CIRCLE('',#73898,7.68475569621939);
#17921=CIRCLE('',#73899,7.6860274156871);
#17922=CIRCLE('',#73900,7.4441241331261);
#17923=CIRCLE('',#73901,7.44962098873202);
#17924=CIRCLE('',#73902,7.44412180952238);
#17925=CIRCLE('',#73903,7.44962082790162);
#17926=CIRCLE('',#73904,7.44412154997683);
#17927=CIRCLE('',#73905,7.4496207652638);
#17928=CIRCLE('',#73906,7.44412175052952);
#17929=CIRCLE('',#73907,7.44962098477913);
#17930=CIRCLE('',#73908,7.44412174529551);
#17931=CIRCLE('',#73909,7.44962097025448);
#17932=CIRCLE('',#73910,7.44412158364088);
#17933=CIRCLE('',#73911,7.44962082581289);
#17934=CIRCLE('',#73912,7.44412158122055);
#17935=CIRCLE('',#73913,7.44962082724999);
#17936=CIRCLE('',#73914,7.44412161528393);
#17937=CIRCLE('',#73915,7.44962123096025);
#17938=CIRCLE('',#73916,7.44412179534068);
#17939=CIRCLE('',#73917,7.44962098648082);
#17940=CIRCLE('',#73918,7.44412174137443);
#17941=CIRCLE('',#73919,7.44962074392395);
#17942=CIRCLE('',#73920,7.44412180128965);
#17943=CIRCLE('',#73921,7.4496207975329);
#17944=CIRCLE('',#73922,7.44412154466149);
#17945=CIRCLE('',#73923,7.44962083948352);
#17946=CIRCLE('',#73924,7.44412191376129);
#17947=CIRCLE('',#73925,7.44962082298598);
#17948=CIRCLE('',#73926,7.44412173712964);
#17949=CIRCLE('',#73927,7.44962099064716);
#17950=CIRCLE('',#73928,7.44412164601454);
#17951=CIRCLE('',#73929,7.44962091021146);
#17952=CIRCLE('',#73930,7.44412161917552);
#17953=CIRCLE('',#73931,7.44962093879096);
#17954=CIRCLE('',#73932,7.44412153423081);
#17955=CIRCLE('',#73933,7.44962107444784);
#17956=CIRCLE('',#73934,7.44412183990525);
#17957=CIRCLE('',#73935,7.44962103513103);
#17958=CIRCLE('',#73936,7.44412166798311);
#17959=CIRCLE('',#73937,7.44962107754971);
#17960=CIRCLE('',#73938,7.4441216537555);
#17961=CIRCLE('',#73939,7.4496206428889);
#17962=CIRCLE('',#73940,7.44412167613138);
#17963=CIRCLE('',#73941,7.44962100045877);
#17964=CIRCLE('',#73942,7.44412169957312);
#17965=CIRCLE('',#73943,7.44962075048619);
#17966=CIRCLE('',#73944,7.44412154619005);
#17967=CIRCLE('',#73945,7.44962091788761);
#17968=CIRCLE('',#73946,7.44412170737385);
#17969=CIRCLE('',#73947,7.44962106412872);
#17970=CIRCLE('',#73948,7.44412169520957);
#17971=CIRCLE('',#73949,7.44962101012624);
#17972=CIRCLE('',#73950,7.44412165636468);
#17973=CIRCLE('',#73951,7.44962088978097);
#17974=CIRCLE('',#73952,7.44412171376414);
#17975=CIRCLE('',#73953,7.44962092331337);
#17976=CIRCLE('',#73954,7.44412153513632);
#17977=CIRCLE('',#73955,7.44962090241827);
#17978=CIRCLE('',#73956,7.44412157163877);
#17979=CIRCLE('',#73957,7.44962220320026);
#17980=CIRCLE('',#73958,7.44380150548939);
#17981=CIRCLE('',#73959,7.44380000680351);
#17982=CIRCLE('',#73960,7.4438001907365);
#17983=CIRCLE('',#73961,7.44379998723725);
#17984=CIRCLE('',#73962,7.44380000199902);
#17985=CIRCLE('',#73963,7.44379993030849);
#17986=CIRCLE('',#73964,7.44379976545896);
#17987=CIRCLE('',#73965,7.4437999487249);
#17988=CIRCLE('',#73966,7.44380009861783);
#17989=CIRCLE('',#73967,7.4437998982179);
#17990=CIRCLE('',#73968,7.44380017020166);
#17991=CIRCLE('',#73969,7.44379940853564);
#17992=CIRCLE('',#73970,7.44380004651171);
#17993=CIRCLE('',#73971,7.44379989072602);
#17994=CIRCLE('',#73972,7.44379996753508);
#17995=CIRCLE('',#73973,7.44380026452087);
#17996=CIRCLE('',#73974,7.44380001448714);
#17997=CIRCLE('',#73975,7.44379978702513);
#17998=CIRCLE('',#73976,7.44379988901668);
#17999=CIRCLE('',#73977,7.44379976723227);
#18000=CIRCLE('',#73978,7.44380009914586);
#18001=CIRCLE('',#73979,7.44380008131669);
#18002=CIRCLE('',#73980,7.4437999315236);
#18003=CIRCLE('',#73981,7.44379996658801);
#18004=CIRCLE('',#73982,7.44380005441912);
#18005=CIRCLE('',#73983,7.44380010128159);
#18006=CIRCLE('',#73984,7.44379996239169);
#18007=CIRCLE('',#73985,7.44380004600786);
#18008=CIRCLE('',#73986,7.44380002572478);
#18009=CIRCLE('',#73987,7.68894244416909);
#18010=CIRCLE('',#73989,7.69154643806877);
#18011=CIRCLE('',#73990,7.69254667889009);
#18012=CIRCLE('',#73991,7.69306086011482);
#18013=CIRCLE('',#73992,7.68894234890342);
#18014=CIRCLE('',#73994,7.69154662654791);
#18015=CIRCLE('',#73995,7.69254646639703);
#18016=CIRCLE('',#73996,7.69306109538576);
#18017=CIRCLE('',#73997,7.68894231004885);
#18018=CIRCLE('',#73999,7.69154650794579);
#18019=CIRCLE('',#74000,7.69254643716538);
#18020=CIRCLE('',#74001,7.69306098564575);
#18021=CIRCLE('',#74002,7.68894214032325);
#18022=CIRCLE('',#74004,7.69154695753898);
#18023=CIRCLE('',#74005,7.69254640742847);
#18024=CIRCLE('',#74006,7.69306102978304);
#18025=CIRCLE('',#74007,7.68894230068754);
#18026=CIRCLE('',#74009,7.6915466516697);
#18027=CIRCLE('',#74010,7.69254652874586);
#18028=CIRCLE('',#74011,7.69306103950312);
#18029=CIRCLE('',#74012,7.68894217261782);
#18030=CIRCLE('',#74014,7.6915468492434);
#18031=CIRCLE('',#74015,7.69254635550889);
#18032=CIRCLE('',#74016,7.69306106289197);
#18033=CIRCLE('',#74017,7.68894227017874);
#18034=CIRCLE('',#74019,7.69154650939399);
#18035=CIRCLE('',#74020,7.69254642329256);
#18036=CIRCLE('',#74021,7.69306091598276);
#18037=CIRCLE('',#74022,7.68894227758912);
#18038=CIRCLE('',#74024,7.69154669278215);
#18039=CIRCLE('',#74025,7.69254632430852);
#18040=CIRCLE('',#74026,7.69306090803412);
#18041=CIRCLE('',#74027,7.68894208372619);
#18042=CIRCLE('',#74029,7.69154674898312);
#18043=CIRCLE('',#74030,7.69254616753055);
#18044=CIRCLE('',#74031,7.69306114235764);
#18045=CIRCLE('',#74032,7.68894230100823);
#18046=CIRCLE('',#74034,7.69154694513176);
#18047=CIRCLE('',#74035,7.69254629731355);
#18048=CIRCLE('',#74036,7.69306123255489);
#18049=CIRCLE('',#74037,7.68894220126532);
#18050=CIRCLE('',#74039,7.69154643777242);
#18051=CIRCLE('',#74040,7.69254642561957);
#18052=CIRCLE('',#74041,7.69306066636817);
#18053=CIRCLE('',#74042,7.68894231213788);
#18054=CIRCLE('',#74044,7.6915465723561);
#18055=CIRCLE('',#74045,7.69254635178032);
#18056=CIRCLE('',#74046,7.69306080893017);
#18057=CIRCLE('',#74047,7.68894221503211);
#18058=CIRCLE('',#74049,7.6915466326821);
#18059=CIRCLE('',#74050,7.69254654865938);
#18060=CIRCLE('',#74051,7.69306113942179);
#18061=CIRCLE('',#74052,7.6889421698178);
#18062=CIRCLE('',#74054,7.69154662159575);
#18063=CIRCLE('',#74055,7.69254659525327);
#18064=CIRCLE('',#74056,7.6930609598333);
#18065=CIRCLE('',#74057,7.68894217840434);
#18066=CIRCLE('',#74059,7.69154657054028);
#18067=CIRCLE('',#74060,7.69254661883229);
#18068=CIRCLE('',#74061,7.69306076749964);
#18069=CIRCLE('',#74062,7.6889422576405);
#18070=CIRCLE('',#74064,7.69154662261387);
#18071=CIRCLE('',#74065,7.69254645368903);
#18072=CIRCLE('',#74066,7.69306084906152);
#18073=CIRCLE('',#74067,7.68894217718232);
#18074=CIRCLE('',#74069,7.6915464115028);
#18075=CIRCLE('',#74070,7.69254622518674);
#18076=CIRCLE('',#74071,7.69306080188211);
#18077=CIRCLE('',#74072,7.68894206501938);
#18078=CIRCLE('',#74074,7.69154674301802);
#18079=CIRCLE('',#74075,7.69254664274991);
#18080=CIRCLE('',#74076,7.69306095020453);
#18081=CIRCLE('',#74077,7.68894200646331);
#18082=CIRCLE('',#74079,7.69154677190965);
#18083=CIRCLE('',#74080,7.69254659932621);
#18084=CIRCLE('',#74081,7.69306102148478);
#18085=CIRCLE('',#74082,7.68894217824212);
#18086=CIRCLE('',#74084,7.69154656930193);
#18087=CIRCLE('',#74085,7.69254660059922);
#18088=CIRCLE('',#74086,7.69306110352981);
#18089=CIRCLE('',#74087,7.68894229148283);
#18090=CIRCLE('',#74088,7.69305583026409);
#18091=CIRCLE('',#74090,7.69154675624609);
#18092=CIRCLE('',#74091,7.69254128953939);
#18093=CIRCLE('',#74092,7.68894235630222);
#18094=CIRCLE('',#74094,7.693061068196);
#18095=CIRCLE('',#74095,7.69154691308647);
#18096=CIRCLE('',#74096,7.69254635983995);
#18097=CIRCLE('',#74097,7.68894209982254);
#18098=CIRCLE('',#74099,7.69154654828669);
#18099=CIRCLE('',#74100,7.69254651461116);
#18100=CIRCLE('',#74101,7.69306097724112);
#18101=CIRCLE('',#74102,7.68894224453809);
#18102=CIRCLE('',#74104,7.69154647613157);
#18103=CIRCLE('',#74105,7.69254630388625);
#18104=CIRCLE('',#74106,7.69306121587964);
#18105=CIRCLE('',#74107,7.68894206378456);
#18106=CIRCLE('',#74109,7.69154649978663);
#18107=CIRCLE('',#74110,7.69254629177802);
#18108=CIRCLE('',#74111,7.69306081211227);
#18109=CIRCLE('',#74112,7.68894199816537);
#18110=CIRCLE('',#74114,7.69154666770906);
#18111=CIRCLE('',#74115,7.69254632743289);
#18112=CIRCLE('',#74116,7.69306094639951);
#18113=CIRCLE('',#74117,7.68894215868675);
#18114=CIRCLE('',#74119,7.69154658380995);
#18115=CIRCLE('',#74120,7.69254652211315);
#18116=CIRCLE('',#74121,7.69306080752694);
#18117=CIRCLE('',#74122,7.6889421547065);
#18118=CIRCLE('',#74124,7.69154672679512);
#18119=CIRCLE('',#74125,7.69254664713157);
#18120=CIRCLE('',#74126,7.69306105760353);
#18121=CIRCLE('',#74127,7.68866079157655);
#18122=CIRCLE('',#74129,7.68493063279481);
#18123=CIRCLE('',#74130,7.69242158874635);
#18124=CIRCLE('',#74131,7.68866085610895);
#18125=CIRCLE('',#74133,7.68493073427246);
#18126=CIRCLE('',#74134,7.69242153534071);
#18127=CIRCLE('',#74135,7.68866057768082);
#18128=CIRCLE('',#74137,7.68493065739063);
#18129=CIRCLE('',#74138,7.69242136477564);
#18130=CIRCLE('',#74139,7.68866046048346);
#18131=CIRCLE('',#74141,7.68493071227508);
#18132=CIRCLE('',#74142,7.69242129349027);
#18133=CIRCLE('',#74143,7.68866070478409);
#18134=CIRCLE('',#74145,7.68493080555999);
#18135=CIRCLE('',#74146,7.69242166647581);
#18136=CIRCLE('',#74147,7.68866102373785);
#18137=CIRCLE('',#74149,7.68493073465088);
#18138=CIRCLE('',#74150,7.69242161162231);
#18139=CIRCLE('',#74151,7.68866070214171);
#18140=CIRCLE('',#74153,7.68493083698717);
#18141=CIRCLE('',#74154,7.69242127471809);
#18142=CIRCLE('',#74155,7.68866070803868);
#18143=CIRCLE('',#74157,7.68493077752384);
#18144=CIRCLE('',#74158,7.69242159894978);
#18145=CIRCLE('',#74159,7.68866068058214);
#18146=CIRCLE('',#74161,7.68493077403634);
#18147=CIRCLE('',#74162,7.69242172204927);
#18148=CIRCLE('',#74163,7.68866061784442);
#18149=CIRCLE('',#74165,7.68493085519223);
#18150=CIRCLE('',#74166,7.69242164669672);
#18151=CIRCLE('',#74167,7.68866071969335);
#18152=CIRCLE('',#74169,7.68493083532197);
#18153=CIRCLE('',#74170,7.69242155382646);
#18154=CIRCLE('',#74171,7.68866097614275);
#18155=CIRCLE('',#74173,7.68493088965889);
#18156=CIRCLE('',#74174,7.69242155472373);
#18157=CIRCLE('',#74175,7.68866091405694);
#18158=CIRCLE('',#74177,7.68493087532503);
#18159=CIRCLE('',#74178,7.69242155958861);
#18160=CIRCLE('',#74179,7.6886605506081);
#18161=CIRCLE('',#74181,7.68493084729003);
#18162=CIRCLE('',#74182,7.69242157979543);
#18163=CIRCLE('',#74183,7.68866092479545);
#18164=CIRCLE('',#74185,7.68493081256949);
#18165=CIRCLE('',#74186,7.69242124981822);
#18166=CIRCLE('',#74187,7.68866062458902);
#18167=CIRCLE('',#74189,7.68493062347516);
#18168=CIRCLE('',#74190,7.69242159436639);
#18169=CIRCLE('',#74191,7.68866058647684);
#18170=CIRCLE('',#74193,7.68493051543894);
#18171=CIRCLE('',#74194,7.69242137066694);
#18172=CIRCLE('',#74195,7.68866068309314);
#18173=CIRCLE('',#74197,7.68493068209183);
#18174=CIRCLE('',#74198,7.69242157194857);
#18175=CIRCLE('',#74199,7.68866082607717);
#18176=CIRCLE('',#74201,7.68493060370205);
#18177=CIRCLE('',#74202,7.69242145062432);
#18178=CIRCLE('',#74203,7.68866071711247);
#18179=CIRCLE('',#74205,7.68493098747741);
#18180=CIRCLE('',#74206,7.69242140154801);
#18181=CIRCLE('',#74207,7.68866067715954);
#18182=CIRCLE('',#74209,7.68493081669674);
#18183=CIRCLE('',#74210,7.69242147628779);
#18184=CIRCLE('',#74211,7.68866088453931);
#18185=CIRCLE('',#74213,7.6849306078979);
#18186=CIRCLE('',#74214,7.69242158409723);
#18187=CIRCLE('',#74215,7.68866096259156);
#18188=CIRCLE('',#74217,7.68493074117565);
#18189=CIRCLE('',#74218,7.6924217292055);
#18190=CIRCLE('',#74219,7.68866054447294);
#18191=CIRCLE('',#74221,7.68493089689092);
#18192=CIRCLE('',#74222,7.69242137389086);
#18193=CIRCLE('',#74223,7.6886607771901);
#18194=CIRCLE('',#74225,7.68493065069607);
#18195=CIRCLE('',#74226,7.69242148743181);
#18196=CIRCLE('',#74227,7.68866048060024);
#18197=CIRCLE('',#74229,7.68493057949617);
#18198=CIRCLE('',#74230,7.69242134436988);
#18199=CIRCLE('',#74231,7.68866077886559);
#18200=CIRCLE('',#74233,7.68493056970141);
#18201=CIRCLE('',#74234,7.69242169940791);
#18202=CIRCLE('',#74235,7.68866069476782);
#18203=CIRCLE('',#74237,7.68493069136092);
#18204=CIRCLE('',#74238,7.69242165135084);
#18205=CIRCLE('',#74239,7.44726893187504);
#18206=CIRCLE('',#74240,7.44947055337963);
#18207=CIRCLE('',#74241,7.44726922435689);
#18208=CIRCLE('',#74242,7.44947035700538);
#18209=CIRCLE('',#74243,7.44726911447711);
#18210=CIRCLE('',#74244,7.44947024139007);
#18211=CIRCLE('',#74245,7.44726890407395);
#18212=CIRCLE('',#74246,7.44947046676801);
#18213=CIRCLE('',#74247,7.44726901139079);
#18214=CIRCLE('',#74248,7.44947025629349);
#18215=CIRCLE('',#74249,7.44726922475947);
#18216=CIRCLE('',#74250,7.44947040140503);
#18217=CIRCLE('',#74251,7.44726905730899);
#18218=CIRCLE('',#74252,7.44947047782816);
#18219=CIRCLE('',#74253,7.44726918025779);
#18220=CIRCLE('',#74254,7.4494705297753);
#18221=CIRCLE('',#74255,7.44726931950462);
#18222=CIRCLE('',#74256,7.44947031239334);
#18223=CIRCLE('',#74257,7.44726901770317);
#18224=CIRCLE('',#74258,7.44947057242369);
#18225=CIRCLE('',#74259,7.44726903924226);
#18226=CIRCLE('',#74260,7.44947028478251);
#18227=CIRCLE('',#74261,7.44726894258544);
#18228=CIRCLE('',#74262,7.44947038945979);
#18229=CIRCLE('',#74263,7.44726926857445);
#18230=CIRCLE('',#74264,7.44947054644512);
#18231=CIRCLE('',#74265,7.44726916275161);
#18232=CIRCLE('',#74266,7.44947051640123);
#18233=CIRCLE('',#74267,7.44726899142121);
#18234=CIRCLE('',#74268,7.44947023322216);
#18235=CIRCLE('',#74269,7.44726916809674);
#18236=CIRCLE('',#74270,7.4494704560091);
#18237=CIRCLE('',#74271,7.44726925582064);
#18238=CIRCLE('',#74272,7.4494703409082);
#18239=CIRCLE('',#74273,7.44726899307573);
#18240=CIRCLE('',#74274,7.44947038677876);
#18241=CIRCLE('',#74275,7.44726913176375);
#18242=CIRCLE('',#74276,7.44947037014665);
#18243=CIRCLE('',#74277,7.44726906379561);
#18244=CIRCLE('',#74278,7.44947043308436);
#18245=CIRCLE('',#74279,7.44726900882387);
#18246=CIRCLE('',#74280,7.44947053089161);
#18247=CIRCLE('',#74281,7.44726899765228);
#18248=CIRCLE('',#74282,7.44947032882606);
#18249=CIRCLE('',#74283,7.44726896098699);
#18250=CIRCLE('',#74284,7.44947051052289);
#18251=CIRCLE('',#74285,7.44726884235526);
#18252=CIRCLE('',#74286,7.44947035672427);
#18253=CIRCLE('',#74287,7.4472689273175);
#18254=CIRCLE('',#74288,7.44947048644835);
#18255=CIRCLE('',#74289,7.44726899435253);
#18256=CIRCLE('',#74290,7.44947041903508);
#18257=CIRCLE('',#74291,7.44726886787733);
#18258=CIRCLE('',#74292,7.44947031904415);
#18259=CIRCLE('',#74293,7.44726912411596);
#18260=CIRCLE('',#74294,7.44947025413867);
#18261=CIRCLE('',#74295,7.44726903781441);
#18262=CIRCLE('',#74296,7.44947046972415);
#18263=CIRCLE('',#74297,7.44279297622348);
#18264=CIRCLE('',#74298,7.44938663848418);
#18265=CIRCLE('',#74299,7.44279152433174);
#18266=CIRCLE('',#74300,7.44938647943049);
#18267=CIRCLE('',#74301,7.44279186948023);
#18268=CIRCLE('',#74302,7.44938649896905);
#18269=CIRCLE('',#74303,7.44279179346431);
#18270=CIRCLE('',#74304,7.4493867369477);
#18271=CIRCLE('',#74305,7.44279170217027);
#18272=CIRCLE('',#74306,7.44938643383611);
#18273=CIRCLE('',#74307,7.44279175403518);
#18274=CIRCLE('',#74308,7.44938669614748);
#18275=CIRCLE('',#74309,7.44279173998518);
#18276=CIRCLE('',#74310,7.44938644404911);
#18277=CIRCLE('',#74311,7.44279180610017);
#18278=CIRCLE('',#74312,7.44938660521199);
#18279=CIRCLE('',#74313,7.44279157690661);
#18280=CIRCLE('',#74314,7.4493865971617);
#18281=CIRCLE('',#74315,7.44279168044848);
#18282=CIRCLE('',#74316,7.44938664408774);
#18283=CIRCLE('',#74317,7.44279151478295);
#18284=CIRCLE('',#74318,7.44938641050267);
#18285=CIRCLE('',#74319,7.44279159211148);
#18286=CIRCLE('',#74320,7.44938674882838);
#18287=CIRCLE('',#74321,7.44279173978052);
#18288=CIRCLE('',#74322,7.44938664066163);
#18289=CIRCLE('',#74323,7.44279187426533);
#18290=CIRCLE('',#74324,7.44938674154436);
#18291=CIRCLE('',#74325,7.4427917186894);
#18292=CIRCLE('',#74326,7.44938644598291);
#18293=CIRCLE('',#74327,7.44279156987268);
#18294=CIRCLE('',#74328,7.44938669306736);
#18295=CIRCLE('',#74329,7.44279186354848);
#18296=CIRCLE('',#74330,7.44938658334004);
#18297=CIRCLE('',#74331,7.44279172011691);
#18298=CIRCLE('',#74332,7.44938654099507);
#18299=CIRCLE('',#74333,7.44279154487388);
#18300=CIRCLE('',#74334,7.44938643919626);
#18301=CIRCLE('',#74335,7.44279169235632);
#18302=CIRCLE('',#74336,7.44938661848526);
#18303=CIRCLE('',#74337,7.44279153983535);
#18304=CIRCLE('',#74338,7.44938660972236);
#18305=CIRCLE('',#74339,7.44279172819363);
#18306=CIRCLE('',#74340,7.44938649240783);
#18307=CIRCLE('',#74341,7.44279144437215);
#18308=CIRCLE('',#74342,7.44938664563379);
#18309=CIRCLE('',#74343,7.44279157057872);
#18310=CIRCLE('',#74344,7.44938664600317);
#18311=CIRCLE('',#74345,7.44279166161903);
#18312=CIRCLE('',#74346,7.44938664447462);
#18313=CIRCLE('',#74347,7.4427916397829);
#18314=CIRCLE('',#74348,7.44938658372445);
#18315=CIRCLE('',#74349,7.44279157245851);
#18316=CIRCLE('',#74350,7.44938641775037);
#18317=CIRCLE('',#74351,7.44279169699838);
#18318=CIRCLE('',#74352,7.4493867450934);
#18319=CIRCLE('',#74353,7.4427916925524);
#18320=CIRCLE('',#74354,7.44938776348471);
#18321=CIRCLE('',#74355,7.68983511182372);
#18322=CIRCLE('',#74356,7.69301883077793);
#18323=CIRCLE('',#74358,7.68356108711578);
#18324=CIRCLE('',#74359,7.69198153688764);
#18325=CIRCLE('',#74360,7.6898349590935);
#18326=CIRCLE('',#74361,7.69301892560717);
#18327=CIRCLE('',#74363,7.68356157880052);
#18328=CIRCLE('',#74364,7.69198149127838);
#18329=CIRCLE('',#74365,7.68983486095025);
#18330=CIRCLE('',#74366,7.69301873113243);
#18331=CIRCLE('',#74368,7.68356126410177);
#18332=CIRCLE('',#74369,7.69198185871291);
#18333=CIRCLE('',#74370,7.68983498346275);
#18334=CIRCLE('',#74371,7.69301884923081);
#18335=CIRCLE('',#74373,7.68356161321587);
#18336=CIRCLE('',#74374,7.69198163216993);
#18337=CIRCLE('',#74375,7.68983525253744);
#18338=CIRCLE('',#74376,7.69301874197828);
#18339=CIRCLE('',#74378,7.68356149577362);
#18340=CIRCLE('',#74379,7.69198177259241);
#18341=CIRCLE('',#74380,7.6898350821565);
#18342=CIRCLE('',#74381,7.69301890869412);
#18343=CIRCLE('',#74383,7.68356131636576);
#18344=CIRCLE('',#74384,7.69198162591331);
#18345=CIRCLE('',#74385,7.68983508845765);
#18346=CIRCLE('',#74386,7.69301856377739);
#18347=CIRCLE('',#74388,7.68356096635524);
#18348=CIRCLE('',#74389,7.69198148894895);
#18349=CIRCLE('',#74390,7.68983489163653);
#18350=CIRCLE('',#74391,7.69301860717921);
#18351=CIRCLE('',#74393,7.68356109745221);
#18352=CIRCLE('',#74394,7.69198160697471);
#18353=CIRCLE('',#74395,7.68983495320323);
#18354=CIRCLE('',#74396,7.69301872744581);
#18355=CIRCLE('',#74398,7.68356097839941);
#18356=CIRCLE('',#74399,7.69198180730794);
#18357=CIRCLE('',#74400,7.6898348056083);
#18358=CIRCLE('',#74401,7.69301894532186);
#18359=CIRCLE('',#74403,7.68356155537256);
#18360=CIRCLE('',#74404,7.69198154302483);
#18361=CIRCLE('',#74405,7.68983478733256);
#18362=CIRCLE('',#74406,7.69301861129838);
#18363=CIRCLE('',#74408,7.68356132050169);
#18364=CIRCLE('',#74409,7.69198160962373);
#18365=CIRCLE('',#74410,7.6898350635965);
#18366=CIRCLE('',#74411,7.69301869003358);
#18367=CIRCLE('',#74413,7.68356146760216);
#18368=CIRCLE('',#74414,7.69198176950467);
#18369=CIRCLE('',#74415,7.68983514693778);
#18370=CIRCLE('',#74416,7.69301860446202);
#18371=CIRCLE('',#74418,7.68356117230564);
#18372=CIRCLE('',#74419,7.69198166634701);
#18373=CIRCLE('',#74420,7.68983502565558);
#18374=CIRCLE('',#74421,7.69301871453826);
#18375=CIRCLE('',#74423,7.68356136461527);
#18376=CIRCLE('',#74424,7.69198156882603);
#18377=CIRCLE('',#74425,7.68983486471204);
#18378=CIRCLE('',#74426,7.69301880820276);
#18379=CIRCLE('',#74428,7.6835614892657);
#18380=CIRCLE('',#74429,7.69198165345857);
#18381=CIRCLE('',#74430,7.68983489049233);
#18382=CIRCLE('',#74431,7.69301869930148);
#18383=CIRCLE('',#74433,7.68356141591065);
#18384=CIRCLE('',#74434,7.69198155169492);
#18385=CIRCLE('',#74435,7.68983517907979);
#18386=CIRCLE('',#74436,7.69301869436094);
#18387=CIRCLE('',#74438,7.68356149750982);
#18388=CIRCLE('',#74439,7.69198167371507);
#18389=CIRCLE('',#74440,7.68983511391616);
#18390=CIRCLE('',#74441,7.69301879179767);
#18391=CIRCLE('',#74443,7.68356108644306);
#18392=CIRCLE('',#74444,7.69198150436164);
#18393=CIRCLE('',#74445,7.68983479811495);
#18394=CIRCLE('',#74446,7.69301864826701);
#18395=CIRCLE('',#74448,7.68356158149942);
#18396=CIRCLE('',#74449,7.69198163455412);
#18397=CIRCLE('',#74450,7.6898351085822);
#18398=CIRCLE('',#74451,7.69301906315715);
#18399=CIRCLE('',#74452,7.68983488463856);
#18400=CIRCLE('',#74454,7.68356129710826);
#18401=CIRCLE('',#74455,7.69197999153342);
#18402=CIRCLE('',#74456,7.6930185941024);
#18403=CIRCLE('',#74458,7.68983487958893);
#18404=CIRCLE('',#74459,7.68356097068493);
#18405=CIRCLE('',#74460,7.69198183398909);
#18406=CIRCLE('',#74461,7.69301893341851);
#18407=CIRCLE('',#74463,7.68356105584901);
#18408=CIRCLE('',#74464,7.691981635138);
#18409=CIRCLE('',#74465,7.68983492376419);
#18410=CIRCLE('',#74466,7.69301870860216);
#18411=CIRCLE('',#74468,7.68356148397883);
#18412=CIRCLE('',#74469,7.69198173167317);
#18413=CIRCLE('',#74470,7.68983500343551);
#18414=CIRCLE('',#74471,7.69301882102673);
#18415=CIRCLE('',#74473,7.6835618363572);
#18416=CIRCLE('',#74474,7.69198181002405);
#18417=CIRCLE('',#74475,7.68983478848117);
#18418=CIRCLE('',#74476,7.6930186974174);
#18419=CIRCLE('',#74478,7.68356093215567);
#18420=CIRCLE('',#74479,7.69198175834627);
#18421=CIRCLE('',#74480,7.68983498544143);
#18422=CIRCLE('',#74481,7.69301860697724);
#18423=CIRCLE('',#74483,7.68356149559124);
#18424=CIRCLE('',#74484,7.69198186433126);
#18425=CIRCLE('',#74485,7.68983488114589);
#18426=CIRCLE('',#74486,7.69301896558328);
#18427=CIRCLE('',#74488,7.6835614765364);
#18428=CIRCLE('',#74489,7.69198148285223);
#18429=CIRCLE('',#74490,7.68983489375441);
#18430=CIRCLE('',#74492,7.6835617812463);
#18431=CIRCLE('',#74493,7.69198149369972);
#18432=CIRCLE('',#74494,7.69301888026525);
#18433=CIRCLE('',#74495,7.68779224917023);
#18434=CIRCLE('',#74496,7.69298006574425);
#18435=CIRCLE('',#74497,7.68779273536459);
#18436=CIRCLE('',#74499,7.69207574501788);
#18437=CIRCLE('',#74500,7.69213146141502);
#18438=CIRCLE('',#74501,7.69297998710772);
#18439=CIRCLE('',#74502,7.68779251605245);
#18440=CIRCLE('',#74504,7.69207574680839);
#18441=CIRCLE('',#74505,7.69213138451493);
#18442=CIRCLE('',#74506,7.69297998713124);
#18443=CIRCLE('',#74507,7.68779249899382);
#18444=CIRCLE('',#74509,7.69207597534737);
#18445=CIRCLE('',#74510,7.69213128631069);
#18446=CIRCLE('',#74511,7.69297994261074);
#18447=CIRCLE('',#74512,7.68779239378566);
#18448=CIRCLE('',#74514,7.69207570721692);
#18449=CIRCLE('',#74515,7.69213126984507);
#18450=CIRCLE('',#74516,7.69298018311711);
#18451=CIRCLE('',#74517,7.68779224134649);
#18452=CIRCLE('',#74519,7.69207556007882);
#18453=CIRCLE('',#74520,7.69213113842492);
#18454=CIRCLE('',#74521,7.69297969649806);
#18455=CIRCLE('',#74522,7.68779272659023);
#18456=CIRCLE('',#74524,7.69207579966006);
#18457=CIRCLE('',#74525,7.69213110313893);
#18458=CIRCLE('',#74526,7.69297999256842);
#18459=CIRCLE('',#74527,7.68779254733851);
#18460=CIRCLE('',#74529,7.69207587499486);
#18461=CIRCLE('',#74530,7.69213147841857);
#18462=CIRCLE('',#74531,7.69298003584678);
#18463=CIRCLE('',#74532,7.68779243244237);
#18464=CIRCLE('',#74534,7.69207592300941);
#18465=CIRCLE('',#74535,7.69213135839676);
#18466=CIRCLE('',#74536,7.69297963916946);
#18467=CIRCLE('',#74537,7.68779251761288);
#18468=CIRCLE('',#74539,7.69207559530714);
#18469=CIRCLE('',#74540,7.6921311551946);
#18470=CIRCLE('',#74541,7.69297987944067);
#18471=CIRCLE('',#74542,7.68779249007612);
#18472=CIRCLE('',#74544,7.69207589105174);
#18473=CIRCLE('',#74545,7.69213126619558);
#18474=CIRCLE('',#74546,7.6929798488236);
#18475=CIRCLE('',#74547,7.6877924665024);
#18476=CIRCLE('',#74549,7.69207585096444);
#18477=CIRCLE('',#74550,7.69213117664494);
#18478=CIRCLE('',#74551,7.6929799084806);
#18479=CIRCLE('',#74552,7.68779254617694);
#18480=CIRCLE('',#74554,7.69207557938261);
#18481=CIRCLE('',#74555,7.69213141206415);
#18482=CIRCLE('',#74556,7.69298005187903);
#18483=CIRCLE('',#74557,7.68779234786784);
#18484=CIRCLE('',#74559,7.69207555411377);
#18485=CIRCLE('',#74560,7.69213122220794);
#18486=CIRCLE('',#74561,7.69297992931294);
#18487=CIRCLE('',#74562,7.68779235903073);
#18488=CIRCLE('',#74564,7.69207559882269);
#18489=CIRCLE('',#74565,7.69213134942084);
#18490=CIRCLE('',#74566,7.69297972485294);
#18491=CIRCLE('',#74567,7.68779240123187);
#18492=CIRCLE('',#74569,7.69207573005627);
#18493=CIRCLE('',#74570,7.6921314015989);
#18494=CIRCLE('',#74571,7.69297970104874);
#18495=CIRCLE('',#74572,7.68779265551721);
#18496=CIRCLE('',#74574,7.69207589268163);
#18497=CIRCLE('',#74575,7.69213129959809);
#18498=CIRCLE('',#74576,7.69297968668024);
#18499=CIRCLE('',#74577,7.68779250869095);
#18500=CIRCLE('',#74579,7.69207588950927);
#18501=CIRCLE('',#74580,7.69213118506032);
#18502=CIRCLE('',#74581,7.69297988881807);
#18503=CIRCLE('',#74582,7.68779254555987);
#18504=CIRCLE('',#74584,7.69207550114612);
#18505=CIRCLE('',#74585,7.69213140964143);
#18506=CIRCLE('',#74586,7.69297991283635);
#18507=CIRCLE('',#74587,7.68779256256697);
#18508=CIRCLE('',#74589,7.69207573432771);
#18509=CIRCLE('',#74590,7.69213108454268);
#18510=CIRCLE('',#74591,7.69297992164463);
#18511=CIRCLE('',#74592,7.68779246229219);
#18512=CIRCLE('',#74594,7.69207557758637);
#18513=CIRCLE('',#74595,7.69213122910806);
#18514=CIRCLE('',#74596,7.69297951678655);
#18515=CIRCLE('',#74597,7.68779259311327);
#18516=CIRCLE('',#74599,7.6920758095773);
#18517=CIRCLE('',#74600,7.69213132888472);
#18518=CIRCLE('',#74601,7.6929797349126);
#18519=CIRCLE('',#74602,7.68779229636856);
#18520=CIRCLE('',#74604,7.69207562800561);
#18521=CIRCLE('',#74605,7.69213129153528);
#18522=CIRCLE('',#74606,7.692979834602);
#18523=CIRCLE('',#74607,7.68779266377073);
#18524=CIRCLE('',#74609,7.69207580213767);
#18525=CIRCLE('',#74610,7.6921315768473);
#18526=CIRCLE('',#74611,7.6929798230198);
#18527=CIRCLE('',#74612,7.68779254437404);
#18528=CIRCLE('',#74614,7.69207579340574);
#18529=CIRCLE('',#74615,7.69213126647313);
#18530=CIRCLE('',#74616,7.69297986777709);
#18531=CIRCLE('',#74617,7.68779245760159);
#18532=CIRCLE('',#74619,7.69207587460581);
#18533=CIRCLE('',#74620,7.69213107713119);
#18534=CIRCLE('',#74621,7.69297962621885);
#18535=CIRCLE('',#74622,7.68779243327501);
#18536=CIRCLE('',#74624,7.69207575079905);
#18537=CIRCLE('',#74625,7.69213132479969);
#18538=CIRCLE('',#74626,7.69298016664327);
#18539=CIRCLE('',#74627,7.6877923130605);
#18540=CIRCLE('',#74629,7.69207563694128);
#18541=CIRCLE('',#74630,7.69213116149794);
#18542=CIRCLE('',#74632,7.69298010510988);
#18543=CIRCLE('',#74633,7.69207576876764);
#18544=CIRCLE('',#74634,7.69213137879866);
#18545=CIRCLE('',#74635,7.44783641328649);
#18546=CIRCLE('',#74636,7.44783619459759);
#18547=CIRCLE('',#74637,7.44783667431494);
#18548=CIRCLE('',#74638,7.44783648690676);
#18549=CIRCLE('',#74639,7.44783636287797);
#18550=CIRCLE('',#74640,7.44783640046195);
#18551=CIRCLE('',#74641,7.44783629700487);
#18552=CIRCLE('',#74642,7.44783663820312);
#18553=CIRCLE('',#74643,7.4478364715662);
#18554=CIRCLE('',#74644,7.44783642856168);
#18555=CIRCLE('',#74645,7.44783643761439);
#18556=CIRCLE('',#74646,7.44783628905208);
#18557=CIRCLE('',#74647,7.447836548411);
#18558=CIRCLE('',#74648,7.447836498267);
#18559=CIRCLE('',#74649,7.44783622055948);
#18560=CIRCLE('',#74650,7.44783648709306);
#18561=CIRCLE('',#74651,7.44783649023616);
#18562=CIRCLE('',#74652,7.44783617526261);
#18563=CIRCLE('',#74653,7.44783638695771);
#18564=CIRCLE('',#74654,7.44783631507359);
#18565=CIRCLE('',#74655,7.4478362653215);
#18566=CIRCLE('',#74656,7.44783645134482);
#18567=CIRCLE('',#74657,7.44783627824958);
#18568=CIRCLE('',#74658,7.44783626083019);
#18569=CIRCLE('',#74659,7.44783643327715);
#18570=CIRCLE('',#74660,7.44783624465886);
#18571=CIRCLE('',#74661,7.44783631919974);
#18572=CIRCLE('',#74662,7.44783653783281);
#18573=CIRCLE('',#74663,7.44783620529739);
#18574=CIRCLE('',#74664,7.44803384909972);
#18575=CIRCLE('',#74665,7.44913307740183);
#18576=CIRCLE('',#74666,7.44803378567223);
#18577=CIRCLE('',#74667,7.44913310329878);
#18578=CIRCLE('',#74668,7.44803395927175);
#18579=CIRCLE('',#74669,7.44913311974701);
#18580=CIRCLE('',#74670,7.44803383645474);
#18581=CIRCLE('',#74671,7.44913289345156);
#18582=CIRCLE('',#74672,7.44803362260767);
#18583=CIRCLE('',#74673,7.44913288056903);
#18584=CIRCLE('',#74674,7.4480340141458);
#18585=CIRCLE('',#74675,7.4491330132607);
#18586=CIRCLE('',#74676,7.44803385602116);
#18587=CIRCLE('',#74677,7.44913295277711);
#18588=CIRCLE('',#74678,7.44803381421713);
#18589=CIRCLE('',#74679,7.44913281398462);
#18590=CIRCLE('',#74680,7.44803357600266);
#18591=CIRCLE('',#74681,7.44913295928944);
#18592=CIRCLE('',#74682,7.44803372945488);
#18593=CIRCLE('',#74683,7.4491329086292);
#18594=CIRCLE('',#74684,7.44803385612153);
#18595=CIRCLE('',#74685,7.44913287591789);
#18596=CIRCLE('',#74686,7.44803366892573);
#18597=CIRCLE('',#74687,7.44913297852707);
#18598=CIRCLE('',#74688,7.44803375446823);
#18599=CIRCLE('',#74689,7.44913288728968);
#18600=CIRCLE('',#74690,7.44803393218021);
#18601=CIRCLE('',#74691,7.44913297522573);
#18602=CIRCLE('',#74692,7.44803396683527);
#18603=CIRCLE('',#74693,7.44913300336485);
#18604=CIRCLE('',#74694,7.44803398523721);
#18605=CIRCLE('',#74695,7.44913299643533);
#18606=CIRCLE('',#74696,7.44803363076045);
#18607=CIRCLE('',#74697,7.44913306325659);
#18608=CIRCLE('',#74698,7.44803379354534);
#18609=CIRCLE('',#74699,7.44913305942148);
#18610=CIRCLE('',#74700,7.44803356826013);
#18611=CIRCLE('',#74701,7.44913290424177);
#18612=CIRCLE('',#74702,7.44803365409408);
#18613=CIRCLE('',#74703,7.44913280824488);
#18614=CIRCLE('',#74704,7.44803384284203);
#18615=CIRCLE('',#74705,7.44913294744356);
#18616=CIRCLE('',#74706,7.44803374549019);
#18617=CIRCLE('',#74707,7.44913301853901);
#18618=CIRCLE('',#74708,7.448033631895);
#18619=CIRCLE('',#74709,7.44913287088553);
#18620=CIRCLE('',#74710,7.44803395331646);
#18621=CIRCLE('',#74711,7.44913293159264);
#18622=CIRCLE('',#74712,7.44803389776359);
#18623=CIRCLE('',#74713,7.44913287459541);
#18624=CIRCLE('',#74714,7.44803371713281);
#18625=CIRCLE('',#74715,7.44913302945975);
#18626=CIRCLE('',#74716,7.44803360602241);
#18627=CIRCLE('',#74717,7.44913294186345);
#18628=CIRCLE('',#74718,7.44803394375277);
#18629=CIRCLE('',#74719,7.44913289030108);
#18630=CIRCLE('',#74720,7.44803392778243);
#18631=CIRCLE('',#74721,7.44913457387208);
#18632=CIRCLE('',#74722,7.6904915120903);
#18633=CIRCLE('',#74724,7.68602767954961);
#18634=CIRCLE('',#74725,7.68475595845984);
#18635=CIRCLE('',#74726,7.69049164556693);
#18636=CIRCLE('',#74728,7.6860274549623);
#18637=CIRCLE('',#74729,7.68475556041045);
#18638=CIRCLE('',#74730,7.6904914556618);
#18639=CIRCLE('',#74732,7.68602772470303);
#18640=CIRCLE('',#74733,7.68475559025044);
#18641=CIRCLE('',#74734,7.69049175372012);
#18642=CIRCLE('',#74736,7.6860275414872);
#18643=CIRCLE('',#74737,7.68475567016952);
#18644=CIRCLE('',#74738,7.69049157315506);
#18645=CIRCLE('',#74740,7.68602741691704);
#18646=CIRCLE('',#74741,7.68475573644778);
#18647=CIRCLE('',#74742,7.69049155795063);
#18648=CIRCLE('',#74744,7.68602762817755);
#18649=CIRCLE('',#74745,7.68475544644014);
#18650=CIRCLE('',#74746,7.69049170913725);
#18651=CIRCLE('',#74748,7.68602777328572);
#18652=CIRCLE('',#74749,7.68475579598828);
#18653=CIRCLE('',#74750,7.69049144376189);
#18654=CIRCLE('',#74752,7.6860275519339);
#18655=CIRCLE('',#74753,7.6847555903237);
#18656=CIRCLE('',#74754,7.69049150439373);
#18657=CIRCLE('',#74756,7.686027572523);
#18658=CIRCLE('',#74757,7.68475576796661);
#18659=CIRCLE('',#74758,7.69049166867953);
#18660=CIRCLE('',#74760,7.68602749781699);
#18661=CIRCLE('',#74761,7.68475564415941);
#18662=CIRCLE('',#74762,7.69049175623011);
#18663=CIRCLE('',#74764,7.68602768679713);
#18664=CIRCLE('',#74765,7.68475579407389);
#18665=CIRCLE('',#74766,7.6904915982339);
#18666=CIRCLE('',#74768,7.68602761932373);
#18667=CIRCLE('',#74769,7.68475551206412);
#18668=CIRCLE('',#74770,7.69049167739998);
#18669=CIRCLE('',#74772,7.68602773560612);
#18670=CIRCLE('',#74773,7.68475597254698);
#18671=CIRCLE('',#74774,7.69049163908932);
#18672=CIRCLE('',#74776,7.68602763499796);
#18673=CIRCLE('',#74777,7.68475561008889);
#18674=CIRCLE('',#74778,7.6904916039111);
#18675=CIRCLE('',#74780,7.68602777697084);
#18676=CIRCLE('',#74781,7.6847552872152);
#18677=CIRCLE('',#74782,7.69049166011924);
#18678=CIRCLE('',#74784,7.68602740222055);
#18679=CIRCLE('',#74785,7.6847559748612);
#18680=CIRCLE('',#74786,7.69049163611726);
#18681=CIRCLE('',#74788,7.68602755640669);
#18682=CIRCLE('',#74789,7.68475572461281);
#18683=CIRCLE('',#74790,7.69049164231659);
#18684=CIRCLE('',#74792,7.68602794546063);
#18685=CIRCLE('',#74793,7.68475546250343);
#18686=CIRCLE('',#74794,7.69049174506469);
#18687=CIRCLE('',#74796,7.6860275018867);
#18688=CIRCLE('',#74797,7.68475596896432);
#18689=CIRCLE('',#74798,7.69049150169301);
#18690=CIRCLE('',#74800,7.68602755868742);
#18691=CIRCLE('',#74801,7.68475566164481);
#18692=CIRCLE('',#74802,7.69049164829637);
#18693=CIRCLE('',#74804,7.6860277100533);
#18694=CIRCLE('',#74805,7.6847557649482);
#18695=CIRCLE('',#74806,7.69049145756513);
#18696=CIRCLE('',#74808,7.68602763433344);
#18697=CIRCLE('',#74809,7.68475571189682);
#18698=CIRCLE('',#74810,7.69049185304065);
#18699=CIRCLE('',#74812,7.68602765932689);
#18700=CIRCLE('',#74813,7.68475566956354);
#18701=CIRCLE('',#74814,7.69049165343505);
#18702=CIRCLE('',#74816,7.68602771109147);
#18703=CIRCLE('',#74817,7.68475539161365);
#18704=CIRCLE('',#74818,7.69049160121944);
#18705=CIRCLE('',#74820,7.68602760824521);
#18706=CIRCLE('',#74821,7.68475571500764);
#18707=CIRCLE('',#74822,7.6904915211749);
#18708=CIRCLE('',#74824,7.68602780856199);
#18709=CIRCLE('',#74825,7.6847557298162);
#18710=CIRCLE('',#74826,7.69049161397159);
#18711=CIRCLE('',#74828,7.68602759104342);
#18712=CIRCLE('',#74829,7.68475569860617);
#18713=CIRCLE('',#74830,7.69049161093906);
#18714=CIRCLE('',#74832,7.68602750154123);
#18715=CIRCLE('',#74833,7.68475569620964);
#18716=CIRCLE('',#74834,7.69071964350128);
#18717=CIRCLE('',#74835,7.69290937402825);
#18718=CIRCLE('',#74837,7.69247305559261);
#18719=CIRCLE('',#74838,7.68510858657417);
#18720=CIRCLE('',#74839,7.69071931991587);
#18721=CIRCLE('',#74840,7.6929095092742);
#18722=CIRCLE('',#74842,7.69247312683449);
#18723=CIRCLE('',#74843,7.68510841365212);
#18724=CIRCLE('',#74844,7.69071947734155);
#18725=CIRCLE('',#74845,7.69290960887181);
#18726=CIRCLE('',#74847,7.6924732208011);
#18727=CIRCLE('',#74848,7.68510854536878);
#18728=CIRCLE('',#74849,7.69071956256004);
#18729=CIRCLE('',#74850,7.69290939950309);
#18730=CIRCLE('',#74852,7.69247301618986);
#18731=CIRCLE('',#74853,7.68510859125701);
#18732=CIRCLE('',#74854,7.69071941009078);
#18733=CIRCLE('',#74855,7.69290942451445);
#18734=CIRCLE('',#74857,7.69247338976127);
#18735=CIRCLE('',#74858,7.68510814883287);
#18736=CIRCLE('',#74859,7.69071972027508);
#18737=CIRCLE('',#74860,7.69290958457193);
#18738=CIRCLE('',#74862,7.6924731006824);
#18739=CIRCLE('',#74863,7.68510844570157);
#18740=CIRCLE('',#74864,7.69071937182503);
#18741=CIRCLE('',#74865,7.69290951045335);
#18742=CIRCLE('',#74867,7.69247329398241);
#18743=CIRCLE('',#74868,7.68510857658084);
#18744=CIRCLE('',#74869,7.69071926896768);
#18745=CIRCLE('',#74870,7.69290926400206);
#18746=CIRCLE('',#74872,7.692472965827);
#18747=CIRCLE('',#74873,7.68510829632141);
#18748=CIRCLE('',#74874,7.69071976525315);
#18749=CIRCLE('',#74875,7.69290953088483);
#18750=CIRCLE('',#74877,7.69247297613951);
#18751=CIRCLE('',#74878,7.68510844465906);
#18752=CIRCLE('',#74879,7.69071952736592);
#18753=CIRCLE('',#74880,7.69290961078093);
#18754=CIRCLE('',#74882,7.69247336192443);
#18755=CIRCLE('',#74883,7.68510823576118);
#18756=CIRCLE('',#74884,7.69071910488742);
#18757=CIRCLE('',#74885,7.69290954220584);
#18758=CIRCLE('',#74887,7.69247305116375);
#18759=CIRCLE('',#74888,7.68510837553656);
#18760=CIRCLE('',#74889,7.6907197818452);
#18761=CIRCLE('',#74890,7.69290927403745);
#18762=CIRCLE('',#74892,7.6924731485281);
#18763=CIRCLE('',#74893,7.68510832326911);
#18764=CIRCLE('',#74894,7.69071950406307);
#18765=CIRCLE('',#74895,7.69290936631444);
#18766=CIRCLE('',#74897,7.69247307464989);
#18767=CIRCLE('',#74898,7.68510828425941);
#18768=CIRCLE('',#74899,7.69071946216712);
#18769=CIRCLE('',#74900,7.69290941446719);
#18770=CIRCLE('',#74902,7.69247304873191);
#18771=CIRCLE('',#74903,7.6851083560009);
#18772=CIRCLE('',#74904,7.69071926915612);
#18773=CIRCLE('',#74905,7.6929095789677);
#18774=CIRCLE('',#74907,7.69247302612856);
#18775=CIRCLE('',#74908,7.68510835534118);
#18776=CIRCLE('',#74909,7.69071925895707);
#18777=CIRCLE('',#74910,7.69290940858428);
#18778=CIRCLE('',#74912,7.69247308969198);
#18779=CIRCLE('',#74913,7.68510875718082);
#18780=CIRCLE('',#74914,7.69071945745377);
#18781=CIRCLE('',#74915,7.69290954197672);
#18782=CIRCLE('',#74917,7.69247324003157);
#18783=CIRCLE('',#74918,7.68510829808067);
#18784=CIRCLE('',#74919,7.69071947369913);
#18785=CIRCLE('',#74920,7.69290944451111);
#18786=CIRCLE('',#74922,7.69247321275003);
#18787=CIRCLE('',#74923,7.68510855412572);
#18788=CIRCLE('',#74924,7.6907198263024);
#18789=CIRCLE('',#74925,7.69290958609505);
#18790=CIRCLE('',#74927,7.69247307307029);
#18791=CIRCLE('',#74928,7.68510848229127);
#18792=CIRCLE('',#74929,7.69071931272457);
#18793=CIRCLE('',#74930,7.69290934384014);
#18794=CIRCLE('',#74932,7.69247294135857);
#18795=CIRCLE('',#74933,7.68510825693569);
#18796=CIRCLE('',#74934,7.69071969279383);
#18797=CIRCLE('',#74935,7.69290930370595);
#18798=CIRCLE('',#74937,7.69247310846389);
#18799=CIRCLE('',#74938,7.68510846585307);
#18800=CIRCLE('',#74939,7.69071948749216);
#18801=CIRCLE('',#74940,7.69290949403575);
#18802=CIRCLE('',#74942,7.69247315728539);
#18803=CIRCLE('',#74943,7.68510834082781);
#18804=CIRCLE('',#74944,7.69071939997457);
#18805=CIRCLE('',#74945,7.69290952855682);
#18806=CIRCLE('',#74947,7.69247303776945);
#18807=CIRCLE('',#74948,7.68510842071755);
#18808=CIRCLE('',#74949,7.69071963796669);
#18809=CIRCLE('',#74950,7.69290955191827);
#18810=CIRCLE('',#74952,7.69247316177193);
#18811=CIRCLE('',#74953,7.68510871141278);
#18812=CIRCLE('',#74954,7.69071941194508);
#18813=CIRCLE('',#74955,7.69290933842463);
#18814=CIRCLE('',#74957,7.69247308417318);
#18815=CIRCLE('',#74958,7.68510847787708);
#18816=CIRCLE('',#74959,7.69071991530501);
#18817=CIRCLE('',#74960,7.69290952062919);
#18818=CIRCLE('',#74962,7.69247329581856);
#18819=CIRCLE('',#74963,7.68510876545971);
#18820=CIRCLE('',#74964,7.6907197867592);
#18821=CIRCLE('',#74965,7.69290935515063);
#18822=CIRCLE('',#74967,7.69247337609866);
#18823=CIRCLE('',#74968,7.68510850861234);
#18824=CIRCLE('',#74969,7.69071945403784);
#18825=CIRCLE('',#74970,7.69290948998167);
#18826=CIRCLE('',#74972,7.69247313314689);
#18827=CIRCLE('',#74973,7.68510869604205);
#18828=CIRCLE('',#74974,7.69071944059307);
#18829=CIRCLE('',#74975,7.69290947143365);
#18830=CIRCLE('',#74977,7.69247316514867);
#18831=CIRCLE('',#74978,7.68510842022998);
#18832=CIRCLE('',#74979,7.44380002391397);
#18833=CIRCLE('',#74980,7.44379988874145);
#18834=CIRCLE('',#74981,7.44379993329164);
#18835=CIRCLE('',#74982,7.44380010832843);
#18836=CIRCLE('',#74983,7.44379991927684);
#18837=CIRCLE('',#74984,7.44379996464395);
#18838=CIRCLE('',#74985,7.44379988209734);
#18839=CIRCLE('',#74986,7.44380007941013);
#18840=CIRCLE('',#74987,7.44380009743758);
#18841=CIRCLE('',#74988,7.44380000595013);
#18842=CIRCLE('',#74989,7.44380013326231);
#18843=CIRCLE('',#74990,7.44379982184739);
#18844=CIRCLE('',#74991,7.44380001233149);
#18845=CIRCLE('',#74992,7.44379999221544);
#18846=CIRCLE('',#74993,7.44380023882436);
#18847=CIRCLE('',#74994,7.44379986021619);
#18848=CIRCLE('',#74995,7.44380004659804);
#18849=CIRCLE('',#74996,7.443799928756);
#18850=CIRCLE('',#74997,7.44380004662724);
#18851=CIRCLE('',#74998,7.44380011330874);
#18852=CIRCLE('',#74999,7.44379977393382);
#18853=CIRCLE('',#75000,7.44379999983162);
#18854=CIRCLE('',#75001,7.4437998681116);
#18855=CIRCLE('',#75002,7.44379987082435);
#18856=CIRCLE('',#75003,7.44380008391067);
#18857=CIRCLE('',#75004,7.44379991228719);
#18858=CIRCLE('',#75005,7.44380010924942);
#18859=CIRCLE('',#75006,7.44379986338863);
#18860=CIRCLE('',#75007,7.44379982284248);
#18861=CIRCLE('',#75008,7.4484934050301);
#18862=CIRCLE('',#75009,7.44849353356002);
#18863=CIRCLE('',#75010,7.44849326907406);
#18864=CIRCLE('',#75011,7.44849352280214);
#18865=CIRCLE('',#75012,7.44849342827269);
#18866=CIRCLE('',#75013,7.44849355988569);
#18867=CIRCLE('',#75014,7.4484931655973);
#18868=CIRCLE('',#75015,7.44849349295533);
#18869=CIRCLE('',#75016,7.44849326543234);
#18870=CIRCLE('',#75017,7.44849328197373);
#18871=CIRCLE('',#75018,7.44849352929703);
#18872=CIRCLE('',#75019,7.44849369791231);
#18873=CIRCLE('',#75020,7.44849332823307);
#18874=CIRCLE('',#75021,7.44849313701309);
#18875=CIRCLE('',#75022,7.44849327087256);
#18876=CIRCLE('',#75023,7.44849366004089);
#18877=CIRCLE('',#75024,7.44849335581452);
#18878=CIRCLE('',#75025,7.44849343783287);
#18879=CIRCLE('',#75026,7.44849348296527);
#18880=CIRCLE('',#75027,7.44849352337264);
#18881=CIRCLE('',#75028,7.44849316873619);
#18882=CIRCLE('',#75029,7.4484930581785);
#18883=CIRCLE('',#75030,7.44849340237214);
#18884=CIRCLE('',#75031,7.4484933646783);
#18885=CIRCLE('',#75032,7.44849311306844);
#18886=CIRCLE('',#75033,7.44849351728013);
#18887=CIRCLE('',#75034,7.44849339086825);
#18888=CIRCLE('',#75035,7.44849329819119);
#18889=CIRCLE('',#75036,7.44849349744587);
#18890=CIRCLE('',#75037,7.68866066419057);
#18891=CIRCLE('',#75039,7.69242169940883);
#18892=CIRCLE('',#75040,7.68493056987366);
#18893=CIRCLE('',#75041,7.68866083559874);
#18894=CIRCLE('',#75043,7.69242134353274);
#18895=CIRCLE('',#75044,7.68493057966198);
#18896=CIRCLE('',#75045,7.68866052233263);
#18897=CIRCLE('',#75047,7.69242148555441);
#18898=CIRCLE('',#75048,7.6849306508943);
#18899=CIRCLE('',#75049,7.68866073227249);
#18900=CIRCLE('',#75051,7.69242137324144);
#18901=CIRCLE('',#75052,7.68493089713476);
#18902=CIRCLE('',#75053,7.68866055304563);
#18903=CIRCLE('',#75055,7.69242172920828);
#18904=CIRCLE('',#75056,7.68493074123893);
#18905=CIRCLE('',#75057,7.68866094033109);
#18906=CIRCLE('',#75059,7.69242158192493);
#18907=CIRCLE('',#75060,7.68493060823818);
#18908=CIRCLE('',#75061,7.68866085719634);
#18909=CIRCLE('',#75063,7.69242147569298);
#18910=CIRCLE('',#75064,7.68493081691442);
#18911=CIRCLE('',#75065,7.68866062157112);
#18912=CIRCLE('',#75067,7.69242140132481);
#18913=CIRCLE('',#75068,7.68493098751244);
#18914=CIRCLE('',#75069,7.6886606753037);
#18915=CIRCLE('',#75071,7.69242144995276);
#18916=CIRCLE('',#75072,7.68493060396243);
#18917=CIRCLE('',#75073,7.68866084384972);
#18918=CIRCLE('',#75075,7.69242157147528);
#18919=CIRCLE('',#75076,7.6849306822516);
#18920=CIRCLE('',#75077,7.68866063109866);
#18921=CIRCLE('',#75079,7.6924213701606);
#18922=CIRCLE('',#75080,7.68493051561203);
#18923=CIRCLE('',#75081,7.68866059173287);
#18924=CIRCLE('',#75083,7.69242159344046);
#18925=CIRCLE('',#75084,7.68493062385534);
#18926=CIRCLE('',#75085,7.68866063284343);
#18927=CIRCLE('',#75087,7.69242124923371);
#18928=CIRCLE('',#75088,7.68493081278867);
#18929=CIRCLE('',#75089,7.6886608720667);
#18930=CIRCLE('',#75091,7.69242157913419);
#18931=CIRCLE('',#75092,7.68493084754879);
#18932=CIRCLE('',#75093,7.68866055711081);
#18933=CIRCLE('',#75095,7.69242155909154);
#18934=CIRCLE('',#75096,7.68493087550972);
#18935=CIRCLE('',#75097,7.68866089124528);
#18936=CIRCLE('',#75099,7.69242155407184);
#18937=CIRCLE('',#75100,7.6849308899177);
#18938=CIRCLE('',#75101,7.68866092368706);
#18939=CIRCLE('',#75103,7.69242155333496);
#18940=CIRCLE('',#75104,7.68493083551118);
#18941=CIRCLE('',#75105,7.68866067406947);
#18942=CIRCLE('',#75107,7.69242164601768);
#18943=CIRCLE('',#75108,7.68493085548053);
#18944=CIRCLE('',#75109,7.6886606467417);
#18945=CIRCLE('',#75110,7.68866065581878);
#18946=CIRCLE('',#75112,7.69242172154919);
#18947=CIRCLE('',#75113,7.68493083314559);
#18948=CIRCLE('',#75115,7.68866068182422);
#18949=CIRCLE('',#75116,7.69242159733574);
#18950=CIRCLE('',#75117,7.68493077787954);
#18951=CIRCLE('',#75119,7.69242127445083);
#18952=CIRCLE('',#75120,7.68493083815641);
#18953=CIRCLE('',#75121,7.68866066847167);
#18954=CIRCLE('',#75123,7.6924216099892);
#18955=CIRCLE('',#75124,7.68493073504257);
#18956=CIRCLE('',#75125,7.68866096801022);
#18957=CIRCLE('',#75127,7.69242166583259);
#18958=CIRCLE('',#75128,7.68493080608032);
#18959=CIRCLE('',#75129,7.68866070474647);
#18960=CIRCLE('',#75131,7.69242129303047);
#18961=CIRCLE('',#75132,7.68493071252555);
#18962=CIRCLE('',#75133,7.68866043240635);
#18963=CIRCLE('',#75135,7.69242136302723);
#18964=CIRCLE('',#75136,7.68493065757089);
#18965=CIRCLE('',#75137,7.68866061806458);
#18966=CIRCLE('',#75139,7.69242153493746);
#18967=CIRCLE('',#75140,7.68493073461862);
#18968=CIRCLE('',#75141,7.68866080163369);
#18969=CIRCLE('',#75143,7.69242158727534);
#18970=CIRCLE('',#75144,7.68493063280848);
#18971=CIRCLE('',#75145,7.68866076262201);
#18972=CIRCLE('',#75147,7.69242165119922);
#18973=CIRCLE('',#75148,7.68493069139677);
#18974=CIRCLE('',#75149,7.69127081155463);
#18975=CIRCLE('',#75150,7.69127055626591);
#18976=CIRCLE('',#75152,7.6861924517877);
#18977=CIRCLE('',#75153,7.68457503867442);
#18978=CIRCLE('',#75154,7.6912705500939);
#18979=CIRCLE('',#75156,7.68619242340395);
#18980=CIRCLE('',#75157,7.68457492993712);
#18981=CIRCLE('',#75158,7.69127068455703);
#18982=CIRCLE('',#75160,7.68619244919569);
#18983=CIRCLE('',#75161,7.68457463844531);
#18984=CIRCLE('',#75162,7.69127057713307);
#18985=CIRCLE('',#75164,7.68619237618486);
#18986=CIRCLE('',#75165,7.68457487674192);
#18987=CIRCLE('',#75166,7.69127048812816);
#18988=CIRCLE('',#75168,7.68619233802125);
#18989=CIRCLE('',#75169,7.6845748287119);
#18990=CIRCLE('',#75170,7.69127075034649);
#18991=CIRCLE('',#75172,7.68619237967728);
#18992=CIRCLE('',#75173,7.68457479157528);
#18993=CIRCLE('',#75174,7.69127036571813);
#18994=CIRCLE('',#75176,7.68619238988181);
#18995=CIRCLE('',#75177,7.68457461725162);
#18996=CIRCLE('',#75178,7.69127045249863);
#18997=CIRCLE('',#75180,7.68619204829374);
#18998=CIRCLE('',#75181,7.68457453773685);
#18999=CIRCLE('',#75182,7.69127064638078);
#19000=CIRCLE('',#75184,7.68619237600206);
#19001=CIRCLE('',#75185,7.68457478724656);
#19002=CIRCLE('',#75186,7.69127052554701);
#19003=CIRCLE('',#75188,7.68619240585107);
#19004=CIRCLE('',#75189,7.68457487023324);
#19005=CIRCLE('',#75190,7.69127052911353);
#19006=CIRCLE('',#75192,7.68619238696948);
#19007=CIRCLE('',#75193,7.68457496082485);
#19008=CIRCLE('',#75194,7.69127058561488);
#19009=CIRCLE('',#75196,7.68619247930092);
#19010=CIRCLE('',#75197,7.68457506128994);
#19011=CIRCLE('',#75198,7.69127080923463);
#19012=CIRCLE('',#75200,7.68619233888281);
#19013=CIRCLE('',#75201,7.68457463519578);
#19014=CIRCLE('',#75202,7.69127078773471);
#19015=CIRCLE('',#75204,7.68619219935353);
#19016=CIRCLE('',#75205,7.68457470543677);
#19017=CIRCLE('',#75206,7.691270399181);
#19018=CIRCLE('',#75208,7.68619198962228);
#19019=CIRCLE('',#75209,7.68457489833632);
#19020=CIRCLE('',#75210,7.691270688111);
#19021=CIRCLE('',#75212,7.68619233399208);
#19022=CIRCLE('',#75213,7.68457465206514);
#19023=CIRCLE('',#75214,7.69127056208363);
#19024=CIRCLE('',#75216,7.68619215948943);
#19025=CIRCLE('',#75217,7.68457483692094);
#19026=CIRCLE('',#75218,7.6912704118498);
#19027=CIRCLE('',#75220,7.68619216603717);
#19028=CIRCLE('',#75221,7.68457486107603);
#19029=CIRCLE('',#75222,7.69127053799002);
#19030=CIRCLE('',#75224,7.68619226704931);
#19031=CIRCLE('',#75225,7.68457463070158);
#19032=CIRCLE('',#75226,7.69127082549637);
#19033=CIRCLE('',#75228,7.6861921483599);
#19034=CIRCLE('',#75229,7.68457475933392);
#19035=CIRCLE('',#75230,7.69127049467909);
#19036=CIRCLE('',#75232,7.68619245625766);
#19037=CIRCLE('',#75233,7.6845747401418);
#19038=CIRCLE('',#75234,7.69127062955969);
#19039=CIRCLE('',#75236,7.6861923379648);
#19040=CIRCLE('',#75237,7.68457443282951);
#19041=CIRCLE('',#75238,7.69127051810462);
#19042=CIRCLE('',#75240,7.6861922613237);
#19043=CIRCLE('',#75241,7.68457458319326);
#19044=CIRCLE('',#75242,7.6912706708803);
#19045=CIRCLE('',#75244,7.68619213256596);
#19046=CIRCLE('',#75245,7.68457492991314);
#19047=CIRCLE('',#75246,7.69127080600108);
#19048=CIRCLE('',#75248,7.68619218432956);
#19049=CIRCLE('',#75249,7.68457489251587);
#19050=CIRCLE('',#75250,7.69127055889231);
#19051=CIRCLE('',#75252,7.68619230107384);
#19052=CIRCLE('',#75253,7.68457493081918);
#19053=CIRCLE('',#75254,7.69127080456184);
#19054=CIRCLE('',#75256,7.68619211116728);
#19055=CIRCLE('',#75257,7.68457463883207);
#19056=CIRCLE('',#75259,7.68619251400998);
#19057=CIRCLE('',#75260,7.6845748205109);
#19058=CIRCLE('',#75261,7.4427916924565);
#19059=CIRCLE('',#75262,7.44938674509435);
#19060=CIRCLE('',#75263,7.4427916969997);
#19061=CIRCLE('',#75264,7.44938641775046);
#19062=CIRCLE('',#75265,7.44279157245494);
#19063=CIRCLE('',#75266,7.44938658372192);
#19064=CIRCLE('',#75267,7.44279163978452);
#19065=CIRCLE('',#75268,7.44938664447408);
#19066=CIRCLE('',#75269,7.44279166161825);
#19067=CIRCLE('',#75270,7.44938664600266);
#19068=CIRCLE('',#75271,7.4427915705808);
#19069=CIRCLE('',#75272,7.4493866456339);
#19070=CIRCLE('',#75273,7.44279144437261);
#19071=CIRCLE('',#75274,7.44938649240699);
#19072=CIRCLE('',#75275,7.44279172819205);
#19073=CIRCLE('',#75276,7.44938660972169);
#19074=CIRCLE('',#75277,7.44279153983529);
#19075=CIRCLE('',#75278,7.44938661848499);
#19076=CIRCLE('',#75279,7.44279169235746);
#19077=CIRCLE('',#75280,7.4493864391964);
#19078=CIRCLE('',#75281,7.44279154487525);
#19079=CIRCLE('',#75282,7.44938654099421);
#19080=CIRCLE('',#75283,7.44279172011711);
#19081=CIRCLE('',#75284,7.44938658333673);
#19082=CIRCLE('',#75285,7.4427918635513);
#19083=CIRCLE('',#75286,7.44938669306789);
#19084=CIRCLE('',#75287,7.44279156987455);
#19085=CIRCLE('',#75288,7.44938644598266);
#19086=CIRCLE('',#75289,7.44279171868799);
#19087=CIRCLE('',#75290,7.44938674154503);
#19088=CIRCLE('',#75291,7.44279187426517);
#19089=CIRCLE('',#75292,7.44938664065949);
#19090=CIRCLE('',#75293,7.4427917397805);
#19091=CIRCLE('',#75294,7.44938674882648);
#19092=CIRCLE('',#75295,7.44279159211471);
#19093=CIRCLE('',#75296,7.4493864104988);
#19094=CIRCLE('',#75297,7.4427915147825);
#19095=CIRCLE('',#75298,7.44938664409182);
#19096=CIRCLE('',#75299,7.4427916804493);
#19097=CIRCLE('',#75300,7.44938659716179);
#19098=CIRCLE('',#75301,7.44279157690395);
#19099=CIRCLE('',#75302,7.4493866052108);
#19100=CIRCLE('',#75303,7.4427918060999);
#19101=CIRCLE('',#75304,7.44938644404683);
#19102=CIRCLE('',#75305,7.44279173998652);
#19103=CIRCLE('',#75306,7.44938669614659);
#19104=CIRCLE('',#75307,7.44279175403481);
#19105=CIRCLE('',#75308,7.44938643383545);
#19106=CIRCLE('',#75309,7.4427917021702);
#19107=CIRCLE('',#75310,7.44938673694741);
#19108=CIRCLE('',#75311,7.44279179346418);
#19109=CIRCLE('',#75312,7.44938649896921);
#19110=CIRCLE('',#75313,7.44279186948);
#19111=CIRCLE('',#75314,7.44938647943056);
#19112=CIRCLE('',#75315,7.44279152433162);
#19113=CIRCLE('',#75316,7.44938663848424);
#19114=CIRCLE('',#75317,7.44279176344005);
#19115=CIRCLE('',#75318,7.44938662526195);
#19116=CIRCLE('',#75319,7.44244299886662);
#19117=CIRCLE('',#75320,7.44095548421823);
#19118=CIRCLE('',#75321,7.44244298946305);
#19119=CIRCLE('',#75322,7.440954223166);
#19120=CIRCLE('',#75323,7.4424427311987);
#19121=CIRCLE('',#75324,7.44095387434625);
#19122=CIRCLE('',#75325,7.44244277833805);
#19123=CIRCLE('',#75326,7.44095736009521);
#19124=CIRCLE('',#75327,7.44244288256841);
#19125=CIRCLE('',#75328,7.44095752755222);
#19126=CIRCLE('',#75329,7.44244270744006);
#19127=CIRCLE('',#75330,7.44095501712413);
#19128=CIRCLE('',#75331,7.44244304911953);
#19129=CIRCLE('',#75332,7.44095203379445);
#19130=CIRCLE('',#75333,7.44244280952999);
#19131=CIRCLE('',#75334,7.44095769834498);
#19132=CIRCLE('',#75335,7.44244289587029);
#19133=CIRCLE('',#75336,7.44095745023879);
#19134=CIRCLE('',#75337,7.44244302207017);
#19135=CIRCLE('',#75338,7.44095760338765);
#19136=CIRCLE('',#75339,7.44244281563661);
#19137=CIRCLE('',#75340,7.4409577473395);
#19138=CIRCLE('',#75341,7.44244321398108);
#19139=CIRCLE('',#75342,7.44095779132071);
#19140=CIRCLE('',#75343,7.44244315736397);
#19141=CIRCLE('',#75344,7.4409577080112);
#19142=CIRCLE('',#75345,7.44244295675951);
#19143=CIRCLE('',#75346,7.44095736424415);
#19144=CIRCLE('',#75347,7.44244298039767);
#19145=CIRCLE('',#75348,7.44095496920714);
#19146=CIRCLE('',#75349,7.44244271315192);
#19147=CIRCLE('',#75350,7.44095755998995);
#19148=CIRCLE('',#75351,7.44244297307453);
#19149=CIRCLE('',#75352,7.44095766223601);
#19150=CIRCLE('',#75353,7.4424429736192);
#19151=CIRCLE('',#75354,7.440957801943);
#19152=CIRCLE('',#75355,7.44244272416091);
#19153=CIRCLE('',#75356,7.44095740321613);
#19154=CIRCLE('',#75357,7.44244273072479);
#19155=CIRCLE('',#75358,7.44095491418459);
#19156=CIRCLE('',#75359,7.44244311098566);
#19157=CIRCLE('',#75360,7.44095786108218);
#19158=CIRCLE('',#75361,7.44244297361896);
#19159=CIRCLE('',#75362,7.44095570443945);
#19160=CIRCLE('',#75363,7.44244305661406);
#19161=CIRCLE('',#75364,7.44095759956823);
#19162=CIRCLE('',#75365,7.44244283248213);
#19163=CIRCLE('',#75366,7.44095776193031);
#19164=CIRCLE('',#75367,7.44244305468507);
#19165=CIRCLE('',#75368,7.44095754355548);
#19166=CIRCLE('',#75369,7.44244311316591);
#19167=CIRCLE('',#75370,7.4409575180813);
#19168=CIRCLE('',#75371,7.44244309319939);
#19169=CIRCLE('',#75372,7.44095757869953);
#19170=CIRCLE('',#75373,7.44244306799778);
#19171=CIRCLE('',#75374,7.44095769610902);
#19172=CIRCLE('',#75375,7.44244283771634);
#19173=CIRCLE('',#75376,7.44095775953863);
#19174=CIRCLE('',#75377,7.68779987598528);
#19175=CIRCLE('',#75379,7.69213911214462);
#19176=CIRCLE('',#75380,7.6920756369326);
#19177=CIRCLE('',#75381,7.69298007561764);
#19178=CIRCLE('',#75382,7.68780001961496);
#19179=CIRCLE('',#75384,7.69213927835789);
#19180=CIRCLE('',#75385,7.6920757509153);
#19181=CIRCLE('',#75386,7.69297964419018);
#19182=CIRCLE('',#75387,7.68780004212317);
#19183=CIRCLE('',#75389,7.69213902840961);
#19184=CIRCLE('',#75390,7.69207587461716);
#19185=CIRCLE('',#75391,7.69297980034034);
#19186=CIRCLE('',#75392,7.6878001308452);
#19187=CIRCLE('',#75394,7.69213921734648);
#19188=CIRCLE('',#75395,7.69207579361869);
#19189=CIRCLE('',#75396,7.69297983101562);
#19190=CIRCLE('',#75397,7.68780025023278);
#19191=CIRCLE('',#75399,7.69213952883728);
#19192=CIRCLE('',#75400,7.69207580197621);
#19193=CIRCLE('',#75401,7.69297982478878);
#19194=CIRCLE('',#75402,7.68779986441889);
#19195=CIRCLE('',#75404,7.6921392380946);
#19196=CIRCLE('',#75405,7.69207562806071);
#19197=CIRCLE('',#75406,7.69297964858726);
#19198=CIRCLE('',#75407,7.68780017958496);
#19199=CIRCLE('',#75409,7.69213927808702);
#19200=CIRCLE('',#75410,7.69207580973648);
#19201=CIRCLE('',#75411,7.69297955940116);
#19202=CIRCLE('',#75412,7.6878000487883);
#19203=CIRCLE('',#75414,7.69213918193528);
#19204=CIRCLE('',#75415,7.69207557777341);
#19205=CIRCLE('',#75416,7.69297987360811);
#19206=CIRCLE('',#75417,7.68780014906733);
#19207=CIRCLE('',#75419,7.69213903655958);
#19208=CIRCLE('',#75420,7.69207573433436);
#19209=CIRCLE('',#75421,7.69297987702054);
#19210=CIRCLE('',#75422,7.68780012097624);
#19211=CIRCLE('',#75424,7.69213935945283);
#19212=CIRCLE('',#75425,7.69207550113426);
#19213=CIRCLE('',#75426,7.69297981265693);
#19214=CIRCLE('',#75427,7.68780009515455);
#19215=CIRCLE('',#75429,7.69213913633929);
#19216=CIRCLE('',#75430,7.69207588964463);
#19217=CIRCLE('',#75431,7.69297974048077);
#19218=CIRCLE('',#75432,7.6878002419802);
#19219=CIRCLE('',#75434,7.69213925351272);
#19220=CIRCLE('',#75435,7.69207589283663);
#19221=CIRCLE('',#75436,7.69297965290336);
#19222=CIRCLE('',#75437,7.68779998772601);
#19223=CIRCLE('',#75439,7.6921393541975);
#19224=CIRCLE('',#75440,7.6920757304034);
#19225=CIRCLE('',#75441,7.69297967023091);
#19226=CIRCLE('',#75442,7.68779994551434);
#19227=CIRCLE('',#75444,7.69213930088781);
#19228=CIRCLE('',#75445,7.69207559901337);
#19229=CIRCLE('',#75446,7.69297989596743);
#19230=CIRCLE('',#75447,7.68779991185942);
#19231=CIRCLE('',#75449,7.69213917580588);
#19232=CIRCLE('',#75450,7.6920755545249);
#19233=CIRCLE('',#75451,7.69297996142688);
#19234=CIRCLE('',#75452,7.68780013268247);
#19235=CIRCLE('',#75454,7.69213936384868);
#19236=CIRCLE('',#75455,7.69207557960442);
#19237=CIRCLE('',#75456,7.69297986023381);
#19238=CIRCLE('',#75457,7.68780005293755);
#19239=CIRCLE('',#75459,7.69213913010854);
#19240=CIRCLE('',#75460,7.69207585108794);
#19241=CIRCLE('',#75461,7.69297978582869);
#19242=CIRCLE('',#75462,7.68780007656642);
#19243=CIRCLE('',#75464,7.69213921788967);
#19244=CIRCLE('',#75465,7.69207589128317);
#19245=CIRCLE('',#75466,7.69297984684176);
#19246=CIRCLE('',#75467,7.68780010408504);
#19247=CIRCLE('',#75468,7.69298334471343);
#19248=CIRCLE('',#75470,7.69213910727534);
#19249=CIRCLE('',#75471,7.6920757654561);
#19250=CIRCLE('',#75472,7.68779996873446);
#19251=CIRCLE('',#75474,7.69297991901627);
#19252=CIRCLE('',#75475,7.69213930969562);
#19253=CIRCLE('',#75476,7.69207592317019);
#19254=CIRCLE('',#75477,7.68780013382243);
#19255=CIRCLE('',#75479,7.69213942886634);
#19256=CIRCLE('',#75480,7.6920758753375);
#19257=CIRCLE('',#75481,7.69297992907677);
#19258=CIRCLE('',#75482,7.68780029888024);
#19259=CIRCLE('',#75484,7.69213905821546);
#19260=CIRCLE('',#75485,7.69207580074562);
#19261=CIRCLE('',#75486,7.69297961425628);
#19262=CIRCLE('',#75487,7.68779982784028);
#19263=CIRCLE('',#75489,7.69213908924868);
#19264=CIRCLE('',#75490,7.69207556045218);
#19265=CIRCLE('',#75491,7.69298013005251);
#19266=CIRCLE('',#75492,7.68779998030444);
#19267=CIRCLE('',#75494,7.69213921944148);
#19268=CIRCLE('',#75495,7.69207570737084);
#19269=CIRCLE('',#75496,7.69297990621452);
#19270=CIRCLE('',#75497,7.68780008546734);
#19271=CIRCLE('',#75499,7.69213923785092);
#19272=CIRCLE('',#75500,7.69207597549898);
#19273=CIRCLE('',#75501,7.69297993767572);
#19274=CIRCLE('',#75502,7.68780010256743);
#19275=CIRCLE('',#75504,7.69213933368374);
#19276=CIRCLE('',#75505,7.69207574696965);
#19277=CIRCLE('',#75506,7.69297995944248);
#19278=CIRCLE('',#75507,7.68780030910691);
#19279=CIRCLE('',#75509,7.69213941349967);
#19280=CIRCLE('',#75510,7.69207574512427);
#19281=CIRCLE('',#75511,7.69297998602037);
#19282=CIRCLE('',#75512,7.68779983566749);
#19283=CIRCLE('',#75514,7.69213933139663);
#19284=CIRCLE('',#75515,7.69207576875101);
#19285=CIRCLE('',#75516,7.69298010510637);
#19286=CIRCLE('',#75517,7.68749379848418);
#19287=CIRCLE('',#75518,7.68301220936602);
#19288=CIRCLE('',#75520,7.68336765832104);
#19289=CIRCLE('',#75521,7.6919138393445);
#19290=CIRCLE('',#75522,7.68749368284053);
#19291=CIRCLE('',#75523,7.68301221189442);
#19292=CIRCLE('',#75525,7.68336749358452);
#19293=CIRCLE('',#75526,7.69191387505139);
#19294=CIRCLE('',#75527,7.6874936500375);
#19295=CIRCLE('',#75528,7.68301221407298);
#19296=CIRCLE('',#75530,7.68336735652439);
#19297=CIRCLE('',#75531,7.6919140322907);
#19298=CIRCLE('',#75532,7.68749361405354);
#19299=CIRCLE('',#75533,7.68301221215543);
#19300=CIRCLE('',#75535,7.6833673735488);
#19301=CIRCLE('',#75536,7.69191393357619);
#19302=CIRCLE('',#75537,7.6874936404206);
#19303=CIRCLE('',#75538,7.68301221332253);
#19304=CIRCLE('',#75540,7.68336740565764);
#19305=CIRCLE('',#75541,7.69191406168244);
#19306=CIRCLE('',#75542,7.68749365696169);
#19307=CIRCLE('',#75543,7.68301221294907);
#19308=CIRCLE('',#75545,7.68336733055345);
#19309=CIRCLE('',#75546,7.69191418046433);
#19310=CIRCLE('',#75547,7.68749354363047);
#19311=CIRCLE('',#75548,7.68301221095471);
#19312=CIRCLE('',#75550,7.68336738565683);
#19313=CIRCLE('',#75551,7.69191372264169);
#19314=CIRCLE('',#75552,7.68749349224528);
#19315=CIRCLE('',#75553,7.68301221064353);
#19316=CIRCLE('',#75555,7.68336738932367);
#19317=CIRCLE('',#75556,7.69191396675306);
#19318=CIRCLE('',#75557,7.68749348186479);
#19319=CIRCLE('',#75558,7.68301221199004);
#19320=CIRCLE('',#75560,7.68336735043043);
#19321=CIRCLE('',#75561,7.69191399165648);
#19322=CIRCLE('',#75562,7.6874936906741);
#19323=CIRCLE('',#75563,7.6830122101649);
#19324=CIRCLE('',#75565,7.68336749295722);
#19325=CIRCLE('',#75566,7.69191368406498);
#19326=CIRCLE('',#75567,7.68749375958476);
#19327=CIRCLE('',#75568,7.68301221355929);
#19328=CIRCLE('',#75570,7.68336761356554);
#19329=CIRCLE('',#75571,7.69191369346876);
#19330=CIRCLE('',#75572,7.68749349900514);
#19331=CIRCLE('',#75573,7.68301221076865);
#19332=CIRCLE('',#75575,7.68336753179772);
#19333=CIRCLE('',#75576,7.69191383055458);
#19334=CIRCLE('',#75577,7.68749375089716);
#19335=CIRCLE('',#75578,7.68301221150777);
#19336=CIRCLE('',#75580,7.68336747881597);
#19337=CIRCLE('',#75581,7.69191397460675);
#19338=CIRCLE('',#75582,7.68749352075251);
#19339=CIRCLE('',#75583,7.68301221097374);
#19340=CIRCLE('',#75585,7.68336756935006);
#19341=CIRCLE('',#75586,7.69191398566389);
#19342=CIRCLE('',#75587,7.68749364370246);
#19343=CIRCLE('',#75588,7.68301221186137);
#19344=CIRCLE('',#75590,7.68336744364852);
#19345=CIRCLE('',#75591,7.69191378010229);
#19346=CIRCLE('',#75592,7.68749362324088);
#19347=CIRCLE('',#75593,7.68301221420808);
#19348=CIRCLE('',#75595,7.68336717811929);
#19349=CIRCLE('',#75596,7.69191369357022);
#19350=CIRCLE('',#75597,7.68749372241741);
#19351=CIRCLE('',#75598,7.68301221285528);
#19352=CIRCLE('',#75600,7.68336758509296);
#19353=CIRCLE('',#75601,7.69191402168073);
#19354=CIRCLE('',#75602,7.68749342450953);
#19355=CIRCLE('',#75603,7.68301221387731);
#19356=CIRCLE('',#75605,7.68336728225106);
#19357=CIRCLE('',#75606,7.69191373128225);
#19358=CIRCLE('',#75607,7.68749330062709);
#19359=CIRCLE('',#75608,7.68301221092703);
#19360=CIRCLE('',#75610,7.6833673135599);
#19361=CIRCLE('',#75611,7.69191383199074);
#19362=CIRCLE('',#75612,7.68749350532316);
#19363=CIRCLE('',#75613,7.68301220914882);
#19364=CIRCLE('',#75615,7.68336732981034);
#19365=CIRCLE('',#75616,7.69191374607332);
#19366=CIRCLE('',#75617,7.68749344497074);
#19367=CIRCLE('',#75618,7.68301221052208);
#19368=CIRCLE('',#75620,7.68336743835863);
#19369=CIRCLE('',#75621,7.6919136898869);
#19370=CIRCLE('',#75622,7.68749352925105);
#19371=CIRCLE('',#75623,7.6830122108982);
#19372=CIRCLE('',#75625,7.68336749193465);
#19373=CIRCLE('',#75626,7.69191374707215);
#19374=CIRCLE('',#75627,7.68749342834959);
#19375=CIRCLE('',#75628,7.68301221156059);
#19376=CIRCLE('',#75630,7.68336746141577);
#19377=CIRCLE('',#75631,7.69191379733266);
#19378=CIRCLE('',#75632,7.68749361435392);
#19379=CIRCLE('',#75633,7.68301221014136);
#19380=CIRCLE('',#75635,7.68336753222251);
#19381=CIRCLE('',#75636,7.69191372571);
#19382=CIRCLE('',#75637,7.68749381076509);
#19383=CIRCLE('',#75638,7.68301221123153);
#19384=CIRCLE('',#75640,7.68336754629794);
#19385=CIRCLE('',#75641,7.69191383423275);
#19386=CIRCLE('',#75642,7.68749342355177);
#19387=CIRCLE('',#75643,7.68301221354761);
#19388=CIRCLE('',#75645,7.68336748605867);
#19389=CIRCLE('',#75646,7.6919137494078);
#19390=CIRCLE('',#75647,7.68749358233999);
#19391=CIRCLE('',#75648,7.68301221002473);
#19392=CIRCLE('',#75650,7.68336726913135);
#19393=CIRCLE('',#75651,7.69191389093633);
#19394=CIRCLE('',#75652,7.68749376897362);
#19395=CIRCLE('',#75653,7.68301221192537);
#19396=CIRCLE('',#75655,7.68336744990501);
#19397=CIRCLE('',#75656,7.69191370262879);
#19398=CIRCLE('',#75657,7.44803384851454);
#19399=CIRCLE('',#75658,7.44913450462972);
#19400=CIRCLE('',#75659,7.44803398219469);
#19401=CIRCLE('',#75660,7.44913469696842);
#19402=CIRCLE('',#75661,7.44803387896228);
#19403=CIRCLE('',#75662,7.44913455497489);
#19404=CIRCLE('',#75663,7.44803375459079);
#19405=CIRCLE('',#75664,7.44913437189458);
#19406=CIRCLE('',#75665,7.44803357474873);
#19407=CIRCLE('',#75666,7.44913453499902);
#19408=CIRCLE('',#75667,7.44803385001612);
#19409=CIRCLE('',#75668,7.44913451718387);
#19410=CIRCLE('',#75669,7.44803391202732);
#19411=CIRCLE('',#75670,7.44913461578382);
#19412=CIRCLE('',#75671,7.44803360525087);
#19413=CIRCLE('',#75672,7.4491345971037);
#19414=CIRCLE('',#75673,7.44803378927701);
#19415=CIRCLE('',#75674,7.44913432274363);
#19416=CIRCLE('',#75675,7.44803368961488);
#19417=CIRCLE('',#75676,7.44913456568358);
#19418=CIRCLE('',#75677,7.44803365322234);
#19419=CIRCLE('',#75678,7.44913480209481);
#19420=CIRCLE('',#75679,7.44803390829095);
#19421=CIRCLE('',#75680,7.44913460310339);
#19422=CIRCLE('',#75681,7.44803389391838);
#19423=CIRCLE('',#75682,7.44913450509804);
#19424=CIRCLE('',#75683,7.44803392620582);
#19425=CIRCLE('',#75684,7.44913469047441);
#19426=CIRCLE('',#75685,7.44803382347946);
#19427=CIRCLE('',#75686,7.44913463784643);
#19428=CIRCLE('',#75687,7.44803355457882);
#19429=CIRCLE('',#75688,7.44913452161491);
#19430=CIRCLE('',#75689,7.4480337889387);
#19431=CIRCLE('',#75690,7.44913473774987);
#19432=CIRCLE('',#75691,7.448033913198);
#19433=CIRCLE('',#75692,7.44913445044758);
#19434=CIRCLE('',#75693,7.44803397228211);
#19435=CIRCLE('',#75694,7.44913447637274);
#19436=CIRCLE('',#75695,7.44803364060588);
#19437=CIRCLE('',#75696,7.44913448737058);
#19438=CIRCLE('',#75697,7.4480336731345);
#19439=CIRCLE('',#75698,7.44913441547656);
#19440=CIRCLE('',#75699,7.44803395858171);
#19441=CIRCLE('',#75700,7.44913447418484);
#19442=CIRCLE('',#75701,7.44803370781974);
#19443=CIRCLE('',#75702,7.44913452595731);
#19444=CIRCLE('',#75703,7.44803398418143);
#19445=CIRCLE('',#75704,7.44913433288211);
#19446=CIRCLE('',#75705,7.4480338757853);
#19447=CIRCLE('',#75706,7.44913460036394);
#19448=CIRCLE('',#75707,7.44803388492082);
#19449=CIRCLE('',#75708,7.44913465652709);
#19450=CIRCLE('',#75709,7.44803384571758);
#19451=CIRCLE('',#75710,7.44913454636581);
#19452=CIRCLE('',#75711,7.44803400343632);
#19453=CIRCLE('',#75712,7.44913456029597);
#19454=CIRCLE('',#75713,7.44803398483153);
#19455=CIRCLE('',#75714,7.44913457166606);
#19456=CIRCLE('',#75715,7.4413211943494);
#19457=CIRCLE('',#75716,7.44901103064392);
#19458=CIRCLE('',#75717,7.44132095495296);
#19459=CIRCLE('',#75718,7.4490108071008);
#19460=CIRCLE('',#75719,7.44132110146733);
#19461=CIRCLE('',#75720,7.44901084248561);
#19462=CIRCLE('',#75721,7.44132115396875);
#19463=CIRCLE('',#75722,7.4490108478241);
#19464=CIRCLE('',#75723,7.44132088248758);
#19465=CIRCLE('',#75724,7.44901098371057);
#19466=CIRCLE('',#75725,7.44132119244584);
#19467=CIRCLE('',#75726,7.44901084522929);
#19468=CIRCLE('',#75727,7.44132104374616);
#19469=CIRCLE('',#75728,7.4490108674322);
#19470=CIRCLE('',#75729,7.44132094601478);
#19471=CIRCLE('',#75730,7.44901095358382);
#19472=CIRCLE('',#75731,7.44132123695688);
#19473=CIRCLE('',#75732,7.44901100863758);
#19474=CIRCLE('',#75733,7.44132128324603);
#19475=CIRCLE('',#75734,7.44901122973375);
#19476=CIRCLE('',#75735,7.441321102259);
#19477=CIRCLE('',#75736,7.44901091613927);
#19478=CIRCLE('',#75737,7.44132135859951);
#19479=CIRCLE('',#75738,7.44901110309397);
#19480=CIRCLE('',#75739,7.44132112331111);
#19481=CIRCLE('',#75740,7.44901083347829);
#19482=CIRCLE('',#75741,7.44132113658644);
#19483=CIRCLE('',#75742,7.44901114277293);
#19484=CIRCLE('',#75743,7.44132111690915);
#19485=CIRCLE('',#75744,7.44901102648347);
#19486=CIRCLE('',#75745,7.44132120475744);
#19487=CIRCLE('',#75746,7.44901099402831);
#19488=CIRCLE('',#75747,7.44132096463125);
#19489=CIRCLE('',#75748,7.44901083584814);
#19490=CIRCLE('',#75749,7.4413210929216);
#19491=CIRCLE('',#75750,7.4490110982641);
#19492=CIRCLE('',#75751,7.44132132070251);
#19493=CIRCLE('',#75752,7.44901109082903);
#19494=CIRCLE('',#75753,7.44132120601386);
#19495=CIRCLE('',#75754,7.4490109760887);
#19496=CIRCLE('',#75755,7.44132094853748);
#19497=CIRCLE('',#75756,7.44901104573919);
#19498=CIRCLE('',#75757,7.44132133289946);
#19499=CIRCLE('',#75758,7.44901091837957);
#19500=CIRCLE('',#75759,7.44132104242884);
#19501=CIRCLE('',#75760,7.44901110784316);
#19502=CIRCLE('',#75761,7.44132131435686);
#19503=CIRCLE('',#75762,7.44901111063083);
#19504=CIRCLE('',#75763,7.44132116557491);
#19505=CIRCLE('',#75764,7.44901114766872);
#19506=CIRCLE('',#75765,7.44132105308794);
#19507=CIRCLE('',#75766,7.44901111040163);
#19508=CIRCLE('',#75767,7.44132115326213);
#19509=CIRCLE('',#75768,7.44901094168477);
#19510=CIRCLE('',#75769,7.44132132093481);
#19511=CIRCLE('',#75770,7.44901098494123);
#19512=CIRCLE('',#75771,7.44132106569402);
#19513=CIRCLE('',#75772,7.44901109317039);
#19514=CIRCLE('',#75773,7.69071959970527);
#19515=CIRCLE('',#75774,7.69290939170015);
#19516=CIRCLE('',#75776,7.68510869473579);
#19517=CIRCLE('',#75777,7.69247313181522);
#19518=CIRCLE('',#75778,7.69071955964098);
#19519=CIRCLE('',#75779,7.69290924111574);
#19520=CIRCLE('',#75781,7.68510850730758);
#19521=CIRCLE('',#75782,7.69247337495618);
#19522=CIRCLE('',#75783,7.69071987258783);
#19523=CIRCLE('',#75784,7.69290934854507);
#19524=CIRCLE('',#75786,7.68510876399039);
#19525=CIRCLE('',#75787,7.69247329496086);
#19526=CIRCLE('',#75788,7.69071994582592);
#19527=CIRCLE('',#75789,7.69290933421014);
#19528=CIRCLE('',#75791,7.68510847654784);
#19529=CIRCLE('',#75792,7.69247308294324);
#19530=CIRCLE('',#75793,7.69071960871418);
#19531=CIRCLE('',#75794,7.69290940799771);
#19532=CIRCLE('',#75796,7.68510870977505);
#19533=CIRCLE('',#75797,7.69247316111689);
#19534=CIRCLE('',#75798,7.69071969948865);
#19535=CIRCLE('',#75799,7.6929094723082);
#19536=CIRCLE('',#75801,7.68510841922913);
#19537=CIRCLE('',#75802,7.69247303678556);
#19538=CIRCLE('',#75803,7.69071954763419);
#19539=CIRCLE('',#75804,7.69290907104058);
#19540=CIRCLE('',#75806,7.68510846447336);
#19541=CIRCLE('',#75807,7.69247310718083);
#19542=CIRCLE('',#75808,7.69071966170006);
#19543=CIRCLE('',#75809,7.69290922853116);
#19544=CIRCLE('',#75811,7.68510825538929);
#19545=CIRCLE('',#75812,7.69247294051526);
#19546=CIRCLE('',#75813,7.69071939845317);
#19547=CIRCLE('',#75814,7.69290936931524);
#19548=CIRCLE('',#75816,7.68510848083308);
#19549=CIRCLE('',#75817,7.69247307202873);
#19550=CIRCLE('',#75818,7.69071981594158);
#19551=CIRCLE('',#75819,7.6929093391863);
#19552=CIRCLE('',#75821,7.68510855261831);
#19553=CIRCLE('',#75822,7.69247321174325);
#19554=CIRCLE('',#75823,7.69071957035312);
#19555=CIRCLE('',#75824,7.69290951603948);
#19556=CIRCLE('',#75826,7.68510829636783);
#19557=CIRCLE('',#75827,7.69247323943103);
#19558=CIRCLE('',#75828,7.69071963430168);
#19559=CIRCLE('',#75829,7.6929093702572);
#19560=CIRCLE('',#75831,7.68510875562769);
#19561=CIRCLE('',#75832,7.69247308876346);
#19562=CIRCLE('',#75833,7.69071942344645);
#19563=CIRCLE('',#75834,7.69290950832545);
#19564=CIRCLE('',#75836,7.68510835375617);
#19565=CIRCLE('',#75837,7.69247302527313);
#19566=CIRCLE('',#75838,7.69071939950264);
#19567=CIRCLE('',#75839,7.69290936749314);
#19568=CIRCLE('',#75841,7.68510836777632);
#19569=CIRCLE('',#75842,7.69247305611594);
#19570=CIRCLE('',#75843,7.69071961909296);
#19571=CIRCLE('',#75844,7.69290919018266);
#19572=CIRCLE('',#75846,7.68510828270712);
#19573=CIRCLE('',#75847,7.6924730737966);
#19574=CIRCLE('',#75848,7.69071953135699);
#19575=CIRCLE('',#75849,7.69290916339466);
#19576=CIRCLE('',#75851,7.6851083217593);
#19577=CIRCLE('',#75852,7.69247314750845);
#19578=CIRCLE('',#75853,7.69071986907438);
#19579=CIRCLE('',#75854,7.69290953902085);
#19580=CIRCLE('',#75856,7.68510837394138);
#19581=CIRCLE('',#75857,7.69247305034484);
#19582=CIRCLE('',#75858,7.69071930171358);
#19583=CIRCLE('',#75859,7.69290932887283);
#19584=CIRCLE('',#75860,7.69071977715674);
#19585=CIRCLE('',#75862,7.68510823425748);
#19586=CIRCLE('',#75863,7.69247335097436);
#19587=CIRCLE('',#75864,7.69290935866333);
#19588=CIRCLE('',#75866,7.69071979600336);
#19589=CIRCLE('',#75867,7.68510844318284);
#19590=CIRCLE('',#75868,7.69247297516043);
#19591=CIRCLE('',#75869,7.69290922621531);
#19592=CIRCLE('',#75871,7.68510829481802);
#19593=CIRCLE('',#75872,7.69247296501133);
#19594=CIRCLE('',#75873,7.690719430586);
#19595=CIRCLE('',#75874,7.69290943818744);
#19596=CIRCLE('',#75876,7.6851085752498);
#19597=CIRCLE('',#75877,7.69247329305699);
#19598=CIRCLE('',#75878,7.6907195047278);
#19599=CIRCLE('',#75879,7.69290943255748);
#19600=CIRCLE('',#75881,7.6851084444481);
#19601=CIRCLE('',#75882,7.69247310035162);
#19602=CIRCLE('',#75883,7.69071977042907);
#19603=CIRCLE('',#75884,7.6929094119709);
#19604=CIRCLE('',#75886,7.68510814741828);
#19605=CIRCLE('',#75887,7.69247338886281);
#19606=CIRCLE('',#75888,7.69071960333338);
#19607=CIRCLE('',#75889,7.69290924908488);
#19608=CIRCLE('',#75891,7.68510858977449);
#19609=CIRCLE('',#75892,7.69247301517223);
#19610=CIRCLE('',#75893,7.69071961584303);
#19611=CIRCLE('',#75894,7.69290943617607);
#19612=CIRCLE('',#75896,7.68510854394081);
#19613=CIRCLE('',#75897,7.69247321977988);
#19614=CIRCLE('',#75898,7.69071960742313);
#19615=CIRCLE('',#75899,7.69290947518489);
#19616=CIRCLE('',#75901,7.6851084124167);
#19617=CIRCLE('',#75902,7.692473125738);
#19618=CIRCLE('',#75903,7.69071948944326);
#19619=CIRCLE('',#75904,7.69290916341741);
#19620=CIRCLE('',#75906,7.68510858529319);
#19621=CIRCLE('',#75907,7.69247305436387);
#19622=CIRCLE('',#75908,7.69071973580169);
#19623=CIRCLE('',#75910,7.68510842030487);
#19624=CIRCLE('',#75911,7.69247333638098);
#19625=CIRCLE('',#75912,7.69290942736885);
#19626=CIRCLE('',#75913,7.68652125258421);
#19627=CIRCLE('',#75914,7.69282875740582);
#19628=CIRCLE('',#75915,7.68652100331372);
#19629=CIRCLE('',#75917,7.6914667428899);
#19630=CIRCLE('',#75918,7.69259295877942);
#19631=CIRCLE('',#75919,7.6928285833299);
#19632=CIRCLE('',#75920,7.68652127594459);
#19633=CIRCLE('',#75922,7.69146681080176);
#19634=CIRCLE('',#75923,7.69259297862081);
#19635=CIRCLE('',#75924,7.69282843296274);
#19636=CIRCLE('',#75925,7.68652090920759);
#19637=CIRCLE('',#75927,7.69146684910729);
#19638=CIRCLE('',#75928,7.69259297478972);
#19639=CIRCLE('',#75929,7.69282860552218);
#19640=CIRCLE('',#75930,7.68652108293123);
#19641=CIRCLE('',#75932,7.69146686813508);
#19642=CIRCLE('',#75933,7.69259330949854);
#19643=CIRCLE('',#75934,7.69282869815639);
#19644=CIRCLE('',#75935,7.68652074921531);
#19645=CIRCLE('',#75937,7.69146690596385);
#19646=CIRCLE('',#75938,7.69259299948719);
#19647=CIRCLE('',#75939,7.6928286906566);
#19648=CIRCLE('',#75940,7.68652109333483);
#19649=CIRCLE('',#75942,7.69146675750791);
#19650=CIRCLE('',#75943,7.6925931093011);
#19651=CIRCLE('',#75944,7.69282869693757);
#19652=CIRCLE('',#75945,7.68652104364437);
#19653=CIRCLE('',#75947,7.69146695632385);
#19654=CIRCLE('',#75948,7.69259310070212);
#19655=CIRCLE('',#75949,7.69282887352166);
#19656=CIRCLE('',#75950,7.68652108043192);
#19657=CIRCLE('',#75952,7.69146699472229);
#19658=CIRCLE('',#75953,7.69259277764863);
#19659=CIRCLE('',#75954,7.69282890930485);
#19660=CIRCLE('',#75955,7.68652092359468);
#19661=CIRCLE('',#75957,7.69146705541028);
#19662=CIRCLE('',#75958,7.69259296496278);
#19663=CIRCLE('',#75959,7.69282843664662);
#19664=CIRCLE('',#75960,7.68652115719435);
#19665=CIRCLE('',#75962,7.69146673705696);
#19666=CIRCLE('',#75963,7.69259321935627);
#19667=CIRCLE('',#75964,7.69282882471994);
#19668=CIRCLE('',#75965,7.68652064772346);
#19669=CIRCLE('',#75967,7.69146698196332);
#19670=CIRCLE('',#75968,7.69259287177747);
#19671=CIRCLE('',#75969,7.69282868899355);
#19672=CIRCLE('',#75970,7.68652103514881);
#19673=CIRCLE('',#75972,7.69146685569191);
#19674=CIRCLE('',#75973,7.69259309981762);
#19675=CIRCLE('',#75974,7.69282854518402);
#19676=CIRCLE('',#75975,7.68652103954227);
#19677=CIRCLE('',#75977,7.69146694444271);
#19678=CIRCLE('',#75978,7.69259317491516);
#19679=CIRCLE('',#75979,7.69282857118346);
#19680=CIRCLE('',#75980,7.68652091557019);
#19681=CIRCLE('',#75982,7.69146693442679);
#19682=CIRCLE('',#75983,7.69259322507444);
#19683=CIRCLE('',#75984,7.69282862399722);
#19684=CIRCLE('',#75985,7.6865210214333);
#19685=CIRCLE('',#75987,7.69146696851046);
#19686=CIRCLE('',#75988,7.69259302665222);
#19687=CIRCLE('',#75989,7.69282879735318);
#19688=CIRCLE('',#75990,7.68652119183878);
#19689=CIRCLE('',#75992,7.6914669639946);
#19690=CIRCLE('',#75993,7.69259292103988);
#19691=CIRCLE('',#75994,7.69282874450741);
#19692=CIRCLE('',#75995,7.68652105551807);
#19693=CIRCLE('',#75997,7.69146714762904);
#19694=CIRCLE('',#75998,7.69259288284633);
#19695=CIRCLE('',#75999,7.69282866315263);
#19696=CIRCLE('',#76000,7.68652089784828);
#19697=CIRCLE('',#76002,7.69146679082288);
#19698=CIRCLE('',#76003,7.69259284738132);
#19699=CIRCLE('',#76004,7.6928286055099);
#19700=CIRCLE('',#76005,7.68652117428447);
#19701=CIRCLE('',#76007,7.69146687423611);
#19702=CIRCLE('',#76008,7.69259312630066);
#19703=CIRCLE('',#76009,7.69282854762959);
#19704=CIRCLE('',#76010,7.68652091794378);
#19705=CIRCLE('',#76012,7.69146693235952);
#19706=CIRCLE('',#76013,7.69259296419184);
#19707=CIRCLE('',#76014,7.6928286411893);
#19708=CIRCLE('',#76015,7.68652109672698);
#19709=CIRCLE('',#76017,7.69146698605118);
#19710=CIRCLE('',#76018,7.69259315091713);
#19711=CIRCLE('',#76019,7.69282866039554);
#19712=CIRCLE('',#76020,7.68652107644955);
#19713=CIRCLE('',#76022,7.69146698903455);
#19714=CIRCLE('',#76023,7.69259283508703);
#19715=CIRCLE('',#76024,7.69282861894892);
#19716=CIRCLE('',#76025,7.68652105529621);
#19717=CIRCLE('',#76027,7.69146674605424);
#19718=CIRCLE('',#76028,7.69259335565016);
#19719=CIRCLE('',#76029,7.69282853049398);
#19720=CIRCLE('',#76030,7.68652116318974);
#19721=CIRCLE('',#76032,7.69146694427004);
#19722=CIRCLE('',#76033,7.69259292454759);
#19723=CIRCLE('',#76034,7.6928285859662);
#19724=CIRCLE('',#76035,7.68652097175582);
#19725=CIRCLE('',#76037,7.6914667707658);
#19726=CIRCLE('',#76038,7.69259272968989);
#19727=CIRCLE('',#76039,7.69282886046399);
#19728=CIRCLE('',#76040,7.68652116672586);
#19729=CIRCLE('',#76042,7.69146683433244);
#19730=CIRCLE('',#76043,7.69259301880423);
#19731=CIRCLE('',#76044,7.69282879163902);
#19732=CIRCLE('',#76045,7.68652116214323);
#19733=CIRCLE('',#76047,7.69146685349496);
#19734=CIRCLE('',#76048,7.69259288894782);
#19735=CIRCLE('',#76050,7.69282889360003);
#19736=CIRCLE('',#76051,7.69146687684282);
#19737=CIRCLE('',#76052,7.69259298503778);
#19738=CIRCLE('',#76053,7.44849410662996);
#19739=CIRCLE('',#76054,7.44849381909938);
#19740=CIRCLE('',#76055,7.44849352954868);
#19741=CIRCLE('',#76056,7.44849366767847);
#19742=CIRCLE('',#76057,7.44849372412611);
#19743=CIRCLE('',#76058,7.44849351536438);
#19744=CIRCLE('',#76059,7.44849386390378);
#19745=CIRCLE('',#76060,7.44849383559205);
#19746=CIRCLE('',#76061,7.44849362513138);
#19747=CIRCLE('',#76062,7.44849403562714);
#19748=CIRCLE('',#76063,7.44849380156);
#19749=CIRCLE('',#76064,7.44849359869955);
#19750=CIRCLE('',#76065,7.44849353315651);
#19751=CIRCLE('',#76066,7.44849367933962);
#19752=CIRCLE('',#76067,7.44849361815174);
#19753=CIRCLE('',#76068,7.44849354947402);
#19754=CIRCLE('',#76069,7.44849360859411);
#19755=CIRCLE('',#76070,7.44849387443723);
#19756=CIRCLE('',#76071,7.44849384303392);
#19757=CIRCLE('',#76072,7.44849367558001);
#19758=CIRCLE('',#76073,7.4484935470774);
#19759=CIRCLE('',#76074,7.44849384385892);
#19760=CIRCLE('',#76075,7.44849359872572);
#19761=CIRCLE('',#76076,7.44849408646692);
#19762=CIRCLE('',#76077,7.44849355781418);
#19763=CIRCLE('',#76078,7.4484936666066);
#19764=CIRCLE('',#76079,7.44849345259137);
#19765=CIRCLE('',#76080,7.44849356703623);
#19766=CIRCLE('',#76081,7.44849370149879);
#19767=CIRCLE('',#76082,7.44865568659265);
#19768=CIRCLE('',#76083,7.44865937960774);
#19769=CIRCLE('',#76084,7.44865913396485);
#19770=CIRCLE('',#76085,7.44865931568455);
#19771=CIRCLE('',#76086,7.44865925259037);
#19772=CIRCLE('',#76087,7.44865929525452);
#19773=CIRCLE('',#76088,7.44865921080257);
#19774=CIRCLE('',#76089,7.44865955529151);
#19775=CIRCLE('',#76090,7.44865928674846);
#19776=CIRCLE('',#76091,7.44865922499772);
#19777=CIRCLE('',#76092,7.44865931108114);
#19778=CIRCLE('',#76093,7.44865928116721);
#19779=CIRCLE('',#76094,7.44865918721158);
#19780=CIRCLE('',#76095,7.44865919870178);
#19781=CIRCLE('',#76096,7.44865899043498);
#19782=CIRCLE('',#76097,7.4486591905494);
#19783=CIRCLE('',#76098,7.44865927813933);
#19784=CIRCLE('',#76099,7.44865918139085);
#19785=CIRCLE('',#76100,7.44865899005308);
#19786=CIRCLE('',#76101,7.44865934134193);
#19787=CIRCLE('',#76102,7.44865927352978);
#19788=CIRCLE('',#76103,7.44865923002346);
#19789=CIRCLE('',#76104,7.44865948062892);
#19790=CIRCLE('',#76105,7.44865965464616);
#19791=CIRCLE('',#76106,7.44865928521786);
#19792=CIRCLE('',#76107,7.4486594721013);
#19793=CIRCLE('',#76108,7.44865959839951);
#19794=CIRCLE('',#76109,7.44865921433909);
#19795=CIRCLE('',#76110,7.44865908323347);
#19796=CIRCLE('',#76111,7.4486593118649);
#19797=CIRCLE('',#76112,7.44865908538773);
#19798=CIRCLE('',#76113,7.44865921583991);
#19799=CIRCLE('',#76114,7.44865905758467);
#19800=CIRCLE('',#76115,7.44865917327891);
#19801=CIRCLE('',#76116,7.44865915459675);
#19802=CIRCLE('',#76117,7.44865925173067);
#19803=CIRCLE('',#76118,7.44865941707331);
#19804=CIRCLE('',#76119,7.44865926585465);
#19805=CIRCLE('',#76120,7.44865916843667);
#19806=CIRCLE('',#76121,7.44865944335422);
#19807=CIRCLE('',#76122,7.448659413303);
#19808=CIRCLE('',#76123,7.44865942691477);
#19809=CIRCLE('',#76124,7.44865940352853);
#19810=CIRCLE('',#76125,7.44865923760662);
#19811=CIRCLE('',#76126,7.4486589261236);
#19812=CIRCLE('',#76127,7.44865921280821);
#19813=CIRCLE('',#76128,7.44865925297232);
#19814=CIRCLE('',#76129,7.44865925983128);
#19815=CIRCLE('',#76130,7.44865905615583);
#19816=CIRCLE('',#76131,7.44865931020424);
#19817=CIRCLE('',#76132,7.44865920703909);
#19818=CIRCLE('',#76133,7.44865931223064);
#19819=CIRCLE('',#76134,7.44865933486815);
#19820=CIRCLE('',#76135,7.44865945618035);
#19821=CIRCLE('',#76136,7.44865951918199);
#19822=CIRCLE('',#76137,7.44865939903092);
#19823=CIRCLE('',#76138,7.44865894316317);
#19824=CIRCLE('',#76139,7.44865840446174);
#19825=CIRCLE('',#76140,7.69127072586956);
#19826=CIRCLE('',#76142,7.68457460674455);
#19827=CIRCLE('',#76143,7.68619211118041);
#19828=CIRCLE('',#76144,7.69127048035928);
#19829=CIRCLE('',#76146,7.6845748989775);
#19830=CIRCLE('',#76147,7.68619230097393);
#19831=CIRCLE('',#76148,7.69127072734795);
#19832=CIRCLE('',#76150,7.68457486072764);
#19833=CIRCLE('',#76151,7.68619218421117);
#19834=CIRCLE('',#76152,7.69127059228028);
#19835=CIRCLE('',#76154,7.68457489788836);
#19836=CIRCLE('',#76155,7.68619213247947);
#19837=CIRCLE('',#76156,7.69127043945911);
#19838=CIRCLE('',#76158,7.68457455052392);
#19839=CIRCLE('',#76159,7.68619226163088);
#19840=CIRCLE('',#76160,7.69127055095902);
#19841=CIRCLE('',#76162,7.68457440060584);
#19842=CIRCLE('',#76163,7.68619233813979);
#19843=CIRCLE('',#76164,7.69127041614661);
#19844=CIRCLE('',#76166,7.68457470784324);
#19845=CIRCLE('',#76167,7.68619245636635);
#19846=CIRCLE('',#76168,7.69127074694672);
#19847=CIRCLE('',#76170,7.68457472723724);
#19848=CIRCLE('',#76171,7.68619214830769);
#19849=CIRCLE('',#76172,7.6912704594167);
#19850=CIRCLE('',#76174,7.68457459816734);
#19851=CIRCLE('',#76175,7.68619226715557);
#19852=CIRCLE('',#76176,7.69127033329633);
#19853=CIRCLE('',#76178,7.68457482854662);
#19854=CIRCLE('',#76179,7.68619216619574);
#19855=CIRCLE('',#76180,7.69127048343821);
#19856=CIRCLE('',#76182,7.68457480457462);
#19857=CIRCLE('',#76183,7.68619215958249);
#19858=CIRCLE('',#76184,7.69127060962555);
#19859=CIRCLE('',#76186,7.68457461941056);
#19860=CIRCLE('',#76187,7.68619233436519);
#19861=CIRCLE('',#76188,7.69127032053058);
#19862=CIRCLE('',#76190,7.68457486588462);
#19863=CIRCLE('',#76191,7.68619198984053);
#19864=CIRCLE('',#76192,7.6912707090811);
#19865=CIRCLE('',#76194,7.68457467311279);
#19866=CIRCLE('',#76195,7.68619219941248);
#19867=CIRCLE('',#76196,7.69127073069181);
#19868=CIRCLE('',#76198,7.68457460246984);
#19869=CIRCLE('',#76199,7.68619233913455);
#19870=CIRCLE('',#76200,7.69127050692399);
#19871=CIRCLE('',#76202,7.68457502878878);
#19872=CIRCLE('',#76203,7.68619247937977);
#19873=CIRCLE('',#76204,7.69127044695868);
#19874=CIRCLE('',#76206,7.68457492840789);
#19875=CIRCLE('',#76207,7.68619238711067);
#19876=CIRCLE('',#76208,7.69127044714542);
#19877=CIRCLE('',#76210,7.68457483781455);
#19878=CIRCLE('',#76211,7.68619239818768);
#19879=CIRCLE('',#76212,7.6912705679341);
#19880=CIRCLE('',#76214,7.68457475473604);
#19881=CIRCLE('',#76215,7.6861923761129);
#19882=CIRCLE('',#76216,7.69127037387414);
#19883=CIRCLE('',#76218,7.68457450488223);
#19884=CIRCLE('',#76219,7.68619204868803);
#19885=CIRCLE('',#76220,7.69127028712799);
#19886=CIRCLE('',#76222,7.68457458476216);
#19887=CIRCLE('',#76223,7.68619239048162);
#19888=CIRCLE('',#76224,7.6912706719256);
#19889=CIRCLE('',#76226,7.6845747590727);
#19890=CIRCLE('',#76227,7.68619238035232);
#19891=CIRCLE('',#76228,7.69127041025873);
#19892=CIRCLE('',#76230,7.68457479696758);
#19893=CIRCLE('',#76231,7.68619233870747);
#19894=CIRCLE('',#76232,7.69127049859815);
#19895=CIRCLE('',#76234,7.68457484445074);
#19896=CIRCLE('',#76235,7.68619237638544);
#19897=CIRCLE('',#76236,7.69127060614202);
#19898=CIRCLE('',#76238,7.68457460589843);
#19899=CIRCLE('',#76239,7.68619244940214);
#19900=CIRCLE('',#76240,7.69127047150333);
#19901=CIRCLE('',#76242,7.68457489791198);
#19902=CIRCLE('',#76243,7.68619242344552);
#19903=CIRCLE('',#76244,7.69127045407736);
#19904=CIRCLE('',#76246,7.68457500660473);
#19905=CIRCLE('',#76247,7.6861924517686);
#19906=CIRCLE('',#76248,7.6912707330029);
#19907=CIRCLE('',#76250,7.68457466228632);
#19908=CIRCLE('',#76251,7.68619251401022);
#19909=CIRCLE('',#76252,7.69146686787997);
#19910=CIRCLE('',#76254,7.82251840653599);
#19911=CIRCLE('',#76255,7.5);
#19912=CIRCLE('',#76256,7.59069481717915);
#19913=CIRCLE('',#76257,7.69258716744121);
#19914=CIRCLE('',#76259,7.68762526081301);
#19915=CIRCLE('',#76260,7.69302723584648);
#19916=CIRCLE('',#76261,7.6914669335521);
#19917=CIRCLE('',#76263,7.8225175300266);
#19918=CIRCLE('',#76264,7.5);
#19919=CIRCLE('',#76265,7.59069440111666);
#19920=CIRCLE('',#76266,7.69258698386699);
#19921=CIRCLE('',#76268,7.6876252599103);
#19922=CIRCLE('',#76269,7.69302682389199);
#19923=CIRCLE('',#76270,7.69146690421046);
#19924=CIRCLE('',#76272,7.82251875480618);
#19925=CIRCLE('',#76273,7.5);
#19926=CIRCLE('',#76274,7.59069338205172);
#19927=CIRCLE('',#76275,7.69258686333969);
#19928=CIRCLE('',#76277,7.68762525574649);
#19929=CIRCLE('',#76278,7.69302727554353);
#19930=CIRCLE('',#76279,7.69146709488188);
#19931=CIRCLE('',#76281,7.82251728176977);
#19932=CIRCLE('',#76282,7.5);
#19933=CIRCLE('',#76283,7.59069543016537);
#19934=CIRCLE('',#76284,7.69258682496256);
#19935=CIRCLE('',#76286,7.68762526082337);
#19936=CIRCLE('',#76287,7.69302713009884);
#19937=CIRCLE('',#76288,7.69146671807737);
#19938=CIRCLE('',#76290,7.82251832350922);
#19939=CIRCLE('',#76291,7.5);
#19940=CIRCLE('',#76292,7.59069396884935);
#19941=CIRCLE('',#76293,7.69258678977922);
#19942=CIRCLE('',#76295,7.68762526056082);
#19943=CIRCLE('',#76296,7.69302727988512);
#19944=CIRCLE('',#76297,7.69146679685476);
#19945=CIRCLE('',#76299,7.82251933308047);
#19946=CIRCLE('',#76300,7.5);
#19947=CIRCLE('',#76301,7.59069343155577);
#19948=CIRCLE('',#76302,7.69258706872097);
#19949=CIRCLE('',#76304,7.68762525718788);
#19950=CIRCLE('',#76305,7.69302681329328);
#19951=CIRCLE('',#76306,7.69146687729561);
#19952=CIRCLE('',#76308,7.82251862585163);
#19953=CIRCLE('',#76309,7.5);
#19954=CIRCLE('',#76310,7.59069479464637);
#19955=CIRCLE('',#76311,7.6925869064859);
#19956=CIRCLE('',#76313,7.68762525251179);
#19957=CIRCLE('',#76314,7.69302733400162);
#19958=CIRCLE('',#76315,7.69146691743636);
#19959=CIRCLE('',#76317,7.82250967679436);
#19960=CIRCLE('',#76318,7.50000000248332);
#19961=CIRCLE('',#76319,7.59068816853269);
#19962=CIRCLE('',#76320,7.69258709343339);
#19963=CIRCLE('',#76322,7.68762523296301);
#19964=CIRCLE('',#76323,7.6930279875728);
#19965=CIRCLE('',#76324,7.69146692446018);
#19966=CIRCLE('',#76326,7.8225175108103);
#19967=CIRCLE('',#76327,7.49999999940595);
#19968=CIRCLE('',#76328,7.59069378897348);
#19969=CIRCLE('',#76329,7.6925867774697);
#19970=CIRCLE('',#76331,7.68762526045872);
#19971=CIRCLE('',#76332,7.69302685790954);
#19972=CIRCLE('',#76333,7.69146666499951);
#19973=CIRCLE('',#76335,7.8225186365657);
#19974=CIRCLE('',#76336,7.5);
#19975=CIRCLE('',#76337,7.5906952985796);
#19976=CIRCLE('',#76338,7.69258729805551);
#19977=CIRCLE('',#76340,7.68762525347159);
#19978=CIRCLE('',#76341,7.69302718749449);
#19979=CIRCLE('',#76342,7.69146686263873);
#19980=CIRCLE('',#76344,7.82251721175383);
#19981=CIRCLE('',#76345,7.5);
#19982=CIRCLE('',#76346,7.59069451273781);
#19983=CIRCLE('',#76347,7.69258686754086);
#19984=CIRCLE('',#76349,7.68762526096746);
#19985=CIRCLE('',#76350,7.69302674459465);
#19986=CIRCLE('',#76351,7.69146671373895);
#19987=CIRCLE('',#76353,7.82251808428171);
#19988=CIRCLE('',#76354,7.5);
#19989=CIRCLE('',#76355,7.59069374492181);
#19990=CIRCLE('',#76356,7.69258667231221);
#19991=CIRCLE('',#76358,7.68762525764248);
#19992=CIRCLE('',#76359,7.69302694483297);
#19993=CIRCLE('',#76360,7.6914667777091);
#19994=CIRCLE('',#76362,7.82251948114017);
#19995=CIRCLE('',#76363,7.5);
#19996=CIRCLE('',#76364,7.59069550339663);
#19997=CIRCLE('',#76365,7.69258696142463);
#19998=CIRCLE('',#76367,7.68762525340374);
#19999=CIRCLE('',#76368,7.69302753262858);
#20000=CIRCLE('',#76369,7.69146682910809);
#20001=CIRCLE('',#76371,7.82251845684075);
#20002=CIRCLE('',#76372,7.4999999942942);
#20003=CIRCLE('',#76373,7.59069770697273);
#20004=CIRCLE('',#76374,7.69258687256424);
#20005=CIRCLE('',#76376,7.68762525883221);
#20006=CIRCLE('',#76377,7.69302540852278);
#20007=CIRCLE('',#76378,7.69146682537179);
#20008=CIRCLE('',#76380,7.82251740569397);
#20009=CIRCLE('',#76381,7.5);
#20010=CIRCLE('',#76382,7.5906938352263);
#20011=CIRCLE('',#76383,7.69258692758798);
#20012=CIRCLE('',#76385,7.68762526064097);
#20013=CIRCLE('',#76386,7.69302747298765);
#20014=CIRCLE('',#76387,7.69146668182604);
#20015=CIRCLE('',#76389,7.82249259703888);
#20016=CIRCLE('',#76390,7.50000000673024);
#20017=CIRCLE('',#76391,7.59066676519396);
#20018=CIRCLE('',#76392,7.69258690134813);
#20019=CIRCLE('',#76394,7.68762517911986);
#20020=CIRCLE('',#76395,7.69303027347115);
#20021=CIRCLE('',#76396,7.69146681677351);
#20022=CIRCLE('',#76398,7.82252001763851);
#20023=CIRCLE('',#76399,7.5);
#20024=CIRCLE('',#76400,7.5906957203843);
#20025=CIRCLE('',#76401,7.6925869212363);
#20026=CIRCLE('',#76403,7.68762525249949);
#20027=CIRCLE('',#76404,7.69302688449732);
#20028=CIRCLE('',#76405,7.6914667677436);
#20029=CIRCLE('',#76407,7.82251273949175);
#20030=CIRCLE('',#76408,7.50000000064172);
#20031=CIRCLE('',#76409,7.59069442908617);
#20032=CIRCLE('',#76410,7.69258691740677);
#20033=CIRCLE('',#76412,7.68762525458648);
#20034=CIRCLE('',#76413,7.69302693606317);
#20035=CIRCLE('',#76414,7.69146678671437);
#20036=CIRCLE('',#76416,7.8225191103349);
#20037=CIRCLE('',#76417,7.5);
#20038=CIRCLE('',#76418,7.59069367691366);
#20039=CIRCLE('',#76419,7.6925872519601);
#20040=CIRCLE('',#76421,7.68762525742582);
#20041=CIRCLE('',#76422,7.69302681144429);
#20042=CIRCLE('',#76423,7.69146690370976);
#20043=CIRCLE('',#76425,7.82252001537044);
#20044=CIRCLE('',#76426,7.5);
#20045=CIRCLE('',#76427,7.59069563834516);
#20046=CIRCLE('',#76428,7.69258694194281);
#20047=CIRCLE('',#76430,7.68762525324496);
#20048=CIRCLE('',#76431,7.69302701810835);
#20049=CIRCLE('',#76432,7.69146668394716);
#20050=CIRCLE('',#76434,7.8225179891651);
#20051=CIRCLE('',#76435,7.5);
#20052=CIRCLE('',#76436,7.59069461311006);
#20053=CIRCLE('',#76437,7.69258705176433);
#20054=CIRCLE('',#76439,7.68762526126733);
#20055=CIRCLE('',#76440,7.6930269002785);
#20056=CIRCLE('',#76441,7.69146695448782);
#20057=CIRCLE('',#76443,7.82251924419094);
#20058=CIRCLE('',#76444,7.5);
#20059=CIRCLE('',#76445,7.5906956283804);
#20060=CIRCLE('',#76446,7.69258672080425);
#20061=CIRCLE('',#76448,7.68762525373694);
#20062=CIRCLE('',#76449,7.69302738155323);
#20063=CIRCLE('',#76450,7.69146697187919);
#20064=CIRCLE('',#76452,7.82251727378208);
#20065=CIRCLE('',#76453,7.5);
#20066=CIRCLE('',#76454,7.59069479425888);
#20067=CIRCLE('',#76455,7.69258690733685);
#20068=CIRCLE('',#76457,7.68762526044002);
#20069=CIRCLE('',#76458,7.69302754569702);
#20070=CIRCLE('',#76459,7.69146666607425);
#20071=CIRCLE('',#76461,7.59069441948473);
#20072=CIRCLE('',#76462,7.82251798645301);
#20073=CIRCLE('',#76463,7.5);
#20074=CIRCLE('',#76464,7.6925871618964);
#20075=CIRCLE('',#76466,7.68762525885893);
#20076=CIRCLE('',#76467,7.69302665420329);
#20077=CIRCLE('',#76468,7.69146689979605);
#20078=CIRCLE('',#76470,7.82251978501935);
#20079=CIRCLE('',#76471,7.5);
#20080=CIRCLE('',#76472,7.59069590106119);
#20081=CIRCLE('',#76473,7.69258681409144);
#20082=CIRCLE('',#76475,7.6876252550984);
#20083=CIRCLE('',#76476,7.69302724211033);
#20084=CIRCLE('',#76477,7.69146681916298);
#20085=CIRCLE('',#76479,7.82249229350671);
#20086=CIRCLE('',#76480,7.50000000534226);
#20087=CIRCLE('',#76481,7.59067387639011);
#20088=CIRCLE('',#76482,7.69258704209278);
#20089=CIRCLE('',#76484,7.68762520350044);
#20090=CIRCLE('',#76485,7.69302958178729);
#20091=CIRCLE('',#76486,7.69146689253006);
#20092=CIRCLE('',#76488,7.82251865702507);
#20093=CIRCLE('',#76489,7.5);
#20094=CIRCLE('',#76490,7.5906939527085);
#20095=CIRCLE('',#76491,7.69258711727703);
#20096=CIRCLE('',#76493,7.68762525990507);
#20097=CIRCLE('',#76494,7.69302679994652);
#20098=CIRCLE('',#76495,7.69146679484481);
#20099=CIRCLE('',#76497,7.82251964766403);
#20100=CIRCLE('',#76498,7.5);
#20101=CIRCLE('',#76499,7.59069606874455);
#20102=CIRCLE('',#76500,7.6925871115328);
#20103=CIRCLE('',#76502,7.68762525495669);
#20104=CIRCLE('',#76503,7.693027073272);
#20105=CIRCLE('',#76504,7.44244283769794);
#20106=CIRCLE('',#76505,7.44095770943715);
#20107=CIRCLE('',#76506,7.44244306799496);
#20108=CIRCLE('',#76507,7.44095757010981);
#20109=CIRCLE('',#76508,7.44244309319976);
#20110=CIRCLE('',#76509,7.44095742817923);
#20111=CIRCLE('',#76510,7.44244311316663);
#20112=CIRCLE('',#76511,7.44095754355266);
#20113=CIRCLE('',#76512,7.44244305468164);
#20114=CIRCLE('',#76513,7.44095776188464);
#20115=CIRCLE('',#76514,7.44244283248188);
#20116=CIRCLE('',#76515,7.44095758755588);
#20117=CIRCLE('',#76516,7.44244305661218);
#20118=CIRCLE('',#76517,7.44095764658766);
#20119=CIRCLE('',#76518,7.44244297361853);
#20120=CIRCLE('',#76519,7.44095787039397);
#20121=CIRCLE('',#76520,7.44244311098298);
#20122=CIRCLE('',#76521,7.44095785023995);
#20123=CIRCLE('',#76522,7.44244273072371);
#20124=CIRCLE('',#76523,7.4409574148811);
#20125=CIRCLE('',#76524,7.44244272416301);
#20126=CIRCLE('',#76525,7.44095780193666);
#20127=CIRCLE('',#76526,7.44244297361728);
#20128=CIRCLE('',#76527,7.440957610396);
#20129=CIRCLE('',#76528,7.4424429730741);
#20130=CIRCLE('',#76529,7.44095755696898);
#20131=CIRCLE('',#76530,7.44244271315511);
#20132=CIRCLE('',#76531,7.44095776333132);
#20133=CIRCLE('',#76532,7.44244298039844);
#20134=CIRCLE('',#76533,7.44095780334038);
#20135=CIRCLE('',#76534,7.44244295675995);
#20136=CIRCLE('',#76535,7.44095761896929);
#20137=CIRCLE('',#76536,7.44244315736419);
#20138=CIRCLE('',#76537,7.44095780583516);
#20139=CIRCLE('',#76538,7.44244321398115);
#20140=CIRCLE('',#76539,7.44095772672058);
#20141=CIRCLE('',#76540,7.44244281563632);
#20142=CIRCLE('',#76541,7.44095770658529);
#20143=CIRCLE('',#76542,7.44244302207351);
#20144=CIRCLE('',#76543,7.44095746764818);
#20145=CIRCLE('',#76544,7.44244289586982);
#20146=CIRCLE('',#76545,7.44095768094371);
#20147=CIRCLE('',#76546,7.44244280952974);
#20148=CIRCLE('',#76547,7.44095773094304);
#20149=CIRCLE('',#76548,7.4424430491187);
#20150=CIRCLE('',#76549,7.44095767432048);
#20151=CIRCLE('',#76550,7.44244270743924);
#20152=CIRCLE('',#76551,7.44095752751371);
#20153=CIRCLE('',#76552,7.44244288256829);
#20154=CIRCLE('',#76553,7.44095736787357);
#20155=CIRCLE('',#76554,7.44244277833773);
#20156=CIRCLE('',#76555,7.44095751266216);
#20157=CIRCLE('',#76556,7.44244273120023);
#20158=CIRCLE('',#76557,7.44095773230911);
#20159=CIRCLE('',#76558,7.44244298946042);
#20160=CIRCLE('',#76559,7.44095782336618);
#20161=CIRCLE('',#76560,7.44244299886607);
#20162=CIRCLE('',#76561,7.44095775950143);
#20163=CIRCLE('',#76562,7.4490144514855);
#20164=CIRCLE('',#76564,7.44132516904529);
#20165=CIRCLE('',#76565,7.44901473192042);
#20166=CIRCLE('',#76567,7.44132484712343);
#20167=CIRCLE('',#76568,7.44901479614434);
#20168=CIRCLE('',#76570,7.44132482041918);
#20169=CIRCLE('',#76571,7.44901479564489);
#20170=CIRCLE('',#76573,7.44132496027544);
#20171=CIRCLE('',#76574,7.44901507868705);
#20172=CIRCLE('',#76576,7.44132520829404);
#20173=CIRCLE('',#76577,7.44901501492555);
#20174=CIRCLE('',#76579,7.44132488589972);
#20175=CIRCLE('',#76580,7.44901478829298);
#20176=CIRCLE('',#76582,7.44132486965578);
#20177=CIRCLE('',#76583,7.44901473111701);
#20178=CIRCLE('',#76585,7.44132485677684);
#20179=CIRCLE('',#76586,7.44901484613321);
#20180=CIRCLE('',#76588,7.44132500892796);
#20181=CIRCLE('',#76589,7.44901483116979);
#20182=CIRCLE('',#76591,7.44132496353816);
#20183=CIRCLE('',#76592,7.44901486184386);
#20184=CIRCLE('',#76594,7.44132491390273);
#20185=CIRCLE('',#76595,7.44901487890267);
#20186=CIRCLE('',#76597,7.44132504759939);
#20187=CIRCLE('',#76598,7.44901483114893);
#20188=CIRCLE('',#76600,7.44132499108792);
#20189=CIRCLE('',#76601,7.44901499426344);
#20190=CIRCLE('',#76603,7.4413246644582);
#20191=CIRCLE('',#76604,7.44901483808788);
#20192=CIRCLE('',#76606,7.44132492098853);
#20193=CIRCLE('',#76607,7.44901479349699);
#20194=CIRCLE('',#76609,7.44132509181846);
#20195=CIRCLE('',#76610,7.44901473074534);
#20196=CIRCLE('',#76612,7.44132489601627);
#20197=CIRCLE('',#76613,7.44901472236486);
#20198=CIRCLE('',#76615,7.44132507039419);
#20199=CIRCLE('',#76616,7.44901483480963);
#20200=CIRCLE('',#76618,7.44132469514174);
#20201=CIRCLE('',#76619,7.44901479709459);
#20202=CIRCLE('',#76621,7.44132504572367);
#20203=CIRCLE('',#76622,7.44901468721301);
#20204=CIRCLE('',#76624,7.44132502969007);
#20205=CIRCLE('',#76625,7.44901473934094);
#20206=CIRCLE('',#76627,7.44132472221971);
#20207=CIRCLE('',#76628,7.44901475240328);
#20208=CIRCLE('',#76630,7.44132510783735);
#20209=CIRCLE('',#76631,7.44901479470681);
#20210=CIRCLE('',#76633,7.4413250143831);
#20211=CIRCLE('',#76634,7.44901503648164);
#20212=CIRCLE('',#76636,7.44132470383829);
#20213=CIRCLE('',#76637,7.44901468881883);
#20214=CIRCLE('',#76639,7.44132501660734);
#20215=CIRCLE('',#76640,7.44901508212225);
#20216=CIRCLE('',#76642,7.44132490803545);
#20217=CIRCLE('',#76643,7.4490147610041);
#20218=CIRCLE('',#76645,7.44132506641251);
#20219=CIRCLE('',#76646,7.44901494283557);
#20220=CIRCLE('',#76648,7.44132440239759);
#20221=CIRCLE('',#76649,7.68749376892044);
#20222=CIRCLE('',#76650,7.68301219198009);
#20223=CIRCLE('',#76652,7.69191389092581);
#20224=CIRCLE('',#76653,7.68336726913004);
#20225=CIRCLE('',#76654,7.68749358218551);
#20226=CIRCLE('',#76655,7.68301219563752);
#20227=CIRCLE('',#76657,7.69191374939714);
#20228=CIRCLE('',#76658,7.68336748606017);
#20229=CIRCLE('',#76659,7.68749342341548);
#20230=CIRCLE('',#76660,7.6830121930893);
#20231=CIRCLE('',#76662,7.69191383422036);
#20232=CIRCLE('',#76663,7.6833675462965);
#20233=CIRCLE('',#76664,7.68749355836631);
#20234=CIRCLE('',#76665,7.68301219225916);
#20235=CIRCLE('',#76667,7.69191372570169);
#20236=CIRCLE('',#76668,7.68336753222351);
#20237=CIRCLE('',#76669,7.68749361423602);
#20238=CIRCLE('',#76670,7.68301219362676);
#20239=CIRCLE('',#76672,7.69191379732158);
#20240=CIRCLE('',#76673,7.68336746141775);
#20241=CIRCLE('',#76674,7.68749342824239);
#20242=CIRCLE('',#76675,7.68301219329349);
#20243=CIRCLE('',#76677,7.69191374706803);
#20244=CIRCLE('',#76678,7.68336749193853);
#20245=CIRCLE('',#76679,7.68749352909174);
#20246=CIRCLE('',#76680,7.68301219252271);
#20247=CIRCLE('',#76682,7.69191368987804);
#20248=CIRCLE('',#76683,7.68336743836054);
#20249=CIRCLE('',#76684,7.68749344500409);
#20250=CIRCLE('',#76685,7.68301219123024);
#20251=CIRCLE('',#76687,7.69191374606969);
#20252=CIRCLE('',#76688,7.68336732981191);
#20253=CIRCLE('',#76689,7.68749350523767);
#20254=CIRCLE('',#76690,7.68301219285518);
#20255=CIRCLE('',#76692,7.6919138319802);
#20256=CIRCLE('',#76693,7.68336731355951);
#20257=CIRCLE('',#76694,7.68749330057477);
#20258=CIRCLE('',#76695,7.68301219615952);
#20259=CIRCLE('',#76697,7.69191373127678);
#20260=CIRCLE('',#76698,7.68336728225312);
#20261=CIRCLE('',#76699,7.68749342441889);
#20262=CIRCLE('',#76700,7.68301219484171);
#20263=CIRCLE('',#76702,7.69191402167153);
#20264=CIRCLE('',#76703,7.68336758509357);
#20265=CIRCLE('',#76704,7.6874937223061);
#20266=CIRCLE('',#76705,7.68301219642771);
#20267=CIRCLE('',#76707,7.69191369356068);
#20268=CIRCLE('',#76708,7.68336717812141);
#20269=CIRCLE('',#76709,7.68749362319715);
#20270=CIRCLE('',#76710,7.68301219414976);
#20271=CIRCLE('',#76712,7.69191378009799);
#20272=CIRCLE('',#76713,7.68336744364646);
#20273=CIRCLE('',#76714,7.68749364365068);
#20274=CIRCLE('',#76715,7.68301219269508);
#20275=CIRCLE('',#76717,7.69191398565423);
#20276=CIRCLE('',#76718,7.6833675693493);
#20277=CIRCLE('',#76719,7.68749352067635);
#20278=CIRCLE('',#76720,7.68301219368827);
#20279=CIRCLE('',#76722,7.69191397459453);
#20280=CIRCLE('',#76723,7.68336747881971);
#20281=CIRCLE('',#76724,7.687493750851);
#20282=CIRCLE('',#76725,7.68301219327867);
#20283=CIRCLE('',#76727,7.6919138305455);
#20284=CIRCLE('',#76728,7.6833675318038);
#20285=CIRCLE('',#76729,7.6874934988961);
#20286=CIRCLE('',#76730,7.68301217777242);
#20287=CIRCLE('',#76731,7.68748726252765);
#20288=CIRCLE('',#76733,7.69191369346136);
#20289=CIRCLE('',#76734,7.68336107784681);
#20290=CIRCLE('',#76735,7.68301219232485);
#20291=CIRCLE('',#76737,7.68749369060519);
#20292=CIRCLE('',#76738,7.69191368405268);
#20293=CIRCLE('',#76739,7.68336749296103);
#20294=CIRCLE('',#76740,7.68301219423829);
#20295=CIRCLE('',#76742,7.69191399164696);
#20296=CIRCLE('',#76743,7.68336735042955);
#20297=CIRCLE('',#76744,7.68749348176495);
#20298=CIRCLE('',#76745,7.68301219268255);
#20299=CIRCLE('',#76747,7.69191396674004);
#20300=CIRCLE('',#76748,7.68336738932368);
#20301=CIRCLE('',#76749,7.6874934921015);
#20302=CIRCLE('',#76750,7.68301219326198);
#20303=CIRCLE('',#76752,7.69191372263682);
#20304=CIRCLE('',#76753,7.68336738565898);
#20305=CIRCLE('',#76754,7.68749354355261);
#20306=CIRCLE('',#76755,7.68301219519444);
#20307=CIRCLE('',#76757,7.69191418045274);
#20308=CIRCLE('',#76758,7.68336733055388);
#20309=CIRCLE('',#76759,7.68749365685344);
#20310=CIRCLE('',#76760,7.68301219552715);
#20311=CIRCLE('',#76762,7.69191406167057);
#20312=CIRCLE('',#76763,7.68336740565433);
#20313=CIRCLE('',#76764,7.68749364032046);
#20314=CIRCLE('',#76765,7.68301219454201);
#20315=CIRCLE('',#76767,7.69191393356503);
#20316=CIRCLE('',#76768,7.68336737355074);
#20317=CIRCLE('',#76769,7.68749361389151);
#20318=CIRCLE('',#76770,7.6830121964021);
#20319=CIRCLE('',#76772,7.6919140322792);
#20320=CIRCLE('',#76773,7.68336735652281);
#20321=CIRCLE('',#76774,7.68749364999818);
#20322=CIRCLE('',#76775,7.68301219423073);
#20323=CIRCLE('',#76777,7.6919138750408);
#20324=CIRCLE('',#76778,7.68336749358252);
#20325=CIRCLE('',#76779,7.687493682695);
#20326=CIRCLE('',#76780,7.6830121913286);
#20327=CIRCLE('',#76782,7.69191383933637);
#20328=CIRCLE('',#76783,7.68336765832302);
#20329=CIRCLE('',#76784,7.68749379841072);
#20330=CIRCLE('',#76786,7.6919137026217);
#20331=CIRCLE('',#76787,7.68336744990483);
#20332=CIRCLE('',#76788,7.68301219395284);
#20333=CIRCLE('',#76816,7.44132107797583);
#20334=CIRCLE('',#76817,7.44901098494131);
#20335=CIRCLE('',#76818,7.44132132093448);
#20336=CIRCLE('',#76819,7.44901094168559);
#20337=CIRCLE('',#76820,7.44132115326169);
#20338=CIRCLE('',#76821,7.44901111040069);
#20339=CIRCLE('',#76822,7.4413210530835);
#20340=CIRCLE('',#76823,7.44901114767026);
#20341=CIRCLE('',#76824,7.44132116557519);
#20342=CIRCLE('',#76825,7.44901111062852);
#20343=CIRCLE('',#76826,7.4413213143581);
#20344=CIRCLE('',#76827,7.44901110784486);
#20345=CIRCLE('',#76828,7.44132104242765);
#20346=CIRCLE('',#76829,7.44901091837715);
#20347=CIRCLE('',#76830,7.44132133289912);
#20348=CIRCLE('',#76831,7.44901104574036);
#20349=CIRCLE('',#76832,7.44132094853763);
#20350=CIRCLE('',#76833,7.44901097608923);
#20351=CIRCLE('',#76834,7.44132120601532);
#20352=CIRCLE('',#76835,7.44901109082872);
#20353=CIRCLE('',#76836,7.44132132070303);
#20354=CIRCLE('',#76837,7.44901109826273);
#20355=CIRCLE('',#76838,7.44132109292228);
#20356=CIRCLE('',#76839,7.44901083584621);
#20357=CIRCLE('',#76840,7.44132096463299);
#20358=CIRCLE('',#76841,7.44901099402833);
#20359=CIRCLE('',#76842,7.4413212047583);
#20360=CIRCLE('',#76843,7.44901102648147);
#20361=CIRCLE('',#76844,7.44132111690801);
#20362=CIRCLE('',#76845,7.44901114277106);
#20363=CIRCLE('',#76846,7.44132113658756);
#20364=CIRCLE('',#76847,7.44901083347679);
#20365=CIRCLE('',#76848,7.44132112331147);
#20366=CIRCLE('',#76849,7.44901110309528);
#20367=CIRCLE('',#76850,7.44132135859989);
#20368=CIRCLE('',#76851,7.44901091613842);
#20369=CIRCLE('',#76852,7.44132110226029);
#20370=CIRCLE('',#76853,7.44901122973458);
#20371=CIRCLE('',#76854,7.44132128324485);
#20372=CIRCLE('',#76855,7.44901100863801);
#20373=CIRCLE('',#76856,7.44132123695719);
#20374=CIRCLE('',#76857,7.44901095358546);
#20375=CIRCLE('',#76858,7.44132094601733);
#20376=CIRCLE('',#76859,7.44901086743548);
#20377=CIRCLE('',#76860,7.44132104374503);
#20378=CIRCLE('',#76861,7.44901084522942);
#20379=CIRCLE('',#76862,7.44132119244628);
#20380=CIRCLE('',#76863,7.4490109837086);
#20381=CIRCLE('',#76864,7.44132088248784);
#20382=CIRCLE('',#76865,7.44901084782327);
#20383=CIRCLE('',#76866,7.44132115396878);
#20384=CIRCLE('',#76867,7.4490108424845);
#20385=CIRCLE('',#76868,7.44132110146778);
#20386=CIRCLE('',#76869,7.44901080710049);
#20387=CIRCLE('',#76870,7.4413209549527);
#20388=CIRCLE('',#76871,7.4490110306471);
#20389=CIRCLE('',#76872,7.44132119434995);
#20390=CIRCLE('',#76873,7.4490110973393);
#20391=CIRCLE('',#76874,7.44096163290917);
#20392=CIRCLE('',#76875,7.44244523922687);
#20393=CIRCLE('',#76876,7.44096407826071);
#20394=CIRCLE('',#76877,7.44244536654789);
#20395=CIRCLE('',#76878,7.44096431502101);
#20396=CIRCLE('',#76879,7.44244539029637);
#20397=CIRCLE('',#76880,7.44096110369019);
#20398=CIRCLE('',#76881,7.44244518327569);
#20399=CIRCLE('',#76882,7.44096431779229);
#20400=CIRCLE('',#76883,7.44244519836295);
#20401=CIRCLE('',#76884,7.44096158135734);
#20402=CIRCLE('',#76885,7.44244549869616);
#20403=CIRCLE('',#76886,7.44096453896483);
#20404=CIRCLE('',#76887,7.44244541427963);
#20405=CIRCLE('',#76888,7.44096231054569);
#20406=CIRCLE('',#76889,7.44244541753372);
#20407=CIRCLE('',#76890,7.44096437264636);
#20408=CIRCLE('',#76891,7.4424453223831);
#20409=CIRCLE('',#76892,7.44096446338278);
#20410=CIRCLE('',#76893,7.44244557095827);
#20411=CIRCLE('',#76894,7.44096277132953);
#20412=CIRCLE('',#76895,7.44244557551138);
#20413=CIRCLE('',#76896,7.44096431516055);
#20414=CIRCLE('',#76897,7.44244547318913);
#20415=CIRCLE('',#76898,7.44096446933956);
#20416=CIRCLE('',#76899,7.44244540321972);
#20417=CIRCLE('',#76900,7.44096428290229);
#20418=CIRCLE('',#76901,7.44244515431675);
#20419=CIRCLE('',#76902,7.44096420555444);
#20420=CIRCLE('',#76903,7.44244556754339);
#20421=CIRCLE('',#76904,7.44096234565355);
#20422=CIRCLE('',#76905,7.44244540483046);
#20423=CIRCLE('',#76906,7.44096082293892);
#20424=CIRCLE('',#76907,7.44244512639587);
#20425=CIRCLE('',#76908,7.44096039470945);
#20426=CIRCLE('',#76909,7.4424450755022);
#20427=CIRCLE('',#76910,7.44096406266067);
#20428=CIRCLE('',#76911,7.44244522712707);
#20429=CIRCLE('',#76912,7.44096433481613);
#20430=CIRCLE('',#76913,7.4424452051413);
#20431=CIRCLE('',#76914,7.44096156994441);
#20432=CIRCLE('',#76915,7.44244537053809);
#20433=CIRCLE('',#76916,7.44095843279229);
#20434=CIRCLE('',#76917,7.44244517593898);
#20435=CIRCLE('',#76918,7.44096426134897);
#20436=CIRCLE('',#76919,7.44244529727346);
#20437=CIRCLE('',#76920,7.44096403234586);
#20438=CIRCLE('',#76921,7.44244532704227);
#20439=CIRCLE('',#76922,7.44096419576632);
#20440=CIRCLE('',#76923,7.44244508418218);
#20441=CIRCLE('',#76924,7.44096433950973);
#20442=CIRCLE('',#76925,7.44244551802685);
#20443=CIRCLE('',#76926,7.44096450056671);
#20444=CIRCLE('',#76927,7.44244556495398);
#20445=CIRCLE('',#76928,7.44096417004577);
#20446=CIRCLE('',#76929,7.44244524080392);
#20447=CIRCLE('',#76930,7.44096030726756);
#20448=CIRCLE('',#76931,7.44243697652006);
#20449=CIRCLE('',#76932,7.6865219858248);
#20450=CIRCLE('',#76934,7.69259356655966);
#20451=CIRCLE('',#76935,7.69146685349983);
#20452=CIRCLE('',#76936,7.69282882739483);
#20453=CIRCLE('',#76937,7.68652199057024);
#20454=CIRCLE('',#76939,7.69259369657614);
#20455=CIRCLE('',#76940,7.69146683430398);
#20456=CIRCLE('',#76941,7.69282880669103);
#20457=CIRCLE('',#76942,7.68652179559924);
#20458=CIRCLE('',#76944,7.69259340746021);
#20459=CIRCLE('',#76945,7.691466770726);
#20460=CIRCLE('',#76946,7.69282855100629);
#20461=CIRCLE('',#76947,7.68652198594906);
#20462=CIRCLE('',#76949,7.69259360268407);
#20463=CIRCLE('',#76950,7.69146694460064);
#20464=CIRCLE('',#76951,7.69282855102511);
#20465=CIRCLE('',#76952,7.6865218785945);
#20466=CIRCLE('',#76954,7.69259403322546);
#20467=CIRCLE('',#76955,7.691466746238);
#20468=CIRCLE('',#76956,7.69282867576847);
#20469=CIRCLE('',#76957,7.68652189966966);
#20470=CIRCLE('',#76959,7.69259351263286);
#20471=CIRCLE('',#76960,7.69146698897258);
#20472=CIRCLE('',#76961,7.69282864997746);
#20473=CIRCLE('',#76962,7.68652192033685);
#20474=CIRCLE('',#76964,7.69259382860018);
#20475=CIRCLE('',#76965,7.69146698613297);
#20476=CIRCLE('',#76966,7.6928286936219);
#20477=CIRCLE('',#76967,7.68652172845389);
#20478=CIRCLE('',#76969,7.69259364164714);
#20479=CIRCLE('',#76970,7.69146693267229);
#20480=CIRCLE('',#76971,7.69282862604479);
#20481=CIRCLE('',#76972,7.68652199760421);
#20482=CIRCLE('',#76974,7.69259380387986);
#20483=CIRCLE('',#76975,7.69146687436047);
#20484=CIRCLE('',#76976,7.69282864390347);
#20485=CIRCLE('',#76977,7.68652169413379);
#20486=CIRCLE('',#76979,7.69259352494882);
#20487=CIRCLE('',#76980,7.69146679101874);
#20488=CIRCLE('',#76981,7.6928287469085);
#20489=CIRCLE('',#76982,7.68652187802919);
#20490=CIRCLE('',#76984,7.69259356016282);
#20491=CIRCLE('',#76985,7.691467148089);
#20492=CIRCLE('',#76986,7.69282870572607);
#20493=CIRCLE('',#76987,7.68652201488452);
#20494=CIRCLE('',#76989,7.69259359852887);
#20495=CIRCLE('',#76990,7.69146696424068);
#20496=CIRCLE('',#76991,7.69282881299637);
#20497=CIRCLE('',#76992,7.68652184436031);
#20498=CIRCLE('',#76994,7.69259370349727);
#20499=CIRCLE('',#76995,7.69146696882247);
#20500=CIRCLE('',#76996,7.692828605017);
#20501=CIRCLE('',#76997,7.68652173871916);
#20502=CIRCLE('',#76999,7.69259390260136);
#20503=CIRCLE('',#77000,7.6914669348861);
#20504=CIRCLE('',#77001,7.69282861236544);
#20505=CIRCLE('',#77002,7.68652186283024);
#20506=CIRCLE('',#77004,7.69259385249028);
#20507=CIRCLE('',#77005,7.69146694463207);
#20508=CIRCLE('',#77006,7.69282860917482);
#20509=CIRCLE('',#77007,7.68652185817288);
#20510=CIRCLE('',#77009,7.69259377730403);
#20511=CIRCLE('',#77010,7.69146685597649);
#20512=CIRCLE('',#77011,7.69282867861488);
#20513=CIRCLE('',#77012,7.68652147082297);
#20514=CIRCLE('',#77013,7.69282887165906);
#20515=CIRCLE('',#77015,7.69259354930379);
#20516=CIRCLE('',#77016,7.69146699781378);
#20517=CIRCLE('',#77017,7.68652198036796);
#20518=CIRCLE('',#77019,7.6928284639639);
#20519=CIRCLE('',#77020,7.69259389688855);
#20520=CIRCLE('',#77021,7.69146673727659);
#20521=CIRCLE('',#77022,7.68652174668928);
#20522=CIRCLE('',#77024,7.69259364248133);
#20523=CIRCLE('',#77025,7.6914670556374);
#20524=CIRCLE('',#77026,7.69282887904053);
#20525=CIRCLE('',#77027,7.68652190379035);
#20526=CIRCLE('',#77029,7.69259345492421);
#20527=CIRCLE('',#77030,7.69146699481387);
#20528=CIRCLE('',#77031,7.69282881879384);
#20529=CIRCLE('',#77032,7.68652186672836);
#20530=CIRCLE('',#77034,7.69259377821932);
#20531=CIRCLE('',#77035,7.6914669565814);
#20532=CIRCLE('',#77036,7.69282865899933);
#20533=CIRCLE('',#77037,7.68652191668875);
#20534=CIRCLE('',#77039,7.69259378690776);
#20535=CIRCLE('',#77040,7.69146675768012);
#20536=CIRCLE('',#77041,7.69282872733812);
#20537=CIRCLE('',#77042,7.68652157256796);
#20538=CIRCLE('',#77044,7.69259367709038);
#20539=CIRCLE('',#77045,7.69146690611445);
#20540=CIRCLE('',#77046,7.69282864252631);
#20541=CIRCLE('',#77047,7.68652190628653);
#20542=CIRCLE('',#77049,7.69259398711421);
#20543=CIRCLE('',#77050,7.69146686903634);
#20544=CIRCLE('',#77051,7.69282859515984);
#20545=CIRCLE('',#77052,7.68652173300724);
#20546=CIRCLE('',#77054,7.69259365254763);
#20547=CIRCLE('',#77055,7.69146684927592);
#20548=CIRCLE('',#77056,7.69282842455778);
#20549=CIRCLE('',#77057,7.68652209975129);
#20550=CIRCLE('',#77059,7.69259365638295);
#20551=CIRCLE('',#77060,7.69146681076176);
#20552=CIRCLE('',#77061,7.69282857884792);
#20553=CIRCLE('',#77062,7.6865218269609);
#20554=CIRCLE('',#77064,7.69259363649161);
#20555=CIRCLE('',#77065,7.69146674289333);
#20556=CIRCLE('',#77066,7.69282882374801);
#20557=CIRCLE('',#77067,7.6865220526541);
#20558=CIRCLE('',#77069,7.69259366273547);
#20559=CIRCLE('',#77070,7.69146687686865);
#20560=CIRCLE('',#77071,7.69282889340358);
#20561=CIRCLE('',#77072,7.44708419294032);
#20562=CIRCLE('',#77073,7.44708561793515);
#20563=CIRCLE('',#77074,7.44708600142821);
#20564=CIRCLE('',#77075,7.44708641170203);
#20565=CIRCLE('',#77076,7.44708560826829);
#20566=CIRCLE('',#77077,7.44708515266404);
#20567=CIRCLE('',#77078,7.44708543844587);
#20568=CIRCLE('',#77079,7.44708521174704);
#20569=CIRCLE('',#77080,7.44708527016981);
#20570=CIRCLE('',#77081,7.44708459620124);
#20571=CIRCLE('',#77082,7.44708505445453);
#20572=CIRCLE('',#77083,7.44708454602176);
#20573=CIRCLE('',#77084,7.44708534479393);
#20574=CIRCLE('',#77085,7.44708562750459);
#20575=CIRCLE('',#77086,7.44708578392729);
#20576=CIRCLE('',#77087,7.44708545070702);
#20577=CIRCLE('',#77088,7.44708472173902);
#20578=CIRCLE('',#77089,7.44708366242392);
#20579=CIRCLE('',#77090,7.44708569711275);
#20580=CIRCLE('',#77091,7.4470842021165);
#20581=CIRCLE('',#77092,7.44708438198736);
#20582=CIRCLE('',#77093,7.44708479532805);
#20583=CIRCLE('',#77094,7.44708591037287);
#20584=CIRCLE('',#77095,7.44708525478703);
#20585=CIRCLE('',#77096,7.44708597637106);
#20586=CIRCLE('',#77097,7.44708599827779);
#20587=CIRCLE('',#77098,7.44708594245394);
#20588=CIRCLE('',#77099,7.44708653118089);
#20589=CIRCLE('',#77100,7.44708486685733);
#20590=CIRCLE('',#77101,7.44865545447364);
#20591=CIRCLE('',#77102,7.44865939903026);
#20592=CIRCLE('',#77103,7.44865951919544);
#20593=CIRCLE('',#77104,7.44865945619483);
#20594=CIRCLE('',#77105,7.44865934537791);
#20595=CIRCLE('',#77106,7.44865932466116);
#20596=CIRCLE('',#77107,7.44865920703867);
#20597=CIRCLE('',#77108,7.44865931020773);
#20598=CIRCLE('',#77109,7.44865905615679);
#20599=CIRCLE('',#77110,7.4486592598318);
#20600=CIRCLE('',#77111,7.44865928637504);
#20601=CIRCLE('',#77112,7.44865925240711);
#20602=CIRCLE('',#77113,7.44865896325401);
#20603=CIRCLE('',#77114,7.44865928152926);
#20604=CIRCLE('',#77115,7.44865939449395);
#20605=CIRCLE('',#77116,7.44865941621312);
#20606=CIRCLE('',#77117,7.44865941330856);
#20607=CIRCLE('',#77118,7.44865944336093);
#20608=CIRCLE('',#77119,7.44865922828271);
#20609=CIRCLE('',#77120,7.44865933672944);
#20610=CIRCLE('',#77121,7.44865941706835);
#20611=CIRCLE('',#77122,7.44865925172642);
#20612=CIRCLE('',#77123,7.44865915460453);
#20613=CIRCLE('',#77124,7.44865917328653);
#20614=CIRCLE('',#77125,7.4486590458652);
#20615=CIRCLE('',#77126,7.44865920197224);
#20616=CIRCLE('',#77127,7.4486590853991);
#20617=CIRCLE('',#77128,7.44865931187507);
#20618=CIRCLE('',#77129,7.44865912418389);
#20619=CIRCLE('',#77130,7.44865926283462);
#20620=CIRCLE('',#77131,7.44865959840247);
#20621=CIRCLE('',#77132,7.44865947209281);
#20622=CIRCLE('',#77133,7.448659285211);
#20623=CIRCLE('',#77134,7.44865965464314);
#20624=CIRCLE('',#77135,7.4486594992884);
#20625=CIRCLE('',#77136,7.44865925212478);
#20626=CIRCLE('',#77137,7.44865927353072);
#20627=CIRCLE('',#77138,7.44865934135186);
#20628=CIRCLE('',#77139,7.44865899006064);
#20629=CIRCLE('',#77140,7.4486591813801);
#20630=CIRCLE('',#77141,7.44865933458729);
#20631=CIRCLE('',#77142,7.44865925740424);
#20632=CIRCLE('',#77143,7.44865899043323);
#20633=CIRCLE('',#77144,7.4486591987037);
#20634=CIRCLE('',#77145,7.44865918721473);
#20635=CIRCLE('',#77146,7.44865928117158);
#20636=CIRCLE('',#77147,7.44865931234976);
#20637=CIRCLE('',#77148,7.44865922650077);
#20638=CIRCLE('',#77149,7.44865928675125);
#20639=CIRCLE('',#77150,7.44865955530131);
#20640=CIRCLE('',#77151,7.44865926751029);
#20641=CIRCLE('',#77152,7.4486593624084);
#20642=CIRCLE('',#77153,7.44865929684653);
#20643=CIRCLE('',#77154,7.44865936809075);
#20644=CIRCLE('',#77155,7.44865917887384);
#20645=CIRCLE('',#77156,7.44865943280146);
#20646=CIRCLE('',#77157,7.44865921044527);
#20647=CIRCLE('',#77158,7.44865545099262);
#20648=CIRCLE('',#77159,7.69146687677613);
#20649=CIRCLE('',#77160,7.69259385246013);
#20650=CIRCLE('',#77162,7.59069874782905);
#20651=CIRCLE('',#77163,7.5);
#20652=CIRCLE('',#77164,7.82252136132111);
#20653=CIRCLE('',#77165,7.69146690843554);
#20654=CIRCLE('',#77167,7.6930292059074);
#20655=CIRCLE('',#77168,7.68762402195699);
#20656=CIRCLE('',#77169,7.69259377727589);
#20657=CIRCLE('',#77171,7.59069211449223);
#20658=CIRCLE('',#77172,7.50000000166363);
#20659=CIRCLE('',#77173,7.82251325481052);
#20660=CIRCLE('',#77174,7.69146675991688);
#20661=CIRCLE('',#77176,7.69303011297896);
#20662=CIRCLE('',#77177,7.68762407921375);
#20663=CIRCLE('',#77178,7.69259354927485);
#20664=CIRCLE('',#77180,7.59069769736449);
#20665=CIRCLE('',#77181,7.5);
#20666=CIRCLE('',#77182,7.82251999913105);
#20667=CIRCLE('',#77183,7.69146691035308);
#20668=CIRCLE('',#77185,7.69302947585912);
#20669=CIRCLE('',#77186,7.68762361462464);
#20670=CIRCLE('',#77187,7.69259389685879);
#20671=CIRCLE('',#77189,7.59069939624143);
#20672=CIRCLE('',#77190,7.5);
#20673=CIRCLE('',#77191,7.82251960680243);
#20674=CIRCLE('',#77192,7.69146668179339);
#20675=CIRCLE('',#77194,7.69302912297621);
#20676=CIRCLE('',#77195,7.68762414399008);
#20677=CIRCLE('',#77196,7.69259364245232);
#20678=CIRCLE('',#77198,7.59069600435376);
#20679=CIRCLE('',#77199,7.49999999874647);
#20680=CIRCLE('',#77200,7.82252200020871);
#20681=CIRCLE('',#77201,7.69146698767325);
#20682=CIRCLE('',#77203,7.69302909653028);
#20683=CIRCLE('',#77204,7.68762361645412);
#20684=CIRCLE('',#77205,7.69259345652704);
#20685=CIRCLE('',#77207,7.59069728841729);
#20686=CIRCLE('',#77208,7.5);
#20687=CIRCLE('',#77209,7.82251866109699);
#20688=CIRCLE('',#77210,7.69146697030562);
#20689=CIRCLE('',#77212,7.69302954298555);
#20690=CIRCLE('',#77213,7.68762412063256);
#20691=CIRCLE('',#77215,7.59069979460845);
#20692=CIRCLE('',#77216,7.82251748897697);
#20693=CIRCLE('',#77217,7.69259378687915);
#20694=CIRCLE('',#77219,7.5906965376454);
#20695=CIRCLE('',#77220,7.5);
#20696=CIRCLE('',#77221,7.82252007915959);
#20697=CIRCLE('',#77222,7.69146669971079);
#20698=CIRCLE('',#77224,7.69302935579719);
#20699=CIRCLE('',#77225,7.68762414150259);
#20700=CIRCLE('',#77226,7.69259367706596);
#20701=CIRCLE('',#77228,7.59069776346958);
#20702=CIRCLE('',#77229,7.5);
#20703=CIRCLE('',#77230,7.82251960093144);
#20704=CIRCLE('',#77231,7.69146682697528);
#20705=CIRCLE('',#77233,7.69302926405833);
#20706=CIRCLE('',#77234,7.68762375277491);
#20707=CIRCLE('',#77235,7.69259398708472);
#20708=CIRCLE('',#77237,7.59069794350898);
#20709=CIRCLE('',#77238,7.5);
#20710=CIRCLE('',#77239,7.82251987647052);
#20711=CIRCLE('',#77240,7.69146679719617);
#20712=CIRCLE('',#77242,7.69302918497997);
#20713=CIRCLE('',#77243,7.68762412023477);
#20714=CIRCLE('',#77244,7.69259365251753);
#20715=CIRCLE('',#77246,7.59069258889142);
#20716=CIRCLE('',#77247,7.50000000205533);
#20717=CIRCLE('',#77248,7.82251175100706);
#20718=CIRCLE('',#77249,7.69146677708364);
#20719=CIRCLE('',#77251,7.6930299715105);
#20720=CIRCLE('',#77252,7.68762395064371);
#20721=CIRCLE('',#77253,7.69259365635744);
#20722=CIRCLE('',#77255,7.59069822792092);
#20723=CIRCLE('',#77256,7.5);
#20724=CIRCLE('',#77257,7.82251954047492);
#20725=CIRCLE('',#77258,7.69146673573611);
#20726=CIRCLE('',#77260,7.69302919174222);
#20727=CIRCLE('',#77261,7.68762427055975);
#20728=CIRCLE('',#77262,7.69259363646344);
#20729=CIRCLE('',#77264,7.59069647196464);
#20730=CIRCLE('',#77265,7.5);
#20731=CIRCLE('',#77266,7.82252147084837);
#20732=CIRCLE('',#77267,7.69146669772047);
#20733=CIRCLE('',#77269,7.69302957755455);
#20734=CIRCLE('',#77270,7.68762378726061);
#20735=CIRCLE('',#77271,7.6925936627046);
#20736=CIRCLE('',#77273,7.59069961187685);
#20737=CIRCLE('',#77274,7.5);
#20738=CIRCLE('',#77275,7.82251898575182);
#20739=CIRCLE('',#77276,7.69146684104373);
#20740=CIRCLE('',#77278,7.69302968603334);
#20741=CIRCLE('',#77279,7.68762426893667);
#20742=CIRCLE('',#77280,7.69259352803836);
#20743=CIRCLE('',#77282,7.59067639984585);
#20744=CIRCLE('',#77283,7.49999999294556);
#20745=CIRCLE('',#77284,7.82252591612768);
#20746=CIRCLE('',#77285,7.69146684492744);
#20747=CIRCLE('',#77287,7.69302416594306);
#20748=CIRCLE('',#77288,7.68762143965011);
#20749=CIRCLE('',#77289,7.69259369654752);
#20750=CIRCLE('',#77291,7.59067895629939);
#20751=CIRCLE('',#77292,7.50000000515093);
#20752=CIRCLE('',#77293,7.82249887507338);
#20753=CIRCLE('',#77294,7.69146673782841);
#20754=CIRCLE('',#77296,7.69303172916898);
#20755=CIRCLE('',#77297,7.68762421120419);
#20756=CIRCLE('',#77298,7.69259340743115);
#20757=CIRCLE('',#77300,7.59069883361731);
#20758=CIRCLE('',#77301,7.5);
#20759=CIRCLE('',#77302,7.82251900978043);
#20760=CIRCLE('',#77303,7.69146672944481);
#20761=CIRCLE('',#77305,7.69302925783024);
#20762=CIRCLE('',#77306,7.68762403548546);
#20763=CIRCLE('',#77307,7.69259360265325);
#20764=CIRCLE('',#77309,7.59069234582906);
#20765=CIRCLE('',#77310,7.50000000204315);
#20766=CIRCLE('',#77311,7.82251190864904);
#20767=CIRCLE('',#77312,7.69146687267438);
#20768=CIRCLE('',#77314,7.6930300327545);
#20769=CIRCLE('',#77315,7.68762420011832);
#20770=CIRCLE('',#77316,7.69259403319664);
#20771=CIRCLE('',#77318,7.59069832506839);
#20772=CIRCLE('',#77319,7.5);
#20773=CIRCLE('',#77320,7.82252133604163);
#20774=CIRCLE('',#77321,7.69146668069641);
#20775=CIRCLE('',#77323,7.69302933000856);
#20776=CIRCLE('',#77324,7.68762385993089);
#20777=CIRCLE('',#77325,7.69259351260242);
#20778=CIRCLE('',#77327,7.59069953203992);
#20779=CIRCLE('',#77328,7.49999999916126);
#20780=CIRCLE('',#77329,7.82252167476504);
#20781=CIRCLE('',#77330,7.69146689993987);
#20782=CIRCLE('',#77332,7.69302894205857);
#20783=CIRCLE('',#77333,7.68762386124297);
#20784=CIRCLE('',#77334,7.69259382856953);
#20785=CIRCLE('',#77336,7.59069658460535);
#20786=CIRCLE('',#77337,7.5);
#20787=CIRCLE('',#77338,7.82251979523547);
#20788=CIRCLE('',#77339,7.69146690128489);
#20789=CIRCLE('',#77341,7.69302933458611);
#20790=CIRCLE('',#77342,7.68762413533275);
#20791=CIRCLE('',#77343,7.69259364161605);
#20792=CIRCLE('',#77345,7.59067929887621);
#20793=CIRCLE('',#77346,7.49999999332733);
#20794=CIRCLE('',#77347,7.82252591988282);
#20795=CIRCLE('',#77348,7.69146689318844);
#20796=CIRCLE('',#77350,7.69302410711918);
#20797=CIRCLE('',#77351,7.68762099378799);
#20798=CIRCLE('',#77352,7.69259380384968);
#20799=CIRCLE('',#77354,7.59069962299981);
#20800=CIRCLE('',#77355,7.49999999937961);
#20801=CIRCLE('',#77356,7.82252173215583);
#20802=CIRCLE('',#77357,7.69146681270038);
#20803=CIRCLE('',#77359,7.69302893927606);
#20804=CIRCLE('',#77360,7.68762367868796);
#20805=CIRCLE('',#77361,7.69259352492098);
#20806=CIRCLE('',#77363,7.59069572709328);
#20807=CIRCLE('',#77364,7.5);
#20808=CIRCLE('',#77365,7.82252094087956);
#20809=CIRCLE('',#77366,7.69146671041594);
#20810=CIRCLE('',#77368,7.69302952805748);
#20811=CIRCLE('',#77369,7.68762376227097);
#20812=CIRCLE('',#77370,7.69259356013278);
#20813=CIRCLE('',#77372,7.59069385159072);
#20814=CIRCLE('',#77373,7.50000000212692);
#20815=CIRCLE('',#77374,7.8225116641969);
#20816=CIRCLE('',#77375,7.69146704737195);
#20817=CIRCLE('',#77377,7.6930302213243);
#20818=CIRCLE('',#77378,7.68762409347789);
#20819=CIRCLE('',#77379,7.69259359850366);
#20820=CIRCLE('',#77381,7.59068937344032);
#20821=CIRCLE('',#77382,7.49999999790811);
#20822=CIRCLE('',#77383,7.82252249489037);
#20823=CIRCLE('',#77384,7.69146692025778);
#20824=CIRCLE('',#77386,7.69302791572941);
#20825=CIRCLE('',#77387,7.68762336613701);
#20826=CIRCLE('',#77388,7.69259369059137);
#20827=CIRCLE('',#77390,7.59068004933096);
#20828=CIRCLE('',#77391,7.50000000528208);
#20829=CIRCLE('',#77392,7.82249852360222);
#20830=CIRCLE('',#77393,7.69146694937379);
#20831=CIRCLE('',#77395,7.69303144785881);
#20832=CIRCLE('',#77396,7.68762406157333);
#20833=CIRCLE('',#77397,7.6925939025748);
#20834=CIRCLE('',#77399,7.59069691634231);
#20835=CIRCLE('',#77400,7.5);
#20836=CIRCLE('',#77401,7.82252063468176);
#20837=CIRCLE('',#77402,7.69146688362149);
#20838=CIRCLE('',#77404,7.69302929330036);
#20839=CIRCLE('',#77405,7.68762381313008);
#20840=CIRCLE('',#77407,7.59070352038018);
#20841=CIRCLE('',#77408,7.5);
#20842=CIRCLE('',#77409,7.82251782820925);
#20843=CIRCLE('',#77411,7.69302934908707);
#20844=CIRCLE('',#77412,7.69259384669478);
#20845=CIRCLE('',#77413,7.68762391142974);
#20846=CIRCLE('',#77416,7.44901494297204);
#20847=CIRCLE('',#77417,7.44132506654215);
#20848=CIRCLE('',#77419,7.44901476114322);
#20849=CIRCLE('',#77420,7.44132490818521);
#20850=CIRCLE('',#77422,7.44901509298134);
#20851=CIRCLE('',#77423,7.44132503659772);
#20852=CIRCLE('',#77425,7.44901469632941);
#20853=CIRCLE('',#77426,7.44132470988597);
#20854=CIRCLE('',#77428,7.44901504095824);
#20855=CIRCLE('',#77429,7.44132501451318);
#20856=CIRCLE('',#77431,7.44901483010211);
#20857=CIRCLE('',#77432,7.44132514658019);
#20858=CIRCLE('',#77434,7.44901479188647);
#20859=CIRCLE('',#77435,7.44132476474595);
#20860=CIRCLE('',#77437,7.44901472892966);
#20861=CIRCLE('',#77438,7.44132502466893);
#20862=CIRCLE('',#77440,7.44901468919714);
#20863=CIRCLE('',#77441,7.44132504613859);
#20864=CIRCLE('',#77443,7.44901486108914);
#20865=CIRCLE('',#77444,7.44132476292834);
#20866=CIRCLE('',#77446,7.44901483491887);
#20867=CIRCLE('',#77447,7.44132507072986);
#20868=CIRCLE('',#77449,7.44901472271123);
#20869=CIRCLE('',#77450,7.4413248964315);
#20870=CIRCLE('',#77452,7.44901471799794);
#20871=CIRCLE('',#77453,7.44132508046603);
#20872=CIRCLE('',#77455,7.44901479385614);
#20873=CIRCLE('',#77456,7.44132492111921);
#20874=CIRCLE('',#77458,7.44901488147878);
#20875=CIRCLE('',#77459,7.44132470821559);
#20876=CIRCLE('',#77461,7.44901498855247);
#20877=CIRCLE('',#77462,7.44132499121307);
#20878=CIRCLE('',#77464,7.44901483127117);
#20879=CIRCLE('',#77465,7.44132504797884);
#20880=CIRCLE('',#77467,7.44901489864582);
#20881=CIRCLE('',#77468,7.44132493649476);
#20882=CIRCLE('',#77470,7.44901486221692);
#20883=CIRCLE('',#77471,7.44132496814157);
#20884=CIRCLE('',#77473,7.44901483539481);
#20885=CIRCLE('',#77474,7.44132500908834);
#20886=CIRCLE('',#77476,7.44901490637958);
#20887=CIRCLE('',#77477,7.44132492102672);
#20888=CIRCLE('',#77479,7.44901473158954);
#20889=CIRCLE('',#77480,7.44132485247813);
#20890=CIRCLE('',#77482,7.4490147691237);
#20891=CIRCLE('',#77483,7.4413249053069);
#20892=CIRCLE('',#77485,7.44901503522182);
#20893=CIRCLE('',#77486,7.44132521103752);
#20894=CIRCLE('',#77488,7.44901507867795);
#20895=CIRCLE('',#77489,7.44132496020567);
#20896=CIRCLE('',#77491,7.44901485555681);
#20897=CIRCLE('',#77492,7.44132488477906);
#20898=CIRCLE('',#77494,7.44901484283174);
#20899=CIRCLE('',#77495,7.44132489754185);
#20900=CIRCLE('',#77497,7.44901477941788);
#20901=CIRCLE('',#77498,7.44132522014264);
#20902=CIRCLE('',#77500,7.44901488052498);
#20903=CIRCLE('',#77501,7.44132492046871);
#20904=CIRCLE('',#77529,7.44096471604082);
#20905=CIRCLE('',#77531,7.44244280479572);
#20906=CIRCLE('',#77532,7.44096416773314);
#20907=CIRCLE('',#77533,7.44244635429767);
#20908=CIRCLE('',#77534,7.44096478167989);
#20909=CIRCLE('',#77536,7.44244637802895);
#20910=CIRCLE('',#77537,7.44096485769064);
#20911=CIRCLE('',#77539,7.44244602496989);
#20912=CIRCLE('',#77540,7.44096452100884);
#20913=CIRCLE('',#77542,7.44244619382863);
#20914=CIRCLE('',#77543,7.44096449640376);
#20915=CIRCLE('',#77545,7.44244617677346);
#20916=CIRCLE('',#77546,7.44096457251793);
#20917=CIRCLE('',#77548,7.44244606805147);
#20918=CIRCLE('',#77549,7.44096415252455);
#20919=CIRCLE('',#77550,7.4424462802272);
#20920=CIRCLE('',#77551,7.4409643905002);
#20921=CIRCLE('',#77553,7.44244297309812);
#20922=CIRCLE('',#77554,7.440964522414);
#20923=CIRCLE('',#77556,7.44244281349285);
#20924=CIRCLE('',#77557,7.44096444919983);
#20925=CIRCLE('',#77559,7.44244591738352);
#20926=CIRCLE('',#77560,7.44096472203706);
#20927=CIRCLE('',#77562,7.44244303675119);
#20928=CIRCLE('',#77563,7.44096433176278);
#20929=CIRCLE('',#77564,7.44244641043208);
#20930=CIRCLE('',#77565,7.44096493845626);
#20931=CIRCLE('',#77567,7.44244635687994);
#20932=CIRCLE('',#77568,7.44096466855212);
#20933=CIRCLE('',#77570,7.44244606261698);
#20934=CIRCLE('',#77571,7.44096415428745);
#20935=CIRCLE('',#77572,7.44244639328344);
#20936=CIRCLE('',#77573,7.44096469441773);
#20937=CIRCLE('',#77575,7.44244630739266);
#20938=CIRCLE('',#77576,7.44096419562405);
#20939=CIRCLE('',#77577,7.44244624249257);
#20940=CIRCLE('',#77578,7.4409645724652);
#20941=CIRCLE('',#77580,7.44244637955912);
#20942=CIRCLE('',#77581,7.440964794856);
#20943=CIRCLE('',#77583,7.44244316277483);
#20944=CIRCLE('',#77584,7.44096432388314);
#20945=CIRCLE('',#77585,7.44244637094867);
#20946=CIRCLE('',#77586,7.44096418647052);
#20947=CIRCLE('',#77587,7.44244622685979);
#20948=CIRCLE('',#77588,7.44096487306209);
#20949=CIRCLE('',#77590,7.44244622980629);
#20950=CIRCLE('',#77591,7.44096479527389);
#20951=CIRCLE('',#77593,7.4424460518505);
#20952=CIRCLE('',#77594,7.44096474402759);
#20953=CIRCLE('',#77596,7.44244294054158);
#20954=CIRCLE('',#77597,7.4409647417251);
#20955=CIRCLE('',#77599,7.44244620220576);
#20956=CIRCLE('',#77600,7.4409646578587);
#20957=CIRCLE('',#77602,7.44244618615641);
#20958=CIRCLE('',#77603,7.44096450421653);
#20959=CIRCLE('',#77605,7.44244303871399);
#20960=CIRCLE('',#77606,7.44096475675713);
#20961=CIRCLE('',#77608,7.44244301437565);
#20962=CIRCLE('',#77610,7.4470849954363);
#20963=CIRCLE('',#77611,7.44708566575379);
#20964=CIRCLE('',#77612,7.4470854060469);
#20965=CIRCLE('',#77613,7.4470852658502);
#20966=CIRCLE('',#77614,7.44708613132106);
#20967=CIRCLE('',#77615,7.44708473838514);
#20968=CIRCLE('',#77616,7.44708613257339);
#20969=CIRCLE('',#77617,7.44708536736408);
#20970=CIRCLE('',#77618,7.44708498295746);
#20971=CIRCLE('',#77619,7.44708484853103);
#20972=CIRCLE('',#77620,7.44708634291999);
#20973=CIRCLE('',#77621,7.44708473348576);
#20974=CIRCLE('',#77622,7.4470839111118);
#20975=CIRCLE('',#77623,7.44708556794052);
#20976=CIRCLE('',#77624,7.44708535112535);
#20977=CIRCLE('',#77625,7.44708660484889);
#20978=CIRCLE('',#77626,7.44708634387299);
#20979=CIRCLE('',#77627,7.44708553329505);
#20980=CIRCLE('',#77628,7.44708613245776);
#20981=CIRCLE('',#77629,7.4470848224883);
#20982=CIRCLE('',#77630,7.44708488318781);
#20983=CIRCLE('',#77631,7.44708557450435);
#20984=CIRCLE('',#77632,7.44708512104896);
#20985=CIRCLE('',#77633,7.44708624028346);
#20986=CIRCLE('',#77634,7.44708479120748);
#20987=CIRCLE('',#77635,7.44708627845845);
#20988=CIRCLE('',#77636,7.44708548323966);
#20989=CIRCLE('',#77637,7.44708601562468);
#20990=CIRCLE('',#77638,7.44708424622066);
#20991=CIRCLE('',#77643,7.);
#20992=CIRCLE('',#77644,7.);
#20993=CIRCLE('',#77646,4.5);
#20994=CIRCLE('',#77647,4.5);
#20995=CIRCLE('',#77648,4.5);
#20996=CIRCLE('',#77649,4.5);
#20997=CIRCLE('',#77650,4.5);
#20998=CIRCLE('',#77651,4.5);
#20999=CIRCLE('',#77653,6.5);
#21000=CIRCLE('',#77654,6.5);
#21001=CIRCLE('',#77655,6.5);
#21002=CIRCLE('',#77657,5.99999999999999);
#21003=CIRCLE('',#77659,5.9);
#21004=CIRCLE('',#77661,5.39999999999997);
#21005=CIRCLE('',#77662,5.9);
#21006=CIRCLE('',#77664,5.9);
#21007=CIRCLE('',#77668,5.99999999999999);
#21008=CIRCLE('',#77671,5.4);
#21009=CIRCLE('',#77678,6.);
#21010=CIRCLE('',#77680,6.);
#21011=CIRCLE('',#77683,2.5);
#21012=CIRCLE('',#77684,2.5);
#21013=CIRCLE('',#77685,2.5);
#21014=CIRCLE('',#77687,2.50000000008162);
#21015=CIRCLE('',#77688,2.79999999966249);
#21016=CIRCLE('',#77690,2.5);
#21017=CIRCLE('',#77693,2.79999999971483);
#21018=CIRCLE('',#77695,6.00000000044796);
#21019=CIRCLE('',#77696,6.00000000044796);
#21020=CIRCLE('',#77697,6.00000000044794);
#21021=CIRCLE('',#77698,6.00000000044795);
#21022=CIRCLE('',#77701,35.000000093214);
#21023=CIRCLE('',#77703,4.50000000012307);
#21024=CIRCLE('',#77713,2.5);
#21025=CIRCLE('',#77714,2.5);
#21026=CIRCLE('',#77716,3.9999999997442);
#21027=CIRCLE('',#77717,2.80668844013728);
#21028=CIRCLE('',#77718,3.9999999997442);
#21029=CIRCLE('',#77719,3.9999999997442);
#21030=CIRCLE('',#77720,2.80668844013726);
#21031=CIRCLE('',#77721,1.64999996202742);
#21032=CIRCLE('',#77723,4.);
#21033=CIRCLE('',#77724,4.);
#21034=CIRCLE('',#77725,4.);
#21035=CIRCLE('',#77726,4.);
#21036=CIRCLE('',#77728,1.65);
#21037=CIRCLE('',#77729,2.025);
#21038=CIRCLE('',#77731,3.826794919);
#21039=CIRCLE('',#77741,2.5);
#21040=CIRCLE('',#77742,2.5);
#21041=CIRCLE('',#77743,2.5);
#21042=CIRCLE('',#77745,2.);
#21043=CIRCLE('',#77747,2.);
#21044=CIRCLE('',#77753,1.65);
#21045=CIRCLE('',#77754,1.65);
#21046=B_SPLINE_CURVE_WITH_KNOTS('',3,(#92442,#92443,#92444,#92445,#92446,
#92447),.UNSPECIFIED.,.F.,.F.,(4,2,4),(-0.0592625039988469,-0.0381784708554363,
-1.00000000442108E-6),.UNSPECIFIED.);
#21047=B_SPLINE_CURVE_WITH_KNOTS('',3,(#92449,#92450,#92451,#92452,#92453,
#92454,#92455,#92456,#92457,#92458),.UNSPECIFIED.,.F.,.F.,(4,2,2,2,4),(9.99985499371358E-7,
0.00990798547874647,0.0199209917052848,0.0400020007437245,0.0800923349447478),
 .UNSPECIFIED.);
#21048=B_SPLINE_CURVE_WITH_KNOTS('',3,(#92464,#92465,#92466,#92467,#92468,
#92469),.UNSPECIFIED.,.F.,.F.,(4,2,4),(0.,0.016366392747835,0.032834133837728),
 .UNSPECIFIED.);
#21049=B_SPLINE_CURVE_WITH_KNOTS('',3,(#92471,#92472,#92473,#92474,#92475,
#92476,#92477,#92478,#92479,#92480),.UNSPECIFIED.,.F.,.F.,(4,3,3,4),(3.12055520624018E-12,
7.37661517073135E-5,0.000147532580837493,0.00027986750847265),
 .UNSPECIFIED.);
#21050=B_SPLINE_CURVE_WITH_KNOTS('',3,(#92482,#92483,#92484,#92485,#92486,
#92487),.UNSPECIFIED.,.F.,.F.,(4,2,4),(1.000000003925E-6,0.0379299703047647,
0.0758579941174657),.UNSPECIFIED.);
#21051=B_SPLINE_CURVE_WITH_KNOTS('',3,(#92489,#92490,#92491,#92492,#92493,
#92494,#92495,#92496,#92497,#92498),.UNSPECIFIED.,.F.,.F.,(4,2,2,2,4),(1.00013078331987E-6,
0.00990710921000036,0.0199202404646063,0.0400015002295186,0.0800923350090046),
 .UNSPECIFIED.);
#21052=B_SPLINE_CURVE_WITH_KNOTS('',3,(#92504,#92505,#92506,#92507,#92508,
#92509),.UNSPECIFIED.,.F.,.F.,(4,2,4),(0.,0.016366874952083,0.0328340574266459),
 .UNSPECIFIED.);
#21053=B_SPLINE_CURVE_WITH_KNOTS('',3,(#92511,#92512,#92513,#92514,#92515,
#92516,#92517,#92518,#92519,#92520),.UNSPECIFIED.,.F.,.F.,(4,3,3,4),(2.15830403525905E-12,
7.37661523423699E-5,0.000147532582109008,0.000279867507510834),
 .UNSPECIFIED.);
#21054=B_SPLINE_CURVE_WITH_KNOTS('',3,(#92522,#92523,#92524,#92525,#92526,
#92527),.UNSPECIFIED.,.F.,.F.,(4,2,4),(1.00000000432393E-6,0.0379299702663971,
0.0758579940911893),.UNSPECIFIED.);
#21055=B_SPLINE_CURVE_WITH_KNOTS('',3,(#92529,#92530,#92531,#92532,#92533,
#92534,#92535,#92536,#92537,#92538),.UNSPECIFIED.,.F.,.F.,(4,2,2,2,4),(1.00017476251821E-6,
0.0099071092209813,0.0199202404680647,0.0400015001924167,0.0800923349270695),
 .UNSPECIFIED.);
#21056=B_SPLINE_CURVE_WITH_KNOTS('',3,(#92544,#92545,#92546,#92547,#92548,
#92549),.UNSPECIFIED.,.F.,.F.,(4,2,4),(0.,0.0163668763525077,0.0328340636938574),
 .UNSPECIFIED.);
#21057=B_SPLINE_CURVE_WITH_KNOTS('',3,(#92551,#92552,#92553,#92554,#92555,
#92556,#92557,#92558,#92559,#92560),.UNSPECIFIED.,.F.,.F.,(4,3,3,4),(2.52904142129497E-12,
7.37661520584279E-5,0.000147532581535914,0.00027986750749572),
 .UNSPECIFIED.);
#21058=B_SPLINE_CURVE_WITH_KNOTS('',3,(#92562,#92563,#92564,#92565,#92566,
#92567),.UNSPECIFIED.,.F.,.F.,(4,2,4),(1.00000000433087E-6,0.0379299703178269,
0.0758579941192071),.UNSPECIFIED.);
#21059=B_SPLINE_CURVE_WITH_KNOTS('',3,(#92569,#92570,#92571,#92572,#92573,
#92574,#92575,#92576,#92577,#92578),.UNSPECIFIED.,.F.,.F.,(4,2,2,2,4),(1.00014526185026E-6,
0.00990710922096496,0.0199202404714764,0.0400015002087619,0.0800923349616018),
 .UNSPECIFIED.);
#21060=B_SPLINE_CURVE_WITH_KNOTS('',3,(#92584,#92585,#92586,#92587,#92588,
#92589),.UNSPECIFIED.,.F.,.F.,(4,2,4),(0.,0.0163668761217582,0.0328340625366268),
 .UNSPECIFIED.);
#21061=B_SPLINE_CURVE_WITH_KNOTS('',3,(#92591,#92592,#92593,#92594,#92595,
#92596,#92597,#92598,#92599,#92600),.UNSPECIFIED.,.F.,.F.,(4,3,3,4),(2.88097431277638E-12,
7.37661520465302E-5,0.000147532581515671,0.000279867510177933),
 .UNSPECIFIED.);
#21062=B_SPLINE_CURVE_WITH_KNOTS('',3,(#92602,#92603,#92604,#92605,#92606,
#92607),.UNSPECIFIED.,.F.,.F.,(4,2,4),(1.00000000441414E-6,0.0379299703846838,
0.0758579942063754),.UNSPECIFIED.);
#21063=B_SPLINE_CURVE_WITH_KNOTS('',3,(#92609,#92610,#92611,#92612,#92613,
#92614,#92615,#92616,#92617,#92618),.UNSPECIFIED.,.F.,.F.,(4,2,2,2,4),(1.00010992915299E-6,
0.0099071091906864,0.019920240414248,0.040001500107306,0.080092334757455),
 .UNSPECIFIED.);
#21064=B_SPLINE_CURVE_WITH_KNOTS('',3,(#92624,#92625,#92626,#92627,#92628,
#92629),.UNSPECIFIED.,.F.,.F.,(4,2,4),(0.,0.0163668780737397,0.0328340708943008),
 .UNSPECIFIED.);
#21065=B_SPLINE_CURVE_WITH_KNOTS('',3,(#92631,#92632,#92633,#92634,#92635,
#92636,#92637,#92638,#92639,#92640),.UNSPECIFIED.,.F.,.F.,(4,3,3,4),(2.17438718025666E-12,
7.37661519451421E-5,0.000147532581312125,0.000279867506786178),
 .UNSPECIFIED.);
#21066=B_SPLINE_CURVE_WITH_KNOTS('',3,(#92642,#92643,#92644,#92645,#92646,
#92647),.UNSPECIFIED.,.F.,.F.,(4,2,4),(1.00000000362519E-6,0.0379299702686182,
0.07585799407784),.UNSPECIFIED.);
#21067=B_SPLINE_CURVE_WITH_KNOTS('',3,(#92649,#92650,#92651,#92652,#92653,
#92654,#92655,#92656,#92657,#92658),.UNSPECIFIED.,.F.,.F.,(4,2,2,2,4),(1.00008837944867E-6,
0.00990710923003866,0.0199202405024881,0.0400015002946333,0.080092335142938),
 .UNSPECIFIED.);
#21068=B_SPLINE_CURVE_WITH_KNOTS('',3,(#92664,#92665,#92666,#92667,#92668,
#92669),.UNSPECIFIED.,.F.,.F.,(4,2,4),(0.,0.0163663928143568,0.0328341344900907),
 .UNSPECIFIED.);
#21069=B_SPLINE_CURVE_WITH_KNOTS('',3,(#92671,#92672,#92673,#92674,#92675,
#92676,#92677,#92678,#92679,#92680),.UNSPECIFIED.,.F.,.F.,(4,3,3,4),(2.64934922214782E-12,
7.37661518159472E-5,0.000147532581049749,0.000279867507628596),
 .UNSPECIFIED.);
#21070=B_SPLINE_CURVE_WITH_KNOTS('',3,(#92682,#92683,#92684,#92685,#92686,
#92687),.UNSPECIFIED.,.F.,.F.,(4,2,4),(1.00000000451822E-6,0.0379299702450166,
0.0758579940565196),.UNSPECIFIED.);
#21071=B_SPLINE_CURVE_WITH_KNOTS('',3,(#92689,#92690,#92691,#92692,#92693,
#92694,#92695,#92696,#92697,#92698),.UNSPECIFIED.,.F.,.F.,(4,2,2,2,4),(1.00014647044652E-6,
0.00990710920230482,0.0199202404453444,0.0400015001848174,0.0800923349138297),
 .UNSPECIFIED.);
#21072=B_SPLINE_CURVE_WITH_KNOTS('',3,(#92704,#92705,#92706,#92707,#92708,
#92709),.UNSPECIFIED.,.F.,.F.,(4,2,4),(0.,0.0163663706141495,0.0328340656287997),
 .UNSPECIFIED.);
#21073=B_SPLINE_CURVE_WITH_KNOTS('',3,(#92711,#92712,#92713,#92714,#92715,
#92716,#92717,#92718,#92719,#92720),.UNSPECIFIED.,.F.,.F.,(4,3,3,4),(2.78736780820764E-12,
7.3766151409991E-5,0.00014753258024197,0.000279867509359074),
 .UNSPECIFIED.);
#21074=B_SPLINE_CURVE_WITH_KNOTS('',3,(#92722,#92723,#92724,#92725,#92726,
#92727),.UNSPECIFIED.,.F.,.F.,(4,2,4),(1.00000000405091E-6,0.0379299703316601,
0.0758579941712396),.UNSPECIFIED.);
#21075=B_SPLINE_CURVE_WITH_KNOTS('',3,(#92729,#92730,#92731,#92732,#92733,
#92734,#92735,#92736,#92737,#92738),.UNSPECIFIED.,.F.,.F.,(4,2,2,2,4),(1.0001287590813E-6,
0.00990710922500387,0.0199202404932373,0.040001500277097,0.0800923351051997),
 .UNSPECIFIED.);
#21076=B_SPLINE_CURVE_WITH_KNOTS('',3,(#92744,#92745,#92746,#92747,#92748,
#92749),.UNSPECIFIED.,.F.,.F.,(4,2,4),(0.,0.0163663733575533,0.0328340772555867),
 .UNSPECIFIED.);
#21077=B_SPLINE_CURVE_WITH_KNOTS('',3,(#92751,#92752,#92753,#92754,#92755,
#92756,#92757,#92758,#92759,#92760),.UNSPECIFIED.,.F.,.F.,(4,3,3,4),(3.46919833266426E-12,
7.37661524662696E-5,0.0001475325823551,0.000279867508005713),
 .UNSPECIFIED.);
#21078=B_SPLINE_CURVE_WITH_KNOTS('',3,(#92762,#92763,#92764,#92765,#92766,
#92767),.UNSPECIFIED.,.F.,.F.,(4,2,4),(1.00000000386265E-6,0.0379299702966132,
0.07585799410702),.UNSPECIFIED.);
#21079=B_SPLINE_CURVE_WITH_KNOTS('',3,(#92769,#92770,#92771,#92772,#92773,
#92774,#92775,#92776,#92777,#92778),.UNSPECIFIED.,.F.,.F.,(4,2,2,2,4),(1.00009055644546E-6,
0.00990710921856916,0.0199202404809799,0.0400015002530257,0.0800923350565718),
 .UNSPECIFIED.);
#21080=B_SPLINE_CURVE_WITH_KNOTS('',3,(#92784,#92785,#92786,#92787,#92788,
#92789),.UNSPECIFIED.,.F.,.F.,(4,2,4),(0.,0.0163663707641851,0.0328340662430508),
 .UNSPECIFIED.);
#21081=B_SPLINE_CURVE_WITH_KNOTS('',3,(#92791,#92792,#92793,#92794,#92795,
#92796,#92797,#92798,#92799,#92800),.UNSPECIFIED.,.F.,.F.,(4,3,3,4),(2.50094752839556E-12,
7.37661519728823E-5,0.000147532581366429,0.000279867507647884),
 .UNSPECIFIED.);
#21082=B_SPLINE_CURVE_WITH_KNOTS('',3,(#92802,#92803,#92804,#92805,#92806,
#92807),.UNSPECIFIED.,.F.,.F.,(4,2,4),(1.00000000426148E-6,0.0379299702609412,
0.0758579940783564),.UNSPECIFIED.);
#21083=B_SPLINE_CURVE_WITH_KNOTS('',3,(#92809,#92810,#92811,#92812,#92813,
#92814,#92815,#92816,#92817,#92818),.UNSPECIFIED.,.F.,.F.,(4,2,2,2,4),(1.00016604854426E-6,
0.00990710920452595,0.0199202404482969,0.0400015001930305,0.0800923349310915),
 .UNSPECIFIED.);
#21084=B_SPLINE_CURVE_WITH_KNOTS('',3,(#92824,#92825,#92826,#92827,#92828,
#92829),.UNSPECIFIED.,.F.,.F.,(4,2,4),(0.,0.01636639315645,0.0328341357805788),
 .UNSPECIFIED.);
#21085=B_SPLINE_CURVE_WITH_KNOTS('',3,(#92831,#92832,#92833,#92834,#92835,
#92836,#92837,#92838,#92839,#92840),.UNSPECIFIED.,.F.,.F.,(4,3,3,4),(2.94307093505262E-12,
7.37661527913104E-5,0.000147532583003831,0.000279867507750485),
 .UNSPECIFIED.);
#21086=B_SPLINE_CURVE_WITH_KNOTS('',3,(#92842,#92843,#92844,#92845,#92846,
#92847),.UNSPECIFIED.,.F.,.F.,(4,2,4),(1.00000000359874E-6,0.0379299703013,
0.075857994144482),.UNSPECIFIED.);
#21087=B_SPLINE_CURVE_WITH_KNOTS('',3,(#92849,#92850,#92851,#92852,#92853,
#92854,#92855,#92856,#92857,#92858),.UNSPECIFIED.,.F.,.F.,(4,2,2,2,4),(1.00013394837672E-6,
0.00990710922800834,0.0199202404912242,0.0400015002501556,0.0800923350518471),
 .UNSPECIFIED.);
#21088=B_SPLINE_CURVE_WITH_KNOTS('',3,(#92864,#92865,#92866,#92867,#92868,
#92869),.UNSPECIFIED.,.F.,.F.,(4,2,4),(0.,0.0163663710780007,0.032834067324964),
 .UNSPECIFIED.);
#21089=B_SPLINE_CURVE_WITH_KNOTS('',3,(#92871,#92872,#92873,#92874,#92875,
#92876,#92877,#92878,#92879,#92880),.UNSPECIFIED.,.F.,.F.,(4,3,3,4),(3.2213193587114E-12,
7.3766151590614E-5,0.000147532580599784,0.000279867509316411),
 .UNSPECIFIED.);
#21090=B_SPLINE_CURVE_WITH_KNOTS('',3,(#92882,#92883,#92884,#92885,#92886,
#92887),.UNSPECIFIED.,.F.,.F.,(4,2,4),(1.00000000392768E-6,0.037929970348679,
0.075857994134376),.UNSPECIFIED.);
#21091=B_SPLINE_CURVE_WITH_KNOTS('',3,(#92889,#92890,#92891,#92892,#92893,
#92894,#92895,#92896,#92897,#92898),.UNSPECIFIED.,.F.,.F.,(4,2,2,2,4),(9.9997700206558E-7,
0.00990798545880012,0.0199209916821671,0.0400020007165947,0.0800923349030195),
 .UNSPECIFIED.);
#21092=B_SPLINE_CURVE_WITH_KNOTS('',3,(#92904,#92905,#92906,#92907,#92908,
#92909),.UNSPECIFIED.,.F.,.F.,(4,2,4),(0.,0.0163663718390811,0.0328340706570268),
 .UNSPECIFIED.);
#21093=B_SPLINE_CURVE_WITH_KNOTS('',3,(#92911,#92912,#92913,#92914,#92915,
#92916,#92917,#92918,#92919,#92920),.UNSPECIFIED.,.F.,.F.,(4,3,3,4),(2.5445448407392E-12,
7.37661519646406E-5,0.000147532581351944,0.000279867507127543),
 .UNSPECIFIED.);
#21094=B_SPLINE_CURVE_WITH_KNOTS('',3,(#92922,#92923,#92924,#92925,#92926,
#92927),.UNSPECIFIED.,.F.,.F.,(4,2,4),(1.0000000036189E-6,0.0379299702266974,
0.0758579940621541),.UNSPECIFIED.);
#21095=B_SPLINE_CURVE_WITH_KNOTS('',3,(#92929,#92930,#92931,#92932,#92933,
#92934,#92935,#92936,#92937,#92938),.UNSPECIFIED.,.F.,.F.,(4,2,2,2,4),(9.99988358708106E-7,
0.00990798546912516,0.0199209916873161,0.0400020007141071,0.0800923348808819),
 .UNSPECIFIED.);
#21096=B_SPLINE_CURVE_WITH_KNOTS('',3,(#92944,#92945,#92946,#92947,#92948,
#92949),.UNSPECIFIED.,.F.,.F.,(4,2,4),(0.,0.0163668779555029,0.0328340697895225),
 .UNSPECIFIED.);
#21097=B_SPLINE_CURVE_WITH_KNOTS('',3,(#92951,#92952,#92953,#92954,#92955,
#92956,#92957,#92958,#92959,#92960),.UNSPECIFIED.,.F.,.F.,(4,3,3,4),(2.81817145205986E-12,
7.37661516072452E-5,0.000147532580637628,0.000279867508117206),
 .UNSPECIFIED.);
#21098=B_SPLINE_CURVE_WITH_KNOTS('',3,(#92962,#92963,#92964,#92965,#92966,
#92967),.UNSPECIFIED.,.F.,.F.,(4,2,4),(1.00000000417821E-6,0.0379299702638397,
0.0758579940710071),.UNSPECIFIED.);
#21099=B_SPLINE_CURVE_WITH_KNOTS('',3,(#92969,#92970,#92971,#92972,#92973,
#92974,#92975,#92976,#92977,#92978),.UNSPECIFIED.,.F.,.F.,(4,2,2,2,4),(1.00014734702119E-6,
0.00990710921590618,0.0199202404703475,0.0400015002220982,0.0800923349919604),
 .UNSPECIFIED.);
#21100=B_SPLINE_CURVE_WITH_KNOTS('',3,(#92984,#92985,#92986,#92987,#92988,
#92989),.UNSPECIFIED.,.F.,.F.,(4,2,4),(0.,0.0163668780647285,0.032834070559676),
 .UNSPECIFIED.);
#21101=B_SPLINE_CURVE_WITH_KNOTS('',3,(#92991,#92992,#92993,#92994,#92995,
#92996,#92997,#92998,#92999,#93000),.UNSPECIFIED.,.F.,.F.,(4,3,3,4),(3.17358619411357E-12,
7.37661526734922E-5,0.000147532582768413,0.000279867509043945),
 .UNSPECIFIED.);
#21102=B_SPLINE_CURVE_WITH_KNOTS('',3,(#93002,#93003,#93004,#93005,#93006,
#93007),.UNSPECIFIED.,.F.,.F.,(4,2,4),(1.00000000444189E-6,0.0379299703416276,
0.0758579941445551),.UNSPECIFIED.);
#21103=B_SPLINE_CURVE_WITH_KNOTS('',3,(#93009,#93010,#93011,#93012,#93013,
#93014,#93015,#93016,#93017,#93018),.UNSPECIFIED.,.F.,.F.,(4,2,2,2,4),(1.00000822225027E-6,
0.00990092359092381,0.0199067792115138,0.0399734104969956,0.0800924093120953),
 .UNSPECIFIED.);
#21104=B_SPLINE_CURVE_WITH_KNOTS('',3,(#93024,#93025,#93026,#93027,#93028,
#93029),.UNSPECIFIED.,.F.,.F.,(4,2,4),(0.,0.0163668790308347,0.0328340750476689),
 .UNSPECIFIED.);
#21105=B_SPLINE_CURVE_WITH_KNOTS('',3,(#93031,#93032,#93033,#93034,#93035,
#93036,#93037,#93038,#93039,#93040),.UNSPECIFIED.,.F.,.F.,(4,3,3,4),(2.10757257581087E-12,
7.37661524777434E-5,0.000147532582380299,0.000279867505938687),
 .UNSPECIFIED.);
#21106=B_SPLINE_CURVE_WITH_KNOTS('',3,(#93042,#93043,#93044,#93045,#93046,
#93047),.UNSPECIFIED.,.F.,.F.,(4,2,4),(1.00000000390311E-6,0.0379299702530284,
0.0758579940725049),.UNSPECIFIED.);
#21107=B_SPLINE_CURVE_WITH_KNOTS('',3,(#93049,#93050,#93051,#93052,#93053,
#93054,#93055,#93056,#93057,#93058),.UNSPECIFIED.,.F.,.F.,(4,2,2,2,4),(9.99973126498073E-7,
0.00990798551049127,0.0199209917726281,0.0400020008332237,0.0800923351454191),
 .UNSPECIFIED.);
#21108=B_SPLINE_CURVE_WITH_KNOTS('',3,(#93064,#93065,#93066,#93067,#93068,
#93069),.UNSPECIFIED.,.F.,.F.,(4,2,4),(0.,0.0163668787190169,0.0328340732796807),
 .UNSPECIFIED.);
#21109=B_SPLINE_CURVE_WITH_KNOTS('',3,(#93071,#93072,#93073,#93074,#93075,
#93076,#93077,#93078,#93079,#93080),.UNSPECIFIED.,.F.,.F.,(4,3,3,4),(2.49687519012765E-12,
7.37661519882218E-5,0.000147532581397849,0.000279867507261817),
 .UNSPECIFIED.);
#21110=B_SPLINE_CURVE_WITH_KNOTS('',3,(#93082,#93083,#93084,#93085,#93086,
#93087),.UNSPECIFIED.,.F.,.F.,(4,2,4),(1.00000000414424E-6,0.0379299702789192,
0.0758579940530802),.UNSPECIFIED.);
#21111=B_SPLINE_CURVE_WITH_KNOTS('',3,(#93089,#93090,#93091,#93092,#93093,
#93094,#93095,#93096,#93097,#93098),.UNSPECIFIED.,.F.,.F.,(4,2,2,2,4),(1.00014742275135E-6,
0.00990710919278961,0.0199202404213151,0.0400015001384411,0.0800923348165605),
 .UNSPECIFIED.);
#21112=B_SPLINE_CURVE_WITH_KNOTS('',3,(#93104,#93105,#93106,#93107,#93108,
#93109),.UNSPECIFIED.,.F.,.F.,(4,2,4),(0.,0.0163663713767149,0.0328340684866575),
 .UNSPECIFIED.);
#21113=B_SPLINE_CURVE_WITH_KNOTS('',3,(#93111,#93112,#93113,#93114,#93115,
#93116,#93117,#93118,#93119,#93120),.UNSPECIFIED.,.F.,.F.,(4,3,3,4),(3.0256058344888E-12,
7.37661519876092E-5,0.000147532581400851,0.000279867509036399),
 .UNSPECIFIED.);
#21114=B_SPLINE_CURVE_WITH_KNOTS('',3,(#93122,#93123,#93124,#93125,#93126,
#93127),.UNSPECIFIED.,.F.,.F.,(4,2,4),(1.00000000404653E-6,0.0379299702945319,
0.0758579941263343),.UNSPECIFIED.);
#21115=B_SPLINE_CURVE_WITH_KNOTS('',3,(#93129,#93130,#93131,#93132,#93133,
#93134,#93135,#93136,#93137,#93138),.UNSPECIFIED.,.F.,.F.,(4,2,2,2,4),(9.99980262838728E-7,
0.00990798549176339,0.0199209917417096,0.040002000814808,0.0800923350984535),
 .UNSPECIFIED.);
#21116=B_SPLINE_CURVE_WITH_KNOTS('',3,(#93144,#93145,#93146,#93147,#93148,
#93149),.UNSPECIFIED.,.F.,.F.,(4,2,4),(0.,0.0163668992924121,0.0328341351884076),
 .UNSPECIFIED.);
#21117=B_SPLINE_CURVE_WITH_KNOTS('',3,(#93151,#93152,#93153,#93154,#93155,
#93156,#93157,#93158,#93159,#93160),.UNSPECIFIED.,.F.,.F.,(4,3,3,4),(3.40751591842374E-12,
7.37661512684975E-5,0.000147532579958051,0.000279867508816005),
 .UNSPECIFIED.);
#21118=B_SPLINE_CURVE_WITH_KNOTS('',3,(#93162,#93163,#93164,#93165,#93166,
#93167),.UNSPECIFIED.,.F.,.F.,(4,2,4),(1.00000000455291E-6,0.0379299703035672,
0.0758579941397041),.UNSPECIFIED.);
#21119=B_SPLINE_CURVE_WITH_KNOTS('',3,(#93169,#93170,#93171,#93172,#93173,
#93174,#93175,#93176,#93177,#93178),.UNSPECIFIED.,.F.,.F.,(4,2,2,2,4),(1.00011613515136E-6,
0.0099071092388292,0.0199202405152284,0.0400015002954983,0.0800923351443803),
 .UNSPECIFIED.);
#21120=B_SPLINE_CURVE_WITH_KNOTS('',3,(#93184,#93185,#93186,#93187,#93188,
#93189),.UNSPECIFIED.,.F.,.F.,(4,2,4),(0.,0.0163669013159866,0.0328341564473171),
 .UNSPECIFIED.);
#21121=B_SPLINE_CURVE_WITH_KNOTS('',3,(#93191,#93192,#93193,#93194,#93195,
#93196,#93197,#93198,#93199,#93200),.UNSPECIFIED.,.F.,.F.,(4,3,3,4),(2.38430817117071E-12,
7.37661520320999E-5,0.000147532581486473,0.000279867506432603),
 .UNSPECIFIED.);
#21122=B_SPLINE_CURVE_WITH_KNOTS('',3,(#93202,#93203,#93204,#93205,#93206,
#93207),.UNSPECIFIED.,.F.,.F.,(4,2,4),(1.00000000416434E-6,0.0379299702998902,
0.0758579941108125),.UNSPECIFIED.);
#21123=B_SPLINE_CURVE_WITH_KNOTS('',3,(#93209,#93210,#93211,#93212,#93213,
#93214,#93215,#93216,#93217,#93218),.UNSPECIFIED.,.F.,.F.,(4,2,2,2,4),(1.0001326989014E-6,
0.00990710921300061,0.0199202404553874,0.0400015001785639,0.0800923349002753),
 .UNSPECIFIED.);
#21124=B_SPLINE_CURVE_WITH_KNOTS('',3,(#93224,#93225,#93226,#93227,#93228,
#93229),.UNSPECIFIED.,.F.,.F.,(4,2,4),(0.,0.0163663722316209,0.0328340721658131),
 .UNSPECIFIED.);
#21125=B_SPLINE_CURVE_WITH_KNOTS('',3,(#93231,#93232,#93233,#93234,#93235,
#93236,#93237,#93238,#93239,#93240),.UNSPECIFIED.,.F.,.F.,(4,3,3,4),(2.73095436148419E-12,
7.37661519688125E-5,0.000147532581358385,0.000279867507995266),
 .UNSPECIFIED.);
#21126=B_SPLINE_CURVE_WITH_KNOTS('',3,(#93242,#93243,#93244,#93245,#93246,
#93247),.UNSPECIFIED.,.F.,.F.,(4,2,4),(1.00000000457373E-6,0.0379299703677344,
0.0758579942099292),.UNSPECIFIED.);
#21127=B_SPLINE_CURVE_WITH_KNOTS('',3,(#93249,#93250,#93251,#93252,#93253,
#93254,#93255,#93256,#93257,#93258),.UNSPECIFIED.,.F.,.F.,(4,2,2,2,4),(1.00012017720786E-6,
0.00990710919520347,0.0199202404356974,0.0400015001784051,0.0800923349040917),
 .UNSPECIFIED.);
#21128=B_SPLINE_CURVE_WITH_KNOTS('',3,(#93264,#93265,#93266,#93267,#93268,
#93269),.UNSPECIFIED.,.F.,.F.,(4,2,4),(3.83630396277799E-12,0.0163668745938823,
0.0328340565233965),.UNSPECIFIED.);
#21129=B_SPLINE_CURVE_WITH_KNOTS('',3,(#93271,#93272,#93273,#93274,#93275,
#93276,#93277,#93278,#93279,#93280),.UNSPECIFIED.,.F.,.F.,(4,3,3,4),(3.25946590633978E-12,
7.37661521820108E-5,0.000147532581786437,0.00027986750976964),
 .UNSPECIFIED.);
#21130=B_SPLINE_CURVE_WITH_KNOTS('',3,(#93282,#93283,#93284,#93285,#93286,
#93287),.UNSPECIFIED.,.F.,.F.,(4,2,4),(1.00000000415046E-6,0.0379299703148109,
0.0758579941369265),.UNSPECIFIED.);
#21131=B_SPLINE_CURVE_WITH_KNOTS('',3,(#93289,#93290,#93291,#93292,#93293,
#93294,#93295,#93296,#93297,#93298),.UNSPECIFIED.,.F.,.F.,(4,2,2,2,4),(1.00012063412176E-6,
0.00990710919855529,0.0199202404331729,0.0400015001406257,0.0800923348263209),
 .UNSPECIFIED.);
#21132=B_SPLINE_CURVE_WITH_KNOTS('',3,(#93304,#93305,#93306,#93307,#93308,
#93309),.UNSPECIFIED.,.F.,.F.,(4,2,4),(0.,0.0163668752628176,0.0328340592043943),
 .UNSPECIFIED.);
#21133=B_SPLINE_CURVE_WITH_KNOTS('',3,(#93311,#93312,#93313,#93314,#93315,
#93316,#93317,#93318,#93319,#93320),.UNSPECIFIED.,.F.,.F.,(4,3,3,4),(2.29487801882904E-12,
7.37661521139689E-5,0.000147532581650881,0.000279867507355526),
 .UNSPECIFIED.);
#21134=B_SPLINE_CURVE_WITH_KNOTS('',3,(#93322,#93323,#93324,#93325,#93326,
#93327),.UNSPECIFIED.,.F.,.F.,(4,2,4),(1.00000000393238E-6,0.0379299702930691,
0.075857994094199),.UNSPECIFIED.);
#21135=B_SPLINE_CURVE_WITH_KNOTS('',3,(#93329,#93330,#93331,#93332,#93333,
#93334,#93335,#93336,#93337,#93338),.UNSPECIFIED.,.F.,.F.,(4,2,2,2,4),(9.99989189735644E-7,
0.00990798549187738,0.0199209917267273,0.0400020007675218,0.0800923349869818),
 .UNSPECIFIED.);
#21136=B_SPLINE_CURVE_WITH_KNOTS('',3,(#93344,#93345,#93346,#93347,#93348,
#93349),.UNSPECIFIED.,.F.,.F.,(4,2,4),(0.,0.0163663702233432,0.0328340634422152),
 .UNSPECIFIED.);
#21137=B_SPLINE_CURVE_WITH_KNOTS('',3,(#93351,#93352,#93353,#93354,#93355,
#93356,#93357,#93358,#93359,#93360),.UNSPECIFIED.,.F.,.F.,(4,3,3,4),(2.84831854509737E-12,
7.37661522492544E-5,0.000147532581921937,0.000279867509387217),
 .UNSPECIFIED.);
#21138=B_SPLINE_CURVE_WITH_KNOTS('',3,(#93362,#93363,#93364,#93365,#93366,
#93367),.UNSPECIFIED.,.F.,.F.,(4,2,4),(1.00000000471945E-6,0.0379299702451825,
0.0758579940332816),.UNSPECIFIED.);
#21139=B_SPLINE_CURVE_WITH_KNOTS('',3,(#93369,#93370,#93371,#93372,#93373,
#93374,#93375,#93376,#93377,#93378),.UNSPECIFIED.,.F.,.F.,(4,2,2,2,4),(9.99982675614226E-7,
0.0099079855147948,0.0199209917696819,0.0400020008257346,0.080092335117848),
 .UNSPECIFIED.);
#21140=B_SPLINE_CURVE_WITH_KNOTS('',3,(#93384,#93385,#93386,#93387,#93388,
#93389),.UNSPECIFIED.,.F.,.F.,(4,2,4),(0.,0.0163668783924265,0.032834071637775),
 .UNSPECIFIED.);
#21141=B_SPLINE_CURVE_WITH_KNOTS('',3,(#93391,#93392,#93393,#93394,#93395,
#93396,#93397,#93398,#93399,#93400),.UNSPECIFIED.,.F.,.F.,(4,3,3,4),(3.02052600740393E-12,
7.37661515665198E-5,0.000147532580553431,0.000279867508957916),
 .UNSPECIFIED.);
#21142=B_SPLINE_CURVE_WITH_KNOTS('',3,(#93402,#93403,#93404,#93405,#93406,
#93407),.UNSPECIFIED.,.F.,.F.,(4,2,4),(1.00000000469169E-6,0.0379299703573031,
0.0758579941482047),.UNSPECIFIED.);
#21143=B_SPLINE_CURVE_WITH_KNOTS('',3,(#93409,#93410,#93411,#93412,#93413,
#93414,#93415,#93416,#93417,#93418),.UNSPECIFIED.,.F.,.F.,(4,2,2,2,4),(1.00011190317721E-6,
0.00990710920835209,0.019920240458195,0.0400015002087949,0.0800923349658839),
 .UNSPECIFIED.);
#21144=B_SPLINE_CURVE_WITH_KNOTS('',3,(#93424,#93425,#93426,#93427,#93428,
#93429),.UNSPECIFIED.,.F.,.F.,(4,2,4),(0.,0.0163663732731319,0.032834076643976),
 .UNSPECIFIED.);
#21145=B_SPLINE_CURVE_WITH_KNOTS('',3,(#93431,#93432,#93433,#93434,#93435,
#93436,#93437,#93438,#93439,#93440),.UNSPECIFIED.,.F.,.F.,(4,3,3,4),(2.40629713607431E-12,
7.3766152893624E-5,0.000147532583211465,0.000279867506089791),
 .UNSPECIFIED.);
#21146=B_SPLINE_CURVE_WITH_KNOTS('',3,(#93442,#93443,#93444,#93445,#93446,
#93447),.UNSPECIFIED.,.F.,.F.,(4,2,4),(1.00000000385909E-6,0.0379299702449765,
0.0758579940418474),.UNSPECIFIED.);
#21147=B_SPLINE_CURVE_WITH_KNOTS('',3,(#93449,#93450,#93451,#93452,#93453,
#93454,#93455,#93456,#93457,#93458),.UNSPECIFIED.,.F.,.F.,(4,2,2,2,4),(1.00016638365941E-6,
0.00990710918754969,0.0199202404186389,0.0400015001540122,0.0800923348470809),
 .UNSPECIFIED.);
#21148=B_SPLINE_CURVE_WITH_KNOTS('',3,(#93464,#93465,#93466,#93467,#93468,
#93469),.UNSPECIFIED.,.F.,.F.,(4,2,4),(0.,0.0163668772734967,0.0328340674544946),
 .UNSPECIFIED.);
#21149=B_SPLINE_CURVE_WITH_KNOTS('',3,(#93471,#93472,#93473,#93474,#93475,
#93476,#93477,#93478,#93479,#93480),.UNSPECIFIED.,.F.,.F.,(4,3,3,4),(2.7020001199329E-12,
7.37661511205436E-5,0.000147532579662811,0.000279867506975402),
 .UNSPECIFIED.);
#21150=B_SPLINE_CURVE_WITH_KNOTS('',3,(#93482,#93483,#93484,#93485,#93486,
#93487),.UNSPECIFIED.,.F.,.F.,(4,2,4),(1.00000000378671E-6,0.0379299702724514,
0.0758579940657682),.UNSPECIFIED.);
#21151=B_SPLINE_CURVE_WITH_KNOTS('',3,(#93489,#93490,#93491,#93492,#93493,
#93494,#93495,#93496,#93497,#93498),.UNSPECIFIED.,.F.,.F.,(4,2,2,2,4),(1.00012567259566E-6,
0.00990710919527812,0.0199202404298848,0.0400015001616016,0.0800923348642403),
 .UNSPECIFIED.);
#21152=B_SPLINE_CURVE_WITH_KNOTS('',3,(#93504,#93505,#93506,#93507,#93508,
#93509),.UNSPECIFIED.,.F.,.F.,(4,2,4),(0.,0.0163668767440042,0.0328340647550787),
 .UNSPECIFIED.);
#21153=B_SPLINE_CURVE_WITH_KNOTS('',3,(#93511,#93512,#93513,#93514,#93515,
#93516,#93517,#93518,#93519,#93520),.UNSPECIFIED.,.F.,.F.,(4,3,3,4),(3.05699471743467E-12,
7.37661510434139E-5,0.000147532579507185,0.000279867509435222),
 .UNSPECIFIED.);
#21154=B_SPLINE_CURVE_WITH_KNOTS('',3,(#93522,#93523,#93524,#93525,#93526,
#93527),.UNSPECIFIED.,.F.,.F.,(4,2,4),(1.00000000405056E-6,0.0379299703561028,
0.075857994162927),.UNSPECIFIED.);
#21155=B_SPLINE_CURVE_WITH_KNOTS('',3,(#93529,#93530,#93531,#93532,#93533,
#93534,#93535,#93536,#93537,#93538),.UNSPECIFIED.,.F.,.F.,(4,2,2,2,4),(1.00011518016948E-6,
0.00990710920032543,0.0199202404477273,0.0400015002058067,0.0800923349587456),
 .UNSPECIFIED.);
#21156=B_SPLINE_CURVE_WITH_KNOTS('',3,(#93544,#93545,#93546,#93547,#93548,
#93549),.UNSPECIFIED.,.F.,.F.,(4,2,4),(0.,0.016366369401344,0.0328340610916559),
 .UNSPECIFIED.);
#21157=B_SPLINE_CURVE_WITH_KNOTS('',3,(#93551,#93552,#93553,#93554,#93555,
#93556,#93557,#93558,#93559,#93560),.UNSPECIFIED.,.F.,.F.,(4,3,3,4),(2.30225153103726E-12,
7.37661521669142E-5,0.000147532581753493,0.000279867507571026),
 .UNSPECIFIED.);
#21158=B_SPLINE_CURVE_WITH_KNOTS('',3,(#93562,#93563,#93564,#93565,#93566,
#93567),.UNSPECIFIED.,.F.,.F.,(4,2,4),(1.00000000436556E-6,0.0379299702578409,
0.0758579940974071),.UNSPECIFIED.);
#21159=B_SPLINE_CURVE_WITH_KNOTS('',3,(#93569,#93570,#93571,#93572,#93573,
#93574,#93575,#93576,#93577,#93578),.UNSPECIFIED.,.F.,.F.,(4,2,2,2,4),(1.00016793091942E-6,
0.0099071092151007,0.0199202404525576,0.0400015001511786,0.0800923348409666),
 .UNSPECIFIED.);
#21160=B_SPLINE_CURVE_WITH_KNOTS('',3,(#93584,#93585,#93586,#93587,#93588,
#93589),.UNSPECIFIED.,.F.,.F.,(4,2,4),(-0.0328438284890723,-0.0141443269679191,
-0.0109909790759362),.UNSPECIFIED.);
#21161=B_SPLINE_CURVE_WITH_KNOTS('',3,(#93594,#93595,#93596,#93597),
 .UNSPECIFIED.,.F.,.F.,(4,4),(-0.0109909790759362,0.),.UNSPECIFIED.);
#21162=B_SPLINE_CURVE_WITH_KNOTS('',3,(#93598,#93599,#93600,#93601,#93602,
#93603),.UNSPECIFIED.,.F.,.F.,(4,2,4),(-0.0270230498387851,-0.0216021935132955,
-0.016285344354504),.UNSPECIFIED.);
#21163=B_SPLINE_CURVE_WITH_KNOTS('',3,(#93612,#93613,#93614,#93615,#93616,
#93617),.UNSPECIFIED.,.F.,.F.,(4,2,4),(-0.016285344354504,-0.0148457764538674,
0.),.UNSPECIFIED.);
#21164=B_SPLINE_CURVE_WITH_KNOTS('',3,(#93618,#93619,#93620,#93621),
 .UNSPECIFIED.,.F.,.F.,(4,4),(-0.0758581196727035,-0.0592625039988469),
 .UNSPECIFIED.);
#21165=B_SPLINE_CURVE_WITH_KNOTS('',3,(#93643,#93644,#93645,#93646,#93647,
#93648),.UNSPECIFIED.,.F.,.F.,(4,2,4),(9.99999999955596E-7,0.0185727541481888,
0.0324222158011904),.UNSPECIFIED.);
#21166=B_SPLINE_CURVE_WITH_KNOTS('',3,(#93654,#93655,#93656,#93657,#93658,
#93659,#93660,#93661,#93662,#93663),.UNSPECIFIED.,.F.,.F.,(4,2,2,2,4),(1.00000000424299E-6,
0.0379563433916625,0.0569679482505531,0.0664477168182853,0.0758271106987986),
 .UNSPECIFIED.);
#21167=B_SPLINE_CURVE_WITH_KNOTS('',3,(#93665,#93666,#93667,#93668,#93669,
#93670),.UNSPECIFIED.,.F.,.F.,(4,2,4),(4.06438238585956E-10,0.0379279704158864,
0.0758568871894573),.UNSPECIFIED.);
#21168=B_SPLINE_CURVE_WITH_KNOTS('',3,(#93672,#93673,#93674,#93675,#93676,
#93677),.UNSPECIFIED.,.F.,.F.,(4,2,4),(4.33743085104919E-12,0.0139935348994338,
0.0280841169043245),.UNSPECIFIED.);
#21169=B_SPLINE_CURVE_WITH_KNOTS('',3,(#93679,#93680,#93681,#93682,#93683,
#93684),.UNSPECIFIED.,.F.,.F.,(4,2,4),(9.99999224806747E-7,0.0162155345072075,
0.0323312975240217),.UNSPECIFIED.);
#21170=B_SPLINE_CURVE_WITH_KNOTS('',3,(#93690,#93691,#93692,#93693,#93694,
#93695,#93696,#93697,#93698,#93699),.UNSPECIFIED.,.F.,.F.,(4,2,2,2,4),(1.00000000407308E-6,
0.0379563433696533,0.0569679482437729,0.0664477168002803,0.0758271106578579),
 .UNSPECIFIED.);
#21171=B_SPLINE_CURVE_WITH_KNOTS('',3,(#93701,#93702,#93703,#93704,#93705,
#93706),.UNSPECIFIED.,.F.,.F.,(4,2,4),(4.06757014420253E-10,0.0379279703868986,
0.0758568871285899),.UNSPECIFIED.);
#21172=B_SPLINE_CURVE_WITH_KNOTS('',3,(#93708,#93709,#93710,#93711,#93712,
#93713),.UNSPECIFIED.,.F.,.F.,(4,2,4),(6.99834882007157E-12,0.013993537777293,
0.0280841250980986),.UNSPECIFIED.);
#21173=B_SPLINE_CURVE_WITH_KNOTS('',3,(#93715,#93716,#93717,#93718,#93719,
#93720),.UNSPECIFIED.,.F.,.F.,(4,2,4),(9.99999224629494E-7,0.0162155364639106,
0.0323313007103116),.UNSPECIFIED.);
#21174=B_SPLINE_CURVE_WITH_KNOTS('',3,(#93726,#93727,#93728,#93729,#93730,
#93731,#93732,#93733,#93734,#93735),.UNSPECIFIED.,.F.,.F.,(4,2,2,2,4),(1.00000000378622E-6,
0.037956817286507,0.0569686595417362,0.0664485464642953,0.0758271106620216),
 .UNSPECIFIED.);
#21175=B_SPLINE_CURVE_WITH_KNOTS('',3,(#93737,#93738,#93739,#93740,#93741,
#93742),.UNSPECIFIED.,.F.,.F.,(4,2,4),(4.63120919050251E-10,0.0379279704591495,
0.0758568871468356),.UNSPECIFIED.);
#21176=B_SPLINE_CURVE_WITH_KNOTS('',3,(#93744,#93745,#93746,#93747,#93748,
#93749),.UNSPECIFIED.,.F.,.F.,(4,2,4),(8.63811169450238E-12,0.0139935396137458,
0.0280841305290667),.UNSPECIFIED.);
#21177=B_SPLINE_CURVE_WITH_KNOTS('',3,(#93751,#93752,#93753,#93754,#93755,
#93756),.UNSPECIFIED.,.F.,.F.,(4,2,4),(9.99999224316896E-7,0.0162160349179906,
0.0323312991030676),.UNSPECIFIED.);
#21178=B_SPLINE_CURVE_WITH_KNOTS('',3,(#93762,#93763,#93764,#93765,#93766,
#93767,#93768,#93769,#93770,#93771),.UNSPECIFIED.,.F.,.F.,(4,2,2,2,4),(1.00000000406093E-6,
0.037956343374081,0.0569679482574388,0.0664477168139411,0.0758271106626968),
 .UNSPECIFIED.);
#21179=B_SPLINE_CURVE_WITH_KNOTS('',3,(#93773,#93774,#93775,#93776,#93777,
#93778),.UNSPECIFIED.,.F.,.F.,(4,2,4),(3.92675587073167E-10,0.037927970360737,
0.0758568871110415),.UNSPECIFIED.);
#21180=B_SPLINE_CURVE_WITH_KNOTS('',3,(#93780,#93781,#93782,#93783,#93784,
#93785),.UNSPECIFIED.,.F.,.F.,(4,2,4),(1.58913783375628E-11,0.0139935478892337,
0.0280841525392221),.UNSPECIFIED.);
#21181=B_SPLINE_CURVE_WITH_KNOTS('',3,(#93787,#93788,#93789,#93790,#93791,
#93792),.UNSPECIFIED.,.F.,.F.,(4,2,4),(9.99999224520166E-7,0.0162155358781851,
0.0323312933119785),.UNSPECIFIED.);
#21182=B_SPLINE_CURVE_WITH_KNOTS('',3,(#93798,#93799,#93800,#93801,#93802,
#93803,#93804,#93805,#93806,#93807),.UNSPECIFIED.,.F.,.F.,(4,2,2,2,4),(1.00000000369756E-6,
0.0379563434110503,0.0569679482969297,0.0664477168651638,0.0758271107410538),
 .UNSPECIFIED.);
#21183=B_SPLINE_CURVE_WITH_KNOTS('',3,(#93809,#93810,#93811,#93812,#93813,
#93814),.UNSPECIFIED.,.F.,.F.,(4,2,4),(3.99842486074308E-10,0.0379279703576063,
0.0758568870804365),.UNSPECIFIED.);
#21184=B_SPLINE_CURVE_WITH_KNOTS('',3,(#93816,#93817,#93818,#93819,#93820,
#93821),.UNSPECIFIED.,.F.,.F.,(4,2,4),(1.22693307893903E-11,0.0139935437268641,
0.0280841401722759),.UNSPECIFIED.);
#21185=B_SPLINE_CURVE_WITH_KNOTS('',3,(#93823,#93824,#93825,#93826,#93827,
#93828),.UNSPECIFIED.,.F.,.F.,(4,2,4),(9.99999224684185E-7,0.0162155357538767,
0.0323312957951966),.UNSPECIFIED.);
#21186=B_SPLINE_CURVE_WITH_KNOTS('',3,(#93834,#93835,#93836,#93837,#93838,
#93839,#93840,#93841,#93842,#93843),.UNSPECIFIED.,.F.,.F.,(4,2,2,2,4),(1.00000000379667E-6,
0.0379563433696758,0.0569679482212681,0.0664477167812651,0.0758271106479268),
 .UNSPECIFIED.);
#21187=B_SPLINE_CURVE_WITH_KNOTS('',3,(#93845,#93846,#93847,#93848,#93849,
#93850),.UNSPECIFIED.,.F.,.F.,(4,2,4),(4.67025503490487E-10,0.037927970471215,
0.0758568871651145),.UNSPECIFIED.);
#21188=B_SPLINE_CURVE_WITH_KNOTS('',3,(#93852,#93853,#93854,#93855,#93856,
#93857),.UNSPECIFIED.,.F.,.F.,(4,2,4),(3.51810538021842E-12,0.0139935355162212,
0.0280841208099387),.UNSPECIFIED.);
#21189=B_SPLINE_CURVE_WITH_KNOTS('',3,(#93859,#93860,#93861,#93862,#93863,
#93864),.UNSPECIFIED.,.F.,.F.,(4,2,4),(9.999992243271E-7,0.016216036316379,
0.0323313046569059),.UNSPECIFIED.);
#21190=B_SPLINE_CURVE_WITH_KNOTS('',3,(#93870,#93871,#93872,#93873,#93874,
#93875,#93876,#93877,#93878,#93879),.UNSPECIFIED.,.F.,.F.,(4,2,2,2,4),(1.00000000425964E-6,
0.037956817259286,0.0569686594990577,0.0664485464162528,0.0758271106124966),
 .UNSPECIFIED.);
#21191=B_SPLINE_CURVE_WITH_KNOTS('',3,(#93881,#93882,#93883,#93884,#93885,
#93886),.UNSPECIFIED.,.F.,.F.,(4,2,4),(3.68350940632322E-10,0.0379279703483229,
0.0758568871354953),.UNSPECIFIED.);
#21192=B_SPLINE_CURVE_WITH_KNOTS('',3,(#93888,#93889,#93890,#93891,#93892,
#93893),.UNSPECIFIED.,.F.,.F.,(4,2,4),(2.49236911550552E-12,0.0139935338696049,
0.0280841166260514),.UNSPECIFIED.);
#21193=B_SPLINE_CURVE_WITH_KNOTS('',3,(#93895,#93896,#93897,#93898,#93899,
#93900),.UNSPECIFIED.,.F.,.F.,(4,2,4),(9.99999224696981E-7,0.0162155368944896,
0.0323313032520044),.UNSPECIFIED.);
#21194=B_SPLINE_CURVE_WITH_KNOTS('',3,(#93906,#93907,#93908,#93909,#93910,
#93911,#93912,#93913,#93914,#93915),.UNSPECIFIED.,.F.,.F.,(4,2,2,2,4),(1.00000000432823E-6,
0.0379563433944539,0.0569679482649521,0.0664477168316037,0.0758271107060209),
 .UNSPECIFIED.);
#21195=B_SPLINE_CURVE_WITH_KNOTS('',3,(#93917,#93918,#93919,#93920,#93921,
#93922),.UNSPECIFIED.,.F.,.F.,(4,2,4),(4.41129519225011E-10,0.0379279704414067,
0.0758568871645413),.UNSPECIFIED.);
#21196=B_SPLINE_CURVE_WITH_KNOTS('',3,(#93924,#93925,#93926,#93927,#93928,
#93929),.UNSPECIFIED.,.F.,.F.,(4,2,4),(0.,0.013993531306137,0.0280841099083931),
 .UNSPECIFIED.);
#21197=B_SPLINE_CURVE_WITH_KNOTS('',3,(#93931,#93932,#93933,#93934,#93935,
#93936),.UNSPECIFIED.,.F.,.F.,(4,2,4),(9.99999224281765E-7,0.0162160348181736,
0.032331303545734),.UNSPECIFIED.);
#21198=B_SPLINE_CURVE_WITH_KNOTS('',3,(#93942,#93943,#93944,#93945,#93946,
#93947,#93948,#93949,#93950,#93951),.UNSPECIFIED.,.F.,.F.,(4,2,2,2,4),(1.00000000356021E-6,
0.0379563433798304,0.0569679482573238,0.0664477168162998,0.0758271106759946),
 .UNSPECIFIED.);
#21199=B_SPLINE_CURVE_WITH_KNOTS('',3,(#93953,#93954,#93955,#93956,#93957,
#93958),.UNSPECIFIED.,.F.,.F.,(4,2,4),(4.1900957551012E-10,0.0379279704210826,
0.0758568871645112),.UNSPECIFIED.);
#21200=B_SPLINE_CURVE_WITH_KNOTS('',3,(#93960,#93961,#93962,#93963,#93964,
#93965),.UNSPECIFIED.,.F.,.F.,(4,2,4),(1.24119165113354E-11,0.0139935438438368,
0.0280841407058771),.UNSPECIFIED.);
#21201=B_SPLINE_CURVE_WITH_KNOTS('',3,(#93967,#93968,#93969,#93970,#93971,
#93972),.UNSPECIFIED.,.F.,.F.,(4,2,4),(9.99999224431024E-7,0.0162160333729869,
0.0323312937322819),.UNSPECIFIED.);
#21202=B_SPLINE_CURVE_WITH_KNOTS('',3,(#93978,#93979,#93980,#93981,#93982,
#93983,#93984,#93985,#93986,#93987),.UNSPECIFIED.,.F.,.F.,(4,2,2,2,4),(1.00000000436287E-6,
0.0379563433599197,0.056967948210949,0.0664477167676862,0.0758271106367201),
 .UNSPECIFIED.);
#21203=B_SPLINE_CURVE_WITH_KNOTS('',3,(#93989,#93990,#93991,#93992,#93993,
#93994),.UNSPECIFIED.,.F.,.F.,(4,2,4),(4.52709987453159E-10,0.0379279704650473,
0.0758568871764037),.UNSPECIFIED.);
#21204=B_SPLINE_CURVE_WITH_KNOTS('',3,(#93996,#93997,#93998,#93999,#94000,
#94001),.UNSPECIFIED.,.F.,.F.,(4,2,4),(1.71019733157448E-11,0.0139935490883922,
0.0280841550414123),.UNSPECIFIED.);
#21205=B_SPLINE_CURVE_WITH_KNOTS('',3,(#94003,#94004,#94005,#94006,#94007,
#94008),.UNSPECIFIED.,.F.,.F.,(4,2,4),(0.,0.0162146158527736,0.0323304210442275),
 .UNSPECIFIED.);
#21206=B_SPLINE_CURVE_WITH_KNOTS('',3,(#94014,#94015,#94016,#94017,#94018,
#94019,#94020,#94021,#94022,#94023),.UNSPECIFIED.,.F.,.F.,(4,2,2,2,4),(1.00000000413671E-6,
0.037956343355812,0.0569679481985058,0.0664477167564262,0.0758271106214051),
 .UNSPECIFIED.);
#21207=B_SPLINE_CURVE_WITH_KNOTS('',3,(#94025,#94026,#94027,#94028,#94029,
#94030),.UNSPECIFIED.,.F.,.F.,(4,2,4),(4.50704316609119E-10,0.0379279704742771,
0.0758568872115808),.UNSPECIFIED.);
#21208=B_SPLINE_CURVE_WITH_KNOTS('',3,(#94032,#94033,#94034,#94035,#94036,
#94037),.UNSPECIFIED.,.F.,.F.,(4,2,4),(1.1315969324254E-11,0.0139935427060249,
0.0280841376217774),.UNSPECIFIED.);
#21209=B_SPLINE_CURVE_WITH_KNOTS('',3,(#94039,#94040,#94041,#94042,#94043,
#94044),.UNSPECIFIED.,.F.,.F.,(4,2,4),(9.99999224704977E-7,0.0162160818110645,
0.0323313688967677),.UNSPECIFIED.);
#21210=B_SPLINE_CURVE_WITH_KNOTS('',3,(#94050,#94051,#94052,#94053,#94054,
#94055,#94056,#94057,#94058,#94059),.UNSPECIFIED.,.F.,.F.,(4,2,2,2,4),(1.00000000408188E-6,
0.0379568172594891,0.0569686594994689,0.06644854641549,0.07582711061623),
 .UNSPECIFIED.);
#21211=B_SPLINE_CURVE_WITH_KNOTS('',3,(#94061,#94062,#94063,#94064,#94065,
#94066),.UNSPECIFIED.,.F.,.F.,(4,2,4),(4.53942780162584E-10,0.0379279704428565,
0.0758568871390405),.UNSPECIFIED.);
#21212=B_SPLINE_CURVE_WITH_KNOTS('',3,(#94068,#94069,#94070,#94071,#94072,
#94073),.UNSPECIFIED.,.F.,.F.,(4,2,4),(9.54664759693469E-12,0.0139935407727207,
0.0280841357480742),.UNSPECIFIED.);
#21213=B_SPLINE_CURVE_WITH_KNOTS('',3,(#94075,#94076,#94077,#94078,#94079,
#94080),.UNSPECIFIED.,.F.,.F.,(4,2,4),(9.99999224540365E-7,0.0162155366783889,
0.0323312991674447),.UNSPECIFIED.);
#21214=B_SPLINE_CURVE_WITH_KNOTS('',3,(#94086,#94087,#94088,#94089,#94090,
#94091,#94092,#94093,#94094,#94095),.UNSPECIFIED.,.F.,.F.,(4,2,2,2,4),(1.00000000364162E-6,
0.0379568172549171,0.0569686594920516,0.0664485464067164,0.0758271105977281),
 .UNSPECIFIED.);
#21215=B_SPLINE_CURVE_WITH_KNOTS('',3,(#94097,#94098,#94099,#94100,#94101,
#94102),.UNSPECIFIED.,.F.,.F.,(4,2,4),(4.45560040758764E-10,0.0379279704071412,
0.0758568870806577),.UNSPECIFIED.);
#21216=B_SPLINE_CURVE_WITH_KNOTS('',3,(#94104,#94105,#94106,#94107,#94108,
#94109),.UNSPECIFIED.,.F.,.F.,(4,2,4),(1.32865392961759E-11,0.0139935448170323,
0.028084143171579),.UNSPECIFIED.);
#21217=B_SPLINE_CURVE_WITH_KNOTS('',3,(#94111,#94112,#94113,#94114,#94115,
#94116),.UNSPECIFIED.,.F.,.F.,(4,2,4),(9.99999224337034E-7,0.0162160343091742,
0.0323312950264872),.UNSPECIFIED.);
#21218=B_SPLINE_CURVE_WITH_KNOTS('',3,(#94122,#94123,#94124,#94125,#94126,
#94127,#94128,#94129,#94130,#94131),.UNSPECIFIED.,.F.,.F.,(4,2,2,2,4),(1.00000000399103E-6,
0.0379568172873199,0.0569686595159996,0.0664485464437832,0.0758271106644221),
 .UNSPECIFIED.);
#21219=B_SPLINE_CURVE_WITH_KNOTS('',3,(#94133,#94134,#94135,#94136,#94137,
#94138),.UNSPECIFIED.,.F.,.F.,(4,2,4),(4.07805439493781E-10,0.0379279703896745,
0.0758568871301433),.UNSPECIFIED.);
#21220=B_SPLINE_CURVE_WITH_KNOTS('',3,(#94140,#94141,#94142,#94143,#94144,
#94145),.UNSPECIFIED.,.F.,.F.,(4,2,4),(1.43882151926213E-11,0.0139935461168279,
0.0280841488166543),.UNSPECIFIED.);
#21221=B_SPLINE_CURVE_WITH_KNOTS('',3,(#94147,#94148,#94149,#94150,#94151,
#94152),.UNSPECIFIED.,.F.,.F.,(4,2,4),(9.99999224565596E-7,0.0162155350301745,
0.0323312922684458),.UNSPECIFIED.);
#21222=B_SPLINE_CURVE_WITH_KNOTS('',3,(#94158,#94159,#94160,#94161,#94162,
#94163,#94164,#94165,#94166,#94167),.UNSPECIFIED.,.F.,.F.,(4,2,2,2,4),(-0.0758271700234285,
-0.0664543880836614,-0.0569813146737242,-0.0379831721396834,-0.0221455761492257),
 .UNSPECIFIED.);
#21223=B_SPLINE_CURVE_WITH_KNOTS('',3,(#94172,#94173,#94174,#94175),
 .UNSPECIFIED.,.F.,.F.,(4,4),(-0.0221455761492257,-9.99999999980183E-7),
 .UNSPECIFIED.);
#21224=B_SPLINE_CURVE_WITH_KNOTS('',3,(#94177,#94178,#94179,#94180,#94181,
#94182),.UNSPECIFIED.,.F.,.F.,(4,2,4),(4.30157251214004E-10,0.0379279704161376,
0.0758568871359327),.UNSPECIFIED.);
#21225=B_SPLINE_CURVE_WITH_KNOTS('',3,(#94184,#94185,#94186,#94187,#94188,
#94189),.UNSPECIFIED.,.F.,.F.,(4,2,4),(1.12023496069153E-11,0.0139935425843184,
0.0280841373842571),.UNSPECIFIED.);
#21226=B_SPLINE_CURVE_WITH_KNOTS('',3,(#94191,#94192,#94193,#94194,#94195,
#94196),.UNSPECIFIED.,.F.,.F.,(4,2,4),(9.99999224499498E-7,0.0162160340438454,
0.0323312958745362),.UNSPECIFIED.);
#21227=B_SPLINE_CURVE_WITH_KNOTS('',3,(#94202,#94203,#94204,#94205,#94206,
#94207,#94208,#94209,#94210,#94211),.UNSPECIFIED.,.F.,.F.,(4,2,2,2,4),(1.00000000386564E-6,
0.0379563433383663,0.0569679481833149,0.0664477167348935,0.075827110588995),
 .UNSPECIFIED.);
#21228=B_SPLINE_CURVE_WITH_KNOTS('',3,(#94213,#94214,#94215,#94216,#94217,
#94218),.UNSPECIFIED.,.F.,.F.,(4,2,4),(5.00598833072905E-10,0.0379279705397505,
0.0758568872272186),.UNSPECIFIED.);
#21229=B_SPLINE_CURVE_WITH_KNOTS('',3,(#94220,#94221,#94222,#94223,#94224,
#94225),.UNSPECIFIED.,.F.,.F.,(4,2,4),(1.07902976010742E-11,0.0139935419946153,
0.0280841374988874),.UNSPECIFIED.);
#21230=B_SPLINE_CURVE_WITH_KNOTS('',3,(#94227,#94228,#94229,#94230,#94231,
#94232),.UNSPECIFIED.,.F.,.F.,(4,2,4),(9.99999224512423E-7,0.0162155368357054,
0.0323312989032803),.UNSPECIFIED.);
#21231=B_SPLINE_CURVE_WITH_KNOTS('',3,(#94238,#94239,#94240,#94241,#94242,
#94243,#94244,#94245,#94246,#94247),.UNSPECIFIED.,.F.,.F.,(4,2,2,2,4),(1.00000000413658E-6,
0.0379568172452287,0.0569686594899139,0.0664485464004263,0.075827110594861),
 .UNSPECIFIED.);
#21232=B_SPLINE_CURVE_WITH_KNOTS('',3,(#94249,#94250,#94251,#94252,#94253,
#94254),.UNSPECIFIED.,.F.,.F.,(4,2,4),(4.41601881795433E-10,0.0379279704780061,
0.0758568872380842),.UNSPECIFIED.);
#21233=B_SPLINE_CURVE_WITH_KNOTS('',3,(#94256,#94257,#94258,#94259,#94260,
#94261),.UNSPECIFIED.,.F.,.F.,(4,2,4),(1.11945846996415E-11,0.0139935425581397,
0.0280841384616102),.UNSPECIFIED.);
#21234=B_SPLINE_CURVE_WITH_KNOTS('',3,(#94263,#94264,#94265,#94266,#94267,
#94268),.UNSPECIFIED.,.F.,.F.,(4,2,4),(9.99999224334761E-7,0.0162160341154941,
0.0323312959179037),.UNSPECIFIED.);
#21235=B_SPLINE_CURVE_WITH_KNOTS('',3,(#94274,#94275,#94276,#94277,#94278,
#94279,#94280,#94281,#94282,#94283),.UNSPECIFIED.,.F.,.F.,(4,2,2,2,4),(1.00000000363513E-6,
0.0379563433668786,0.056967948246606,0.0664477168006794,0.075827110651616),
 .UNSPECIFIED.);
#21236=B_SPLINE_CURVE_WITH_KNOTS('',3,(#94285,#94286,#94287,#94288,#94289,
#94290),.UNSPECIFIED.,.F.,.F.,(4,2,4),(4.12300237846166E-10,0.0379279703799779,
0.0758568871008718),.UNSPECIFIED.);
#21237=B_SPLINE_CURVE_WITH_KNOTS('',3,(#94292,#94293,#94294,#94295,#94296,
#94297),.UNSPECIFIED.,.F.,.F.,(4,2,4),(8.75187855439104E-12,0.0139935398483156,
0.0280841287853482),.UNSPECIFIED.);
#21238=B_SPLINE_CURVE_WITH_KNOTS('',3,(#94299,#94300,#94301,#94302,#94303,
#94304),.UNSPECIFIED.,.F.,.F.,(4,2,4),(9.99999224518061E-7,0.0162155367220943,
0.0323312998042448),.UNSPECIFIED.);
#21239=B_SPLINE_CURVE_WITH_KNOTS('',3,(#94310,#94311,#94312,#94313,#94314,
#94315,#94316,#94317,#94318,#94319),.UNSPECIFIED.,.F.,.F.,(4,2,2,2,4),(1.00000000375627E-6,
0.0379568172655732,0.0569686594889428,0.0664485464097976,0.0758271106265263),
 .UNSPECIFIED.);
#21240=B_SPLINE_CURVE_WITH_KNOTS('',3,(#94321,#94322,#94323,#94324,#94325,
#94326),.UNSPECIFIED.,.F.,.F.,(4,2,4),(4.8792649542259E-10,0.0379279704959347,
0.075856887169228),.UNSPECIFIED.);
#21241=B_SPLINE_CURVE_WITH_KNOTS('',3,(#94328,#94329,#94330,#94331,#94332,
#94333),.UNSPECIFIED.,.F.,.F.,(4,2,4),(1.15848085350532E-11,0.0139935428846778,
0.0280841380768979),.UNSPECIFIED.);
#21242=B_SPLINE_CURVE_WITH_KNOTS('',3,(#94335,#94336,#94337,#94338,#94339,
#94340),.UNSPECIFIED.,.F.,.F.,(4,2,4),(9.99999224886843E-7,0.0162155815394017,
0.0323313648688343),.UNSPECIFIED.);
#21243=B_SPLINE_CURVE_WITH_KNOTS('',3,(#94346,#94347,#94348,#94349,#94350,
#94351,#94352,#94353,#94354,#94355),.UNSPECIFIED.,.F.,.F.,(4,2,2,2,4),(1.00000000377922E-6,
0.0379568172709777,0.0569686595142048,0.0664485464331935,0.0758271106440092),
 .UNSPECIFIED.);
#21244=B_SPLINE_CURVE_WITH_KNOTS('',3,(#94357,#94358,#94359,#94360,#94361,
#94362),.UNSPECIFIED.,.F.,.F.,(4,2,4),(4.02285801780176E-10,0.0379279703983211,
0.0758568871633483),.UNSPECIFIED.);
#21245=B_SPLINE_CURVE_WITH_KNOTS('',3,(#94364,#94365,#94366,#94367,#94368,
#94369),.UNSPECIFIED.,.F.,.F.,(4,2,4),(7.63640398019089E-12,0.0139935385798663,
0.0280841271630634),.UNSPECIFIED.);
#21246=B_SPLINE_CURVE_WITH_KNOTS('',3,(#94371,#94372,#94373,#94374,#94375,
#94376),.UNSPECIFIED.,.F.,.F.,(4,2,4),(9.99999224383416E-7,0.0162160350398016,
0.0323312999701239),.UNSPECIFIED.);
#21247=B_SPLINE_CURVE_WITH_KNOTS('',3,(#94382,#94383,#94384,#94385,#94386,
#94387,#94388,#94389,#94390,#94391),.UNSPECIFIED.,.F.,.F.,(4,2,2,2,4),(1.00000000414352E-6,
0.0379568172834359,0.0569686595273031,0.0664485464513015,0.075827110649782),
 .UNSPECIFIED.);
#21248=B_SPLINE_CURVE_WITH_KNOTS('',3,(#94393,#94394,#94395,#94396,#94397,
#94398),.UNSPECIFIED.,.F.,.F.,(4,2,4),(4.50592995525949E-10,0.037927970445616,
0.0758568871542498),.UNSPECIFIED.);
#21249=B_SPLINE_CURVE_WITH_KNOTS('',3,(#94400,#94401,#94402,#94403,#94404,
#94405),.UNSPECIFIED.,.F.,.F.,(4,2,4),(1.61499532360511E-11,0.0139935481505983,
0.0280841523577774),.UNSPECIFIED.);
#21250=B_SPLINE_CURVE_WITH_KNOTS('',3,(#94407,#94408,#94409,#94410,#94411,
#94412),.UNSPECIFIED.,.F.,.F.,(4,2,4),(9.99999224621297E-7,0.0162155344678765,
0.0323312900667826),.UNSPECIFIED.);
#21251=B_SPLINE_CURVE_WITH_KNOTS('',3,(#94418,#94419,#94420,#94421,#94422,
#94423,#94424,#94425,#94426,#94427),.UNSPECIFIED.,.F.,.F.,(4,2,2,2,4),(1.00000000406719E-6,
0.0379563433891528,0.0569679482616479,0.0664477168250839,0.0758271106891875),
 .UNSPECIFIED.);
#21252=B_SPLINE_CURVE_WITH_KNOTS('',3,(#94429,#94430,#94431,#94432,#94433,
#94434),.UNSPECIFIED.,.F.,.F.,(4,2,4),(4.85813906449347E-10,0.0379279704877334,
0.0758568871526431),.UNSPECIFIED.);
#21253=B_SPLINE_CURVE_WITH_KNOTS('',3,(#94436,#94437,#94438,#94439,#94440,
#94441),.UNSPECIFIED.,.F.,.F.,(4,2,4),(7.09238533573901E-12,0.0139935379133358,
0.0280841263197077),.UNSPECIFIED.);
#21254=B_SPLINE_CURVE_WITH_KNOTS('',3,(#94443,#94444,#94445,#94446,#94447,
#94448),.UNSPECIFIED.,.F.,.F.,(4,2,4),(9.99999224719861E-7,0.0162155351467326,
0.0323312974128403),.UNSPECIFIED.);
#21255=B_SPLINE_CURVE_WITH_KNOTS('',3,(#94454,#94455,#94456,#94457,#94458,
#94459,#94460,#94461,#94462,#94463),.UNSPECIFIED.,.F.,.F.,(4,2,2,2,4),(1.00000000397735E-6,
0.0379563433805459,0.0569679482540589,0.0664477168149957,0.0758271106758986),
 .UNSPECIFIED.);
#21256=B_SPLINE_CURVE_WITH_KNOTS('',3,(#94465,#94466,#94467,#94468,#94469,
#94470),.UNSPECIFIED.,.F.,.F.,(4,2,4),(4.00195118598817E-10,0.0379279703924894,
0.075856887158006),.UNSPECIFIED.);
#21257=B_SPLINE_CURVE_WITH_KNOTS('',3,(#94472,#94473,#94474,#94475,#94476,
#94477),.UNSPECIFIED.,.F.,.F.,(4,2,4),(1.06230877155031E-11,0.0139935419498799,
0.0280841336437773),.UNSPECIFIED.);
#21258=B_SPLINE_CURVE_WITH_KNOTS('',3,(#94479,#94480,#94481,#94482,#94483,
#94484),.UNSPECIFIED.,.F.,.F.,(4,2,4),(9.99999224736563E-7,0.016216079244363,
0.0323313639624725),.UNSPECIFIED.);
#21259=B_SPLINE_CURVE_WITH_KNOTS('',3,(#94490,#94491,#94492,#94493,#94494,
#94495,#94496,#94497,#94498,#94499),.UNSPECIFIED.,.F.,.F.,(4,2,2,2,4),(1.00000000417821E-6,
0.0379563433979393,0.0569679482732456,0.0664477168381609,0.0758271107099495),
 .UNSPECIFIED.);
#21260=B_SPLINE_CURVE_WITH_KNOTS('',3,(#94501,#94502,#94503,#94504,#94505,
#94506),.UNSPECIFIED.,.F.,.F.,(4,2,4),(4.0532723640096E-10,0.0379279703802278,
0.0758568871197231),.UNSPECIFIED.);
#21261=B_SPLINE_CURVE_WITH_KNOTS('',3,(#94508,#94509,#94510,#94511,#94512,
#94513),.UNSPECIFIED.,.F.,.F.,(4,2,4),(1.12206825926819E-11,0.0139935425716113,
0.028084137770905),.UNSPECIFIED.);
#21262=B_SPLINE_CURVE_WITH_KNOTS('',3,(#94515,#94516,#94517,#94518,#94519,
#94520),.UNSPECIFIED.,.F.,.F.,(4,2,4),(9.9999922448182E-7,0.0162160353978402,
0.0323312982641253),.UNSPECIFIED.);
#21263=B_SPLINE_CURVE_WITH_KNOTS('',3,(#94526,#94527,#94528,#94529,#94530,
#94531,#94532,#94533,#94534,#94535),.UNSPECIFIED.,.F.,.F.,(4,2,2,2,4),(1.00000000387064E-6,
0.0379568172584223,0.0569686594876483,0.0664485464050056,0.075827110600589),
 .UNSPECIFIED.);
#21264=B_SPLINE_CURVE_WITH_KNOTS('',3,(#94537,#94538,#94539,#94540,#94541,
#94542),.UNSPECIFIED.,.F.,.F.,(4,2,4),(4.12888251482128E-10,0.0379279704138806,
0.0758568871648448),.UNSPECIFIED.);
#21265=B_SPLINE_CURVE_WITH_KNOTS('',3,(#94544,#94545,#94546,#94547,#94548,
#94549),.UNSPECIFIED.,.F.,.F.,(4,2,4),(0.,0.0139935332973863,0.0280841151669687),
 .UNSPECIFIED.);
#21266=B_SPLINE_CURVE_WITH_KNOTS('',3,(#94551,#94552,#94553,#94554,#94555,
#94556),.UNSPECIFIED.,.F.,.F.,(4,2,4),(9.99999224551354E-7,0.0162155349792288,
0.0323312997435385),.UNSPECIFIED.);
#21267=B_SPLINE_CURVE_WITH_KNOTS('',3,(#94562,#94563,#94564,#94565,#94566,
#94567,#94568,#94569,#94570,#94571),.UNSPECIFIED.,.F.,.F.,(4,2,2,2,4),(1.00000000356798E-6,
0.0379568172412224,0.0569686594552851,0.0664485463696981,0.0758271105702251),
 .UNSPECIFIED.);
#21268=B_SPLINE_CURVE_WITH_KNOTS('',3,(#94573,#94574,#94575,#94576,#94577,
#94578),.UNSPECIFIED.,.F.,.F.,(4,2,4),(3.64868537171598E-10,0.0379279703614429,
0.0758568871712085),.UNSPECIFIED.);
#21269=B_SPLINE_CURVE_WITH_KNOTS('',3,(#94580,#94581,#94582,#94583,#94584,
#94585),.UNSPECIFIED.,.F.,.F.,(4,2,4),(6.44180871999126E-12,0.0139935372731912,
0.0280841226769515),.UNSPECIFIED.);
#21270=B_SPLINE_CURVE_WITH_KNOTS('',3,(#94587,#94588,#94589,#94590,#94591,
#94592),.UNSPECIFIED.,.F.,.F.,(4,2,4),(9.99999224526279E-7,0.0162155344780205,
0.032331296485654),.UNSPECIFIED.);
#21271=B_SPLINE_CURVE_WITH_KNOTS('',3,(#94598,#94599,#94600,#94601,#94602,
#94603,#94604,#94605,#94606,#94607),.UNSPECIFIED.,.F.,.F.,(4,2,2,2,4),(1.00000000349721E-6,
0.0379563433579657,0.0569679482030397,0.0664477167607536,0.0758271106218004),
 .UNSPECIFIED.);
#21272=B_SPLINE_CURVE_WITH_KNOTS('',3,(#94609,#94610,#94611,#94612,#94613,
#94614),.UNSPECIFIED.,.F.,.F.,(4,2,4),(4.26548368142854E-10,0.0379279704250161,
0.0758568871602098),.UNSPECIFIED.);
#21273=B_SPLINE_CURVE_WITH_KNOTS('',3,(#94616,#94617,#94618,#94619,#94620,
#94621),.UNSPECIFIED.,.F.,.F.,(4,2,4),(3.13376810563237E-12,0.0139935334468091,
0.0280841165406132),.UNSPECIFIED.);
#21274=B_SPLINE_CURVE_WITH_KNOTS('',3,(#94623,#94624,#94625,#94626,#94627,
#94628),.UNSPECIFIED.,.F.,.F.,(4,2,4),(9.99999224127026E-7,0.0162160349129812,
0.0323313031017378),.UNSPECIFIED.);
#21275=B_SPLINE_CURVE_WITH_KNOTS('',3,(#94634,#94635,#94636,#94637,#94638,
#94639,#94640,#94641,#94642,#94643),.UNSPECIFIED.,.F.,.F.,(4,2,2,2,4),(1.00000000397699E-6,
0.0379563433877628,0.0569679482648382,0.0664477168267006,0.0758271106864307),
 .UNSPECIFIED.);
#21276=B_SPLINE_CURVE_WITH_KNOTS('',3,(#94645,#94646,#94647,#94648,#94649,
#94650),.UNSPECIFIED.,.F.,.F.,(4,2,4),(4.51041142554055E-10,0.0379279704343085,
0.0758568871257714),.UNSPECIFIED.);
#21277=B_SPLINE_CURVE_WITH_KNOTS('',3,(#94652,#94653,#94654,#94655,#94656,
#94657),.UNSPECIFIED.,.F.,.F.,(4,2,4),(1.03812220056963E-11,0.0139935416117796,
0.0280841359913486),.UNSPECIFIED.);
#21278=B_SPLINE_CURVE_WITH_KNOTS('',3,(#94659,#94660,#94661,#94662,#94663,
#94664),.UNSPECIFIED.,.F.,.F.,(4,2,4),(9.99999224857224E-7,0.0162155810644067,
0.0323313650204243),.UNSPECIFIED.);
#21279=B_SPLINE_CURVE_WITH_KNOTS('',3,(#94670,#94671,#94672,#94673,#94674,
#94675,#94676,#94677,#94678,#94679),.UNSPECIFIED.,.F.,.F.,(4,2,2,2,4),(1.0000000038219E-6,
0.0379568172482033,0.0569686594889151,0.0664485463999001,0.0758271105862111),
 .UNSPECIFIED.);
#21280=B_SPLINE_CURVE_WITH_KNOTS('',3,(#94681,#94682,#94683,#94684,#94685,
#94686),.UNSPECIFIED.,.F.,.F.,(4,2,4),(-0.0758570191918898,-0.0376794341351815,
0.),.UNSPECIFIED.);
#21281=B_SPLINE_CURVE_WITH_KNOTS('',3,(#94687,#94688,#94689,#94690,#94691,
#94692),.UNSPECIFIED.,.F.,.F.,(4,2,4),(-0.0282156346918979,-0.0107712544614244,
0.),.UNSPECIFIED.);
#21282=B_SPLINE_CURVE_WITH_KNOTS('',3,(#94700,#94701,#94702,#94703,#94704,
#94705),.UNSPECIFIED.,.F.,.F.,(4,2,4),(0.,0.0318022370756533,0.0638030678347898),
 .UNSPECIFIED.);
#21283=B_SPLINE_CURVE_WITH_KNOTS('',3,(#94706,#94707,#94708,#94709,#94710,
#94711,#94712,#94713),.UNSPECIFIED.,.F.,.F.,(4,2,2,4),(1.00002351979535E-6,
0.0322596484045106,0.048328981783262,0.0657704479132027),.UNSPECIFIED.);
#21284=B_SPLINE_CURVE_WITH_KNOTS('',3,(#94717,#94718,#94719,#94720,#94721,
#94722,#94723,#94724),.UNSPECIFIED.,.F.,.F.,(4,2,2,4),(-0.0546200763337987,
-0.0278707187231514,-0.0145797848975232,-9.99992618986541E-7),
 .UNSPECIFIED.);
#21285=B_SPLINE_CURVE_WITH_KNOTS('',3,(#94728,#94729,#94730,#94731,#94732,
#94733),.UNSPECIFIED.,.F.,.F.,(4,2,4),(0.,0.0318022364823239,0.0638030654864799),
 .UNSPECIFIED.);
#21286=B_SPLINE_CURVE_WITH_KNOTS('',3,(#94734,#94735,#94736,#94737,#94738,
#94739,#94740,#94741),.UNSPECIFIED.,.F.,.F.,(4,2,2,4),(1.00001841571144E-6,
0.032259648553329,0.0483293807870212,0.065770447844771),.UNSPECIFIED.);
#21287=B_SPLINE_CURVE_WITH_KNOTS('',3,(#94745,#94746,#94747,#94748,#94749,
#94750,#94751,#94752,#94753,#94754,#94755,#94756),.UNSPECIFIED.,.F.,.F.,
(4,2,2,2,2,4),(-0.0574506082503417,-0.0538408015157791,-0.0502541378176846,
-0.0430780609089014,-0.0287160413013061,-1.00000000285982E-6),
 .UNSPECIFIED.);
#21288=B_SPLINE_CURVE_WITH_KNOTS('',3,(#94767,#94768,#94769,#94770,#94771,
#94772),.UNSPECIFIED.,.F.,.F.,(4,2,4),(-0.0576729188689788,-0.0288412634208716,
-1.67970789167565E-9),.UNSPECIFIED.);
#21289=B_SPLINE_CURVE_WITH_KNOTS('',3,(#94774,#94775,#94776,#94777,#94778,
#94779),.UNSPECIFIED.,.F.,.F.,(4,2,4),(-0.0573169284412124,-0.0286580503374737,
-1.00000000297085E-6),.UNSPECIFIED.);
#21290=B_SPLINE_CURVE_WITH_KNOTS('',3,(#94786,#94787,#94788,#94789,#94790,
#94791,#94792,#94793),.UNSPECIFIED.,.F.,.F.,(4,2,2,4),(-0.0565385909428617,
-0.0289781083737342,-0.0150821709628815,-9.99995018437222E-7),
 .UNSPECIFIED.);
#21291=B_SPLINE_CURVE_WITH_KNOTS('',3,(#94797,#94798,#94799,#94800,#94801,
#94802),.UNSPECIFIED.,.F.,.F.,(4,2,4),(0.,0.0322203319290619,0.0646290674001349),
 .UNSPECIFIED.);
#21292=B_SPLINE_CURVE_WITH_KNOTS('',3,(#94803,#94804,#94805,#94806,#94807,
#94808,#94809,#94810),.UNSPECIFIED.,.F.,.F.,(4,2,2,4),(1.00000000422679E-6,
0.0321173160094374,0.0481218021664386,0.0656773384695804),.UNSPECIFIED.);
#21293=B_SPLINE_CURVE_WITH_KNOTS('',3,(#94814,#94815,#94816,#94817,#94818,
#94819,#94820,#94821),.UNSPECIFIED.,.F.,.F.,(4,2,2,4),(-0.0565222177897274,
-0.0287750557807116,-0.0149768293136968,-9.9999999243635E-7),
 .UNSPECIFIED.);
#21294=B_SPLINE_CURVE_WITH_KNOTS('',3,(#94825,#94826,#94827,#94828,#94829,
#94830),.UNSPECIFIED.,.F.,.F.,(4,2,4),(0.,0.0322203317627138,0.0646290667350684),
 .UNSPECIFIED.);
#21295=B_SPLINE_CURVE_WITH_KNOTS('',3,(#94831,#94832,#94833,#94834,#94835,
#94836,#94837,#94838),.UNSPECIFIED.,.F.,.F.,(4,2,2,4),(9.99991096423042E-7,
0.0321173160104707,0.0481218021604403,0.0656773383081977),.UNSPECIFIED.);
#21296=B_SPLINE_CURVE_WITH_KNOTS('',3,(#94842,#94843,#94844,#94845,#94846,
#94847),.UNSPECIFIED.,.F.,.F.,(4,2,4),(-0.0571302337105162,-0.0285614237412303,
-1.08116577482442E-7),.UNSPECIFIED.);
#21297=B_SPLINE_CURVE_WITH_KNOTS('',3,(#94852,#94853,#94854,#94855,#94856,
#94857),.UNSPECIFIED.,.F.,.F.,(4,2,4),(-0.057780362676554,-0.0288853032294261,
0.),.UNSPECIFIED.);
#21298=B_SPLINE_CURVE_WITH_KNOTS('',3,(#94867,#94868,#94869,#94870,#94871,
#94872,#94873,#94874,#94875,#94876,#94877,#94878),.UNSPECIFIED.,.F.,.F.,
(4,2,2,2,2,4),(-0.0566496423577783,-0.0283349494939652,-0.014173165215246,
-0.00709713719677714,-0.00356047877726275,-9.99998007325086E-7),
 .UNSPECIFIED.);
#21299=B_SPLINE_CURVE_WITH_KNOTS('',3,(#94882,#94883,#94884,#94885,#94886,
#94887),.UNSPECIFIED.,.F.,.F.,(4,2,4),(-0.0195678427684003,-0.0097789163088001,
-1.00000000131592E-6),.UNSPECIFIED.);
#21300=B_SPLINE_CURVE_WITH_KNOTS('',3,(#94892,#94893,#94894,#94895,#94896,
#94897,#94898,#94899,#94900,#94901,#94902,#94903),.UNSPECIFIED.,.F.,.F.,
(4,2,2,2,2,4),(-0.0561346680975214,-0.0280769187502913,-0.0140437952091259,
-0.00703222858058154,-0.00352782999598223,-9.99998002995885E-7),
 .UNSPECIFIED.);
#21301=B_SPLINE_CURVE_WITH_KNOTS('',3,(#94905,#94906,#94907,#94908,#94909,
#94910,#94911,#94912,#94913,#94914,#94915,#94916),.UNSPECIFIED.,.F.,.F.,
(4,2,2,2,2,4),(-0.0574560295636826,-0.0538528231387187,-0.0502681692185173,
-0.0430935180878714,-0.0287239461347426,-1.00000000320677E-6),
 .UNSPECIFIED.);
#21302=B_SPLINE_CURVE_WITH_KNOTS('',3,(#94919,#94920,#94921,#94922,#94923,
#94924,#94925),.UNSPECIFIED.,.F.,.F.,(4,3,4),(0.561466076970076,0.571428571428571,
0.573654350219912),.UNSPECIFIED.);
#21303=B_SPLINE_CURVE_WITH_KNOTS('',3,(#94929,#94930,#94931,#94932,#94933,
#94934),.UNSPECIFIED.,.F.,.F.,(4,2,4),(-0.0573159301739154,-0.028658877119166,
-1.49350296713147E-9),.UNSPECIFIED.);
#21304=B_SPLINE_CURVE_WITH_KNOTS('',3,(#94936,#94937,#94938,#94939,#94940,
#94941),.UNSPECIFIED.,.F.,.F.,(4,2,4),(-0.057672909991192,-0.0288316538962247,
0.),.UNSPECIFIED.);
#21305=B_SPLINE_CURVE_WITH_KNOTS('',3,(#94948,#94949,#94950,#94951,#94952,
#94953),.UNSPECIFIED.,.F.,.F.,(4,2,4),(-0.0574770388054117,-0.0287417250918333,
-8.17334270396264E-7),.UNSPECIFIED.);
#21306=B_SPLINE_CURVE_WITH_KNOTS('',3,(#94958,#94959,#94960,#94961,#94962,
#94963,#94964,#94965,#94966,#94967,#94968,#94969),.UNSPECIFIED.,.F.,.F.,
(4,2,2,2,2,4),(-0.0561043953618418,-0.0280676019824481,-0.0140500801416394,
-0.00703969588014835,-0.00353423521231409,-9.99997658238257E-7),
 .UNSPECIFIED.);
#21307=B_SPLINE_CURVE_WITH_KNOTS('',3,(#94973,#94974,#94975,#94976,#94977,
#94978),.UNSPECIFIED.,.F.,.F.,(4,2,4),(-0.057780356336134,-0.0288950562791449,
0.),.UNSPECIFIED.);
#21308=B_SPLINE_CURVE_WITH_KNOTS('',3,(#94983,#94984,#94985,#94986,#94987,
#94988),.UNSPECIFIED.,.F.,.F.,(4,2,4),(-0.0571301202613454,-0.0285688614738928,
0.),.UNSPECIFIED.);
#21309=B_SPLINE_CURVE_WITH_KNOTS('',3,(#94992,#94993,#94994,#94995,#94996,
#94997),.UNSPECIFIED.,.F.,.F.,(4,2,4),(-0.0576223282239704,-0.0288154818312603,
-4.30884426246665E-9),.UNSPECIFIED.);
#21310=B_SPLINE_CURVE_WITH_KNOTS('',3,(#94999,#95000,#95001,#95002,#95003,
#95004),.UNSPECIFIED.,.F.,.F.,(4,2,4),(-0.0573676464321654,-0.0286819361988204,
0.),.UNSPECIFIED.);
#21311=B_SPLINE_CURVE_WITH_KNOTS('',3,(#95011,#95012,#95013,#95014,#95015,
#95016),.UNSPECIFIED.,.F.,.F.,(4,2,4),(-0.0574342915312409,-0.0287114331456016,
0.),.UNSPECIFIED.);
#21312=B_SPLINE_CURVE_WITH_KNOTS('',3,(#95018,#95019,#95020,#95021,#95022,
#95023),.UNSPECIFIED.,.F.,.F.,(4,2,4),(-0.0568985403506689,-0.0284516023352449,
0.),.UNSPECIFIED.);
#21313=B_SPLINE_CURVE_WITH_KNOTS('',3,(#95025,#95026,#95027,#95028,#95029,
#95030,#95031),.UNSPECIFIED.,.F.,.F.,(4,3,4),(0.556108173865715,0.558333952657055,
0.56829644714547),.UNSPECIFIED.);
#21314=B_SPLINE_CURVE_WITH_KNOTS('',3,(#95036,#95037,#95038,#95039,#95040,
#95041,#95042,#95043,#95044,#95045,#95046,#95047),.UNSPECIFIED.,.F.,.F.,
(4,2,2,2,2,4),(-0.0570428819745678,-0.053445882283523,-0.0498799833985174,
-0.0427507600747344,-0.0285037200159628,-1.0000000026239E-6),
 .UNSPECIFIED.);
#21315=B_SPLINE_CURVE_WITH_KNOTS('',3,(#95049,#95050,#95051,#95052,#95053,
#95054,#95055),.UNSPECIFIED.,.F.,.F.,(4,3,4),(0.211502584834035,0.214285714285714,
0.223668160738941),.UNSPECIFIED.);
#21316=B_SPLINE_CURVE_WITH_KNOTS('',3,(#95058,#95059,#95060,#95061,#95062,
#95063,#95064,#95065,#95066,#95067,#95068,#95069),.UNSPECIFIED.,.F.,.F.,
(4,2,2,2,2,4),(-0.0570603956094416,-0.0285361344066156,-0.0142653177533523,
-0.00713983414874365,-0.00357971212702635,-9.99998303868496E-7),
 .UNSPECIFIED.);
#21317=B_SPLINE_CURVE_WITH_KNOTS('',3,(#95073,#95074,#95075,#95076,#95077,
#95078),.UNSPECIFIED.,.F.,.F.,(4,2,4),(-0.0568990633806027,-0.0284467206821982,
0.),.UNSPECIFIED.);
#21318=B_SPLINE_CURVE_WITH_KNOTS('',3,(#95080,#95081,#95082,#95083,#95084,
#95085),.UNSPECIFIED.,.F.,.F.,(4,2,4),(-0.0572914498457208,-0.0286510536431491,
-5.32725437971115E-7),.UNSPECIFIED.);
#21319=B_SPLINE_CURVE_WITH_KNOTS('',3,(#95088,#95089,#95090,#95091,#95092,
#95093,#95094),.UNSPECIFIED.,.F.,.F.,(4,3,4),(0.492524364188642,0.5,0.504719756176228),
 .UNSPECIFIED.);
#21320=B_SPLINE_CURVE_WITH_KNOTS('',3,(#95098,#95099,#95100,#95101,#95102,
#95103),.UNSPECIFIED.,.F.,.F.,(4,2,4),(-0.0573676595233862,-0.0286856897691478,
-3.24605807949115E-9),.UNSPECIFIED.);
#21321=B_SPLINE_CURVE_WITH_KNOTS('',3,(#95105,#95106,#95107,#95108,#95109,
#95110),.UNSPECIFIED.,.F.,.F.,(4,2,4),(-0.0576233201986482,-0.0288078428910178,
-9.99999995414337E-7),.UNSPECIFIED.);
#21322=B_SPLINE_CURVE_WITH_KNOTS('',3,(#95117,#95118,#95119,#95120,#95121,
#95122,#95123,#95124,#95125,#95126,#95127,#95128),.UNSPECIFIED.,.F.,.F.,
(4,2,2,2,2,4),(-0.0575510646040713,-0.0539361302807107,-0.0503439519248105,
-0.0431560029091156,-0.0287668658360023,-6.83499958589739E-7),
 .UNSPECIFIED.);
#21323=B_SPLINE_CURVE_WITH_KNOTS('',3,(#95133,#95134,#95135,#95136,#95137,
#95138),.UNSPECIFIED.,.F.,.F.,(4,2,4),(-0.0569454872676998,-0.0284745632844492,
0.),.UNSPECIFIED.);
#21324=B_SPLINE_CURVE_WITH_KNOTS('',3,(#95142,#95143,#95144,#95145,#95146,
#95147,#95148,#95149,#95150,#95151,#95152,#95153),.UNSPECIFIED.,.F.,.F.,
(4,2,2,2,2,4),(-0.0577515660945151,-0.0541295044023544,-0.0505262579966018,
-0.0433144621568262,-0.028870780592887,-1.00000000295003E-6),
 .UNSPECIFIED.);
#21325=B_SPLINE_CURVE_WITH_KNOTS('',3,(#95157,#95158,#95159,#95160,#95161,
#95162,#95163),.UNSPECIFIED.,.F.,.F.,(4,3,4),(0.216822083469361,0.226204530183523,
0.228987659635173),.UNSPECIFIED.);
#21326=B_SPLINE_CURVE_WITH_KNOTS('',3,(#95164,#95165,#95166,#95167,#95168,
#95169,#95170,#95171,#95172,#95173,#95174,#95175),.UNSPECIFIED.,.F.,.F.,
(4,2,2,2,2,4),(-0.0560479076491692,-0.0280423569795766,-0.014043826238136,
-0.00703895705498456,-0.0035352576931815,-9.9999747336922E-7),
 .UNSPECIFIED.);
#21327=B_SPLINE_CURVE_WITH_KNOTS('',3,(#95179,#95180,#95181,#95182,#95183,
#95184,#95185,#95186,#95187,#95188,#95189,#95190),.UNSPECIFIED.,.F.,.F.,
(4,2,2,2,2,4),(-0.0566023976945684,-0.0283201143529454,-0.0141826474504683,
-0.00710842036500782,-0.00357007369472462,-9.9999751700883E-7),
 .UNSPECIFIED.);
#21328=B_SPLINE_CURVE_WITH_KNOTS('',3,(#95192,#95193,#95194,#95195,#95196,
#95197,#95198,#95199,#95200,#95201,#95202,#95203),.UNSPECIFIED.,.F.,.F.,
(4,2,2,2,2,4),(-0.057449477443241,-0.0538288949054542,-0.0502387956155639,
-0.0430598494232536,-0.0287081071699643,-1.00000000289452E-6),
 .UNSPECIFIED.);
#21329=B_SPLINE_CURVE_WITH_KNOTS('',3,(#95210,#95211,#95212,#95213,#95214,
#95215),.UNSPECIFIED.,.F.,.F.,(4,2,4),(-0.0572909149330641,-0.0286403950999783,
0.),.UNSPECIFIED.);
#21330=B_SPLINE_CURVE_WITH_KNOTS('',3,(#95217,#95218,#95219,#95220,#95221,
#95222),.UNSPECIFIED.,.F.,.F.,(4,2,4),(-0.0568990693197607,-0.0284523472314896,
0.),.UNSPECIFIED.);
#21331=B_SPLINE_CURVE_WITH_KNOTS('',3,(#95224,#95225,#95226,#95227,#95228,
#95229,#95230),.UNSPECIFIED.,.F.,.F.,(4,3,4),(0.48715514075043,0.491874896926658,
0.499350532549397),.UNSPECIFIED.);
#21332=B_SPLINE_CURVE_WITH_KNOTS('',3,(#95235,#95236,#95237,#95238,#95239,
#95240),.UNSPECIFIED.,.F.,.F.,(4,2,4),(-0.0569334986336709,-0.028463750652435,
0.),.UNSPECIFIED.);
#21333=B_SPLINE_CURVE_WITH_KNOTS('',3,(#95242,#95243,#95244,#95245,#95246,
#95247,#95248),.UNSPECIFIED.,.F.,.F.,(4,3,4),(0.280433082999174,0.285714285714286,
0.292621536178163),.UNSPECIFIED.);
#21334=B_SPLINE_CURVE_WITH_KNOTS('',3,(#95251,#95252,#95253,#95254,#95255,
#95256),.UNSPECIFIED.,.F.,.F.,(4,2,4),(-0.0576789591924046,-0.0288354074676834,
0.),.UNSPECIFIED.);
#21335=B_SPLINE_CURVE_WITH_KNOTS('',3,(#95260,#95261,#95262,#95263,#95264,
#95265),.UNSPECIFIED.,.F.,.F.,(4,2,4),(-0.0569460402994186,-0.0284714798019895,
-5.58604225278371E-7),.UNSPECIFIED.);
#21336=B_SPLINE_CURVE_WITH_KNOTS('',3,(#95270,#95271,#95272,#95273,#95274,
#95275,#95276,#95277,#95278,#95279,#95280,#95281),.UNSPECIFIED.,.F.,.F.,
(4,2,2,2,2,4),(-0.0567857357688743,-0.0284022147232368,-0.0142045302570797,
-0.00711221946963176,-0.00356783632949885,-9.99998100444099E-7),
 .UNSPECIFIED.);
#21337=B_SPLINE_CURVE_WITH_KNOTS('',3,(#95285,#95286,#95287,#95288,#95289,
#95290,#95291,#95292,#95293,#95294,#95295,#95296),.UNSPECIFIED.,.F.,.F.,
(4,2,2,2,2,4),(-0.0562112132080888,-0.0281141846482453,-0.014059733108161,
-0.00703911312658264,-0.00353058973831441,-9.99998096606457E-7),
 .UNSPECIFIED.);
#21338=B_SPLINE_CURVE_WITH_KNOTS('',3,(#95298,#95299,#95300,#95301,#95302,
#95303),.UNSPECIFIED.,.F.,.F.,(4,2,4),(-0.0571470876313668,-0.0285778247753777,
0.),.UNSPECIFIED.);
#21339=B_SPLINE_CURVE_WITH_KNOTS('',3,(#95306,#95307,#95308,#95309,#95310,
#95311,#95312),.UNSPECIFIED.,.F.,.F.,(4,3,4),(0.42358846369814,0.428571428571429,
0.435775021750423),.UNSPECIFIED.);
#21340=B_SPLINE_CURVE_WITH_KNOTS('',3,(#95316,#95317,#95318,#95319,#95320,
#95321,#95322,#95323,#95324,#95325,#95326,#95327),.UNSPECIFIED.,.F.,.F.,
(4,2,2,2,2,4),(-0.056491689856467,-0.0282631794095709,-0.0141502161320577,
-0.00709071219975629,-0.00356034429513153,-9.99997614407541E-7),
 .UNSPECIFIED.);
#21341=B_SPLINE_CURVE_WITH_KNOTS('',3,(#95329,#95330,#95331,#95332,#95333,
#95334,#95335,#95336,#95337,#95338,#95339,#95340),.UNSPECIFIED.,.F.,.F.,
(4,2,2,2,2,4),(-0.0576025270320224,-0.0539702627479672,-0.0503692695304019,
-0.0431697930140531,-0.0287820217781061,0.),.UNSPECIFIED.);
#21342=B_SPLINE_CURVE_WITH_KNOTS('',3,(#95347,#95348,#95349,#95350,#95351,
#95352,#95353,#95354,#95355,#95356,#95357,#95358),.UNSPECIFIED.,.F.,.F.,
(4,2,2,2,2,4),(-0.0576015134966977,-0.0539845538225833,-0.0503896326973789,
-0.0431957729790647,-0.0287931162727432,-1.00000000270717E-6),
 .UNSPECIFIED.);
#21343=B_SPLINE_CURVE_WITH_KNOTS('',3,(#95362,#95363,#95364,#95365,#95366,
#95367,#95368,#95369,#95370,#95371),.UNSPECIFIED.,.F.,.F.,(4,3,3,4),(0.423693445108574,
0.425620451530082,0.435349091794206,0.435879799328077),.UNSPECIFIED.);
#21344=B_SPLINE_CURVE_WITH_KNOTS('',3,(#95372,#95373,#95374,#95375,#95376,
#95377),.UNSPECIFIED.,.F.,.F.,(4,2,4),(-0.0569012107371194,-0.0284528191557688,
0.),.UNSPECIFIED.);
#21345=B_SPLINE_CURVE_WITH_KNOTS('',3,(#95381,#95382,#95383,#95384,#95385,
#95386,#95387,#95388,#95389,#95390,#95391,#95392),.UNSPECIFIED.,.F.,.F.,
(4,2,2,2,2,4),(-0.0565652487692742,-0.0283008643122265,-0.0141717032683938,
-0.00710245601855418,-0.00356680599387045,-9.99997547592113E-7),
 .UNSPECIFIED.);
#21346=B_SPLINE_CURVE_WITH_KNOTS('',3,(#95394,#95395,#95396,#95397,#95398,
#95399,#95400,#95401,#95402,#95403,#95404,#95405),.UNSPECIFIED.,.F.,.F.,
(4,2,2,2,2,4),(-0.057501043497419,-0.0538762460046872,-0.0502825459294232,
-0.0430968152660369,-0.0287331731616107,-1.00000000260309E-6),
 .UNSPECIFIED.);
#21347=B_SPLINE_CURVE_WITH_KNOTS('',3,(#95412,#95413,#95414,#95415,#95416,
#95417),.UNSPECIFIED.,.F.,.F.,(4,2,4),(-0.0571470909339385,-0.028569266384501,
0.),.UNSPECIFIED.);
#21348=B_SPLINE_CURVE_WITH_KNOTS('',3,(#95419,#95420,#95421,#95422,#95423,
#95424,#95425,#95426,#95427,#95428,#95429,#95430),.UNSPECIFIED.,.F.,.F.,
(4,2,2,2,2,4),(-0.056963594349972,-0.0533866976743353,-0.0498311496816505,
-0.042716432598767,-0.0284736097788437,0.),.UNSPECIFIED.);
#21349=B_SPLINE_CURVE_WITH_KNOTS('',3,(#95432,#95433,#95434,#95435,#95436,
#95437,#95438),.UNSPECIFIED.,.F.,.F.,(4,3,4),(0.418382980245726,0.425586573424719,
0.430569538466614),.UNSPECIFIED.);
#21350=B_SPLINE_CURVE_WITH_KNOTS('',3,(#95443,#95444,#95445,#95446,#95447,
#95448),.UNSPECIFIED.,.F.,.F.,(4,2,4),(-0.0568968449092943,-0.02844581624333,
0.),.UNSPECIFIED.);
#21351=B_SPLINE_CURVE_WITH_KNOTS('',3,(#95450,#95451,#95452,#95453,#95454,
#95455,#95456),.UNSPECIFIED.,.F.,.F.,(4,3,4),(0.349369696074498,0.357142857142857,
0.361565077307018),.UNSPECIFIED.);
#21352=B_SPLINE_CURVE_WITH_KNOTS('',3,(#95459,#95460,#95461,#95462,#95463,
#95464),.UNSPECIFIED.,.F.,.F.,(4,2,4),(-0.0576283753952648,-0.0288101399450005,
0.),.UNSPECIFIED.);
#21353=B_SPLINE_CURVE_WITH_KNOTS('',3,(#95468,#95469,#95470,#95471,#95472,
#95473),.UNSPECIFIED.,.F.,.F.,(4,2,4),(-0.0569022074868186,-0.0284493899561334,
-1.0000000028286E-6),.UNSPECIFIED.);
#21354=B_SPLINE_CURVE_WITH_KNOTS('',3,(#95482,#95483,#95484,#95485,#95486,
#95487,#95488,#95489,#95490,#95491,#95492,#95493),.UNSPECIFIED.,.F.,.F.,
(4,2,2,2,2,4),(-0.056854015708012,-0.0284350428379476,-0.0142190433503679,
-0.00711841544860163,-0.0035700841982292,-9.99999247833419E-7),
 .UNSPECIFIED.);
#21355=B_SPLINE_CURVE_WITH_KNOTS('',3,(#95497,#95498,#95499,#95500,#95501,
#95502),.UNSPECIFIED.,.F.,.F.,(4,2,4),(-0.0570232805196483,-0.0285078556311891,
-1.09020267119453E-9),.UNSPECIFIED.);
#21356=B_SPLINE_CURVE_WITH_KNOTS('',3,(#95504,#95505,#95506,#95507,#95508,
#95509),.UNSPECIFIED.,.F.,.F.,(4,2,4),(-0.057023271731261,-0.0285154214692224,
0.),.UNSPECIFIED.);
#21357=B_SPLINE_CURVE_WITH_KNOTS('',3,(#95511,#95512,#95513,#95514,#95515,
#95516,#95517),.UNSPECIFIED.,.F.,.F.,(4,3,4),(0.349440546254527,0.359118183105585,
0.36160232099164),.UNSPECIFIED.);
#21358=B_SPLINE_CURVE_WITH_KNOTS('',3,(#95518,#95519,#95520,#95521,#95522,
#95523,#95524),.UNSPECIFIED.,.F.,.F.,(4,3,4),(0.354658719256804,0.357142857142857,
0.366820493993916),.UNSPECIFIED.);
#21359=B_SPLINE_CURVE_WITH_KNOTS('',3,(#95528,#95529,#95530,#95531,#95532,
#95533,#95534,#95535,#95536,#95537,#95538,#95539),.UNSPECIFIED.,.F.,.F.,
(4,2,2,2,2,4),(-0.0565283690570396,-0.0282817312463688,-0.0141608157756246,
-0.00709651449638661,-0.0035635432192549,-9.9999757965272E-7),
 .UNSPECIFIED.);
#21360=B_SPLINE_CURVE_WITH_KNOTS('',3,(#95541,#95542,#95543,#95544,#95545,
#95546,#95547,#95548,#95549,#95550,#95551,#95552),.UNSPECIFIED.,.F.,.F.,
(4,2,2,2,2,4),(-0.0575523718254953,-0.0539243377199946,-0.0503269858744379,
-0.0431343708071144,-0.0287586370093804,-1.00000000284595E-6),
 .UNSPECIFIED.);
#21361=B_SPLINE_CURVE_WITH_KNOTS('',3,(#95559,#95560,#95561,#95562,#95563,
#95564),.UNSPECIFIED.,.F.,.F.,(4,2,4),(-0.0576291512983601,-0.0288190103098961,
-7.73829620326349E-7),.UNSPECIFIED.);
#21362=B_SPLINE_CURVE_WITH_KNOTS('',3,(#95568,#95569,#95570,#95571,#95572,
#95573,#95574),.UNSPECIFIED.,.F.,.F.,(4,3,4),(0.354554262465766,0.35897648262994,
0.366749643698295),.UNSPECIFIED.);
#21363=B_SPLINE_CURVE_WITH_KNOTS('',3,(#95575,#95576,#95577,#95578,#95579,
#95580),.UNSPECIFIED.,.F.,.F.,(4,2,4),(-0.0568968542642774,-0.0284510332534586,
0.),.UNSPECIFIED.);
#21364=B_SPLINE_CURVE_WITH_KNOTS('',3,(#95594,#95595,#95596,#95597,#95598,
#95599),.UNSPECIFIED.,.F.,.F.,(4,2,4),(-0.0253041165894682,-0.0126519422562814,
-1.27103497865599E-9),.UNSPECIFIED.);
#21365=B_SPLINE_CURVE_WITH_KNOTS('',3,(#95619,#95620,#95621,#95622,#95623,
#95624),.UNSPECIFIED.,.F.,.F.,(4,2,4),(1.22797086782227E-9,0.0126519421698446,
0.0253041165830267),.UNSPECIFIED.);
#21366=B_SPLINE_CURVE_WITH_KNOTS('',3,(#95629,#95630,#95631,#95632,#95633,
#95634,#95635),.UNSPECIFIED.,.F.,.F.,(4,3,4),(0.354554262464466,0.35897648262994,
0.366749643698293),.UNSPECIFIED.);
#21367=B_SPLINE_CURVE_WITH_KNOTS('',3,(#95667,#95668,#95669,#95670,#95671,
#95672),.UNSPECIFIED.,.F.,.F.,(4,2,4),(1.22886243997288E-9,0.0126519421847456,
0.0253041066747003),.UNSPECIFIED.);
#21368=B_SPLINE_CURVE_WITH_KNOTS('',3,(#95677,#95678,#95679,#95680,#95681,
#95682,#95683),.UNSPECIFIED.,.F.,.F.,(4,3,4),(0.354554262465908,0.35897648262994,
0.366749643698296),.UNSPECIFIED.);
#21369=B_SPLINE_CURVE_WITH_KNOTS('',3,(#95715,#95716,#95717,#95718,#95719,
#95720),.UNSPECIFIED.,.F.,.F.,(4,2,4),(1.13389382337564E-9,0.0126519420571103,
0.0253041165505429),.UNSPECIFIED.);
#21370=B_SPLINE_CURVE_WITH_KNOTS('',3,(#95725,#95726,#95727,#95728,#95729,
#95730,#95731),.UNSPECIFIED.,.F.,.F.,(4,3,4),(0.354554262471115,0.35897648262994,
0.366749643698296),.UNSPECIFIED.);
#21371=B_SPLINE_CURVE_WITH_KNOTS('',3,(#95763,#95764,#95765,#95766,#95767,
#95768),.UNSPECIFIED.,.F.,.F.,(4,2,4),(1.25614526516976E-9,0.0126519421969114,
0.0253041165716633),.UNSPECIFIED.);
#21372=B_SPLINE_CURVE_WITH_KNOTS('',3,(#95773,#95774,#95775,#95776,#95777,
#95778,#95779),.UNSPECIFIED.,.F.,.F.,(4,3,4),(0.354554262465665,0.35897648262994,
0.366749643597688),.UNSPECIFIED.);
#21373=B_SPLINE_CURVE_WITH_KNOTS('',3,(#95811,#95812,#95813,#95814,#95815,
#95816),.UNSPECIFIED.,.F.,.F.,(4,2,4),(1.23585522307083E-9,0.0126519421620591,
0.0253041165217407),.UNSPECIFIED.);
#21374=B_SPLINE_CURVE_WITH_KNOTS('',3,(#95821,#95822,#95823,#95824,#95825,
#95826,#95827),.UNSPECIFIED.,.F.,.F.,(4,3,4),(0.354554262462879,0.35897648262994,
0.366749643698301),.UNSPECIFIED.);
#21375=B_SPLINE_CURVE_WITH_KNOTS('',3,(#95859,#95860,#95861,#95862,#95863,
#95864),.UNSPECIFIED.,.F.,.F.,(4,2,4),(1.25375314193379E-9,0.0126519422133957,
0.0253041068088959),.UNSPECIFIED.);
#21376=B_SPLINE_CURVE_WITH_KNOTS('',3,(#95869,#95870,#95871,#95872,#95873,
#95874,#95875),.UNSPECIFIED.,.F.,.F.,(4,3,4),(0.354554262465713,0.35897648262993,
0.366749643698289),.UNSPECIFIED.);
#21377=B_SPLINE_CURVE_WITH_KNOTS('',3,(#95904,#95905,#95906,#95907,#95908,
#95909),.UNSPECIFIED.,.F.,.F.,(4,2,4),(1.21054583768177E-9,0.0126519421279297,
0.0253041165445498),.UNSPECIFIED.);
#21378=B_SPLINE_CURVE_WITH_KNOTS('',3,(#95940,#95941,#95942,#95943,#95944,
#95945),.UNSPECIFIED.,.F.,.F.,(4,2,4),(1.24500010488438E-9,0.0126519422047664,
0.0253041166155102),.UNSPECIFIED.);
#21379=B_SPLINE_CURVE_WITH_KNOTS('',3,(#95950,#95951,#95952,#95953,#95954,
#95955,#95956),.UNSPECIFIED.,.F.,.F.,(4,3,4),(0.354554262464056,0.35897648262994,
0.366749643698291),.UNSPECIFIED.);
#21380=B_SPLINE_CURVE_WITH_KNOTS('',3,(#95988,#95989,#95990,#95991,#95992,
#95993),.UNSPECIFIED.,.F.,.F.,(4,2,4),(1.2271250292988E-9,0.0126519421558845,
0.0253041165535596),.UNSPECIFIED.);
#21381=B_SPLINE_CURVE_WITH_KNOTS('',3,(#95998,#95999,#96000,#96001,#96002,
#96003,#96004),.UNSPECIFIED.,.F.,.F.,(4,3,4),(0.354554262463436,0.35897648262994,
0.366749643698311),.UNSPECIFIED.);
#21382=B_SPLINE_CURVE_WITH_KNOTS('',3,(#96036,#96037,#96038,#96039,#96040,
#96041),.UNSPECIFIED.,.F.,.F.,(4,2,4),(1.14384665945145E-9,0.0126519420645045,
0.0253041165155239),.UNSPECIFIED.);
#21383=B_SPLINE_CURVE_WITH_KNOTS('',3,(#96046,#96047,#96048,#96049,#96050,
#96051,#96052),.UNSPECIFIED.,.F.,.F.,(4,3,4),(0.354554262467878,0.35897648262994,
0.366749643698312),.UNSPECIFIED.);
#21384=B_SPLINE_CURVE_WITH_KNOTS('',3,(#96084,#96085,#96086,#96087,#96088,
#96089),.UNSPECIFIED.,.F.,.F.,(4,2,4),(1.27010831980957E-9,0.0126519422191132,
0.0253041067971292),.UNSPECIFIED.);
#21385=B_SPLINE_CURVE_WITH_KNOTS('',3,(#96094,#96095,#96096,#96097,#96098,
#96099,#96100),.UNSPECIFIED.,.F.,.F.,(4,3,4),(0.354554262465897,0.35897648262994,
0.366749643698316),.UNSPECIFIED.);
#21386=B_SPLINE_CURVE_WITH_KNOTS('',3,(#96132,#96133,#96134,#96135,#96136,
#96137),.UNSPECIFIED.,.F.,.F.,(4,2,4),(1.27669895031569E-9,0.0126519422171678,
0.0253041165713666),.UNSPECIFIED.);
#21387=B_SPLINE_CURVE_WITH_KNOTS('',3,(#96142,#96143,#96144,#96145,#96146,
#96147,#96148),.UNSPECIFIED.,.F.,.F.,(4,3,4),(0.35455426246392,0.35897648262994,
0.366749643698315),.UNSPECIFIED.);
#21388=B_SPLINE_CURVE_WITH_KNOTS('',3,(#96180,#96181,#96182,#96183,#96184,
#96185),.UNSPECIFIED.,.F.,.F.,(4,2,4),(1.24828610089926E-9,0.0126519421970288,
0.025304116576285),.UNSPECIFIED.);
#21389=B_SPLINE_CURVE_WITH_KNOTS('',3,(#96190,#96191,#96192,#96193,#96194,
#96195,#96196),.UNSPECIFIED.,.F.,.F.,(4,3,4),(0.354554262462922,0.35897648262994,
0.366749643698316),.UNSPECIFIED.);
#21390=B_SPLINE_CURVE_WITH_KNOTS('',3,(#96228,#96229,#96230,#96231,#96232,
#96233),.UNSPECIFIED.,.F.,.F.,(4,2,4),(1.17451322090098E-9,0.0126519421270214,
0.0253041066457466),.UNSPECIFIED.);
#21391=B_SPLINE_CURVE_WITH_KNOTS('',3,(#96238,#96239,#96240,#96241,#96242,
#96243,#96244),.UNSPECIFIED.,.F.,.F.,(4,3,4),(0.354554262469628,0.35897648262994,
0.366749643698311),.UNSPECIFIED.);
#21392=B_SPLINE_CURVE_WITH_KNOTS('',3,(#96276,#96277,#96278,#96279,#96280,
#96281),.UNSPECIFIED.,.F.,.F.,(4,2,4),(1.25626333734773E-9,0.0126519421841047,
0.0253041165416163),.UNSPECIFIED.);
#21393=B_SPLINE_CURVE_WITH_KNOTS('',3,(#96286,#96287,#96288,#96289,#96290,
#96291,#96292),.UNSPECIFIED.,.F.,.F.,(4,3,4),(0.354554262467893,0.35897648262994,
0.366749643698315),.UNSPECIFIED.);
#21394=B_SPLINE_CURVE_WITH_KNOTS('',3,(#96324,#96325,#96326,#96327,#96328,
#96329),.UNSPECIFIED.,.F.,.F.,(4,2,4),(1.28286378602738E-9,0.0126519422213083,
0.025304116568378),.UNSPECIFIED.);
#21395=B_SPLINE_CURVE_WITH_KNOTS('',3,(#96334,#96335,#96336,#96337,#96338,
#96339,#96340),.UNSPECIFIED.,.F.,.F.,(4,3,4),(0.354554262466374,0.35897648262994,
0.366749643698312),.UNSPECIFIED.);
#21396=B_SPLINE_CURVE_WITH_KNOTS('',3,(#96372,#96373,#96374,#96375,#96376,
#96377),.UNSPECIFIED.,.F.,.F.,(4,2,4),(1.22233787626692E-9,0.0126519421803246,
0.025304106896539),.UNSPECIFIED.);
#21397=B_SPLINE_CURVE_WITH_KNOTS('',3,(#96382,#96383,#96384,#96385,#96386,
#96387,#96388),.UNSPECIFIED.,.F.,.F.,(4,3,4),(0.354554262464919,0.35897648262994,
0.366749643698291),.UNSPECIFIED.);
#21398=B_SPLINE_CURVE_WITH_KNOTS('',3,(#96420,#96421,#96422,#96423,#96424,
#96425),.UNSPECIFIED.,.F.,.F.,(4,2,4),(1.1695959771263E-9,0.0126519420867781,
0.0253041165465765),.UNSPECIFIED.);
#21399=B_SPLINE_CURVE_WITH_KNOTS('',3,(#96430,#96431,#96432,#96433,#96434,
#96435,#96436),.UNSPECIFIED.,.F.,.F.,(4,3,4),(0.354554262461511,0.35897648262994,
0.366749643698308),.UNSPECIFIED.);
#21400=B_SPLINE_CURVE_WITH_KNOTS('',3,(#96468,#96469,#96470,#96471,#96472,
#96473),.UNSPECIFIED.,.F.,.F.,(4,2,4),(1.14093229735712E-9,0.0126519420364998,
0.0253041164963297),.UNSPECIFIED.);
#21401=B_SPLINE_CURVE_WITH_KNOTS('',3,(#96478,#96479,#96480,#96481,#96482,
#96483,#96484),.UNSPECIFIED.,.F.,.F.,(4,3,4),(0.354554262463035,0.35897648262994,
0.366749643698315),.UNSPECIFIED.);
#21402=B_SPLINE_CURVE_WITH_KNOTS('',3,(#96516,#96517,#96518,#96519,#96520,
#96521),.UNSPECIFIED.,.F.,.F.,(4,2,4),(1.20804074884595E-9,0.0126519421458698,
0.0253041067969118),.UNSPECIFIED.);
#21403=B_SPLINE_CURVE_WITH_KNOTS('',3,(#96526,#96527,#96528,#96529,#96530,
#96531,#96532),.UNSPECIFIED.,.F.,.F.,(4,3,4),(0.354554262464831,0.35897648262994,
0.366749643698314),.UNSPECIFIED.);
#21404=B_SPLINE_CURVE_WITH_KNOTS('',3,(#96564,#96565,#96566,#96567,#96568,
#96569),.UNSPECIFIED.,.F.,.F.,(4,2,4),(1.27795252779781E-9,0.0126519422530381,
0.0253041068907193),.UNSPECIFIED.);
#21405=B_SPLINE_CURVE_WITH_KNOTS('',3,(#96574,#96575,#96576,#96577,#96578,
#96579,#96580),.UNSPECIFIED.,.F.,.F.,(4,3,4),(0.354554262463694,0.35897648262994,
0.366749643698315),.UNSPECIFIED.);
#21406=B_SPLINE_CURVE_WITH_KNOTS('',3,(#96612,#96613,#96614,#96615,#96616,
#96617),.UNSPECIFIED.,.F.,.F.,(4,2,4),(1.24746944309948E-9,0.0126519422080134,
0.0253041165805001),.UNSPECIFIED.);
#21407=B_SPLINE_CURVE_WITH_KNOTS('',3,(#96622,#96623,#96624,#96625,#96626,
#96627,#96628),.UNSPECIFIED.,.F.,.F.,(4,3,4),(0.354554262464067,0.35897648262994,
0.366749643698313),.UNSPECIFIED.);
#21408=B_SPLINE_CURVE_WITH_KNOTS('',3,(#96660,#96661,#96662,#96663,#96664,
#96665),.UNSPECIFIED.,.F.,.F.,(4,2,4),(1.20027758822408E-9,0.0126519421518311,
0.0253041067937676),.UNSPECIFIED.);
#21409=B_SPLINE_CURVE_WITH_KNOTS('',3,(#96670,#96671,#96672,#96673,#96674,
#96675,#96676),.UNSPECIFIED.,.F.,.F.,(4,3,4),(0.354554262466755,0.35897648262994,
0.366749643698314),.UNSPECIFIED.);
#21410=B_SPLINE_CURVE_WITH_KNOTS('',3,(#96708,#96709,#96710,#96711,#96712,
#96713),.UNSPECIFIED.,.F.,.F.,(4,2,4),(1.27554372607159E-9,0.0126519422389094,
0.0253041066678855),.UNSPECIFIED.);
#21411=B_SPLINE_CURVE_WITH_KNOTS('',3,(#96718,#96719,#96720,#96721,#96722,
#96723,#96724),.UNSPECIFIED.,.F.,.F.,(4,3,4),(0.35455426245947,0.35897648262994,
0.366749643698315),.UNSPECIFIED.);
#21412=B_SPLINE_CURVE_WITH_KNOTS('',3,(#96756,#96757,#96758,#96759,#96760,
#96761),.UNSPECIFIED.,.F.,.F.,(4,2,4),(1.1855147445423E-9,0.0126519421080607,
0.0253041145041627),.UNSPECIFIED.);
#21413=B_SPLINE_CURVE_WITH_KNOTS('',3,(#96777,#96778,#96779,#96780,#96781,
#96782,#96783),.UNSPECIFIED.,.F.,.F.,(4,3,4),(0.354554262463581,0.35897648262994,
0.366749643698313),.UNSPECIFIED.);
#21414=B_SPLINE_CURVE_WITH_KNOTS('',3,(#96804,#96805,#96806,#96807,#96808,
#96809),.UNSPECIFIED.,.F.,.F.,(4,2,4),(1.18324628300808E-9,0.0126519421085243,
0.0253041165600097),.UNSPECIFIED.);
#21415=B_SPLINE_CURVE_WITH_KNOTS('',3,(#96816,#96817,#96818,#96819,#96820,
#96821,#96822),.UNSPECIFIED.,.F.,.F.,(4,3,4),(0.354554262466107,0.358976482629941,
0.366749643597822),.UNSPECIFIED.);
#21416=B_SPLINE_CURVE_WITH_KNOTS('',3,(#96852,#96853,#96854,#96855,#96856,
#96857),.UNSPECIFIED.,.F.,.F.,(4,2,4),(1.25428146867077E-9,0.0126519422262571,
0.025304116573377),.UNSPECIFIED.);
#21417=B_SPLINE_CURVE_WITH_KNOTS('',3,(#96862,#96863,#96864,#96865,#96866,
#96867,#96868),.UNSPECIFIED.,.F.,.F.,(4,3,4),(0.354554262464714,0.35897648262994,
0.366749643698308),.UNSPECIFIED.);
#21418=B_SPLINE_CURVE_WITH_KNOTS('',3,(#96900,#96901,#96902,#96903,#96904,
#96905),.UNSPECIFIED.,.F.,.F.,(4,2,4),(1.20977334660385E-9,0.0126519421769555,
0.0253041067646983),.UNSPECIFIED.);
#21419=B_SPLINE_CURVE_WITH_KNOTS('',3,(#96910,#96911,#96912,#96913,#96914,
#96915,#96916),.UNSPECIFIED.,.F.,.F.,(4,3,4),(0.354554262461012,0.35897648262994,
0.366749643698309),.UNSPECIFIED.);
#21420=B_SPLINE_CURVE_WITH_KNOTS('',3,(#96932,#96933,#96934,#96935,#96936,
#96937,#96938),.UNSPECIFIED.,.F.,.F.,(4,3,4),(0.354554262463031,0.358976482629941,
0.366749643698308),.UNSPECIFIED.);
#21421=B_SPLINE_CURVE_WITH_KNOTS('',3,(#96969,#96970,#96971,#96972,#96973,
#96974),.UNSPECIFIED.,.F.,.F.,(4,2,4),(-0.025301896117623,-0.0126507931980699,
0.),.UNSPECIFIED.);
#21422=B_SPLINE_CURVE_WITH_KNOTS('',3,(#96991,#96992,#96993,#96994,#96995,
#96996),.UNSPECIFIED.,.F.,.F.,(4,2,4),(0.,0.0126507931358136,0.0253018398292252),
 .UNSPECIFIED.);
#21423=B_SPLINE_CURVE_WITH_KNOTS('',3,(#97027,#97028,#97029,#97030,#97031,
#97032),.UNSPECIFIED.,.F.,.F.,(4,2,4),(0.,0.0126507931414294,0.0253018407176949),
 .UNSPECIFIED.);
#21424=B_SPLINE_CURVE_WITH_KNOTS('',3,(#97063,#97064,#97065,#97066,#97067,
#97068),.UNSPECIFIED.,.F.,.F.,(4,2,4),(0.,0.0126507932051544,0.0253018397046649),
 .UNSPECIFIED.);
#21425=B_SPLINE_CURVE_WITH_KNOTS('',3,(#97099,#97100,#97101,#97102,#97103,
#97104),.UNSPECIFIED.,.F.,.F.,(4,2,4),(0.,0.0126507931990055,0.0253018403750161),
 .UNSPECIFIED.);
#21426=B_SPLINE_CURVE_WITH_KNOTS('',3,(#97135,#97136,#97137,#97138,#97139,
#97140),.UNSPECIFIED.,.F.,.F.,(4,2,4),(0.,0.0126507931801839,0.0253018454104523),
 .UNSPECIFIED.);
#21427=B_SPLINE_CURVE_WITH_KNOTS('',3,(#97171,#97172,#97173,#97174,#97175,
#97176),.UNSPECIFIED.,.F.,.F.,(4,2,4),(0.,0.0126507932159568,0.0253018398833246),
 .UNSPECIFIED.);
#21428=B_SPLINE_CURVE_WITH_KNOTS('',3,(#97207,#97208,#97209,#97210,#97211,
#97212),.UNSPECIFIED.,.F.,.F.,(4,2,4),(0.,0.0126507931255922,0.0253018388190776),
 .UNSPECIFIED.);
#21429=B_SPLINE_CURVE_WITH_KNOTS('',3,(#97243,#97244,#97245,#97246,#97247,
#97248),.UNSPECIFIED.,.F.,.F.,(4,2,4),(0.,0.0126507931615463,0.0253018378775686),
 .UNSPECIFIED.);
#21430=B_SPLINE_CURVE_WITH_KNOTS('',3,(#97279,#97280,#97281,#97282,#97283,
#97284),.UNSPECIFIED.,.F.,.F.,(4,2,4),(0.,0.0126507931939829,0.0253018409739029),
 .UNSPECIFIED.);
#21431=B_SPLINE_CURVE_WITH_KNOTS('',3,(#97315,#97316,#97317,#97318,#97319,
#97320),.UNSPECIFIED.,.F.,.F.,(4,2,4),(0.,0.0126507931551591,0.0253018408201183),
 .UNSPECIFIED.);
#21432=B_SPLINE_CURVE_WITH_KNOTS('',3,(#97351,#97352,#97353,#97354,#97355,
#97356),.UNSPECIFIED.,.F.,.F.,(4,2,4),(0.,0.0126507931660361,0.0253018422985339),
 .UNSPECIFIED.);
#21433=B_SPLINE_CURVE_WITH_KNOTS('',3,(#97387,#97388,#97389,#97390,#97391,
#97392),.UNSPECIFIED.,.F.,.F.,(4,2,4),(0.,0.0126507931795489,0.025301839656477),
 .UNSPECIFIED.);
#21434=B_SPLINE_CURVE_WITH_KNOTS('',3,(#97423,#97424,#97425,#97426,#97427,
#97428),.UNSPECIFIED.,.F.,.F.,(4,2,4),(0.,0.01265079313631,0.0253018368638526),
 .UNSPECIFIED.);
#21435=B_SPLINE_CURVE_WITH_KNOTS('',3,(#97456,#97457,#97458,#97459,#97460,
#97461),.UNSPECIFIED.,.F.,.F.,(4,2,4),(0.,0.012650792312641,0.0253018368495781),
 .UNSPECIFIED.);
#21436=B_SPLINE_CURVE_WITH_KNOTS('',3,(#97486,#97487,#97488,#97489,#97490,
#97491),.UNSPECIFIED.,.F.,.F.,(4,2,4),(0.,0.0126507931787782,0.0253018436051588),
 .UNSPECIFIED.);
#21437=B_SPLINE_CURVE_WITH_KNOTS('',3,(#97522,#97523,#97524,#97525,#97526,
#97527),.UNSPECIFIED.,.F.,.F.,(4,2,4),(0.,0.0126507932173269,0.025301841499238),
 .UNSPECIFIED.);
#21438=B_SPLINE_CURVE_WITH_KNOTS('',3,(#97558,#97559,#97560,#97561,#97562,
#97563),.UNSPECIFIED.,.F.,.F.,(4,2,4),(0.,0.0126507931648626,0.0253018400005243),
 .UNSPECIFIED.);
#21439=B_SPLINE_CURVE_WITH_KNOTS('',3,(#97594,#97595,#97596,#97597,#97598,
#97599),.UNSPECIFIED.,.F.,.F.,(4,2,4),(0.,0.0126507931986836,0.0253018399228487),
 .UNSPECIFIED.);
#21440=B_SPLINE_CURVE_WITH_KNOTS('',3,(#97630,#97631,#97632,#97633,#97634,
#97635),.UNSPECIFIED.,.F.,.F.,(4,2,4),(0.,0.0126507931659456,0.0253018397804687),
 .UNSPECIFIED.);
#21441=B_SPLINE_CURVE_WITH_KNOTS('',3,(#97666,#97667,#97668,#97669,#97670,
#97671),.UNSPECIFIED.,.F.,.F.,(4,2,4),(0.,0.0126507931509,0.0253018442887582),
 .UNSPECIFIED.);
#21442=B_SPLINE_CURVE_WITH_KNOTS('',3,(#97702,#97703,#97704,#97705,#97706,
#97707),.UNSPECIFIED.,.F.,.F.,(4,2,4),(0.,0.0126507932004658,0.0253018400813751),
 .UNSPECIFIED.);
#21443=B_SPLINE_CURVE_WITH_KNOTS('',3,(#97738,#97739,#97740,#97741,#97742,
#97743),.UNSPECIFIED.,.F.,.F.,(4,2,4),(0.,0.0126507931937709,0.0253018404936856),
 .UNSPECIFIED.);
#21444=B_SPLINE_CURVE_WITH_KNOTS('',3,(#97774,#97775,#97776,#97777,#97778,
#97779),.UNSPECIFIED.,.F.,.F.,(4,2,4),(0.,0.012650793170194,0.0253018416319173),
 .UNSPECIFIED.);
#21445=B_SPLINE_CURVE_WITH_KNOTS('',3,(#97810,#97811,#97812,#97813,#97814,
#97815),.UNSPECIFIED.,.F.,.F.,(4,2,4),(0.,0.012650793154378,0.0253018399998241),
 .UNSPECIFIED.);
#21446=B_SPLINE_CURVE_WITH_KNOTS('',3,(#97846,#97847,#97848,#97849,#97850,
#97851),.UNSPECIFIED.,.F.,.F.,(4,2,4),(0.,0.0126507931692436,0.0253018366163615),
 .UNSPECIFIED.);
#21447=B_SPLINE_CURVE_WITH_KNOTS('',3,(#97882,#97883,#97884,#97885,#97886,
#97887),.UNSPECIFIED.,.F.,.F.,(4,2,4),(0.,0.0126507931424441,0.0253018434987612),
 .UNSPECIFIED.);
#21448=B_SPLINE_CURVE_WITH_KNOTS('',3,(#97918,#97919,#97920,#97921,#97922,
#97923),.UNSPECIFIED.,.F.,.F.,(4,2,4),(0.,0.012650793177975,0.0253018389948225),
 .UNSPECIFIED.);
#21449=B_SPLINE_CURVE_WITH_KNOTS('',3,(#97954,#97955,#97956,#97957,#97958,
#97959),.UNSPECIFIED.,.F.,.F.,(4,2,4),(0.,0.0126507931974926,0.0253018394441971),
 .UNSPECIFIED.);
#21450=B_SPLINE_CURVE_WITH_KNOTS('',3,(#98001,#98002,#98003,#98004,#98005,
#98006),.UNSPECIFIED.,.F.,.F.,(4,2,4),(-0.0252968222747317,-0.0126485340355752,
-3.97891684877916E-11),.UNSPECIFIED.);
#21451=B_SPLINE_CURVE_WITH_KNOTS('',3,(#98027,#98028,#98029,#98030,#98031,
#98032),.UNSPECIFIED.,.F.,.F.,(4,2,4),(2.4930055133702E-11,0.0126487642954686,
0.0252973918365075),.UNSPECIFIED.);
#21452=B_SPLINE_CURVE_WITH_KNOTS('',3,(#98060,#98061,#98062,#98063,#98064,
#98065),.UNSPECIFIED.,.F.,.F.,(4,2,4),(1.06299847981298E-12,0.0126487806109542,
0.0252974322648405),.UNSPECIFIED.);
#21453=B_SPLINE_CURVE_WITH_KNOTS('',3,(#98093,#98094,#98095,#98096,#98097,
#98098),.UNSPECIFIED.,.F.,.F.,(4,2,4),(0.,0.0126487819673612,0.0252974355355889),
 .UNSPECIFIED.);
#21454=B_SPLINE_CURVE_WITH_KNOTS('',3,(#98126,#98127,#98128,#98129,#98130,
#98131),.UNSPECIFIED.,.F.,.F.,(4,2,4),(2.02216262117331E-11,0.0126485332971288,
0.0252968216372051),.UNSPECIFIED.);
#21455=B_SPLINE_CURVE_WITH_KNOTS('',3,(#98159,#98160,#98161,#98162,#98163,
#98164),.UNSPECIFIED.,.F.,.F.,(4,2,4),(7.79977517694186E-12,0.0126487761627237,
0.0252974213259377),.UNSPECIFIED.);
#21456=B_SPLINE_CURVE_WITH_KNOTS('',3,(#98192,#98193,#98194,#98195,#98196,
#98197),.UNSPECIFIED.,.F.,.F.,(4,2,4),(2.34210737441738E-11,0.0126485332359888,
0.0252968215446288),.UNSPECIFIED.);
#21457=B_SPLINE_CURVE_WITH_KNOTS('',3,(#98225,#98226,#98227,#98228,#98229,
#98230),.UNSPECIFIED.,.F.,.F.,(4,2,4),(1.19327002275374E-11,0.0126487730325725,
0.0252974135839664),.UNSPECIFIED.);
#21458=B_SPLINE_CURVE_WITH_KNOTS('',3,(#98253,#98254,#98255,#98256,#98257,
#98258,#98259),.UNSPECIFIED.,.F.,.F.,(4,3,4),(0.349440546428683,0.359118183105575,
0.366891343983517),.UNSPECIFIED.);
#21459=B_SPLINE_CURVE_WITH_KNOTS('',3,(#98260,#98261,#98262,#98263,#98264,
#98265),.UNSPECIFIED.,.F.,.F.,(4,2,4),(7.32486372522864E-12,0.012648776417134,
0.0252974219410064),.UNSPECIFIED.);
#21460=B_SPLINE_CURVE_WITH_KNOTS('',3,(#98293,#98294,#98295,#98296,#98297,
#98298),.UNSPECIFIED.,.F.,.F.,(4,2,4),(2.09439513833029E-11,0.0126487669063908,
0.0252973984035197),.UNSPECIFIED.);
#21461=B_SPLINE_CURVE_WITH_KNOTS('',3,(#98326,#98327,#98328,#98329,#98330,
#98331),.UNSPECIFIED.,.F.,.F.,(4,2,4),(1.75967404397773E-11,0.0126487691768794,
0.0252974041382715),.UNSPECIFIED.);
#21462=B_SPLINE_CURVE_WITH_KNOTS('',3,(#98359,#98360,#98361,#98362,#98363,
#98364),.UNSPECIFIED.,.F.,.F.,(4,2,4),(1.83356697675752E-11,0.0126485331736315,
0.0252968214947279),.UNSPECIFIED.);
#21463=B_SPLINE_CURVE_WITH_KNOTS('',3,(#98392,#98393,#98394,#98395,#98396,
#98397),.UNSPECIFIED.,.F.,.F.,(4,2,4),(0.,0.0126487818894144,0.0252974352300546),
 .UNSPECIFIED.);
#21464=B_SPLINE_CURVE_WITH_KNOTS('',3,(#98420,#98421,#98422,#98423,#98424,
#98425,#98426),.UNSPECIFIED.,.F.,.F.,(4,3,4),(0.34944054642042,0.359118183105584,
0.366891343966254),.UNSPECIFIED.);
#21465=B_SPLINE_CURVE_WITH_KNOTS('',3,(#98427,#98428,#98429,#98430,#98431,
#98432),.UNSPECIFIED.,.F.,.F.,(4,2,4),(2.2110290768274E-11,0.0126487661437097,
0.0252973965918914),.UNSPECIFIED.);
#21466=B_SPLINE_CURVE_WITH_KNOTS('',3,(#98455,#98456,#98457,#98458,#98459,
#98460,#98461),.UNSPECIFIED.,.F.,.F.,(4,3,4),(0.34944054643076,0.359118183105584,
0.366891343982794),.UNSPECIFIED.);
#21467=B_SPLINE_CURVE_WITH_KNOTS('',3,(#98462,#98463,#98464,#98465,#98466,
#98467),.UNSPECIFIED.,.F.,.F.,(4,2,4),(1.85027300324741E-11,0.0126487683840182,
0.0252974020813789),.UNSPECIFIED.);
#21468=B_SPLINE_CURVE_WITH_KNOTS('',3,(#98495,#98496,#98497,#98498,#98499,
#98500),.UNSPECIFIED.,.F.,.F.,(4,2,4),(6.19813334009103E-12,0.0126487769390593,
0.0252974231853191),.UNSPECIFIED.);
#21469=B_SPLINE_CURVE_WITH_KNOTS('',3,(#98528,#98529,#98530,#98531,#98532,
#98533),.UNSPECIFIED.,.F.,.F.,(4,2,4),(2.73609851843378E-11,0.0126485332881475,
0.0252968216301982),.UNSPECIFIED.);
#21470=B_SPLINE_CURVE_WITH_KNOTS('',3,(#98556,#98557,#98558,#98559,#98560,
#98561,#98562),.UNSPECIFIED.,.F.,.F.,(4,3,4),(0.349440546443715,0.359118183105584,
0.366891343968371),.UNSPECIFIED.);
#21471=B_SPLINE_CURVE_WITH_KNOTS('',3,(#98563,#98564,#98565,#98566,#98567,
#98568),.UNSPECIFIED.,.F.,.F.,(4,2,4),(2.1438238389322E-11,0.0126485333091484,
0.0252968216454632),.UNSPECIFIED.);
#21472=B_SPLINE_CURVE_WITH_KNOTS('',3,(#98596,#98597,#98598,#98599,#98600,
#98601),.UNSPECIFIED.,.F.,.F.,(4,2,4),(0.,0.0126487830481352,0.0252974383448801),
 .UNSPECIFIED.);
#21473=B_SPLINE_CURVE_WITH_KNOTS('',3,(#98629,#98630,#98631,#98632,#98633,
#98634),.UNSPECIFIED.,.F.,.F.,(4,2,4),(1.81243554678628E-11,0.0126485332044211,
0.0252968215077904),.UNSPECIFIED.);
#21474=B_SPLINE_CURVE_WITH_KNOTS('',3,(#98662,#98663,#98664,#98665,#98666,
#98667),.UNSPECIFIED.,.F.,.F.,(4,2,4),(2.03986063368461E-11,0.0126487673816439,
0.0252973996335729),.UNSPECIFIED.);
#21475=B_SPLINE_CURVE_WITH_KNOTS('',3,(#98695,#98696,#98697,#98698,#98699,
#98700),.UNSPECIFIED.,.F.,.F.,(4,2,4),(2.09995354766813E-11,0.0126487669715886,
0.025297398571651),.UNSPECIFIED.);
#21476=B_SPLINE_CURVE_WITH_KNOTS('',3,(#98728,#98729,#98730,#98731,#98732,
#98733),.UNSPECIFIED.,.F.,.F.,(4,2,4),(1.41098486060602E-11,0.0126487722024124,
0.0252974114970913),.UNSPECIFIED.);
#21477=B_SPLINE_CURVE_WITH_KNOTS('',3,(#98756,#98757,#98758,#98759,#98760,
#98761,#98762),.UNSPECIFIED.,.F.,.F.,(4,3,4),(0.349440546421231,0.359118183105583,
0.366891343969192),.UNSPECIFIED.);
#21478=B_SPLINE_CURVE_WITH_KNOTS('',3,(#98763,#98764,#98765,#98766,#98767,
#98768),.UNSPECIFIED.,.F.,.F.,(4,2,4),(2.14692335976709E-11,0.0126487665330256,
0.0252973975434842),.UNSPECIFIED.);
#21479=B_SPLINE_CURVE_WITH_KNOTS('',3,(#98791,#98792,#98793,#98794,#98795,
#98796,#98797),.UNSPECIFIED.,.F.,.F.,(4,3,4),(0.349440546426762,0.359118183105585,
0.36689134398469),.UNSPECIFIED.);
#21480=B_SPLINE_CURVE_WITH_KNOTS('',3,(#98798,#98799,#98800,#98801,#98802,
#98803),.UNSPECIFIED.,.F.,.F.,(4,2,4),(1.42644977650254E-11,0.0126487720073413,
0.0252974110349891),.UNSPECIFIED.);
#21481=B_SPLINE_CURVE_WITH_KNOTS('',3,(#98826,#98827,#98828,#98829,#98830,
#98831,#98832),.UNSPECIFIED.,.F.,.F.,(4,3,4),(0.349440546444724,0.359118183105575,
0.366891343976162),.UNSPECIFIED.);
#21482=B_SPLINE_CURVE_WITH_KNOTS('',3,(#98833,#98834,#98835,#98836,#98837,
#98838),.UNSPECIFIED.,.F.,.F.,(4,2,4),(2.30917275227515E-11,0.0126487657781454,
0.0252973956021664),.UNSPECIFIED.);
#21483=B_SPLINE_CURVE_WITH_KNOTS('',3,(#98866,#98867,#98868,#98869,#98870,
#98871),.UNSPECIFIED.,.F.,.F.,(4,2,4),(3.48171027160651E-12,0.0126487789656072,
0.0252974281398367),.UNSPECIFIED.);
#21484=B_SPLINE_CURVE_WITH_KNOTS('',3,(#98899,#98900,#98901,#98902,#98903,
#98904),.UNSPECIFIED.,.F.,.F.,(4,2,4),(2.39852113345501E-11,0.0126485332174892,
0.0252968215388629),.UNSPECIFIED.);
#21485=B_SPLINE_CURVE_WITH_KNOTS('',3,(#98932,#98933,#98934,#98935,#98936,
#98937),.UNSPECIFIED.,.F.,.F.,(4,2,4),(2.27914024165646E-11,0.0126487660730579,
0.025297396383094),.UNSPECIFIED.);
#21486=B_SPLINE_CURVE_WITH_KNOTS('',3,(#98959,#98960,#98961,#98962,#98963,
#98964,#98965),.UNSPECIFIED.,.F.,.F.,(4,3,4),(0.34944054635293,0.359118183105576,
0.366891343960253),.UNSPECIFIED.);
#21487=B_SPLINE_CURVE_WITH_KNOTS('',3,(#98977,#98978,#98979,#98980,#98981,
#98982),.UNSPECIFIED.,.F.,.F.,(4,2,4),(-0.0253024024802803,-0.0126513104386297,
-3.22408107156225E-11),.UNSPECIFIED.);
#21488=B_SPLINE_CURVE_WITH_KNOTS('',3,(#98992,#98993,#98994,#98995,#98996,
#98997),.UNSPECIFIED.,.F.,.F.,(4,2,4),(0.,0.0126514186993098,0.0253028391623086),
 .UNSPECIFIED.);
#21489=B_SPLINE_CURVE_WITH_KNOTS('',3,(#99017,#99018,#99019,#99020,#99021,
#99022),.UNSPECIFIED.,.F.,.F.,(4,2,4),(0.,0.0126513104266705,0.0253026028382203),
 .UNSPECIFIED.);
#21490=B_SPLINE_CURVE_WITH_KNOTS('',3,(#99042,#99043,#99044,#99045,#99046,
#99047),.UNSPECIFIED.,.F.,.F.,(4,2,4),(0.,0.0126513104352019,0.0253026054726913),
 .UNSPECIFIED.);
#21491=B_SPLINE_CURVE_WITH_KNOTS('',3,(#99067,#99068,#99069,#99070,#99071,
#99072),.UNSPECIFIED.,.F.,.F.,(4,2,4),(0.,0.0126514192705249,0.0253028843562621),
 .UNSPECIFIED.);
#21492=B_SPLINE_CURVE_WITH_KNOTS('',3,(#99092,#99093,#99094,#99095,#99096,
#99097),.UNSPECIFIED.,.F.,.F.,(4,2,4),(3.07303747784289E-11,0.0126513104659004,
0.0253025998666621),.UNSPECIFIED.);
#21493=B_SPLINE_CURVE_WITH_KNOTS('',3,(#99117,#99118,#99119,#99120,#99121,
#99122),.UNSPECIFIED.,.F.,.F.,(4,2,4),(0.,0.012651415837005,0.025302853406244),
 .UNSPECIFIED.);
#21494=B_SPLINE_CURVE_WITH_KNOTS('',3,(#99142,#99143,#99144,#99145,#99146,
#99147),.UNSPECIFIED.,.F.,.F.,(4,2,4),(3.17187722703119E-11,0.0126513104750006,
0.025302575716232),.UNSPECIFIED.);
#21495=B_SPLINE_CURVE_WITH_KNOTS('',3,(#99167,#99168,#99169,#99170,#99171,
#99172),.UNSPECIFIED.,.F.,.F.,(4,2,4),(0.,0.0126513104444747,0.0253025668836647),
 .UNSPECIFIED.);
#21496=B_SPLINE_CURVE_WITH_KNOTS('',3,(#99192,#99193,#99194,#99195,#99196,
#99197),.UNSPECIFIED.,.F.,.F.,(4,2,4),(0.,0.0126514173543735,0.0253028567149204),
 .UNSPECIFIED.);
#21497=B_SPLINE_CURVE_WITH_KNOTS('',3,(#99217,#99218,#99219,#99220,#99221,
#99222),.UNSPECIFIED.,.F.,.F.,(4,2,4),(1.21088415704605E-11,0.0126513104312721,
0.025302596907673),.UNSPECIFIED.);
#21498=B_SPLINE_CURVE_WITH_KNOTS('',3,(#99242,#99243,#99244,#99245,#99246,
#99247),.UNSPECIFIED.,.F.,.F.,(4,2,4),(0.,0.0126514160175796,0.0253028651351513),
 .UNSPECIFIED.);
#21499=B_SPLINE_CURVE_WITH_KNOTS('',3,(#99267,#99268,#99269,#99270,#99271,
#99272),.UNSPECIFIED.,.F.,.F.,(4,2,4),(0.,0.0126513104367901,0.0253025876817578),
 .UNSPECIFIED.);
#21500=B_SPLINE_CURVE_WITH_KNOTS('',3,(#99292,#99293,#99294,#99295,#99296,
#99297),.UNSPECIFIED.,.F.,.F.,(4,2,4),(1.85760836726596E-11,0.012651310426484,
0.0253026171941702),.UNSPECIFIED.);
#21501=B_SPLINE_CURVE_WITH_KNOTS('',3,(#99317,#99318,#99319,#99320,#99321,
#99322),.UNSPECIFIED.,.F.,.F.,(4,2,4),(3.0195017719144E-9,0.0126513119669391,
0.0253025600041394),.UNSPECIFIED.);
#21502=B_SPLINE_CURVE_WITH_KNOTS('',3,(#99342,#99343,#99344,#99345,#99346,
#99347),.UNSPECIFIED.,.F.,.F.,(4,2,4),(0.,0.0126514153988426,0.0253028618808356),
 .UNSPECIFIED.);
#21503=B_SPLINE_CURVE_WITH_KNOTS('',3,(#99367,#99368,#99369,#99370,#99371,
#99372),.UNSPECIFIED.,.F.,.F.,(4,2,4),(0.,0.0126514155647745,0.0253028678646022),
 .UNSPECIFIED.);
#21504=B_SPLINE_CURVE_WITH_KNOTS('',3,(#99392,#99393,#99394,#99395,#99396,
#99397),.UNSPECIFIED.,.F.,.F.,(4,2,4),(0.,0.01265141535393,0.0253028708923844),
 .UNSPECIFIED.);
#21505=B_SPLINE_CURVE_WITH_KNOTS('',3,(#99417,#99418,#99419,#99420,#99421,
#99422),.UNSPECIFIED.,.F.,.F.,(4,2,4),(0.,0.0126513104241505,0.0253026011176279),
 .UNSPECIFIED.);
#21506=B_SPLINE_CURVE_WITH_KNOTS('',3,(#99442,#99443,#99444,#99445,#99446,
#99447),.UNSPECIFIED.,.F.,.F.,(4,2,4),(0.,0.0126513104450393,0.0253025900704875),
 .UNSPECIFIED.);
#21507=B_SPLINE_CURVE_WITH_KNOTS('',3,(#99467,#99468,#99469,#99470,#99471,
#99472),.UNSPECIFIED.,.F.,.F.,(4,2,4),(0.,0.0126514181045253,0.0253028758811497),
 .UNSPECIFIED.);
#21508=B_SPLINE_CURVE_WITH_KNOTS('',3,(#99492,#99493,#99494,#99495,#99496,
#99497),.UNSPECIFIED.,.F.,.F.,(4,2,4),(0.,0.0126514168979517,0.0253028479507141),
 .UNSPECIFIED.);
#21509=B_SPLINE_CURVE_WITH_KNOTS('',3,(#99517,#99518,#99519,#99520,#99521,
#99522),.UNSPECIFIED.,.F.,.F.,(4,2,4),(1.03319412963558E-11,0.0126513104477166,
0.0253025953666836),.UNSPECIFIED.);
#21510=B_SPLINE_CURVE_WITH_KNOTS('',3,(#99542,#99543,#99544,#99545,#99546,
#99547),.UNSPECIFIED.,.F.,.F.,(4,2,4),(0.,0.0126513104317339,0.0253026134134014),
 .UNSPECIFIED.);
#21511=B_SPLINE_CURVE_WITH_KNOTS('',3,(#99567,#99568,#99569,#99570,#99571,
#99572),.UNSPECIFIED.,.F.,.F.,(4,2,4),(1.4734659535817E-11,0.0126513104749262,
0.0253025667468672),.UNSPECIFIED.);
#21512=B_SPLINE_CURVE_WITH_KNOTS('',3,(#99592,#99593,#99594,#99595,#99596,
#99597),.UNSPECIFIED.,.F.,.F.,(4,2,4),(0.,0.0126513104535364,0.025302578952868),
 .UNSPECIFIED.);
#21513=B_SPLINE_CURVE_WITH_KNOTS('',3,(#99617,#99618,#99619,#99620,#99621,
#99622),.UNSPECIFIED.,.F.,.F.,(4,2,4),(0.,0.0126514183264595,0.0253028634934918),
 .UNSPECIFIED.);
#21514=B_SPLINE_CURVE_WITH_KNOTS('',3,(#99642,#99643,#99644,#99645,#99646,
#99647),.UNSPECIFIED.,.F.,.F.,(4,2,4),(0.,0.0126513104631919,0.0253025656851542),
 .UNSPECIFIED.);
#21515=B_SPLINE_CURVE_WITH_KNOTS('',3,(#99667,#99668,#99669,#99670,#99671,
#99672),.UNSPECIFIED.,.F.,.F.,(4,2,4),(1.83621424804334E-11,0.0126513104370361,
0.0253026040775267),.UNSPECIFIED.);
#21516=B_SPLINE_CURVE_WITH_KNOTS('',3,(#99700,#99701,#99702,#99703,#99704,
#99705),.UNSPECIFIED.,.F.,.F.,(4,2,4),(-0.0252992074861097,-0.0126497276181275,
-4.51872914086771E-11),.UNSPECIFIED.);
#21517=B_SPLINE_CURVE_WITH_KNOTS('',3,(#99711,#99712,#99713,#99714,#99715,
#99716,#99717),.UNSPECIFIED.,.F.,.F.,(4,3,4),(0.34944054625452,0.359118183105574,
0.361602320900268),.UNSPECIFIED.);
#21518=B_SPLINE_CURVE_WITH_KNOTS('',3,(#99718,#99719,#99720,#99721,#99722,
#99723,#99724),.UNSPECIFIED.,.F.,.F.,(4,3,4),(0.354658719348169,0.357142857142857,
0.36682049399392),.UNSPECIFIED.);
#21519=B_SPLINE_CURVE_WITH_KNOTS('',3,(#99749,#99750,#99751,#99752,#99753,
#99754),.UNSPECIFIED.,.F.,.F.,(4,2,4),(-0.025299207529245,-0.0126497275618106,
-4.79960515775701E-11),.UNSPECIFIED.);
#21520=B_SPLINE_CURVE_WITH_KNOTS('',3,(#99760,#99761,#99762,#99763,#99764,
#99765,#99766),.UNSPECIFIED.,.F.,.F.,(4,3,4),(0.34944054625453,0.359118183105579,
0.361602320908138),.UNSPECIFIED.);
#21521=B_SPLINE_CURVE_WITH_KNOTS('',3,(#99767,#99768,#99769,#99770,#99771,
#99772,#99773),.UNSPECIFIED.,.F.,.F.,(4,3,4),(0.354658719340306,0.357142857142857,
0.366820493993925),.UNSPECIFIED.);
#21522=B_SPLINE_CURVE_WITH_KNOTS('',3,(#99798,#99799,#99800,#99801,#99802,
#99803),.UNSPECIFIED.,.F.,.F.,(4,2,4),(-0.0252992074685758,-0.0126497275506734,
0.),.UNSPECIFIED.);
#21523=B_SPLINE_CURVE_WITH_KNOTS('',3,(#99809,#99810,#99811,#99812,#99813,
#99814,#99815),.UNSPECIFIED.,.F.,.F.,(4,3,4),(0.349440546254528,0.359118183105579,
0.361602320895715),.UNSPECIFIED.);
#21524=B_SPLINE_CURVE_WITH_KNOTS('',3,(#99816,#99817,#99818,#99819,#99820,
#99821,#99822),.UNSPECIFIED.,.F.,.F.,(4,3,4),(0.354658719352732,0.357142857142857,
0.366820493993922),.UNSPECIFIED.);
#21525=B_SPLINE_CURVE_WITH_KNOTS('',3,(#99847,#99848,#99849,#99850,#99851,
#99852),.UNSPECIFIED.,.F.,.F.,(4,2,4),(-0.0252992075308213,-0.0126497276054392,
-6.4287731388335E-11),.UNSPECIFIED.);
#21526=B_SPLINE_CURVE_WITH_KNOTS('',3,(#99858,#99859,#99860,#99861,#99862,
#99863,#99864),.UNSPECIFIED.,.F.,.F.,(4,3,4),(0.349440546254525,0.359118183105574,
0.361602320910271),.UNSPECIFIED.);
#21527=B_SPLINE_CURVE_WITH_KNOTS('',3,(#99865,#99866,#99867,#99868,#99869,
#99870,#99871),.UNSPECIFIED.,.F.,.F.,(4,3,4),(0.35465871933817,0.357142857142857,
0.366820493993925),.UNSPECIFIED.);
#21528=B_SPLINE_CURVE_WITH_KNOTS('',3,(#99896,#99897,#99898,#99899,#99900,
#99901),.UNSPECIFIED.,.F.,.F.,(4,2,4),(-0.0252992075674429,-0.0126497276439361,
-7.94698716555242E-11),.UNSPECIFIED.);
#21529=B_SPLINE_CURVE_WITH_KNOTS('',3,(#99907,#99908,#99909,#99910,#99911,
#99912,#99913),.UNSPECIFIED.,.F.,.F.,(4,3,4),(0.349440546254528,0.359118183105575,
0.361602320917548),.UNSPECIFIED.);
#21530=B_SPLINE_CURVE_WITH_KNOTS('',3,(#99914,#99915,#99916,#99917,#99918,
#99919,#99920),.UNSPECIFIED.,.F.,.F.,(4,3,4),(0.354658719330895,0.357142857142857,
0.366820493993926),.UNSPECIFIED.);
#21531=B_SPLINE_CURVE_WITH_KNOTS('',3,(#99945,#99946,#99947,#99948,#99949,
#99950),.UNSPECIFIED.,.F.,.F.,(4,2,4),(-0.0252992075443036,-0.0126497275685402,
0.),.UNSPECIFIED.);
#21532=B_SPLINE_CURVE_WITH_KNOTS('',3,(#99956,#99957,#99958,#99959,#99960,
#99961,#99962),.UNSPECIFIED.,.F.,.F.,(4,3,4),(0.349440546254499,0.359118183105556,
0.361602320891685),.UNSPECIFIED.);
#21533=B_SPLINE_CURVE_WITH_KNOTS('',3,(#99963,#99964,#99965,#99966,#99967,
#99968,#99969),.UNSPECIFIED.,.F.,.F.,(4,3,4),(0.354658719356734,0.357142857142857,
0.366820493993918),.UNSPECIFIED.);
#21534=B_SPLINE_CURVE_WITH_KNOTS('',3,(#99994,#99995,#99996,#99997,#99998,
#99999),.UNSPECIFIED.,.F.,.F.,(4,2,4),(-0.0252992075564514,-0.0126497275878325,
-3.48532661065271E-11),.UNSPECIFIED.);
#21535=B_SPLINE_CURVE_WITH_KNOTS('',3,(#100005,#100006,#100007,#100008,
#100009,#100010,#100011),.UNSPECIFIED.,.F.,.F.,(4,3,4),(0.349440546254505,
0.359118183105556,0.361602320899659),.UNSPECIFIED.);
#21536=B_SPLINE_CURVE_WITH_KNOTS('',3,(#100012,#100013,#100014,#100015,
#100016,#100017,#100018),.UNSPECIFIED.,.F.,.F.,(4,3,4),(0.354658719348767,
0.357142857142857,0.366820493993923),.UNSPECIFIED.);
#21537=B_SPLINE_CURVE_WITH_KNOTS('',3,(#100043,#100044,#100045,#100046,
#100047,#100048),.UNSPECIFIED.,.F.,.F.,(4,2,4),(-0.0252992075025414,-0.0126497275798582,
-1.42233204381004E-11),.UNSPECIFIED.);
#21538=B_SPLINE_CURVE_WITH_KNOTS('',3,(#100054,#100055,#100056,#100057,
#100058,#100059,#100060),.UNSPECIFIED.,.F.,.F.,(4,3,4),(0.349440546254509,
0.359118183105557,0.361602320896234),.UNSPECIFIED.);
#21539=B_SPLINE_CURVE_WITH_KNOTS('',3,(#100061,#100062,#100063,#100064,
#100065,#100066,#100067),.UNSPECIFIED.,.F.,.F.,(4,3,4),(0.354658719352205,
0.357142857142857,0.366820493993925),.UNSPECIFIED.);
#21540=B_SPLINE_CURVE_WITH_KNOTS('',3,(#100092,#100093,#100094,#100095,
#100096,#100097),.UNSPECIFIED.,.F.,.F.,(4,2,4),(-0.0252992074674949,-0.0126497275846532,
-3.89155270508201E-11),.UNSPECIFIED.);
#21541=B_SPLINE_CURVE_WITH_KNOTS('',3,(#100103,#100104,#100105,#100106,
#100107,#100108,#100109),.UNSPECIFIED.,.F.,.F.,(4,3,4),(0.349440546254512,
0.359118183105557,0.361602320897654),.UNSPECIFIED.);
#21542=B_SPLINE_CURVE_WITH_KNOTS('',3,(#100110,#100111,#100112,#100113,
#100114,#100115,#100116),.UNSPECIFIED.,.F.,.F.,(4,3,4),(0.354658719350777,
0.357142857142857,0.366820493993927),.UNSPECIFIED.);
#21543=B_SPLINE_CURVE_WITH_KNOTS('',3,(#100141,#100142,#100143,#100144,
#100145,#100146),.UNSPECIFIED.,.F.,.F.,(4,2,4),(-0.0252992074820837,-0.012649727615419,
-2.83656396982135E-11),.UNSPECIFIED.);
#21544=B_SPLINE_CURVE_WITH_KNOTS('',3,(#100152,#100153,#100154,#100155,
#100156,#100157,#100158),.UNSPECIFIED.,.F.,.F.,(4,3,4),(0.349440546254527,
0.359118183105584,0.361602320896335),.UNSPECIFIED.);
#21545=B_SPLINE_CURVE_WITH_KNOTS('',3,(#100159,#100160,#100161,#100162,
#100163,#100164,#100165),.UNSPECIFIED.,.F.,.F.,(4,3,4),(0.354658719352108,
0.357142857142857,0.366820493993918),.UNSPECIFIED.);
#21546=B_SPLINE_CURVE_WITH_KNOTS('',3,(#100190,#100191,#100192,#100193,
#100194,#100195),.UNSPECIFIED.,.F.,.F.,(4,2,4),(-0.0252992074819737,-0.012649727562162,
-2.75737106758545E-11),.UNSPECIFIED.);
#21547=B_SPLINE_CURVE_WITH_KNOTS('',3,(#100201,#100202,#100203,#100204,
#100205,#100206,#100207),.UNSPECIFIED.,.F.,.F.,(4,3,4),(0.349440546254526,
0.359118183105584,0.361602320903358),.UNSPECIFIED.);
#21548=B_SPLINE_CURVE_WITH_KNOTS('',3,(#100208,#100209,#100210,#100211,
#100212,#100213,#100214),.UNSPECIFIED.,.F.,.F.,(4,3,4),(0.354658719345086,
0.357142857142857,0.366820493993917),.UNSPECIFIED.);
#21549=B_SPLINE_CURVE_WITH_KNOTS('',3,(#100239,#100240,#100241,#100242,
#100243,#100244),.UNSPECIFIED.,.F.,.F.,(4,2,4),(-0.0252992074565818,-0.0126497275867138,
-2.09927422667455E-11),.UNSPECIFIED.);
#21550=B_SPLINE_CURVE_WITH_KNOTS('',3,(#100250,#100251,#100252,#100253,
#100254,#100255,#100256),.UNSPECIFIED.,.F.,.F.,(4,3,4),(0.349440546254526,
0.359118183105584,0.361602320894819),.UNSPECIFIED.);
#21551=B_SPLINE_CURVE_WITH_KNOTS('',3,(#100257,#100258,#100259,#100260,
#100261,#100262,#100263),.UNSPECIFIED.,.F.,.F.,(4,3,4),(0.354658719353623,
0.357142857142857,0.366820493993916),.UNSPECIFIED.);
#21552=B_SPLINE_CURVE_WITH_KNOTS('',3,(#100288,#100289,#100290,#100291,
#100292,#100293),.UNSPECIFIED.,.F.,.F.,(4,2,4),(-0.0252992075329033,-0.0126497275798029,
-2.34377101060446E-11),.UNSPECIFIED.);
#21553=B_SPLINE_CURVE_WITH_KNOTS('',3,(#100299,#100300,#100301,#100302,
#100303,#100304,#100305),.UNSPECIFIED.,.F.,.F.,(4,3,4),(0.349440546254526,
0.359118183105585,0.361602320898788),.UNSPECIFIED.);
#21554=B_SPLINE_CURVE_WITH_KNOTS('',3,(#100306,#100307,#100308,#100309,
#100310,#100311,#100312),.UNSPECIFIED.,.F.,.F.,(4,3,4),(0.354658719349655,
0.357142857142857,0.366820493993916),.UNSPECIFIED.);
#21555=B_SPLINE_CURVE_WITH_KNOTS('',3,(#100337,#100338,#100339,#100340,
#100341,#100342),.UNSPECIFIED.,.F.,.F.,(4,2,4),(-0.0252992075070475,-0.0126497275566533,
-2.2880430189387E-11),.UNSPECIFIED.);
#21556=B_SPLINE_CURVE_WITH_KNOTS('',3,(#100348,#100349,#100350,#100351,
#100352,#100353,#100354),.UNSPECIFIED.,.F.,.F.,(4,3,4),(0.349440546254526,
0.359118183105584,0.361602320894655),.UNSPECIFIED.);
#21557=B_SPLINE_CURVE_WITH_KNOTS('',3,(#100355,#100356,#100357,#100358,
#100359,#100360,#100361),.UNSPECIFIED.,.F.,.F.,(4,3,4),(0.354658719353787,
0.357142857142857,0.366820493993916),.UNSPECIFIED.);
#21558=B_SPLINE_CURVE_WITH_KNOTS('',3,(#100383,#100384,#100385,#100386,
#100387,#100388),.UNSPECIFIED.,.F.,.F.,(4,2,4),(-0.025299207444391,-0.0126497275600756,
0.),.UNSPECIFIED.);
#21559=B_SPLINE_CURVE_WITH_KNOTS('',3,(#100414,#100415,#100416,#100417,
#100418,#100419),.UNSPECIFIED.,.F.,.F.,(4,2,4),(-0.0252992075196953,-0.0126497275585676,
0.),.UNSPECIFIED.);
#21560=B_SPLINE_CURVE_WITH_KNOTS('',3,(#100425,#100426,#100427,#100428,
#100429,#100430,#100431),.UNSPECIFIED.,.F.,.F.,(4,3,4),(0.349440546254527,
0.359118183105584,0.361602320894789),.UNSPECIFIED.);
#21561=B_SPLINE_CURVE_WITH_KNOTS('',3,(#100432,#100433,#100434,#100435,
#100436,#100437,#100438),.UNSPECIFIED.,.F.,.F.,(4,3,4),(0.354658719353653,
0.357142857142857,0.366820493993915),.UNSPECIFIED.);
#21562=B_SPLINE_CURVE_WITH_KNOTS('',3,(#100463,#100464,#100465,#100466,
#100467,#100468),.UNSPECIFIED.,.F.,.F.,(4,2,4),(-0.0252992074993662,-0.0126497275569599,
0.),.UNSPECIFIED.);
#21563=B_SPLINE_CURVE_WITH_KNOTS('',3,(#100474,#100475,#100476,#100477,
#100478,#100479,#100480),.UNSPECIFIED.,.F.,.F.,(4,3,4),(0.349440546254526,
0.359118183105584,0.361602320897223),.UNSPECIFIED.);
#21564=B_SPLINE_CURVE_WITH_KNOTS('',3,(#100481,#100482,#100483,#100484,
#100485,#100486,#100487),.UNSPECIFIED.,.F.,.F.,(4,3,4),(0.35465871935122,
0.357142857142857,0.366820493993917),.UNSPECIFIED.);
#21565=B_SPLINE_CURVE_WITH_KNOTS('',3,(#100512,#100513,#100514,#100515,
#100516,#100517),.UNSPECIFIED.,.F.,.F.,(4,2,4),(-0.0252992075499003,-0.0126497275861227,
-2.70313389727495E-11),.UNSPECIFIED.);
#21566=B_SPLINE_CURVE_WITH_KNOTS('',3,(#100523,#100524,#100525,#100526,
#100527,#100528,#100529),.UNSPECIFIED.,.F.,.F.,(4,3,4),(0.349440546254538,
0.359118183105585,0.361602320901477),.UNSPECIFIED.);
#21567=B_SPLINE_CURVE_WITH_KNOTS('',3,(#100530,#100531,#100532,#100533,
#100534,#100535,#100536),.UNSPECIFIED.,.F.,.F.,(4,3,4),(0.354658719346978,
0.357142857142857,0.366820493993928),.UNSPECIFIED.);
#21568=B_SPLINE_CURVE_WITH_KNOTS('',3,(#100561,#100562,#100563,#100564,
#100565,#100566),.UNSPECIFIED.,.F.,.F.,(4,2,4),(-0.0252992074665769,-0.0126497276102527,
-3.18740624172253E-11),.UNSPECIFIED.);
#21569=B_SPLINE_CURVE_WITH_KNOTS('',3,(#100572,#100573,#100574,#100575,
#100576,#100577,#100578),.UNSPECIFIED.,.F.,.F.,(4,3,4),(0.349440546254528,
0.359118183105584,0.361602320899168),.UNSPECIFIED.);
#21570=B_SPLINE_CURVE_WITH_KNOTS('',3,(#100579,#100580,#100581,#100582,
#100583,#100584,#100585),.UNSPECIFIED.,.F.,.F.,(4,3,4),(0.354658719349277,
0.357142857142857,0.366820493993918),.UNSPECIFIED.);
#21571=B_SPLINE_CURVE_WITH_KNOTS('',3,(#100610,#100611,#100612,#100613,
#100614,#100615),.UNSPECIFIED.,.F.,.F.,(4,2,4),(-0.0252992075104434,-0.0126497276265894,
-5.31206086062941E-11),.UNSPECIFIED.);
#21572=B_SPLINE_CURVE_WITH_KNOTS('',3,(#100621,#100622,#100623,#100624,
#100625,#100626,#100627),.UNSPECIFIED.,.F.,.F.,(4,3,4),(0.349440546254525,
0.359118183105584,0.361602320908414),.UNSPECIFIED.);
#21573=B_SPLINE_CURVE_WITH_KNOTS('',3,(#100628,#100629,#100630,#100631,
#100632,#100633,#100634),.UNSPECIFIED.,.F.,.F.,(4,3,4),(0.354658719340028,
0.357142857142857,0.366820493993916),.UNSPECIFIED.);
#21574=B_SPLINE_CURVE_WITH_KNOTS('',3,(#100659,#100660,#100661,#100662,
#100663,#100664),.UNSPECIFIED.,.F.,.F.,(4,2,4),(-0.0252992075512971,-0.0126497276191108,
-3.96639145139321E-11),.UNSPECIFIED.);
#21575=B_SPLINE_CURVE_WITH_KNOTS('',3,(#100670,#100671,#100672,#100673,
#100674,#100675,#100676),.UNSPECIFIED.,.F.,.F.,(4,3,4),(0.349440546254525,
0.359118183105584,0.361602320899554),.UNSPECIFIED.);
#21576=B_SPLINE_CURVE_WITH_KNOTS('',3,(#100677,#100678,#100679,#100680,
#100681,#100682,#100683),.UNSPECIFIED.,.F.,.F.,(4,3,4),(0.354658719348888,
0.357142857142857,0.366820493993916),.UNSPECIFIED.);
#21577=B_SPLINE_CURVE_WITH_KNOTS('',3,(#100708,#100709,#100710,#100711,
#100712,#100713),.UNSPECIFIED.,.F.,.F.,(4,2,4),(-0.0252992075592725,-0.0126497275811909,
-1.37217980034077E-11),.UNSPECIFIED.);
#21578=B_SPLINE_CURVE_WITH_KNOTS('',3,(#100719,#100720,#100721,#100722,
#100723,#100724,#100725),.UNSPECIFIED.,.F.,.F.,(4,3,4),(0.349440546254526,
0.359118183105584,0.361602320896881),.UNSPECIFIED.);
#21579=B_SPLINE_CURVE_WITH_KNOTS('',3,(#100726,#100727,#100728,#100729,
#100730,#100731,#100732),.UNSPECIFIED.,.F.,.F.,(4,3,4),(0.354658719351561,
0.357142857142857,0.366820493993916),.UNSPECIFIED.);
#21580=B_SPLINE_CURVE_WITH_KNOTS('',3,(#100757,#100758,#100759,#100760,
#100761,#100762),.UNSPECIFIED.,.F.,.F.,(4,2,4),(-0.0252992074877316,-0.0126497275715462,
-3.83596869546476E-11),.UNSPECIFIED.);
#21581=B_SPLINE_CURVE_WITH_KNOTS('',3,(#100768,#100769,#100770,#100771,
#100772,#100773,#100774),.UNSPECIFIED.,.F.,.F.,(4,3,4),(0.349440546254526,
0.359118183105585,0.361602320902751),.UNSPECIFIED.);
#21582=B_SPLINE_CURVE_WITH_KNOTS('',3,(#100775,#100776,#100777,#100778,
#100779,#100780,#100781),.UNSPECIFIED.,.F.,.F.,(4,3,4),(0.354658719345692,
0.357142857142857,0.366820493993916),.UNSPECIFIED.);
#21583=B_SPLINE_CURVE_WITH_KNOTS('',3,(#100806,#100807,#100808,#100809,
#100810,#100811),.UNSPECIFIED.,.F.,.F.,(4,2,4),(-0.0252992075355198,-0.0126497275638241,
-1.5956104493231E-11),.UNSPECIFIED.);
#21584=B_SPLINE_CURVE_WITH_KNOTS('',3,(#100817,#100818,#100819,#100820,
#100821,#100822,#100823),.UNSPECIFIED.,.F.,.F.,(4,3,4),(0.349440546254526,
0.359118183105584,0.361602320894257),.UNSPECIFIED.);
#21585=B_SPLINE_CURVE_WITH_KNOTS('',3,(#100824,#100825,#100826,#100827,
#100828,#100829,#100830),.UNSPECIFIED.,.F.,.F.,(4,3,4),(0.354658719354185,
0.357142857142857,0.366820493993915),.UNSPECIFIED.);
#21586=B_SPLINE_CURVE_WITH_KNOTS('',3,(#100855,#100856,#100857,#100858,
#100859,#100860),.UNSPECIFIED.,.F.,.F.,(4,2,4),(-0.0252992075880614,-0.0126497276978079,
-1.04693153452073E-10),.UNSPECIFIED.);
#21587=B_SPLINE_CURVE_WITH_KNOTS('',3,(#100877,#100878,#100879,#100880,
#100881,#100882,#100883),.UNSPECIFIED.,.F.,.F.,(4,3,4),(0.354658719352825,
0.357142857142857,0.366820493993845),.UNSPECIFIED.);
#21588=B_SPLINE_CURVE_WITH_KNOTS('',3,(#100888,#100889,#100890,#100891,
#100892,#100893,#100894),.UNSPECIFIED.,.F.,.F.,(4,3,4),(0.349440546254584,
0.359118183105571,0.361602320905615),.UNSPECIFIED.);
#21589=B_SPLINE_CURVE_WITH_KNOTS('',3,(#100905,#100906,#100907,#100908,
#100909,#100910),.UNSPECIFIED.,.F.,.F.,(4,2,4),(-0.0252992075859009,-0.0126497275934163,
-3.14907752652083E-11),.UNSPECIFIED.);
#21590=B_SPLINE_CURVE_WITH_KNOTS('',3,(#100913,#100914,#100915,#100916,
#100917,#100918,#100919),.UNSPECIFIED.,.F.,.F.,(4,3,4),(0.354658719349017,
0.357142857142857,0.366820493993916),.UNSPECIFIED.);
#21591=B_SPLINE_CURVE_WITH_KNOTS('',3,(#100922,#100923,#100924,#100925,
#100926,#100927,#100928),.UNSPECIFIED.,.F.,.F.,(4,3,4),(0.349440546254519,
0.359118183105576,0.361602320899417),.UNSPECIFIED.);
#21592=B_SPLINE_CURVE_WITH_KNOTS('',3,(#100953,#100954,#100955,#100956,
#100957,#100958),.UNSPECIFIED.,.F.,.F.,(4,2,4),(-0.02529920751647,-0.0126497276304353,
-7.15628598046969E-11),.UNSPECIFIED.);
#21593=B_SPLINE_CURVE_WITH_KNOTS('',3,(#100964,#100965,#100966,#100967,
#100968,#100969,#100970),.UNSPECIFIED.,.F.,.F.,(4,3,4),(0.349440546254522,
0.359118183105575,0.361602320915514),.UNSPECIFIED.);
#21594=B_SPLINE_CURVE_WITH_KNOTS('',3,(#100971,#100972,#100973,#100974,
#100975,#100976,#100977),.UNSPECIFIED.,.F.,.F.,(4,3,4),(0.354658719332922,
0.357142857142857,0.366820493993919),.UNSPECIFIED.);
#21595=B_SPLINE_CURVE_WITH_KNOTS('',3,(#101002,#101003,#101004,#101005,
#101006,#101007),.UNSPECIFIED.,.F.,.F.,(4,2,4),(-0.0252992075126512,-0.012649727600527,
-5.9683594871851E-11),.UNSPECIFIED.);
#21596=B_SPLINE_CURVE_WITH_KNOTS('',3,(#101013,#101014,#101015,#101016,
#101017,#101018,#101019),.UNSPECIFIED.,.F.,.F.,(4,3,4),(0.34944054625452,
0.359118183105575,0.361602320910578),.UNSPECIFIED.);
#21597=B_SPLINE_CURVE_WITH_KNOTS('',3,(#101020,#101021,#101022,#101023,
#101024,#101025,#101026),.UNSPECIFIED.,.F.,.F.,(4,3,4),(0.354658719337858,
0.357142857142857,0.366820493993919),.UNSPECIFIED.);
#21598=B_SPLINE_CURVE_WITH_KNOTS('',3,(#101051,#101052,#101053,#101054,
#101055,#101056),.UNSPECIFIED.,.F.,.F.,(4,2,4),(-0.0252992074769014,-0.0126497275766772,
-2.69583487477743E-11),.UNSPECIFIED.);
#21599=B_SPLINE_CURVE_WITH_KNOTS('',3,(#101062,#101063,#101064,#101065,
#101066,#101067,#101068),.UNSPECIFIED.,.F.,.F.,(4,3,4),(0.349440546254521,
0.359118183105576,0.361602320899696),.UNSPECIFIED.);
#21600=B_SPLINE_CURVE_WITH_KNOTS('',3,(#101069,#101070,#101071,#101072,
#101073,#101074,#101075),.UNSPECIFIED.,.F.,.F.,(4,3,4),(0.35465871934874,
0.357142857142857,0.366820493993919),.UNSPECIFIED.);
#21601=B_SPLINE_CURVE_WITH_KNOTS('',3,(#101105,#101106,#101107,#101108,
#101109,#101110),.UNSPECIFIED.,.F.,.F.,(4,2,4),(-0.0253041039872367,-0.0126521677792654,
0.),.UNSPECIFIED.);
#21602=B_SPLINE_CURVE_WITH_KNOTS('',3,(#101146,#101147,#101148,#101149,
#101150,#101151),.UNSPECIFIED.,.F.,.F.,(4,2,4),(-0.0253041039005391,-0.0126521677027421,
0.),.UNSPECIFIED.);
#21603=B_SPLINE_CURVE_WITH_KNOTS('',3,(#101187,#101188,#101189,#101190,
#101191,#101192),.UNSPECIFIED.,.F.,.F.,(4,2,4),(-0.0253041039632652,-0.012652167781081,
0.),.UNSPECIFIED.);
#21604=B_SPLINE_CURVE_WITH_KNOTS('',3,(#101228,#101229,#101230,#101231,
#101232,#101233),.UNSPECIFIED.,.F.,.F.,(4,2,4),(-0.0253041039571526,-0.0126521677600083,
0.),.UNSPECIFIED.);
#21605=B_SPLINE_CURVE_WITH_KNOTS('',3,(#101269,#101270,#101271,#101272,
#101273,#101274),.UNSPECIFIED.,.F.,.F.,(4,2,4),(-0.0253041038880339,-0.0126521676975068,
0.),.UNSPECIFIED.);
#21606=B_SPLINE_CURVE_WITH_KNOTS('',3,(#101310,#101311,#101312,#101313,
#101314,#101315),.UNSPECIFIED.,.F.,.F.,(4,2,4),(-0.0253041039499959,-0.0126521677582051,
0.),.UNSPECIFIED.);
#21607=B_SPLINE_CURVE_WITH_KNOTS('',3,(#101351,#101352,#101353,#101354,
#101355,#101356),.UNSPECIFIED.,.F.,.F.,(4,2,4),(-0.0253041038968693,-0.0126521677390511,
0.),.UNSPECIFIED.);
#21608=B_SPLINE_CURVE_WITH_KNOTS('',3,(#101392,#101393,#101394,#101395,
#101396,#101397),.UNSPECIFIED.,.F.,.F.,(4,2,4),(-0.025304103953758,-0.0126521677536738,
0.),.UNSPECIFIED.);
#21609=B_SPLINE_CURVE_WITH_KNOTS('',3,(#101433,#101434,#101435,#101436,
#101437,#101438),.UNSPECIFIED.,.F.,.F.,(4,2,4),(-0.0253041039231198,-0.0126521677416848,
0.),.UNSPECIFIED.);
#21610=B_SPLINE_CURVE_WITH_KNOTS('',3,(#101474,#101475,#101476,#101477,
#101478,#101479),.UNSPECIFIED.,.F.,.F.,(4,2,4),(-0.0253041039323966,-0.0126521677644877,
0.),.UNSPECIFIED.);
#21611=B_SPLINE_CURVE_WITH_KNOTS('',3,(#101515,#101516,#101517,#101518,
#101519,#101520),.UNSPECIFIED.,.F.,.F.,(4,2,4),(-0.0253041039471639,-0.0126521677898284,
0.),.UNSPECIFIED.);
#21612=B_SPLINE_CURVE_WITH_KNOTS('',3,(#101556,#101557,#101558,#101559,
#101560,#101561),.UNSPECIFIED.,.F.,.F.,(4,2,4),(-0.0253041039397315,-0.0126521677657765,
0.),.UNSPECIFIED.);
#21613=B_SPLINE_CURVE_WITH_KNOTS('',3,(#101597,#101598,#101599,#101600,
#101601,#101602),.UNSPECIFIED.,.F.,.F.,(4,2,4),(-0.0253041038956333,-0.0126521677148479,
0.),.UNSPECIFIED.);
#21614=B_SPLINE_CURVE_WITH_KNOTS('',3,(#101638,#101639,#101640,#101641,
#101642,#101643),.UNSPECIFIED.,.F.,.F.,(4,2,4),(-0.0253041039012348,-0.0126521676969631,
0.),.UNSPECIFIED.);
#21615=B_SPLINE_CURVE_WITH_KNOTS('',3,(#101679,#101680,#101681,#101682,
#101683,#101684),.UNSPECIFIED.,.F.,.F.,(4,2,4),(-0.0253041040308761,-0.0126521678473633,
0.),.UNSPECIFIED.);
#21616=B_SPLINE_CURVE_WITH_KNOTS('',3,(#101720,#101721,#101722,#101723,
#101724,#101725),.UNSPECIFIED.,.F.,.F.,(4,2,4),(-0.0253041039070892,-0.012652167715741,
0.),.UNSPECIFIED.);
#21617=B_SPLINE_CURVE_WITH_KNOTS('',3,(#101761,#101762,#101763,#101764,
#101765,#101766),.UNSPECIFIED.,.F.,.F.,(4,2,4),(-0.0253041038669996,-0.0126521677219567,
0.),.UNSPECIFIED.);
#21618=B_SPLINE_CURVE_WITH_KNOTS('',3,(#101802,#101803,#101804,#101805,
#101806,#101807),.UNSPECIFIED.,.F.,.F.,(4,2,4),(-0.0253041038574588,-0.0126521676654783,
0.),.UNSPECIFIED.);
#21619=B_SPLINE_CURVE_WITH_KNOTS('',3,(#101843,#101844,#101845,#101846,
#101847,#101848),.UNSPECIFIED.,.F.,.F.,(4,2,4),(-0.0253041039409774,-0.0126521677661099,
0.),.UNSPECIFIED.);
#21620=B_SPLINE_CURVE_WITH_KNOTS('',3,(#101884,#101885,#101886,#101887,
#101888,#101889),.UNSPECIFIED.,.F.,.F.,(4,2,4),(-0.0253041039068838,-0.0126521677169225,
0.),.UNSPECIFIED.);
#21621=B_SPLINE_CURVE_WITH_KNOTS('',3,(#101925,#101926,#101927,#101928,
#101929,#101930),.UNSPECIFIED.,.F.,.F.,(4,2,4),(-0.0253041039770956,-0.0126521677689033,
0.),.UNSPECIFIED.);
#21622=B_SPLINE_CURVE_WITH_KNOTS('',3,(#101963,#101964,#101965,#101966,
#101967,#101968),.UNSPECIFIED.,.F.,.F.,(4,2,4),(-0.0253041039055625,-0.0126521677474333,
0.),.UNSPECIFIED.);
#21623=B_SPLINE_CURVE_WITH_KNOTS('',3,(#101994,#101995,#101996,#101997,
#101998,#101999),.UNSPECIFIED.,.F.,.F.,(4,2,4),(-0.0253041039293055,-0.0126521677635233,
0.),.UNSPECIFIED.);
#21624=B_SPLINE_CURVE_WITH_KNOTS('',3,(#102035,#102036,#102037,#102038,
#102039,#102040),.UNSPECIFIED.,.F.,.F.,(4,2,4),(-0.0253041039232594,-0.0126521677538064,
0.),.UNSPECIFIED.);
#21625=B_SPLINE_CURVE_WITH_KNOTS('',3,(#102076,#102077,#102078,#102079,
#102080,#102081),.UNSPECIFIED.,.F.,.F.,(4,2,4),(-0.02530410389646,-0.0126521677360228,
0.),.UNSPECIFIED.);
#21626=B_SPLINE_CURVE_WITH_KNOTS('',3,(#102117,#102118,#102119,#102120,
#102121,#102122),.UNSPECIFIED.,.F.,.F.,(4,2,4),(-0.0253041039850785,-0.0126521678235967,
0.),.UNSPECIFIED.);
#21627=B_SPLINE_CURVE_WITH_KNOTS('',3,(#102158,#102159,#102160,#102161,
#102162,#102163),.UNSPECIFIED.,.F.,.F.,(4,2,4),(-0.0253041038917768,-0.0126521677471262,
0.),.UNSPECIFIED.);
#21628=B_SPLINE_CURVE_WITH_KNOTS('',3,(#102199,#102200,#102201,#102202,
#102203,#102204),.UNSPECIFIED.,.F.,.F.,(4,2,4),(-0.0253041039399128,-0.01265216776193,
0.),.UNSPECIFIED.);
#21629=B_SPLINE_CURVE_WITH_KNOTS('',3,(#102240,#102241,#102242,#102243,
#102244,#102245),.UNSPECIFIED.,.F.,.F.,(4,2,4),(-0.0253041038279282,-0.0126521676565885,
0.),.UNSPECIFIED.);
#21630=B_SPLINE_CURVE_WITH_KNOTS('',3,(#102275,#102276,#102277,#102278,
#102279,#102280),.UNSPECIFIED.,.F.,.F.,(4,2,4),(-0.0252994184233411,-0.0126495849026555,
0.),.UNSPECIFIED.);
#21631=B_SPLINE_CURVE_WITH_KNOTS('',3,(#102295,#102296,#102297,#102298,
#102299,#102300,#102301),.UNSPECIFIED.,.F.,.F.,(4,3,4),(0.349298845963836,
0.35897648262994,0.366749642030242),.UNSPECIFIED.);
#21632=B_SPLINE_CURVE_WITH_KNOTS('',3,(#102310,#102311,#102312,#102313,
#102314,#102315),.UNSPECIFIED.,.F.,.F.,(4,2,4),(-0.025299364436483,-0.0126495718869962,
0.),.UNSPECIFIED.);
#21633=B_SPLINE_CURVE_WITH_KNOTS('',3,(#102330,#102331,#102332,#102333,
#102334,#102335,#102336),.UNSPECIFIED.,.F.,.F.,(4,3,4),(0.349298845971303,
0.358976482629938,0.366749642018671),.UNSPECIFIED.);
#21634=B_SPLINE_CURVE_WITH_KNOTS('',3,(#102345,#102346,#102347,#102348,
#102349,#102350),.UNSPECIFIED.,.F.,.F.,(4,2,4),(-0.0252994181275643,-0.0126495848436817,
0.),.UNSPECIFIED.);
#21635=B_SPLINE_CURVE_WITH_KNOTS('',3,(#102365,#102366,#102367,#102368,
#102369,#102370,#102371),.UNSPECIFIED.,.F.,.F.,(4,3,4),(0.3492988459672,
0.358976482629936,0.366749642025355),.UNSPECIFIED.);
#21636=B_SPLINE_CURVE_WITH_KNOTS('',3,(#102380,#102381,#102382,#102383,
#102384,#102385),.UNSPECIFIED.,.F.,.F.,(4,2,4),(-0.0252994180828767,-0.0126495848091462,
0.),.UNSPECIFIED.);
#21637=B_SPLINE_CURVE_WITH_KNOTS('',3,(#102400,#102401,#102402,#102403,
#102404,#102405,#102406),.UNSPECIFIED.,.F.,.F.,(4,3,4),(0.34929884596835,
0.358976482629936,0.366749642036658),.UNSPECIFIED.);
#21638=B_SPLINE_CURVE_WITH_KNOTS('',3,(#102415,#102416,#102417,#102418,
#102419,#102420),.UNSPECIFIED.,.F.,.F.,(4,2,4),(-0.0252994182000983,-0.0126495848420178,
0.),.UNSPECIFIED.);
#21639=B_SPLINE_CURVE_WITH_KNOTS('',3,(#102435,#102436,#102437,#102438,
#102439,#102440,#102441),.UNSPECIFIED.,.F.,.F.,(4,3,4),(0.349298845930643,
0.358976482629938,0.366749642035256),.UNSPECIFIED.);
#21640=B_SPLINE_CURVE_WITH_KNOTS('',3,(#102450,#102451,#102452,#102453,
#102454,#102455),.UNSPECIFIED.,.F.,.F.,(4,2,4),(-0.0252994179754861,-0.0126495848168498,
0.),.UNSPECIFIED.);
#21641=B_SPLINE_CURVE_WITH_KNOTS('',3,(#102470,#102471,#102472,#102473,
#102474,#102475,#102476),.UNSPECIFIED.,.F.,.F.,(4,3,4),(0.349298845948969,
0.358976482629922,0.366749642024373),.UNSPECIFIED.);
#21642=B_SPLINE_CURVE_WITH_KNOTS('',3,(#102485,#102486,#102487,#102488,
#102489,#102490),.UNSPECIFIED.,.F.,.F.,(4,2,4),(-0.0252994179869716,-0.0126495848061804,
0.),.UNSPECIFIED.);
#21643=B_SPLINE_CURVE_WITH_KNOTS('',3,(#102505,#102506,#102507,#102508,
#102509,#102510,#102511),.UNSPECIFIED.,.F.,.F.,(4,3,4),(0.349298845956751,
0.358976482629922,0.366749642032673),.UNSPECIFIED.);
#21644=B_SPLINE_CURVE_WITH_KNOTS('',3,(#102520,#102521,#102522,#102523,
#102524,#102525),.UNSPECIFIED.,.F.,.F.,(4,2,4),(-0.0252994179954849,-0.0126495848078521,
0.),.UNSPECIFIED.);
#21645=B_SPLINE_CURVE_WITH_KNOTS('',3,(#102540,#102541,#102542,#102543,
#102544,#102545,#102546),.UNSPECIFIED.,.F.,.F.,(4,3,4),(0.349298845945899,
0.358976482629922,0.366749642023676),.UNSPECIFIED.);
#21646=B_SPLINE_CURVE_WITH_KNOTS('',3,(#102555,#102556,#102557,#102558,
#102559,#102560),.UNSPECIFIED.,.F.,.F.,(4,2,4),(-0.0252993639960928,-0.0126495717892771,
0.),.UNSPECIFIED.);
#21647=B_SPLINE_CURVE_WITH_KNOTS('',3,(#102575,#102576,#102577,#102578,
#102579,#102580,#102581),.UNSPECIFIED.,.F.,.F.,(4,3,4),(0.349298845963625,
0.358976482629922,0.36674964202969),.UNSPECIFIED.);
#21648=B_SPLINE_CURVE_WITH_KNOTS('',3,(#102590,#102591,#102592,#102593,
#102594,#102595),.UNSPECIFIED.,.F.,.F.,(4,2,4),(-0.0252994181967913,-0.0126495848488086,
0.),.UNSPECIFIED.);
#21649=B_SPLINE_CURVE_WITH_KNOTS('',3,(#102610,#102611,#102612,#102613,
#102614,#102615,#102616),.UNSPECIFIED.,.F.,.F.,(4,3,4),(0.349298845932533,
0.35897648262994,0.36674964202247),.UNSPECIFIED.);
#21650=B_SPLINE_CURVE_WITH_KNOTS('',3,(#102625,#102626,#102627,#102628,
#102629,#102630),.UNSPECIFIED.,.F.,.F.,(4,2,4),(-0.0252993643205837,-0.0126495718771281,
0.),.UNSPECIFIED.);
#21651=B_SPLINE_CURVE_WITH_KNOTS('',3,(#102645,#102646,#102647,#102648,
#102649,#102650,#102651),.UNSPECIFIED.,.F.,.F.,(4,3,4),(0.349298845921702,
0.35897648262994,0.366749642024241),.UNSPECIFIED.);
#21652=B_SPLINE_CURVE_WITH_KNOTS('',3,(#102660,#102661,#102662,#102663,
#102664,#102665),.UNSPECIFIED.,.F.,.F.,(4,2,4),(-0.0252993635718202,-0.0126495716991594,
0.),.UNSPECIFIED.);
#21653=B_SPLINE_CURVE_WITH_KNOTS('',3,(#102680,#102681,#102682,#102683,
#102684,#102685,#102686),.UNSPECIFIED.,.F.,.F.,(4,3,4),(0.349298845969534,
0.35897648262994,0.366749642035329),.UNSPECIFIED.);
#21654=B_SPLINE_CURVE_WITH_KNOTS('',3,(#102695,#102696,#102697,#102698,
#102699,#102700),.UNSPECIFIED.,.F.,.F.,(4,2,4),(-0.0252994179273683,-0.0126495847910784,
0.),.UNSPECIFIED.);
#21655=B_SPLINE_CURVE_WITH_KNOTS('',3,(#102715,#102716,#102717,#102718,
#102719,#102720,#102721),.UNSPECIFIED.,.F.,.F.,(4,3,4),(0.34929884595549,
0.35897648262994,0.366749642022583),.UNSPECIFIED.);
#21656=B_SPLINE_CURVE_WITH_KNOTS('',3,(#102730,#102731,#102732,#102733,
#102734,#102735),.UNSPECIFIED.,.F.,.F.,(4,2,4),(-0.0252993644889527,-0.0126495719101191,
0.),.UNSPECIFIED.);
#21657=B_SPLINE_CURVE_WITH_KNOTS('',3,(#102750,#102751,#102752,#102753,
#102754,#102755,#102756),.UNSPECIFIED.,.F.,.F.,(4,3,4),(0.349298845947852,
0.35897648262994,0.366749642016953),.UNSPECIFIED.);
#21658=B_SPLINE_CURVE_WITH_KNOTS('',3,(#102765,#102766,#102767,#102768,
#102769,#102770),.UNSPECIFIED.,.F.,.F.,(4,2,4),(-0.0252994181077383,-0.0126495848252762,
0.),.UNSPECIFIED.);
#21659=B_SPLINE_CURVE_WITH_KNOTS('',3,(#102785,#102786,#102787,#102788,
#102789,#102790,#102791),.UNSPECIFIED.,.F.,.F.,(4,3,4),(0.349298845953694,
0.35897648262994,0.366749642014227),.UNSPECIFIED.);
#21660=B_SPLINE_CURVE_WITH_KNOTS('',3,(#102800,#102801,#102802,#102803,
#102804,#102805),.UNSPECIFIED.,.F.,.F.,(4,2,4),(-0.0252994180307134,-0.0126495848285684,
0.),.UNSPECIFIED.);
#21661=B_SPLINE_CURVE_WITH_KNOTS('',3,(#102820,#102821,#102822,#102823,
#102824,#102825,#102826),.UNSPECIFIED.,.F.,.F.,(4,3,4),(0.349298845961314,
0.35897648262994,0.366749642024527),.UNSPECIFIED.);
#21662=B_SPLINE_CURVE_WITH_KNOTS('',3,(#102835,#102836,#102837,#102838,
#102839,#102840),.UNSPECIFIED.,.F.,.F.,(4,2,4),(-0.0252993640217252,-0.0126495718156864,
0.),.UNSPECIFIED.);
#21663=B_SPLINE_CURVE_WITH_KNOTS('',3,(#102855,#102856,#102857,#102858,
#102859,#102860,#102861),.UNSPECIFIED.,.F.,.F.,(4,3,4),(0.349298845962747,
0.35897648262994,0.366749642025728),.UNSPECIFIED.);
#21664=B_SPLINE_CURVE_WITH_KNOTS('',3,(#102870,#102871,#102872,#102873,
#102874,#102875),.UNSPECIFIED.,.F.,.F.,(4,2,4),(-0.0252993637637311,-0.0126495717496519,
0.),.UNSPECIFIED.);
#21665=B_SPLINE_CURVE_WITH_KNOTS('',3,(#102890,#102891,#102892,#102893,
#102894,#102895,#102896),.UNSPECIFIED.,.F.,.F.,(4,3,4),(0.34929884594429,
0.35897648262994,0.366749642019548),.UNSPECIFIED.);
#21666=B_SPLINE_CURVE_WITH_KNOTS('',3,(#102905,#102906,#102907,#102908,
#102909,#102910),.UNSPECIFIED.,.F.,.F.,(4,2,4),(-0.0252993637208719,-0.0126495717243885,
0.),.UNSPECIFIED.);
#21667=B_SPLINE_CURVE_WITH_KNOTS('',3,(#102925,#102926,#102927,#102928,
#102929,#102930,#102931),.UNSPECIFIED.,.F.,.F.,(4,3,4),(0.349298845943498,
0.35897648262994,0.366749642024082),.UNSPECIFIED.);
#21668=B_SPLINE_CURVE_WITH_KNOTS('',3,(#102940,#102941,#102942,#102943,
#102944,#102945),.UNSPECIFIED.,.F.,.F.,(4,2,4),(-0.0252994182535981,-0.0126495848574988,
0.),.UNSPECIFIED.);
#21669=B_SPLINE_CURVE_WITH_KNOTS('',3,(#102960,#102961,#102962,#102963,
#102964,#102965,#102966),.UNSPECIFIED.,.F.,.F.,(4,3,4),(0.349298845939575,
0.35897648262994,0.366749642029799),.UNSPECIFIED.);
#21670=B_SPLINE_CURVE_WITH_KNOTS('',3,(#102975,#102976,#102977,#102978,
#102979,#102980),.UNSPECIFIED.,.F.,.F.,(4,2,4),(-0.0252994180810671,-0.0126495848269979,
0.),.UNSPECIFIED.);
#21671=B_SPLINE_CURVE_WITH_KNOTS('',3,(#102995,#102996,#102997,#102998,
#102999,#103000,#103001),.UNSPECIFIED.,.F.,.F.,(4,3,4),(0.349298845945691,
0.35897648262994,0.366749642035111),.UNSPECIFIED.);
#21672=B_SPLINE_CURVE_WITH_KNOTS('',3,(#103010,#103011,#103012,#103013,
#103014,#103015),.UNSPECIFIED.,.F.,.F.,(4,2,4),(-0.0252994181543156,-0.012649584865264,
0.),.UNSPECIFIED.);
#21673=B_SPLINE_CURVE_WITH_KNOTS('',3,(#103030,#103031,#103032,#103033,
#103034,#103035,#103036),.UNSPECIFIED.,.F.,.F.,(4,3,4),(0.349298845951285,
0.35897648262994,0.366749642035188),.UNSPECIFIED.);
#21674=B_SPLINE_CURVE_WITH_KNOTS('',3,(#103045,#103046,#103047,#103048,
#103049,#103050),.UNSPECIFIED.,.F.,.F.,(4,2,4),(-0.0252994183497646,-0.0126495848853004,
0.),.UNSPECIFIED.);
#21675=B_SPLINE_CURVE_WITH_KNOTS('',3,(#103065,#103066,#103067,#103068,
#103069,#103070,#103071),.UNSPECIFIED.,.F.,.F.,(4,3,4),(0.349298845943866,
0.35897648262994,0.366749642036405),.UNSPECIFIED.);
#21676=B_SPLINE_CURVE_WITH_KNOTS('',3,(#103080,#103081,#103082,#103083,
#103084,#103085),.UNSPECIFIED.,.F.,.F.,(4,2,4),(-0.0252993644655463,-0.0126495719273563,
0.),.UNSPECIFIED.);
#21677=B_SPLINE_CURVE_WITH_KNOTS('',3,(#103100,#103101,#103102,#103103,
#103104,#103105,#103106),.UNSPECIFIED.,.F.,.F.,(4,3,4),(0.349298845958209,
0.35897648262994,0.366749642025503),.UNSPECIFIED.);
#21678=B_SPLINE_CURVE_WITH_KNOTS('',3,(#103115,#103116,#103117,#103118,
#103119,#103120),.UNSPECIFIED.,.F.,.F.,(4,2,4),(-0.0252993642339217,-0.0126495718654069,
0.),.UNSPECIFIED.);
#21679=B_SPLINE_CURVE_WITH_KNOTS('',3,(#103135,#103136,#103137,#103138,
#103139,#103140,#103141),.UNSPECIFIED.,.F.,.F.,(4,3,4),(0.34929884594229,
0.358976482629936,0.366749642031194),.UNSPECIFIED.);
#21680=B_SPLINE_CURVE_WITH_KNOTS('',3,(#103150,#103151,#103152,#103153,
#103154,#103155),.UNSPECIFIED.,.F.,.F.,(4,2,4),(-0.0252993643902813,-0.0126495719066374,
0.),.UNSPECIFIED.);
#21681=B_SPLINE_CURVE_WITH_KNOTS('',3,(#103170,#103171,#103172,#103173,
#103174,#103175,#103176),.UNSPECIFIED.,.F.,.F.,(4,3,4),(0.349298845965109,
0.358976482629922,0.366749642028045),.UNSPECIFIED.);
#21682=B_SPLINE_CURVE_WITH_KNOTS('',3,(#103185,#103186,#103187,#103188,
#103189,#103190),.UNSPECIFIED.,.F.,.F.,(4,2,4),(-0.0252993639302304,-0.0126495717682941,
0.),.UNSPECIFIED.);
#21683=B_SPLINE_CURVE_WITH_KNOTS('',3,(#103205,#103206,#103207,#103208,
#103209,#103210,#103211),.UNSPECIFIED.,.F.,.F.,(4,3,4),(0.349298845937363,
0.35897648262994,0.366749642034294),.UNSPECIFIED.);
#21684=B_SPLINE_CURVE_WITH_KNOTS('',3,(#103220,#103221,#103222,#103223,
#103224,#103225),.UNSPECIFIED.,.F.,.F.,(4,2,4),(-0.0252993641752915,-0.0126495718180406,
0.),.UNSPECIFIED.);
#21685=B_SPLINE_CURVE_WITH_KNOTS('',3,(#103240,#103241,#103242,#103243,
#103244,#103245,#103246),.UNSPECIFIED.,.F.,.F.,(4,3,4),(0.349298845962219,
0.35897648262994,0.366749642022716),.UNSPECIFIED.);
#21686=B_SPLINE_CURVE_WITH_KNOTS('',3,(#103255,#103256,#103257,#103258,
#103259,#103260),.UNSPECIFIED.,.F.,.F.,(4,2,4),(-0.0252994180664517,-0.0126495848125946,
0.),.UNSPECIFIED.);
#21687=B_SPLINE_CURVE_WITH_KNOTS('',3,(#103275,#103276,#103277,#103278,
#103279,#103280,#103281),.UNSPECIFIED.,.F.,.F.,(4,3,4),(0.349298845879221,
0.358976482629941,0.36674964202409),.UNSPECIFIED.);
#21688=B_SPLINE_CURVE_WITH_KNOTS('',3,(#103290,#103291,#103292,#103293,
#103294,#103295),.UNSPECIFIED.,.F.,.F.,(4,2,4),(-0.025296958792191,-0.012648355834516,
0.),.UNSPECIFIED.);
#21689=B_SPLINE_CURVE_WITH_KNOTS('',3,(#103306,#103307,#103308,#103309,
#103310,#103311,#103312),.UNSPECIFIED.,.F.,.F.,(4,3,4),(0.418312080788897,
0.428571428571429,0.435775021767613),.UNSPECIFIED.);
#21690=B_SPLINE_CURVE_WITH_KNOTS('',3,(#103321,#103322,#103323,#103324,
#103325,#103326),.UNSPECIFIED.,.F.,.F.,(4,2,4),(-0.0252969554483052,-0.0126483549025546,
0.),.UNSPECIFIED.);
#21691=B_SPLINE_CURVE_WITH_KNOTS('',3,(#103337,#103338,#103339,#103340,
#103341,#103342,#103343),.UNSPECIFIED.,.F.,.F.,(4,3,4),(0.418312080810239,
0.428571428568827,0.435775021479951),.UNSPECIFIED.);
#21692=B_SPLINE_CURVE_WITH_KNOTS('',3,(#103352,#103353,#103354,#103355,
#103356,#103357),.UNSPECIFIED.,.F.,.F.,(4,2,4),(-0.025297157865339,-0.0126484038625859,
0.),.UNSPECIFIED.);
#21693=B_SPLINE_CURVE_WITH_KNOTS('',3,(#103368,#103369,#103370,#103371,
#103372,#103373,#103374),.UNSPECIFIED.,.F.,.F.,(4,3,4),(0.41831208080354,
0.428571428571429,0.4357750217547),.UNSPECIFIED.);
#21694=B_SPLINE_CURVE_WITH_KNOTS('',3,(#103383,#103384,#103385,#103386,
#103387,#103388),.UNSPECIFIED.,.F.,.F.,(4,2,4),(-0.0252969589615879,-0.0126483559234329,
0.),.UNSPECIFIED.);
#21695=B_SPLINE_CURVE_WITH_KNOTS('',3,(#103399,#103400,#103401,#103402,
#103403,#103404,#103405),.UNSPECIFIED.,.F.,.F.,(4,3,4),(0.418312080798011,
0.428571428571429,0.435775021762071),.UNSPECIFIED.);
#21696=B_SPLINE_CURVE_WITH_KNOTS('',3,(#103414,#103415,#103416,#103417,
#103418,#103419),.UNSPECIFIED.,.F.,.F.,(4,2,4),(-0.0252969587987205,-0.0126483557936413,
0.),.UNSPECIFIED.);
#21697=B_SPLINE_CURVE_WITH_KNOTS('',3,(#103430,#103431,#103432,#103433,
#103434,#103435,#103436),.UNSPECIFIED.,.F.,.F.,(4,3,4),(0.418312080798033,
0.428571428571429,0.43577502176659),.UNSPECIFIED.);
#21698=B_SPLINE_CURVE_WITH_KNOTS('',3,(#103445,#103446,#103447,#103448,
#103449,#103450),.UNSPECIFIED.,.F.,.F.,(4,2,4),(-0.0252969587895803,-0.0126483557947713,
0.),.UNSPECIFIED.);
#21699=B_SPLINE_CURVE_WITH_KNOTS('',3,(#103461,#103462,#103463,#103464,
#103465,#103466,#103467),.UNSPECIFIED.,.F.,.F.,(4,3,4),(0.418312080811542,
0.428571428571429,0.435775021766799),.UNSPECIFIED.);
#21700=B_SPLINE_CURVE_WITH_KNOTS('',3,(#103476,#103477,#103478,#103479,
#103480,#103481),.UNSPECIFIED.,.F.,.F.,(4,2,4),(-0.0252969588307827,-0.0126483558513836,
0.),.UNSPECIFIED.);
#21701=B_SPLINE_CURVE_WITH_KNOTS('',3,(#103492,#103493,#103494,#103495,
#103496,#103497,#103498),.UNSPECIFIED.,.F.,.F.,(4,3,4),(0.418312080793796,
0.428571428571429,0.435775021765992),.UNSPECIFIED.);
#21702=B_SPLINE_CURVE_WITH_KNOTS('',3,(#103507,#103508,#103509,#103510,
#103511,#103512),.UNSPECIFIED.,.F.,.F.,(4,2,4),(-0.0252969588840719,-0.0126483558613075,
0.),.UNSPECIFIED.);
#21703=B_SPLINE_CURVE_WITH_KNOTS('',3,(#103523,#103524,#103525,#103526,
#103527,#103528,#103529),.UNSPECIFIED.,.F.,.F.,(4,3,4),(0.418312080801105,
0.428571428571429,0.43577502176165),.UNSPECIFIED.);
#21704=B_SPLINE_CURVE_WITH_KNOTS('',3,(#103538,#103539,#103540,#103541,
#103542,#103543),.UNSPECIFIED.,.F.,.F.,(4,2,4),(-0.0252969587965309,-0.0126483558081197,
0.),.UNSPECIFIED.);
#21705=B_SPLINE_CURVE_WITH_KNOTS('',3,(#103554,#103555,#103556,#103557,
#103558,#103559,#103560),.UNSPECIFIED.,.F.,.F.,(4,3,4),(0.41831208081577,
0.428571428571429,0.435775021758859),.UNSPECIFIED.);
#21706=B_SPLINE_CURVE_WITH_KNOTS('',3,(#103569,#103570,#103571,#103572,
#103573,#103574),.UNSPECIFIED.,.F.,.F.,(4,2,4),(-0.0252969587879319,-0.0126483558043734,
0.),.UNSPECIFIED.);
#21707=B_SPLINE_CURVE_WITH_KNOTS('',3,(#103585,#103586,#103587,#103588,
#103589,#103590,#103591),.UNSPECIFIED.,.F.,.F.,(4,3,4),(0.418312080803554,
0.428571428571429,0.435775021758034),.UNSPECIFIED.);
#21708=B_SPLINE_CURVE_WITH_KNOTS('',3,(#103600,#103601,#103602,#103603,
#103604,#103605),.UNSPECIFIED.,.F.,.F.,(4,2,4),(-0.0252969588289607,-0.0126483558674192,
0.),.UNSPECIFIED.);
#21709=B_SPLINE_CURVE_WITH_KNOTS('',3,(#103616,#103617,#103618,#103619,
#103620,#103621,#103622),.UNSPECIFIED.,.F.,.F.,(4,3,4),(0.41831208080598,
0.428571428571429,0.435775021762065),.UNSPECIFIED.);
#21710=B_SPLINE_CURVE_WITH_KNOTS('',3,(#103631,#103632,#103633,#103634,
#103635,#103636),.UNSPECIFIED.,.F.,.F.,(4,2,4),(-0.0252969588379448,-0.0126483558443588,
0.),.UNSPECIFIED.);
#21711=B_SPLINE_CURVE_WITH_KNOTS('',3,(#103647,#103648,#103649,#103650,
#103651,#103652,#103653),.UNSPECIFIED.,.F.,.F.,(4,3,4),(0.418312080802205,
0.428571428571429,0.435775021765829),.UNSPECIFIED.);
#21712=B_SPLINE_CURVE_WITH_KNOTS('',3,(#103662,#103663,#103664,#103665,
#103666,#103667),.UNSPECIFIED.,.F.,.F.,(4,2,4),(-0.0252969588740578,-0.0126483558687873,
0.),.UNSPECIFIED.);
#21713=B_SPLINE_CURVE_WITH_KNOTS('',3,(#103678,#103679,#103680,#103681,
#103682,#103683,#103684),.UNSPECIFIED.,.F.,.F.,(4,3,4),(0.41831208081761,
0.428571428571429,0.435775021762013),.UNSPECIFIED.);
#21714=B_SPLINE_CURVE_WITH_KNOTS('',3,(#103693,#103694,#103695,#103696,
#103697,#103698),.UNSPECIFIED.,.F.,.F.,(4,2,4),(-0.0252969588665305,-0.0126483558558781,
0.),.UNSPECIFIED.);
#21715=B_SPLINE_CURVE_WITH_KNOTS('',3,(#103709,#103710,#103711,#103712,
#103713,#103714,#103715),.UNSPECIFIED.,.F.,.F.,(4,3,4),(0.418312080799316,
0.428571428571429,0.435775021764603),.UNSPECIFIED.);
#21716=B_SPLINE_CURVE_WITH_KNOTS('',3,(#103724,#103725,#103726,#103727,
#103728,#103729),.UNSPECIFIED.,.F.,.F.,(4,2,4),(-0.0252969588070961,-0.0126483558109704,
0.),.UNSPECIFIED.);
#21717=B_SPLINE_CURVE_WITH_KNOTS('',3,(#103740,#103741,#103742,#103743,
#103744,#103745,#103746),.UNSPECIFIED.,.F.,.F.,(4,3,4),(0.418312080790721,
0.428571428571429,0.435775021760828),.UNSPECIFIED.);
#21718=B_SPLINE_CURVE_WITH_KNOTS('',3,(#103755,#103756,#103757,#103758,
#103759,#103760),.UNSPECIFIED.,.F.,.F.,(4,2,4),(-0.0252969587698119,-0.0126483558105197,
0.),.UNSPECIFIED.);
#21719=B_SPLINE_CURVE_WITH_KNOTS('',3,(#103771,#103772,#103773,#103774,
#103775,#103776,#103777),.UNSPECIFIED.,.F.,.F.,(4,3,4),(0.418312080813446,
0.428571428571429,0.43577502176075),.UNSPECIFIED.);
#21720=B_SPLINE_CURVE_WITH_KNOTS('',3,(#103786,#103787,#103788,#103789,
#103790,#103791),.UNSPECIFIED.,.F.,.F.,(4,2,4),(-0.0252969588634707,-0.0126483558476927,
0.),.UNSPECIFIED.);
#21721=B_SPLINE_CURVE_WITH_KNOTS('',3,(#103802,#103803,#103804,#103805,
#103806,#103807,#103808),.UNSPECIFIED.,.F.,.F.,(4,3,4),(0.418312080804051,
0.428571428571429,0.435775021758984),.UNSPECIFIED.);
#21722=B_SPLINE_CURVE_WITH_KNOTS('',3,(#103817,#103818,#103819,#103820,
#103821,#103822),.UNSPECIFIED.,.F.,.F.,(4,2,4),(-0.0252969588415939,-0.0126483558254068,
0.),.UNSPECIFIED.);
#21723=B_SPLINE_CURVE_WITH_KNOTS('',3,(#103833,#103834,#103835,#103836,
#103837,#103838,#103839),.UNSPECIFIED.,.F.,.F.,(4,3,4),(0.418312080799403,
0.428571428571429,0.435775021765068),.UNSPECIFIED.);
#21724=B_SPLINE_CURVE_WITH_KNOTS('',3,(#103848,#103849,#103850,#103851,
#103852,#103853),.UNSPECIFIED.,.F.,.F.,(4,2,4),(-0.0252969588213482,-0.012648355813714,
0.),.UNSPECIFIED.);
#21725=B_SPLINE_CURVE_WITH_KNOTS('',3,(#103864,#103865,#103866,#103867,
#103868,#103869,#103870),.UNSPECIFIED.,.F.,.F.,(4,3,4),(0.418312080807609,
0.428571428571429,0.435775021753525),.UNSPECIFIED.);
#21726=B_SPLINE_CURVE_WITH_KNOTS('',3,(#103879,#103880,#103881,#103882,
#103883,#103884),.UNSPECIFIED.,.F.,.F.,(4,2,4),(-0.0252969587836844,-0.0126483558118128,
0.),.UNSPECIFIED.);
#21727=B_SPLINE_CURVE_WITH_KNOTS('',3,(#103895,#103896,#103897,#103898,
#103899,#103900,#103901),.UNSPECIFIED.,.F.,.F.,(4,3,4),(0.418312080808486,
0.428571428571429,0.435775021760694),.UNSPECIFIED.);
#21728=B_SPLINE_CURVE_WITH_KNOTS('',3,(#103910,#103911,#103912,#103913,
#103914,#103915),.UNSPECIFIED.,.F.,.F.,(4,2,4),(-0.025296958843695,-0.0126483558867024,
0.),.UNSPECIFIED.);
#21729=B_SPLINE_CURVE_WITH_KNOTS('',3,(#103926,#103927,#103928,#103929,
#103930,#103931,#103932),.UNSPECIFIED.,.F.,.F.,(4,3,4),(0.418312080808666,
0.428571428571429,0.435775021775203),.UNSPECIFIED.);
#21730=B_SPLINE_CURVE_WITH_KNOTS('',3,(#103941,#103942,#103943,#103944,
#103945,#103946),.UNSPECIFIED.,.F.,.F.,(4,2,4),(-0.0252969589066171,-0.0126483559109774,
0.),.UNSPECIFIED.);
#21731=B_SPLINE_CURVE_WITH_KNOTS('',3,(#103957,#103958,#103959,#103960,
#103961,#103962,#103963),.UNSPECIFIED.,.F.,.F.,(4,3,4),(0.418312080805564,
0.428571428571429,0.435775021766875),.UNSPECIFIED.);
#21732=B_SPLINE_CURVE_WITH_KNOTS('',3,(#103972,#103973,#103974,#103975,
#103976,#103977),.UNSPECIFIED.,.F.,.F.,(4,2,4),(-0.025296958834738,-0.0126483558248854,
0.),.UNSPECIFIED.);
#21733=B_SPLINE_CURVE_WITH_KNOTS('',3,(#103988,#103989,#103990,#103991,
#103992,#103993,#103994),.UNSPECIFIED.,.F.,.F.,(4,3,4),(0.418312080801487,
0.428571428571429,0.435775021756058),.UNSPECIFIED.);
#21734=B_SPLINE_CURVE_WITH_KNOTS('',3,(#104003,#104004,#104005,#104006,
#104007,#104008),.UNSPECIFIED.,.F.,.F.,(4,2,4),(-0.0252969588750053,-0.0126483558821439,
0.),.UNSPECIFIED.);
#21735=B_SPLINE_CURVE_WITH_KNOTS('',3,(#104019,#104020,#104021,#104022,
#104023,#104024,#104025),.UNSPECIFIED.,.F.,.F.,(4,3,4),(0.418312080794997,
0.428571428571429,0.435775021752916),.UNSPECIFIED.);
#21736=B_SPLINE_CURVE_WITH_KNOTS('',3,(#104034,#104035,#104036,#104037,
#104038,#104039),.UNSPECIFIED.,.F.,.F.,(4,2,4),(-0.0252969588282311,-0.0126483558783853,
0.),.UNSPECIFIED.);
#21737=B_SPLINE_CURVE_WITH_KNOTS('',3,(#104050,#104051,#104052,#104053,
#104054,#104055,#104056),.UNSPECIFIED.,.F.,.F.,(4,3,4),(0.418312080810649,
0.428571428571429,0.435775021752433),.UNSPECIFIED.);
#21738=B_SPLINE_CURVE_WITH_KNOTS('',3,(#104065,#104066,#104067,#104068,
#104069,#104070),.UNSPECIFIED.,.F.,.F.,(4,2,4),(-0.0252969588845412,-0.0126483558846912,
0.),.UNSPECIFIED.);
#21739=B_SPLINE_CURVE_WITH_KNOTS('',3,(#104081,#104082,#104083,#104084,
#104085,#104086,#104087),.UNSPECIFIED.,.F.,.F.,(4,3,4),(0.418312080811903,
0.428571428571429,0.435775021768874),.UNSPECIFIED.);
#21740=B_SPLINE_CURVE_WITH_KNOTS('',3,(#104096,#104097,#104098,#104099,
#104100,#104101),.UNSPECIFIED.,.F.,.F.,(4,2,4),(-0.0252963500157696,-0.0126482087099505,
0.),.UNSPECIFIED.);
#21741=B_SPLINE_CURVE_WITH_KNOTS('',3,(#104112,#104113,#104114,#104115,
#104116,#104117,#104118),.UNSPECIFIED.,.F.,.F.,(4,3,4),(0.418312080811404,
0.428571428568158,0.435775021492859),.UNSPECIFIED.);
#21742=B_SPLINE_CURVE_WITH_KNOTS('',3,(#104127,#104128,#104129,#104130,
#104131,#104132),.UNSPECIFIED.,.F.,.F.,(4,2,4),(-0.0252969588787896,-0.0126483558460195,
0.),.UNSPECIFIED.);
#21743=B_SPLINE_CURVE_WITH_KNOTS('',3,(#104143,#104144,#104145,#104146,
#104147,#104148,#104149),.UNSPECIFIED.,.F.,.F.,(4,3,4),(0.418312080803512,
0.428571428571429,0.435775021758132),.UNSPECIFIED.);
#21744=B_SPLINE_CURVE_WITH_KNOTS('',3,(#104158,#104159,#104160,#104161,
#104162,#104163),.UNSPECIFIED.,.F.,.F.,(4,2,4),(-0.0252969588807337,-0.01264835587897,
0.),.UNSPECIFIED.);
#21745=B_SPLINE_CURVE_WITH_KNOTS('',3,(#104174,#104175,#104176,#104177,
#104178,#104179,#104180),.UNSPECIFIED.,.F.,.F.,(4,3,4),(0.41831208078803,
0.428571428571429,0.435775021765591),.UNSPECIFIED.);
#21746=B_SPLINE_CURVE_WITH_KNOTS('',3,(#104191,#104192,#104193,#104194,
#104195,#104196),.UNSPECIFIED.,.F.,.F.,(4,2,4),(-0.0252969686694848,-0.0126483614906356,
-6.97684167383361E-11),.UNSPECIFIED.);
#21747=B_SPLINE_CURVE_WITH_KNOTS('',3,(#104213,#104214,#104215,#104216,
#104217,#104218,#104219),.UNSPECIFIED.,.F.,.F.,(4,3,4),(0.34936969607449,
0.357142857142857,0.361565077308306),.UNSPECIFIED.);
#21748=B_SPLINE_CURVE_WITH_KNOTS('',3,(#104220,#104221,#104222,#104223,
#104224,#104225),.UNSPECIFIED.,.F.,.F.,(4,2,4),(7.00580731665936E-10,0.012648362193168,
0.0252968604256022),.UNSPECIFIED.);
#21749=B_SPLINE_CURVE_WITH_KNOTS('',3,(#104256,#104257,#104258,#104259,
#104260,#104261,#104262),.UNSPECIFIED.,.F.,.F.,(4,3,4),(0.349369696074507,
0.357142857142857,0.361565077306898),.UNSPECIFIED.);
#21750=B_SPLINE_CURVE_WITH_KNOTS('',3,(#104263,#104264,#104265,#104266,
#104267,#104268),.UNSPECIFIED.,.F.,.F.,(4,2,4),(7.69823548708584E-10,0.0126483622614854,
0.0252968526961796),.UNSPECIFIED.);
#21751=B_SPLINE_CURVE_WITH_KNOTS('',3,(#104299,#104300,#104301,#104302,
#104303,#104304,#104305),.UNSPECIFIED.,.F.,.F.,(4,3,4),(0.349369696074506,
0.357142857142857,0.361565077301677),.UNSPECIFIED.);
#21752=B_SPLINE_CURVE_WITH_KNOTS('',3,(#104306,#104307,#104308,#104309,
#104310,#104311),.UNSPECIFIED.,.F.,.F.,(4,2,4),(7.50211286994472E-10,0.0126483622730504,
0.0252968521458539),.UNSPECIFIED.);
#21753=B_SPLINE_CURVE_WITH_KNOTS('',3,(#104342,#104343,#104344,#104345,
#104346,#104347,#104348),.UNSPECIFIED.,.F.,.F.,(4,3,4),(0.349369696074504,
0.357142857142857,0.361565077307123),.UNSPECIFIED.);
#21754=B_SPLINE_CURVE_WITH_KNOTS('',3,(#104349,#104350,#104351,#104352,
#104353,#104354),.UNSPECIFIED.,.F.,.F.,(4,2,4),(7.32488769304241E-10,0.0126483622343914,
0.0252969687268146),.UNSPECIFIED.);
#21755=B_SPLINE_CURVE_WITH_KNOTS('',3,(#104385,#104386,#104387,#104388,
#104389,#104390,#104391),.UNSPECIFIED.,.F.,.F.,(4,3,4),(0.349369696074505,
0.357142857142857,0.361565077309921),.UNSPECIFIED.);
#21756=B_SPLINE_CURVE_WITH_KNOTS('',3,(#104392,#104393,#104394,#104395,
#104396,#104397),.UNSPECIFIED.,.F.,.F.,(4,2,4),(8.14431072066256E-10,0.0126483623470854,
0.0252968548170038),.UNSPECIFIED.);
#21757=B_SPLINE_CURVE_WITH_KNOTS('',3,(#104428,#104429,#104430,#104431,
#104432,#104433,#104434),.UNSPECIFIED.,.F.,.F.,(4,3,4),(0.349369696074496,
0.357142857142857,0.361565077307065),.UNSPECIFIED.);
#21758=B_SPLINE_CURVE_WITH_KNOTS('',3,(#104435,#104436,#104437,#104438,
#104439,#104440),.UNSPECIFIED.,.F.,.F.,(4,2,4),(7.81136850193204E-10,0.0126483622731924,
0.0252969686706485),.UNSPECIFIED.);
#21759=B_SPLINE_CURVE_WITH_KNOTS('',3,(#104469,#104470,#104471,#104472,
#104473,#104474),.UNSPECIFIED.,.F.,.F.,(4,2,4),(8.10397729245745E-10,0.0126483623554498,
0.025296856312765),.UNSPECIFIED.);
#21760=B_SPLINE_CURVE_WITH_KNOTS('',3,(#104499,#104500,#104501,#104502,
#104503,#104504,#104505),.UNSPECIFIED.,.F.,.F.,(4,3,4),(0.349369696074502,
0.357142857142857,0.361565077308727),.UNSPECIFIED.);
#21761=B_SPLINE_CURVE_WITH_KNOTS('',3,(#104506,#104507,#104508,#104509,
#104510,#104511),.UNSPECIFIED.,.F.,.F.,(4,2,4),(8.04641163913392E-10,0.0126483623562947,
0.0252968547386476),.UNSPECIFIED.);
#21762=B_SPLINE_CURVE_WITH_KNOTS('',3,(#104542,#104543,#104544,#104545,
#104546,#104547,#104548),.UNSPECIFIED.,.F.,.F.,(4,3,4),(0.349369696074505,
0.357142857142857,0.361565077309479),.UNSPECIFIED.);
#21763=B_SPLINE_CURVE_WITH_KNOTS('',3,(#104549,#104550,#104551,#104552,
#104553,#104554),.UNSPECIFIED.,.F.,.F.,(4,2,4),(7.62322842763532E-10,0.0126483622669495,
0.0252968591342625),.UNSPECIFIED.);
#21764=B_SPLINE_CURVE_WITH_KNOTS('',3,(#104585,#104586,#104587,#104588,
#104589,#104590,#104591),.UNSPECIFIED.,.F.,.F.,(4,3,4),(0.349369696074486,
0.357142857142857,0.361565077304992),.UNSPECIFIED.);
#21765=B_SPLINE_CURVE_WITH_KNOTS('',3,(#104592,#104593,#104594,#104595,
#104596,#104597),.UNSPECIFIED.,.F.,.F.,(4,2,4),(8.65804712474563E-10,0.0126483624251677,
0.0252968581181851),.UNSPECIFIED.);
#21766=B_SPLINE_CURVE_WITH_KNOTS('',3,(#104628,#104629,#104630,#104631,
#104632,#104633,#104634),.UNSPECIFIED.,.F.,.F.,(4,3,4),(0.349369696074485,
0.357142857142857,0.361565077306903),.UNSPECIFIED.);
#21767=B_SPLINE_CURVE_WITH_KNOTS('',3,(#104635,#104636,#104637,#104638,
#104639,#104640),.UNSPECIFIED.,.F.,.F.,(4,2,4),(8.39204876451129E-10,0.0126483623445493,
0.0252969686854641),.UNSPECIFIED.);
#21768=B_SPLINE_CURVE_WITH_KNOTS('',3,(#104671,#104672,#104673,#104674,
#104675,#104676,#104677),.UNSPECIFIED.,.F.,.F.,(4,3,4),(0.349369696074483,
0.357142857142857,0.361565077308867),.UNSPECIFIED.);
#21769=B_SPLINE_CURVE_WITH_KNOTS('',3,(#104678,#104679,#104680,#104681,
#104682,#104683),.UNSPECIFIED.,.F.,.F.,(4,2,4),(6.69232072890605E-10,0.0126483621759807,
0.0252968521824175),.UNSPECIFIED.);
#21770=B_SPLINE_CURVE_WITH_KNOTS('',3,(#104714,#104715,#104716,#104717,
#104718,#104719,#104720),.UNSPECIFIED.,.F.,.F.,(4,3,4),(0.349369696074482,
0.357142857142857,0.361565077309969),.UNSPECIFIED.);
#21771=B_SPLINE_CURVE_WITH_KNOTS('',3,(#104721,#104722,#104723,#104724,
#104725,#104726),.UNSPECIFIED.,.F.,.F.,(4,2,4),(8.06443979909319E-10,0.0126483623181598,
0.0252968594199354),.UNSPECIFIED.);
#21772=B_SPLINE_CURVE_WITH_KNOTS('',3,(#104757,#104758,#104759,#104760,
#104761,#104762,#104763),.UNSPECIFIED.,.F.,.F.,(4,3,4),(0.349369696074483,
0.357142857142857,0.361565077303164),.UNSPECIFIED.);
#21773=B_SPLINE_CURVE_WITH_KNOTS('',3,(#104764,#104765,#104766,#104767,
#104768,#104769),.UNSPECIFIED.,.F.,.F.,(4,2,4),(7.81820570877324E-10,0.012648362295298,
0.0252968584739717),.UNSPECIFIED.);
#21774=B_SPLINE_CURVE_WITH_KNOTS('',3,(#104800,#104801,#104802,#104803,
#104804,#104805,#104806),.UNSPECIFIED.,.F.,.F.,(4,3,4),(0.349369696074483,
0.357142857142857,0.361565077304905),.UNSPECIFIED.);
#21775=B_SPLINE_CURVE_WITH_KNOTS('',3,(#104807,#104808,#104809,#104810,
#104811,#104812),.UNSPECIFIED.,.F.,.F.,(4,2,4),(7.71314115196913E-10,0.0126483622892186,
0.0252968544306222),.UNSPECIFIED.);
#21776=B_SPLINE_CURVE_WITH_KNOTS('',3,(#104843,#104844,#104845,#104846,
#104847,#104848,#104849),.UNSPECIFIED.,.F.,.F.,(4,3,4),(0.349369696074483,
0.357142857142857,0.361565077306421),.UNSPECIFIED.);
#21777=B_SPLINE_CURVE_WITH_KNOTS('',3,(#104850,#104851,#104852,#104853,
#104854,#104855),.UNSPECIFIED.,.F.,.F.,(4,2,4),(7.63409067584006E-10,0.0126483622648431,
0.0252969687459862),.UNSPECIFIED.);
#21778=B_SPLINE_CURVE_WITH_KNOTS('',3,(#104886,#104887,#104888,#104889,
#104890,#104891,#104892),.UNSPECIFIED.,.F.,.F.,(4,3,4),(0.349369696074485,
0.357142857142857,0.361565077307845),.UNSPECIFIED.);
#21779=B_SPLINE_CURVE_WITH_KNOTS('',3,(#104893,#104894,#104895,#104896,
#104897,#104898),.UNSPECIFIED.,.F.,.F.,(4,2,4),(7.41711010567428E-10,0.0126483622632217,
0.0252969687427512),.UNSPECIFIED.);
#21780=B_SPLINE_CURVE_WITH_KNOTS('',3,(#104929,#104930,#104931,#104932,
#104933,#104934,#104935),.UNSPECIFIED.,.F.,.F.,(4,3,4),(0.349369696074508,
0.357142857142857,0.361565077311298),.UNSPECIFIED.);
#21781=B_SPLINE_CURVE_WITH_KNOTS('',3,(#104936,#104937,#104938,#104939,
#104940,#104941),.UNSPECIFIED.,.F.,.F.,(4,2,4),(8.26445337013183E-10,0.0126483623626397,
0.02529685160036),.UNSPECIFIED.);
#21782=B_SPLINE_CURVE_WITH_KNOTS('',3,(#104972,#104973,#104974,#104975,
#104976,#104977,#104978),.UNSPECIFIED.,.F.,.F.,(4,3,4),(0.349369696074486,
0.357142857142857,0.36156507730966),.UNSPECIFIED.);
#21783=B_SPLINE_CURVE_WITH_KNOTS('',3,(#104979,#104980,#104981,#104982,
#104983,#104984),.UNSPECIFIED.,.F.,.F.,(4,2,4),(7.94101837835612E-10,0.0126483622803908,
0.025296968651002),.UNSPECIFIED.);
#21784=B_SPLINE_CURVE_WITH_KNOTS('',3,(#105015,#105016,#105017,#105018,
#105019,#105020,#105021),.UNSPECIFIED.,.F.,.F.,(4,3,4),(0.349369696074483,
0.357142857142857,0.361565077307964),.UNSPECIFIED.);
#21785=B_SPLINE_CURVE_WITH_KNOTS('',3,(#105022,#105023,#105024,#105025,
#105026,#105027),.UNSPECIFIED.,.F.,.F.,(4,2,4),(8.07063340628222E-10,0.012648362327054,
0.0252968589528559),.UNSPECIFIED.);
#21786=B_SPLINE_CURVE_WITH_KNOTS('',3,(#105058,#105059,#105060,#105061,
#105062,#105063,#105064),.UNSPECIFIED.,.F.,.F.,(4,3,4),(0.349369696074483,
0.357142857142857,0.361565077309104),.UNSPECIFIED.);
#21787=B_SPLINE_CURVE_WITH_KNOTS('',3,(#105065,#105066,#105067,#105068,
#105069,#105070),.UNSPECIFIED.,.F.,.F.,(4,2,4),(7.65451655524924E-10,0.0126483622724694,
0.0252968591854015),.UNSPECIFIED.);
#21788=B_SPLINE_CURVE_WITH_KNOTS('',3,(#105101,#105102,#105103,#105104,
#105105,#105106,#105107),.UNSPECIFIED.,.F.,.F.,(4,3,4),(0.349369696218661,
0.357142857142857,0.361565077308603),.UNSPECIFIED.);
#21789=B_SPLINE_CURVE_WITH_KNOTS('',3,(#105108,#105109,#105110,#105111,
#105112,#105113),.UNSPECIFIED.,.F.,.F.,(4,2,4),(7.81105724995815E-10,0.0126483623097206,
0.0252968567736768),.UNSPECIFIED.);
#21790=B_SPLINE_CURVE_WITH_KNOTS('',3,(#105144,#105145,#105146,#105147,
#105148,#105149,#105150),.UNSPECIFIED.,.F.,.F.,(4,3,4),(0.349369696074482,
0.357142857142857,0.361565077306041),.UNSPECIFIED.);
#21791=B_SPLINE_CURVE_WITH_KNOTS('',3,(#105151,#105152,#105153,#105154,
#105155,#105156),.UNSPECIFIED.,.F.,.F.,(4,2,4),(8.00844415925551E-10,0.0126483623092148,
0.0252968593149661),.UNSPECIFIED.);
#21792=B_SPLINE_CURVE_WITH_KNOTS('',3,(#105187,#105188,#105189,#105190,
#105191,#105192,#105193),.UNSPECIFIED.,.F.,.F.,(4,3,4),(0.349369696074482,
0.357142857142857,0.361565077235015),.UNSPECIFIED.);
#21793=B_SPLINE_CURVE_WITH_KNOTS('',3,(#105194,#105195,#105196,#105197,
#105198,#105199),.UNSPECIFIED.,.F.,.F.,(4,2,4),(7.92615025759124E-10,0.0126483623291085,
0.0252969675663554),.UNSPECIFIED.);
#21794=B_SPLINE_CURVE_WITH_KNOTS('',3,(#105231,#105232,#105233,#105234,
#105235,#105236,#105237),.UNSPECIFIED.,.F.,.F.,(4,3,4),(0.349369696074483,
0.357142857142857,0.361565077309371),.UNSPECIFIED.);
#21795=B_SPLINE_CURVE_WITH_KNOTS('',3,(#105238,#105239,#105240,#105241,
#105242,#105243),.UNSPECIFIED.,.F.,.F.,(4,2,4),(7.5751650602434E-10,0.0126483622660331,
0.0252968596312452),.UNSPECIFIED.);
#21796=B_SPLINE_CURVE_WITH_KNOTS('',3,(#105273,#105274,#105275,#105276,
#105277,#105278,#105279),.UNSPECIFIED.,.F.,.F.,(4,3,4),(0.349369696074489,
0.357142857142857,0.361565077306682),.UNSPECIFIED.);
#21797=B_SPLINE_CURVE_WITH_KNOTS('',3,(#105280,#105281,#105282,#105283,
#105284,#105285),.UNSPECIFIED.,.F.,.F.,(4,2,4),(7.3826513221905E-10,0.0126483622505896,
0.0252968535266115),.UNSPECIFIED.);
#21798=B_SPLINE_CURVE_WITH_KNOTS('',3,(#105316,#105317,#105318,#105319,
#105320,#105321,#105322),.UNSPECIFIED.,.F.,.F.,(4,3,4),(0.349369696074491,
0.357142857142857,0.36156507730807),.UNSPECIFIED.);
#21799=B_SPLINE_CURVE_WITH_KNOTS('',3,(#105323,#105324,#105325,#105326,
#105327,#105328),.UNSPECIFIED.,.F.,.F.,(4,2,4),(8.11323775009062E-10,0.0126483623175429,
0.0252969686971379),.UNSPECIFIED.);
#21800=B_SPLINE_CURVE_WITH_KNOTS('',3,(#105359,#105360,#105361,#105362,
#105363,#105364,#105365),.UNSPECIFIED.,.F.,.F.,(4,3,4),(0.349369696074491,
0.357142857142857,0.361565077311784),.UNSPECIFIED.);
#21801=B_SPLINE_CURVE_WITH_KNOTS('',3,(#105366,#105367,#105368,#105369,
#105370,#105371),.UNSPECIFIED.,.F.,.F.,(4,2,4),(8.09533550101154E-10,0.0126483623456002,
0.0252968596199317),.UNSPECIFIED.);
#21802=B_SPLINE_CURVE_WITH_KNOTS('',3,(#105391,#105392,#105393,#105394,
#105395,#105396,#105397),.UNSPECIFIED.,.F.,.F.,(4,3,4),(0.349369696074489,
0.357142857142857,0.36156507730976),.UNSPECIFIED.);
#21803=B_SPLINE_CURVE_WITH_KNOTS('',3,(#105424,#105425,#105426,#105427,
#105428,#105429),.UNSPECIFIED.,.F.,.F.,(4,2,4),(-0.0253004834485108,-0.0126501091547225,
0.),.UNSPECIFIED.);
#21804=B_SPLINE_CURVE_WITH_KNOTS('',3,(#105450,#105451,#105452,#105453,
#105454,#105455,#105456),.UNSPECIFIED.,.F.,.F.,(4,3,4),(0.418382980245727,
0.425586573424719,0.43056953839039),.UNSPECIFIED.);
#21805=B_SPLINE_CURVE_WITH_KNOTS('',3,(#105457,#105458,#105459,#105460,
#105461,#105462),.UNSPECIFIED.,.F.,.F.,(4,2,4),(0.,0.0126500391806866,0.025300173152611),
 .UNSPECIFIED.);
#21806=B_SPLINE_CURVE_WITH_KNOTS('',3,(#105497,#105498,#105499,#105500,
#105501,#105502,#105503),.UNSPECIFIED.,.F.,.F.,(4,3,4),(0.418382980245723,
0.425586573424717,0.430569538378419),.UNSPECIFIED.);
#21807=B_SPLINE_CURVE_WITH_KNOTS('',3,(#105504,#105505,#105506,#105507,
#105508,#105509),.UNSPECIFIED.,.F.,.F.,(4,2,4),(0.,0.0126500373960896,0.0253001674275433),
 .UNSPECIFIED.);
#21808=B_SPLINE_CURVE_WITH_KNOTS('',3,(#105544,#105545,#105546,#105547,
#105548,#105549,#105550),.UNSPECIFIED.,.F.,.F.,(4,3,4),(0.418382980245722,
0.425586573424716,0.430569538399632),.UNSPECIFIED.);
#21809=B_SPLINE_CURVE_WITH_KNOTS('',3,(#105551,#105552,#105553,#105554,
#105555,#105556),.UNSPECIFIED.,.F.,.F.,(4,2,4),(0.,0.0126500411768972,0.0253001831563636),
 .UNSPECIFIED.);
#21810=B_SPLINE_CURVE_WITH_KNOTS('',3,(#105591,#105592,#105593,#105594,
#105595,#105596,#105597),.UNSPECIFIED.,.F.,.F.,(4,3,4),(0.418382980245724,
0.425586573424717,0.430569538392051),.UNSPECIFIED.);
#21811=B_SPLINE_CURVE_WITH_KNOTS('',3,(#105598,#105599,#105600,#105601,
#105602,#105603),.UNSPECIFIED.,.F.,.F.,(4,2,4),(0.,0.0126500418776801,0.0253001843093937),
 .UNSPECIFIED.);
#21812=B_SPLINE_CURVE_WITH_KNOTS('',3,(#105638,#105639,#105640,#105641,
#105642,#105643,#105644),.UNSPECIFIED.,.F.,.F.,(4,3,4),(0.418382980245725,
0.425586573424718,0.4305695383971),.UNSPECIFIED.);
#21813=B_SPLINE_CURVE_WITH_KNOTS('',3,(#105645,#105646,#105647,#105648,
#105649,#105650),.UNSPECIFIED.,.F.,.F.,(4,2,4),(0.,0.0126500363474391,0.025300163098201),
 .UNSPECIFIED.);
#21814=B_SPLINE_CURVE_WITH_KNOTS('',3,(#105685,#105686,#105687,#105688,
#105689,#105690,#105691),.UNSPECIFIED.,.F.,.F.,(4,3,4),(0.418382980245724,
0.425586573424719,0.430569538393884),.UNSPECIFIED.);
#21815=B_SPLINE_CURVE_WITH_KNOTS('',3,(#105692,#105693,#105694,#105695,
#105696,#105697),.UNSPECIFIED.,.F.,.F.,(4,2,4),(0.,0.0126500414911137,0.0253001827568244),
 .UNSPECIFIED.);
#21816=B_SPLINE_CURVE_WITH_KNOTS('',3,(#105732,#105733,#105734,#105735,
#105736,#105737,#105738),.UNSPECIFIED.,.F.,.F.,(4,3,4),(0.418382980245725,
0.425586573424719,0.430569538386616),.UNSPECIFIED.);
#21817=B_SPLINE_CURVE_WITH_KNOTS('',3,(#105739,#105740,#105741,#105742,
#105743,#105744),.UNSPECIFIED.,.F.,.F.,(4,2,4),(0.,0.0126500410508636,0.0253001825996073),
 .UNSPECIFIED.);
#21818=B_SPLINE_CURVE_WITH_KNOTS('',3,(#105779,#105780,#105781,#105782,
#105783,#105784,#105785),.UNSPECIFIED.,.F.,.F.,(4,3,4),(0.418382980245726,
0.425586573424719,0.430569538390433),.UNSPECIFIED.);
#21819=B_SPLINE_CURVE_WITH_KNOTS('',3,(#105786,#105787,#105788,#105789,
#105790,#105791),.UNSPECIFIED.,.F.,.F.,(4,2,4),(0.,0.0126500463105737,0.0253002044259655),
 .UNSPECIFIED.);
#21820=B_SPLINE_CURVE_WITH_KNOTS('',3,(#105826,#105827,#105828,#105829,
#105830,#105831,#105832),.UNSPECIFIED.,.F.,.F.,(4,3,4),(0.418382980245725,
0.425586573424719,0.430569538389505),.UNSPECIFIED.);
#21821=B_SPLINE_CURVE_WITH_KNOTS('',3,(#105833,#105834,#105835,#105836,
#105837,#105838),.UNSPECIFIED.,.F.,.F.,(4,2,4),(0.,0.0126500469432477,0.0253002069662176),
 .UNSPECIFIED.);
#21822=B_SPLINE_CURVE_WITH_KNOTS('',3,(#105873,#105874,#105875,#105876,
#105877,#105878,#105879),.UNSPECIFIED.,.F.,.F.,(4,3,4),(0.418382980245725,
0.425586573424719,0.430569538398029),.UNSPECIFIED.);
#21823=B_SPLINE_CURVE_WITH_KNOTS('',3,(#105880,#105881,#105882,#105883,
#105884,#105885),.UNSPECIFIED.,.F.,.F.,(4,2,4),(0.,0.0126500409124451,0.0253001820291273),
 .UNSPECIFIED.);
#21824=B_SPLINE_CURVE_WITH_KNOTS('',3,(#105920,#105921,#105922,#105923,
#105924,#105925,#105926),.UNSPECIFIED.,.F.,.F.,(4,3,4),(0.418382980245725,
0.425586573424719,0.430569538391061),.UNSPECIFIED.);
#21825=B_SPLINE_CURVE_WITH_KNOTS('',3,(#105927,#105928,#105929,#105930,
#105931,#105932),.UNSPECIFIED.,.F.,.F.,(4,2,4),(0.,0.0126500343052672,0.025300152987705),
 .UNSPECIFIED.);
#21826=B_SPLINE_CURVE_WITH_KNOTS('',3,(#105967,#105968,#105969,#105970,
#105971,#105972,#105973),.UNSPECIFIED.,.F.,.F.,(4,3,4),(0.418382980245725,
0.425586573424719,0.430569538390843),.UNSPECIFIED.);
#21827=B_SPLINE_CURVE_WITH_KNOTS('',3,(#105974,#105975,#105976,#105977,
#105978,#105979),.UNSPECIFIED.,.F.,.F.,(4,2,4),(0.,0.0126500451007784,0.0253001993831248),
 .UNSPECIFIED.);
#21828=B_SPLINE_CURVE_WITH_KNOTS('',3,(#106014,#106015,#106016,#106017,
#106018,#106019,#106020),.UNSPECIFIED.,.F.,.F.,(4,3,4),(0.418382980245737,
0.425586573424719,0.430569538385267),.UNSPECIFIED.);
#21829=B_SPLINE_CURVE_WITH_KNOTS('',3,(#106021,#106022,#106023,#106024,
#106025,#106026),.UNSPECIFIED.,.F.,.F.,(4,2,4),(0.,0.0126500265595761,0.0253001225025087),
 .UNSPECIFIED.);
#21830=B_SPLINE_CURVE_WITH_KNOTS('',3,(#106059,#106060,#106061,#106062,
#106063,#106064),.UNSPECIFIED.,.F.,.F.,(4,2,4),(0.,0.0126500408464834,0.0253001817619994),
 .UNSPECIFIED.);
#21831=B_SPLINE_CURVE_WITH_KNOTS('',3,(#106093,#106094,#106095,#106096,
#106097,#106098,#106099),.UNSPECIFIED.,.F.,.F.,(4,3,4),(0.418382980245723,
0.425586573424718,0.430569538398013),.UNSPECIFIED.);
#21832=B_SPLINE_CURVE_WITH_KNOTS('',3,(#106100,#106101,#106102,#106103,
#106104,#106105),.UNSPECIFIED.,.F.,.F.,(4,2,4),(0.,0.0126500337393545,0.0253001522465286),
 .UNSPECIFIED.);
#21833=B_SPLINE_CURVE_WITH_KNOTS('',3,(#106140,#106141,#106142,#106143,
#106144,#106145,#106146),.UNSPECIFIED.,.F.,.F.,(4,3,4),(0.418382980245725,
0.425586573424719,0.430569538387757),.UNSPECIFIED.);
#21834=B_SPLINE_CURVE_WITH_KNOTS('',3,(#106147,#106148,#106149,#106150,
#106151,#106152),.UNSPECIFIED.,.F.,.F.,(4,2,4),(0.,0.0126500416219824,0.0253001832968014),
 .UNSPECIFIED.);
#21835=B_SPLINE_CURVE_WITH_KNOTS('',3,(#106187,#106188,#106189,#106190,
#106191,#106192,#106193),.UNSPECIFIED.,.F.,.F.,(4,3,4),(0.418382980245725,
0.425586573424719,0.43056953838762),.UNSPECIFIED.);
#21836=B_SPLINE_CURVE_WITH_KNOTS('',3,(#106194,#106195,#106196,#106197,
#106198,#106199),.UNSPECIFIED.,.F.,.F.,(4,2,4),(0.,0.0126500323628606,0.0253001465573658),
 .UNSPECIFIED.);
#21837=B_SPLINE_CURVE_WITH_KNOTS('',3,(#106234,#106235,#106236,#106237,
#106238,#106239,#106240),.UNSPECIFIED.,.F.,.F.,(4,3,4),(0.418382980245734,
0.425586573424719,0.430569538393455),.UNSPECIFIED.);
#21838=B_SPLINE_CURVE_WITH_KNOTS('',3,(#106241,#106242,#106243,#106244,
#106245,#106246),.UNSPECIFIED.,.F.,.F.,(4,2,4),(0.,0.0126500346168763,0.0253001558984566),
 .UNSPECIFIED.);
#21839=B_SPLINE_CURVE_WITH_KNOTS('',3,(#106281,#106282,#106283,#106284,
#106285,#106286,#106287),.UNSPECIFIED.,.F.,.F.,(4,3,4),(0.418382980245729,
0.425586573424719,0.430569538392008),.UNSPECIFIED.);
#21840=B_SPLINE_CURVE_WITH_KNOTS('',3,(#106288,#106289,#106290,#106291,
#106292,#106293),.UNSPECIFIED.,.F.,.F.,(4,2,4),(0.,0.0126500414343824,0.025300184143714),
 .UNSPECIFIED.);
#21841=B_SPLINE_CURVE_WITH_KNOTS('',3,(#106328,#106329,#106330,#106331,
#106332,#106333,#106334),.UNSPECIFIED.,.F.,.F.,(4,3,4),(0.418382980245735,
0.425586573424719,0.430569538400022),.UNSPECIFIED.);
#21842=B_SPLINE_CURVE_WITH_KNOTS('',3,(#106335,#106336,#106337,#106338,
#106339,#106340),.UNSPECIFIED.,.F.,.F.,(4,2,4),(0.,0.0126500380777214,0.0253001702961879),
 .UNSPECIFIED.);
#21843=B_SPLINE_CURVE_WITH_KNOTS('',3,(#106375,#106376,#106377,#106378,
#106379,#106380,#106381),.UNSPECIFIED.,.F.,.F.,(4,3,4),(0.418382980245724,
0.425586573424719,0.430569538389702),.UNSPECIFIED.);
#21844=B_SPLINE_CURVE_WITH_KNOTS('',3,(#106382,#106383,#106384,#106385,
#106386,#106387),.UNSPECIFIED.,.F.,.F.,(4,2,4),(0.,0.0126500397057998,0.0253001753999798),
 .UNSPECIFIED.);
#21845=B_SPLINE_CURVE_WITH_KNOTS('',3,(#106422,#106423,#106424,#106425,
#106426,#106427,#106428),.UNSPECIFIED.,.F.,.F.,(4,3,4),(0.418382980245737,
0.425586573424719,0.430569538402528),.UNSPECIFIED.);
#21846=B_SPLINE_CURVE_WITH_KNOTS('',3,(#106429,#106430,#106431,#106432,
#106433,#106434),.UNSPECIFIED.,.F.,.F.,(4,2,4),(0.,0.0126500408866683,0.0253001802457082),
 .UNSPECIFIED.);
#21847=B_SPLINE_CURVE_WITH_KNOTS('',3,(#106469,#106470,#106471,#106472,
#106473,#106474,#106475),.UNSPECIFIED.,.F.,.F.,(4,3,4),(0.418382980245736,
0.425586573424719,0.430569538397518),.UNSPECIFIED.);
#21848=B_SPLINE_CURVE_WITH_KNOTS('',3,(#106476,#106477,#106478,#106479,
#106480,#106481),.UNSPECIFIED.,.F.,.F.,(4,2,4),(0.,0.0126500372775695,0.0253001652845494),
 .UNSPECIFIED.);
#21849=B_SPLINE_CURVE_WITH_KNOTS('',3,(#106516,#106517,#106518,#106519,
#106520,#106521,#106522),.UNSPECIFIED.,.F.,.F.,(4,3,4),(0.418382980245731,
0.425586573424719,0.430569538388258),.UNSPECIFIED.);
#21850=B_SPLINE_CURVE_WITH_KNOTS('',3,(#106523,#106524,#106525,#106526,
#106527,#106528),.UNSPECIFIED.,.F.,.F.,(4,2,4),(0.,0.0126500414738515,0.0253001843471962),
 .UNSPECIFIED.);
#21851=B_SPLINE_CURVE_WITH_KNOTS('',3,(#106563,#106564,#106565,#106566,
#106567,#106568,#106569),.UNSPECIFIED.,.F.,.F.,(4,3,4),(0.418382980245733,
0.425586573424719,0.430569538390303),.UNSPECIFIED.);
#21852=B_SPLINE_CURVE_WITH_KNOTS('',3,(#106570,#106571,#106572,#106573,
#106574,#106575),.UNSPECIFIED.,.F.,.F.,(4,2,4),(0.,0.0126500431760547,0.0253001897296639),
 .UNSPECIFIED.);
#21853=B_SPLINE_CURVE_WITH_KNOTS('',3,(#106610,#106611,#106612,#106613,
#106614,#106615,#106616),.UNSPECIFIED.,.F.,.F.,(4,3,4),(0.418382980245732,
0.425586573424719,0.430569538389363),.UNSPECIFIED.);
#21854=B_SPLINE_CURVE_WITH_KNOTS('',3,(#106617,#106618,#106619,#106620,
#106621,#106622),.UNSPECIFIED.,.F.,.F.,(4,2,4),(0.,0.0126500312589351,0.0253001419686268),
 .UNSPECIFIED.);
#21855=B_SPLINE_CURVE_WITH_KNOTS('',3,(#106657,#106658,#106659,#106660,
#106661,#106662,#106663),.UNSPECIFIED.,.F.,.F.,(4,3,4),(0.418382980245735,
0.425586573424719,0.430569538384267),.UNSPECIFIED.);
#21856=B_SPLINE_CURVE_WITH_KNOTS('',3,(#106664,#106665,#106666,#106667,
#106668,#106669),.UNSPECIFIED.,.F.,.F.,(4,2,4),(0.,0.0126500413506874,0.0253001821506214),
 .UNSPECIFIED.);
#21857=B_SPLINE_CURVE_WITH_KNOTS('',3,(#106704,#106705,#106706,#106707,
#106708,#106709,#106710),.UNSPECIFIED.,.F.,.F.,(4,3,4),(0.418382980245734,
0.425586573424719,0.430569538388081),.UNSPECIFIED.);
#21858=B_SPLINE_CURVE_WITH_KNOTS('',3,(#106711,#106712,#106713,#106714,
#106715,#106716),.UNSPECIFIED.,.F.,.F.,(4,2,4),(0.,0.0126500449936537,0.0253001972767284),
 .UNSPECIFIED.);
#21859=B_SPLINE_CURVE_WITH_KNOTS('',3,(#106736,#106737,#106738,#106739,
#106740,#106741,#106742),.UNSPECIFIED.,.F.,.F.,(4,3,4),(0.418382980245736,
0.425586573424719,0.430569538291038),.UNSPECIFIED.);
#21860=B_SPLINE_CURVE_WITH_KNOTS('',3,(#106769,#106770,#106771,#106772,
#106773,#106774),.UNSPECIFIED.,.F.,.F.,(4,2,4),(-0.0253039373669134,-0.0126520853650402,
-1.68311233006424E-11),.UNSPECIFIED.);
#21861=B_SPLINE_CURVE_WITH_KNOTS('',3,(#106792,#106793,#106794,#106795,
#106796,#106797),.UNSPECIFIED.,.F.,.F.,(4,2,4),(5.00322396733526E-11,0.0126520854893629,
0.0253039374589922),.UNSPECIFIED.);
#21862=B_SPLINE_CURVE_WITH_KNOTS('',3,(#106822,#106823,#106824,#106825,
#106826,#106827),.UNSPECIFIED.,.F.,.F.,(4,2,4),(0.,0.0126521070316687,0.0253039905324995),
 .UNSPECIFIED.);
#21863=B_SPLINE_CURVE_WITH_KNOTS('',3,(#106852,#106853,#106854,#106855,
#106856,#106857),.UNSPECIFIED.,.F.,.F.,(4,2,4),(3.2725810366945E-11,0.012652085552786,
0.0253039375042351),.UNSPECIFIED.);
#21864=B_SPLINE_CURVE_WITH_KNOTS('',3,(#106882,#106883,#106884,#106885,
#106886,#106887),.UNSPECIFIED.,.F.,.F.,(4,2,4),(3.62590749629602E-11,0.0126520854371781,
0.0253039374058216),.UNSPECIFIED.);
#21865=B_SPLINE_CURVE_WITH_KNOTS('',3,(#106912,#106913,#106914,#106915,
#106916,#106917),.UNSPECIFIED.,.F.,.F.,(4,2,4),(2.02885766718425E-11,0.0126520854063949,
0.0253039373604974),.UNSPECIFIED.);
#21866=B_SPLINE_CURVE_WITH_KNOTS('',3,(#106942,#106943,#106944,#106945,
#106946,#106947),.UNSPECIFIED.,.F.,.F.,(4,2,4),(0.,0.0126521067265982,0.0253039898193607),
 .UNSPECIFIED.);
#21867=B_SPLINE_CURVE_WITH_KNOTS('',3,(#106972,#106973,#106974,#106975,
#106976,#106977),.UNSPECIFIED.,.F.,.F.,(4,2,4),(3.68450136684406E-11,0.0126520854796589,
0.0253039374247473),.UNSPECIFIED.);
#21868=B_SPLINE_CURVE_WITH_KNOTS('',3,(#107002,#107003,#107004,#107005,
#107006,#107007),.UNSPECIFIED.,.F.,.F.,(4,2,4),(2.96031499286255E-11,0.0126520854663196,
0.0253039374535887),.UNSPECIFIED.);
#21869=B_SPLINE_CURVE_WITH_KNOTS('',3,(#107032,#107033,#107034,#107035,
#107036,#107037),.UNSPECIFIED.,.F.,.F.,(4,2,4),(4.94442604005428E-11,0.0126520854736033,
0.0253039374303011),.UNSPECIFIED.);
#21870=B_SPLINE_CURVE_WITH_KNOTS('',3,(#107062,#107063,#107064,#107065,
#107066,#107067),.UNSPECIFIED.,.F.,.F.,(4,2,4),(3.71849020065102E-11,0.0126520855144434,
0.0253039374629825),.UNSPECIFIED.);
#21871=B_SPLINE_CURVE_WITH_KNOTS('',3,(#107092,#107093,#107094,#107095,
#107096,#107097),.UNSPECIFIED.,.F.,.F.,(4,2,4),(0.,0.0126521066711647,0.0253039897145172),
 .UNSPECIFIED.);
#21872=B_SPLINE_CURVE_WITH_KNOTS('',3,(#107122,#107123,#107124,#107125,
#107126,#107127),.UNSPECIFIED.,.F.,.F.,(4,2,4),(3.91930707781718E-11,0.0126520854197006,
0.0253039373881218),.UNSPECIFIED.);
#21873=B_SPLINE_CURVE_WITH_KNOTS('',3,(#107152,#107153,#107154,#107155,
#107156,#107157),.UNSPECIFIED.,.F.,.F.,(4,2,4),(3.22351797597082E-11,0.0126520854379891,
0.0253039374147879),.UNSPECIFIED.);
#21874=B_SPLINE_CURVE_WITH_KNOTS('',3,(#107182,#107183,#107184,#107185,
#107186,#107187),.UNSPECIFIED.,.F.,.F.,(4,2,4),(0.,0.0126521071464492,0.0253039907276813),
 .UNSPECIFIED.);
#21875=B_SPLINE_CURVE_WITH_KNOTS('',3,(#107212,#107213,#107214,#107215,
#107216,#107217),.UNSPECIFIED.,.F.,.F.,(4,2,4),(2.49933480749287E-11,0.012652085408633,
0.0253039373642647),.UNSPECIFIED.);
#21876=B_SPLINE_CURVE_WITH_KNOTS('',3,(#107242,#107243,#107244,#107245,
#107246,#107247),.UNSPECIFIED.,.F.,.F.,(4,2,4),(2.40689927792338E-11,0.0126520853975297,
0.0253039373640824),.UNSPECIFIED.);
#21877=B_SPLINE_CURVE_WITH_KNOTS('',3,(#107272,#107273,#107274,#107275,
#107276,#107277),.UNSPECIFIED.,.F.,.F.,(4,2,4),(0.,0.0126521065211899,0.025303989285167),
 .UNSPECIFIED.);
#21878=B_SPLINE_CURVE_WITH_KNOTS('',3,(#107302,#107303,#107304,#107305,
#107306,#107307),.UNSPECIFIED.,.F.,.F.,(4,2,4),(4.20186388401848E-11,0.0126520855280583,
0.0253039374729705),.UNSPECIFIED.);
#21879=B_SPLINE_CURVE_WITH_KNOTS('',3,(#107332,#107333,#107334,#107335,
#107336,#107337),.UNSPECIFIED.,.F.,.F.,(4,2,4),(4.83695302925847E-11,0.0126520855344403,
0.0253039374579568),.UNSPECIFIED.);
#21880=B_SPLINE_CURVE_WITH_KNOTS('',3,(#107362,#107363,#107364,#107365,
#107366,#107367),.UNSPECIFIED.,.F.,.F.,(4,2,4),(0.,0.0126521066564263,0.025303989600833),
 .UNSPECIFIED.);
#21881=B_SPLINE_CURVE_WITH_KNOTS('',3,(#107392,#107393,#107394,#107395,
#107396,#107397),.UNSPECIFIED.,.F.,.F.,(4,2,4),(0.,0.0126521065478162,0.0253039894337947),
 .UNSPECIFIED.);
#21882=B_SPLINE_CURVE_WITH_KNOTS('',3,(#107422,#107423,#107424,#107425,
#107426,#107427),.UNSPECIFIED.,.F.,.F.,(4,2,4),(3.73971469161031E-11,0.0126520854361138,
0.0253039374245403),.UNSPECIFIED.);
#21883=B_SPLINE_CURVE_WITH_KNOTS('',3,(#107452,#107453,#107454,#107455,
#107456,#107457),.UNSPECIFIED.,.F.,.F.,(4,2,4),(0.,0.0126521067630497,0.0253039898367866),
 .UNSPECIFIED.);
#21884=B_SPLINE_CURVE_WITH_KNOTS('',3,(#107482,#107483,#107484,#107485,
#107486,#107487),.UNSPECIFIED.,.F.,.F.,(4,2,4),(0.,0.0126521069832498,0.0253039905019251),
 .UNSPECIFIED.);
#21885=B_SPLINE_CURVE_WITH_KNOTS('',3,(#107512,#107513,#107514,#107515,
#107516,#107517),.UNSPECIFIED.,.F.,.F.,(4,2,4),(0.,0.0126521057049491,0.0253039872136905),
 .UNSPECIFIED.);
#21886=B_SPLINE_CURVE_WITH_KNOTS('',3,(#107542,#107543,#107544,#107545,
#107546,#107547),.UNSPECIFIED.,.F.,.F.,(4,2,4),(3.70643827480995E-11,0.0126520855149235,
0.0253039374681902),.UNSPECIFIED.);
#21887=B_SPLINE_CURVE_WITH_KNOTS('',3,(#107572,#107573,#107574,#107575,
#107576,#107577),.UNSPECIFIED.,.F.,.F.,(4,2,4),(2.5219425645624E-11,0.0126520853989294,
0.0253039373990772),.UNSPECIFIED.);
#21888=B_SPLINE_CURVE_WITH_KNOTS('',3,(#107602,#107603,#107604,#107605,
#107606,#107607),.UNSPECIFIED.,.F.,.F.,(4,2,4),(0.,0.0126521068930367,0.0253039901669712),
 .UNSPECIFIED.);
#21889=B_SPLINE_CURVE_WITH_KNOTS('',3,(#107638,#107639,#107640,#107641,
#107642,#107643),.UNSPECIFIED.,.F.,.F.,(4,2,4),(-0.0239802018525615,-0.0121950471650718,
0.),.UNSPECIFIED.);
#21890=B_SPLINE_CURVE_WITH_KNOTS('',3,(#107656,#107657,#107658,#107659,
#107660,#107661,#107662,#107663,#107664,#107665),.UNSPECIFIED.,.F.,.F.,
(4,3,3,4),(0.280433083274049,0.285714285714286,0.295522983040218,0.297856505248244),
 .UNSPECIFIED.);
#21891=B_SPLINE_CURVE_WITH_KNOTS('',3,(#107666,#107667,#107668,#107669,
#107670,#107671),.UNSPECIFIED.,.F.,.F.,(4,2,4),(1.96584679017892E-11,0.0121950713546208,
0.0239801149705389),.UNSPECIFIED.);
#21892=B_SPLINE_CURVE_WITH_KNOTS('',3,(#107690,#107691,#107692,#107693,
#107694,#107695,#107696,#107697,#107698,#107699),.UNSPECIFIED.,.F.,.F.,
(4,3,3,4),(0.280433083285969,0.285714285714286,0.295522995362072,0.297856505172786),
 .UNSPECIFIED.);
#21893=B_SPLINE_CURVE_WITH_KNOTS('',3,(#107700,#107701,#107702,#107703,
#107704,#107705),.UNSPECIFIED.,.F.,.F.,(4,2,4),(0.,0.012195047336033,0.0239801017797112),
 .UNSPECIFIED.);
#21894=B_SPLINE_CURVE_WITH_KNOTS('',3,(#107724,#107725,#107726,#107727,
#107728,#107729,#107730,#107731,#107732,#107733),.UNSPECIFIED.,.F.,.F.,
(4,3,3,4),(0.280433083276854,0.285714285714286,0.295522991230299,0.297856505265968),
 .UNSPECIFIED.);
#21895=B_SPLINE_CURVE_WITH_KNOTS('',3,(#107734,#107735,#107736,#107737,
#107738,#107739),.UNSPECIFIED.,.F.,.F.,(4,2,4),(0.,0.0121950484646937,0.0239801019007123),
 .UNSPECIFIED.);
#21896=B_SPLINE_CURVE_WITH_KNOTS('',3,(#107758,#107759,#107760,#107761,
#107762,#107763,#107764,#107765,#107766,#107767),.UNSPECIFIED.,.F.,.F.,
(4,3,3,4),(0.280433083284697,0.285714285714286,0.295522993835511,0.297856505255382),
 .UNSPECIFIED.);
#21897=B_SPLINE_CURVE_WITH_KNOTS('',3,(#107768,#107769,#107770,#107771,
#107772,#107773),.UNSPECIFIED.,.F.,.F.,(4,2,4),(1.35452992190566E-11,0.0121950714296532,
0.0239801142217455),.UNSPECIFIED.);
#21898=B_SPLINE_CURVE_WITH_KNOTS('',3,(#107792,#107793,#107794,#107795,
#107796,#107797,#107798,#107799,#107800,#107801),.UNSPECIFIED.,.F.,.F.,
(4,3,3,4),(0.280433083290967,0.285714285714286,0.295522994762218,0.297856505265025),
 .UNSPECIFIED.);
#21899=B_SPLINE_CURVE_WITH_KNOTS('',3,(#107802,#107803,#107804,#107805,
#107806,#107807),.UNSPECIFIED.,.F.,.F.,(4,2,4),(0.,0.0121950482292334,0.0239801014592522),
 .UNSPECIFIED.);
#21900=B_SPLINE_CURVE_WITH_KNOTS('',3,(#107826,#107827,#107828,#107829,
#107830,#107831,#107832,#107833,#107834,#107835),.UNSPECIFIED.,.F.,.F.,
(4,3,3,4),(0.280433083288239,0.285714285714286,0.295522996978597,0.297856505254091),
 .UNSPECIFIED.);
#21901=B_SPLINE_CURVE_WITH_KNOTS('',3,(#107836,#107837,#107838,#107839,
#107840,#107841),.UNSPECIFIED.,.F.,.F.,(4,2,4),(1.58847548231737E-11,0.0121950487701971,
0.0239801006388348),.UNSPECIFIED.);
#21902=B_SPLINE_CURVE_WITH_KNOTS('',3,(#107860,#107861,#107862,#107863,
#107864,#107865,#107866,#107867,#107868,#107869),.UNSPECIFIED.,.F.,.F.,
(4,3,3,4),(0.280433083282487,0.285714285714286,0.295523001219465,0.297856505259234),
 .UNSPECIFIED.);
#21903=B_SPLINE_CURVE_WITH_KNOTS('',3,(#107870,#107871,#107872,#107873,
#107874,#107875),.UNSPECIFIED.,.F.,.F.,(4,2,4),(3.69147784996206E-12,0.0121950483221972,
0.0239800995344619),.UNSPECIFIED.);
#21904=B_SPLINE_CURVE_WITH_KNOTS('',3,(#107894,#107895,#107896,#107897,
#107898,#107899,#107900,#107901,#107902,#107903),.UNSPECIFIED.,.F.,.F.,
(4,3,3,4),(0.280433083270248,0.285714285714286,0.29552299698461,0.297856505261087),
 .UNSPECIFIED.);
#21905=B_SPLINE_CURVE_WITH_KNOTS('',3,(#107904,#107905,#107906,#107907,
#107908,#107909),.UNSPECIFIED.,.F.,.F.,(4,2,4),(3.16935510257326E-11,0.0121950711124471,
0.0239802523921913),.UNSPECIFIED.);
#21906=B_SPLINE_CURVE_WITH_KNOTS('',3,(#107928,#107929,#107930,#107931,
#107932,#107933,#107934,#107935,#107936,#107937),.UNSPECIFIED.,.F.,.F.,
(4,3,3,4),(0.280433083278328,0.285714285714286,0.295522993463896,0.297856505255155),
 .UNSPECIFIED.);
#21907=B_SPLINE_CURVE_WITH_KNOTS('',3,(#107938,#107939,#107940,#107941,
#107942,#107943),.UNSPECIFIED.,.F.,.F.,(4,2,4),(0.,0.0121950479326978,0.0239802446945865),
 .UNSPECIFIED.);
#21908=B_SPLINE_CURVE_WITH_KNOTS('',3,(#107962,#107963,#107964,#107965,
#107966,#107967,#107968,#107969,#107970,#107971),.UNSPECIFIED.,.F.,.F.,
(4,3,3,4),(0.280433083278448,0.285714285714286,0.295522984237966,0.297856505262794),
 .UNSPECIFIED.);
#21909=B_SPLINE_CURVE_WITH_KNOTS('',3,(#107972,#107973,#107974,#107975,
#107976,#107977),.UNSPECIFIED.,.F.,.F.,(4,2,4),(1.19422519947047E-11,0.0121950722182005,
0.0239801149202022),.UNSPECIFIED.);
#21910=B_SPLINE_CURVE_WITH_KNOTS('',3,(#107996,#107997,#107998,#107999,
#108000,#108001,#108002,#108003,#108004,#108005),.UNSPECIFIED.,.F.,.F.,
(4,3,3,4),(0.280433083272196,0.285714285714286,0.295522983838497,0.297856505268764),
 .UNSPECIFIED.);
#21911=B_SPLINE_CURVE_WITH_KNOTS('',3,(#108006,#108007,#108008,#108009,
#108010,#108011),.UNSPECIFIED.,.F.,.F.,(4,2,4),(2.37913079241714E-11,0.0121950715982599,
0.0239801154865616),.UNSPECIFIED.);
#21912=B_SPLINE_CURVE_WITH_KNOTS('',3,(#108030,#108031,#108032,#108033,
#108034,#108035,#108036,#108037,#108038,#108039),.UNSPECIFIED.,.F.,.F.,
(4,3,3,4),(0.280433083265126,0.285714285714286,0.295522972255689,0.297856505261105),
 .UNSPECIFIED.);
#21913=B_SPLINE_CURVE_WITH_KNOTS('',3,(#108040,#108041,#108042,#108043,
#108044,#108045),.UNSPECIFIED.,.F.,.F.,(4,2,4),(1.79830820846869E-11,0.0121950496409893,
0.0239801035787929),.UNSPECIFIED.);
#21914=B_SPLINE_CURVE_WITH_KNOTS('',3,(#108064,#108065,#108066,#108067,
#108068,#108069,#108070,#108071,#108072,#108073),.UNSPECIFIED.,.F.,.F.,
(4,3,3,4),(0.280433083271004,0.285714285714286,0.295523013441985,0.297856505260165),
 .UNSPECIFIED.);
#21915=B_SPLINE_CURVE_WITH_KNOTS('',3,(#108074,#108075,#108076,#108077,
#108078,#108079),.UNSPECIFIED.,.F.,.F.,(4,2,4),(1.86023239308098E-11,0.0121950714651211,
0.0239801130672781),.UNSPECIFIED.);
#21916=B_SPLINE_CURVE_WITH_KNOTS('',3,(#108098,#108099,#108100,#108101,
#108102,#108103,#108104,#108105,#108106,#108107),.UNSPECIFIED.,.F.,.F.,
(4,3,3,4),(0.280433083273177,0.285714285714286,0.295522970086385,0.297856505263728),
 .UNSPECIFIED.);
#21917=B_SPLINE_CURVE_WITH_KNOTS('',3,(#108108,#108109,#108110,#108111,
#108112,#108113),.UNSPECIFIED.,.F.,.F.,(4,2,4),(0.,0.01219507291151,0.0239801176553648),
 .UNSPECIFIED.);
#21918=B_SPLINE_CURVE_WITH_KNOTS('',3,(#108132,#108133,#108134,#108135,
#108136,#108137,#108138,#108139,#108140,#108141),.UNSPECIFIED.,.F.,.F.,
(4,3,3,4),(0.280433083276883,0.285714285714286,0.295522990479267,0.297856505260856),
 .UNSPECIFIED.);
#21919=B_SPLINE_CURVE_WITH_KNOTS('',3,(#108142,#108143,#108144,#108145,
#108146,#108147),.UNSPECIFIED.,.F.,.F.,(4,2,4),(1.53035637300338E-11,0.01219504982936,
0.0239802464558618),.UNSPECIFIED.);
#21920=B_SPLINE_CURVE_WITH_KNOTS('',3,(#108166,#108167,#108168,#108169,
#108170,#108171,#108172,#108173,#108174,#108175),.UNSPECIFIED.,.F.,.F.,
(4,3,3,4),(0.280433083287991,0.285714285714286,0.295522992480121,0.297856505269155),
 .UNSPECIFIED.);
#21921=B_SPLINE_CURVE_WITH_KNOTS('',3,(#108176,#108177,#108178,#108179,
#108180,#108181),.UNSPECIFIED.,.F.,.F.,(4,2,4),(0.,0.0121950472906913,0.0239801004075415),
 .UNSPECIFIED.);
#21922=B_SPLINE_CURVE_WITH_KNOTS('',3,(#108200,#108201,#108202,#108203,
#108204,#108205,#108206,#108207,#108208,#108209),.UNSPECIFIED.,.F.,.F.,
(4,3,3,4),(0.280433083278512,0.285714285714286,0.295522990639051,0.297856505260552),
 .UNSPECIFIED.);
#21923=B_SPLINE_CURVE_WITH_KNOTS('',3,(#108210,#108211,#108212,#108213,
#108214,#108215),.UNSPECIFIED.,.F.,.F.,(4,2,4),(1.43098409550063E-11,0.0121950484351843,
0.0239801006439196),.UNSPECIFIED.);
#21924=B_SPLINE_CURVE_WITH_KNOTS('',3,(#108234,#108235,#108236,#108237,
#108238,#108239,#108240,#108241,#108242,#108243),.UNSPECIFIED.,.F.,.F.,
(4,3,3,4),(0.280433083287628,0.285714285714286,0.29552299030318,0.297856505246354),
 .UNSPECIFIED.);
#21925=B_SPLINE_CURVE_WITH_KNOTS('',3,(#108244,#108245,#108246,#108247,
#108248,#108249),.UNSPECIFIED.,.F.,.F.,(4,2,4),(0.,0.0121950478615351,0.0239802452375475),
 .UNSPECIFIED.);
#21926=B_SPLINE_CURVE_WITH_KNOTS('',3,(#108268,#108269,#108270,#108271,
#108272,#108273,#108274,#108275,#108276,#108277),.UNSPECIFIED.,.F.,.F.,
(4,3,3,4),(0.280433083285338,0.285714285714286,0.295522998736992,0.297856505260913),
 .UNSPECIFIED.);
#21927=B_SPLINE_CURVE_WITH_KNOTS('',3,(#108278,#108279,#108280,#108281,
#108282,#108283),.UNSPECIFIED.,.F.,.F.,(4,2,4),(1.23192632431422E-11,0.0121950718427872,
0.0239801151610334),.UNSPECIFIED.);
#21928=B_SPLINE_CURVE_WITH_KNOTS('',3,(#108302,#108303,#108304,#108305,
#108306,#108307,#108308,#108309,#108310,#108311),.UNSPECIFIED.,.F.,.F.,
(4,3,3,4),(0.280433083281084,0.285714285714286,0.295523005586588,0.29785650526148),
 .UNSPECIFIED.);
#21929=B_SPLINE_CURVE_WITH_KNOTS('',3,(#108312,#108313,#108314,#108315,
#108316,#108317),.UNSPECIFIED.,.F.,.F.,(4,2,4),(0.,0.0121950485817599,0.0239802616992687),
 .UNSPECIFIED.);
#21930=B_SPLINE_CURVE_WITH_KNOTS('',3,(#108336,#108337,#108338,#108339,
#108340,#108341,#108342,#108343,#108344,#108345),.UNSPECIFIED.,.F.,.F.,
(4,3,3,4),(0.280433083273359,0.285714285714286,0.29552298438251,0.297856505254811),
 .UNSPECIFIED.);
#21931=B_SPLINE_CURVE_WITH_KNOTS('',3,(#108346,#108347,#108348,#108349,
#108350,#108351),.UNSPECIFIED.,.F.,.F.,(4,2,4),(0.,0.012195047999912,0.0239801007748419),
 .UNSPECIFIED.);
#21932=B_SPLINE_CURVE_WITH_KNOTS('',3,(#108370,#108371,#108372,#108373,
#108374,#108375,#108376,#108377,#108378,#108379),.UNSPECIFIED.,.F.,.F.,
(4,3,3,4),(0.28043308327774,0.285714285714286,0.295522991827137,0.297856505260904),
 .UNSPECIFIED.);
#21933=B_SPLINE_CURVE_WITH_KNOTS('',3,(#108380,#108381,#108382,#108383,
#108384,#108385),.UNSPECIFIED.,.F.,.F.,(4,2,4),(1.7066885657581E-11,0.0121950714643382,
0.0239802435135067),.UNSPECIFIED.);
#21934=B_SPLINE_CURVE_WITH_KNOTS('',3,(#108404,#108405,#108406,#108407,
#108408,#108409,#108410,#108411,#108412,#108413),.UNSPECIFIED.,.F.,.F.,
(4,3,3,4),(0.280433083267565,0.285714285714286,0.29552299565643,0.297856505250778),
 .UNSPECIFIED.);
#21935=B_SPLINE_CURVE_WITH_KNOTS('',3,(#108414,#108415,#108416,#108417,
#108418,#108419),.UNSPECIFIED.,.F.,.F.,(4,2,4),(0.,0.0121950489545227,0.0239802380202973),
 .UNSPECIFIED.);
#21936=B_SPLINE_CURVE_WITH_KNOTS('',3,(#108438,#108439,#108440,#108441,
#108442,#108443,#108444,#108445,#108446,#108447),.UNSPECIFIED.,.F.,.F.,
(4,3,3,4),(0.28043308327945,0.285714285714286,0.295523008074204,0.297856505255121),
 .UNSPECIFIED.);
#21937=B_SPLINE_CURVE_WITH_KNOTS('',3,(#108448,#108449,#108450,#108451,
#108452,#108453),.UNSPECIFIED.,.F.,.F.,(4,2,4),(3.70023008560456E-12,0.0121950487788839,
0.0239801006020893),.UNSPECIFIED.);
#21938=B_SPLINE_CURVE_WITH_KNOTS('',3,(#108472,#108473,#108474,#108475,
#108476,#108477,#108478,#108479,#108480,#108481),.UNSPECIFIED.,.F.,.F.,
(4,3,3,4),(0.280433083278303,0.285714285714286,0.295522997600256,0.297856505256509),
 .UNSPECIFIED.);
#21939=B_SPLINE_CURVE_WITH_KNOTS('',3,(#108482,#108483,#108484,#108485,
#108486,#108487),.UNSPECIFIED.,.F.,.F.,(4,2,4),(1.94609576978618E-11,0.0121950711287126,
0.0239801127297749),.UNSPECIFIED.);
#21940=B_SPLINE_CURVE_WITH_KNOTS('',3,(#108506,#108507,#108508,#108509,
#108510,#108511,#108512,#108513,#108514,#108515),.UNSPECIFIED.,.F.,.F.,
(4,3,3,4),(0.280433083281729,0.285714285714286,0.295522987820966,0.297856505269623),
 .UNSPECIFIED.);
#21941=B_SPLINE_CURVE_WITH_KNOTS('',3,(#108516,#108517,#108518,#108519,
#108520,#108521),.UNSPECIFIED.,.F.,.F.,(4,2,4),(0.,0.0121950465272298,0.0239800988628031),
 .UNSPECIFIED.);
#21942=B_SPLINE_CURVE_WITH_KNOTS('',3,(#108540,#108541,#108542,#108543,
#108544,#108545,#108546,#108547,#108548,#108549),.UNSPECIFIED.,.F.,.F.,
(4,3,3,4),(0.280433083277661,0.285714285714286,0.295523015653847,0.297856505175428),
 .UNSPECIFIED.);
#21943=B_SPLINE_CURVE_WITH_KNOTS('',3,(#108550,#108551,#108552,#108553,
#108554,#108555),.UNSPECIFIED.,.F.,.F.,(4,2,4),(3.87647476110657E-11,0.0121950705143623,
0.0239801118280503),.UNSPECIFIED.);
#21944=B_SPLINE_CURVE_WITH_KNOTS('',3,(#108574,#108575,#108576,#108577,
#108578,#108579,#108580,#108581,#108582,#108583),.UNSPECIFIED.,.F.,.F.,
(4,3,3,4),(0.280433083277927,0.285714285714286,0.295522982173905,0.297856505255156),
 .UNSPECIFIED.);
#21945=B_SPLINE_CURVE_WITH_KNOTS('',3,(#108584,#108585,#108586,#108587,
#108588,#108589),.UNSPECIFIED.,.F.,.F.,(4,2,4),(3.62025672719479E-11,0.0121950717827385,
0.0239802380575927),.UNSPECIFIED.);
#21946=B_SPLINE_CURVE_WITH_KNOTS('',3,(#108625,#108626,#108627,#108628,
#108629,#108630),.UNSPECIFIED.,.F.,.F.,(4,2,4),(-0.0253011686839678,-0.0126507408832311,
0.),.UNSPECIFIED.);
#21947=B_SPLINE_CURVE_WITH_KNOTS('',3,(#108661,#108662,#108663,#108664,
#108665,#108666),.UNSPECIFIED.,.F.,.F.,(4,2,4),(-0.0253011842158085,-0.0126507472101198,
0.),.UNSPECIFIED.);
#21948=B_SPLINE_CURVE_WITH_KNOTS('',3,(#108697,#108698,#108699,#108700,
#108701,#108702),.UNSPECIFIED.,.F.,.F.,(4,2,4),(-0.0253011598820241,-0.0126507373294872,
0.),.UNSPECIFIED.);
#21949=B_SPLINE_CURVE_WITH_KNOTS('',3,(#108733,#108734,#108735,#108736,
#108737,#108738),.UNSPECIFIED.,.F.,.F.,(4,2,4),(-0.0253011788463282,-0.0126507450350469,
0.),.UNSPECIFIED.);
#21950=B_SPLINE_CURVE_WITH_KNOTS('',3,(#108769,#108770,#108771,#108772,
#108773,#108774),.UNSPECIFIED.,.F.,.F.,(4,2,4),(-0.0253011577904646,-0.0126507365079484,
0.),.UNSPECIFIED.);
#21951=B_SPLINE_CURVE_WITH_KNOTS('',3,(#108805,#108806,#108807,#108808,
#108809,#108810),.UNSPECIFIED.,.F.,.F.,(4,2,4),(-0.0253012250062976,-0.0126507412061137,
0.),.UNSPECIFIED.);
#21952=B_SPLINE_CURVE_WITH_KNOTS('',3,(#108841,#108842,#108843,#108844,
#108845,#108846),.UNSPECIFIED.,.F.,.F.,(4,2,4),(-0.0253011816847251,-0.0126507461326866,
0.),.UNSPECIFIED.);
#21953=B_SPLINE_CURVE_WITH_KNOTS('',3,(#108877,#108878,#108879,#108880,
#108881,#108882),.UNSPECIFIED.,.F.,.F.,(4,2,4),(-0.0253012223511792,-0.0126507403440478,
0.),.UNSPECIFIED.);
#21954=B_SPLINE_CURVE_WITH_KNOTS('',3,(#108913,#108914,#108915,#108916,
#108917,#108918),.UNSPECIFIED.,.F.,.F.,(4,2,4),(-0.0253016719835357,-0.0126509447160589,
0.),.UNSPECIFIED.);
#21955=B_SPLINE_CURVE_WITH_KNOTS('',3,(#108949,#108950,#108951,#108952,
#108953,#108954),.UNSPECIFIED.,.F.,.F.,(4,2,4),(-0.025301225482847,-0.0126507413694676,
0.),.UNSPECIFIED.);
#21956=B_SPLINE_CURVE_WITH_KNOTS('',3,(#108985,#108986,#108987,#108988,
#108989,#108990),.UNSPECIFIED.,.F.,.F.,(4,2,4),(-0.0253012382215821,-0.0126507466593568,
0.),.UNSPECIFIED.);
#21957=B_SPLINE_CURVE_WITH_KNOTS('',3,(#109021,#109022,#109023,#109024,
#109025,#109026),.UNSPECIFIED.,.F.,.F.,(4,2,4),(-0.0253011573204577,-0.012650736311468,
0.),.UNSPECIFIED.);
#21958=B_SPLINE_CURVE_WITH_KNOTS('',3,(#109057,#109058,#109059,#109060,
#109061,#109062),.UNSPECIFIED.,.F.,.F.,(4,2,4),(-0.0253012336000751,-0.0126507450371835,
0.),.UNSPECIFIED.);
#21959=B_SPLINE_CURVE_WITH_KNOTS('',3,(#109093,#109094,#109095,#109096,
#109097,#109098),.UNSPECIFIED.,.F.,.F.,(4,2,4),(-0.0253011662532075,-0.0126507399598049,
0.),.UNSPECIFIED.);
#21960=B_SPLINE_CURVE_WITH_KNOTS('',3,(#109126,#109127,#109128,#109129,
#109130,#109131),.UNSPECIFIED.,.F.,.F.,(4,2,4),(-0.0253012343126556,-0.0126507458318833,
-1.68951004922424E-9),.UNSPECIFIED.);
#21961=B_SPLINE_CURVE_WITH_KNOTS('',3,(#109156,#109157,#109158,#109159,
#109160,#109161),.UNSPECIFIED.,.F.,.F.,(4,2,4),(-0.0253011892711839,-0.0126507493052928,
0.),.UNSPECIFIED.);
#21962=B_SPLINE_CURVE_WITH_KNOTS('',3,(#109192,#109193,#109194,#109195,
#109196,#109197),.UNSPECIFIED.,.F.,.F.,(4,2,4),(-0.0253012396201875,-0.0126507472829344,
0.),.UNSPECIFIED.);
#21963=B_SPLINE_CURVE_WITH_KNOTS('',3,(#109228,#109229,#109230,#109231,
#109232,#109233),.UNSPECIFIED.,.F.,.F.,(4,2,4),(-0.0253011545055926,-0.0126507352075945,
0.),.UNSPECIFIED.);
#21964=B_SPLINE_CURVE_WITH_KNOTS('',3,(#109264,#109265,#109266,#109267,
#109268,#109269),.UNSPECIFIED.,.F.,.F.,(4,2,4),(-0.0253012183482151,-0.0126507384139842,
0.),.UNSPECIFIED.);
#21965=B_SPLINE_CURVE_WITH_KNOTS('',3,(#109300,#109301,#109302,#109303,
#109304,#109305),.UNSPECIFIED.,.F.,.F.,(4,2,4),(-0.0253011924401833,-0.012650750468979,
0.),.UNSPECIFIED.);
#21966=B_SPLINE_CURVE_WITH_KNOTS('',3,(#109336,#109337,#109338,#109339,
#109340,#109341),.UNSPECIFIED.,.F.,.F.,(4,2,4),(-0.025301227630379,-0.0126507422531963,
0.),.UNSPECIFIED.);
#21967=B_SPLINE_CURVE_WITH_KNOTS('',3,(#109372,#109373,#109374,#109375,
#109376,#109377),.UNSPECIFIED.,.F.,.F.,(4,2,4),(-0.0253012454181613,-0.0126507494057004,
0.),.UNSPECIFIED.);
#21968=B_SPLINE_CURVE_WITH_KNOTS('',3,(#109408,#109409,#109410,#109411,
#109412,#109413),.UNSPECIFIED.,.F.,.F.,(4,2,4),(-0.0253011792550513,-0.0126507451606773,
0.),.UNSPECIFIED.);
#21969=B_SPLINE_CURVE_WITH_KNOTS('',3,(#109444,#109445,#109446,#109447,
#109448,#109449),.UNSPECIFIED.,.F.,.F.,(4,2,4),(-0.025302199809708,-0.0126511583700983,
0.),.UNSPECIFIED.);
#21970=B_SPLINE_CURVE_WITH_KNOTS('',3,(#109481,#109482,#109483,#109484,
#109485,#109486),.UNSPECIFIED.,.F.,.F.,(4,2,4),(-0.0253011840298263,-0.0126507471467937,
0.),.UNSPECIFIED.);
#21971=B_SPLINE_CURVE_WITH_KNOTS('',3,(#109516,#109517,#109518,#109519,
#109520,#109521),.UNSPECIFIED.,.F.,.F.,(4,2,4),(-0.0253011859268071,-0.0126507478575772,
0.),.UNSPECIFIED.);
#21972=B_SPLINE_CURVE_WITH_KNOTS('',3,(#109552,#109553,#109554,#109555,
#109556,#109557),.UNSPECIFIED.,.F.,.F.,(4,2,4),(-0.025301169220318,-0.0126507411821087,
0.),.UNSPECIFIED.);
#21973=B_SPLINE_CURVE_WITH_KNOTS('',3,(#109588,#109589,#109590,#109591,
#109592,#109593),.UNSPECIFIED.,.F.,.F.,(4,2,4),(-0.0253012393925589,-0.0126507468711187,
0.),.UNSPECIFIED.);
#21974=B_SPLINE_CURVE_WITH_KNOTS('',3,(#109624,#109625,#109626,#109627,
#109628,#109629),.UNSPECIFIED.,.F.,.F.,(4,2,4),(-0.0253012437221507,-0.0126507489284059,
0.),.UNSPECIFIED.);
#21975=B_SPLINE_CURVE_WITH_KNOTS('',3,(#109657,#109658,#109659,#109660,
#109661,#109662),.UNSPECIFIED.,.F.,.F.,(4,2,4),(-0.0252968356990071,-0.0126485400410685,
0.),.UNSPECIFIED.);
#21976=B_SPLINE_CURVE_WITH_KNOTS('',3,(#109678,#109679,#109680,#109681,
#109682,#109683,#109684),.UNSPECIFIED.,.F.,.F.,(4,3,4),(0.285597313263199,
0.292504563548801,0.29778576616136),.UNSPECIFIED.);
#21977=B_SPLINE_CURVE_WITH_KNOTS('',3,(#109700,#109701,#109702,#109703,
#109704,#109705),.UNSPECIFIED.,.F.,.F.,(4,2,4),(-0.0252965361700464,-0.0126482848477994,
0.),.UNSPECIFIED.);
#21978=B_SPLINE_CURVE_WITH_KNOTS('',3,(#109721,#109722,#109723,#109724,
#109725,#109726,#109727),.UNSPECIFIED.,.F.,.F.,(4,3,4),(0.285597313263249,
0.292504563548819,0.297785766263882),.UNSPECIFIED.);
#21979=B_SPLINE_CURVE_WITH_KNOTS('',3,(#109743,#109744,#109745,#109746,
#109747,#109748),.UNSPECIFIED.,.F.,.F.,(4,2,4),(-0.0252968357524213,-0.0126485400643503,
0.),.UNSPECIFIED.);
#21980=B_SPLINE_CURVE_WITH_KNOTS('',3,(#109764,#109765,#109766,#109767,
#109768,#109769,#109770),.UNSPECIFIED.,.F.,.F.,(4,3,4),(0.285597313263242,
0.292504563548821,0.297785766263882),.UNSPECIFIED.);
#21981=B_SPLINE_CURVE_WITH_KNOTS('',3,(#109786,#109787,#109788,#109789,
#109790,#109791),.UNSPECIFIED.,.F.,.F.,(4,2,4),(-0.0252968357378529,-0.012648540059275,
0.),.UNSPECIFIED.);
#21982=B_SPLINE_CURVE_WITH_KNOTS('',3,(#109807,#109808,#109809,#109810,
#109811,#109812,#109813),.UNSPECIFIED.,.F.,.F.,(4,3,4),(0.285597313263251,
0.292504563548821,0.297785766263885),.UNSPECIFIED.);
#21983=B_SPLINE_CURVE_WITH_KNOTS('',3,(#109829,#109830,#109831,#109832,
#109833,#109834),.UNSPECIFIED.,.F.,.F.,(4,2,4),(-0.0252968357985692,-0.0126485400760452,
0.),.UNSPECIFIED.);
#21984=B_SPLINE_CURVE_WITH_KNOTS('',3,(#109850,#109851,#109852,#109853,
#109854,#109855,#109856),.UNSPECIFIED.,.F.,.F.,(4,3,4),(0.285597313263242,
0.292504563548821,0.297785766263878),.UNSPECIFIED.);
#21985=B_SPLINE_CURVE_WITH_KNOTS('',3,(#109872,#109873,#109874,#109875,
#109876,#109877),.UNSPECIFIED.,.F.,.F.,(4,2,4),(-0.0252968357636569,-0.012648540092616,
-1.44209019725672E-11),.UNSPECIFIED.);
#21986=B_SPLINE_CURVE_WITH_KNOTS('',3,(#109893,#109894,#109895,#109896,
#109897,#109898,#109899),.UNSPECIFIED.,.F.,.F.,(4,3,4),(0.285597313263247,
0.292504563548818,0.297785766263879),.UNSPECIFIED.);
#21987=B_SPLINE_CURVE_WITH_KNOTS('',3,(#109915,#109916,#109917,#109918,
#109919,#109920),.UNSPECIFIED.,.F.,.F.,(4,2,4),(-0.0252962100658619,-0.0126482866101926,
0.),.UNSPECIFIED.);
#21988=B_SPLINE_CURVE_WITH_KNOTS('',3,(#109936,#109937,#109938,#109939,
#109940,#109941,#109942),.UNSPECIFIED.,.F.,.F.,(4,3,4),(0.285597313263248,
0.292504563548819,0.297785766161452),.UNSPECIFIED.);
#21989=B_SPLINE_CURVE_WITH_KNOTS('',3,(#109958,#109959,#109960,#109961,
#109962,#109963),.UNSPECIFIED.,.F.,.F.,(4,2,4),(-0.0252968357810003,-0.012648540091324,
0.),.UNSPECIFIED.);
#21990=B_SPLINE_CURVE_WITH_KNOTS('',3,(#109979,#109980,#109981,#109982,
#109983,#109984,#109985),.UNSPECIFIED.,.F.,.F.,(4,3,4),(0.285597313263238,
0.292504563548819,0.297785766263878),.UNSPECIFIED.);
#21991=B_SPLINE_CURVE_WITH_KNOTS('',3,(#110001,#110002,#110003,#110004,
#110005,#110006),.UNSPECIFIED.,.F.,.F.,(4,2,4),(-0.0252968357048677,-0.0126485400491316,
0.),.UNSPECIFIED.);
#21992=B_SPLINE_CURVE_WITH_KNOTS('',3,(#110022,#110023,#110024,#110025,
#110026,#110027,#110028),.UNSPECIFIED.,.F.,.F.,(4,3,4),(0.285597313263247,
0.292504563548818,0.297785766263879),.UNSPECIFIED.);
#21993=B_SPLINE_CURVE_WITH_KNOTS('',3,(#110044,#110045,#110046,#110047,
#110048,#110049),.UNSPECIFIED.,.F.,.F.,(4,2,4),(-0.0252968357538185,-0.0126485400631416,
0.),.UNSPECIFIED.);
#21994=B_SPLINE_CURVE_WITH_KNOTS('',3,(#110065,#110066,#110067,#110068,
#110069,#110070,#110071),.UNSPECIFIED.,.F.,.F.,(4,3,4),(0.28559731326324,
0.292504563548819,0.297785766263876),.UNSPECIFIED.);
#21995=B_SPLINE_CURVE_WITH_KNOTS('',3,(#110087,#110088,#110089,#110090,
#110091,#110092),.UNSPECIFIED.,.F.,.F.,(4,2,4),(-0.02529683573446,-0.0126485400816567,
-1.60400685789153E-11),.UNSPECIFIED.);
#21996=B_SPLINE_CURVE_WITH_KNOTS('',3,(#110108,#110109,#110110,#110111,
#110112,#110113,#110114),.UNSPECIFIED.,.F.,.F.,(4,3,4),(0.285597313263248,
0.292504563548819,0.297785766263886),.UNSPECIFIED.);
#21997=B_SPLINE_CURVE_WITH_KNOTS('',3,(#110130,#110131,#110132,#110133,
#110134,#110135),.UNSPECIFIED.,.F.,.F.,(4,2,4),(-0.0252968357641617,-0.012648540066526,
0.),.UNSPECIFIED.);
#21998=B_SPLINE_CURVE_WITH_KNOTS('',3,(#110151,#110152,#110153,#110154,
#110155,#110156,#110157),.UNSPECIFIED.,.F.,.F.,(4,3,4),(0.28559731326324,
0.292504563548819,0.297785766263877),.UNSPECIFIED.);
#21999=B_SPLINE_CURVE_WITH_KNOTS('',3,(#110173,#110174,#110175,#110176,
#110177,#110178),.UNSPECIFIED.,.F.,.F.,(4,2,4),(-0.0252968357896558,-0.0126485400701538,
0.),.UNSPECIFIED.);
#22000=B_SPLINE_CURVE_WITH_KNOTS('',3,(#110194,#110195,#110196,#110197,
#110198,#110199,#110200),.UNSPECIFIED.,.F.,.F.,(4,3,4),(0.285597313263243,
0.292504563548818,0.297785766263875),.UNSPECIFIED.);
#22001=B_SPLINE_CURVE_WITH_KNOTS('',3,(#110216,#110217,#110218,#110219,
#110220,#110221),.UNSPECIFIED.,.F.,.F.,(4,2,4),(-0.0252962100515733,-0.0126482866018716,
0.),.UNSPECIFIED.);
#22002=B_SPLINE_CURVE_WITH_KNOTS('',3,(#110237,#110238,#110239,#110240,
#110241,#110242,#110243),.UNSPECIFIED.,.F.,.F.,(4,3,4),(0.285597313263226,
0.292504563548819,0.297785766161952),.UNSPECIFIED.);
#22003=B_SPLINE_CURVE_WITH_KNOTS('',3,(#110259,#110260,#110261,#110262,
#110263,#110264),.UNSPECIFIED.,.F.,.F.,(4,2,4),(-0.0252968357284577,-0.0126485400553069,
0.),.UNSPECIFIED.);
#22004=B_SPLINE_CURVE_WITH_KNOTS('',3,(#110280,#110281,#110282,#110283,
#110284,#110285,#110286),.UNSPECIFIED.,.F.,.F.,(4,3,4),(0.285597313263246,
0.292504563548817,0.297785766263879),.UNSPECIFIED.);
#22005=B_SPLINE_CURVE_WITH_KNOTS('',3,(#110302,#110303,#110304,#110305,
#110306,#110307),.UNSPECIFIED.,.F.,.F.,(4,2,4),(-0.0252968356959624,-0.0126485400460954,
0.),.UNSPECIFIED.);
#22006=B_SPLINE_CURVE_WITH_KNOTS('',3,(#110323,#110324,#110325,#110326,
#110327,#110328,#110329),.UNSPECIFIED.,.F.,.F.,(4,3,4),(0.285597313263248,
0.292504563548818,0.297785766162127),.UNSPECIFIED.);
#22007=B_SPLINE_CURVE_WITH_KNOTS('',3,(#110345,#110346,#110347,#110348,
#110349,#110350),.UNSPECIFIED.,.F.,.F.,(4,2,4),(-0.0252968357533458,-0.0126485400629371,
0.),.UNSPECIFIED.);
#22008=B_SPLINE_CURVE_WITH_KNOTS('',3,(#110366,#110367,#110368,#110369,
#110370,#110371,#110372),.UNSPECIFIED.,.F.,.F.,(4,3,4),(0.285597313263239,
0.292504563548819,0.297785766263876),.UNSPECIFIED.);
#22009=B_SPLINE_CURVE_WITH_KNOTS('',3,(#110388,#110389,#110390,#110391,
#110392,#110393),.UNSPECIFIED.,.F.,.F.,(4,2,4),(-0.0252968357468296,-0.0126485400548369,
0.),.UNSPECIFIED.);
#22010=B_SPLINE_CURVE_WITH_KNOTS('',3,(#110409,#110410,#110411,#110412,
#110413,#110414,#110415),.UNSPECIFIED.,.F.,.F.,(4,3,4),(0.28559731326325,
0.29250456354882,0.297785766263875),.UNSPECIFIED.);
#22011=B_SPLINE_CURVE_WITH_KNOTS('',3,(#110431,#110432,#110433,#110434,
#110435,#110436),.UNSPECIFIED.,.F.,.F.,(4,2,4),(-0.0252968357312852,-0.0126485401030248,
-1.36424656294043E-11),.UNSPECIFIED.);
#22012=B_SPLINE_CURVE_WITH_KNOTS('',3,(#110452,#110453,#110454,#110455,
#110456,#110457,#110458),.UNSPECIFIED.,.F.,.F.,(4,3,4),(0.285597313263231,
0.29250456354882,0.297785766263871),.UNSPECIFIED.);
#22013=B_SPLINE_CURVE_WITH_KNOTS('',3,(#110474,#110475,#110476,#110477,
#110478,#110479),.UNSPECIFIED.,.F.,.F.,(4,2,4),(-0.0252968357450572,-0.0126485400721381,
0.),.UNSPECIFIED.);
#22014=B_SPLINE_CURVE_WITH_KNOTS('',3,(#110495,#110496,#110497,#110498,
#110499,#110500,#110501),.UNSPECIFIED.,.F.,.F.,(4,3,4),(0.285597313263232,
0.292504563548818,0.297785766263874),.UNSPECIFIED.);
#22015=B_SPLINE_CURVE_WITH_KNOTS('',3,(#110517,#110518,#110519,#110520,
#110521,#110522),.UNSPECIFIED.,.F.,.F.,(4,2,4),(-0.0252968357143134,-0.0126485400567964,
-1.93689682348452E-11),.UNSPECIFIED.);
#22016=B_SPLINE_CURVE_WITH_KNOTS('',3,(#110538,#110539,#110540,#110541,
#110542,#110543,#110544),.UNSPECIFIED.,.F.,.F.,(4,3,4),(0.28559731326322,
0.292504563548818,0.297785766263867),.UNSPECIFIED.);
#22017=B_SPLINE_CURVE_WITH_KNOTS('',3,(#110560,#110561,#110562,#110563,
#110564,#110565),.UNSPECIFIED.,.F.,.F.,(4,2,4),(-0.0252968357957303,-0.0126485400617688,
0.),.UNSPECIFIED.);
#22018=B_SPLINE_CURVE_WITH_KNOTS('',3,(#110581,#110582,#110583,#110584,
#110585,#110586,#110587),.UNSPECIFIED.,.F.,.F.,(4,3,4),(0.285597313263247,
0.29250456354882,0.297785766162087),.UNSPECIFIED.);
#22019=B_SPLINE_CURVE_WITH_KNOTS('',3,(#110603,#110604,#110605,#110606,
#110607,#110608),.UNSPECIFIED.,.F.,.F.,(4,2,4),(-0.02529683571073,-0.0126485400556655,
0.),.UNSPECIFIED.);
#22020=B_SPLINE_CURVE_WITH_KNOTS('',3,(#110624,#110625,#110626,#110627,
#110628,#110629,#110630),.UNSPECIFIED.,.F.,.F.,(4,3,4),(0.285597313263225,
0.29250456354882,0.297785766161269),.UNSPECIFIED.);
#22021=B_SPLINE_CURVE_WITH_KNOTS('',3,(#110646,#110647,#110648,#110649,
#110650,#110651),.UNSPECIFIED.,.F.,.F.,(4,2,4),(-0.0252962192621954,-0.0126482903584362,
0.),.UNSPECIFIED.);
#22022=B_SPLINE_CURVE_WITH_KNOTS('',3,(#110667,#110668,#110669,#110670,
#110671,#110672,#110673),.UNSPECIFIED.,.F.,.F.,(4,3,4),(0.28559731326323,
0.29250456354882,0.297785766161143),.UNSPECIFIED.);
#22023=B_SPLINE_CURVE_WITH_KNOTS('',3,(#110689,#110690,#110691,#110692,
#110693,#110694),.UNSPECIFIED.,.F.,.F.,(4,2,4),(-0.0252968357981397,-0.0126485400435585,
0.),.UNSPECIFIED.);
#22024=B_SPLINE_CURVE_WITH_KNOTS('',3,(#110710,#110711,#110712,#110713,
#110714,#110715,#110716),.UNSPECIFIED.,.F.,.F.,(4,3,4),(0.285597313263077,
0.292504563548664,0.29778576626372),.UNSPECIFIED.);
#22025=B_SPLINE_CURVE_WITH_KNOTS('',3,(#110732,#110733,#110734,#110735,
#110736,#110737),.UNSPECIFIED.,.F.,.F.,(4,2,4),(-0.0252968358008816,-0.0126485400633527,
0.),.UNSPECIFIED.);
#22026=B_SPLINE_CURVE_WITH_KNOTS('',3,(#110753,#110754,#110755,#110756,
#110757,#110758,#110759),.UNSPECIFIED.,.F.,.F.,(4,3,4),(0.285597313263235,
0.29250456354882,0.297785766263876),.UNSPECIFIED.);
#22027=B_SPLINE_CURVE_WITH_KNOTS('',3,(#110775,#110776,#110777,#110778,
#110779,#110780),.UNSPECIFIED.,.F.,.F.,(4,2,4),(-0.0252965522558592,-0.0126482890945447,
0.),.UNSPECIFIED.);
#22028=B_SPLINE_CURVE_WITH_KNOTS('',3,(#110796,#110797,#110798,#110799,
#110800,#110801,#110802),.UNSPECIFIED.,.F.,.F.,(4,3,4),(0.285597313263115,
0.292504563548722,0.297785766263765),.UNSPECIFIED.);
#22029=B_SPLINE_CURVE_WITH_KNOTS('',3,(#110818,#110819,#110820,#110821,
#110822,#110823),.UNSPECIFIED.,.F.,.F.,(4,2,4),(-0.0252968358006324,-0.0126485401203243,
-1.55508869670307E-11),.UNSPECIFIED.);
#22030=B_SPLINE_CURVE_WITH_KNOTS('',3,(#110839,#110840,#110841,#110842,
#110843,#110844,#110845),.UNSPECIFIED.,.F.,.F.,(4,3,4),(0.28559731326323,
0.292504563548818,0.297785766263871),.UNSPECIFIED.);
#22031=B_SPLINE_CURVE_WITH_KNOTS('',3,(#110861,#110862,#110863,#110864,
#110865,#110866),.UNSPECIFIED.,.F.,.F.,(4,2,4),(-0.0252968357955371,-0.0126485400856769,
0.),.UNSPECIFIED.);
#22032=B_SPLINE_CURVE_WITH_KNOTS('',3,(#110882,#110883,#110884,#110885,
#110886,#110887,#110888),.UNSPECIFIED.,.F.,.F.,(4,3,4),(0.285597313263132,
0.292504563548721,0.297785766161844),.UNSPECIFIED.);
#22033=B_SPLINE_CURVE_WITH_KNOTS('',3,(#110906,#110907,#110908,#110909,
#110910,#110911),.UNSPECIFIED.,.F.,.F.,(4,2,4),(-0.0253021439456766,-0.0126510635839076,
0.),.UNSPECIFIED.);
#22034=B_SPLINE_CURVE_WITH_KNOTS('',3,(#110931,#110932,#110933,#110934,
#110935,#110936),.UNSPECIFIED.,.F.,.F.,(4,2,4),(-0.0253021899398336,-0.0126510747308192,
0.),.UNSPECIFIED.);
#22035=B_SPLINE_CURVE_WITH_KNOTS('',3,(#110956,#110957,#110958,#110959,
#110960,#110961),.UNSPECIFIED.,.F.,.F.,(4,2,4),(-0.0253021070217382,-0.0126510669277047,
0.),.UNSPECIFIED.);
#22036=B_SPLINE_CURVE_WITH_KNOTS('',3,(#110981,#110982,#110983,#110984,
#110985,#110986),.UNSPECIFIED.,.F.,.F.,(4,2,4),(-0.0253021927970414,-0.0126510754230541,
0.),.UNSPECIFIED.);
#22037=B_SPLINE_CURVE_WITH_KNOTS('',3,(#111006,#111007,#111008,#111009,
#111010,#111011),.UNSPECIFIED.,.F.,.F.,(4,2,4),(-0.0253022032712972,-0.0126510779593872,
0.),.UNSPECIFIED.);
#22038=B_SPLINE_CURVE_WITH_KNOTS('',3,(#111031,#111032,#111033,#111034,
#111035,#111036),.UNSPECIFIED.,.F.,.F.,(4,2,4),(-0.025302125896764,-0.0126510592235906,
0.),.UNSPECIFIED.);
#22039=B_SPLINE_CURVE_WITH_KNOTS('',3,(#111056,#111057,#111058,#111059,
#111060,#111061),.UNSPECIFIED.,.F.,.F.,(4,2,4),(-0.0253021609281757,-0.0126510677054464,
0.),.UNSPECIFIED.);
#22040=B_SPLINE_CURVE_WITH_KNOTS('',3,(#111081,#111082,#111083,#111084,
#111085,#111086),.UNSPECIFIED.,.F.,.F.,(4,2,4),(-0.025302142839597,-0.0126510754321364,
0.),.UNSPECIFIED.);
#22041=B_SPLINE_CURVE_WITH_KNOTS('',3,(#111106,#111107,#111108,#111109,
#111110,#111111),.UNSPECIFIED.,.F.,.F.,(4,2,4),(-0.0253020820197401,-0.0126510608438811,
0.),.UNSPECIFIED.);
#22042=B_SPLINE_CURVE_WITH_KNOTS('',3,(#111131,#111132,#111133,#111134,
#111135,#111136),.UNSPECIFIED.,.F.,.F.,(4,2,4),(-0.0253021871069684,-0.0126510740451975,
0.),.UNSPECIFIED.);
#22043=B_SPLINE_CURVE_WITH_KNOTS('',3,(#111156,#111157,#111158,#111159,
#111160,#111161),.UNSPECIFIED.,.F.,.F.,(4,2,4),(-0.025302149705,-0.0126510649876481,
0.),.UNSPECIFIED.);
#22044=B_SPLINE_CURVE_WITH_KNOTS('',3,(#111181,#111182,#111183,#111184,
#111185,#111186),.UNSPECIFIED.,.F.,.F.,(4,2,4),(-0.0253020798756929,-0.0126510600294986,
0.),.UNSPECIFIED.);
#22045=B_SPLINE_CURVE_WITH_KNOTS('',3,(#111206,#111207,#111208,#111209,
#111210,#111211),.UNSPECIFIED.,.F.,.F.,(4,2,4),(-0.0253020866229389,-0.0126510616784989,
0.),.UNSPECIFIED.);
#22046=B_SPLINE_CURVE_WITH_KNOTS('',3,(#111231,#111232,#111233,#111234,
#111235,#111236),.UNSPECIFIED.,.F.,.F.,(4,2,4),(-0.0253020878185704,-0.0126510619506973,
0.),.UNSPECIFIED.);
#22047=B_SPLINE_CURVE_WITH_KNOTS('',3,(#111256,#111257,#111258,#111259,
#111260,#111261),.UNSPECIFIED.,.F.,.F.,(4,2,4),(-0.0253022023503169,-0.0126510769560669,
0.),.UNSPECIFIED.);
#22048=B_SPLINE_CURVE_WITH_KNOTS('',3,(#111281,#111282,#111283,#111284,
#111285,#111286),.UNSPECIFIED.,.F.,.F.,(4,2,4),(-0.0253021184453625,-0.0126510574029242,
0.),.UNSPECIFIED.);
#22049=B_SPLINE_CURVE_WITH_KNOTS('',3,(#111306,#111307,#111308,#111309,
#111310,#111311),.UNSPECIFIED.,.F.,.F.,(4,2,4),(-0.0253021758358634,-0.012651071322494,
0.),.UNSPECIFIED.);
#22050=B_SPLINE_CURVE_WITH_KNOTS('',3,(#111331,#111332,#111333,#111334,
#111335,#111336),.UNSPECIFIED.,.F.,.F.,(4,2,4),(-0.0253020938917967,-0.0126510634950911,
0.),.UNSPECIFIED.);
#22051=B_SPLINE_CURVE_WITH_KNOTS('',3,(#111356,#111357,#111358,#111359,
#111360,#111361),.UNSPECIFIED.,.F.,.F.,(4,2,4),(-0.0253021022560184,-0.0126510654632121,
0.),.UNSPECIFIED.);
#22052=B_SPLINE_CURVE_WITH_KNOTS('',3,(#111381,#111382,#111383,#111384,
#111385,#111386),.UNSPECIFIED.,.F.,.F.,(4,2,4),(-0.0253021159724824,-0.0126510689880673,
0.),.UNSPECIFIED.);
#22053=B_SPLINE_CURVE_WITH_KNOTS('',3,(#111406,#111407,#111408,#111409,
#111410,#111411),.UNSPECIFIED.,.F.,.F.,(4,2,4),(-0.0253021883308794,-0.0126510743448658,
0.),.UNSPECIFIED.);
#22054=B_SPLINE_CURVE_WITH_KNOTS('',3,(#111431,#111432,#111433,#111434,
#111435,#111436),.UNSPECIFIED.,.F.,.F.,(4,2,4),(-0.0253021990250197,-0.0126510769120973,
0.),.UNSPECIFIED.);
#22055=B_SPLINE_CURVE_WITH_KNOTS('',3,(#111456,#111457,#111458,#111459,
#111460,#111461),.UNSPECIFIED.,.F.,.F.,(4,2,4),(-0.0253021158044732,-0.0126510687683093,
0.),.UNSPECIFIED.);
#22056=B_SPLINE_CURVE_WITH_KNOTS('',3,(#111481,#111482,#111483,#111484,
#111485,#111486),.UNSPECIFIED.,.F.,.F.,(4,2,4),(-0.0253021521740526,-0.0126510655702641,
0.),.UNSPECIFIED.);
#22057=B_SPLINE_CURVE_WITH_KNOTS('',3,(#111506,#111507,#111508,#111509,
#111510,#111511),.UNSPECIFIED.,.F.,.F.,(4,2,4),(-0.0253020706818732,-0.0126510582491332,
0.),.UNSPECIFIED.);
#22058=B_SPLINE_CURVE_WITH_KNOTS('',3,(#111531,#111532,#111533,#111534,
#111535,#111536),.UNSPECIFIED.,.F.,.F.,(4,2,4),(-0.0253021317551461,-0.0126510606484672,
0.),.UNSPECIFIED.);
#22059=B_SPLINE_CURVE_WITH_KNOTS('',3,(#111556,#111557,#111558,#111559,
#111560,#111561),.UNSPECIFIED.,.F.,.F.,(4,2,4),(-0.0253021549968402,-0.0126510662743969,
0.),.UNSPECIFIED.);
#22060=B_SPLINE_CURVE_WITH_KNOTS('',3,(#111581,#111582,#111583,#111584,
#111585,#111586),.UNSPECIFIED.,.F.,.F.,(4,2,4),(-0.025302121984863,-0.012651070596378,
0.),.UNSPECIFIED.);
#22061=B_SPLINE_CURVE_WITH_KNOTS('',3,(#111606,#111607,#111608,#111609,
#111610,#111611),.UNSPECIFIED.,.F.,.F.,(4,2,4),(-0.0253021247416108,-0.0126510589319846,
0.),.UNSPECIFIED.);
#22062=B_SPLINE_CURVE_WITH_KNOTS('',3,(#111627,#111628,#111629,#111630,
#111631,#111632),.UNSPECIFIED.,.F.,.F.,(4,2,4),(-0.0253038261819231,-0.0126517946770251,
0.),.UNSPECIFIED.);
#22063=B_SPLINE_CURVE_WITH_KNOTS('',3,(#111652,#111653,#111654,#111655,
#111656,#111657),.UNSPECIFIED.,.F.,.F.,(4,2,4),(-0.0253038261618308,-0.0126517946582728,
0.),.UNSPECIFIED.);
#22064=B_SPLINE_CURVE_WITH_KNOTS('',3,(#111677,#111678,#111679,#111680,
#111681,#111682),.UNSPECIFIED.,.F.,.F.,(4,2,4),(-0.0253038261636585,-0.0126517946628466,
0.),.UNSPECIFIED.);
#22065=B_SPLINE_CURVE_WITH_KNOTS('',3,(#111702,#111703,#111704,#111705,
#111706,#111707),.UNSPECIFIED.,.F.,.F.,(4,2,4),(-0.0253038261705201,-0.0126517946637361,
0.),.UNSPECIFIED.);
#22066=B_SPLINE_CURVE_WITH_KNOTS('',3,(#111727,#111728,#111729,#111730,
#111731,#111732),.UNSPECIFIED.,.F.,.F.,(4,2,4),(-0.0253038261771642,-0.0126517946734875,
0.),.UNSPECIFIED.);
#22067=B_SPLINE_CURVE_WITH_KNOTS('',3,(#111752,#111753,#111754,#111755,
#111756,#111757),.UNSPECIFIED.,.F.,.F.,(4,2,4),(-0.0253038261793075,-0.0126517946600724,
0.),.UNSPECIFIED.);
#22068=B_SPLINE_CURVE_WITH_KNOTS('',3,(#111777,#111778,#111779,#111780,
#111781,#111782),.UNSPECIFIED.,.F.,.F.,(4,2,4),(-0.0253038260537912,-0.0126517945966899,
0.),.UNSPECIFIED.);
#22069=B_SPLINE_CURVE_WITH_KNOTS('',3,(#111802,#111803,#111804,#111805,
#111806,#111807),.UNSPECIFIED.,.F.,.F.,(4,2,4),(-0.0253038260654538,-0.0126517945962593,
0.),.UNSPECIFIED.);
#22070=B_SPLINE_CURVE_WITH_KNOTS('',3,(#111827,#111828,#111829,#111830,
#111831,#111832),.UNSPECIFIED.,.F.,.F.,(4,2,4),(-0.0253038261582367,-0.0126517946456034,
0.),.UNSPECIFIED.);
#22071=B_SPLINE_CURVE_WITH_KNOTS('',3,(#111852,#111853,#111854,#111855,
#111856,#111857),.UNSPECIFIED.,.F.,.F.,(4,2,4),(-0.0253038261809024,-0.0126517946637246,
0.),.UNSPECIFIED.);
#22072=B_SPLINE_CURVE_WITH_KNOTS('',3,(#111877,#111878,#111879,#111880,
#111881,#111882),.UNSPECIFIED.,.F.,.F.,(4,2,4),(-0.0253038262366878,-0.012651794713052,
0.),.UNSPECIFIED.);
#22073=B_SPLINE_CURVE_WITH_KNOTS('',3,(#111902,#111903,#111904,#111905,
#111906,#111907),.UNSPECIFIED.,.F.,.F.,(4,2,4),(-0.0253038261934627,-0.0126517946811558,
0.),.UNSPECIFIED.);
#22074=B_SPLINE_CURVE_WITH_KNOTS('',3,(#111927,#111928,#111929,#111930,
#111931,#111932),.UNSPECIFIED.,.F.,.F.,(4,2,4),(-0.0253038261820815,-0.0126517946816107,
0.),.UNSPECIFIED.);
#22075=B_SPLINE_CURVE_WITH_KNOTS('',3,(#111952,#111953,#111954,#111955,
#111956,#111957),.UNSPECIFIED.,.F.,.F.,(4,2,4),(-0.0253038261910213,-0.0126517946722807,
0.),.UNSPECIFIED.);
#22076=B_SPLINE_CURVE_WITH_KNOTS('',3,(#111977,#111978,#111979,#111980,
#111981,#111982),.UNSPECIFIED.,.F.,.F.,(4,2,4),(-0.0253038261161507,-0.0126517946202027,
0.),.UNSPECIFIED.);
#22077=B_SPLINE_CURVE_WITH_KNOTS('',3,(#112002,#112003,#112004,#112005,
#112006,#112007),.UNSPECIFIED.,.F.,.F.,(4,2,4),(-0.0253038261824897,-0.0126517946767165,
0.),.UNSPECIFIED.);
#22078=B_SPLINE_CURVE_WITH_KNOTS('',3,(#112027,#112028,#112029,#112030,
#112031,#112032),.UNSPECIFIED.,.F.,.F.,(4,2,4),(-0.0253038261177518,-0.0126517946220728,
0.),.UNSPECIFIED.);
#22079=B_SPLINE_CURVE_WITH_KNOTS('',3,(#112052,#112053,#112054,#112055,
#112056,#112057),.UNSPECIFIED.,.F.,.F.,(4,2,4),(-0.0253038260398844,-0.012651794577381,
0.),.UNSPECIFIED.);
#22080=B_SPLINE_CURVE_WITH_KNOTS('',3,(#112077,#112078,#112079,#112080,
#112081,#112082),.UNSPECIFIED.,.F.,.F.,(4,2,4),(-0.0253038262042702,-0.0126517946823898,
0.),.UNSPECIFIED.);
#22081=B_SPLINE_CURVE_WITH_KNOTS('',3,(#112102,#112103,#112104,#112105,
#112106,#112107),.UNSPECIFIED.,.F.,.F.,(4,2,4),(-0.0253038261656433,-0.0126517946704612,
0.),.UNSPECIFIED.);
#22082=B_SPLINE_CURVE_WITH_KNOTS('',3,(#112127,#112128,#112129,#112130,
#112131,#112132),.UNSPECIFIED.,.F.,.F.,(4,2,4),(-0.0253038262116252,-0.0126517946724291,
0.),.UNSPECIFIED.);
#22083=B_SPLINE_CURVE_WITH_KNOTS('',3,(#112152,#112153,#112154,#112155,
#112156,#112157),.UNSPECIFIED.,.F.,.F.,(4,2,4),(-0.0253038260383867,-0.0126517945850157,
0.),.UNSPECIFIED.);
#22084=B_SPLINE_CURVE_WITH_KNOTS('',3,(#112177,#112178,#112179,#112180,
#112181,#112182),.UNSPECIFIED.,.F.,.F.,(4,2,4),(-0.0253038260350243,-0.0126517945880563,
0.),.UNSPECIFIED.);
#22085=B_SPLINE_CURVE_WITH_KNOTS('',3,(#112202,#112203,#112204,#112205,
#112206,#112207),.UNSPECIFIED.,.F.,.F.,(4,2,4),(-0.0253038261822948,-0.0126517946782481,
0.),.UNSPECIFIED.);
#22086=B_SPLINE_CURVE_WITH_KNOTS('',3,(#112227,#112228,#112229,#112230,
#112231,#112232),.UNSPECIFIED.,.F.,.F.,(4,2,4),(-0.0253038260539314,-0.0126517945868141,
0.),.UNSPECIFIED.);
#22087=B_SPLINE_CURVE_WITH_KNOTS('',3,(#112252,#112253,#112254,#112255,
#112256,#112257),.UNSPECIFIED.,.F.,.F.,(4,2,4),(-0.025303826121645,-0.0126517946312714,
0.),.UNSPECIFIED.);
#22088=B_SPLINE_CURVE_WITH_KNOTS('',3,(#112277,#112278,#112279,#112280,
#112281,#112282),.UNSPECIFIED.,.F.,.F.,(4,2,4),(-0.0253038261942185,-0.0126517946844356,
0.),.UNSPECIFIED.);
#22089=B_SPLINE_CURVE_WITH_KNOTS('',3,(#112302,#112303,#112304,#112305,
#112306,#112307),.UNSPECIFIED.,.F.,.F.,(4,2,4),(-0.025303826173704,-0.0126517946618426,
0.),.UNSPECIFIED.);
#22090=B_SPLINE_CURVE_WITH_KNOTS('',3,(#112327,#112328,#112329,#112330,
#112331,#112332),.UNSPECIFIED.,.F.,.F.,(4,2,4),(-0.0253038261369524,-0.0126517946406959,
0.),.UNSPECIFIED.);
#22091=B_SPLINE_CURVE_WITH_KNOTS('',3,(#112358,#112359,#112360,#112361,
#112362,#112363),.UNSPECIFIED.,.F.,.F.,(4,2,4),(-0.0253042779522863,-0.012652023863074,
-1.26281767681702E-9),.UNSPECIFIED.);
#22092=B_SPLINE_CURVE_WITH_KNOTS('',3,(#112377,#112378,#112379,#112380,
#112381,#112382),.UNSPECIFIED.,.F.,.F.,(4,2,4),(1.1700669172451E-9,0.0126520237688829,
0.0253042779723858),.UNSPECIFIED.);
#22093=B_SPLINE_CURVE_WITH_KNOTS('',3,(#112386,#112387,#112388,#112389,
#112390,#112391,#112392,#112393,#112394,#112395),.UNSPECIFIED.,.F.,.F.,
(4,3,3,4),(0.423693445112789,0.425620451530082,0.435349112748823,0.435879799328077),
 .UNSPECIFIED.);
#22094=B_SPLINE_CURVE_WITH_KNOTS('',3,(#112423,#112424,#112425,#112426,
#112427,#112428),.UNSPECIFIED.,.F.,.F.,(4,2,4),(1.15992411025749E-9,0.0126520237432614,
0.0253042712906343),.UNSPECIFIED.);
#22095=B_SPLINE_CURVE_WITH_KNOTS('',3,(#112432,#112433,#112434,#112435,
#112436,#112437,#112438,#112439,#112440,#112441),.UNSPECIFIED.,.F.,.F.,
(4,3,3,4),(0.423693445112179,0.425620451529627,0.435349127020628,0.435879799327622),
 .UNSPECIFIED.);
#22096=B_SPLINE_CURVE_WITH_KNOTS('',3,(#112469,#112470,#112471,#112472,
#112473,#112474),.UNSPECIFIED.,.F.,.F.,(4,2,4),(1.11407146647048E-9,0.0126520237062802,
0.0253042779618027),.UNSPECIFIED.);
#22097=B_SPLINE_CURVE_WITH_KNOTS('',3,(#112478,#112479,#112480,#112481,
#112482,#112483,#112484,#112485,#112486,#112487),.UNSPECIFIED.,.F.,.F.,
(4,3,3,4),(0.423693445112109,0.425620451530078,0.435349107778184,0.435879799328077),
 .UNSPECIFIED.);
#22098=B_SPLINE_CURVE_WITH_KNOTS('',3,(#112515,#112516,#112517,#112518,
#112519,#112520),.UNSPECIFIED.,.F.,.F.,(4,2,4),(1.18075426500004E-9,0.0126520237729946,
0.0253042779397471),.UNSPECIFIED.);
#22099=B_SPLINE_CURVE_WITH_KNOTS('',3,(#112524,#112525,#112526,#112527,
#112528,#112529,#112530,#112531,#112532,#112533),.UNSPECIFIED.,.F.,.F.,
(4,3,3,4),(0.423693445111464,0.42562045153008,0.43534911319926,0.435879799328077),
 .UNSPECIFIED.);
#22100=B_SPLINE_CURVE_WITH_KNOTS('',3,(#112561,#112562,#112563,#112564,
#112565,#112566),.UNSPECIFIED.,.F.,.F.,(4,2,4),(1.16849614942433E-9,0.0126520237539986,
0.0253042779543373),.UNSPECIFIED.);
#22101=B_SPLINE_CURVE_WITH_KNOTS('',3,(#112570,#112571,#112572,#112573,
#112574,#112575,#112576,#112577,#112578,#112579),.UNSPECIFIED.,.F.,.F.,
(4,3,3,4),(0.423693445106931,0.425620451530083,0.435349096540701,0.435879799328077),
 .UNSPECIFIED.);
#22102=B_SPLINE_CURVE_WITH_KNOTS('',3,(#112607,#112608,#112609,#112610,
#112611,#112612),.UNSPECIFIED.,.F.,.F.,(4,2,4),(1.16282290389696E-9,0.0126520237489755,
0.0253042779541902),.UNSPECIFIED.);
#22103=B_SPLINE_CURVE_WITH_KNOTS('',3,(#112616,#112617,#112618,#112619,
#112620,#112621,#112622,#112623,#112624,#112625),.UNSPECIFIED.,.F.,.F.,
(4,3,3,4),(0.423693445111984,0.425620451530082,0.43534912265206,0.435879799328077),
 .UNSPECIFIED.);
#22104=B_SPLINE_CURVE_WITH_KNOTS('',3,(#112650,#112651,#112652,#112653,
#112654,#112655),.UNSPECIFIED.,.F.,.F.,(4,2,4),(1.18800802144311E-9,0.0126520237832224,
0.025304277956622),.UNSPECIFIED.);
#22105=B_SPLINE_CURVE_WITH_KNOTS('',3,(#112681,#112682,#112683,#112684,
#112685,#112686),.UNSPECIFIED.,.F.,.F.,(4,2,4),(1.2101211537022E-9,0.0126520238473612,
0.0253042780494095),.UNSPECIFIED.);
#22106=B_SPLINE_CURVE_WITH_KNOTS('',3,(#112690,#112691,#112692,#112693,
#112694,#112695,#112696,#112697,#112698,#112699),.UNSPECIFIED.,.F.,.F.,
(4,3,3,4),(0.423693445109638,0.425620451530082,0.435349112840729,0.435879799328077),
 .UNSPECIFIED.);
#22107=B_SPLINE_CURVE_WITH_KNOTS('',3,(#112727,#112728,#112729,#112730,
#112731,#112732),.UNSPECIFIED.,.F.,.F.,(4,2,4),(1.22235445067349E-9,0.0126520238432788,
0.0253042779912354),.UNSPECIFIED.);
#22108=B_SPLINE_CURVE_WITH_KNOTS('',3,(#112736,#112737,#112738,#112739,
#112740,#112741,#112742,#112743,#112744,#112745),.UNSPECIFIED.,.F.,.F.,
(4,3,3,4),(0.423693445113625,0.425620451530082,0.435349157516574,0.435879799328077),
 .UNSPECIFIED.);
#22109=B_SPLINE_CURVE_WITH_KNOTS('',3,(#112773,#112774,#112775,#112776,
#112777,#112778),.UNSPECIFIED.,.F.,.F.,(4,2,4),(1.17023127225093E-9,0.0126520237785776,
0.0253042779737898),.UNSPECIFIED.);
#22110=B_SPLINE_CURVE_WITH_KNOTS('',3,(#112782,#112783,#112784,#112785,
#112786,#112787,#112788,#112789,#112790,#112791),.UNSPECIFIED.,.F.,.F.,
(4,3,3,4),(0.423693445113355,0.425620451530082,0.435349129767105,0.435879799328077),
 .UNSPECIFIED.);
#22111=B_SPLINE_CURVE_WITH_KNOTS('',3,(#112819,#112820,#112821,#112822,
#112823,#112824),.UNSPECIFIED.,.F.,.F.,(4,2,4),(1.28536851121112E-9,0.0126520239134261,
0.0253042780053408),.UNSPECIFIED.);
#22112=B_SPLINE_CURVE_WITH_KNOTS('',3,(#112828,#112829,#112830,#112831,
#112832,#112833,#112834,#112835,#112836,#112837),.UNSPECIFIED.,.F.,.F.,
(4,3,3,4),(0.423693445111432,0.425620451530082,0.435349117131884,0.435879799328077),
 .UNSPECIFIED.);
#22113=B_SPLINE_CURVE_WITH_KNOTS('',3,(#112865,#112866,#112867,#112868,
#112869,#112870),.UNSPECIFIED.,.F.,.F.,(4,2,4),(1.17556302170415E-9,0.0126520237584382,
0.0253042779055835),.UNSPECIFIED.);
#22114=B_SPLINE_CURVE_WITH_KNOTS('',3,(#112874,#112875,#112876,#112877,
#112878,#112879,#112880,#112881,#112882,#112883),.UNSPECIFIED.,.F.,.F.,
(4,3,3,4),(0.423693445111161,0.425620451530082,0.435349124551651,0.435879799328077),
 .UNSPECIFIED.);
#22115=B_SPLINE_CURVE_WITH_KNOTS('',3,(#112911,#112912,#112913,#112914,
#112915,#112916),.UNSPECIFIED.,.F.,.F.,(4,2,4),(1.22626055802122E-9,0.0126520238411188,
0.0253042779960663),.UNSPECIFIED.);
#22116=B_SPLINE_CURVE_WITH_KNOTS('',3,(#112920,#112921,#112922,#112923,
#112924,#112925,#112926,#112927,#112928,#112929),.UNSPECIFIED.,.F.,.F.,
(4,3,3,4),(0.423693445108059,0.425620451530082,0.435349094660655,0.435879799328077),
 .UNSPECIFIED.);
#22117=B_SPLINE_CURVE_WITH_KNOTS('',3,(#112957,#112958,#112959,#112960,
#112961,#112962),.UNSPECIFIED.,.F.,.F.,(4,2,4),(1.106444852458E-9,0.0126520237073674,
0.0253042779997113),.UNSPECIFIED.);
#22118=B_SPLINE_CURVE_WITH_KNOTS('',3,(#112966,#112967,#112968,#112969,
#112970,#112971,#112972,#112973,#112974,#112975),.UNSPECIFIED.,.F.,.F.,
(4,3,3,4),(0.42369344511326,0.425620451530082,0.43534910544585,0.435879799328077),
 .UNSPECIFIED.);
#22119=B_SPLINE_CURVE_WITH_KNOTS('',3,(#113003,#113004,#113005,#113006,
#113007,#113008),.UNSPECIFIED.,.F.,.F.,(4,2,4),(1.27267692598761E-9,0.012652023900116,
0.025304278035874),.UNSPECIFIED.);
#22120=B_SPLINE_CURVE_WITH_KNOTS('',3,(#113012,#113013,#113014,#113015,
#113016,#113017,#113018,#113019,#113020,#113021),.UNSPECIFIED.,.F.,.F.,
(4,3,3,4),(0.423693445114586,0.425620451530082,0.435349109594699,0.435879799328077),
 .UNSPECIFIED.);
#22121=B_SPLINE_CURVE_WITH_KNOTS('',3,(#113049,#113050,#113051,#113052,
#113053,#113054),.UNSPECIFIED.,.F.,.F.,(4,2,4),(1.23842331568108E-9,0.0126520238471676,
0.0253042779962425),.UNSPECIFIED.);
#22122=B_SPLINE_CURVE_WITH_KNOTS('',3,(#113058,#113059,#113060,#113061,
#113062,#113063,#113064,#113065,#113066,#113067),.UNSPECIFIED.,.F.,.F.,
(4,3,3,4),(0.423693445111866,0.425620451530082,0.435349102000603,0.435879799328077),
 .UNSPECIFIED.);
#22123=B_SPLINE_CURVE_WITH_KNOTS('',3,(#113095,#113096,#113097,#113098,
#113099,#113100),.UNSPECIFIED.,.F.,.F.,(4,2,4),(1.15725186408572E-9,0.0126520237695305,
0.0253042712996014),.UNSPECIFIED.);
#22124=B_SPLINE_CURVE_WITH_KNOTS('',3,(#113104,#113105,#113106,#113107,
#113108,#113109,#113110,#113111,#113112,#113113),.UNSPECIFIED.,.F.,.F.,
(4,3,3,4),(0.423693445111451,0.425620451530082,0.435349090690307,0.435879799328077),
 .UNSPECIFIED.);
#22125=B_SPLINE_CURVE_WITH_KNOTS('',3,(#113141,#113142,#113143,#113144,
#113145,#113146),.UNSPECIFIED.,.F.,.F.,(4,2,4),(1.14185159363066E-9,0.0126520237378726,
0.0253042715112374),.UNSPECIFIED.);
#22126=B_SPLINE_CURVE_WITH_KNOTS('',3,(#113150,#113151,#113152,#113153,
#113154,#113155,#113156,#113157,#113158,#113159),.UNSPECIFIED.,.F.,.F.,
(4,3,3,4),(0.423693445113878,0.425620451530082,0.435349119213872,0.435879799328077),
 .UNSPECIFIED.);
#22127=B_SPLINE_CURVE_WITH_KNOTS('',3,(#113187,#113188,#113189,#113190,
#113191,#113192),.UNSPECIFIED.,.F.,.F.,(4,2,4),(1.16461691057117E-9,0.0126520237709924,
0.0253042713679864),.UNSPECIFIED.);
#22128=B_SPLINE_CURVE_WITH_KNOTS('',3,(#113196,#113197,#113198,#113199,
#113200,#113201,#113202,#113203,#113204,#113205),.UNSPECIFIED.,.F.,.F.,
(4,3,3,4),(0.423693445112217,0.425620451530082,0.435349133653143,0.435879799328077),
 .UNSPECIFIED.);
#22129=B_SPLINE_CURVE_WITH_KNOTS('',3,(#113233,#113234,#113235,#113236,
#113237,#113238),.UNSPECIFIED.,.F.,.F.,(4,2,4),(1.19393976681407E-9,0.012652023807887,
0.025304277979508),.UNSPECIFIED.);
#22130=B_SPLINE_CURVE_WITH_KNOTS('',3,(#113242,#113243,#113244,#113245,
#113246,#113247,#113248,#113249,#113250,#113251),.UNSPECIFIED.,.F.,.F.,
(4,3,3,4),(0.423693445114459,0.425620451530082,0.435349141726896,0.435879799328077),
 .UNSPECIFIED.);
#22131=B_SPLINE_CURVE_WITH_KNOTS('',3,(#113279,#113280,#113281,#113282,
#113283,#113284),.UNSPECIFIED.,.F.,.F.,(4,2,4),(1.18834254830485E-9,0.0126520238105013,
0.0253042780047543),.UNSPECIFIED.);
#22132=B_SPLINE_CURVE_WITH_KNOTS('',3,(#113288,#113289,#113290,#113291,
#113292,#113293,#113294,#113295,#113296,#113297),.UNSPECIFIED.,.F.,.F.,
(4,3,3,4),(0.42369344511739,0.425620451530082,0.435349104601121,0.435879799328077),
 .UNSPECIFIED.);
#22133=B_SPLINE_CURVE_WITH_KNOTS('',3,(#113325,#113326,#113327,#113328,
#113329,#113330),.UNSPECIFIED.,.F.,.F.,(4,2,4),(1.16347538958191E-9,0.0126520237493745,
0.0253042779226141),.UNSPECIFIED.);
#22134=B_SPLINE_CURVE_WITH_KNOTS('',3,(#113334,#113335,#113336,#113337,
#113338,#113339,#113340,#113341,#113342,#113343),.UNSPECIFIED.,.F.,.F.,
(4,3,3,4),(0.42369344511639,0.425620451530082,0.435349124373817,0.435879799328077),
 .UNSPECIFIED.);
#22135=B_SPLINE_CURVE_WITH_KNOTS('',3,(#113371,#113372,#113373,#113374,
#113375,#113376),.UNSPECIFIED.,.F.,.F.,(4,2,4),(1.19336501661349E-9,0.0126520238269788,
0.0253042780057151),.UNSPECIFIED.);
#22136=B_SPLINE_CURVE_WITH_KNOTS('',3,(#113393,#113394,#113395,#113396,
#113397,#113398,#113399,#113400,#113401,#113402),.UNSPECIFIED.,.F.,.F.,
(4,3,3,4),(0.423693445110999,0.425620451530082,0.435349097348392,0.435879799328077),
 .UNSPECIFIED.);
#22137=B_SPLINE_CURVE_WITH_KNOTS('',3,(#113418,#113419,#113420,#113421,
#113422,#113423),.UNSPECIFIED.,.F.,.F.,(4,2,4),(1.2375369201656E-9,0.0126520238657896,
0.0253042779874803),.UNSPECIFIED.);
#22138=B_SPLINE_CURVE_WITH_KNOTS('',3,(#113428,#113429,#113430,#113431,
#113432,#113433,#113434,#113435,#113436,#113437),.UNSPECIFIED.,.F.,.F.,
(4,3,3,4),(0.423693445114954,0.425620451530081,0.435349115952807,0.435879799328076),
 .UNSPECIFIED.);
#22139=B_SPLINE_CURVE_WITH_KNOTS('',3,(#113463,#113464,#113465,#113466,
#113467,#113468),.UNSPECIFIED.,.F.,.F.,(4,2,4),(1.20901278985797E-9,0.012652023824525,
0.0253042780280582),.UNSPECIFIED.);
#22140=B_SPLINE_CURVE_WITH_KNOTS('',3,(#113472,#113473,#113474,#113475,
#113476,#113477,#113478,#113479,#113480,#113481),.UNSPECIFIED.,.F.,.F.,
(4,3,3,4),(0.423693445116275,0.42562045153008,0.435349117168475,0.435879799328076),
 .UNSPECIFIED.);
#22141=B_SPLINE_CURVE_WITH_KNOTS('',3,(#113509,#113510,#113511,#113512,
#113513,#113514),.UNSPECIFIED.,.F.,.F.,(4,2,4),(1.17875583662026E-9,0.0126520237881625,
0.0253042780043191),.UNSPECIFIED.);
#22142=B_SPLINE_CURVE_WITH_KNOTS('',3,(#113518,#113519,#113520,#113521,
#113522,#113523,#113524,#113525,#113526,#113527),.UNSPECIFIED.,.F.,.F.,
(4,3,3,4),(0.423693445111073,0.425620451530046,0.43534911295555,0.435879799328042),
 .UNSPECIFIED.);
#22143=B_SPLINE_CURVE_WITH_KNOTS('',3,(#113555,#113556,#113557,#113558,
#113559,#113560),.UNSPECIFIED.,.F.,.F.,(4,2,4),(1.20261278446102E-9,0.0126520238272278,
0.0253042779650853),.UNSPECIFIED.);
#22144=B_SPLINE_CURVE_WITH_KNOTS('',3,(#113564,#113565,#113566,#113567,
#113568,#113569,#113570,#113571,#113572,#113573),.UNSPECIFIED.,.F.,.F.,
(4,3,3,4),(0.423693445111824,0.425620451530081,0.43534910285596,0.435879799328077),
 .UNSPECIFIED.);
#22145=B_SPLINE_CURVE_WITH_KNOTS('',3,(#113601,#113602,#113603,#113604,
#113605,#113606),.UNSPECIFIED.,.F.,.F.,(4,2,4),(1.20880002326826E-9,0.0126520238377698,
0.0253042780378564),.UNSPECIFIED.);
#22146=B_SPLINE_CURVE_WITH_KNOTS('',3,(#113610,#113611,#113612,#113613,
#113614,#113615,#113616,#113617,#113618,#113619),.UNSPECIFIED.,.F.,.F.,
(4,3,3,4),(0.42369344511094,0.425620451530084,0.435349107308875,0.435879799328079),
 .UNSPECIFIED.);
#22147=B_SPLINE_CURVE_WITH_KNOTS('',3,(#113637,#113638,#113639,#113640,
#113641,#113642,#113643,#113644,#113645,#113646),.UNSPECIFIED.,.F.,.F.,
(4,3,3,4),(0.423693445114842,0.425620451530082,0.43534908570091,0.435879799328077),
 .UNSPECIFIED.);
#22148=B_SPLINE_CURVE_WITH_KNOTS('',3,(#113674,#113675,#113676,#113677,
#113678,#113679),.UNSPECIFIED.,.F.,.F.,(4,2,4),(-0.0253007225797769,-0.0126503093936141,
0.),.UNSPECIFIED.);
#22149=B_SPLINE_CURVE_WITH_KNOTS('',3,(#113690,#113691,#113692,#113693,
#113694,#113695),.UNSPECIFIED.,.F.,.F.,(4,2,4),(5.88572981754996E-11,0.012650362637997,
0.0253009421921536),.UNSPECIFIED.);
#22150=B_SPLINE_CURVE_WITH_KNOTS('',3,(#113723,#113724,#113725,#113726,
#113727,#113728),.UNSPECIFIED.,.F.,.F.,(4,2,4),(6.4603455012057E-13,0.012650362567377,
0.0253009421633366),.UNSPECIFIED.);
#22151=B_SPLINE_CURVE_WITH_KNOTS('',3,(#113756,#113757,#113758,#113759,
#113760,#113761),.UNSPECIFIED.,.F.,.F.,(4,2,4),(2.71656584680603E-11,0.0126503625947692,
0.0253009421778162),.UNSPECIFIED.);
#22152=B_SPLINE_CURVE_WITH_KNOTS('',3,(#113789,#113790,#113791,#113792,
#113793,#113794),.UNSPECIFIED.,.F.,.F.,(4,2,4),(1.56002353552081E-11,0.012650362595027,
0.0253009422056366),.UNSPECIFIED.);
#22153=B_SPLINE_CURVE_WITH_KNOTS('',3,(#113822,#113823,#113824,#113825,
#113826,#113827),.UNSPECIFIED.,.F.,.F.,(4,2,4),(1.07002170564841E-11,0.012650362575683,
0.0253009421765229),.UNSPECIFIED.);
#22154=B_SPLINE_CURVE_WITH_KNOTS('',3,(#113855,#113856,#113857,#113858,
#113859,#113860),.UNSPECIFIED.,.F.,.F.,(4,2,4),(2.95270400716744E-11,0.0126503626042908,
0.0253009421738308),.UNSPECIFIED.);
#22155=B_SPLINE_CURVE_WITH_KNOTS('',3,(#113888,#113889,#113890,#113891,
#113892,#113893),.UNSPECIFIED.,.F.,.F.,(4,2,4),(5.34197508784737E-11,0.0126503626330273,
0.0253009421896363),.UNSPECIFIED.);
#22156=B_SPLINE_CURVE_WITH_KNOTS('',3,(#113921,#113922,#113923,#113924,
#113925,#113926),.UNSPECIFIED.,.F.,.F.,(4,2,4),(0.,0.0126503625628352,0.025300942169246),
 .UNSPECIFIED.);
#22157=B_SPLINE_CURVE_WITH_KNOTS('',3,(#113954,#113955,#113956,#113957,
#113958,#113959),.UNSPECIFIED.,.F.,.F.,(4,2,4),(0.,0.0126502910580625,0.0253006468831475),
 .UNSPECIFIED.);
#22158=B_SPLINE_CURVE_WITH_KNOTS('',3,(#113987,#113988,#113989,#113990,
#113991,#113992),.UNSPECIFIED.,.F.,.F.,(4,2,4),(1.51033193667582E-11,0.0126502983372392,
0.0253006769133421),.UNSPECIFIED.);
#22159=B_SPLINE_CURVE_WITH_KNOTS('',3,(#114020,#114021,#114022,#114023,
#114024,#114025),.UNSPECIFIED.,.F.,.F.,(4,2,4),(5.56132844431405E-11,0.0126503626325985,
0.0253009421779566),.UNSPECIFIED.);
#22160=B_SPLINE_CURVE_WITH_KNOTS('',3,(#114053,#114054,#114055,#114056,
#114057,#114058),.UNSPECIFIED.,.F.,.F.,(4,2,4),(6.25195221049412E-12,0.0126503625909652,
0.0253009421864759),.UNSPECIFIED.);
#22161=B_SPLINE_CURVE_WITH_KNOTS('',3,(#114086,#114087,#114088,#114089,
#114090,#114091),.UNSPECIFIED.,.F.,.F.,(4,2,4),(0.,0.0126503625566611,0.0253009421443978),
 .UNSPECIFIED.);
#22162=B_SPLINE_CURVE_WITH_KNOTS('',3,(#114116,#114117,#114118,#114119,
#114120,#114121),.UNSPECIFIED.,.F.,.F.,(4,2,4),(0.,0.0126503625643437,0.0253009421646361),
 .UNSPECIFIED.);
#22163=B_SPLINE_CURVE_WITH_KNOTS('',3,(#114143,#114144,#114145,#114146,
#114147,#114148),.UNSPECIFIED.,.F.,.F.,(4,2,4),(0.,0.0126502899166928,0.0253006421576979),
 .UNSPECIFIED.);
#22164=B_SPLINE_CURVE_WITH_KNOTS('',3,(#114176,#114177,#114178,#114179,
#114180,#114181),.UNSPECIFIED.,.F.,.F.,(4,2,4),(0.,0.0126503625623808,0.0253009421582833),
 .UNSPECIFIED.);
#22165=B_SPLINE_CURVE_WITH_KNOTS('',3,(#114209,#114210,#114211,#114212,
#114213,#114214),.UNSPECIFIED.,.F.,.F.,(4,2,4),(0.,0.0126502911500827,0.0253006472795662),
 .UNSPECIFIED.);
#22166=B_SPLINE_CURVE_WITH_KNOTS('',3,(#114242,#114243,#114244,#114245,
#114246,#114247),.UNSPECIFIED.,.F.,.F.,(4,2,4),(0.,0.0126502936779606,0.0253006577235599),
 .UNSPECIFIED.);
#22167=B_SPLINE_CURVE_WITH_KNOTS('',3,(#114275,#114276,#114277,#114278,
#114279,#114280),.UNSPECIFIED.,.F.,.F.,(4,2,4),(0.,0.012650287926731,0.0253006339425118),
 .UNSPECIFIED.);
#22168=B_SPLINE_CURVE_WITH_KNOTS('',3,(#114308,#114309,#114310,#114311,
#114312,#114313),.UNSPECIFIED.,.F.,.F.,(4,2,4),(0.,0.0126502886773374,0.025300637020662),
 .UNSPECIFIED.);
#22169=B_SPLINE_CURVE_WITH_KNOTS('',3,(#114341,#114342,#114343,#114344,
#114345,#114346),.UNSPECIFIED.,.F.,.F.,(4,2,4),(1.44578481018274E-11,0.01265029636312,
0.0253006688299366),.UNSPECIFIED.);
#22170=B_SPLINE_CURVE_WITH_KNOTS('',3,(#114374,#114375,#114376,#114377,
#114378,#114379),.UNSPECIFIED.,.F.,.F.,(4,2,4),(5.41752395831836E-11,0.0126503626593091,
0.0253009422415678),.UNSPECIFIED.);
#22171=B_SPLINE_CURVE_WITH_KNOTS('',3,(#114407,#114408,#114409,#114410,
#114411,#114412),.UNSPECIFIED.,.F.,.F.,(4,2,4),(3.09190381982686E-11,0.0126503626247606,
0.0253009422203617),.UNSPECIFIED.);
#22172=B_SPLINE_CURVE_WITH_KNOTS('',3,(#114440,#114441,#114442,#114443,
#114444,#114445),.UNSPECIFIED.,.F.,.F.,(4,2,4),(9.36296347676373E-11,0.0126503626925452,
0.0253009422282069),.UNSPECIFIED.);
#22173=B_SPLINE_CURVE_WITH_KNOTS('',3,(#114473,#114474,#114475,#114476,
#114477,#114478),.UNSPECIFIED.,.F.,.F.,(4,2,4),(7.07874032726965E-11,0.0126503626643126,
0.0253009422144023),.UNSPECIFIED.);
#22174=B_SPLINE_CURVE_WITH_KNOTS('',3,(#114506,#114507,#114508,#114509,
#114510,#114511),.UNSPECIFIED.,.F.,.F.,(4,2,4),(2.09563593890109E-11,0.0126503626199398,
0.025300942218264),.UNSPECIFIED.);
#22175=B_SPLINE_CURVE_WITH_KNOTS('',3,(#114539,#114540,#114541,#114542,
#114543,#114544),.UNSPECIFIED.,.F.,.F.,(4,2,4),(5.43237340880536E-11,0.0126503626330034,
0.0253009421773611),.UNSPECIFIED.);
#22176=B_SPLINE_CURVE_WITH_KNOTS('',3,(#114572,#114573,#114574,#114575,
#114576,#114577),.UNSPECIFIED.,.F.,.F.,(4,2,4),(0.,0.0126502912747948,0.0253006477804102),
 .UNSPECIFIED.);
#22177=B_SPLINE_CURVE_WITH_KNOTS('',3,(#114616,#114617,#114618,#114619,
#114620,#114621),.UNSPECIFIED.,.F.,.F.,(4,2,4),(-0.0252968045231955,-0.0126485258141896,
-2.22512321068624E-11),.UNSPECIFIED.);
#22178=B_SPLINE_CURVE_WITH_KNOTS('',3,(#114633,#114634,#114635,#114636,
#114637,#114638,#114639),.UNSPECIFIED.,.F.,.F.,(4,3,4),(0.41838298048767,
0.425586573424719,0.435845921192635),.UNSPECIFIED.);
#22179=B_SPLINE_CURVE_WITH_KNOTS('',3,(#114640,#114641,#114642,#114643,
#114644,#114645),.UNSPECIFIED.,.F.,.F.,(4,2,4),(4.66294882059351E-11,0.0126485259138885,
0.0252970983760051),.UNSPECIFIED.);
#22180=B_SPLINE_CURVE_WITH_KNOTS('',3,(#114664,#114665,#114666,#114667,
#114668,#114669,#114670),.UNSPECIFIED.,.F.,.F.,(4,3,4),(0.418382980503281,
0.425586573427989,0.435845921181019),.UNSPECIFIED.);
#22181=B_SPLINE_CURVE_WITH_KNOTS('',3,(#114671,#114672,#114673,#114674,
#114675,#114676),.UNSPECIFIED.,.F.,.F.,(4,2,4),(7.11845429795811E-11,0.0126485259324948,
0.0252971191976161),.UNSPECIFIED.);
#22182=B_SPLINE_CURVE_WITH_KNOTS('',3,(#114695,#114696,#114697,#114698,
#114699,#114700,#114701),.UNSPECIFIED.,.F.,.F.,(4,3,4),(0.418382980491422,
0.425586573424719,0.435845921184262),.UNSPECIFIED.);
#22183=B_SPLINE_CURVE_WITH_KNOTS('',3,(#114702,#114703,#114704,#114705,
#114706,#114707),.UNSPECIFIED.,.F.,.F.,(4,2,4),(2.24980277352272E-11,0.0126485258472688,
0.0252968045308311),.UNSPECIFIED.);
#22184=B_SPLINE_CURVE_WITH_KNOTS('',3,(#114726,#114727,#114728,#114729,
#114730,#114731,#114732),.UNSPECIFIED.,.F.,.F.,(4,3,4),(0.418382980513766,
0.425586573424719,0.435845921185484),.UNSPECIFIED.);
#22185=B_SPLINE_CURVE_WITH_KNOTS('',3,(#114733,#114734,#114735,#114736,
#114737,#114738),.UNSPECIFIED.,.F.,.F.,(4,2,4),(0.,0.0126485258164944,0.0252971009464653),
 .UNSPECIFIED.);
#22186=B_SPLINE_CURVE_WITH_KNOTS('',3,(#114757,#114758,#114759,#114760,
#114761,#114762,#114763),.UNSPECIFIED.,.F.,.F.,(4,3,4),(0.41838298049633,
0.42558657342472,0.435845921201898),.UNSPECIFIED.);
#22187=B_SPLINE_CURVE_WITH_KNOTS('',3,(#114764,#114765,#114766,#114767,
#114768,#114769),.UNSPECIFIED.,.F.,.F.,(4,2,4),(0.,0.0126485258144204,0.0252971006606839),
 .UNSPECIFIED.);
#22188=B_SPLINE_CURVE_WITH_KNOTS('',3,(#114788,#114789,#114790,#114791,
#114792,#114793,#114794),.UNSPECIFIED.,.F.,.F.,(4,3,4),(0.418382980505268,
0.425586573424719,0.435845921194646),.UNSPECIFIED.);
#22189=B_SPLINE_CURVE_WITH_KNOTS('',3,(#114795,#114796,#114797,#114798,
#114799,#114800),.UNSPECIFIED.,.F.,.F.,(4,2,4),(4.26339680314858E-11,0.0126485258971309,
0.0252971049135187),.UNSPECIFIED.);
#22190=B_SPLINE_CURVE_WITH_KNOTS('',3,(#114819,#114820,#114821,#114822,
#114823,#114824,#114825),.UNSPECIFIED.,.F.,.F.,(4,3,4),(0.418382980489403,
0.425586573424719,0.435845921190568),.UNSPECIFIED.);
#22191=B_SPLINE_CURVE_WITH_KNOTS('',3,(#114826,#114827,#114828,#114829,
#114830,#114831),.UNSPECIFIED.,.F.,.F.,(4,2,4),(0.,0.0126485258278667,0.0252968045262884),
 .UNSPECIFIED.);
#22192=B_SPLINE_CURVE_WITH_KNOTS('',3,(#114850,#114851,#114852,#114853,
#114854,#114855,#114856),.UNSPECIFIED.,.F.,.F.,(4,3,4),(0.418382980479098,
0.425586573428812,0.435845921190934),.UNSPECIFIED.);
#22193=B_SPLINE_CURVE_WITH_KNOTS('',3,(#114857,#114858,#114859,#114860,
#114861,#114862),.UNSPECIFIED.,.F.,.F.,(4,2,4),(3.90943730181204E-11,0.0126485258853341,
0.0252971112237266),.UNSPECIFIED.);
#22194=B_SPLINE_CURVE_WITH_KNOTS('',3,(#114881,#114882,#114883,#114884,
#114885,#114886,#114887),.UNSPECIFIED.,.F.,.F.,(4,3,4),(0.418382980500125,
0.425586573424719,0.435845921187664),.UNSPECIFIED.);
#22195=B_SPLINE_CURVE_WITH_KNOTS('',3,(#114888,#114889,#114890,#114891,
#114892,#114893),.UNSPECIFIED.,.F.,.F.,(4,2,4),(0.,0.0126485257976926,0.0252971245771656),
 .UNSPECIFIED.);
#22196=B_SPLINE_CURVE_WITH_KNOTS('',3,(#114912,#114913,#114914,#114915,
#114916,#114917,#114918),.UNSPECIFIED.,.F.,.F.,(4,3,4),(0.418382980499946,
0.425586573424719,0.43584592119258),.UNSPECIFIED.);
#22197=B_SPLINE_CURVE_WITH_KNOTS('',3,(#114919,#114920,#114921,#114922,
#114923,#114924),.UNSPECIFIED.,.F.,.F.,(4,2,4),(3.15449347118237E-11,0.0126485258940253,
0.0252970679240388),.UNSPECIFIED.);
#22198=B_SPLINE_CURVE_WITH_KNOTS('',3,(#114943,#114944,#114945,#114946,
#114947,#114948,#114949),.UNSPECIFIED.,.F.,.F.,(4,3,4),(0.41838298051113,
0.425586573424719,0.43584592119673),.UNSPECIFIED.);
#22199=B_SPLINE_CURVE_WITH_KNOTS('',3,(#114950,#114951,#114952,#114953,
#114954,#114955),.UNSPECIFIED.,.F.,.F.,(4,2,4),(2.73994050346722E-11,0.0126485258720225,
0.0252971368971687),.UNSPECIFIED.);
#22200=B_SPLINE_CURVE_WITH_KNOTS('',3,(#114974,#114975,#114976,#114977,
#114978,#114979,#114980),.UNSPECIFIED.,.F.,.F.,(4,3,4),(0.418382980509798,
0.425586573424719,0.435845921192082),.UNSPECIFIED.);
#22201=B_SPLINE_CURVE_WITH_KNOTS('',3,(#114981,#114982,#114983,#114984,
#114985,#114986),.UNSPECIFIED.,.F.,.F.,(4,2,4),(0.,0.012648525759877,0.0252971056115158),
 .UNSPECIFIED.);
#22202=B_SPLINE_CURVE_WITH_KNOTS('',3,(#115005,#115006,#115007,#115008,
#115009,#115010,#115011),.UNSPECIFIED.,.F.,.F.,(4,3,4),(0.418382980515049,
0.425586573424719,0.435845921182687),.UNSPECIFIED.);
#22203=B_SPLINE_CURVE_WITH_KNOTS('',3,(#115012,#115013,#115014,#115015,
#115016,#115017),.UNSPECIFIED.,.F.,.F.,(4,2,4),(1.57213468215666E-11,0.0126485258342171,
0.0252970836244904),.UNSPECIFIED.);
#22204=B_SPLINE_CURVE_WITH_KNOTS('',3,(#115036,#115037,#115038,#115039,
#115040,#115041,#115042),.UNSPECIFIED.,.F.,.F.,(4,3,4),(0.418382980513029,
0.425586573424719,0.435845921203653),.UNSPECIFIED.);
#22205=B_SPLINE_CURVE_WITH_KNOTS('',3,(#115043,#115044,#115045,#115046,
#115047,#115048),.UNSPECIFIED.,.F.,.F.,(4,2,4),(2.05864342097627E-11,0.0126485258407764,
0.0252971103490747),.UNSPECIFIED.);
#22206=B_SPLINE_CURVE_WITH_KNOTS('',3,(#115067,#115068,#115069,#115070,
#115071,#115072,#115073),.UNSPECIFIED.,.F.,.F.,(4,3,4),(0.418382980485447,
0.425586573430397,0.435845921197401),.UNSPECIFIED.);
#22207=B_SPLINE_CURVE_WITH_KNOTS('',3,(#115074,#115075,#115076,#115077,
#115078,#115079),.UNSPECIFIED.,.F.,.F.,(4,2,4),(3.23008789845055E-11,0.0126485258643573,
0.0252968045171681),.UNSPECIFIED.);
#22208=B_SPLINE_CURVE_WITH_KNOTS('',3,(#115098,#115099,#115100,#115101,
#115102,#115103,#115104),.UNSPECIFIED.,.F.,.F.,(4,3,4),(0.418382980476632,
0.425586573424719,0.435845921178522),.UNSPECIFIED.);
#22209=B_SPLINE_CURVE_WITH_KNOTS('',3,(#115105,#115106,#115107,#115108,
#115109,#115110),.UNSPECIFIED.,.F.,.F.,(4,2,4),(1.63062190473775E-11,0.0126485258563253,
0.0252970933324197),.UNSPECIFIED.);
#22210=B_SPLINE_CURVE_WITH_KNOTS('',3,(#115129,#115130,#115131,#115132,
#115133,#115134,#115135),.UNSPECIFIED.,.F.,.F.,(4,3,4),(0.418382980482894,
0.425586573424719,0.435845921193928),.UNSPECIFIED.);
#22211=B_SPLINE_CURVE_WITH_KNOTS('',3,(#115136,#115137,#115138,#115139,
#115140,#115141),.UNSPECIFIED.,.F.,.F.,(4,2,4),(3.7095862061997E-11,0.0126485258540792,
0.0252968044964005),.UNSPECIFIED.);
#22212=B_SPLINE_CURVE_WITH_KNOTS('',3,(#115160,#115161,#115162,#115163,
#115164,#115165,#115166),.UNSPECIFIED.,.F.,.F.,(4,3,4),(0.418382980504012,
0.425586573424719,0.435845921190153),.UNSPECIFIED.);
#22213=B_SPLINE_CURVE_WITH_KNOTS('',3,(#115167,#115168,#115169,#115170,
#115171,#115172),.UNSPECIFIED.,.F.,.F.,(4,2,4),(0.,0.0126485258021332,0.0252971237755114),
 .UNSPECIFIED.);
#22214=B_SPLINE_CURVE_WITH_KNOTS('',3,(#115191,#115192,#115193,#115194,
#115195,#115196,#115197),.UNSPECIFIED.,.F.,.F.,(4,3,4),(0.418382980512901,
0.425586573424719,0.435845921194506),.UNSPECIFIED.);
#22215=B_SPLINE_CURVE_WITH_KNOTS('',3,(#115198,#115199,#115200,#115201,
#115202,#115203),.UNSPECIFIED.,.F.,.F.,(4,2,4),(0.,0.0126485258091614,0.0252971262357942),
 .UNSPECIFIED.);
#22216=B_SPLINE_CURVE_WITH_KNOTS('',3,(#115222,#115223,#115224,#115225,
#115226,#115227,#115228),.UNSPECIFIED.,.F.,.F.,(4,3,4),(0.418382980499795,
0.425586573424719,0.435845921180363),.UNSPECIFIED.);
#22217=B_SPLINE_CURVE_WITH_KNOTS('',3,(#115229,#115230,#115231,#115232,
#115233,#115234),.UNSPECIFIED.,.F.,.F.,(4,2,4),(4.64361638924081E-11,0.0126485259046725,
0.0252970696604553),.UNSPECIFIED.);
#22218=B_SPLINE_CURVE_WITH_KNOTS('',3,(#115253,#115254,#115255,#115256,
#115257,#115258,#115259),.UNSPECIFIED.,.F.,.F.,(4,3,4),(0.418382980506079,
0.425586573424719,0.435845921191126),.UNSPECIFIED.);
#22219=B_SPLINE_CURVE_WITH_KNOTS('',3,(#115260,#115261,#115262,#115263,
#115264,#115265),.UNSPECIFIED.,.F.,.F.,(4,2,4),(3.43470368829114E-11,0.0126485258935371,
0.025297100751394),.UNSPECIFIED.);
#22220=B_SPLINE_CURVE_WITH_KNOTS('',3,(#115284,#115285,#115286,#115287,
#115288,#115289,#115290),.UNSPECIFIED.,.F.,.F.,(4,3,4),(0.418382980491293,
0.425586573424719,0.435845921202337),.UNSPECIFIED.);
#22221=B_SPLINE_CURVE_WITH_KNOTS('',3,(#115291,#115292,#115293,#115294,
#115295,#115296),.UNSPECIFIED.,.F.,.F.,(4,2,4),(0.,0.0126485258178913,0.0252971044575565),
 .UNSPECIFIED.);
#22222=B_SPLINE_CURVE_WITH_KNOTS('',3,(#115315,#115316,#115317,#115318,
#115319,#115320,#115321),.UNSPECIFIED.,.F.,.F.,(4,3,4),(0.418382980502393,
0.425586573424719,0.435845921184591),.UNSPECIFIED.);
#22223=B_SPLINE_CURVE_WITH_KNOTS('',3,(#115322,#115323,#115324,#115325,
#115326,#115327),.UNSPECIFIED.,.F.,.F.,(4,2,4),(1.51903425992353E-11,0.0126485258653875,
0.0252971164487305),.UNSPECIFIED.);
#22224=B_SPLINE_CURVE_WITH_KNOTS('',3,(#115346,#115347,#115348,#115349,
#115350,#115351,#115352),.UNSPECIFIED.,.F.,.F.,(4,3,4),(0.418382980495824,
0.425586573424718,0.435845921198099),.UNSPECIFIED.);
#22225=B_SPLINE_CURVE_WITH_KNOTS('',3,(#115353,#115354,#115355,#115356,
#115357,#115358),.UNSPECIFIED.,.F.,.F.,(4,2,4),(2.98048045712891E-11,0.0126485258797525,
0.0252970894690396),.UNSPECIFIED.);
#22226=B_SPLINE_CURVE_WITH_KNOTS('',3,(#115377,#115378,#115379,#115380,
#115381,#115382,#115383),.UNSPECIFIED.,.F.,.F.,(4,3,4),(0.418382980492499,
0.425586573424717,0.435845921198154),.UNSPECIFIED.);
#22227=B_SPLINE_CURVE_WITH_KNOTS('',3,(#115384,#115385,#115386,#115387,
#115388,#115389),.UNSPECIFIED.,.F.,.F.,(4,2,4),(0.,0.0126485257710713,0.0252971071417041),
 .UNSPECIFIED.);
#22228=B_SPLINE_CURVE_WITH_KNOTS('',3,(#115408,#115409,#115410,#115411,
#115412,#115413,#115414),.UNSPECIFIED.,.F.,.F.,(4,3,4),(0.418382980519489,
0.425586573424717,0.43584592119026),.UNSPECIFIED.);
#22229=B_SPLINE_CURVE_WITH_KNOTS('',3,(#115415,#115416,#115417,#115418,
#115419,#115420),.UNSPECIFIED.,.F.,.F.,(4,2,4),(4.64859468063662E-11,0.0126485259129894,
0.0252970884641446),.UNSPECIFIED.);
#22230=B_SPLINE_CURVE_WITH_KNOTS('',3,(#115439,#115440,#115441,#115442,
#115443,#115444,#115445),.UNSPECIFIED.,.F.,.F.,(4,3,4),(0.418382980516194,
0.425586573427319,0.435845921190088),.UNSPECIFIED.);
#22231=B_SPLINE_CURVE_WITH_KNOTS('',3,(#115446,#115447,#115448,#115449,
#115450,#115451),.UNSPECIFIED.,.F.,.F.,(4,2,4),(0.,0.0126485257202768,0.0252968057988102),
 .UNSPECIFIED.);
#22232=B_SPLINE_CURVE_WITH_KNOTS('',3,(#115470,#115471,#115472,#115473,
#115474,#115475,#115476),.UNSPECIFIED.,.F.,.F.,(4,3,4),(0.4183829805162,
0.425586573424721,0.435845921204263),.UNSPECIFIED.);
#22233=B_SPLINE_CURVE_WITH_KNOTS('',3,(#115477,#115478,#115479,#115480,
#115481,#115482),.UNSPECIFIED.,.F.,.F.,(4,2,4),(0.,0.0126485257808135,0.0252971162212155),
 .UNSPECIFIED.);
#22234=B_SPLINE_CURVE_WITH_KNOTS('',3,(#115500,#115501,#115502,#115503,
#115504,#115505,#115506),.UNSPECIFIED.,.F.,.F.,(4,3,4),(0.418382980217902,
0.425586573424719,0.43584592120451),.UNSPECIFIED.);
#22235=B_SPLINE_CURVE_WITH_KNOTS('',3,(#115518,#115519,#115520,#115521,
#115522,#115523),.UNSPECIFIED.,.F.,.F.,(4,2,4),(-0.0253030036884475,-0.012651613278566,
-6.34804847576831E-11),.UNSPECIFIED.);
#22236=B_SPLINE_CURVE_WITH_KNOTS('',3,(#115533,#115534,#115535,#115536,
#115537,#115538),.UNSPECIFIED.,.F.,.F.,(4,2,4),(3.87453103820511E-11,0.0126516133862915,
0.0253031602499559),.UNSPECIFIED.);
#22237=B_SPLINE_CURVE_WITH_KNOTS('',3,(#115558,#115559,#115560,#115561,
#115562,#115563),.UNSPECIFIED.,.F.,.F.,(4,2,4),(4.58383947136018E-11,0.012651613414177,
0.0253031740182665),.UNSPECIFIED.);
#22238=B_SPLINE_CURVE_WITH_KNOTS('',3,(#115583,#115584,#115585,#115586,
#115587,#115588),.UNSPECIFIED.,.F.,.F.,(4,2,4),(4.18194213214573E-11,0.0126516134067451,
0.0253031663402117),.UNSPECIFIED.);
#22239=B_SPLINE_CURVE_WITH_KNOTS('',3,(#115608,#115609,#115610,#115611,
#115612,#115613),.UNSPECIFIED.,.F.,.F.,(4,2,4),(3.68892339334775E-11,0.0126516134027975,
0.0253031428857036),.UNSPECIFIED.);
#22240=B_SPLINE_CURVE_WITH_KNOTS('',3,(#115633,#115634,#115635,#115636,
#115637,#115638),.UNSPECIFIED.,.F.,.F.,(4,2,4),(2.71107081691789E-11,0.0126516134121481,
0.025303136374457),.UNSPECIFIED.);
#22241=B_SPLINE_CURVE_WITH_KNOTS('',3,(#115658,#115659,#115660,#115661,
#115662,#115663),.UNSPECIFIED.,.F.,.F.,(4,2,4),(3.26941782094869E-11,0.0126516134056775,
0.0253031680303436),.UNSPECIFIED.);
#22242=B_SPLINE_CURVE_WITH_KNOTS('',3,(#115683,#115684,#115685,#115686,
#115687,#115688),.UNSPECIFIED.,.F.,.F.,(4,2,4),(4.29248539613176E-11,0.0126516134308501,
0.0253031435702894),.UNSPECIFIED.);
#22243=B_SPLINE_CURVE_WITH_KNOTS('',3,(#115708,#115709,#115710,#115711,
#115712,#115713),.UNSPECIFIED.,.F.,.F.,(4,2,4),(4.08007483957115E-11,0.0126516133998519,
0.0253031686506958),.UNSPECIFIED.);
#22244=B_SPLINE_CURVE_WITH_KNOTS('',3,(#115733,#115734,#115735,#115736,
#115737,#115738),.UNSPECIFIED.,.F.,.F.,(4,2,4),(3.58839648859037E-11,0.0126516133978681,
0.0253031555621786),.UNSPECIFIED.);
#22245=B_SPLINE_CURVE_WITH_KNOTS('',3,(#115758,#115759,#115760,#115761,
#115762,#115763),.UNSPECIFIED.,.F.,.F.,(4,2,4),(3.84531833298233E-11,0.0126516133967504,
0.0253031484415909),.UNSPECIFIED.);
#22246=B_SPLINE_CURVE_WITH_KNOTS('',3,(#115783,#115784,#115785,#115786,
#115787,#115788),.UNSPECIFIED.,.F.,.F.,(4,2,4),(2.3523365575452E-11,0.0126516133974983,
0.0253031368632556),.UNSPECIFIED.);
#22247=B_SPLINE_CURVE_WITH_KNOTS('',3,(#115808,#115809,#115810,#115811,
#115812,#115813),.UNSPECIFIED.,.F.,.F.,(4,2,4),(3.54867886648582E-11,0.0126516133853951,
0.0253031853795223),.UNSPECIFIED.);
#22248=B_SPLINE_CURVE_WITH_KNOTS('',3,(#115833,#115834,#115835,#115836,
#115837,#115838),.UNSPECIFIED.,.F.,.F.,(4,2,4),(5.96584564652658E-11,0.0126516134216209,
0.0253031646523377),.UNSPECIFIED.);
#22249=B_SPLINE_CURVE_WITH_KNOTS('',3,(#115858,#115859,#115860,#115861,
#115862,#115863),.UNSPECIFIED.,.F.,.F.,(4,2,4),(2.61156380054951E-9,0.0126516146787517,
0.025303174973131),.UNSPECIFIED.);
#22250=B_SPLINE_CURVE_WITH_KNOTS('',3,(#115883,#115884,#115885,#115886,
#115887,#115888),.UNSPECIFIED.,.F.,.F.,(4,2,4),(5.71527271307145E-11,0.0126516134042058,
0.0253031689996759),.UNSPECIFIED.);
#22251=B_SPLINE_CURVE_WITH_KNOTS('',3,(#115908,#115909,#115910,#115911,
#115912,#115913),.UNSPECIFIED.,.F.,.F.,(4,2,4),(6.59575722847113E-11,0.0126516134261569,
0.0253031712577939),.UNSPECIFIED.);
#22252=B_SPLINE_CURVE_WITH_KNOTS('',3,(#115933,#115934,#115935,#115936,
#115937,#115938),.UNSPECIFIED.,.F.,.F.,(4,2,4),(4.89391602995011E-11,0.0126516134447811,
0.0253031474960944),.UNSPECIFIED.);
#22253=B_SPLINE_CURVE_WITH_KNOTS('',3,(#115958,#115959,#115960,#115961,
#115962,#115963),.UNSPECIFIED.,.F.,.F.,(4,2,4),(4.80211333153906E-11,0.0126516134311367,
0.0253031660088819),.UNSPECIFIED.);
#22254=B_SPLINE_CURVE_WITH_KNOTS('',3,(#115983,#115984,#115985,#115986,
#115987,#115988),.UNSPECIFIED.,.F.,.F.,(4,2,4),(3.50832677987883E-11,0.0126516134091697,
0.0253031507487546),.UNSPECIFIED.);
#22255=B_SPLINE_CURVE_WITH_KNOTS('',3,(#116008,#116009,#116010,#116011,
#116012,#116013),.UNSPECIFIED.,.F.,.F.,(4,2,4),(2.28582008011667E-11,0.0126516133708363,
0.0253031658492592),.UNSPECIFIED.);
#22256=B_SPLINE_CURVE_WITH_KNOTS('',3,(#116033,#116034,#116035,#116036,
#116037,#116038),.UNSPECIFIED.,.F.,.F.,(4,2,4),(4.89625279206728E-11,0.0126516134300723,
0.0253031516310349),.UNSPECIFIED.);
#22257=B_SPLINE_CURVE_WITH_KNOTS('',3,(#116058,#116059,#116060,#116061,
#116062,#116063),.UNSPECIFIED.,.F.,.F.,(4,2,4),(5.84024084571817E-11,0.0126516134275552,
0.0253031615539805),.UNSPECIFIED.);
#22258=B_SPLINE_CURVE_WITH_KNOTS('',3,(#116083,#116084,#116085,#116086,
#116087,#116088),.UNSPECIFIED.,.F.,.F.,(4,2,4),(4.19633384918058E-11,0.01265161340334,
0.0253031729642154),.UNSPECIFIED.);
#22259=B_SPLINE_CURVE_WITH_KNOTS('',3,(#116108,#116109,#116110,#116111,
#116112,#116113),.UNSPECIFIED.,.F.,.F.,(4,2,4),(6.65337760895935E-11,0.0126516134575257,
0.0253031412759839),.UNSPECIFIED.);
#22260=B_SPLINE_CURVE_WITH_KNOTS('',3,(#116133,#116134,#116135,#116136,
#116137,#116138),.UNSPECIFIED.,.F.,.F.,(4,2,4),(0.,0.01265144724142,0.0253027587103005),
 .UNSPECIFIED.);
#22261=B_SPLINE_CURVE_WITH_KNOTS('',3,(#116158,#116159,#116160,#116161,
#116162,#116163),.UNSPECIFIED.,.F.,.F.,(4,2,4),(4.59033859231186E-11,0.0126516134106719,
0.0253031557895132),.UNSPECIFIED.);
#22262=B_SPLINE_CURVE_WITH_KNOTS('',3,(#116183,#116184,#116185,#116186,
#116187,#116188),.UNSPECIFIED.,.F.,.F.,(4,2,4),(3.2887239724366E-11,0.0126516134042047,
0.0253031298135651),.UNSPECIFIED.);
#22263=B_SPLINE_CURVE_WITH_KNOTS('',3,(#116208,#116209,#116210,#116211,
#116212,#116213),.UNSPECIFIED.,.F.,.F.,(4,2,4),(4.46558329558303E-11,0.0126516134319913,
0.0253031460002336),.UNSPECIFIED.);
#22264=B_SPLINE_CURVE_WITH_KNOTS('',3,(#116245,#116246,#116247,#116248,
#116249,#116250),.UNSPECIFIED.,.F.,.F.,(4,2,4),(-0.0253003002535201,-0.0126502136751869,
0.),.UNSPECIFIED.);
#22265=B_SPLINE_CURVE_WITH_KNOTS('',3,(#116257,#116258,#116259,#116260,
#116261,#116262,#116263),.UNSPECIFIED.,.F.,.F.,(4,3,4),(0.423588463701997,
0.428571428571429,0.435775021750426),.UNSPECIFIED.);
#22266=B_SPLINE_CURVE_WITH_KNOTS('',3,(#116292,#116293,#116294,#116295,
#116296,#116297),.UNSPECIFIED.,.F.,.F.,(4,2,4),(-0.0253003344256375,-0.0126502201925933,
0.),.UNSPECIFIED.);
#22267=B_SPLINE_CURVE_WITH_KNOTS('',3,(#116304,#116305,#116306,#116307,
#116308,#116309,#116310),.UNSPECIFIED.,.F.,.F.,(4,3,4),(0.423588463698078,
0.428571428571429,0.435775021750426),.UNSPECIFIED.);
#22268=B_SPLINE_CURVE_WITH_KNOTS('',3,(#116339,#116340,#116341,#116342,
#116343,#116344),.UNSPECIFIED.,.F.,.F.,(4,2,4),(-0.0253003283210845,-0.0126502130868413,
0.),.UNSPECIFIED.);
#22269=B_SPLINE_CURVE_WITH_KNOTS('',3,(#116351,#116352,#116353,#116354,
#116355,#116356,#116357),.UNSPECIFIED.,.F.,.F.,(4,3,4),(0.423588463701574,
0.428571428571429,0.435775021750427),.UNSPECIFIED.);
#22270=B_SPLINE_CURVE_WITH_KNOTS('',3,(#116386,#116387,#116388,#116389,
#116390,#116391),.UNSPECIFIED.,.F.,.F.,(4,2,4),(-0.0253002993995992,-0.0126502117370564,
0.),.UNSPECIFIED.);
#22271=B_SPLINE_CURVE_WITH_KNOTS('',3,(#116398,#116399,#116400,#116401,
#116402,#116403,#116404),.UNSPECIFIED.,.F.,.F.,(4,3,4),(0.423588463702291,
0.428571428571429,0.435775021750427),.UNSPECIFIED.);
#22272=B_SPLINE_CURVE_WITH_KNOTS('',3,(#116433,#116434,#116435,#116436,
#116437,#116438),.UNSPECIFIED.,.F.,.F.,(4,2,4),(-0.0253002995693567,-0.0126502089156248,
0.),.UNSPECIFIED.);
#22273=B_SPLINE_CURVE_WITH_KNOTS('',3,(#116445,#116446,#116447,#116448,
#116449,#116450,#116451),.UNSPECIFIED.,.F.,.F.,(4,3,4),(0.423588463706974,
0.428571428571429,0.435775021750427),.UNSPECIFIED.);
#22274=B_SPLINE_CURVE_WITH_KNOTS('',3,(#116480,#116481,#116482,#116483,
#116484,#116485),.UNSPECIFIED.,.F.,.F.,(4,2,4),(-0.02530030063837,-0.0126502070972325,
0.),.UNSPECIFIED.);
#22275=B_SPLINE_CURVE_WITH_KNOTS('',3,(#116492,#116493,#116494,#116495,
#116496,#116497,#116498),.UNSPECIFIED.,.F.,.F.,(4,3,4),(0.423588463701487,
0.428571428571429,0.435775021750431),.UNSPECIFIED.);
#22276=B_SPLINE_CURVE_WITH_KNOTS('',3,(#116527,#116528,#116529,#116530,
#116531,#116532),.UNSPECIFIED.,.F.,.F.,(4,2,4),(-0.0253002888255266,-0.012650205446942,
0.),.UNSPECIFIED.);
#22277=B_SPLINE_CURVE_WITH_KNOTS('',3,(#116539,#116540,#116541,#116542,
#116543,#116544,#116545),.UNSPECIFIED.,.F.,.F.,(4,3,4),(0.423588463699211,
0.428571428571429,0.435775021750432),.UNSPECIFIED.);
#22278=B_SPLINE_CURVE_WITH_KNOTS('',3,(#116574,#116575,#116576,#116577,
#116578,#116579),.UNSPECIFIED.,.F.,.F.,(4,2,4),(-0.0253002899033947,-0.0126502073537179,
0.),.UNSPECIFIED.);
#22279=B_SPLINE_CURVE_WITH_KNOTS('',3,(#116586,#116587,#116588,#116589,
#116590,#116591,#116592),.UNSPECIFIED.,.F.,.F.,(4,3,4),(0.423588463707525,
0.428571428571429,0.435775021750425),.UNSPECIFIED.);
#22280=B_SPLINE_CURVE_WITH_KNOTS('',3,(#116621,#116622,#116623,#116624,
#116625,#116626),.UNSPECIFIED.,.F.,.F.,(4,2,4),(-0.0253002950377611,-0.0126502055337274,
0.),.UNSPECIFIED.);
#22281=B_SPLINE_CURVE_WITH_KNOTS('',3,(#116633,#116634,#116635,#116636,
#116637,#116638,#116639),.UNSPECIFIED.,.F.,.F.,(4,3,4),(0.423588463701111,
0.428571428571429,0.435775021750424),.UNSPECIFIED.);
#22282=B_SPLINE_CURVE_WITH_KNOTS('',3,(#116668,#116669,#116670,#116671,
#116672,#116673),.UNSPECIFIED.,.F.,.F.,(4,2,4),(-0.0253002956570495,-0.012650211905278,
0.),.UNSPECIFIED.);
#22283=B_SPLINE_CURVE_WITH_KNOTS('',3,(#116680,#116681,#116682,#116683,
#116684,#116685,#116686),.UNSPECIFIED.,.F.,.F.,(4,3,4),(0.423588463700703,
0.428571428571429,0.435775021750423),.UNSPECIFIED.);
#22284=B_SPLINE_CURVE_WITH_KNOTS('',3,(#116715,#116716,#116717,#116718,
#116719,#116720),.UNSPECIFIED.,.F.,.F.,(4,2,4),(-0.0253003154846229,-0.0126502108025514,
0.),.UNSPECIFIED.);
#22285=B_SPLINE_CURVE_WITH_KNOTS('',3,(#116727,#116728,#116729,#116730,
#116731,#116732,#116733),.UNSPECIFIED.,.F.,.F.,(4,3,4),(0.423588463700741,
0.428571428571429,0.435775021750425),.UNSPECIFIED.);
#22286=B_SPLINE_CURVE_WITH_KNOTS('',3,(#116762,#116763,#116764,#116765,
#116766,#116767),.UNSPECIFIED.,.F.,.F.,(4,2,4),(-0.0253003226012023,-0.0126502117300696,
0.),.UNSPECIFIED.);
#22287=B_SPLINE_CURVE_WITH_KNOTS('',3,(#116774,#116775,#116776,#116777,
#116778,#116779,#116780),.UNSPECIFIED.,.F.,.F.,(4,3,4),(0.423588463704446,
0.428571428571429,0.435775021750425),.UNSPECIFIED.);
#22288=B_SPLINE_CURVE_WITH_KNOTS('',3,(#116809,#116810,#116811,#116812,
#116813,#116814),.UNSPECIFIED.,.F.,.F.,(4,2,4),(-0.0253003011424229,-0.0126502110863886,
0.),.UNSPECIFIED.);
#22289=B_SPLINE_CURVE_WITH_KNOTS('',3,(#116821,#116822,#116823,#116824,
#116825,#116826,#116827),.UNSPECIFIED.,.F.,.F.,(4,3,4),(0.42358846370506,
0.428571428571429,0.435775021750424),.UNSPECIFIED.);
#22290=B_SPLINE_CURVE_WITH_KNOTS('',3,(#116856,#116857,#116858,#116859,
#116860,#116861),.UNSPECIFIED.,.F.,.F.,(4,2,4),(-0.0253003126779101,-0.012650207513558,
0.),.UNSPECIFIED.);
#22291=B_SPLINE_CURVE_WITH_KNOTS('',3,(#116868,#116869,#116870,#116871,
#116872,#116873,#116874),.UNSPECIFIED.,.F.,.F.,(4,3,4),(0.423588463700609,
0.428571428571429,0.435775021750423),.UNSPECIFIED.);
#22292=B_SPLINE_CURVE_WITH_KNOTS('',3,(#116900,#116901,#116902,#116903,
#116904,#116905),.UNSPECIFIED.,.F.,.F.,(4,2,4),(-0.0253003114676457,-0.012650210849963,
0.),.UNSPECIFIED.);
#22293=B_SPLINE_CURVE_WITH_KNOTS('',3,(#116935,#116936,#116937,#116938,
#116939,#116940),.UNSPECIFIED.,.F.,.F.,(4,2,4),(-0.0253003381099669,-0.0126502129708172,
0.),.UNSPECIFIED.);
#22294=B_SPLINE_CURVE_WITH_KNOTS('',3,(#116947,#116948,#116949,#116950,
#116951,#116952,#116953),.UNSPECIFIED.,.F.,.F.,(4,3,4),(0.423588463705018,
0.428571428571429,0.435775021750423),.UNSPECIFIED.);
#22295=B_SPLINE_CURVE_WITH_KNOTS('',3,(#116982,#116983,#116984,#116985,
#116986,#116987),.UNSPECIFIED.,.F.,.F.,(4,2,4),(-0.0253002919638189,-0.0126502103961476,
0.),.UNSPECIFIED.);
#22296=B_SPLINE_CURVE_WITH_KNOTS('',3,(#116994,#116995,#116996,#116997,
#116998,#116999,#117000),.UNSPECIFIED.,.F.,.F.,(4,3,4),(0.423588463703294,
0.428571428571429,0.435775021750423),.UNSPECIFIED.);
#22297=B_SPLINE_CURVE_WITH_KNOTS('',3,(#117029,#117030,#117031,#117032,
#117033,#117034),.UNSPECIFIED.,.F.,.F.,(4,2,4),(-0.0253003060377706,-0.0126502066926115,
0.),.UNSPECIFIED.);
#22298=B_SPLINE_CURVE_WITH_KNOTS('',3,(#117041,#117042,#117043,#117044,
#117045,#117046,#117047),.UNSPECIFIED.,.F.,.F.,(4,3,4),(0.423588463707126,
0.428571428571429,0.435775021750423),.UNSPECIFIED.);
#22299=B_SPLINE_CURVE_WITH_KNOTS('',3,(#117076,#117077,#117078,#117079,
#117080,#117081),.UNSPECIFIED.,.F.,.F.,(4,2,4),(-0.0253002904690498,-0.0126502049689941,
0.),.UNSPECIFIED.);
#22300=B_SPLINE_CURVE_WITH_KNOTS('',3,(#117088,#117089,#117090,#117091,
#117092,#117093,#117094),.UNSPECIFIED.,.F.,.F.,(4,3,4),(0.423588463703339,
0.428571428571429,0.435775021750424),.UNSPECIFIED.);
#22301=B_SPLINE_CURVE_WITH_KNOTS('',3,(#117123,#117124,#117125,#117126,
#117127,#117128),.UNSPECIFIED.,.F.,.F.,(4,2,4),(-0.0253002929170949,-0.0126502123732119,
0.),.UNSPECIFIED.);
#22302=B_SPLINE_CURVE_WITH_KNOTS('',3,(#117135,#117136,#117137,#117138,
#117139,#117140,#117141),.UNSPECIFIED.,.F.,.F.,(4,3,4),(0.423588463702277,
0.428571428571429,0.435775021750435),.UNSPECIFIED.);
#22303=B_SPLINE_CURVE_WITH_KNOTS('',3,(#117170,#117171,#117172,#117173,
#117174,#117175),.UNSPECIFIED.,.F.,.F.,(4,2,4),(-0.0253003074016301,-0.0126502132546601,
0.),.UNSPECIFIED.);
#22304=B_SPLINE_CURVE_WITH_KNOTS('',3,(#117182,#117183,#117184,#117185,
#117186,#117187,#117188),.UNSPECIFIED.,.F.,.F.,(4,3,4),(0.423588463700518,
0.428571428571429,0.435775021750425),.UNSPECIFIED.);
#22305=B_SPLINE_CURVE_WITH_KNOTS('',3,(#117217,#117218,#117219,#117220,
#117221,#117222),.UNSPECIFIED.,.F.,.F.,(4,2,4),(-0.0253003088399219,-0.0126502137216067,
0.),.UNSPECIFIED.);
#22306=B_SPLINE_CURVE_WITH_KNOTS('',3,(#117229,#117230,#117231,#117232,
#117233,#117234,#117235),.UNSPECIFIED.,.F.,.F.,(4,3,4),(0.423588463703113,
0.428571428571429,0.435775021750423),.UNSPECIFIED.);
#22307=B_SPLINE_CURVE_WITH_KNOTS('',3,(#117264,#117265,#117266,#117267,
#117268,#117269),.UNSPECIFIED.,.F.,.F.,(4,2,4),(-0.0253004034332267,-0.0126502524469241,
0.),.UNSPECIFIED.);
#22308=B_SPLINE_CURVE_WITH_KNOTS('',3,(#117286,#117287,#117288,#117289,
#117290,#117291,#117292),.UNSPECIFIED.,.F.,.F.,(4,3,4),(0.423588464,0.428571428571429,
0.435775021750423),.UNSPECIFIED.);
#22309=B_SPLINE_CURVE_WITH_KNOTS('',3,(#117312,#117313,#117314,#117315,
#117316,#117317),.UNSPECIFIED.,.F.,.F.,(4,2,4),(-0.0253002982362509,-0.0126502053143726,
0.),.UNSPECIFIED.);
#22310=B_SPLINE_CURVE_WITH_KNOTS('',3,(#117320,#117321,#117322,#117323,
#117324,#117325,#117326),.UNSPECIFIED.,.F.,.F.,(4,3,4),(0.423588463703712,
0.428571428571429,0.435775021750422),.UNSPECIFIED.);
#22311=B_SPLINE_CURVE_WITH_KNOTS('',3,(#117358,#117359,#117360,#117361,
#117362,#117363),.UNSPECIFIED.,.F.,.F.,(4,2,4),(-0.0253003050044024,-0.0126502128753276,
0.),.UNSPECIFIED.);
#22312=B_SPLINE_CURVE_WITH_KNOTS('',3,(#117370,#117371,#117372,#117373,
#117374,#117375,#117376),.UNSPECIFIED.,.F.,.F.,(4,3,4),(0.423588463699629,
0.428571428571429,0.435775021750427),.UNSPECIFIED.);
#22313=B_SPLINE_CURVE_WITH_KNOTS('',3,(#117405,#117406,#117407,#117408,
#117409,#117410),.UNSPECIFIED.,.F.,.F.,(4,2,4),(-0.0253004073418385,-0.0126502524207922,
-2.2591730569621E-11),.UNSPECIFIED.);
#22314=B_SPLINE_CURVE_WITH_KNOTS('',3,(#117417,#117418,#117419,#117420,
#117421,#117422,#117423),.UNSPECIFIED.,.F.,.F.,(4,3,4),(0.423588463703243,
0.428571428571429,0.435775021750423),.UNSPECIFIED.);
#22315=B_SPLINE_CURVE_WITH_KNOTS('',3,(#117452,#117453,#117454,#117455,
#117456,#117457),.UNSPECIFIED.,.F.,.F.,(4,2,4),(-0.0253003262789758,-0.0126502195059414,
0.),.UNSPECIFIED.);
#22316=B_SPLINE_CURVE_WITH_KNOTS('',3,(#117464,#117465,#117466,#117467,
#117468,#117469,#117470),.UNSPECIFIED.,.F.,.F.,(4,3,4),(0.4235884637035,
0.428571428571429,0.435775021750422),.UNSPECIFIED.);
#22317=B_SPLINE_CURVE_WITH_KNOTS('',3,(#117499,#117500,#117501,#117502,
#117503,#117504),.UNSPECIFIED.,.F.,.F.,(4,2,4),(-0.0253003219384624,-0.0126502122908252,
0.),.UNSPECIFIED.);
#22318=B_SPLINE_CURVE_WITH_KNOTS('',3,(#117511,#117512,#117513,#117514,
#117515,#117516,#117517),.UNSPECIFIED.,.F.,.F.,(4,3,4),(0.423588463701606,
0.428571428571429,0.435775021750424),.UNSPECIFIED.);
#22319=B_SPLINE_CURVE_WITH_KNOTS('',3,(#117546,#117547,#117548,#117549,
#117550,#117551),.UNSPECIFIED.,.F.,.F.,(4,2,4),(-0.0253003053942314,-0.012650212995059,
0.),.UNSPECIFIED.);
#22320=B_SPLINE_CURVE_WITH_KNOTS('',3,(#117558,#117559,#117560,#117561,
#117562,#117563,#117564),.UNSPECIFIED.,.F.,.F.,(4,3,4),(0.423588463705113,
0.428571428571429,0.435775021750427),.UNSPECIFIED.);
#22321=B_SPLINE_CURVE_WITH_KNOTS('',3,(#117594,#117595,#117596,#117597,
#117598,#117599),.UNSPECIFIED.,.F.,.F.,(4,2,4),(-0.0253041425103788,-0.0126521901452956,
-6.82617870562119E-9),.UNSPECIFIED.);
#22322=B_SPLINE_CURVE_WITH_KNOTS('',3,(#117631,#117632,#117633,#117634,
#117635,#117636),.UNSPECIFIED.,.F.,.F.,(4,2,4),(-0.0253041425255257,-0.0126521901587595,
-6.82582376385077E-9),.UNSPECIFIED.);
#22323=B_SPLINE_CURVE_WITH_KNOTS('',3,(#117668,#117669,#117670,#117671,
#117672,#117673),.UNSPECIFIED.,.F.,.F.,(4,2,4),(-0.025304142490585,-0.0126521901211421,
-6.82654235223401E-9),.UNSPECIFIED.);
#22324=B_SPLINE_CURVE_WITH_KNOTS('',3,(#117705,#117706,#117707,#117708,
#117709,#117710),.UNSPECIFIED.,.F.,.F.,(4,2,4),(-0.0253041424713178,-0.0126521901284008,
-6.82603369661638E-9),.UNSPECIFIED.);
#22325=B_SPLINE_CURVE_WITH_KNOTS('',3,(#117742,#117743,#117744,#117745,
#117746,#117747),.UNSPECIFIED.,.F.,.F.,(4,2,4),(-0.0253041424469162,-0.0126521900930259,
-6.8265111168031E-9),.UNSPECIFIED.);
#22326=B_SPLINE_CURVE_WITH_KNOTS('',3,(#117779,#117780,#117781,#117782,
#117783,#117784),.UNSPECIFIED.,.F.,.F.,(4,2,4),(-0.0253041424488234,-0.0126521901167656,
-6.82550236816293E-9),.UNSPECIFIED.);
#22327=B_SPLINE_CURVE_WITH_KNOTS('',3,(#117816,#117817,#117818,#117819,
#117820,#117821),.UNSPECIFIED.,.F.,.F.,(4,2,4),(-0.025304142540414,-0.0126521901499399,
-6.82589951228607E-9),.UNSPECIFIED.);
#22328=B_SPLINE_CURVE_WITH_KNOTS('',3,(#117853,#117854,#117855,#117856,
#117857,#117858),.UNSPECIFIED.,.F.,.F.,(4,2,4),(-0.025304142479695,-0.0126521901100803,
-6.82574482005482E-9),.UNSPECIFIED.);
#22329=B_SPLINE_CURVE_WITH_KNOTS('',3,(#117890,#117891,#117892,#117893,
#117894,#117895),.UNSPECIFIED.,.F.,.F.,(4,2,4),(-0.0253041424980153,-0.0126521901257506,
-6.82570476875921E-9),.UNSPECIFIED.);
#22330=B_SPLINE_CURVE_WITH_KNOTS('',3,(#117927,#117928,#117929,#117930,
#117931,#117932),.UNSPECIFIED.,.F.,.F.,(4,2,4),(-0.025304142491032,-0.0126521901125237,
-6.82627537135216E-9),.UNSPECIFIED.);
#22331=B_SPLINE_CURVE_WITH_KNOTS('',3,(#117964,#117965,#117966,#117967,
#117968,#117969),.UNSPECIFIED.,.F.,.F.,(4,2,4),(-0.0253041425312974,-0.0126521901352363,
-6.82676192659271E-9),.UNSPECIFIED.);
#22332=B_SPLINE_CURVE_WITH_KNOTS('',3,(#118001,#118002,#118003,#118004,
#118005,#118006),.UNSPECIFIED.,.F.,.F.,(4,2,4),(-0.0253041424787179,-0.012652190106218,
-6.82538371654662E-9),.UNSPECIFIED.);
#22333=B_SPLINE_CURVE_WITH_KNOTS('',3,(#118038,#118039,#118040,#118041,
#118042,#118043),.UNSPECIFIED.,.F.,.F.,(4,2,4),(-0.0253041424998502,-0.0126521901348214,
-6.82580466801475E-9),.UNSPECIFIED.);
#22334=B_SPLINE_CURVE_WITH_KNOTS('',3,(#118075,#118076,#118077,#118078,
#118079,#118080),.UNSPECIFIED.,.F.,.F.,(4,2,4),(-0.025304142498564,-0.0126521901183685,
-6.82583610814302E-9),.UNSPECIFIED.);
#22335=B_SPLINE_CURVE_WITH_KNOTS('',3,(#118112,#118113,#118114,#118115,
#118116,#118117),.UNSPECIFIED.,.F.,.F.,(4,2,4),(-0.0253041424916259,-0.0126521901166737,
-6.82764770762456E-9),.UNSPECIFIED.);
#22336=B_SPLINE_CURVE_WITH_KNOTS('',3,(#118149,#118150,#118151,#118152,
#118153,#118154),.UNSPECIFIED.,.F.,.F.,(4,2,4),(-0.0253041424690007,-0.0126521901065946,
-6.8259175742269E-9),.UNSPECIFIED.);
#22337=B_SPLINE_CURVE_WITH_KNOTS('',3,(#118186,#118187,#118188,#118189,
#118190,#118191),.UNSPECIFIED.,.F.,.F.,(4,2,4),(-0.0253041425161077,-0.0126521901267836,
-6.8255786092597E-9),.UNSPECIFIED.);
#22338=B_SPLINE_CURVE_WITH_KNOTS('',3,(#118223,#118224,#118225,#118226,
#118227,#118228),.UNSPECIFIED.,.F.,.F.,(4,2,4),(-0.0253041424674938,-0.0126521901252898,
-6.8265300703918E-9),.UNSPECIFIED.);
#22339=B_SPLINE_CURVE_WITH_KNOTS('',3,(#118260,#118261,#118262,#118263,
#118264,#118265),.UNSPECIFIED.,.F.,.F.,(4,2,4),(-0.0253041424683401,-0.0126521901028931,
-6.82533373569383E-9),.UNSPECIFIED.);
#22340=B_SPLINE_CURVE_WITH_KNOTS('',3,(#118297,#118298,#118299,#118300,
#118301,#118302),.UNSPECIFIED.,.F.,.F.,(4,2,4),(-0.0253041425372917,-0.0126521901365104,
-6.82659049427992E-9),.UNSPECIFIED.);
#22341=B_SPLINE_CURVE_WITH_KNOTS('',3,(#118334,#118335,#118336,#118337,
#118338,#118339),.UNSPECIFIED.,.F.,.F.,(4,2,4),(-0.0253041425207301,-0.0126521901506318,
-6.82613092786721E-9),.UNSPECIFIED.);
#22342=B_SPLINE_CURVE_WITH_KNOTS('',3,(#118368,#118369,#118370,#118371,
#118372,#118373),.UNSPECIFIED.,.F.,.F.,(4,2,4),(-0.0253041424491209,-0.0126521901251303,
-6.82641140836715E-9),.UNSPECIFIED.);
#22343=B_SPLINE_CURVE_WITH_KNOTS('',3,(#118399,#118400,#118401,#118402,
#118403,#118404),.UNSPECIFIED.,.F.,.F.,(4,2,4),(-0.0253041424633494,-0.0126521901007878,
-6.82618439551419E-9),.UNSPECIFIED.);
#22344=B_SPLINE_CURVE_WITH_KNOTS('',3,(#118436,#118437,#118438,#118439,
#118440,#118441),.UNSPECIFIED.,.F.,.F.,(4,2,4),(-0.0253041424547078,-0.0126521901059465,
-6.82610486538171E-9),.UNSPECIFIED.);
#22345=B_SPLINE_CURVE_WITH_KNOTS('',3,(#118473,#118474,#118475,#118476,
#118477,#118478),.UNSPECIFIED.,.F.,.F.,(4,2,4),(-0.0253041425072535,-0.0126521901327817,
-6.82570005031136E-9),.UNSPECIFIED.);
#22346=B_SPLINE_CURVE_WITH_KNOTS('',3,(#118510,#118511,#118512,#118513,
#118514,#118515),.UNSPECIFIED.,.F.,.F.,(4,2,4),(-0.0253041425403756,-0.0126521901449272,
-6.82594121156899E-9),.UNSPECIFIED.);
#22347=B_SPLINE_CURVE_WITH_KNOTS('',3,(#118547,#118548,#118549,#118550,
#118551,#118552),.UNSPECIFIED.,.F.,.F.,(4,2,4),(-0.0253041425154124,-0.0126521901361906,
-6.82690581496614E-9),.UNSPECIFIED.);
#22348=B_SPLINE_CURVE_WITH_KNOTS('',3,(#118584,#118585,#118586,#118587,
#118588,#118589),.UNSPECIFIED.,.F.,.F.,(4,2,4),(-0.0253041424813593,-0.0126521901081155,
-6.82638875981745E-9),.UNSPECIFIED.);
#22349=B_SPLINE_CURVE_WITH_KNOTS('',3,(#118621,#118622,#118623,#118624,
#118625,#118626),.UNSPECIFIED.,.F.,.F.,(4,2,4),(-0.0253041424562475,-0.0126521901130813,
-6.82592604661636E-9),.UNSPECIFIED.);
#22350=B_SPLINE_CURVE_WITH_KNOTS('',3,(#118652,#118653,#118654,#118655,
#118656,#118657),.UNSPECIFIED.,.F.,.F.,(4,2,4),(-0.0257378279794269,-0.0126489395998484,
-2.53007684247741E-12),.UNSPECIFIED.);
#22351=B_SPLINE_CURVE_WITH_KNOTS('',3,(#118668,#118669,#118670,#118671,
#118672,#118673,#118674,#118675,#118676,#118677),.UNSPECIFIED.,.F.,.F.,
(4,3,3,4),(0.280362344104003,0.290171079270419,0.29250456354882,0.297785765985179),
 .UNSPECIFIED.);
#22352=B_SPLINE_CURVE_WITH_KNOTS('',3,(#118686,#118687,#118688,#118689,
#118690,#118691),.UNSPECIFIED.,.F.,.F.,(4,2,4),(-0.0257380902616007,-0.0126490009764804,
-3.02954050734883E-11),.UNSPECIFIED.);
#22353=B_SPLINE_CURVE_WITH_KNOTS('',3,(#118702,#118703,#118704,#118705,
#118706,#118707,#118708,#118709,#118710,#118711),.UNSPECIFIED.,.F.,.F.,
(4,3,3,4),(0.28036234408759,0.290171081638759,0.292504563548819,0.29778576598543),
 .UNSPECIFIED.);
#22354=B_SPLINE_CURVE_WITH_KNOTS('',3,(#118720,#118721,#118722,#118723,
#118724,#118725),.UNSPECIFIED.,.F.,.F.,(4,2,4),(-0.0257380523508611,-0.0126490009951788,
-3.81559714379698E-11),.UNSPECIFIED.);
#22355=B_SPLINE_CURVE_WITH_KNOTS('',3,(#118736,#118737,#118738,#118739,
#118740,#118741,#118742,#118743,#118744,#118745),.UNSPECIFIED.,.F.,.F.,
(4,3,3,4),(0.28036234408821,0.290171081007977,0.29250456354882,0.297785765981378),
 .UNSPECIFIED.);
#22356=B_SPLINE_CURVE_WITH_KNOTS('',3,(#118754,#118755,#118756,#118757,
#118758,#118759),.UNSPECIFIED.,.F.,.F.,(4,2,4),(-0.0257380907249933,-0.0126490010455048,
-6.705476104929E-11),.UNSPECIFIED.);
#22357=B_SPLINE_CURVE_WITH_KNOTS('',3,(#118770,#118771,#118772,#118773,
#118774,#118775,#118776,#118777,#118778,#118779),.UNSPECIFIED.,.F.,.F.,
(4,3,3,4),(0.280362344098491,0.290171080844525,0.29250456354882,0.297785765984799),
 .UNSPECIFIED.);
#22358=B_SPLINE_CURVE_WITH_KNOTS('',3,(#118788,#118789,#118790,#118791,
#118792,#118793),.UNSPECIFIED.,.F.,.F.,(4,2,4),(-0.0257380554680191,-0.0126490010287918,
-5.39744776650863E-11),.UNSPECIFIED.);
#22359=B_SPLINE_CURVE_WITH_KNOTS('',3,(#118804,#118805,#118806,#118807,
#118808,#118809,#118810,#118811,#118812,#118813),.UNSPECIFIED.,.F.,.F.,
(4,3,3,4),(0.280362344097552,0.290171073932283,0.29250456354882,0.297785765983655),
 .UNSPECIFIED.);
#22360=B_SPLINE_CURVE_WITH_KNOTS('',3,(#118822,#118823,#118824,#118825,
#118826,#118827),.UNSPECIFIED.,.F.,.F.,(4,2,4),(-0.0257377635808991,-0.0126489324097131,
0.),.UNSPECIFIED.);
#22361=B_SPLINE_CURVE_WITH_KNOTS('',3,(#118838,#118839,#118840,#118841,
#118842,#118843,#118844,#118845,#118846,#118847),.UNSPECIFIED.,.F.,.F.,
(4,3,3,4),(0.280362344104031,0.290171080688324,0.29250456354882,0.297785765995541),
 .UNSPECIFIED.);
#22362=B_SPLINE_CURVE_WITH_KNOTS('',3,(#118856,#118857,#118858,#118859,
#118860,#118861),.UNSPECIFIED.,.F.,.F.,(4,2,4),(-0.025737814464929,-0.0126489362667142,
-7.08981484631721E-13),.UNSPECIFIED.);
#22363=B_SPLINE_CURVE_WITH_KNOTS('',3,(#118872,#118873,#118874,#118875,
#118876,#118877,#118878,#118879,#118880,#118881),.UNSPECIFIED.,.F.,.F.,
(4,3,3,4),(0.280362344094927,0.290171080286353,0.29250456354882,0.297785765985366),
 .UNSPECIFIED.);
#22364=B_SPLINE_CURVE_WITH_KNOTS('',3,(#118890,#118891,#118892,#118893,
#118894,#118895),.UNSPECIFIED.,.F.,.F.,(4,2,4),(-0.0257380533657887,-0.0126490009459565,
-1.05018493901099E-11),.UNSPECIFIED.);
#22365=B_SPLINE_CURVE_WITH_KNOTS('',3,(#118906,#118907,#118908,#118909,
#118910,#118911,#118912,#118913,#118914,#118915),.UNSPECIFIED.,.F.,.F.,
(4,3,3,4),(0.280362344104297,0.290171083310114,0.29250456354882,0.297785765989853),
 .UNSPECIFIED.);
#22366=B_SPLINE_CURVE_WITH_KNOTS('',3,(#118924,#118925,#118926,#118927,
#118928,#118929),.UNSPECIFIED.,.F.,.F.,(4,2,4),(-0.0257377135008693,-0.012648921070624,
0.),.UNSPECIFIED.);
#22367=B_SPLINE_CURVE_WITH_KNOTS('',3,(#118940,#118941,#118942,#118943,
#118944,#118945,#118946,#118947,#118948,#118949),.UNSPECIFIED.,.F.,.F.,
(4,3,3,4),(0.28036234409434,0.290171079087173,0.29250456354882,0.297785765982063),
 .UNSPECIFIED.);
#22368=B_SPLINE_CURVE_WITH_KNOTS('',3,(#118958,#118959,#118960,#118961,
#118962,#118963),.UNSPECIFIED.,.F.,.F.,(4,2,4),(-0.0257380894295356,-0.0126490009412378,
-1.8889799446864E-11),.UNSPECIFIED.);
#22369=B_SPLINE_CURVE_WITH_KNOTS('',3,(#118974,#118975,#118976,#118977,
#118978,#118979,#118980,#118981,#118982,#118983),.UNSPECIFIED.,.F.,.F.,
(4,3,3,4),(0.280362344092742,0.290171082917341,0.29250456354882,0.297785765977771),
 .UNSPECIFIED.);
#22370=B_SPLINE_CURVE_WITH_KNOTS('',3,(#118992,#118993,#118994,#118995,
#118996,#118997),.UNSPECIFIED.,.F.,.F.,(4,2,4),(-0.02573774657654,-0.0126489291735479,
-1.30898243633215E-11),.UNSPECIFIED.);
#22371=B_SPLINE_CURVE_WITH_KNOTS('',3,(#119008,#119009,#119010,#119011,
#119012,#119013,#119014,#119015,#119016,#119017),.UNSPECIFIED.,.F.,.F.,
(4,3,3,4),(0.280362344109662,0.290171080351025,0.29250456354882,0.297785765975465),
 .UNSPECIFIED.);
#22372=B_SPLINE_CURVE_WITH_KNOTS('',3,(#119026,#119027,#119028,#119029,
#119030,#119031),.UNSPECIFIED.,.F.,.F.,(4,2,4),(-0.025738054439123,-0.0126490009490752,
-2.59499158272725E-11),.UNSPECIFIED.);
#22373=B_SPLINE_CURVE_WITH_KNOTS('',3,(#119042,#119043,#119044,#119045,
#119046,#119047,#119048,#119049,#119050,#119051),.UNSPECIFIED.,.F.,.F.,
(4,3,3,4),(0.280362344093884,0.290171081351687,0.29250456354882,0.29778576598458),
 .UNSPECIFIED.);
#22374=B_SPLINE_CURVE_WITH_KNOTS('',3,(#119060,#119061,#119062,#119063,
#119064,#119065),.UNSPECIFIED.,.F.,.F.,(4,2,4),(-0.0257380522579974,-0.0126490009637378,
-1.46792578092914E-11),.UNSPECIFIED.);
#22375=B_SPLINE_CURVE_WITH_KNOTS('',3,(#119076,#119077,#119078,#119079,
#119080,#119081,#119082,#119083,#119084,#119085),.UNSPECIFIED.,.F.,.F.,
(4,3,3,4),(0.280362344086871,0.29017107886419,0.29250456354882,0.297785765975111),
 .UNSPECIFIED.);
#22376=B_SPLINE_CURVE_WITH_KNOTS('',3,(#119094,#119095,#119096,#119097,
#119098,#119099),.UNSPECIFIED.,.F.,.F.,(4,2,4),(-0.0257377497019341,-0.0126489292638499,
0.),.UNSPECIFIED.);
#22377=B_SPLINE_CURVE_WITH_KNOTS('',3,(#119110,#119111,#119112,#119113,
#119114,#119115,#119116,#119117,#119118,#119119),.UNSPECIFIED.,.F.,.F.,
(4,3,3,4),(0.280362344097843,0.290171077351318,0.29250456354882,0.297785765986222),
 .UNSPECIFIED.);
#22378=B_SPLINE_CURVE_WITH_KNOTS('',3,(#119128,#119129,#119130,#119131,
#119132,#119133),.UNSPECIFIED.,.F.,.F.,(4,2,4),(-0.0257380889613719,-0.0126490009095234,
0.),.UNSPECIFIED.);
#22379=B_SPLINE_CURVE_WITH_KNOTS('',3,(#119144,#119145,#119146,#119147,
#119148,#119149,#119150,#119151,#119152,#119153),.UNSPECIFIED.,.F.,.F.,
(4,3,3,4),(0.280362344087793,0.290171079520635,0.29250456354882,0.297785765989929),
 .UNSPECIFIED.);
#22380=B_SPLINE_CURVE_WITH_KNOTS('',3,(#119162,#119163,#119164,#119165,
#119166,#119167),.UNSPECIFIED.,.F.,.F.,(4,2,4),(-0.0257380910289757,-0.0126490010077677,
-4.76177708375047E-11),.UNSPECIFIED.);
#22381=B_SPLINE_CURVE_WITH_KNOTS('',3,(#119178,#119179,#119180,#119181,
#119182,#119183,#119184,#119185,#119186,#119187),.UNSPECIFIED.,.F.,.F.,
(4,3,3,4),(0.280362344092674,0.290171082508215,0.29250456354882,0.2977857659921),
 .UNSPECIFIED.);
#22382=B_SPLINE_CURVE_WITH_KNOTS('',3,(#119196,#119197,#119198,#119199,
#119200,#119201),.UNSPECIFIED.,.F.,.F.,(4,2,4),(-0.0257380538364327,-0.0126490009720209,
-4.27359085619639E-11),.UNSPECIFIED.);
#22383=B_SPLINE_CURVE_WITH_KNOTS('',3,(#119212,#119213,#119214,#119215,
#119216,#119217,#119218,#119219,#119220,#119221),.UNSPECIFIED.,.F.,.F.,
(4,3,3,4),(0.280362344096328,0.290171079866836,0.29250456354882,0.29778576599798),
 .UNSPECIFIED.);
#22384=B_SPLINE_CURVE_WITH_KNOTS('',3,(#119230,#119231,#119232,#119233,
#119234,#119235),.UNSPECIFIED.,.F.,.F.,(4,2,4),(-0.0257380885351855,-0.0126490009655906,
-5.36579392029779E-11),.UNSPECIFIED.);
#22385=B_SPLINE_CURVE_WITH_KNOTS('',3,(#119246,#119247,#119248,#119249,
#119250,#119251,#119252,#119253,#119254,#119255),.UNSPECIFIED.,.F.,.F.,
(4,3,3,4),(0.280362344087404,0.290171079583168,0.29250456354882,0.29778576599091),
 .UNSPECIFIED.);
#22386=B_SPLINE_CURVE_WITH_KNOTS('',3,(#119264,#119265,#119266,#119267,
#119268,#119269),.UNSPECIFIED.,.F.,.F.,(4,2,4),(-0.0257380906026673,-0.0126490009878925,
-2.80112807948818E-11),.UNSPECIFIED.);
#22387=B_SPLINE_CURVE_WITH_KNOTS('',3,(#119280,#119281,#119282,#119283,
#119284,#119285,#119286,#119287,#119288,#119289),.UNSPECIFIED.,.F.,.F.,
(4,3,3,4),(0.28036234409184,0.290171081060908,0.29250456354882,0.297785765984655),
 .UNSPECIFIED.);
#22388=B_SPLINE_CURVE_WITH_KNOTS('',3,(#119298,#119299,#119300,#119301,
#119302,#119303),.UNSPECIFIED.,.F.,.F.,(4,2,4),(-0.0257377476829762,-0.0126489293355879,
0.),.UNSPECIFIED.);
#22389=B_SPLINE_CURVE_WITH_KNOTS('',3,(#119314,#119315,#119316,#119317,
#119318,#119319,#119320,#119321,#119322,#119323),.UNSPECIFIED.,.F.,.F.,
(4,3,3,4),(0.280362344098895,0.290171085510633,0.29250456354882,0.297785765984775),
 .UNSPECIFIED.);
#22390=B_SPLINE_CURVE_WITH_KNOTS('',3,(#119332,#119333,#119334,#119335,
#119336,#119337),.UNSPECIFIED.,.F.,.F.,(4,2,4),(-0.0257377936615723,-0.012648931273962,
0.),.UNSPECIFIED.);
#22391=B_SPLINE_CURVE_WITH_KNOTS('',3,(#119348,#119349,#119350,#119351,
#119352,#119353,#119354,#119355,#119356,#119357),.UNSPECIFIED.,.F.,.F.,
(4,3,3,4),(0.280362344096488,0.290171081541738,0.29250456354882,0.297785765992854),
 .UNSPECIFIED.);
#22392=B_SPLINE_CURVE_WITH_KNOTS('',3,(#119366,#119367,#119368,#119369,
#119370,#119371),.UNSPECIFIED.,.F.,.F.,(4,2,4),(-0.0257380555399184,-0.0126490010070952,
-3.87272332258437E-11),.UNSPECIFIED.);
#22393=B_SPLINE_CURVE_WITH_KNOTS('',3,(#119382,#119383,#119384,#119385,
#119386,#119387,#119388,#119389,#119390,#119391),.UNSPECIFIED.,.F.,.F.,
(4,3,3,4),(0.280362344096632,0.290171080874968,0.29250456354882,0.297785765980618),
 .UNSPECIFIED.);
#22394=B_SPLINE_CURVE_WITH_KNOTS('',3,(#119400,#119401,#119402,#119403,
#119404,#119405),.UNSPECIFIED.,.F.,.F.,(4,2,4),(-0.0257380552031559,-0.0126490009621647,
-2.14355651284581E-11),.UNSPECIFIED.);
#22395=B_SPLINE_CURVE_WITH_KNOTS('',3,(#119416,#119417,#119418,#119419,
#119420,#119421,#119422,#119423,#119424,#119425),.UNSPECIFIED.,.F.,.F.,
(4,3,3,4),(0.280362344102986,0.290171073386061,0.292504563548819,0.297785765974851),
 .UNSPECIFIED.);
#22396=B_SPLINE_CURVE_WITH_KNOTS('',3,(#119434,#119435,#119436,#119437,
#119438,#119439),.UNSPECIFIED.,.F.,.F.,(4,2,4),(-0.0257380531289192,-0.0126490009645852,
-2.70962662030083E-11),.UNSPECIFIED.);
#22397=B_SPLINE_CURVE_WITH_KNOTS('',3,(#119450,#119451,#119452,#119453,
#119454,#119455,#119456,#119457,#119458,#119459),.UNSPECIFIED.,.F.,.F.,
(4,3,3,4),(0.280362344089115,0.290171084276077,0.292504563548822,0.297785765972127),
 .UNSPECIFIED.);
#22398=B_SPLINE_CURVE_WITH_KNOTS('',3,(#119468,#119469,#119470,#119471,
#119472,#119473),.UNSPECIFIED.,.F.,.F.,(4,2,4),(-0.0257380896009897,-0.012649000953846,
-1.29762312006676E-11),.UNSPECIFIED.);
#22399=B_SPLINE_CURVE_WITH_KNOTS('',3,(#119484,#119485,#119486,#119487,
#119488,#119489,#119490,#119491,#119492,#119493),.UNSPECIFIED.,.F.,.F.,
(4,3,3,4),(0.280362344103357,0.290171079085373,0.292504563548816,0.297785765978392),
 .UNSPECIFIED.);
#22400=B_SPLINE_CURVE_WITH_KNOTS('',3,(#119502,#119503,#119504,#119505,
#119506,#119507),.UNSPECIFIED.,.F.,.F.,(4,2,4),(-0.025738053166032,-0.0126490009774138,
-3.8124906009962E-11),.UNSPECIFIED.);
#22401=B_SPLINE_CURVE_WITH_KNOTS('',3,(#119518,#119519,#119520,#119521,
#119522,#119523,#119524,#119525,#119526,#119527),.UNSPECIFIED.,.F.,.F.,
(4,3,3,4),(0.280362344088634,0.290171076593144,0.292504563548811,0.29778576598622),
 .UNSPECIFIED.);
#22402=B_SPLINE_CURVE_WITH_KNOTS('',3,(#119536,#119537,#119538,#119539,
#119540,#119541),.UNSPECIFIED.,.F.,.F.,(4,2,4),(-0.0257380507764179,-0.0126490009275113,
0.),.UNSPECIFIED.);
#22403=B_SPLINE_CURVE_WITH_KNOTS('',3,(#119552,#119553,#119554,#119555,
#119556,#119557,#119558,#119559,#119560,#119561),.UNSPECIFIED.,.F.,.F.,
(4,3,3,4),(0.280362344090312,0.290171084260232,0.292504563548813,0.297785765977126),
 .UNSPECIFIED.);
#22404=B_SPLINE_CURVE_WITH_KNOTS('',3,(#119570,#119571,#119572,#119573,
#119574,#119575),.UNSPECIFIED.,.F.,.F.,(4,2,4),(-0.0257380885569789,-0.0126490009347652,
-1.58122993865195E-11),.UNSPECIFIED.);
#22405=B_SPLINE_CURVE_WITH_KNOTS('',3,(#119586,#119587,#119588,#119589,
#119590,#119591,#119592,#119593,#119594,#119595),.UNSPECIFIED.,.F.,.F.,
(4,3,3,4),(0.280362344110013,0.290171077184626,0.292504563548815,0.297785765989047),
 .UNSPECIFIED.);
#22406=B_SPLINE_CURVE_WITH_KNOTS('',3,(#119604,#119605,#119606,#119607,
#119608,#119609),.UNSPECIFIED.,.F.,.F.,(4,2,4),(-0.0257380525083116,-0.0126490009941628,
-2.24978022322908E-11),.UNSPECIFIED.);
#22407=B_SPLINE_CURVE_WITH_KNOTS('',3,(#119620,#119621,#119622,#119623,
#119624,#119625,#119626,#119627,#119628,#119629),.UNSPECIFIED.,.F.,.F.,
(4,3,3,4),(0.280362344001298,0.290171046132489,0.29250456354882,0.297785765999036),
 .UNSPECIFIED.);
#22408=B_SPLINE_CURVE_WITH_KNOTS('',3,(#119638,#119639,#119640,#119641,
#119642,#119643,#119644,#119645,#119646,#119647),.UNSPECIFIED.,.F.,.F.,
(4,3,3,4),(1.78416752250298E-15,8.70313175311398E-5,0.000170023930203073,
0.000253018981535489),.UNSPECIFIED.);
#22409=B_SPLINE_CURVE_WITH_KNOTS('',3,(#119658,#119659,#119660,#119661,
#119662,#119663,#119664,#119665,#119666,#119667),.UNSPECIFIED.,.F.,.F.,
(4,3,3,4),(0.487259899834934,0.497067956779899,0.5,0.504719756176226),
 .UNSPECIFIED.);
#22410=B_SPLINE_CURVE_WITH_KNOTS('',3,(#119676,#119677,#119678,#119679,
#119680,#119681,#119682,#119683,#119684,#119685),.UNSPECIFIED.,.F.,.F.,
(4,3,3,4),(3.41332323048545E-14,8.70313175545581E-5,0.000170023930246138,
0.000253018981134818),.UNSPECIFIED.);
#22411=B_SPLINE_CURVE_WITH_KNOTS('',3,(#119696,#119697,#119698,#119699,
#119700,#119701,#119702,#119703,#119704,#119705),.UNSPECIFIED.,.F.,.F.,
(4,3,3,4),(0.487259899830027,0.497067953928199,0.5,0.504719756176227),
 .UNSPECIFIED.);
#22412=B_SPLINE_CURVE_WITH_KNOTS('',3,(#119714,#119715,#119716,#119717,
#119718,#119719,#119720,#119721,#119722,#119723),.UNSPECIFIED.,.F.,.F.,
(4,3,3,4),(2.45274570368324E-14,8.70313177460311E-5,0.000170023930143113,
0.000253018980672992),.UNSPECIFIED.);
#22413=B_SPLINE_CURVE_WITH_KNOTS('',3,(#119734,#119735,#119736,#119737,
#119738,#119739,#119740,#119741,#119742,#119743),.UNSPECIFIED.,.F.,.F.,
(4,3,3,4),(0.487259899841302,0.497067955279116,0.5,0.504719756176227),
 .UNSPECIFIED.);
#22414=B_SPLINE_CURVE_WITH_KNOTS('',3,(#119752,#119753,#119754,#119755,
#119756,#119757,#119758,#119759,#119760,#119761),.UNSPECIFIED.,.F.,.F.,
(4,3,3,4),(1.70470283076348E-14,8.70313174616613E-5,0.000170023930255742,
0.000253018981768342),.UNSPECIFIED.);
#22415=B_SPLINE_CURVE_WITH_KNOTS('',3,(#119772,#119773,#119774,#119775,
#119776,#119777,#119778,#119779,#119780,#119781),.UNSPECIFIED.,.F.,.F.,
(4,3,3,4),(0.487259899828108,0.497067956582658,0.5,0.504719756176227),
 .UNSPECIFIED.);
#22416=B_SPLINE_CURVE_WITH_KNOTS('',3,(#119790,#119791,#119792,#119793,
#119794,#119795,#119796,#119797,#119798,#119799),.UNSPECIFIED.,.F.,.F.,
(4,3,3,4),(8.61735280637014E-14,8.70313175901959E-5,0.000170023930245986,
0.000253018981322021),.UNSPECIFIED.);
#22417=B_SPLINE_CURVE_WITH_KNOTS('',3,(#119810,#119811,#119812,#119813,
#119814,#119815,#119816,#119817,#119818,#119819),.UNSPECIFIED.,.F.,.F.,
(4,3,3,4),(0.487259899824588,0.497067952915038,0.5,0.504719756176227),
 .UNSPECIFIED.);
#22418=B_SPLINE_CURVE_WITH_KNOTS('',3,(#119828,#119829,#119830,#119831,
#119832,#119833,#119834,#119835,#119836,#119837),.UNSPECIFIED.,.F.,.F.,
(4,3,3,4),(6.4801676788079E-14,8.70313176737056E-5,0.000170023930339139,
0.000253018981507554),.UNSPECIFIED.);
#22419=B_SPLINE_CURVE_WITH_KNOTS('',3,(#119848,#119849,#119850,#119851,
#119852,#119853,#119854,#119855,#119856,#119857),.UNSPECIFIED.,.F.,.F.,
(4,3,3,4),(0.487259899837411,0.497067955332477,0.5,0.504719756176226),
 .UNSPECIFIED.);
#22420=B_SPLINE_CURVE_WITH_KNOTS('',3,(#119866,#119867,#119868,#119869,
#119870,#119871,#119872,#119873,#119874,#119875),.UNSPECIFIED.,.F.,.F.,
(4,3,3,4),(4.46624994070207E-14,8.703131763642E-5,0.0001700239303354,0.000253018981642442),
 .UNSPECIFIED.);
#22421=B_SPLINE_CURVE_WITH_KNOTS('',3,(#119886,#119887,#119888,#119889,
#119890,#119891,#119892,#119893,#119894,#119895),.UNSPECIFIED.,.F.,.F.,
(4,3,3,4),(0.487259899847783,0.497067955749335,0.5,0.504719756176227),
 .UNSPECIFIED.);
#22422=B_SPLINE_CURVE_WITH_KNOTS('',3,(#119904,#119905,#119906,#119907,
#119908,#119909,#119910,#119911,#119912,#119913),.UNSPECIFIED.,.F.,.F.,
(4,3,3,4),(1.90268839248483E-14,8.70313177274394E-5,0.000170023930133409,
0.000253018980982867),.UNSPECIFIED.);
#22423=B_SPLINE_CURVE_WITH_KNOTS('',3,(#119924,#119925,#119926,#119927,
#119928,#119929,#119930,#119931,#119932,#119933),.UNSPECIFIED.,.F.,.F.,
(4,3,3,4),(0.487259899837452,0.497067951424618,0.5,0.504719756176228),
 .UNSPECIFIED.);
#22424=B_SPLINE_CURVE_WITH_KNOTS('',3,(#119942,#119943,#119944,#119945,
#119946,#119947,#119948,#119949,#119950,#119951),.UNSPECIFIED.,.F.,.F.,
(4,3,3,4),(1.63355867732691E-14,8.70313177195555E-5,0.000170023930283018,
0.000253018981197976),.UNSPECIFIED.);
#22425=B_SPLINE_CURVE_WITH_KNOTS('',3,(#119962,#119963,#119964,#119965,
#119966,#119967,#119968,#119969,#119970,#119971),.UNSPECIFIED.,.F.,.F.,
(4,3,3,4),(0.487259899844168,0.497067950844091,0.5,0.504719756176228),
 .UNSPECIFIED.);
#22426=B_SPLINE_CURVE_WITH_KNOTS('',3,(#119980,#119981,#119982,#119983,
#119984,#119985,#119986,#119987,#119988,#119989),.UNSPECIFIED.,.F.,.F.,
(4,3,3,4),(4.32089986161599E-14,8.70313176778163E-5,0.000170023930202668,
0.000253018981062845),.UNSPECIFIED.);
#22427=B_SPLINE_CURVE_WITH_KNOTS('',3,(#120000,#120001,#120002,#120003,
#120004,#120005,#120006,#120007,#120008,#120009),.UNSPECIFIED.,.F.,.F.,
(4,3,3,4),(0.487259899833474,0.497067957211732,0.5,0.504719756176228),
 .UNSPECIFIED.);
#22428=B_SPLINE_CURVE_WITH_KNOTS('',3,(#120018,#120019,#120020,#120021,
#120022,#120023,#120024,#120025,#120026,#120027),.UNSPECIFIED.,.F.,.F.,
(4,3,3,4),(5.85668130751604E-14,8.70313175937449E-5,0.000170023930273888,
0.000253018981217468),.UNSPECIFIED.);
#22429=B_SPLINE_CURVE_WITH_KNOTS('',3,(#120038,#120039,#120040,#120041,
#120042,#120043,#120044,#120045,#120046,#120047),.UNSPECIFIED.,.F.,.F.,
(4,3,3,4),(0.487259899836209,0.497067955102255,0.5,0.504719756176228),
 .UNSPECIFIED.);
#22430=B_SPLINE_CURVE_WITH_KNOTS('',3,(#120056,#120057,#120058,#120059,
#120060,#120061,#120062,#120063,#120064,#120065),.UNSPECIFIED.,.F.,.F.,
(4,3,3,4),(7.01370277151711E-14,8.70313175559056E-5,0.000170023930128497,
0.00025301898233016),.UNSPECIFIED.);
#22431=B_SPLINE_CURVE_WITH_KNOTS('',3,(#120076,#120077,#120078,#120079,
#120080,#120081,#120082,#120083,#120084,#120085),.UNSPECIFIED.,.F.,.F.,
(4,3,3,4),(0.487259899821166,0.497067952690467,0.5,0.504719756176228),
 .UNSPECIFIED.);
#22432=B_SPLINE_CURVE_WITH_KNOTS('',3,(#120094,#120095,#120096,#120097,
#120098,#120099,#120100,#120101,#120102,#120103),.UNSPECIFIED.,.F.,.F.,
(4,3,3,4),(3.4379490863589E-14,8.70313176981463E-5,0.000170023930243521,
0.000253018982813477),.UNSPECIFIED.);
#22433=B_SPLINE_CURVE_WITH_KNOTS('',3,(#120114,#120115,#120116,#120117,
#120118,#120119,#120120,#120121,#120122,#120123),.UNSPECIFIED.,.F.,.F.,
(4,3,3,4),(0.487259899831263,0.497067954216751,0.5,0.504719756173849),
 .UNSPECIFIED.);
#22434=B_SPLINE_CURVE_WITH_KNOTS('',3,(#120132,#120133,#120134,#120135,
#120136,#120137,#120138,#120139,#120140,#120141),.UNSPECIFIED.,.F.,.F.,
(4,3,3,4),(5.43013114251202E-14,8.70313176102924E-5,0.000170023930127259,
0.000253018981186722),.UNSPECIFIED.);
#22435=B_SPLINE_CURVE_WITH_KNOTS('',3,(#120152,#120153,#120154,#120155,
#120156,#120157,#120158,#120159,#120160,#120161),.UNSPECIFIED.,.F.,.F.,
(4,3,3,4),(0.48725989983763,0.497067952795034,0.5,0.504719756176228),
 .UNSPECIFIED.);
#22436=B_SPLINE_CURVE_WITH_KNOTS('',3,(#120170,#120171,#120172,#120173,
#120174,#120175,#120176,#120177,#120178,#120179),.UNSPECIFIED.,.F.,.F.,
(4,3,3,4),(2.41375655958049E-14,8.70313176307348E-5,0.000170023930272469,
0.00025301898123237),.UNSPECIFIED.);
#22437=B_SPLINE_CURVE_WITH_KNOTS('',3,(#120190,#120191,#120192,#120193,
#120194,#120195,#120196,#120197,#120198,#120199),.UNSPECIFIED.,.F.,.F.,
(4,3,3,4),(0.487259899839516,0.497067955878832,0.5,0.504719756176228),
 .UNSPECIFIED.);
#22438=B_SPLINE_CURVE_WITH_KNOTS('',3,(#120208,#120209,#120210,#120211,
#120212,#120213,#120214,#120215,#120216,#120217),.UNSPECIFIED.,.F.,.F.,
(4,3,3,4),(5.85991331726249E-14,8.70313175998023E-5,0.000170023930181731,
0.000253018980908884),.UNSPECIFIED.);
#22439=B_SPLINE_CURVE_WITH_KNOTS('',3,(#120228,#120229,#120230,#120231,
#120232,#120233,#120234,#120235,#120236,#120237),.UNSPECIFIED.,.F.,.F.,
(4,3,3,4),(0.487259899833153,0.497067954345318,0.5,0.50471975617623),
 .UNSPECIFIED.);
#22440=B_SPLINE_CURVE_WITH_KNOTS('',3,(#120246,#120247,#120248,#120249,
#120250,#120251,#120252,#120253,#120254,#120255),.UNSPECIFIED.,.F.,.F.,
(4,3,3,4),(2.95380358239764E-15,8.70313176641763E-5,0.000170023930380612,
0.000253018981633287),.UNSPECIFIED.);
#22441=B_SPLINE_CURVE_WITH_KNOTS('',3,(#120266,#120267,#120268,#120269,
#120270,#120271,#120272,#120273,#120274,#120275),.UNSPECIFIED.,.F.,.F.,
(4,3,3,4),(0.487259899831205,0.497067957272829,0.5,0.504719756176228),
 .UNSPECIFIED.);
#22442=B_SPLINE_CURVE_WITH_KNOTS('',3,(#120284,#120285,#120286,#120287,
#120288,#120289,#120290,#120291,#120292,#120293),.UNSPECIFIED.,.F.,.F.,
(4,3,3,4),(6.94791745557739E-14,8.70313178044004E-5,0.00017002393033166,
0.000253018982522185),.UNSPECIFIED.);
#22443=B_SPLINE_CURVE_WITH_KNOTS('',3,(#120304,#120305,#120306,#120307,
#120308,#120309,#120310,#120311,#120312,#120313),.UNSPECIFIED.,.F.,.F.,
(4,3,3,4),(0.487259899845777,0.497067954429802,0.5,0.504719756176228),
 .UNSPECIFIED.);
#22444=B_SPLINE_CURVE_WITH_KNOTS('',3,(#120322,#120323,#120324,#120325,
#120326,#120327,#120328,#120329,#120330,#120331),.UNSPECIFIED.,.F.,.F.,
(4,3,3,4),(1.05931133367487E-14,8.70313177939862E-5,0.000170023930133989,
0.000253018980682019),.UNSPECIFIED.);
#22445=B_SPLINE_CURVE_WITH_KNOTS('',3,(#120342,#120343,#120344,#120345,
#120346,#120347,#120348,#120349,#120350,#120351),.UNSPECIFIED.,.F.,.F.,
(4,3,3,4),(0.487259899839067,0.497067957978687,0.5,0.504719756176227),
 .UNSPECIFIED.);
#22446=B_SPLINE_CURVE_WITH_KNOTS('',3,(#120360,#120361,#120362,#120363,
#120364,#120365,#120366,#120367,#120368,#120369),.UNSPECIFIED.,.F.,.F.,
(4,3,3,4),(5.08094850759228E-14,8.70313176670443E-5,0.000170023930229356,
0.000253018982807892),.UNSPECIFIED.);
#22447=B_SPLINE_CURVE_WITH_KNOTS('',3,(#120380,#120381,#120382,#120383,
#120384,#120385,#120386,#120387,#120388,#120389),.UNSPECIFIED.,.F.,.F.,
(4,3,3,4),(0.487259899830092,0.497067957473563,0.5,0.504719756176228),
 .UNSPECIFIED.);
#22448=B_SPLINE_CURVE_WITH_KNOTS('',3,(#120398,#120399,#120400,#120401,
#120402,#120403,#120404,#120405,#120406,#120407),.UNSPECIFIED.,.F.,.F.,
(4,3,3,4),(2.04923360970009E-14,8.70313176284759E-5,0.000170023930120259,
0.000253018980880619),.UNSPECIFIED.);
#22449=B_SPLINE_CURVE_WITH_KNOTS('',3,(#120418,#120419,#120420,#120421,
#120422,#120423,#120424,#120425,#120426,#120427),.UNSPECIFIED.,.F.,.F.,
(4,3,3,4),(0.487259899843493,0.497067955675083,0.5,0.504719756176228),
 .UNSPECIFIED.);
#22450=B_SPLINE_CURVE_WITH_KNOTS('',3,(#120436,#120437,#120438,#120439,
#120440,#120441,#120442,#120443,#120444,#120445),.UNSPECIFIED.,.F.,.F.,
(4,3,3,4),(1.46986958788117E-14,8.7031317872638E-5,0.000170023930227489,
0.000253018980856544),.UNSPECIFIED.);
#22451=B_SPLINE_CURVE_WITH_KNOTS('',3,(#120456,#120457,#120458,#120459,
#120460,#120461,#120462,#120463,#120464,#120465),.UNSPECIFIED.,.F.,.F.,
(4,3,3,4),(0.487259899836764,0.497067953025495,0.5,0.504719756176228),
 .UNSPECIFIED.);
#22452=B_SPLINE_CURVE_WITH_KNOTS('',3,(#120474,#120475,#120476,#120477,
#120478,#120479,#120480,#120481,#120482,#120483),.UNSPECIFIED.,.F.,.F.,
(4,3,3,4),(2.60369811470792E-14,8.70313175752751E-5,0.000170023930220742,
0.000253018981334628),.UNSPECIFIED.);
#22453=B_SPLINE_CURVE_WITH_KNOTS('',3,(#120494,#120495,#120496,#120497,
#120498,#120499,#120500,#120501,#120502,#120503),.UNSPECIFIED.,.F.,.F.,
(4,3,3,4),(0.487259899825349,0.497067954507092,0.5,0.504719756176228),
 .UNSPECIFIED.);
#22454=B_SPLINE_CURVE_WITH_KNOTS('',3,(#120512,#120513,#120514,#120515,
#120516,#120517,#120518,#120519,#120520,#120521),.UNSPECIFIED.,.F.,.F.,
(4,3,3,4),(4.69113067077989E-15,8.7031317644139E-5,0.000170023930301228,
0.000253018981429277),.UNSPECIFIED.);
#22455=B_SPLINE_CURVE_WITH_KNOTS('',3,(#120532,#120533,#120534,#120535,
#120536,#120537,#120538,#120539,#120540,#120541),.UNSPECIFIED.,.F.,.F.,
(4,3,3,4),(0.487259899844095,0.497067955819474,0.5,0.50471975617627),
 .UNSPECIFIED.);
#22456=B_SPLINE_CURVE_WITH_KNOTS('',3,(#120550,#120551,#120552,#120553,
#120554,#120555,#120556,#120557,#120558,#120559),.UNSPECIFIED.,.F.,.F.,
(4,3,3,4),(3.4930305600279E-14,8.70313175915354E-5,0.000170023930262545,
0.000253018983021755),.UNSPECIFIED.);
#22457=B_SPLINE_CURVE_WITH_KNOTS('',3,(#120570,#120571,#120572,#120573,
#120574,#120575,#120576,#120577,#120578,#120579),.UNSPECIFIED.,.F.,.F.,
(4,3,3,4),(0.487259899834473,0.497067957474287,0.5,0.504719756169005),
 .UNSPECIFIED.);
#22458=B_SPLINE_CURVE_WITH_KNOTS('',3,(#120588,#120589,#120590,#120591,
#120592,#120593,#120594,#120595,#120596,#120597),.UNSPECIFIED.,.F.,.F.,
(4,3,3,4),(4.37878311359043E-14,8.70313175424253E-5,0.000170023930052117,
0.00025301898111264),.UNSPECIFIED.);
#22459=B_SPLINE_CURVE_WITH_KNOTS('',3,(#120608,#120609,#120610,#120611,
#120612,#120613,#120614,#120615,#120616,#120617),.UNSPECIFIED.,.F.,.F.,
(4,3,3,4),(0.48725989983526,0.497067953412607,0.5,0.504719756176228),
 .UNSPECIFIED.);
#22460=B_SPLINE_CURVE_WITH_KNOTS('',3,(#120626,#120627,#120628,#120629,
#120630,#120631,#120632,#120633,#120634,#120635),.UNSPECIFIED.,.F.,.F.,
(4,3,3,4),(4.39618627902034E-14,8.70313175297401E-5,0.00017002392999475,
0.000253018980685548),.UNSPECIFIED.);
#22461=B_SPLINE_CURVE_WITH_KNOTS('',3,(#120646,#120647,#120648,#120649,
#120650,#120651,#120652,#120653,#120654,#120655),.UNSPECIFIED.,.F.,.F.,
(4,3,3,4),(0.487259899838253,0.497067957395083,0.5,0.504719756176302),
 .UNSPECIFIED.);
#22462=B_SPLINE_CURVE_WITH_KNOTS('',3,(#120664,#120665,#120666,#120667,
#120668,#120669,#120670,#120671,#120672,#120673),.UNSPECIFIED.,.F.,.F.,
(4,3,3,4),(3.42316589032284E-14,8.70313175711171E-5,0.000170023930344364,
0.00025301898162994),.UNSPECIFIED.);
#22463=B_SPLINE_CURVE_WITH_KNOTS('',3,(#120684,#120685,#120686,#120687,
#120688,#120689,#120690,#120691,#120692,#120693),.UNSPECIFIED.,.F.,.F.,
(4,3,3,4),(0.487259899828096,0.497067950830241,0.5,0.504719756176228),
 .UNSPECIFIED.);
#22464=B_SPLINE_CURVE_WITH_KNOTS('',3,(#120702,#120703,#120704,#120705,
#120706,#120707,#120708,#120709,#120710,#120711),.UNSPECIFIED.,.F.,.F.,
(4,3,3,4),(2.21213965425014E-14,8.7031317560607E-5,0.000170023930173682,
0.000253018981224706),.UNSPECIFIED.);
#22465=B_SPLINE_CURVE_WITH_KNOTS('',3,(#120722,#120723,#120724,#120725,
#120726,#120727,#120728,#120729,#120730,#120731),.UNSPECIFIED.,.F.,.F.,
(4,3,3,4),(0.48725989985259,0.49706793422622,0.5,0.504719756176227),
 .UNSPECIFIED.);
#22466=B_SPLINE_CURVE_WITH_KNOTS('',3,(#120742,#120743,#120744,#120745,
#120746,#120747),.UNSPECIFIED.,.F.,.F.,(4,2,4),(-0.025296973443844,-0.0126483645724683,
0.),.UNSPECIFIED.);
#22467=B_SPLINE_CURVE_WITH_KNOTS('',3,(#120764,#120765,#120766,#120767,
#120768,#120769,#120770),.UNSPECIFIED.,.F.,.F.,(4,3,4),(0.280433082999158,
0.285714285714286,0.292621536168419),.UNSPECIFIED.);
#22468=B_SPLINE_CURVE_WITH_KNOTS('',3,(#120771,#120772,#120773,#120774,
#120775,#120776),.UNSPECIFIED.,.F.,.F.,(4,2,4),(0.,0.0126482240284275,0.0252963923636814),
 .UNSPECIFIED.);
#22469=B_SPLINE_CURVE_WITH_KNOTS('',3,(#120807,#120808,#120809,#120810,
#120811,#120812,#120813),.UNSPECIFIED.,.F.,.F.,(4,3,4),(0.280433082999159,
0.285714285714286,0.292621536173129),.UNSPECIFIED.);
#22470=B_SPLINE_CURVE_WITH_KNOTS('',3,(#120814,#120815,#120816,#120817,
#120818,#120819),.UNSPECIFIED.,.F.,.F.,(4,2,4),(0.,0.0126482072034737,0.0252962990115169),
 .UNSPECIFIED.);
#22471=B_SPLINE_CURVE_WITH_KNOTS('',3,(#120850,#120851,#120852,#120853,
#120854,#120855,#120856),.UNSPECIFIED.,.F.,.F.,(4,3,4),(0.280433082999158,
0.285714285714286,0.292621536172136),.UNSPECIFIED.);
#22472=B_SPLINE_CURVE_WITH_KNOTS('',3,(#120857,#120858,#120859,#120860,
#120861,#120862),.UNSPECIFIED.,.F.,.F.,(4,2,4),(0.,0.0126483645169886,0.025296944392472),
 .UNSPECIFIED.);
#22473=B_SPLINE_CURVE_WITH_KNOTS('',3,(#120893,#120894,#120895,#120896,
#120897,#120898,#120899),.UNSPECIFIED.,.F.,.F.,(4,3,4),(0.280433083101589,
0.285714285714286,0.292621536174457),.UNSPECIFIED.);
#22474=B_SPLINE_CURVE_WITH_KNOTS('',3,(#120900,#120901,#120902,#120903,
#120904,#120905),.UNSPECIFIED.,.F.,.F.,(4,2,4),(0.,0.0126483645307332,0.0252969476147786),
 .UNSPECIFIED.);
#22475=B_SPLINE_CURVE_WITH_KNOTS('',3,(#120936,#120937,#120938,#120939,
#120940,#120941,#120942),.UNSPECIFIED.,.F.,.F.,(4,3,4),(0.280433082999175,
0.285714285714286,0.292621536174032),.UNSPECIFIED.);
#22476=B_SPLINE_CURVE_WITH_KNOTS('',3,(#120943,#120944,#120945,#120946,
#120947,#120948),.UNSPECIFIED.,.F.,.F.,(4,2,4),(0.,0.0126482419654942,0.0252964414925125),
 .UNSPECIFIED.);
#22477=B_SPLINE_CURVE_WITH_KNOTS('',3,(#120979,#120980,#120981,#120982,
#120983,#120984,#120985),.UNSPECIFIED.,.F.,.F.,(4,3,4),(0.280433082999174,
0.285714285714286,0.292621536173361),.UNSPECIFIED.);
#22478=B_SPLINE_CURVE_WITH_KNOTS('',3,(#120986,#120987,#120988,#120989,
#120990,#120991),.UNSPECIFIED.,.F.,.F.,(4,2,4),(0.,0.0126482228971245,0.0252963611714074),
 .UNSPECIFIED.);
#22479=B_SPLINE_CURVE_WITH_KNOTS('',3,(#121020,#121021,#121022,#121023,
#121024,#121025),.UNSPECIFIED.,.F.,.F.,(4,2,4),(0.,0.0126483645137511,0.02529697344602),
 .UNSPECIFIED.);
#22480=B_SPLINE_CURVE_WITH_KNOTS('',3,(#121050,#121051,#121052,#121053,
#121054,#121055,#121056),.UNSPECIFIED.,.F.,.F.,(4,3,4),(0.280433082999157,
0.285714285714286,0.29262153617651),.UNSPECIFIED.);
#22481=B_SPLINE_CURVE_WITH_KNOTS('',3,(#121057,#121058,#121059,#121060,
#121061,#121062),.UNSPECIFIED.,.F.,.F.,(4,2,4),(0.,0.0126482295569889,0.025296415324654),
 .UNSPECIFIED.);
#22482=B_SPLINE_CURVE_WITH_KNOTS('',3,(#121093,#121094,#121095,#121096,
#121097,#121098,#121099),.UNSPECIFIED.,.F.,.F.,(4,3,4),(0.280433082999157,
0.285714285714286,0.292621536168029),.UNSPECIFIED.);
#22483=B_SPLINE_CURVE_WITH_KNOTS('',3,(#121100,#121101,#121102,#121103,
#121104,#121105),.UNSPECIFIED.,.F.,.F.,(4,2,4),(0.,0.0126482304749268,0.0252963910036341),
 .UNSPECIFIED.);
#22484=B_SPLINE_CURVE_WITH_KNOTS('',3,(#121136,#121137,#121138,#121139,
#121140,#121141,#121142),.UNSPECIFIED.,.F.,.F.,(4,3,4),(0.280433082999158,
0.285714285714286,0.292621536177272),.UNSPECIFIED.);
#22485=B_SPLINE_CURVE_WITH_KNOTS('',3,(#121143,#121144,#121145,#121146,
#121147,#121148),.UNSPECIFIED.,.F.,.F.,(4,2,4),(0.,0.0126482262354878,0.0252964015583787),
 .UNSPECIFIED.);
#22486=B_SPLINE_CURVE_WITH_KNOTS('',3,(#121179,#121180,#121181,#121182,
#121183,#121184,#121185),.UNSPECIFIED.,.F.,.F.,(4,3,4),(0.280433082999159,
0.285714285714286,0.292621536173701),.UNSPECIFIED.);
#22487=B_SPLINE_CURVE_WITH_KNOTS('',3,(#121186,#121187,#121188,#121189,
#121190,#121191),.UNSPECIFIED.,.F.,.F.,(4,2,4),(0.,0.0126482164487877,0.0252963341335591),
 .UNSPECIFIED.);
#22488=B_SPLINE_CURVE_WITH_KNOTS('',3,(#121222,#121223,#121224,#121225,
#121226,#121227,#121228),.UNSPECIFIED.,.F.,.F.,(4,3,4),(0.280433082999158,
0.285714285714286,0.292621536174503),.UNSPECIFIED.);
#22489=B_SPLINE_CURVE_WITH_KNOTS('',3,(#121229,#121230,#121231,#121232,
#121233,#121234),.UNSPECIFIED.,.F.,.F.,(4,2,4),(0.,0.0126482283807774,0.0252963831989578),
 .UNSPECIFIED.);
#22490=B_SPLINE_CURVE_WITH_KNOTS('',3,(#121265,#121266,#121267,#121268,
#121269,#121270,#121271),.UNSPECIFIED.,.F.,.F.,(4,3,4),(0.280433083100916,
0.285714285714286,0.292621536173779),.UNSPECIFIED.);
#22491=B_SPLINE_CURVE_WITH_KNOTS('',3,(#121272,#121273,#121274,#121275,
#121276,#121277),.UNSPECIFIED.,.F.,.F.,(4,2,4),(0.,0.0126482384135485,0.025296451907903),
 .UNSPECIFIED.);
#22492=B_SPLINE_CURVE_WITH_KNOTS('',3,(#121308,#121309,#121310,#121311,
#121312,#121313,#121314),.UNSPECIFIED.,.F.,.F.,(4,3,4),(0.280433082999158,
0.285714285714286,0.292621536171013),.UNSPECIFIED.);
#22493=B_SPLINE_CURVE_WITH_KNOTS('',3,(#121315,#121316,#121317,#121318,
#121319,#121320),.UNSPECIFIED.,.F.,.F.,(4,2,4),(0.,0.0126482186825741,0.0252963434366669),
 .UNSPECIFIED.);
#22494=B_SPLINE_CURVE_WITH_KNOTS('',3,(#121351,#121352,#121353,#121354,
#121355,#121356,#121357),.UNSPECIFIED.,.F.,.F.,(4,3,4),(0.280433082999157,
0.285714285714286,0.292621536174076),.UNSPECIFIED.);
#22495=B_SPLINE_CURVE_WITH_KNOTS('',3,(#121358,#121359,#121360,#121361,
#121362,#121363),.UNSPECIFIED.,.F.,.F.,(4,2,4),(0.,0.012648236612633,0.0252964210419331),
 .UNSPECIFIED.);
#22496=B_SPLINE_CURVE_WITH_KNOTS('',3,(#121394,#121395,#121396,#121397,
#121398,#121399,#121400),.UNSPECIFIED.,.F.,.F.,(4,3,4),(0.280433082999157,
0.285714285714286,0.292621536176529),.UNSPECIFIED.);
#22497=B_SPLINE_CURVE_WITH_KNOTS('',3,(#121401,#121402,#121403,#121404,
#121405,#121406),.UNSPECIFIED.,.F.,.F.,(4,2,4),(0.,0.0126482376119629,0.0252964485949374),
 .UNSPECIFIED.);
#22498=B_SPLINE_CURVE_WITH_KNOTS('',3,(#121437,#121438,#121439,#121440,
#121441,#121442,#121443),.UNSPECIFIED.,.F.,.F.,(4,3,4),(0.280433082999158,
0.285714285714286,0.292621536169643),.UNSPECIFIED.);
#22499=B_SPLINE_CURVE_WITH_KNOTS('',3,(#121444,#121445,#121446,#121447,
#121448,#121449),.UNSPECIFIED.,.F.,.F.,(4,2,4),(0.,0.0126482392731302,0.025296427401708),
 .UNSPECIFIED.);
#22500=B_SPLINE_CURVE_WITH_KNOTS('',3,(#121480,#121481,#121482,#121483,
#121484,#121485,#121486),.UNSPECIFIED.,.F.,.F.,(4,3,4),(0.280433082999157,
0.285714285714286,0.292621536170285),.UNSPECIFIED.);
#22501=B_SPLINE_CURVE_WITH_KNOTS('',3,(#121487,#121488,#121489,#121490,
#121491,#121492),.UNSPECIFIED.,.F.,.F.,(4,2,4),(0.,0.0126482325288649,0.0252964275932703),
 .UNSPECIFIED.);
#22502=B_SPLINE_CURVE_WITH_KNOTS('',3,(#121523,#121524,#121525,#121526,
#121527,#121528,#121529),.UNSPECIFIED.,.F.,.F.,(4,3,4),(0.280433082999157,
0.285714285714286,0.292621536172335),.UNSPECIFIED.);
#22503=B_SPLINE_CURVE_WITH_KNOTS('',3,(#121530,#121531,#121532,#121533,
#121534,#121535),.UNSPECIFIED.,.F.,.F.,(4,2,4),(0.,0.0126482279436222,0.0252963817618714),
 .UNSPECIFIED.);
#22504=B_SPLINE_CURVE_WITH_KNOTS('',3,(#121566,#121567,#121568,#121569,
#121570,#121571,#121572),.UNSPECIFIED.,.F.,.F.,(4,3,4),(0.280433082999181,
0.285714285714286,0.292621536171598),.UNSPECIFIED.);
#22505=B_SPLINE_CURVE_WITH_KNOTS('',3,(#121573,#121574,#121575,#121576,
#121577,#121578),.UNSPECIFIED.,.F.,.F.,(4,2,4),(0.,0.0126482391688131,0.0252964280773304),
 .UNSPECIFIED.);
#22506=B_SPLINE_CURVE_WITH_KNOTS('',3,(#121609,#121610,#121611,#121612,
#121613,#121614,#121615),.UNSPECIFIED.,.F.,.F.,(4,3,4),(0.280433082999157,
0.285714285714286,0.29262153616907),.UNSPECIFIED.);
#22507=B_SPLINE_CURVE_WITH_KNOTS('',3,(#121616,#121617,#121618,#121619,
#121620,#121621),.UNSPECIFIED.,.F.,.F.,(4,2,4),(0.,0.0126482300329072,0.0252964171687196),
 .UNSPECIFIED.);
#22508=B_SPLINE_CURVE_WITH_KNOTS('',3,(#121652,#121653,#121654,#121655,
#121656,#121657,#121658),.UNSPECIFIED.,.F.,.F.,(4,3,4),(0.280433082999157,
0.285714285714286,0.292621536200935),.UNSPECIFIED.);
#22509=B_SPLINE_CURVE_WITH_KNOTS('',3,(#121659,#121660,#121661,#121662,
#121663,#121664),.UNSPECIFIED.,.F.,.F.,(4,2,4),(0.,0.012648227663072,0.0252962420019202),
 .UNSPECIFIED.);
#22510=B_SPLINE_CURVE_WITH_KNOTS('',3,(#121696,#121697,#121698,#121699,
#121700,#121701,#121702),.UNSPECIFIED.,.F.,.F.,(4,3,4),(0.280433082999157,
0.285714285714286,0.292621536180055),.UNSPECIFIED.);
#22511=B_SPLINE_CURVE_WITH_KNOTS('',3,(#121703,#121704,#121705,#121706,
#121707,#121708),.UNSPECIFIED.,.F.,.F.,(4,2,4),(0.,0.0126482209953414,0.0252963798315834),
 .UNSPECIFIED.);
#22512=B_SPLINE_CURVE_WITH_KNOTS('',3,(#121738,#121739,#121740,#121741,
#121742,#121743,#121744),.UNSPECIFIED.,.F.,.F.,(4,3,4),(0.280433082999159,
0.285714285714286,0.292621536173583),.UNSPECIFIED.);
#22513=B_SPLINE_CURVE_WITH_KNOTS('',3,(#121745,#121746,#121747,#121748,
#121749,#121750),.UNSPECIFIED.,.F.,.F.,(4,2,4),(0.,0.0126483644971886,0.025296973432917),
 .UNSPECIFIED.);
#22514=B_SPLINE_CURVE_WITH_KNOTS('',3,(#121781,#121782,#121783,#121784,
#121785,#121786,#121787),.UNSPECIFIED.,.F.,.F.,(4,3,4),(0.28043308299918,
0.285714285714286,0.292621536175091),.UNSPECIFIED.);
#22515=B_SPLINE_CURVE_WITH_KNOTS('',3,(#121788,#121789,#121790,#121791,
#121792,#121793),.UNSPECIFIED.,.F.,.F.,(4,2,4),(0.,0.0126482219417105,0.0252963558424426),
 .UNSPECIFIED.);
#22516=B_SPLINE_CURVE_WITH_KNOTS('',3,(#121824,#121825,#121826,#121827,
#121828,#121829,#121830),.UNSPECIFIED.,.F.,.F.,(4,3,4),(0.280433082999174,
0.285714285714286,0.292621536175529),.UNSPECIFIED.);
#22517=B_SPLINE_CURVE_WITH_KNOTS('',3,(#121831,#121832,#121833,#121834,
#121835,#121836),.UNSPECIFIED.,.F.,.F.,(4,2,4),(0.,0.0126482161227793,0.025296332460369),
 .UNSPECIFIED.);
#22518=B_SPLINE_CURVE_WITH_KNOTS('',3,(#121867,#121868,#121869,#121870,
#121871,#121872,#121873),.UNSPECIFIED.,.F.,.F.,(4,3,4),(0.28043308310138,
0.285714285714286,0.29262153617452),.UNSPECIFIED.);
#22519=B_SPLINE_CURVE_WITH_KNOTS('',3,(#121874,#121875,#121876,#121877,
#121878,#121879),.UNSPECIFIED.,.F.,.F.,(4,2,4),(0.,0.0126482098067578,0.0252963055994983),
 .UNSPECIFIED.);
#22520=B_SPLINE_CURVE_WITH_KNOTS('',3,(#121910,#121911,#121912,#121913,
#121914,#121915,#121916),.UNSPECIFIED.,.F.,.F.,(4,3,4),(0.280433082999171,
0.285714285714286,0.292621536166647),.UNSPECIFIED.);
#22521=B_SPLINE_CURVE_WITH_KNOTS('',3,(#121917,#121918,#121919,#121920,
#121921,#121922),.UNSPECIFIED.,.F.,.F.,(4,2,4),(0.,0.0126482038455709,0.0252963088950863),
 .UNSPECIFIED.);
#22522=B_SPLINE_CURVE_WITH_KNOTS('',3,(#121942,#121943,#121944,#121945,
#121946,#121947,#121948),.UNSPECIFIED.,.F.,.F.,(4,3,4),(0.280433082999158,
0.285714285714286,0.292621536174994),.UNSPECIFIED.);
#22523=B_SPLINE_CURVE_WITH_KNOTS('',3,(#121971,#121972,#121973,#121974,
#121975,#121976),.UNSPECIFIED.,.F.,.F.,(4,2,4),(5.6486889799842E-11,0.0126507152822395,
0.0253011859160019),.UNSPECIFIED.);
#22524=B_SPLINE_CURVE_WITH_KNOTS('',3,(#121993,#121994,#121995,#121996,
#121997,#121998,#121999),.UNSPECIFIED.,.F.,.F.,(4,3,4),(0.487155140750429,
0.491874896926655,0.499350532547867),.UNSPECIFIED.);
#22525=B_SPLINE_CURVE_WITH_KNOTS('',3,(#122000,#122001,#122002,#122003,
#122004,#122005),.UNSPECIFIED.,.F.,.F.,(4,2,4),(-0.0253011697080569,-0.0126507154103212,
-1.97071942098503E-11),.UNSPECIFIED.);
#22526=B_SPLINE_CURVE_WITH_KNOTS('',3,(#122032,#122033,#122034,#122035,
#122036,#122037,#122038),.UNSPECIFIED.,.F.,.F.,(4,3,4),(0.487155140750429,
0.491874896926656,0.499350532544037),.UNSPECIFIED.);
#22527=B_SPLINE_CURVE_WITH_KNOTS('',3,(#122039,#122040,#122041,#122042,
#122043,#122044),.UNSPECIFIED.,.F.,.F.,(4,2,4),(-0.0253011722932434,-0.0126507154307367,
-1.9720863830841E-11),.UNSPECIFIED.);
#22528=B_SPLINE_CURVE_WITH_KNOTS('',3,(#122071,#122072,#122073,#122074,
#122075,#122076,#122077),.UNSPECIFIED.,.F.,.F.,(4,3,4),(0.487155140750429,
0.491874896926656,0.49935053256116),.UNSPECIFIED.);
#22529=B_SPLINE_CURVE_WITH_KNOTS('',3,(#122078,#122079,#122080,#122081,
#122082,#122083),.UNSPECIFIED.,.F.,.F.,(4,2,4),(-0.0253011660901163,-0.0126507154029974,
-1.91734475518679E-11),.UNSPECIFIED.);
#22530=B_SPLINE_CURVE_WITH_KNOTS('',3,(#122110,#122111,#122112,#122113,
#122114,#122115,#122116),.UNSPECIFIED.,.F.,.F.,(4,3,4),(0.487155140750429,
0.491874896926656,0.499350532539288),.UNSPECIFIED.);
#22531=B_SPLINE_CURVE_WITH_KNOTS('',3,(#122117,#122118,#122119,#122120,
#122121,#122122),.UNSPECIFIED.,.F.,.F.,(4,2,4),(-0.0253011685668152,-0.0126507154315906,
-2.02164084084355E-11),.UNSPECIFIED.);
#22532=B_SPLINE_CURVE_WITH_KNOTS('',3,(#122149,#122150,#122151,#122152,
#122153,#122154,#122155),.UNSPECIFIED.,.F.,.F.,(4,3,4),(0.487155140750429,
0.491874896926656,0.499350532553138),.UNSPECIFIED.);
#22533=B_SPLINE_CURVE_WITH_KNOTS('',3,(#122156,#122157,#122158,#122159,
#122160,#122161),.UNSPECIFIED.,.F.,.F.,(4,2,4),(-0.0253011700469523,-0.0126507154194713,
-1.94551180721092E-11),.UNSPECIFIED.);
#22534=B_SPLINE_CURVE_WITH_KNOTS('',3,(#122188,#122189,#122190,#122191,
#122192,#122193,#122194),.UNSPECIFIED.,.F.,.F.,(4,3,4),(0.487155140750429,
0.491874896926655,0.499350532552386),.UNSPECIFIED.);
#22535=B_SPLINE_CURVE_WITH_KNOTS('',3,(#122195,#122196,#122197,#122198,
#122199,#122200),.UNSPECIFIED.,.F.,.F.,(4,2,4),(-0.0253011664286715,-0.0126507154206639,
-1.996768375645E-11),.UNSPECIFIED.);
#22536=B_SPLINE_CURVE_WITH_KNOTS('',3,(#122227,#122228,#122229,#122230,
#122231,#122232,#122233),.UNSPECIFIED.,.F.,.F.,(4,3,4),(0.48715514075043,
0.491874896926657,0.499350532549246),.UNSPECIFIED.);
#22537=B_SPLINE_CURVE_WITH_KNOTS('',3,(#122234,#122235,#122236,#122237,
#122238,#122239),.UNSPECIFIED.,.F.,.F.,(4,2,4),(-0.0253011651441201,-0.0126507153978601,
-1.92457993986039E-11),.UNSPECIFIED.);
#22538=B_SPLINE_CURVE_WITH_KNOTS('',3,(#122266,#122267,#122268,#122269,
#122270,#122271,#122272),.UNSPECIFIED.,.F.,.F.,(4,3,4),(0.48715514075043,
0.491874896926658,0.499350532543253),.UNSPECIFIED.);
#22539=B_SPLINE_CURVE_WITH_KNOTS('',3,(#122273,#122274,#122275,#122276,
#122277,#122278),.UNSPECIFIED.,.F.,.F.,(4,2,4),(-0.0253011651017512,-0.0126507154393088,
-2.06919863188215E-11),.UNSPECIFIED.);
#22540=B_SPLINE_CURVE_WITH_KNOTS('',3,(#122305,#122306,#122307,#122308,
#122309,#122310,#122311),.UNSPECIFIED.,.F.,.F.,(4,3,4),(0.48715514075043,
0.491874896926658,0.499350532556912),.UNSPECIFIED.);
#22541=B_SPLINE_CURVE_WITH_KNOTS('',3,(#122312,#122313,#122314,#122315,
#122316,#122317),.UNSPECIFIED.,.F.,.F.,(4,2,4),(-0.0253011716954516,-0.0126507154317354,
-1.93546428883806E-11),.UNSPECIFIED.);
#22542=B_SPLINE_CURVE_WITH_KNOTS('',3,(#122344,#122345,#122346,#122347,
#122348,#122349,#122350),.UNSPECIFIED.,.F.,.F.,(4,3,4),(0.48715514075043,
0.491874896926658,0.499350532547458),.UNSPECIFIED.);
#22543=B_SPLINE_CURVE_WITH_KNOTS('',3,(#122351,#122352,#122353,#122354,
#122355,#122356),.UNSPECIFIED.,.F.,.F.,(4,2,4),(-0.0253011677574891,-0.0126507153846773,
-1.91839218122158E-11),.UNSPECIFIED.);
#22544=B_SPLINE_CURVE_WITH_KNOTS('',3,(#122383,#122384,#122385,#122386,
#122387,#122388,#122389),.UNSPECIFIED.,.F.,.F.,(4,3,4),(0.48715514075043,
0.491874896926658,0.499350532553758),.UNSPECIFIED.);
#22545=B_SPLINE_CURVE_WITH_KNOTS('',3,(#122390,#122391,#122392,#122393,
#122394,#122395),.UNSPECIFIED.,.F.,.F.,(4,2,4),(-0.0253011737432215,-0.0126507154147995,
-1.93375662704831E-11),.UNSPECIFIED.);
#22546=B_SPLINE_CURVE_WITH_KNOTS('',3,(#122422,#122423,#122424,#122425,
#122426,#122427,#122428),.UNSPECIFIED.,.F.,.F.,(4,3,4),(0.48715514075043,
0.491874896926658,0.499350532548837),.UNSPECIFIED.);
#22547=B_SPLINE_CURVE_WITH_KNOTS('',3,(#122429,#122430,#122431,#122432,
#122433,#122434),.UNSPECIFIED.,.F.,.F.,(4,2,4),(-0.0253011673355543,-0.0126507154295212,
-1.97535911239388E-11),.UNSPECIFIED.);
#22548=B_SPLINE_CURVE_WITH_KNOTS('',3,(#122461,#122462,#122463,#122464,
#122465,#122466,#122467),.UNSPECIFIED.,.F.,.F.,(4,3,4),(0.48715514075043,
0.491874896926658,0.499350532552698),.UNSPECIFIED.);
#22549=B_SPLINE_CURVE_WITH_KNOTS('',3,(#122468,#122469,#122470,#122471,
#122472,#122473),.UNSPECIFIED.,.F.,.F.,(4,2,4),(-0.0253011661288702,-0.0126507154045511,
-1.98644260762659E-11),.UNSPECIFIED.);
#22550=B_SPLINE_CURVE_WITH_KNOTS('',3,(#122498,#122499,#122500,#122501,
#122502,#122503),.UNSPECIFIED.,.F.,.F.,(4,2,4),(-0.0253011704521776,-0.0126507154221742,
0.),.UNSPECIFIED.);
#22551=B_SPLINE_CURVE_WITH_KNOTS('',3,(#122524,#122525,#122526,#122527,
#122528,#122529,#122530),.UNSPECIFIED.,.F.,.F.,(4,3,4),(0.48715514075043,
0.491874896926658,0.499350532549079),.UNSPECIFIED.);
#22552=B_SPLINE_CURVE_WITH_KNOTS('',3,(#122531,#122532,#122533,#122534,
#122535,#122536),.UNSPECIFIED.,.F.,.F.,(4,2,4),(-0.0253011669290482,-0.0126507153766242,
-1.8918901167897E-11),.UNSPECIFIED.);
#22553=B_SPLINE_CURVE_WITH_KNOTS('',3,(#122563,#122564,#122565,#122566,
#122567,#122568,#122569),.UNSPECIFIED.,.F.,.F.,(4,3,4),(0.48715514075043,
0.49187489692666,0.499350532564458),.UNSPECIFIED.);
#22554=B_SPLINE_CURVE_WITH_KNOTS('',3,(#122570,#122571,#122572,#122573,
#122574,#122575),.UNSPECIFIED.,.F.,.F.,(4,2,4),(-0.0253011658638423,-0.0126507154016559,
-1.91625708356735E-11),.UNSPECIFIED.);
#22555=B_SPLINE_CURVE_WITH_KNOTS('',3,(#122602,#122603,#122604,#122605,
#122606,#122607,#122608),.UNSPECIFIED.,.F.,.F.,(4,3,4),(0.48715514075043,
0.491874896926658,0.499350532549946),.UNSPECIFIED.);
#22556=B_SPLINE_CURVE_WITH_KNOTS('',3,(#122609,#122610,#122611,#122612,
#122613,#122614),.UNSPECIFIED.,.F.,.F.,(4,2,4),(-0.0253011702441171,-0.0126507154203099,
-1.94096856642734E-11),.UNSPECIFIED.);
#22557=B_SPLINE_CURVE_WITH_KNOTS('',3,(#122641,#122642,#122643,#122644,
#122645,#122646,#122647),.UNSPECIFIED.,.F.,.F.,(4,3,4),(0.48715514075043,
0.491874896926658,0.499350532550294),.UNSPECIFIED.);
#22558=B_SPLINE_CURVE_WITH_KNOTS('',3,(#122648,#122649,#122650,#122651,
#122652,#122653),.UNSPECIFIED.,.F.,.F.,(4,2,4),(-0.0253011727064749,-0.0126507154429837,
-1.9765349079659E-11),.UNSPECIFIED.);
#22559=B_SPLINE_CURVE_WITH_KNOTS('',3,(#122680,#122681,#122682,#122683,
#122684,#122685,#122686),.UNSPECIFIED.,.F.,.F.,(4,3,4),(0.48715514075043,
0.491874896926657,0.499350532550754),.UNSPECIFIED.);
#22560=B_SPLINE_CURVE_WITH_KNOTS('',3,(#122687,#122688,#122689,#122690,
#122691,#122692),.UNSPECIFIED.,.F.,.F.,(4,2,4),(-0.0253011673119558,-0.0126507154173595,
-1.93358315470071E-11),.UNSPECIFIED.);
#22561=B_SPLINE_CURVE_WITH_KNOTS('',3,(#122719,#122720,#122721,#122722,
#122723,#122724,#122725),.UNSPECIFIED.,.F.,.F.,(4,3,4),(0.48715514075043,
0.491874896926658,0.499350532545838),.UNSPECIFIED.);
#22562=B_SPLINE_CURVE_WITH_KNOTS('',3,(#122726,#122727,#122728,#122729,
#122730,#122731),.UNSPECIFIED.,.F.,.F.,(4,2,4),(-0.0253011657593956,-0.0126507154253452,
-2.02232536272717E-11),.UNSPECIFIED.);
#22563=B_SPLINE_CURVE_WITH_KNOTS('',3,(#122758,#122759,#122760,#122761,
#122762,#122763,#122764),.UNSPECIFIED.,.F.,.F.,(4,3,4),(0.48715514075043,
0.491874896926658,0.49935053255401),.UNSPECIFIED.);
#22564=B_SPLINE_CURVE_WITH_KNOTS('',3,(#122765,#122766,#122767,#122768,
#122769,#122770),.UNSPECIFIED.,.F.,.F.,(4,2,4),(-0.0253011655833842,-0.0126507154013209,
-1.94681874787772E-11),.UNSPECIFIED.);
#22565=B_SPLINE_CURVE_WITH_KNOTS('',3,(#122797,#122798,#122799,#122800,
#122801,#122802,#122803),.UNSPECIFIED.,.F.,.F.,(4,3,4),(0.48715514075043,
0.491874896926658,0.499350532553005),.UNSPECIFIED.);
#22566=B_SPLINE_CURVE_WITH_KNOTS('',3,(#122804,#122805,#122806,#122807,
#122808,#122809),.UNSPECIFIED.,.F.,.F.,(4,2,4),(-0.0253011660469114,-0.0126507153993854,
-1.99408337064888E-11),.UNSPECIFIED.);
#22567=B_SPLINE_CURVE_WITH_KNOTS('',3,(#122836,#122837,#122838,#122839,
#122840,#122841,#122842),.UNSPECIFIED.,.F.,.F.,(4,3,4),(0.48715514075043,
0.491874896926658,0.499350532550904),.UNSPECIFIED.);
#22568=B_SPLINE_CURVE_WITH_KNOTS('',3,(#122843,#122844,#122845,#122846,
#122847,#122848),.UNSPECIFIED.,.F.,.F.,(4,2,4),(-0.0253011738441044,-0.0126507154351814,
-1.93815970217504E-11),.UNSPECIFIED.);
#22569=B_SPLINE_CURVE_WITH_KNOTS('',3,(#122875,#122876,#122877,#122878,
#122879,#122880,#122881),.UNSPECIFIED.,.F.,.F.,(4,3,4),(0.48715514075043,
0.4918748969267,0.499350532551012),.UNSPECIFIED.);
#22570=B_SPLINE_CURVE_WITH_KNOTS('',3,(#122882,#122883,#122884,#122885,
#122886,#122887),.UNSPECIFIED.,.F.,.F.,(4,2,4),(-0.0253011672758786,-0.0126507154040944,
-1.97396612944267E-11),.UNSPECIFIED.);
#22571=B_SPLINE_CURVE_WITH_KNOTS('',3,(#122914,#122915,#122916,#122917,
#122918,#122919,#122920),.UNSPECIFIED.,.F.,.F.,(4,3,4),(0.48715514075043,
0.491874896926665,0.499350532557549),.UNSPECIFIED.);
#22572=B_SPLINE_CURVE_WITH_KNOTS('',3,(#122921,#122922,#122923,#122924,
#122925,#122926),.UNSPECIFIED.,.F.,.F.,(4,2,4),(-0.0253011654071048,-0.0126507153906956,
-1.85380495676402E-11),.UNSPECIFIED.);
#22573=B_SPLINE_CURVE_WITH_KNOTS('',3,(#122953,#122954,#122955,#122956,
#122957,#122958,#122959),.UNSPECIFIED.,.F.,.F.,(4,3,4),(0.48715514075043,
0.491874896926658,0.499350532557718),.UNSPECIFIED.);
#22574=B_SPLINE_CURVE_WITH_KNOTS('',3,(#122960,#122961,#122962,#122963,
#122964,#122965),.UNSPECIFIED.,.F.,.F.,(4,2,4),(-0.0253011666204797,-0.0126507154156547,
-1.98272821771983E-11),.UNSPECIFIED.);
#22575=B_SPLINE_CURVE_WITH_KNOTS('',3,(#122992,#122993,#122994,#122995,
#122996,#122997,#122998),.UNSPECIFIED.,.F.,.F.,(4,3,4),(0.48715514075043,
0.491874896926732,0.499350532545763),.UNSPECIFIED.);
#22576=B_SPLINE_CURVE_WITH_KNOTS('',3,(#122999,#123000,#123001,#123002,
#123003,#123004),.UNSPECIFIED.,.F.,.F.,(4,2,4),(-0.025301170657439,-0.0126507154100243,
-1.93889730659702E-11),.UNSPECIFIED.);
#22577=B_SPLINE_CURVE_WITH_KNOTS('',3,(#123031,#123032,#123033,#123034,
#123035,#123036,#123037),.UNSPECIFIED.,.F.,.F.,(4,3,4),(0.487155140750422,
0.49187489692665,0.49935053255025),.UNSPECIFIED.);
#22578=B_SPLINE_CURVE_WITH_KNOTS('',3,(#123038,#123039,#123040,#123041,
#123042,#123043),.UNSPECIFIED.,.F.,.F.,(4,2,4),(-0.0253011644296503,-0.0126507153998242,
-1.97393976164584E-11),.UNSPECIFIED.);
#22579=B_SPLINE_CURVE_WITH_KNOTS('',3,(#123059,#123060,#123061,#123062,
#123063,#123064,#123065),.UNSPECIFIED.,.F.,.F.,(4,3,4),(0.487155140750429,
0.491874896926656,0.499350532736371),.UNSPECIFIED.);
#22580=B_SPLINE_CURVE_WITH_KNOTS('',3,(#123088,#123089,#123090,#123091,
#123092,#123093),.UNSPECIFIED.,.F.,.F.,(4,2,4),(-0.025303642668681,-0.0126519393733511,
-4.93077419172483E-11),.UNSPECIFIED.);
#22581=B_SPLINE_CURVE_WITH_KNOTS('',3,(#123106,#123107,#123108,#123109,
#123110,#123111),.UNSPECIFIED.,.F.,.F.,(4,2,4),(5.52409649967746E-11,0.0126519401309947,
0.0253036433584956),.UNSPECIFIED.);
#22582=B_SPLINE_CURVE_WITH_KNOTS('',3,(#123131,#123132,#123133,#123134,
#123135,#123136),.UNSPECIFIED.,.F.,.F.,(4,2,4),(4.64000489761306E-11,0.0126519401026762,
0.0253036433353798),.UNSPECIFIED.);
#22583=B_SPLINE_CURVE_WITH_KNOTS('',3,(#123156,#123157,#123158,#123159,
#123160,#123161),.UNSPECIFIED.,.F.,.F.,(4,2,4),(3.79562095965757E-11,0.0126519401116534,
0.0253036433278902),.UNSPECIFIED.);
#22584=B_SPLINE_CURVE_WITH_KNOTS('',3,(#123181,#123182,#123183,#123184,
#123185,#123186),.UNSPECIFIED.,.F.,.F.,(4,2,4),(4.376061431345E-11,0.0126519401323004,
0.0253036433382299),.UNSPECIFIED.);
#22585=B_SPLINE_CURVE_WITH_KNOTS('',3,(#123206,#123207,#123208,#123209,
#123210,#123211),.UNSPECIFIED.,.F.,.F.,(4,2,4),(3.26183525282446E-11,0.0126519400760263,
0.0253036432997477),.UNSPECIFIED.);
#22586=B_SPLINE_CURVE_WITH_KNOTS('',3,(#123231,#123232,#123233,#123234,
#123235,#123236),.UNSPECIFIED.,.F.,.F.,(4,2,4),(1.78618766070422E-11,0.0126519400801105,
0.0253036432850591),.UNSPECIFIED.);
#22587=B_SPLINE_CURVE_WITH_KNOTS('',3,(#123256,#123257,#123258,#123259,
#123260,#123261),.UNSPECIFIED.,.F.,.F.,(4,2,4),(3.39279843673074E-11,0.012651940111472,
0.0253036433222914),.UNSPECIFIED.);
#22588=B_SPLINE_CURVE_WITH_KNOTS('',3,(#123281,#123282,#123283,#123284,
#123285,#123286),.UNSPECIFIED.,.F.,.F.,(4,2,4),(6.98571819218591E-11,0.0126519401540513,
0.0253036433771993),.UNSPECIFIED.);
#22589=B_SPLINE_CURVE_WITH_KNOTS('',3,(#123306,#123307,#123308,#123309,
#123310,#123311),.UNSPECIFIED.,.F.,.F.,(4,2,4),(3.01248371585428E-11,0.0126519400709428,
0.0253036432886881),.UNSPECIFIED.);
#22590=B_SPLINE_CURVE_WITH_KNOTS('',3,(#123331,#123332,#123333,#123334,
#123335,#123336),.UNSPECIFIED.,.F.,.F.,(4,2,4),(4.97562181263154E-11,0.0126519401134231,
0.0253036433393194),.UNSPECIFIED.);
#22591=B_SPLINE_CURVE_WITH_KNOTS('',3,(#123356,#123357,#123358,#123359,
#123360,#123361),.UNSPECIFIED.,.F.,.F.,(4,2,4),(5.67425406489046E-11,0.0126519401208395,
0.025303643305537),.UNSPECIFIED.);
#22592=B_SPLINE_CURVE_WITH_KNOTS('',3,(#123381,#123382,#123383,#123384,
#123385,#123386),.UNSPECIFIED.,.F.,.F.,(4,2,4),(5.49109704738617E-11,0.01265194014448,
0.0253036433621979),.UNSPECIFIED.);
#22593=B_SPLINE_CURVE_WITH_KNOTS('',3,(#123406,#123407,#123408,#123409,
#123410,#123411),.UNSPECIFIED.,.F.,.F.,(4,2,4),(4.33377220651269E-11,0.0126519400952753,
0.0253036433155586),.UNSPECIFIED.);
#22594=B_SPLINE_CURVE_WITH_KNOTS('',3,(#123431,#123432,#123433,#123434,
#123435,#123436),.UNSPECIFIED.,.F.,.F.,(4,2,4),(7.15206814981132E-11,0.0126519401294615,
0.0253036433132997),.UNSPECIFIED.);
#22595=B_SPLINE_CURVE_WITH_KNOTS('',3,(#123456,#123457,#123458,#123459,
#123460,#123461),.UNSPECIFIED.,.F.,.F.,(4,2,4),(4.56809817642753E-11,0.0126519401030549,
0.0253036433198694),.UNSPECIFIED.);
#22596=B_SPLINE_CURVE_WITH_KNOTS('',3,(#123481,#123482,#123483,#123484,
#123485,#123486),.UNSPECIFIED.,.F.,.F.,(4,2,4),(3.72911203642004E-11,0.0126519400850595,
0.0253036433156901),.UNSPECIFIED.);
#22597=B_SPLINE_CURVE_WITH_KNOTS('',3,(#123506,#123507,#123508,#123509,
#123510,#123511),.UNSPECIFIED.,.F.,.F.,(4,2,4),(3.15364244988512E-11,0.0126519400951044,
0.025303643329179),.UNSPECIFIED.);
#22598=B_SPLINE_CURVE_WITH_KNOTS('',3,(#123531,#123532,#123533,#123534,
#123535,#123536),.UNSPECIFIED.,.F.,.F.,(4,2,4),(2.15246642150142E-11,0.0126519400837596,
0.0253036433411845),.UNSPECIFIED.);
#22599=B_SPLINE_CURVE_WITH_KNOTS('',3,(#123556,#123557,#123558,#123559,
#123560,#123561),.UNSPECIFIED.,.F.,.F.,(4,2,4),(5.25951651961309E-11,0.0126519401235544,
0.0253036433427751),.UNSPECIFIED.);
#22600=B_SPLINE_CURVE_WITH_KNOTS('',3,(#123581,#123582,#123583,#123584,
#123585,#123586),.UNSPECIFIED.,.F.,.F.,(4,2,4),(8.04217133295527E-11,0.012651940139658,
0.0253036433290908),.UNSPECIFIED.);
#22601=B_SPLINE_CURVE_WITH_KNOTS('',3,(#123606,#123607,#123608,#123609,
#123610,#123611),.UNSPECIFIED.,.F.,.F.,(4,2,4),(5.19886781513755E-11,0.0126519401226947,
0.0253036433221645),.UNSPECIFIED.);
#22602=B_SPLINE_CURVE_WITH_KNOTS('',3,(#123631,#123632,#123633,#123634,
#123635,#123636),.UNSPECIFIED.,.F.,.F.,(4,2,4),(2.66805634994813E-11,0.0126519401007409,
0.0253036433160408),.UNSPECIFIED.);
#22603=B_SPLINE_CURVE_WITH_KNOTS('',3,(#123656,#123657,#123658,#123659,
#123660,#123661),.UNSPECIFIED.,.F.,.F.,(4,2,4),(5.55682401312492E-11,0.0126519401226915,
0.0253036433365694),.UNSPECIFIED.);
#22604=B_SPLINE_CURVE_WITH_KNOTS('',3,(#123681,#123682,#123683,#123684,
#123685,#123686),.UNSPECIFIED.,.F.,.F.,(4,2,4),(3.32378535415398E-11,0.012651940098632,
0.0253036433355196),.UNSPECIFIED.);
#22605=B_SPLINE_CURVE_WITH_KNOTS('',3,(#123706,#123707,#123708,#123709,
#123710,#123711),.UNSPECIFIED.,.F.,.F.,(4,2,4),(2.94105947720898E-11,0.012651940101243,
0.0253036433317081),.UNSPECIFIED.);
#22606=B_SPLINE_CURVE_WITH_KNOTS('',3,(#123731,#123732,#123733,#123734,
#123735,#123736),.UNSPECIFIED.,.F.,.F.,(4,2,4),(5.23976660158685E-11,0.0126519400966257,
0.025303643309186),.UNSPECIFIED.);
#22607=B_SPLINE_CURVE_WITH_KNOTS('',3,(#123756,#123757,#123758,#123759,
#123760,#123761),.UNSPECIFIED.,.F.,.F.,(4,2,4),(3.15595498847292E-11,0.0126519401075625,
0.0253036433442606),.UNSPECIFIED.);
#22608=B_SPLINE_CURVE_WITH_KNOTS('',3,(#123781,#123782,#123783,#123784,
#123785,#123786),.UNSPECIFIED.,.F.,.F.,(4,2,4),(3.08817990073898E-11,0.0126519400829584,
0.0253036433089566),.UNSPECIFIED.);
#22609=B_SPLINE_CURVE_WITH_KNOTS('',3,(#123816,#123817,#123818,#123819,
#123820,#123821,#123822,#123823,#123824,#123825),.UNSPECIFIED.,.F.,.F.,
(4,3,3,4),(6.6640610766212E-12,8.705316532067E-5,0.000170036750316901,0.000253022379909538),
 .UNSPECIFIED.);
#22610=B_SPLINE_CURVE_WITH_KNOTS('',3,(#123842,#123843,#123844,#123845,
#123846,#123847,#123848,#123849,#123850,#123851),.UNSPECIFIED.,.F.,.F.,
(4,3,3,4),(0.21150258497194,0.214285714285714,0.224091821226272,0.228883374862199),
 .UNSPECIFIED.);
#22611=B_SPLINE_CURVE_WITH_KNOTS('',3,(#123852,#123853,#123854,#123855,
#123856,#123857,#123858,#123859,#123860,#123861),.UNSPECIFIED.,.F.,.F.,
(4,3,3,4),(9.87472387492481E-14,8.70530730923297E-5,0.000170036649017195,
0.000253022524284304),.UNSPECIFIED.);
#22612=B_SPLINE_CURVE_WITH_KNOTS('',3,(#123893,#123894,#123895,#123896,
#123897,#123898,#123899,#123900,#123901,#123902),.UNSPECIFIED.,.F.,.F.,
(4,3,3,4),(9.66095229123471E-14,8.70530734827142E-5,0.000170036649712784,
0.000253022525284264),.UNSPECIFIED.);
#22613=B_SPLINE_CURVE_WITH_KNOTS('',3,(#123934,#123935,#123936,#123937,
#123938,#123939,#123940,#123941,#123942,#123943),.UNSPECIFIED.,.F.,.F.,
(4,3,3,4),(8.51722419461328E-14,8.70530733731967E-5,0.00017003664969144,
0.00025302252535137),.UNSPECIFIED.);
#22614=B_SPLINE_CURVE_WITH_KNOTS('',3,(#123970,#123971,#123972,#123973,
#123974,#123975,#123976,#123977,#123978,#123979),.UNSPECIFIED.,.F.,.F.,
(4,3,3,4),(0.21150258497204,0.214285714285714,0.224091815977165,0.228883374852172),
 .UNSPECIFIED.);
#22615=B_SPLINE_CURVE_WITH_KNOTS('',3,(#123980,#123981,#123982,#123983,
#123984,#123985,#123986,#123987,#123988,#123989),.UNSPECIFIED.,.F.,.F.,
(4,3,3,4),(1.01626207911617E-13,8.70530731189993E-5,0.000170036648882768,
0.000253022523989131),.UNSPECIFIED.);
#22616=B_SPLINE_CURVE_WITH_KNOTS('',3,(#124016,#124017,#124018,#124019,
#124020,#124021,#124022,#124023,#124024,#124025),.UNSPECIFIED.,.F.,.F.,
(4,3,3,4),(0.211502584960139,0.214285714285714,0.224091816970476,0.228883374861854),
 .UNSPECIFIED.);
#22617=B_SPLINE_CURVE_WITH_KNOTS('',3,(#124026,#124027,#124028,#124029,
#124030,#124031,#124032,#124033,#124034,#124035),.UNSPECIFIED.,.F.,.F.,
(4,3,3,4),(8.80036232291946E-15,8.70530734436068E-5,0.000170036649788735,
0.000253022525475915),.UNSPECIFIED.);
#22618=B_SPLINE_CURVE_WITH_KNOTS('',3,(#124067,#124068,#124069,#124070,
#124071,#124072,#124073,#124074,#124075,#124076),.UNSPECIFIED.,.F.,.F.,
(4,3,3,4),(1.25935783266693E-13,8.70530732380594E-5,0.000170036649043835,
0.000253022524191688),.UNSPECIFIED.);
#22619=B_SPLINE_CURVE_WITH_KNOTS('',3,(#124108,#124109,#124110,#124111,
#124112,#124113,#124114,#124115,#124116,#124117),.UNSPECIFIED.,.F.,.F.,
(4,3,3,4),(6.3468392922729E-14,8.70530730437247E-5,0.000170036649085858,
0.00025302252447051),.UNSPECIFIED.);
#22620=B_SPLINE_CURVE_WITH_KNOTS('',3,(#124149,#124150,#124151,#124152,
#124153,#124154,#124155,#124156,#124157,#124158),.UNSPECIFIED.,.F.,.F.,
(4,3,3,4),(5.57032184678306E-14,8.70530736151203E-5,0.000170036649919078,
0.000253022525565306),.UNSPECIFIED.);
#22621=B_SPLINE_CURVE_WITH_KNOTS('',3,(#124190,#124191,#124192,#124193,
#124194,#124195,#124196,#124197,#124198,#124199),.UNSPECIFIED.,.F.,.F.,
(4,3,3,4),(2.08112962572377E-14,8.70530731469877E-5,0.000170036648983745,
0.000253022524162933),.UNSPECIFIED.);
#22622=B_SPLINE_CURVE_WITH_KNOTS('',3,(#124226,#124227,#124228,#124229,
#124230,#124231,#124232,#124233,#124234,#124235),.UNSPECIFIED.,.F.,.F.,
(4,3,3,4),(0.211502584948017,0.214285714285714,0.224091813954176,0.228883374857004),
 .UNSPECIFIED.);
#22623=B_SPLINE_CURVE_WITH_KNOTS('',3,(#124236,#124237,#124238,#124239,
#124240,#124241,#124242,#124243,#124244,#124245),.UNSPECIFIED.,.F.,.F.,
(4,3,3,4),(1.0312806272257E-13,8.70530736274529E-5,0.000170036649568835,
0.000253022524852173),.UNSPECIFIED.);
#22624=B_SPLINE_CURVE_WITH_KNOTS('',3,(#124277,#124278,#124279,#124280,
#124281,#124282,#124283,#124284,#124285,#124286),.UNSPECIFIED.,.F.,.F.,
(4,3,3,4),(6.10883102621712E-14,8.70530732758973E-5,0.000170036649311073,
0.000253022524688439),.UNSPECIFIED.);
#22625=B_SPLINE_CURVE_WITH_KNOTS('',3,(#124318,#124319,#124320,#124321,
#124322,#124323,#124324,#124325,#124326,#124327),.UNSPECIFIED.,.F.,.F.,
(4,3,3,4),(9.87598498237521E-14,8.70530733707688E-5,0.000170036649518818,
0.000253022525009334),.UNSPECIFIED.);
#22626=B_SPLINE_CURVE_WITH_KNOTS('',3,(#124359,#124360,#124361,#124362,
#124363,#124364,#124365,#124366,#124367,#124368),.UNSPECIFIED.,.F.,.F.,
(4,3,3,4),(1.22916473070759E-13,8.70530733797046E-5,0.000170036649362786,
0.0002530225246876),.UNSPECIFIED.);
#22627=B_SPLINE_CURVE_WITH_KNOTS('',3,(#124395,#124396,#124397,#124398,
#124399,#124400,#124401,#124402,#124403,#124404,#124405,#124406,#124407,
#124408),.UNSPECIFIED.,.F.,.F.,(4,2,2,2,2,2,4),(6.1819644215993E-10,0.0398355571596381,
0.0598130476820354,0.0698194557541455,0.0748266666676206,0.0773312228469091,
0.0797213973169973),.UNSPECIFIED.);
#22628=B_SPLINE_CURVE_WITH_KNOTS('',3,(#124409,#124410,#124411,#124412,
#124413,#124414,#124415,#124416,#124417,#124418),.UNSPECIFIED.,.F.,.F.,
(4,3,3,4),(1.57386796031694E-13,8.70530729486484E-5,0.000170036648862666,
0.000253022524119131),.UNSPECIFIED.);
#22629=B_SPLINE_CURVE_WITH_KNOTS('',3,(#124445,#124446,#124447,#124448,
#124449,#124450,#124451,#124452,#124453,#124454,#124455,#124456,#124457,
#124458),.UNSPECIFIED.,.F.,.F.,(4,2,2,2,2,2,4),(5.57021547245071E-10,0.0398355724600839,
0.0598130687824846,0.0698194724814338,0.0748266812070732,0.0773312362921125,
0.0797214096953586),.UNSPECIFIED.);
#22630=B_SPLINE_CURVE_WITH_KNOTS('',3,(#124459,#124460,#124461,#124462,
#124463,#124464,#124465,#124466,#124467,#124468),.UNSPECIFIED.,.F.,.F.,
(4,3,3,4),(3.67379430042663E-14,8.70530734906078E-5,0.000170036649570195,
0.000253022524992311),.UNSPECIFIED.);
#22631=B_SPLINE_CURVE_WITH_KNOTS('',3,(#124495,#124496,#124497,#124498,
#124499,#124500,#124501,#124502,#124503,#124504,#124505,#124506,#124507,
#124508),.UNSPECIFIED.,.F.,.F.,(4,2,2,2,2,2,4),(5.85094002627536E-10,0.0398355551775198,
0.0598130479271771,0.0698194623582696,0.0748266764456829,0.0773312342105983,
0.079721410169492),.UNSPECIFIED.);
#22632=B_SPLINE_CURVE_WITH_KNOTS('',3,(#124509,#124510,#124511,#124512,
#124513,#124514,#124515,#124516,#124517,#124518),.UNSPECIFIED.,.F.,.F.,
(4,3,3,4),(6.03864091016704E-14,8.70530729984532E-5,0.000170036648893081,
0.000253022524129855),.UNSPECIFIED.);
#22633=B_SPLINE_CURVE_WITH_KNOTS('',3,(#124550,#124551,#124552,#124553,
#124554,#124555,#124556,#124557,#124558,#124559),.UNSPECIFIED.,.F.,.F.,
(4,3,3,4),(1.09033936088854E-13,8.70530732165782E-5,0.000170036649139827,
0.000253022524404992),.UNSPECIFIED.);
#22634=B_SPLINE_CURVE_WITH_KNOTS('',3,(#124591,#124592,#124593,#124594,
#124595,#124596,#124597,#124598,#124599,#124600),.UNSPECIFIED.,.F.,.F.,
(4,3,3,4),(1.18163273935885E-13,8.70530734410755E-5,0.000170036649704182,
0.000253022525309384),.UNSPECIFIED.);
#22635=B_SPLINE_CURVE_WITH_KNOTS('',3,(#124627,#124628,#124629,#124630,
#124631,#124632,#124633,#124634,#124635,#124636),.UNSPECIFIED.,.F.,.F.,
(4,3,3,4),(0.211502584965516,0.214285714285714,0.224091827574402,0.228883374872321),
 .UNSPECIFIED.);
#22636=B_SPLINE_CURVE_WITH_KNOTS('',3,(#124637,#124638,#124639,#124640,
#124641,#124642,#124643,#124644,#124645,#124646),.UNSPECIFIED.,.F.,.F.,
(4,3,3,4),(9.02433971457501E-14,8.70530732466902E-5,0.000170036649065817,
0.000253022524226767),.UNSPECIFIED.);
#22637=B_SPLINE_CURVE_WITH_KNOTS('',3,(#124678,#124679,#124680,#124681,
#124682,#124683,#124684,#124685,#124686,#124687),.UNSPECIFIED.,.F.,.F.,
(4,3,3,4),(7.51514809846539E-14,8.70530731548467E-5,0.000170036649085044,
0.000253022524357496),.UNSPECIFIED.);
#22638=B_SPLINE_CURVE_WITH_KNOTS('',3,(#124719,#124720,#124721,#124722,
#124723,#124724,#124725,#124726,#124727,#124728),.UNSPECIFIED.,.F.,.F.,
(4,3,3,4),(2.53717776951365E-14,8.70530732794565E-5,0.000170036649550751,
0.000253022525164439),.UNSPECIFIED.);
#22639=B_SPLINE_CURVE_WITH_KNOTS('',3,(#124755,#124756,#124757,#124758,
#124759,#124760,#124761,#124762,#124763,#124764),.UNSPECIFIED.,.F.,.F.,
(4,3,3,4),(0.211502584969517,0.214285714285714,0.224091819257381,0.228883374862328),
 .UNSPECIFIED.);
#22640=B_SPLINE_CURVE_WITH_KNOTS('',3,(#124765,#124766,#124767,#124768,
#124769,#124770,#124771,#124772,#124773,#124774),.UNSPECIFIED.,.F.,.F.,
(4,3,3,4),(7.89431934074236E-14,8.70530731075781E-5,0.000170036648965765,
0.000253022524166181),.UNSPECIFIED.);
#22641=B_SPLINE_CURVE_WITH_KNOTS('',3,(#124801,#124802,#124803,#124804,
#124805,#124806,#124807,#124808,#124809,#124810,#124811,#124812,#124813,
#124814),.UNSPECIFIED.,.F.,.F.,(4,2,2,2,2,2,4),(6.34474575368533E-10,0.0398355712933957,
0.059813071467123,0.0698194778032689,0.0748266878437471,0.077331243585381,
0.0797214176266301),.UNSPECIFIED.);
#22642=B_SPLINE_CURVE_WITH_KNOTS('',3,(#124815,#124816,#124817,#124818,
#124819,#124820,#124821,#124822,#124823,#124824),.UNSPECIFIED.,.F.,.F.,
(4,3,3,4),(1.31867107742812E-13,8.70530735910056E-5,0.000170036649834359,
0.000253022525420013),.UNSPECIFIED.);
#22643=B_SPLINE_CURVE_WITH_KNOTS('',3,(#124856,#124857,#124858,#124859,
#124860,#124861,#124862,#124863,#124864,#124865),.UNSPECIFIED.,.F.,.F.,
(4,3,3,4),(5.36960810667672E-14,8.70530735283642E-5,0.000170036649708884,
0.000253022525231527),.UNSPECIFIED.);
#22644=B_SPLINE_CURVE_WITH_KNOTS('',3,(#124897,#124898,#124899,#124900,
#124901,#124902,#124903,#124904,#124905,#124906),.UNSPECIFIED.,.F.,.F.,
(4,3,3,4),(7.80228131461319E-14,8.70530734703482E-5,0.000170036649594559,
0.000253022525060402),.UNSPECIFIED.);
#22645=B_SPLINE_CURVE_WITH_KNOTS('',3,(#124938,#124939,#124940,#124941,
#124942,#124943,#124944,#124945,#124946,#124947),.UNSPECIFIED.,.F.,.F.,
(4,3,3,4),(8.01062290819287E-15,8.7053073630607E-5,0.000170036649876423,
0.000253022525464228),.UNSPECIFIED.);
#22646=B_SPLINE_CURVE_WITH_KNOTS('',3,(#124974,#124975,#124976,#124977,
#124978,#124979,#124980,#124981,#124982,#124983),.UNSPECIFIED.,.F.,.F.,
(4,3,3,4),(0.211502584963299,0.214285714285714,0.224091802941358,0.228883374862355),
 .UNSPECIFIED.);
#22647=B_SPLINE_CURVE_WITH_KNOTS('',3,(#124984,#124985,#124986,#124987,
#124988,#124989,#124990,#124991,#124992,#124993),.UNSPECIFIED.,.F.,.F.,
(4,3,3,4),(8.73844952612567E-14,8.70530734589333E-5,0.000170036649623771,
0.000253022525131072),.UNSPECIFIED.);
#22648=B_SPLINE_CURVE_WITH_KNOTS('',3,(#125020,#125021,#125022,#125023,
#125024,#125025,#125026,#125027,#125028,#125029),.UNSPECIFIED.,.F.,.F.,
(4,3,3,4),(0.211502584978396,0.214285714285714,0.224091828316984,0.228883374866789),
 .UNSPECIFIED.);
#22649=B_SPLINE_CURVE_WITH_KNOTS('',3,(#125030,#125031,#125032,#125033,
#125034,#125035,#125036,#125037,#125038,#125039),.UNSPECIFIED.,.F.,.F.,
(4,3,3,4),(4.13945888189021E-14,8.70530734855099E-5,0.000170036649813318,
0.000253022525483275),.UNSPECIFIED.);
#22650=B_SPLINE_CURVE_WITH_KNOTS('',3,(#125065,#125066,#125067,#125068,
#125069,#125070,#125071,#125072,#125073,#125074,#125075,#125076,#125077,
#125078),.UNSPECIFIED.,.F.,.F.,(4,2,2,2,2,2,4),(9.84438766148368E-11,0.0398356066089345,
0.0598131576187708,0.0698195873416727,0.0748268090853319,0.077331370681033,
0.0797215503067857),.UNSPECIFIED.);
#22651=B_SPLINE_CURVE_WITH_KNOTS('',3,(#125092,#125093,#125094,#125095,
#125096,#125097),.UNSPECIFIED.,.F.,.F.,(4,2,4),(-0.0253009680193219,-0.0126505173686473,
-1.50651325789286E-9),.UNSPECIFIED.);
#22652=B_SPLINE_CURVE_WITH_KNOTS('',3,(#125125,#125126,#125127,#125128,
#125129,#125130),.UNSPECIFIED.,.F.,.F.,(4,2,4),(-0.0253008161710598,-0.0126505173063933,
-1.49706886817813E-9),.UNSPECIFIED.);
#22653=B_SPLINE_CURVE_WITH_KNOTS('',3,(#125158,#125159,#125160,#125161,
#125162,#125163),.UNSPECIFIED.,.F.,.F.,(4,2,4),(-0.0253008162502549,-0.012650517377553,
-1.51926837083094E-9),.UNSPECIFIED.);
#22654=B_SPLINE_CURVE_WITH_KNOTS('',3,(#125191,#125192,#125193,#125194,
#125195,#125196),.UNSPECIFIED.,.F.,.F.,(4,2,4),(-0.0253008161942039,-0.0126505173276397,
-1.51911317899933E-9),.UNSPECIFIED.);
#22655=B_SPLINE_CURVE_WITH_KNOTS('',3,(#125224,#125225,#125226,#125227,
#125228,#125229),.UNSPECIFIED.,.F.,.F.,(4,2,4),(-0.025300816184677,-0.0126505173051501,
-1.51005885226652E-9),.UNSPECIFIED.);
#22656=B_SPLINE_CURVE_WITH_KNOTS('',3,(#125257,#125258,#125259,#125260,
#125261,#125262),.UNSPECIFIED.,.F.,.F.,(4,2,4),(-0.0253008162356417,-0.012650517371839,
-1.5194880978453E-9),.UNSPECIFIED.);
#22657=B_SPLINE_CURVE_WITH_KNOTS('',3,(#125290,#125291,#125292,#125293,
#125294,#125295),.UNSPECIFIED.,.F.,.F.,(4,2,4),(-0.0253008162373823,-0.012650517352546,
-1.5117902658901E-9),.UNSPECIFIED.);
#22658=B_SPLINE_CURVE_WITH_KNOTS('',3,(#125323,#125324,#125325,#125326,
#125327,#125328),.UNSPECIFIED.,.F.,.F.,(4,2,4),(-0.0253009567060839,-0.012650517332386,
-1.49595632756294E-9),.UNSPECIFIED.);
#22659=B_SPLINE_CURVE_WITH_KNOTS('',3,(#125356,#125357,#125358,#125359,
#125360,#125361),.UNSPECIFIED.,.F.,.F.,(4,2,4),(-0.0253009734745182,-0.0126505174081292,
-1.53339678454767E-9),.UNSPECIFIED.);
#22660=B_SPLINE_CURVE_WITH_KNOTS('',3,(#125389,#125390,#125391,#125392,
#125393,#125394),.UNSPECIFIED.,.F.,.F.,(4,2,4),(-0.0253009751682653,-0.0126505173744186,
-1.50967184586737E-9),.UNSPECIFIED.);
#22661=B_SPLINE_CURVE_WITH_KNOTS('',3,(#125422,#125423,#125424,#125425,
#125426,#125427),.UNSPECIFIED.,.F.,.F.,(4,2,4),(-0.0253009628824026,-0.012650517367083,
-1.50349348596035E-9),.UNSPECIFIED.);
#22662=B_SPLINE_CURVE_WITH_KNOTS('',3,(#125455,#125456,#125457,#125458,
#125459,#125460),.UNSPECIFIED.,.F.,.F.,(4,2,4),(-0.0253009682533948,-0.0126505173592761,
-1.50435279511196E-9),.UNSPECIFIED.);
#22663=B_SPLINE_CURVE_WITH_KNOTS('',3,(#125488,#125489,#125490,#125491,
#125492,#125493),.UNSPECIFIED.,.F.,.F.,(4,2,4),(-0.0253008162097125,-0.0126505173692927,
-1.51393972705471E-9),.UNSPECIFIED.);
#22664=B_SPLINE_CURVE_WITH_KNOTS('',3,(#125521,#125522,#125523,#125524,
#125525,#125526),.UNSPECIFIED.,.F.,.F.,(4,2,4),(-0.0253009709382149,-0.0126505173850716,
-1.51950293320047E-9),.UNSPECIFIED.);
#22665=B_SPLINE_CURVE_WITH_KNOTS('',3,(#125551,#125552,#125553,#125554,
#125555,#125556),.UNSPECIFIED.,.F.,.F.,(4,2,4),(-0.0253008162162922,-0.0126505173663554,
-1.50183707484097E-9),.UNSPECIFIED.);
#22666=B_SPLINE_CURVE_WITH_KNOTS('',3,(#125578,#125579,#125580,#125581,
#125582,#125583),.UNSPECIFIED.,.F.,.F.,(4,2,4),(-0.0253008161965179,-0.0126505173531787,
-1.50008382798772E-9),.UNSPECIFIED.);
#22667=B_SPLINE_CURVE_WITH_KNOTS('',3,(#125611,#125612,#125613,#125614,
#125615,#125616),.UNSPECIFIED.,.F.,.F.,(4,2,4),(-0.0253008162312706,-0.0126505173673404,
-1.51304643467021E-9),.UNSPECIFIED.);
#22668=B_SPLINE_CURVE_WITH_KNOTS('',3,(#125644,#125645,#125646,#125647,
#125648,#125649),.UNSPECIFIED.,.F.,.F.,(4,2,4),(-0.0253008161733499,-0.0126505173152187,
-1.50923519515178E-9),.UNSPECIFIED.);
#22669=B_SPLINE_CURVE_WITH_KNOTS('',3,(#125677,#125678,#125679,#125680,
#125681,#125682),.UNSPECIFIED.,.F.,.F.,(4,2,4),(-0.0253009530091239,-0.0126505173737225,
-1.5033947455001E-9),.UNSPECIFIED.);
#22670=B_SPLINE_CURVE_WITH_KNOTS('',3,(#125710,#125711,#125712,#125713,
#125714,#125715),.UNSPECIFIED.,.F.,.F.,(4,2,4),(-0.0253009684925171,-0.0126505173770235,
-1.5125917671166E-9),.UNSPECIFIED.);
#22671=B_SPLINE_CURVE_WITH_KNOTS('',3,(#125743,#125744,#125745,#125746,
#125747,#125748),.UNSPECIFIED.,.F.,.F.,(4,2,4),(-0.0253008162223907,-0.0126505173844459,
-1.51811038739957E-9),.UNSPECIFIED.);
#22672=B_SPLINE_CURVE_WITH_KNOTS('',3,(#125776,#125777,#125778,#125779,
#125780,#125781),.UNSPECIFIED.,.F.,.F.,(4,2,4),(-0.0253008161851833,-0.0126505173103185,
-1.49799530765882E-9),.UNSPECIFIED.);
#22673=B_SPLINE_CURVE_WITH_KNOTS('',3,(#125810,#125811,#125812,#125813,
#125814,#125815),.UNSPECIFIED.,.F.,.F.,(4,2,4),(-0.025300816194907,-0.0126505173454016,
-1.51742879719863E-9),.UNSPECIFIED.);
#22674=B_SPLINE_CURVE_WITH_KNOTS('',3,(#125842,#125843,#125844,#125845,
#125846,#125847),.UNSPECIFIED.,.F.,.F.,(4,2,4),(-0.0253008162162837,-0.0126505173700267,
-1.50907499690822E-9),.UNSPECIFIED.);
#22675=B_SPLINE_CURVE_WITH_KNOTS('',3,(#125875,#125876,#125877,#125878,
#125879,#125880),.UNSPECIFIED.,.F.,.F.,(4,2,4),(-0.0253008162384224,-0.0126505173764547,
-1.50414914204533E-9),.UNSPECIFIED.);
#22676=B_SPLINE_CURVE_WITH_KNOTS('',3,(#125908,#125909,#125910,#125911,
#125912,#125913),.UNSPECIFIED.,.F.,.F.,(4,2,4),(-0.0253008162004374,-0.0126505173491142,
-1.50324420272741E-9),.UNSPECIFIED.);
#22677=B_SPLINE_CURVE_WITH_KNOTS('',3,(#125941,#125942,#125943,#125944,
#125945,#125946),.UNSPECIFIED.,.F.,.F.,(4,2,4),(-0.0253008162124498,-0.012650517365658,
-1.51088165242785E-9),.UNSPECIFIED.);
#22678=B_SPLINE_CURVE_WITH_KNOTS('',3,(#125974,#125975,#125976,#125977,
#125978,#125979),.UNSPECIFIED.,.F.,.F.,(4,2,4),(-0.0253008161865096,-0.01265051732059,
-1.5011254600461E-9),.UNSPECIFIED.);
#22679=B_SPLINE_CURVE_WITH_KNOTS('',3,(#126007,#126008,#126009,#126010,
#126011,#126012),.UNSPECIFIED.,.F.,.F.,(4,2,4),(-0.0253009718038439,-0.0126505173976087,
-1.53092769364371E-9),.UNSPECIFIED.);
#22680=B_SPLINE_CURVE_WITH_KNOTS('',3,(#126041,#126042,#126043,#126044,
#126045,#126046),.UNSPECIFIED.,.F.,.F.,(4,2,4),(-0.0252971444835285,-0.0126486652117214,
0.),.UNSPECIFIED.);
#22681=B_SPLINE_CURVE_WITH_KNOTS('',3,(#126058,#126059,#126060,#126061,
#126062,#126063,#126064),.UNSPECIFIED.,.F.,.F.,(4,3,4),(0.216822083469384,
0.226204530183526,0.228987659635175),.UNSPECIFIED.);
#22682=B_SPLINE_CURVE_WITH_KNOTS('',3,(#126084,#126085,#126086,#126087,
#126088,#126089),.UNSPECIFIED.,.F.,.F.,(4,2,4),(-0.0252971543978597,-0.0126486691839802,
0.),.UNSPECIFIED.);
#22683=B_SPLINE_CURVE_WITH_KNOTS('',3,(#126101,#126102,#126103,#126104,
#126105,#126106,#126107),.UNSPECIFIED.,.F.,.F.,(4,3,4),(0.216822083469368,
0.226204530183526,0.228987659635175),.UNSPECIFIED.);
#22684=B_SPLINE_CURVE_WITH_KNOTS('',3,(#126127,#126128,#126129,#126130,
#126131,#126132),.UNSPECIFIED.,.F.,.F.,(4,2,4),(-0.0252971379173837,-0.0126486624600064,
0.),.UNSPECIFIED.);
#22685=B_SPLINE_CURVE_WITH_KNOTS('',3,(#126144,#126145,#126146,#126147,
#126148,#126149,#126150),.UNSPECIFIED.,.F.,.F.,(4,3,4),(0.216822083469368,
0.226204530183526,0.228987659635175),.UNSPECIFIED.);
#22686=B_SPLINE_CURVE_WITH_KNOTS('',3,(#126170,#126171,#126172,#126173,
#126174,#126175),.UNSPECIFIED.,.F.,.F.,(4,2,4),(-0.025296843893326,-0.0126485434765334,
-1.79759367113785E-11),.UNSPECIFIED.);
#22687=B_SPLINE_CURVE_WITH_KNOTS('',3,(#126187,#126188,#126189,#126190,
#126191,#126192,#126193),.UNSPECIFIED.,.F.,.F.,(4,3,4),(0.216822083469368,
0.226204530183526,0.228987659635175),.UNSPECIFIED.);
#22688=B_SPLINE_CURVE_WITH_KNOTS('',3,(#126213,#126214,#126215,#126216,
#126217,#126218),.UNSPECIFIED.,.F.,.F.,(4,2,4),(-0.0252971503797783,-0.0126486675839431,
0.),.UNSPECIFIED.);
#22689=B_SPLINE_CURVE_WITH_KNOTS('',3,(#126230,#126231,#126232,#126233,
#126234,#126235,#126236),.UNSPECIFIED.,.F.,.F.,(4,3,4),(0.216822083469358,
0.226204530183526,0.228987659635175),.UNSPECIFIED.);
#22690=B_SPLINE_CURVE_WITH_KNOTS('',3,(#126256,#126257,#126258,#126259,
#126260,#126261),.UNSPECIFIED.,.F.,.F.,(4,2,4),(-0.0252971492907873,-0.0126486671489296,
0.),.UNSPECIFIED.);
#22691=B_SPLINE_CURVE_WITH_KNOTS('',3,(#126273,#126274,#126275,#126276,
#126277,#126278,#126279),.UNSPECIFIED.,.F.,.F.,(4,3,4),(0.216822083469368,
0.226204530183526,0.228987659635175),.UNSPECIFIED.);
#22692=B_SPLINE_CURVE_WITH_KNOTS('',3,(#126299,#126300,#126301,#126302,
#126303,#126304),.UNSPECIFIED.,.F.,.F.,(4,2,4),(-0.025296843880375,-0.0126485434460251,
-1.24961256620093E-11),.UNSPECIFIED.);
#22693=B_SPLINE_CURVE_WITH_KNOTS('',3,(#126316,#126317,#126318,#126319,
#126320,#126321,#126322),.UNSPECIFIED.,.F.,.F.,(4,3,4),(0.216822083469358,
0.226204530183526,0.228987659635175),.UNSPECIFIED.);
#22694=B_SPLINE_CURVE_WITH_KNOTS('',3,(#126342,#126343,#126344,#126345,
#126346,#126347),.UNSPECIFIED.,.F.,.F.,(4,2,4),(-0.0252971646096114,-0.0126486733003775,
0.),.UNSPECIFIED.);
#22695=B_SPLINE_CURVE_WITH_KNOTS('',3,(#126359,#126360,#126361,#126362,
#126363,#126364,#126365),.UNSPECIFIED.,.F.,.F.,(4,3,4),(0.216822083469364,
0.226204530183524,0.228987659635174),.UNSPECIFIED.);
#22696=B_SPLINE_CURVE_WITH_KNOTS('',3,(#126385,#126386,#126387,#126388,
#126389,#126390),.UNSPECIFIED.,.F.,.F.,(4,2,4),(-0.0252971681999182,-0.0126486747882726,
0.),.UNSPECIFIED.);
#22697=B_SPLINE_CURVE_WITH_KNOTS('',3,(#126402,#126403,#126404,#126405,
#126406,#126407,#126408),.UNSPECIFIED.,.F.,.F.,(4,3,4),(0.216822083469364,
0.226204530183524,0.228987659635174),.UNSPECIFIED.);
#22698=B_SPLINE_CURVE_WITH_KNOTS('',3,(#126428,#126429,#126430,#126431,
#126432,#126433),.UNSPECIFIED.,.F.,.F.,(4,2,4),(-0.0252971380209954,-0.0126486625735294,
0.),.UNSPECIFIED.);
#22699=B_SPLINE_CURVE_WITH_KNOTS('',3,(#126445,#126446,#126447,#126448,
#126449,#126450,#126451),.UNSPECIFIED.,.F.,.F.,(4,3,4),(0.216822083469354,
0.226204530183524,0.228987659635174),.UNSPECIFIED.);
#22700=B_SPLINE_CURVE_WITH_KNOTS('',3,(#126471,#126472,#126473,#126474,
#126475,#126476),.UNSPECIFIED.,.F.,.F.,(4,2,4),(-0.025297157550282,-0.0126486704428088,
0.),.UNSPECIFIED.);
#22701=B_SPLINE_CURVE_WITH_KNOTS('',3,(#126488,#126489,#126490,#126491,
#126492,#126493,#126494),.UNSPECIFIED.,.F.,.F.,(4,3,4),(0.216822083469364,
0.226204530183524,0.228987659635174),.UNSPECIFIED.);
#22702=B_SPLINE_CURVE_WITH_KNOTS('',3,(#126514,#126515,#126516,#126517,
#126518,#126519),.UNSPECIFIED.,.F.,.F.,(4,2,4),(-0.0252972106396085,-0.0126486717985792,
0.),.UNSPECIFIED.);
#22703=B_SPLINE_CURVE_WITH_KNOTS('',3,(#126531,#126532,#126533,#126534,
#126535,#126536,#126537),.UNSPECIFIED.,.F.,.F.,(4,3,4),(0.216822083469356,
0.226204530183524,0.228987659635174),.UNSPECIFIED.);
#22704=B_SPLINE_CURVE_WITH_KNOTS('',3,(#126557,#126558,#126559,#126560,
#126561,#126562),.UNSPECIFIED.,.F.,.F.,(4,2,4),(-0.0252971534510284,-0.0126486688573293,
0.),.UNSPECIFIED.);
#22705=B_SPLINE_CURVE_WITH_KNOTS('',3,(#126574,#126575,#126576,#126577,
#126578,#126579,#126580),.UNSPECIFIED.,.F.,.F.,(4,3,4),(0.216822083469364,
0.226204530183524,0.228987659635174),.UNSPECIFIED.);
#22706=B_SPLINE_CURVE_WITH_KNOTS('',3,(#126600,#126601,#126602,#126603,
#126604,#126605),.UNSPECIFIED.,.F.,.F.,(4,2,4),(-0.0252971604072883,-0.0126486716236138,
-8.09109723665102E-14),.UNSPECIFIED.);
#22707=B_SPLINE_CURVE_WITH_KNOTS('',3,(#126617,#126618,#126619,#126620,
#126621,#126622,#126623),.UNSPECIFIED.,.F.,.F.,(4,3,4),(0.216822083469356,
0.226204530183524,0.228987659635174),.UNSPECIFIED.);
#22708=B_SPLINE_CURVE_WITH_KNOTS('',3,(#126643,#126644,#126645,#126646,
#126647,#126648),.UNSPECIFIED.,.F.,.F.,(4,2,4),(-0.0252971585311309,-0.0126486708489145,
-4.90309182143989E-13),.UNSPECIFIED.);
#22709=B_SPLINE_CURVE_WITH_KNOTS('',3,(#126660,#126661,#126662,#126663,
#126664,#126665,#126666),.UNSPECIFIED.,.F.,.F.,(4,3,4),(0.216822083469359,
0.226204530183524,0.228987659635174),.UNSPECIFIED.);
#22710=B_SPLINE_CURVE_WITH_KNOTS('',3,(#126686,#126687,#126688,#126689,
#126690,#126691),.UNSPECIFIED.,.F.,.F.,(4,2,4),(-0.0252971600971946,-0.0126486714719039,
0.),.UNSPECIFIED.);
#22711=B_SPLINE_CURVE_WITH_KNOTS('',3,(#126703,#126704,#126705,#126706,
#126707,#126708,#126709),.UNSPECIFIED.,.F.,.F.,(4,3,4),(0.216822083469342,
0.226204530183524,0.228987659635174),.UNSPECIFIED.);
#22712=B_SPLINE_CURVE_WITH_KNOTS('',3,(#126729,#126730,#126731,#126732,
#126733,#126734),.UNSPECIFIED.,.F.,.F.,(4,2,4),(-0.0252971483010817,-0.0126486667440166,
0.),.UNSPECIFIED.);
#22713=B_SPLINE_CURVE_WITH_KNOTS('',3,(#126746,#126747,#126748,#126749,
#126750,#126751,#126752),.UNSPECIFIED.,.F.,.F.,(4,3,4),(0.216822083469362,
0.226204530183522,0.228987659635174),.UNSPECIFIED.);
#22714=B_SPLINE_CURVE_WITH_KNOTS('',3,(#126772,#126773,#126774,#126775,
#126776,#126777),.UNSPECIFIED.,.F.,.F.,(4,2,4),(-0.0252972379215595,-0.0126486787224415,
-4.86898715790218E-13),.UNSPECIFIED.);
#22715=B_SPLINE_CURVE_WITH_KNOTS('',3,(#126789,#126790,#126791,#126792,
#126793,#126794,#126795),.UNSPECIFIED.,.F.,.F.,(4,3,4),(0.216822083469365,
0.226204530183524,0.228987659635174),.UNSPECIFIED.);
#22716=B_SPLINE_CURVE_WITH_KNOTS('',3,(#126815,#126816,#126817,#126818,
#126819,#126820),.UNSPECIFIED.,.F.,.F.,(4,2,4),(-0.0252968437699015,-0.0126485433866258,
-1.85603164781778E-11),.UNSPECIFIED.);
#22717=B_SPLINE_CURVE_WITH_KNOTS('',3,(#126832,#126833,#126834,#126835,
#126836,#126837,#126838),.UNSPECIFIED.,.F.,.F.,(4,3,4),(0.216822083469354,
0.226204530183523,0.228987659635173),.UNSPECIFIED.);
#22718=B_SPLINE_CURVE_WITH_KNOTS('',3,(#126858,#126859,#126860,#126861,
#126862,#126863),.UNSPECIFIED.,.F.,.F.,(4,2,4),(-0.0252971672468309,-0.0126486744551382,
-5.57002360901393E-13),.UNSPECIFIED.);
#22719=B_SPLINE_CURVE_WITH_KNOTS('',3,(#126875,#126876,#126877,#126878,
#126879,#126880,#126881),.UNSPECIFIED.,.F.,.F.,(4,3,4),(0.216822083469377,
0.226204530183522,0.228987659635173),.UNSPECIFIED.);
#22720=B_SPLINE_CURVE_WITH_KNOTS('',3,(#126901,#126902,#126903,#126904,
#126905,#126906),.UNSPECIFIED.,.F.,.F.,(4,2,4),(-0.0252971463408049,-0.0126486659271449,
0.),.UNSPECIFIED.);
#22721=B_SPLINE_CURVE_WITH_KNOTS('',3,(#126918,#126919,#126920,#126921,
#126922,#126923,#126924),.UNSPECIFIED.,.F.,.F.,(4,3,4),(0.216822083469355,
0.22620453018352,0.228987659635174),.UNSPECIFIED.);
#22722=B_SPLINE_CURVE_WITH_KNOTS('',3,(#126941,#126942,#126943,#126944,
#126945,#126946),.UNSPECIFIED.,.F.,.F.,(4,2,4),(-0.0252971476460511,-0.0126486664505831,
0.),.UNSPECIFIED.);
#22723=B_SPLINE_CURVE_WITH_KNOTS('',3,(#126972,#126973,#126974,#126975,
#126976,#126977),.UNSPECIFIED.,.F.,.F.,(4,2,4),(-0.0252968438354448,-0.0126485434423394,
-1.27871359334453E-11),.UNSPECIFIED.);
#22724=B_SPLINE_CURVE_WITH_KNOTS('',3,(#126989,#126990,#126991,#126992,
#126993,#126994,#126995),.UNSPECIFIED.,.F.,.F.,(4,3,4),(0.216822083469191,
0.226204530183371,0.228987659635021),.UNSPECIFIED.);
#22725=B_SPLINE_CURVE_WITH_KNOTS('',3,(#127015,#127016,#127017,#127018,
#127019,#127020),.UNSPECIFIED.,.F.,.F.,(4,2,4),(-0.0252968438482744,-0.0126485434180359,
-2.16074103054353E-11),.UNSPECIFIED.);
#22726=B_SPLINE_CURVE_WITH_KNOTS('',3,(#127032,#127033,#127034,#127035,
#127036,#127037,#127038),.UNSPECIFIED.,.F.,.F.,(4,3,4),(0.216822083469273,
0.226204530183421,0.228987659635071),.UNSPECIFIED.);
#22727=B_SPLINE_CURVE_WITH_KNOTS('',3,(#127058,#127059,#127060,#127061,
#127062,#127063),.UNSPECIFIED.,.F.,.F.,(4,2,4),(-0.0252971457496129,-0.0126486657472849,
-9.65116875306649E-13),.UNSPECIFIED.);
#22728=B_SPLINE_CURVE_WITH_KNOTS('',3,(#127075,#127076,#127077,#127078,
#127079,#127080,#127081),.UNSPECIFIED.,.F.,.F.,(4,3,4),(0.216822083469326,
0.226204530183494,0.228987659635144),.UNSPECIFIED.);
#22729=B_SPLINE_CURVE_WITH_KNOTS('',3,(#127101,#127102,#127103,#127104,
#127105,#127106),.UNSPECIFIED.,.F.,.F.,(4,2,4),(-0.0252968438084748,-0.0126485434315949,
-8.85128428884663E-12),.UNSPECIFIED.);
#22730=B_SPLINE_CURVE_WITH_KNOTS('',3,(#127118,#127119,#127120,#127121,
#127122,#127123,#127124),.UNSPECIFIED.,.F.,.F.,(4,3,4),(0.216822083469354,
0.226204530183518,0.228987659635168),.UNSPECIFIED.);
#22731=B_SPLINE_CURVE_WITH_KNOTS('',3,(#127144,#127145,#127146,#127147,
#127148,#127149),.UNSPECIFIED.,.F.,.F.,(4,2,4),(-0.0252971314486642,-0.0126486598629424,
0.),.UNSPECIFIED.);
#22732=B_SPLINE_CURVE_WITH_KNOTS('',3,(#127161,#127162,#127163,#127164,
#127165,#127166,#127167),.UNSPECIFIED.,.F.,.F.,(4,3,4),(0.216822083469335,
0.226204530183512,0.228987659635174),.UNSPECIFIED.);
#22733=B_SPLINE_CURVE_WITH_KNOTS('',3,(#127187,#127188,#127189,#127190,
#127191,#127192),.UNSPECIFIED.,.F.,.F.,(4,2,4),(-0.0252968438717575,-0.0126485434602566,
-2.32165085767289E-11),.UNSPECIFIED.);
#22734=B_SPLINE_CURVE_WITH_KNOTS('',3,(#127204,#127205,#127206,#127207,
#127208,#127209,#127210),.UNSPECIFIED.,.F.,.F.,(4,3,4),(0.216822083469366,
0.226204530183524,0.228987659635173),.UNSPECIFIED.);
#22735=B_SPLINE_CURVE_WITH_KNOTS('',3,(#127230,#127231,#127232,#127233,
#127234,#127235),.UNSPECIFIED.,.F.,.F.,(4,2,4),(-0.0252971568839752,-0.0126486702042465,
-9.46274655855284E-12),.UNSPECIFIED.);
#22736=B_SPLINE_CURVE_WITH_KNOTS('',3,(#127247,#127248,#127249,#127250,
#127251,#127252,#127253),.UNSPECIFIED.,.F.,.F.,(4,3,4),(0.216822083514415,
0.226204530183526,0.228987659612923),.UNSPECIFIED.);
#22737=B_SPLINE_CURVE_WITH_KNOTS('',3,(#127271,#127272,#127273,#127274,
#127275,#127276),.UNSPECIFIED.,.F.,.F.,(4,2,4),(-0.0253028739767319,-0.012651396576206,
-3.6883829324097E-12),.UNSPECIFIED.);
#22738=B_SPLINE_CURVE_WITH_KNOTS('',3,(#127296,#127297,#127298,#127299,
#127300,#127301),.UNSPECIFIED.,.F.,.F.,(4,2,4),(-0.0253029052518879,-0.0126514041453768,
0.),.UNSPECIFIED.);
#22739=B_SPLINE_CURVE_WITH_KNOTS('',3,(#127321,#127322,#127323,#127324,
#127325,#127326),.UNSPECIFIED.,.F.,.F.,(4,2,4),(-0.0253028728360198,-0.0126513962951784,
0.),.UNSPECIFIED.);
#22740=B_SPLINE_CURVE_WITH_KNOTS('',3,(#127346,#127347,#127348,#127349,
#127350,#127351),.UNSPECIFIED.,.F.,.F.,(4,2,4),(-0.025302907356259,-0.0126513857913042,
0.),.UNSPECIFIED.);
#22741=B_SPLINE_CURVE_WITH_KNOTS('',3,(#127371,#127372,#127373,#127374,
#127375,#127376),.UNSPECIFIED.,.F.,.F.,(4,2,4),(-0.0253028831545656,-0.0126513987913224,
0.),.UNSPECIFIED.);
#22742=B_SPLINE_CURVE_WITH_KNOTS('',3,(#127396,#127397,#127398,#127399,
#127400,#127401),.UNSPECIFIED.,.F.,.F.,(4,2,4),(-0.0253028122000533,-0.0126513816288453,
0.),.UNSPECIFIED.);
#22743=B_SPLINE_CURVE_WITH_KNOTS('',3,(#127421,#127422,#127423,#127424,
#127425,#127426),.UNSPECIFIED.,.F.,.F.,(4,2,4),(-0.0253028437353472,-0.0126513892466307,
0.),.UNSPECIFIED.);
#22744=B_SPLINE_CURVE_WITH_KNOTS('',3,(#127446,#127447,#127448,#127449,
#127450,#127451),.UNSPECIFIED.,.F.,.F.,(4,2,4),(-0.0253028630135161,-0.0126513939175451,
-9.95696580741168E-13),.UNSPECIFIED.);
#22745=B_SPLINE_CURVE_WITH_KNOTS('',3,(#127471,#127472,#127473,#127474,
#127475,#127476),.UNSPECIFIED.,.F.,.F.,(4,2,4),(-0.0253028130466917,-0.0126513818408809,
0.),.UNSPECIFIED.);
#22746=B_SPLINE_CURVE_WITH_KNOTS('',3,(#127496,#127497,#127498,#127499,
#127500,#127501),.UNSPECIFIED.,.F.,.F.,(4,2,4),(-0.0253028790850444,-0.0126513978144101,
0.),.UNSPECIFIED.);
#22747=B_SPLINE_CURVE_WITH_KNOTS('',3,(#127521,#127522,#127523,#127524,
#127525,#127526),.UNSPECIFIED.,.F.,.F.,(4,2,4),(-0.0253028351982294,-0.0126513871967198,
0.),.UNSPECIFIED.);
#22748=B_SPLINE_CURVE_WITH_KNOTS('',3,(#127546,#127547,#127548,#127549,
#127550,#127551),.UNSPECIFIED.,.F.,.F.,(4,2,4),(-0.0253028711195569,-0.0126513958878269,
0.),.UNSPECIFIED.);
#22749=B_SPLINE_CURVE_WITH_KNOTS('',3,(#127571,#127572,#127573,#127574,
#127575,#127576),.UNSPECIFIED.,.F.,.F.,(4,2,4),(-0.0253028106499282,-0.0126513812345954,
0.),.UNSPECIFIED.);
#22750=B_SPLINE_CURVE_WITH_KNOTS('',3,(#127596,#127597,#127598,#127599,
#127600,#127601),.UNSPECIFIED.,.F.,.F.,(4,2,4),(-0.0253028259256569,-0.012651384927295,
0.),.UNSPECIFIED.);
#22751=B_SPLINE_CURVE_WITH_KNOTS('',3,(#127621,#127622,#127623,#127624,
#127625,#127626),.UNSPECIFIED.,.F.,.F.,(4,2,4),(-0.0253028151460171,-0.0126513816870844,
0.),.UNSPECIFIED.);
#22752=B_SPLINE_CURVE_WITH_KNOTS('',3,(#127646,#127647,#127648,#127649,
#127650,#127651),.UNSPECIFIED.,.F.,.F.,(4,2,4),(-0.0253028241929751,-0.0126513845149919,
0.),.UNSPECIFIED.);
#22753=B_SPLINE_CURVE_WITH_KNOTS('',3,(#127671,#127672,#127673,#127674,
#127675,#127676),.UNSPECIFIED.,.F.,.F.,(4,2,4),(-0.0253027974941012,-0.0126513780688482,
0.),.UNSPECIFIED.);
#22754=B_SPLINE_CURVE_WITH_KNOTS('',3,(#127696,#127697,#127698,#127699,
#127700,#127701),.UNSPECIFIED.,.F.,.F.,(4,2,4),(-0.0253028916207358,-0.012651400860891,
-8.60581397810201E-12),.UNSPECIFIED.);
#22755=B_SPLINE_CURVE_WITH_KNOTS('',3,(#127721,#127722,#127723,#127724,
#127725,#127726),.UNSPECIFIED.,.F.,.F.,(4,2,4),(-0.0253028691100921,-0.0126513953986287,
0.),.UNSPECIFIED.);
#22756=B_SPLINE_CURVE_WITH_KNOTS('',3,(#127746,#127747,#127748,#127749,
#127750,#127751),.UNSPECIFIED.,.F.,.F.,(4,2,4),(-0.0253028553317749,-0.0126513920673582,
0.),.UNSPECIFIED.);
#22757=B_SPLINE_CURVE_WITH_KNOTS('',3,(#127771,#127772,#127773,#127774,
#127775,#127776),.UNSPECIFIED.,.F.,.F.,(4,2,4),(-0.0253028299266163,-0.0126513859094088,
0.),.UNSPECIFIED.);
#22758=B_SPLINE_CURVE_WITH_KNOTS('',3,(#127796,#127797,#127798,#127799,
#127800,#127801),.UNSPECIFIED.,.F.,.F.,(4,2,4),(-0.0253028786820699,-0.012651397717359,
0.),.UNSPECIFIED.);
#22759=B_SPLINE_CURVE_WITH_KNOTS('',3,(#127821,#127822,#127823,#127824,
#127825,#127826),.UNSPECIFIED.,.F.,.F.,(4,2,4),(-0.0253028312099245,-0.0126513862313255,
0.),.UNSPECIFIED.);
#22760=B_SPLINE_CURVE_WITH_KNOTS('',3,(#127846,#127847,#127848,#127849,
#127850,#127851),.UNSPECIFIED.,.F.,.F.,(4,2,4),(-0.0253028926284109,-0.0126514011093113,
-1.22269798452646E-11),.UNSPECIFIED.);
#22761=B_SPLINE_CURVE_WITH_KNOTS('',3,(#127871,#127872,#127873,#127874,
#127875,#127876),.UNSPECIFIED.,.F.,.F.,(4,2,4),(-0.0253028799039149,-0.0126513980109877,
0.),.UNSPECIFIED.);
#22762=B_SPLINE_CURVE_WITH_KNOTS('',3,(#127896,#127897,#127898,#127899,
#127900,#127901),.UNSPECIFIED.,.F.,.F.,(4,2,4),(-0.0253028344455026,-0.0126513870067865,
0.),.UNSPECIFIED.);
#22763=B_SPLINE_CURVE_WITH_KNOTS('',3,(#127921,#127922,#127923,#127924,
#127925,#127926),.UNSPECIFIED.,.F.,.F.,(4,2,4),(-0.0253028196011567,-0.0126513834190112,
0.),.UNSPECIFIED.);
#22764=B_SPLINE_CURVE_WITH_KNOTS('',3,(#127946,#127947,#127948,#127949,
#127950,#127951),.UNSPECIFIED.,.F.,.F.,(4,2,4),(-0.0253028454527611,-0.0126513896648064,
0.),.UNSPECIFIED.);
#22765=B_SPLINE_CURVE_WITH_KNOTS('',3,(#127971,#127972,#127973,#127974,
#127975,#127976),.UNSPECIFIED.,.F.,.F.,(4,2,4),(-0.025302850388932,-0.0126513908575762,
0.),.UNSPECIFIED.);
#22766=B_SPLINE_CURVE_WITH_KNOTS('',3,(#127996,#127997,#127998,#127999,
#128000,#128001),.UNSPECIFIED.,.F.,.F.,(4,2,4),(-0.0253033843897737,-0.0126515788041554,
0.),.UNSPECIFIED.);
#22767=B_SPLINE_CURVE_WITH_KNOTS('',3,(#128021,#128022,#128023,#128024,
#128025,#128026),.UNSPECIFIED.,.F.,.F.,(4,2,4),(-0.0253033832420356,-0.0126515785261838,
0.),.UNSPECIFIED.);
#22768=B_SPLINE_CURVE_WITH_KNOTS('',3,(#128046,#128047,#128048,#128049,
#128050,#128051),.UNSPECIFIED.,.F.,.F.,(4,2,4),(-0.0253033740386864,-0.0126515763143982,
0.),.UNSPECIFIED.);
#22769=B_SPLINE_CURVE_WITH_KNOTS('',3,(#128071,#128072,#128073,#128074,
#128075,#128076),.UNSPECIFIED.,.F.,.F.,(4,2,4),(-0.0253033861264452,-0.0126515792102181,
0.),.UNSPECIFIED.);
#22770=B_SPLINE_CURVE_WITH_KNOTS('',3,(#128096,#128097,#128098,#128099,
#128100,#128101),.UNSPECIFIED.,.F.,.F.,(4,2,4),(-0.0253033810482984,-0.0126515780031574,
0.),.UNSPECIFIED.);
#22771=B_SPLINE_CURVE_WITH_KNOTS('',3,(#128121,#128122,#128123,#128124,
#128125,#128126),.UNSPECIFIED.,.F.,.F.,(4,2,4),(-0.0253033777369397,-0.0126515772095753,
0.),.UNSPECIFIED.);
#22772=B_SPLINE_CURVE_WITH_KNOTS('',3,(#128146,#128147,#128148,#128149,
#128150,#128151),.UNSPECIFIED.,.F.,.F.,(4,2,4),(-0.0253033817433229,-0.0126515781718898,
0.),.UNSPECIFIED.);
#22773=B_SPLINE_CURVE_WITH_KNOTS('',3,(#128171,#128172,#128173,#128174,
#128175,#128176),.UNSPECIFIED.,.F.,.F.,(4,2,4),(-0.0253033806303322,-0.0126515778996289,
0.),.UNSPECIFIED.);
#22774=B_SPLINE_CURVE_WITH_KNOTS('',3,(#128196,#128197,#128198,#128199,
#128200,#128201),.UNSPECIFIED.,.F.,.F.,(4,2,4),(-0.0253033856248397,-0.0126515790956557,
0.),.UNSPECIFIED.);
#22775=B_SPLINE_CURVE_WITH_KNOTS('',3,(#128221,#128222,#128223,#128224,
#128225,#128226),.UNSPECIFIED.,.F.,.F.,(4,2,4),(-0.0253033748819442,-0.0126515765228282,
0.),.UNSPECIFIED.);
#22776=B_SPLINE_CURVE_WITH_KNOTS('',3,(#128246,#128247,#128248,#128249,
#128250,#128251),.UNSPECIFIED.,.F.,.F.,(4,2,4),(-0.0253033797315389,-0.0126515776842218,
0.),.UNSPECIFIED.);
#22777=B_SPLINE_CURVE_WITH_KNOTS('',3,(#128271,#128272,#128273,#128274,
#128275,#128276),.UNSPECIFIED.,.F.,.F.,(4,2,4),(-0.0253033826888565,-0.0126515783920459,
0.),.UNSPECIFIED.);
#22778=B_SPLINE_CURVE_WITH_KNOTS('',3,(#128296,#128297,#128298,#128299,
#128300,#128301),.UNSPECIFIED.,.F.,.F.,(4,2,4),(-0.0253033840777337,-0.0126515787360371,
0.),.UNSPECIFIED.);
#22779=B_SPLINE_CURVE_WITH_KNOTS('',3,(#128321,#128322,#128323,#128324,
#128325,#128326),.UNSPECIFIED.,.F.,.F.,(4,2,4),(-0.0253033822757597,-0.0126515782887475,
0.),.UNSPECIFIED.);
#22780=B_SPLINE_CURVE_WITH_KNOTS('',3,(#128346,#128347,#128348,#128349,
#128350,#128351),.UNSPECIFIED.,.F.,.F.,(4,2,4),(-0.0253033742799991,-0.0126515763728792,
0.),.UNSPECIFIED.);
#22781=B_SPLINE_CURVE_WITH_KNOTS('',3,(#128371,#128372,#128373,#128374,
#128375,#128376),.UNSPECIFIED.,.F.,.F.,(4,2,4),(-0.0253033801552282,-0.0126515778085634,
0.),.UNSPECIFIED.);
#22782=B_SPLINE_CURVE_WITH_KNOTS('',3,(#128396,#128397,#128398,#128399,
#128400,#128401),.UNSPECIFIED.,.F.,.F.,(4,2,4),(-0.0253033803562783,-0.0126515778479792,
0.),.UNSPECIFIED.);
#22783=B_SPLINE_CURVE_WITH_KNOTS('',3,(#128421,#128422,#128423,#128424,
#128425,#128426),.UNSPECIFIED.,.F.,.F.,(4,2,4),(-0.0253033694534652,-0.012651575195471,
0.),.UNSPECIFIED.);
#22784=B_SPLINE_CURVE_WITH_KNOTS('',3,(#128446,#128447,#128448,#128449,
#128450,#128451),.UNSPECIFIED.,.F.,.F.,(4,2,4),(-0.0253033830525098,-0.0126515784811636,
0.),.UNSPECIFIED.);
#22785=B_SPLINE_CURVE_WITH_KNOTS('',3,(#128471,#128472,#128473,#128474,
#128475,#128476),.UNSPECIFIED.,.F.,.F.,(4,2,4),(-0.0253033843082028,-0.0126515787848035,
0.),.UNSPECIFIED.);
#22786=B_SPLINE_CURVE_WITH_KNOTS('',3,(#128496,#128497,#128498,#128499,
#128500,#128501),.UNSPECIFIED.,.F.,.F.,(4,2,4),(-0.0253033812413081,-0.0126515780528382,
0.),.UNSPECIFIED.);
#22787=B_SPLINE_CURVE_WITH_KNOTS('',3,(#128521,#128522,#128523,#128524,
#128525,#128526),.UNSPECIFIED.,.F.,.F.,(4,2,4),(-0.0253033830476991,-0.0126515784832709,
0.),.UNSPECIFIED.);
#22788=B_SPLINE_CURVE_WITH_KNOTS('',3,(#128546,#128547,#128548,#128549,
#128550,#128551),.UNSPECIFIED.,.F.,.F.,(4,2,4),(-0.0253033836750068,-0.0126515786334012,
0.),.UNSPECIFIED.);
#22789=B_SPLINE_CURVE_WITH_KNOTS('',3,(#128571,#128572,#128573,#128574,
#128575,#128576),.UNSPECIFIED.,.F.,.F.,(4,2,4),(-0.0253033825810839,-0.0126515756532059,
0.),.UNSPECIFIED.);
#22790=B_SPLINE_CURVE_WITH_KNOTS('',3,(#128596,#128597,#128598,#128599,
#128600,#128601),.UNSPECIFIED.,.F.,.F.,(4,2,4),(-0.0253033895259107,-0.0126515800295567,
0.),.UNSPECIFIED.);
#22791=B_SPLINE_CURVE_WITH_KNOTS('',3,(#128621,#128622,#128623,#128624,
#128625,#128626),.UNSPECIFIED.,.F.,.F.,(4,2,4),(-0.0253033761450526,-0.0126515768170734,
0.),.UNSPECIFIED.);
#22792=B_SPLINE_CURVE_WITH_KNOTS('',3,(#128646,#128647,#128648,#128649,
#128650,#128651),.UNSPECIFIED.,.F.,.F.,(4,2,4),(-0.025303373204294,-0.0126515760996267,
0.),.UNSPECIFIED.);
#22793=B_SPLINE_CURVE_WITH_KNOTS('',3,(#128671,#128672,#128673,#128674,
#128675,#128676),.UNSPECIFIED.,.F.,.F.,(4,2,4),(-0.0253033948806666,-0.0126515786313182,
0.),.UNSPECIFIED.);
#22794=B_SPLINE_CURVE_WITH_KNOTS('',3,(#128696,#128697,#128698,#128699,
#128700,#128701),.UNSPECIFIED.,.F.,.F.,(4,2,4),(-0.0253033736777205,-0.0126515762376764,
0.),.UNSPECIFIED.);
#22795=B_SPLINE_CURVE_WITH_KNOTS('',3,(#128723,#128724,#128725,#128726,
#128727,#128728),.UNSPECIFIED.,.F.,.F.,(4,2,4),(-0.0253043033132767,-0.0126520369393918,
-6.38408319264538E-10),.UNSPECIFIED.);
#22796=B_SPLINE_CURVE_WITH_KNOTS('',3,(#128742,#128743,#128744,#128745,
#128746,#128747),.UNSPECIFIED.,.F.,.F.,(4,2,4),(0.,0.0126520362387386,0.0253042905785001),
 .UNSPECIFIED.);
#22797=B_SPLINE_CURVE_WITH_KNOTS('',3,(#128779,#128780,#128781,#128782,
#128783,#128784),.UNSPECIFIED.,.F.,.F.,(4,2,4),(0.,0.0126520361926197,0.0253043033152966),
 .UNSPECIFIED.);
#22798=B_SPLINE_CURVE_WITH_KNOTS('',3,(#128816,#128817,#128818,#128819,
#128820,#128821),.UNSPECIFIED.,.F.,.F.,(4,2,4),(0.,0.0126520362195973,0.0253043033558742),
 .UNSPECIFIED.);
#22799=B_SPLINE_CURVE_WITH_KNOTS('',3,(#128853,#128854,#128855,#128856,
#128857,#128858),.UNSPECIFIED.,.F.,.F.,(4,2,4),(0.,0.0126520361797729,0.025304303294787),
 .UNSPECIFIED.);
#22800=B_SPLINE_CURVE_WITH_KNOTS('',3,(#128890,#128891,#128892,#128893,
#128894,#128895),.UNSPECIFIED.,.F.,.F.,(4,2,4),(0.,0.0126520361573668,0.0253043032401671),
 .UNSPECIFIED.);
#22801=B_SPLINE_CURVE_WITH_KNOTS('',3,(#128927,#128928,#128929,#128930,
#128931,#128932),.UNSPECIFIED.,.F.,.F.,(4,2,4),(0.,0.0126520361926624,0.0253043032962206),
 .UNSPECIFIED.);
#22802=B_SPLINE_CURVE_WITH_KNOTS('',3,(#128961,#128962,#128963,#128964,
#128965,#128966),.UNSPECIFIED.,.F.,.F.,(4,2,4),(0.,0.0126520361036732,0.0253043031691565),
 .UNSPECIFIED.);
#22803=B_SPLINE_CURVE_WITH_KNOTS('',3,(#128992,#128993,#128994,#128995,
#128996,#128997),.UNSPECIFIED.,.F.,.F.,(4,2,4),(0.,0.0126520361585796,0.0253043032725374),
 .UNSPECIFIED.);
#22804=B_SPLINE_CURVE_WITH_KNOTS('',3,(#129029,#129030,#129031,#129032,
#129033,#129034),.UNSPECIFIED.,.F.,.F.,(4,2,4),(0.,0.0126520362195468,0.0253043033535025),
 .UNSPECIFIED.);
#22805=B_SPLINE_CURVE_WITH_KNOTS('',3,(#129066,#129067,#129068,#129069,
#129070,#129071),.UNSPECIFIED.,.F.,.F.,(4,2,4),(0.,0.0126520362088481,0.0253043033103538),
 .UNSPECIFIED.);
#22806=B_SPLINE_CURVE_WITH_KNOTS('',3,(#129103,#129104,#129105,#129106,
#129107,#129108),.UNSPECIFIED.,.F.,.F.,(4,2,4),(0.,0.0126520361410593,0.0253043032289179),
 .UNSPECIFIED.);
#22807=B_SPLINE_CURVE_WITH_KNOTS('',3,(#129140,#129141,#129142,#129143,
#129144,#129145),.UNSPECIFIED.,.F.,.F.,(4,2,4),(0.,0.0126520362269873,0.0253043033582737),
 .UNSPECIFIED.);
#22808=B_SPLINE_CURVE_WITH_KNOTS('',3,(#129177,#129178,#129179,#129180,
#129181,#129182),.UNSPECIFIED.,.F.,.F.,(4,2,4),(0.,0.012652036199835,0.0253043032947752),
 .UNSPECIFIED.);
#22809=B_SPLINE_CURVE_WITH_KNOTS('',3,(#129214,#129215,#129216,#129217,
#129218,#129219),.UNSPECIFIED.,.F.,.F.,(4,2,4),(0.,0.0126520361816904,0.0253043032966714),
 .UNSPECIFIED.);
#22810=B_SPLINE_CURVE_WITH_KNOTS('',3,(#129251,#129252,#129253,#129254,
#129255,#129256),.UNSPECIFIED.,.F.,.F.,(4,2,4),(0.,0.0126520362137016,0.0253043033359496),
 .UNSPECIFIED.);
#22811=B_SPLINE_CURVE_WITH_KNOTS('',3,(#129288,#129289,#129290,#129291,
#129292,#129293),.UNSPECIFIED.,.F.,.F.,(4,2,4),(0.,0.0126520361685449,0.025304303271054),
 .UNSPECIFIED.);
#22812=B_SPLINE_CURVE_WITH_KNOTS('',3,(#129325,#129326,#129327,#129328,
#129329,#129330),.UNSPECIFIED.,.F.,.F.,(4,2,4),(0.,0.0126520362138179,0.0253043033188563),
 .UNSPECIFIED.);
#22813=B_SPLINE_CURVE_WITH_KNOTS('',3,(#129362,#129363,#129364,#129365,
#129366,#129367),.UNSPECIFIED.,.F.,.F.,(4,2,4),(0.,0.0126520362234447,0.0253043033614193),
 .UNSPECIFIED.);
#22814=B_SPLINE_CURVE_WITH_KNOTS('',3,(#129399,#129400,#129401,#129402,
#129403,#129404),.UNSPECIFIED.,.F.,.F.,(4,2,4),(0.,0.012652036196369,0.0253043033046761),
 .UNSPECIFIED.);
#22815=B_SPLINE_CURVE_WITH_KNOTS('',3,(#129436,#129437,#129438,#129439,
#129440,#129441),.UNSPECIFIED.,.F.,.F.,(4,2,4),(0.,0.0126520361957964,0.0253043033114854),
 .UNSPECIFIED.);
#22816=B_SPLINE_CURVE_WITH_KNOTS('',3,(#129473,#129474,#129475,#129476,
#129477,#129478),.UNSPECIFIED.,.F.,.F.,(4,2,4),(0.,0.0126520362475334,0.025304303358282),
 .UNSPECIFIED.);
#22817=B_SPLINE_CURVE_WITH_KNOTS('',3,(#129511,#129512,#129513,#129514,
#129515,#129516),.UNSPECIFIED.,.F.,.F.,(4,2,4),(0.,0.0126520362011008,0.0253043033315781),
 .UNSPECIFIED.);
#22818=B_SPLINE_CURVE_WITH_KNOTS('',3,(#129547,#129548,#129549,#129550,
#129551,#129552),.UNSPECIFIED.,.F.,.F.,(4,2,4),(0.,0.0126520361475817,0.0253042904271869),
 .UNSPECIFIED.);
#22819=B_SPLINE_CURVE_WITH_KNOTS('',3,(#129584,#129585,#129586,#129587,
#129588,#129589),.UNSPECIFIED.,.F.,.F.,(4,2,4),(0.,0.0126520361853694,0.0253043032746957),
 .UNSPECIFIED.);
#22820=B_SPLINE_CURVE_WITH_KNOTS('',3,(#129621,#129622,#129623,#129624,
#129625,#129626),.UNSPECIFIED.,.F.,.F.,(4,2,4),(0.,0.0126520361360175,0.0253043032161038),
 .UNSPECIFIED.);
#22821=B_SPLINE_CURVE_WITH_KNOTS('',3,(#129658,#129659,#129660,#129661,
#129662,#129663),.UNSPECIFIED.,.F.,.F.,(4,2,4),(0.,0.0126520361850182,0.0253043032915964),
 .UNSPECIFIED.);
#22822=B_SPLINE_CURVE_WITH_KNOTS('',3,(#129695,#129696,#129697,#129698,
#129699,#129700),.UNSPECIFIED.,.F.,.F.,(4,2,4),(0.,0.0126520361578346,0.0253043032710374),
 .UNSPECIFIED.);
#22823=B_SPLINE_CURVE_WITH_KNOTS('',3,(#129732,#129733,#129734,#129735,
#129736,#129737),.UNSPECIFIED.,.F.,.F.,(4,2,4),(0.,0.0126520361522041,0.025304303253814),
 .UNSPECIFIED.);
#22824=B_SPLINE_CURVE_WITH_KNOTS('',3,(#129780,#129781,#129782,#129783,
#129784,#129785),.UNSPECIFIED.,.F.,.F.,(4,2,4),(-0.0253000309094781,-0.0126498687848718,
-4.91224203674756E-10),.UNSPECIFIED.);
#22825=B_SPLINE_CURVE_WITH_KNOTS('',3,(#129803,#129804,#129805,#129806,
#129807,#129808),.UNSPECIFIED.,.F.,.F.,(4,2,4),(1.78041757562141E-11,0.0126499269416387,
0.0253002644237282),.UNSPECIFIED.);
#22826=B_SPLINE_CURVE_WITH_KNOTS('',3,(#129836,#129837,#129838,#129839,
#129840,#129841),.UNSPECIFIED.,.F.,.F.,(4,2,4),(0.,0.0126499190882602,0.025300232813381),
 .UNSPECIFIED.);
#22827=B_SPLINE_CURVE_WITH_KNOTS('',3,(#129869,#129870,#129871,#129872,
#129873,#129874),.UNSPECIFIED.,.F.,.F.,(4,2,4),(0.,0.0126499179894866,0.0253002280646286),
 .UNSPECIFIED.);
#22828=B_SPLINE_CURVE_WITH_KNOTS('',3,(#129902,#129903,#129904,#129905,
#129906,#129907),.UNSPECIFIED.,.F.,.F.,(4,2,4),(0.,0.0126499160711492,0.0253002173995517),
 .UNSPECIFIED.);
#22829=B_SPLINE_CURVE_WITH_KNOTS('',3,(#129935,#129936,#129937,#129938,
#129939,#129940),.UNSPECIFIED.,.F.,.F.,(4,2,4),(0.,0.0126499241869609,0.0253002547372993),
 .UNSPECIFIED.);
#22830=B_SPLINE_CURVE_WITH_KNOTS('',3,(#129968,#129969,#129970,#129971,
#129972,#129973),.UNSPECIFIED.,.F.,.F.,(4,2,4),(0.,0.012649920952608,0.0253002398139683),
 .UNSPECIFIED.);
#22831=B_SPLINE_CURVE_WITH_KNOTS('',3,(#130001,#130002,#130003,#130004,
#130005,#130006),.UNSPECIFIED.,.F.,.F.,(4,2,4),(0.,0.0126499122637278,0.0253002035574413),
 .UNSPECIFIED.);
#22832=B_SPLINE_CURVE_WITH_KNOTS('',3,(#130034,#130035,#130036,#130037,
#130038,#130039),.UNSPECIFIED.,.F.,.F.,(4,2,4),(0.,0.0126499201850027,0.0253002413629696),
 .UNSPECIFIED.);
#22833=B_SPLINE_CURVE_WITH_KNOTS('',3,(#130067,#130068,#130069,#130070,
#130071,#130072),.UNSPECIFIED.,.F.,.F.,(4,2,4),(0.,0.0126499197289081,0.0253002334179211),
 .UNSPECIFIED.);
#22834=B_SPLINE_CURVE_WITH_KNOTS('',3,(#130100,#130101,#130102,#130103,
#130104,#130105),.UNSPECIFIED.,.F.,.F.,(4,2,4),(3.40689536786532E-11,0.0126499313200275,
0.025300279930029),.UNSPECIFIED.);
#22835=B_SPLINE_CURVE_WITH_KNOTS('',3,(#130133,#130134,#130135,#130136,
#130137,#130138),.UNSPECIFIED.,.F.,.F.,(4,2,4),(0.,0.0126499129678583,0.0253002083264279),
 .UNSPECIFIED.);
#22836=B_SPLINE_CURVE_WITH_KNOTS('',3,(#130166,#130167,#130168,#130169,
#130170,#130171),.UNSPECIFIED.,.F.,.F.,(4,2,4),(0.,0.0126499173031919,0.0253002270982126),
 .UNSPECIFIED.);
#22837=B_SPLINE_CURVE_WITH_KNOTS('',3,(#130199,#130200,#130201,#130202,
#130203,#130204),.UNSPECIFIED.,.F.,.F.,(4,2,4),(0.,0.0126499174786902,0.0253002255234055),
 .UNSPECIFIED.);
#22838=B_SPLINE_CURVE_WITH_KNOTS('',3,(#130229,#130230,#130231,#130232,
#130233,#130234),.UNSPECIFIED.,.F.,.F.,(4,2,4),(0.,0.0126499218690464,0.0253002426716667),
 .UNSPECIFIED.);
#22839=B_SPLINE_CURVE_WITH_KNOTS('',3,(#130256,#130257,#130258,#130259,
#130260,#130261),.UNSPECIFIED.,.F.,.F.,(4,2,4),(3.66601265270061E-13,0.0126499208786554,
0.0253002406126026),.UNSPECIFIED.);
#22840=B_SPLINE_CURVE_WITH_KNOTS('',3,(#130289,#130290,#130291,#130292,
#130293,#130294),.UNSPECIFIED.,.F.,.F.,(4,2,4),(0.,0.0126499118483472,0.025300203303257),
 .UNSPECIFIED.);
#22841=B_SPLINE_CURVE_WITH_KNOTS('',3,(#130322,#130323,#130324,#130325,
#130326,#130327),.UNSPECIFIED.,.F.,.F.,(4,2,4),(0.,0.0126499224943342,0.0253002451178913),
 .UNSPECIFIED.);
#22842=B_SPLINE_CURVE_WITH_KNOTS('',3,(#130355,#130356,#130357,#130358,
#130359,#130360),.UNSPECIFIED.,.F.,.F.,(4,2,4),(0.,0.0126499208891092,0.0253002369915565),
 .UNSPECIFIED.);
#22843=B_SPLINE_CURVE_WITH_KNOTS('',3,(#130388,#130389,#130390,#130391,
#130392,#130393),.UNSPECIFIED.,.F.,.F.,(4,2,4),(0.,0.0126499173509548,0.02530022847158),
 .UNSPECIFIED.);
#22844=B_SPLINE_CURVE_WITH_KNOTS('',3,(#130421,#130422,#130423,#130424,
#130425,#130426),.UNSPECIFIED.,.F.,.F.,(4,2,4),(0.,0.0126499220452902,0.0253002430940821),
 .UNSPECIFIED.);
#22845=B_SPLINE_CURVE_WITH_KNOTS('',3,(#130454,#130455,#130456,#130457,
#130458,#130459),.UNSPECIFIED.,.F.,.F.,(4,2,4),(0.,0.0126499180091474,0.0253002282305368),
 .UNSPECIFIED.);
#22846=B_SPLINE_CURVE_WITH_KNOTS('',3,(#130487,#130488,#130489,#130490,
#130491,#130492),.UNSPECIFIED.,.F.,.F.,(4,2,4),(0.,0.012649918574299,0.0253002280488269),
 .UNSPECIFIED.);
#22847=B_SPLINE_CURVE_WITH_KNOTS('',3,(#130520,#130521,#130522,#130523,
#130524,#130525),.UNSPECIFIED.,.F.,.F.,(4,2,4),(1.8513899150215E-12,0.0126499209523983,
0.0253002401365578),.UNSPECIFIED.);
#22848=B_SPLINE_CURVE_WITH_KNOTS('',3,(#130553,#130554,#130555,#130556,
#130557,#130558),.UNSPECIFIED.,.F.,.F.,(4,2,4),(0.,0.0126499148037353,0.0253002131144609),
 .UNSPECIFIED.);
#22849=B_SPLINE_CURVE_WITH_KNOTS('',3,(#130586,#130587,#130588,#130589,
#130590,#130591),.UNSPECIFIED.,.F.,.F.,(4,2,4),(0.,0.0126499223276825,0.025300244583305),
 .UNSPECIFIED.);
#22850=B_SPLINE_CURVE_WITH_KNOTS('',3,(#130619,#130620,#130621,#130622,
#130623,#130624),.UNSPECIFIED.,.F.,.F.,(4,2,4),(0.,0.0126499138887409,0.0253002122279321),
 .UNSPECIFIED.);
#22851=B_SPLINE_CURVE_WITH_KNOTS('',3,(#130652,#130653,#130654,#130655,
#130656,#130657),.UNSPECIFIED.,.F.,.F.,(4,2,4),(0.,0.0126499283749239,0.025300265794938),
 .UNSPECIFIED.);
#22852=B_SPLINE_CURVE_WITH_KNOTS('',3,(#130685,#130686,#130687,#130688,
#130689,#130690),.UNSPECIFIED.,.F.,.F.,(4,2,4),(5.49015481529974E-12,0.0126499266970771,
0.0253002635542269),.UNSPECIFIED.);
#22853=B_SPLINE_CURVE_WITH_KNOTS('',3,(#130729,#130730,#130731,#130732,
#130733,#130734,#130735,#130736,#130737,#130738),.UNSPECIFIED.,.F.,.F.,
(4,3,3,4),(2.21153070827588E-11,8.70314493453333E-5,0.00017002405947175,
0.000253018845956519),.UNSPECIFIED.);
#22854=B_SPLINE_CURVE_WITH_KNOTS('',3,(#130750,#130751,#130752,#130753,
#130754,#130755,#130756,#130757,#130758,#130759),.UNSPECIFIED.,.F.,.F.,
(4,3,3,4),(0.487155140750431,0.491874896926658,0.501682966399308,0.504614996906574),
 .UNSPECIFIED.);
#22855=B_SPLINE_CURVE_WITH_KNOTS('',3,(#130760,#130761,#130762,#130763,
#130764,#130765,#130766,#130767,#130768,#130769),.UNSPECIFIED.,.F.,.F.,
(4,3,3,4),(3.45096454849108E-14,8.70313175711171E-5,0.000170023946878408,
0.000253018998164665),.UNSPECIFIED.);
#22856=B_SPLINE_CURVE_WITH_KNOTS('',3,(#130788,#130789,#130790,#130791,
#130792,#130793,#130794,#130795,#130796,#130797),.UNSPECIFIED.,.F.,.F.,
(4,3,3,4),(0.487155140750431,0.491874896926659,0.501682934290902,0.504614996906058),
 .UNSPECIFIED.);
#22857=B_SPLINE_CURVE_WITH_KNOTS('',3,(#130798,#130799,#130800,#130801,
#130802,#130803,#130804,#130805,#130806,#130807),.UNSPECIFIED.,.F.,.F.,
(4,3,3,4),(4.42529392960305E-14,8.70313175297394E-5,0.000170023946584964,
0.000253018997273752),.UNSPECIFIED.);
#22858=B_SPLINE_CURVE_WITH_KNOTS('',3,(#130826,#130827,#130828,#130829,
#130830,#130831,#130832,#130833,#130834,#130835),.UNSPECIFIED.,.F.,.F.,
(4,3,3,4),(0.487155141219239,0.491874896926658,0.5016829678529,0.504614997100588),
 .UNSPECIFIED.);
#22859=B_SPLINE_CURVE_WITH_KNOTS('',3,(#130836,#130837,#130838,#130839,
#130840,#130841,#130842,#130843,#130844,#130845),.UNSPECIFIED.,.F.,.F.,
(4,3,3,4),(4.40863300248104E-14,8.70313175424259E-5,0.000170023946631832,
0.000253018997693025),.UNSPECIFIED.);
#22860=B_SPLINE_CURVE_WITH_KNOTS('',3,(#130864,#130865,#130866,#130867,
#130868,#130869,#130870,#130871,#130872,#130873),.UNSPECIFIED.,.F.,.F.,
(4,3,3,4),(0.48715514075043,0.491874896926658,0.501682951102274,0.504614996907853),
 .UNSPECIFIED.);
#22861=B_SPLINE_CURVE_WITH_KNOTS('',3,(#130874,#130875,#130876,#130877,
#130878,#130879,#130880,#130881,#130882,#130883),.UNSPECIFIED.,.F.,.F.,
(4,3,3,4),(3.46722191321165E-14,8.70313175915362E-5,0.000170023946671659,
0.00025301899802548),.UNSPECIFIED.);
#22862=B_SPLINE_CURVE_WITH_KNOTS('',3,(#130902,#130903,#130904,#130905,
#130906,#130907,#130908,#130909,#130910,#130911),.UNSPECIFIED.,.F.,.F.,
(4,3,3,4),(0.487155140750431,0.491874896926659,0.501682951028305,0.50461499691759),
 .UNSPECIFIED.);
#22863=B_SPLINE_CURVE_WITH_KNOTS('',3,(#130912,#130913,#130914,#130915,
#130916,#130917,#130918,#130919,#130920,#130921),.UNSPECIFIED.,.F.,.F.,
(4,3,3,4),(4.40712627940313E-15,8.70313176441398E-5,0.000170023946915369,
0.000253018998042543),.UNSPECIFIED.);
#22864=B_SPLINE_CURVE_WITH_KNOTS('',3,(#130940,#130941,#130942,#130943,
#130944,#130945,#130946,#130947,#130948,#130949),.UNSPECIFIED.,.F.,.F.,
(4,3,3,4),(0.48715514075043,0.491874896926657,0.501682983217295,0.504614996910036),
 .UNSPECIFIED.);
#22865=B_SPLINE_CURVE_WITH_KNOTS('',3,(#130950,#130951,#130952,#130953,
#130954,#130955,#130956,#130957,#130958,#130959),.UNSPECIFIED.,.F.,.F.,
(4,3,3,4),(2.20993341838628E-14,8.7031317575276E-5,0.000170023946675526,
0.000253018997790063),.UNSPECIFIED.);
#22866=B_SPLINE_CURVE_WITH_KNOTS('',3,(#130978,#130979,#130980,#130981,
#130982,#130983,#130984,#130985,#130986,#130987),.UNSPECIFIED.,.F.,.F.,
(4,3,3,4),(0.487155140750431,0.491874896926659,0.501682969053896,0.504614996915088),
 .UNSPECIFIED.);
#22867=B_SPLINE_CURVE_WITH_KNOTS('',3,(#130988,#130989,#130990,#130991,
#130992,#130993,#130994,#130995,#130996,#130997),.UNSPECIFIED.,.F.,.F.,
(4,3,3,4),(1.50225347390965E-14,8.70313178726407E-5,0.000170023946784008,
0.000253018997413668),.UNSPECIFIED.);
#22868=B_SPLINE_CURVE_WITH_KNOTS('',3,(#131016,#131017,#131018,#131019,
#131020,#131021,#131022,#131023,#131024,#131025),.UNSPECIFIED.,.F.,.F.,
(4,3,3,4),(0.487155140750431,0.491874896926659,0.501682955711557,0.5046149968907),
 .UNSPECIFIED.);
#22869=B_SPLINE_CURVE_WITH_KNOTS('',3,(#131026,#131027,#131028,#131029,
#131030,#131031,#131032,#131033,#131034,#131035),.UNSPECIFIED.,.F.,.F.,
(4,3,3,4),(2.40986300177914E-14,8.70313176284771E-5,0.000170023946621484,
0.000253018997382508),.UNSPECIFIED.);
#22870=B_SPLINE_CURVE_WITH_KNOTS('',3,(#131054,#131055,#131056,#131057,
#131058,#131059,#131060,#131061,#131062,#131063),.UNSPECIFIED.,.F.,.F.,
(4,3,3,4),(0.487155140750431,0.491874896926659,0.501682948684918,0.504614996896031),
 .UNSPECIFIED.);
#22871=B_SPLINE_CURVE_WITH_KNOTS('',3,(#131064,#131065,#131066,#131067,
#131068,#131069,#131070,#131071,#131072,#131073),.UNSPECIFIED.,.F.,.F.,
(4,3,3,4),(5.11111839094562E-14,8.70313176670455E-5,0.000170023946742311,
0.000253018998036814),.UNSPECIFIED.);
#22872=B_SPLINE_CURVE_WITH_KNOTS('',3,(#131092,#131093,#131094,#131095,
#131096,#131097,#131098,#131099,#131100,#131101),.UNSPECIFIED.,.F.,.F.,
(4,3,3,4),(0.487155140750431,0.491874896926659,0.501682945300711,0.504614996917612),
 .UNSPECIFIED.);
#22873=B_SPLINE_CURVE_WITH_KNOTS('',3,(#131102,#131103,#131104,#131105,
#131106,#131107,#131108,#131109,#131110,#131111),.UNSPECIFIED.,.F.,.F.,
(4,3,3,4),(1.09252828245397E-14,8.70313177939855E-5,0.000170023946750202,
0.000253018997298873),.UNSPECIFIED.);
#22874=B_SPLINE_CURVE_WITH_KNOTS('',3,(#131130,#131131,#131132,#131133,
#131134,#131135,#131136,#131137,#131138,#131139),.UNSPECIFIED.,.F.,.F.,
(4,3,3,4),(0.487155140750431,0.491874896926659,0.501682936956871,0.504614996892545),
 .UNSPECIFIED.);
#22875=B_SPLINE_CURVE_WITH_KNOTS('',3,(#131140,#131141,#131142,#131143,
#131144,#131145,#131146,#131147,#131148,#131149),.UNSPECIFIED.,.F.,.F.,
(4,3,3,4),(8.03179267346919E-14,8.70313175544202E-5,0.00017002394659626,
0.000253018998009225),.UNSPECIFIED.);
#22876=B_SPLINE_CURVE_WITH_KNOTS('',3,(#131168,#131169,#131170,#131171,
#131172,#131173,#131174,#131175,#131176,#131177),.UNSPECIFIED.,.F.,.F.,
(4,3,3,4),(0.487155140750431,0.491874896926659,0.50168294484991,0.504614996903372),
 .UNSPECIFIED.);
#22877=B_SPLINE_CURVE_WITH_KNOTS('',3,(#131178,#131179,#131180,#131181,
#131182,#131183,#131184,#131185,#131186,#131187),.UNSPECIFIED.,.F.,.F.,
(4,3,3,4),(2.68559350286825E-15,8.70313176641771E-5,0.000170023946805897,
0.000253018998059253),.UNSPECIFIED.);
#22878=B_SPLINE_CURVE_WITH_KNOTS('',3,(#131206,#131207,#131208,#131209,
#131210,#131211,#131212,#131213,#131214,#131215),.UNSPECIFIED.,.F.,.F.,
(4,3,3,4),(0.487155140750431,0.491874896926659,0.501682963492984,0.504614996928294),
 .UNSPECIFIED.);
#22879=B_SPLINE_CURVE_WITH_KNOTS('',3,(#131216,#131217,#131218,#131219,
#131220,#131221,#131222,#131223,#131224,#131225),.UNSPECIFIED.,.F.,.F.,
(4,3,3,4),(5.89210988424711E-14,8.70313175998042E-5,0.000170023946622594,
0.000253018997350292),.UNSPECIFIED.);
#22880=B_SPLINE_CURVE_WITH_KNOTS('',3,(#131244,#131245,#131246,#131247,
#131248,#131249,#131250,#131251,#131252,#131253),.UNSPECIFIED.,.F.,.F.,
(4,3,3,4),(0.487155140750431,0.491874896926659,0.501682946832188,0.504614996917156),
 .UNSPECIFIED.);
#22881=B_SPLINE_CURVE_WITH_KNOTS('',3,(#131254,#131255,#131256,#131257,
#131258,#131259,#131260,#131261,#131262,#131263),.UNSPECIFIED.,.F.,.F.,
(4,3,3,4),(2.38020884134642E-14,8.70313176307367E-5,0.000170023946762134,
0.000253018997722667),.UNSPECIFIED.);
#22882=B_SPLINE_CURVE_WITH_KNOTS('',3,(#131282,#131283,#131284,#131285,
#131286,#131287,#131288,#131289,#131290,#131291),.UNSPECIFIED.,.F.,.F.,
(4,3,3,4),(0.487155140750431,0.491874896926659,0.501682964139925,0.504614996914888),
 .UNSPECIFIED.);
#22883=B_SPLINE_CURVE_WITH_KNOTS('',3,(#131292,#131293,#131294,#131295,
#131296,#131297,#131298,#131299,#131300,#131301),.UNSPECIFIED.,.F.,.F.,
(4,3,3,4),(5.46374512450486E-14,8.70313176102908E-5,0.000170023946589689,
0.000253018997649783),.UNSPECIFIED.);
#22884=B_SPLINE_CURVE_WITH_KNOTS('',3,(#131320,#131321,#131322,#131323,
#131324,#131325,#131326,#131327,#131328,#131329),.UNSPECIFIED.,.F.,.F.,
(4,3,3,4),(0.487155140750431,0.491874896926659,0.501682932609467,0.504614996903104),
 .UNSPECIFIED.);
#22885=B_SPLINE_CURVE_WITH_KNOTS('',3,(#131330,#131331,#131332,#131333,
#131334,#131335,#131336,#131337,#131338,#131339),.UNSPECIFIED.,.F.,.F.,
(4,3,3,4),(3.40449100493074E-14,8.70313176981428E-5,0.000170023946803936,
0.000253018997932282),.UNSPECIFIED.);
#22886=B_SPLINE_CURVE_WITH_KNOTS('',3,(#131358,#131359,#131360,#131361,
#131362,#131363,#131364,#131365,#131366,#131367),.UNSPECIFIED.,.F.,.F.,
(4,3,3,4),(0.487155140750431,0.491874896926659,0.501682979942645,0.504614996909924),
 .UNSPECIFIED.);
#22887=B_SPLINE_CURVE_WITH_KNOTS('',3,(#131368,#131369,#131370,#131371,
#131372,#131373,#131374,#131375,#131376,#131377),.UNSPECIFIED.,.F.,.F.,
(4,3,3,4),(7.04341793940837E-14,8.70313175559068E-5,0.000170023946529521,
0.000253018997753187),.UNSPECIFIED.);
#22888=B_SPLINE_CURVE_WITH_KNOTS('',3,(#131396,#131397,#131398,#131399,
#131400,#131401,#131402,#131403,#131404,#131405),.UNSPECIFIED.,.F.,.F.,
(4,3,3,4),(0.487155140750431,0.491874896926659,0.501682957929202,0.504614996911627),
 .UNSPECIFIED.);
#22889=B_SPLINE_CURVE_WITH_KNOTS('',3,(#131406,#131407,#131408,#131409,
#131410,#131411,#131412,#131413,#131414,#131415),.UNSPECIFIED.,.F.,.F.,
(4,3,3,4),(5.8236891808638E-14,8.70313175937467E-5,0.00017002394674638,
0.000253018997690592),.UNSPECIFIED.);
#22890=B_SPLINE_CURVE_WITH_KNOTS('',3,(#131434,#131435,#131436,#131437,
#131438,#131439,#131440,#131441,#131442,#131443),.UNSPECIFIED.,.F.,.F.,
(4,3,3,4),(0.487155140750431,0.491874896926659,0.501682960207111,0.504614996926001),
 .UNSPECIFIED.);
#22891=B_SPLINE_CURVE_WITH_KNOTS('',3,(#131444,#131445,#131446,#131447,
#131448,#131449,#131450,#131451,#131452,#131453),.UNSPECIFIED.,.F.,.F.,
(4,3,3,4),(4.35401475432296E-14,8.70313176778195E-5,0.000170023946767764,
0.000253018997628577),.UNSPECIFIED.);
#22892=B_SPLINE_CURVE_WITH_KNOTS('',3,(#131472,#131473,#131474,#131475,
#131476,#131477,#131478,#131479,#131480,#131481),.UNSPECIFIED.,.F.,.F.,
(4,3,3,4),(0.487155140750431,0.491874896926659,0.50168295550842,0.504614996916598),
 .UNSPECIFIED.);
#22893=B_SPLINE_CURVE_WITH_KNOTS('',3,(#131482,#131483,#131484,#131485,
#131486,#131487,#131488,#131489,#131490,#131491),.UNSPECIFIED.,.F.,.F.,
(4,3,3,4),(1.62990603401336E-14,8.70313177195538E-5,0.000170023946752221,
0.000253018997668107),.UNSPECIFIED.);
#22894=B_SPLINE_CURVE_WITH_KNOTS('',3,(#131510,#131511,#131512,#131513,
#131514,#131515,#131516,#131517,#131518,#131519),.UNSPECIFIED.,.F.,.F.,
(4,3,3,4),(0.487155140750431,0.491874896926659,0.501682952896135,0.504614996920383),
 .UNSPECIFIED.);
#22895=B_SPLINE_CURVE_WITH_KNOTS('',3,(#131520,#131521,#131522,#131523,
#131524,#131525,#131526,#131527,#131528,#131529),.UNSPECIFIED.,.F.,.F.,
(4,3,3,4),(1.90242114645572E-14,8.70313177274409E-5,0.000170023946650131,
0.000253018997500558),.UNSPECIFIED.);
#22896=B_SPLINE_CURVE_WITH_KNOTS('',3,(#131548,#131549,#131550,#131551,
#131552,#131553,#131554,#131555,#131556,#131557),.UNSPECIFIED.,.F.,.F.,
(4,3,3,4),(0.487155140750322,0.491874896944685,0.501682945346985,0.5046149969228),
 .UNSPECIFIED.);
#22897=B_SPLINE_CURVE_WITH_KNOTS('',3,(#131558,#131559,#131560,#131561,
#131562,#131563,#131564,#131565,#131566,#131567),.UNSPECIFIED.,.F.,.F.,
(4,3,3,4),(4.49589306676502E-14,8.70313176364226E-5,0.000170023946820726,
0.000253018998381774),.UNSPECIFIED.);
#22898=B_SPLINE_CURVE_WITH_KNOTS('',3,(#131586,#131587,#131588,#131589,
#131590,#131591,#131592,#131593,#131594,#131595),.UNSPECIFIED.,.F.,.F.,
(4,3,3,4),(0.48715514075043,0.491874896926657,0.501682938066946,0.504614996890883),
 .UNSPECIFIED.);
#22899=B_SPLINE_CURVE_WITH_KNOTS('',3,(#131596,#131597,#131598,#131599,
#131600,#131601,#131602,#131603,#131604,#131605),.UNSPECIFIED.,.F.,.F.,
(4,3,3,4),(6.45004693156233E-14,8.70313176737041E-5,0.000170023946903362,
0.000253018998072501),.UNSPECIFIED.);
#22900=B_SPLINE_CURVE_WITH_KNOTS('',3,(#131624,#131625,#131626,#131627,
#131628,#131629,#131630,#131631,#131632,#131633),.UNSPECIFIED.,.F.,.F.,
(4,3,3,4),(0.487155140750429,0.491874896926656,0.501682960511284,0.504614996906757),
 .UNSPECIFIED.);
#22901=B_SPLINE_CURVE_WITH_KNOTS('',3,(#131634,#131635,#131636,#131637,
#131638,#131639,#131640,#131641,#131642,#131643),.UNSPECIFIED.,.F.,.F.,
(4,3,3,4),(8.58872897030667E-14,8.70313175901969E-5,0.000170023946786314,
0.000253018997863018),.UNSPECIFIED.);
#22902=B_SPLINE_CURVE_WITH_KNOTS('',3,(#131662,#131663,#131664,#131665,
#131666,#131667,#131668,#131669,#131670,#131671),.UNSPECIFIED.,.F.,.F.,
(4,3,3,4),(0.487155140750429,0.491874896926656,0.501682948681635,0.504614996927245),
 .UNSPECIFIED.);
#22903=B_SPLINE_CURVE_WITH_KNOTS('',3,(#131672,#131673,#131674,#131675,
#131676,#131677,#131678,#131679,#131680,#131681),.UNSPECIFIED.,.F.,.F.,
(4,3,3,4),(2.08206417731207E-14,8.70313174616608E-5,0.000170023946642585,
0.000253018998155892),.UNSPECIFIED.);
#22904=B_SPLINE_CURVE_WITH_KNOTS('',3,(#131700,#131701,#131702,#131703,
#131704,#131705,#131706,#131707,#131708,#131709),.UNSPECIFIED.,.F.,.F.,
(4,3,3,4),(0.487155140750429,0.491874896926656,0.501682945866074,0.504614996901574),
 .UNSPECIFIED.);
#22905=B_SPLINE_CURVE_WITH_KNOTS('',3,(#131710,#131711,#131712,#131713,
#131714,#131715,#131716,#131717,#131718,#131719),.UNSPECIFIED.,.F.,.F.,
(4,3,3,4),(2.48137664125078E-14,8.70313177460333E-5,0.000170023946742254,
0.000253018997272817),.UNSPECIFIED.);
#22906=B_SPLINE_CURVE_WITH_KNOTS('',3,(#131738,#131739,#131740,#131741,
#131742,#131743,#131744,#131745,#131746,#131747),.UNSPECIFIED.,.F.,.F.,
(4,3,3,4),(0.48715514075043,0.491874896926657,0.50168298795909,0.504614996907841),
 .UNSPECIFIED.);
#22907=B_SPLINE_CURVE_WITH_KNOTS('',3,(#131748,#131749,#131750,#131751,
#131752,#131753,#131754,#131755,#131756,#131757),.UNSPECIFIED.,.F.,.F.,
(4,3,3,4),(3.3796818005368E-14,8.70313175545553E-5,0.000170023946800974,
0.000253018997690298),.UNSPECIFIED.);
#22908=B_SPLINE_CURVE_WITH_KNOTS('',3,(#131776,#131777,#131778,#131779,
#131780,#131781,#131782,#131783,#131784,#131785),.UNSPECIFIED.,.F.,.F.,
(4,3,3,4),(0.487155140750429,0.491874896926655,0.501682932157906,0.504614996931886),
 .UNSPECIFIED.);
#22909=B_SPLINE_CURVE_WITH_KNOTS('',3,(#131786,#131787,#131788,#131789,
#131790,#131791,#131792,#131793,#131794,#131795),.UNSPECIFIED.,.F.,.F.,
(4,3,3,4),(2.07661001644807E-15,8.70313175311407E-5,0.000170023946662789,
0.000253018997995876),.UNSPECIFIED.);
#22910=B_SPLINE_CURVE_WITH_KNOTS('',3,(#131813,#131814,#131815,#131816,
#131817,#131818,#131819,#131820,#131821,#131822),.UNSPECIFIED.,.F.,.F.,
(4,3,3,4),(0.487155140750429,0.491874896926655,0.501682941477529,0.504614996918119),
 .UNSPECIFIED.);
#22911=B_SPLINE_CURVE_WITH_KNOTS('',3,(#131830,#131831,#131832,#131833,
#131834,#131835),.UNSPECIFIED.,.F.,.F.,(4,2,4),(1.57854982172886E-9,0.0126517047617616,
0.0253036326772259),.UNSPECIFIED.);
#22912=B_SPLINE_CURVE_WITH_KNOTS('',3,(#131849,#131850,#131851,#131852,
#131853,#131854),.UNSPECIFIED.,.F.,.F.,(4,2,4),(2.36098174900286E-11,0.012651852400468,
0.0253034805000543),.UNSPECIFIED.);
#22913=B_SPLINE_CURVE_WITH_KNOTS('',3,(#131877,#131878,#131879,#131880,
#131881,#131882),.UNSPECIFIED.,.F.,.F.,(4,2,4),(3.720761616377E-11,0.0126518524995529,
0.0253034806719167),.UNSPECIFIED.);
#22914=B_SPLINE_CURVE_WITH_KNOTS('',3,(#131905,#131906,#131907,#131908,
#131909,#131910),.UNSPECIFIED.,.F.,.F.,(4,2,4),(3.31366397850511E-11,0.0126518524135823,
0.0253034805076842),.UNSPECIFIED.);
#22915=B_SPLINE_CURVE_WITH_KNOTS('',3,(#131933,#131934,#131935,#131936,
#131937,#131938),.UNSPECIFIED.,.F.,.F.,(4,2,4),(1.35863014051303E-11,0.0126518524614331,
0.0253034806458099),.UNSPECIFIED.);
#22916=B_SPLINE_CURVE_WITH_KNOTS('',3,(#131961,#131962,#131963,#131964,
#131965,#131966),.UNSPECIFIED.,.F.,.F.,(4,2,4),(4.31669193783089E-11,0.0126518524382602,
0.0253034805401726),.UNSPECIFIED.);
#22917=B_SPLINE_CURVE_WITH_KNOTS('',3,(#131989,#131990,#131991,#131992,
#131993,#131994),.UNSPECIFIED.,.F.,.F.,(4,2,4),(6.96683009010555E-11,0.0126518525612664,
0.0253034807264326),.UNSPECIFIED.);
#22918=B_SPLINE_CURVE_WITH_KNOTS('',3,(#132017,#132018,#132019,#132020,
#132021,#132022),.UNSPECIFIED.,.F.,.F.,(4,2,4),(4.19890970197388E-11,0.0126518524349447,
0.0253034805319675),.UNSPECIFIED.);
#22919=B_SPLINE_CURVE_WITH_KNOTS('',3,(#132045,#132046,#132047,#132048,
#132049,#132050),.UNSPECIFIED.,.F.,.F.,(4,2,4),(4.79039532650115E-11,0.0126518525289848,
0.025303480711971),.UNSPECIFIED.);
#22920=B_SPLINE_CURVE_WITH_KNOTS('',3,(#132073,#132074,#132075,#132076,
#132077,#132078),.UNSPECIFIED.,.F.,.F.,(4,2,4),(4.44665067478317E-11,0.0126518525087782,
0.0253034806759089),.UNSPECIFIED.);
#22921=B_SPLINE_CURVE_WITH_KNOTS('',3,(#132101,#132102,#132103,#132104,
#132105,#132106),.UNSPECIFIED.,.F.,.F.,(4,2,4),(3.72079750079819E-11,0.0126518524179389,
0.0253034805068538),.UNSPECIFIED.);
#22922=B_SPLINE_CURVE_WITH_KNOTS('',3,(#132129,#132130,#132131,#132132,
#132133,#132134),.UNSPECIFIED.,.F.,.F.,(4,2,4),(3.82846828684018E-11,0.0126518524409263,
0.0253034805527796),.UNSPECIFIED.);
#22923=B_SPLINE_CURVE_WITH_KNOTS('',3,(#132157,#132158,#132159,#132160,
#132161,#132162),.UNSPECIFIED.,.F.,.F.,(4,2,4),(1.79986607487896E-11,0.0126518524642799,
0.0253034806422095),.UNSPECIFIED.);
#22924=B_SPLINE_CURVE_WITH_KNOTS('',3,(#132185,#132186,#132187,#132188,
#132189,#132190),.UNSPECIFIED.,.F.,.F.,(4,2,4),(4.07151250871006E-11,0.012651852533892,
0.0253034807373435),.UNSPECIFIED.);
#22925=B_SPLINE_CURVE_WITH_KNOTS('',3,(#132213,#132214,#132215,#132216,
#132217,#132218),.UNSPECIFIED.,.F.,.F.,(4,2,4),(2.20594989622044E-9,0.0126518535108752,
0.025303480534335),.UNSPECIFIED.);
#22926=B_SPLINE_CURVE_WITH_KNOTS('',3,(#132241,#132242,#132243,#132244,
#132245,#132246),.UNSPECIFIED.,.F.,.F.,(4,2,4),(1.399374402428E-11,0.0126518524586418,
0.0253034806364679),.UNSPECIFIED.);
#22927=B_SPLINE_CURVE_WITH_KNOTS('',3,(#132269,#132270,#132271,#132272,
#132273,#132274),.UNSPECIFIED.,.F.,.F.,(4,2,4),(3.74743840632193E-11,0.0126518525084182,
0.025303480686356),.UNSPECIFIED.);
#22928=B_SPLINE_CURVE_WITH_KNOTS('',3,(#132297,#132298,#132299,#132300,
#132301,#132302),.UNSPECIFIED.,.F.,.F.,(4,2,4),(4.5835016463154E-11,0.0126518524280129,
0.0253034805099347),.UNSPECIFIED.);
#22929=B_SPLINE_CURVE_WITH_KNOTS('',3,(#132325,#132326,#132327,#132328,
#132329,#132330),.UNSPECIFIED.,.F.,.F.,(4,2,4),(3.4966361747514E-11,0.0126518524971628,
0.0253034806732593),.UNSPECIFIED.);
#22930=B_SPLINE_CURVE_WITH_KNOTS('',3,(#132353,#132354,#132355,#132356,
#132357,#132358),.UNSPECIFIED.,.F.,.F.,(4,2,4),(3.97303333440308E-11,0.012651852433962,
0.0253034805347979),.UNSPECIFIED.);
#22931=B_SPLINE_CURVE_WITH_KNOTS('',3,(#132381,#132382,#132383,#132384,
#132385,#132386),.UNSPECIFIED.,.F.,.F.,(4,2,4),(3.27648748939136E-11,0.0126518525041262,
0.0253034806924794),.UNSPECIFIED.);
#22932=B_SPLINE_CURVE_WITH_KNOTS('',3,(#132409,#132410,#132411,#132412,
#132413,#132414),.UNSPECIFIED.,.F.,.F.,(4,2,4),(3.36371781765561E-11,0.0126518524974542,
0.0253034806785961),.UNSPECIFIED.);
#22933=B_SPLINE_CURVE_WITH_KNOTS('',3,(#132437,#132438,#132439,#132440,
#132441,#132442),.UNSPECIFIED.,.F.,.F.,(4,2,4),(2.79900002971549E-11,0.0126518524054462,
0.0253034805046033),.UNSPECIFIED.);
#22934=B_SPLINE_CURVE_WITH_KNOTS('',3,(#132465,#132466,#132467,#132468,
#132469,#132470),.UNSPECIFIED.,.F.,.F.,(4,2,4),(1.61552872164343E-11,0.0126518523983396,
0.0253034805129489),.UNSPECIFIED.);
#22935=B_SPLINE_CURVE_WITH_KNOTS('',3,(#132493,#132494,#132495,#132496,
#132497,#132498),.UNSPECIFIED.,.F.,.F.,(4,2,4),(3.59283638053901E-11,0.0126518525083403,
0.0253034806945798),.UNSPECIFIED.);
#22936=B_SPLINE_CURVE_WITH_KNOTS('',3,(#132521,#132522,#132523,#132524,
#132525,#132526),.UNSPECIFIED.,.F.,.F.,(4,2,4),(3.19092675899861E-11,0.0126518524958068,
0.0253034806753266),.UNSPECIFIED.);
#22937=B_SPLINE_CURVE_WITH_KNOTS('',3,(#132549,#132550,#132551,#132552,
#132553,#132554),.UNSPECIFIED.,.F.,.F.,(4,2,4),(5.01111450311739E-11,0.0126518524534616,
0.0253034805513483),.UNSPECIFIED.);
#22938=B_SPLINE_CURVE_WITH_KNOTS('',3,(#132577,#132578,#132579,#132580,
#132581,#132582),.UNSPECIFIED.,.F.,.F.,(4,2,4),(3.86162407489939E-11,0.0126518525018019,
0.0253034806727814),.UNSPECIFIED.);
#22939=B_SPLINE_CURVE_WITH_KNOTS('',3,(#132605,#132606,#132607,#132608,
#132609,#132610),.UNSPECIFIED.,.F.,.F.,(4,2,4),(2.26099460019981E-11,0.0126518524785923,
0.0253034806615711),.UNSPECIFIED.);
#22940=B_SPLINE_CURVE_WITH_KNOTS('',3,(#132646,#132647,#132648,#132649,
#132650,#132651),.UNSPECIFIED.,.F.,.F.,(4,2,4),(0.,0.012650581650196,0.025301429662558),
 .UNSPECIFIED.);
#22941=B_SPLINE_CURVE_WITH_KNOTS('',3,(#132658,#132659,#132660,#132661,
#132662,#132663,#132664),.UNSPECIFIED.,.F.,.F.,(4,3,4),(0.492524364188282,
0.5,0.504719756176227),.UNSPECIFIED.);
#22942=B_SPLINE_CURVE_WITH_KNOTS('',3,(#132685,#132686,#132687,#132688,
#132689,#132690),.UNSPECIFIED.,.F.,.F.,(4,2,4),(0.,0.0126505787819665,0.0253014176959488),
 .UNSPECIFIED.);
#22943=B_SPLINE_CURVE_WITH_KNOTS('',3,(#132697,#132698,#132699,#132700,
#132701,#132702,#132703),.UNSPECIFIED.,.F.,.F.,(4,3,4),(0.492524364190509,
0.5,0.504719756176228),.UNSPECIFIED.);
#22944=B_SPLINE_CURVE_WITH_KNOTS('',3,(#132724,#132725,#132726,#132727,
#132728,#132729),.UNSPECIFIED.,.F.,.F.,(4,2,4),(0.,0.0126505799555268,0.0253014225909201),
 .UNSPECIFIED.);
#22945=B_SPLINE_CURVE_WITH_KNOTS('',3,(#132736,#132737,#132738,#132739,
#132740,#132741,#132742),.UNSPECIFIED.,.F.,.F.,(4,3,4),(0.492524364184477,
0.5,0.504719756176228),.UNSPECIFIED.);
#22946=B_SPLINE_CURVE_WITH_KNOTS('',3,(#132763,#132764,#132765,#132766,
#132767,#132768),.UNSPECIFIED.,.F.,.F.,(4,2,4),(0.,0.0126505812154814,0.0253014191594166),
 .UNSPECIFIED.);
#22947=B_SPLINE_CURVE_WITH_KNOTS('',3,(#132775,#132776,#132777,#132778,
#132779,#132780,#132781),.UNSPECIFIED.,.F.,.F.,(4,3,4),(0.492524364184568,
0.5,0.504719756176228),.UNSPECIFIED.);
#22948=B_SPLINE_CURVE_WITH_KNOTS('',3,(#132802,#132803,#132804,#132805,
#132806,#132807),.UNSPECIFIED.,.F.,.F.,(4,2,4),(0.,0.0126505803545275,0.025301424226586),
 .UNSPECIFIED.);
#22949=B_SPLINE_CURVE_WITH_KNOTS('',3,(#132814,#132815,#132816,#132817,
#132818,#132819,#132820),.UNSPECIFIED.,.F.,.F.,(4,3,4),(0.492524364187926,
0.5,0.504719756176228),.UNSPECIFIED.);
#22950=B_SPLINE_CURVE_WITH_KNOTS('',3,(#132841,#132842,#132843,#132844,
#132845,#132846),.UNSPECIFIED.,.F.,.F.,(4,2,4),(0.,0.0126505775499235,0.0253014126906162),
 .UNSPECIFIED.);
#22951=B_SPLINE_CURVE_WITH_KNOTS('',3,(#132853,#132854,#132855,#132856,
#132857,#132858,#132859),.UNSPECIFIED.,.F.,.F.,(4,3,4),(0.492524364187916,
0.5,0.504719756176227),.UNSPECIFIED.);
#22952=B_SPLINE_CURVE_WITH_KNOTS('',3,(#132880,#132881,#132882,#132883,
#132884,#132885),.UNSPECIFIED.,.F.,.F.,(4,2,4),(0.,0.0126505808589483,0.0253014264769213),
 .UNSPECIFIED.);
#22953=B_SPLINE_CURVE_WITH_KNOTS('',3,(#132892,#132893,#132894,#132895,
#132896,#132897,#132898),.UNSPECIFIED.,.F.,.F.,(4,3,4),(0.492524364186843,
0.5,0.504719756176228),.UNSPECIFIED.);
#22954=B_SPLINE_CURVE_WITH_KNOTS('',3,(#132919,#132920,#132921,#132922,
#132923,#132924),.UNSPECIFIED.,.F.,.F.,(4,2,4),(0.,0.0126505811248473,0.02530142745166),
 .UNSPECIFIED.);
#22955=B_SPLINE_CURVE_WITH_KNOTS('',3,(#132931,#132932,#132933,#132934,
#132935,#132936,#132937),.UNSPECIFIED.,.F.,.F.,(4,3,4),(0.492524364186291,
0.5,0.504719756176228),.UNSPECIFIED.);
#22956=B_SPLINE_CURVE_WITH_KNOTS('',3,(#132958,#132959,#132960,#132961,
#132962,#132963),.UNSPECIFIED.,.F.,.F.,(4,2,4),(0.,0.0126505818313986,0.0253014303880561),
 .UNSPECIFIED.);
#22957=B_SPLINE_CURVE_WITH_KNOTS('',3,(#132995,#132996,#132997,#132998,
#132999,#133000),.UNSPECIFIED.,.F.,.F.,(4,2,4),(0.,0.0126505798191397,0.0253014219508626),
 .UNSPECIFIED.);
#22958=B_SPLINE_CURVE_WITH_KNOTS('',3,(#133007,#133008,#133009,#133010,
#133011,#133012,#133013),.UNSPECIFIED.,.F.,.F.,(4,3,4),(0.492524364187932,
0.5,0.504719756176228),.UNSPECIFIED.);
#22959=B_SPLINE_CURVE_WITH_KNOTS('',3,(#133034,#133035,#133036,#133037,
#133038,#133039),.UNSPECIFIED.,.F.,.F.,(4,2,4),(0.,0.0126505777803537,0.0253014137319526),
 .UNSPECIFIED.);
#22960=B_SPLINE_CURVE_WITH_KNOTS('',3,(#133046,#133047,#133048,#133049,
#133050,#133051,#133052),.UNSPECIFIED.,.F.,.F.,(4,3,4),(0.492524364188889,
0.5,0.504719756176228),.UNSPECIFIED.);
#22961=B_SPLINE_CURVE_WITH_KNOTS('',3,(#133073,#133074,#133075,#133076,
#133077,#133078),.UNSPECIFIED.,.F.,.F.,(4,2,4),(0.,0.0126505789353812,0.0253014184523535),
 .UNSPECIFIED.);
#22962=B_SPLINE_CURVE_WITH_KNOTS('',3,(#133085,#133086,#133087,#133088,
#133089,#133090,#133091),.UNSPECIFIED.,.F.,.F.,(4,3,4),(0.492524364188364,
0.5,0.504719756176228),.UNSPECIFIED.);
#22963=B_SPLINE_CURVE_WITH_KNOTS('',3,(#133112,#133113,#133114,#133115,
#133116,#133117),.UNSPECIFIED.,.F.,.F.,(4,2,4),(0.,0.0126505814576675,0.0253014288471314),
 .UNSPECIFIED.);
#22964=B_SPLINE_CURVE_WITH_KNOTS('',3,(#133124,#133125,#133126,#133127,
#133128,#133129,#133130),.UNSPECIFIED.,.F.,.F.,(4,3,4),(0.49252436418111,
0.5,0.504719756176228),.UNSPECIFIED.);
#22965=B_SPLINE_CURVE_WITH_KNOTS('',3,(#133151,#133152,#133153,#133154,
#133155,#133156),.UNSPECIFIED.,.F.,.F.,(4,2,4),(0.,0.0126505805067179,0.0253014249386929),
 .UNSPECIFIED.);
#22966=B_SPLINE_CURVE_WITH_KNOTS('',3,(#133163,#133164,#133165,#133166,
#133167,#133168,#133169),.UNSPECIFIED.,.F.,.F.,(4,3,4),(0.49252436418881,
0.5,0.504719756176228),.UNSPECIFIED.);
#22967=B_SPLINE_CURVE_WITH_KNOTS('',3,(#133187,#133188,#133189,#133190,
#133191,#133192),.UNSPECIFIED.,.F.,.F.,(4,2,4),(0.,0.0126505788899671,0.0253014181768197),
 .UNSPECIFIED.);
#22968=B_SPLINE_CURVE_WITH_KNOTS('',3,(#133214,#133215,#133216,#133217,
#133218,#133219),.UNSPECIFIED.,.F.,.F.,(4,2,4),(0.,0.0126505816109507,0.0253014294816165),
 .UNSPECIFIED.);
#22969=B_SPLINE_CURVE_WITH_KNOTS('',3,(#133226,#133227,#133228,#133229,
#133230,#133231,#133232),.UNSPECIFIED.,.F.,.F.,(4,3,4),(0.492524364186993,
0.5,0.504719756176228),.UNSPECIFIED.);
#22970=B_SPLINE_CURVE_WITH_KNOTS('',3,(#133253,#133254,#133255,#133256,
#133257,#133258),.UNSPECIFIED.,.F.,.F.,(4,2,4),(0.,0.0126505803329357,0.0253014241800918),
 .UNSPECIFIED.);
#22971=B_SPLINE_CURVE_WITH_KNOTS('',3,(#133265,#133266,#133267,#133268,
#133269,#133270,#133271),.UNSPECIFIED.,.F.,.F.,(4,3,4),(0.49252436418892,
0.5,0.504719756176228),.UNSPECIFIED.);
#22972=B_SPLINE_CURVE_WITH_KNOTS('',3,(#133292,#133293,#133294,#133295,
#133296,#133297),.UNSPECIFIED.,.F.,.F.,(4,2,4),(0.,0.0126505772916147,0.025301411659512),
 .UNSPECIFIED.);
#22973=B_SPLINE_CURVE_WITH_KNOTS('',3,(#133304,#133305,#133306,#133307,
#133308,#133309,#133310),.UNSPECIFIED.,.F.,.F.,(4,3,4),(0.492524364186463,
0.5,0.504719756176228),.UNSPECIFIED.);
#22974=B_SPLINE_CURVE_WITH_KNOTS('',3,(#133331,#133332,#133333,#133334,
#133335,#133336),.UNSPECIFIED.,.F.,.F.,(4,2,4),(0.,0.0126505800967122,0.0253014231919566),
 .UNSPECIFIED.);
#22975=B_SPLINE_CURVE_WITH_KNOTS('',3,(#133343,#133344,#133345,#133346,
#133347,#133348,#133349),.UNSPECIFIED.,.F.,.F.,(4,3,4),(0.492524364189609,
0.5,0.504719756176228),.UNSPECIFIED.);
#22976=B_SPLINE_CURVE_WITH_KNOTS('',3,(#133370,#133371,#133372,#133373,
#133374,#133375),.UNSPECIFIED.,.F.,.F.,(4,2,4),(0.,0.0126505783151481,0.0253014157848534),
 .UNSPECIFIED.);
#22977=B_SPLINE_CURVE_WITH_KNOTS('',3,(#133382,#133383,#133384,#133385,
#133386,#133387,#133388),.UNSPECIFIED.,.F.,.F.,(4,3,4),(0.492524364184887,
0.5,0.504719756176228),.UNSPECIFIED.);
#22978=B_SPLINE_CURVE_WITH_KNOTS('',3,(#133409,#133410,#133411,#133412,
#133413,#133414),.UNSPECIFIED.,.F.,.F.,(4,2,4),(0.,0.0126505813529116,0.0253014285382464),
 .UNSPECIFIED.);
#22979=B_SPLINE_CURVE_WITH_KNOTS('',3,(#133427,#133428,#133429,#133430,
#133431,#133432,#133433),.UNSPECIFIED.,.F.,.F.,(4,3,4),(0.492524364,0.5,
0.504719756176228),.UNSPECIFIED.);
#22980=B_SPLINE_CURVE_WITH_KNOTS('',3,(#133449,#133450,#133451,#133452,
#133453,#133454),.UNSPECIFIED.,.F.,.F.,(4,2,4),(0.,0.0126505813382396,0.0253014283032559),
 .UNSPECIFIED.);
#22981=B_SPLINE_CURVE_WITH_KNOTS('',3,(#133457,#133458,#133459,#133460,
#133461,#133462,#133463),.UNSPECIFIED.,.F.,.F.,(4,3,4),(0.492524364188681,
0.5,0.504719756194363),.UNSPECIFIED.);
#22982=B_SPLINE_CURVE_WITH_KNOTS('',3,(#133487,#133488,#133489,#133490,
#133491,#133492),.UNSPECIFIED.,.F.,.F.,(4,2,4),(0.,0.0126505807185899,0.0253014258572568),
 .UNSPECIFIED.);
#22983=B_SPLINE_CURVE_WITH_KNOTS('',3,(#133499,#133500,#133501,#133502,
#133503,#133504,#133505),.UNSPECIFIED.,.F.,.F.,(4,3,4),(0.492524364187148,
0.5,0.504719756176227),.UNSPECIFIED.);
#22984=B_SPLINE_CURVE_WITH_KNOTS('',3,(#133526,#133527,#133528,#133529,
#133530,#133531),.UNSPECIFIED.,.F.,.F.,(4,2,4),(0.,0.01265057904704,0.0253014188722932),
 .UNSPECIFIED.);
#22985=B_SPLINE_CURVE_WITH_KNOTS('',3,(#133538,#133539,#133540,#133541,
#133542,#133543,#133544),.UNSPECIFIED.,.F.,.F.,(4,3,4),(0.492524364186767,
0.5,0.504719756176227),.UNSPECIFIED.);
#22986=B_SPLINE_CURVE_WITH_KNOTS('',3,(#133565,#133566,#133567,#133568,
#133569,#133570),.UNSPECIFIED.,.F.,.F.,(4,2,4),(0.,0.0126505798077898,0.0253014219006744),
 .UNSPECIFIED.);
#22987=B_SPLINE_CURVE_WITH_KNOTS('',3,(#133577,#133578,#133579,#133580,
#133581,#133582,#133583),.UNSPECIFIED.,.F.,.F.,(4,3,4),(0.492524364193697,
0.5,0.504719756176227),.UNSPECIFIED.);
#22988=B_SPLINE_CURVE_WITH_KNOTS('',3,(#133604,#133605,#133606,#133607,
#133608,#133609),.UNSPECIFIED.,.F.,.F.,(4,2,4),(0.,0.0126505808801605,0.0253014264674703),
 .UNSPECIFIED.);
#22989=B_SPLINE_CURVE_WITH_KNOTS('',3,(#133616,#133617,#133618,#133619,
#133620,#133621,#133622),.UNSPECIFIED.,.F.,.F.,(4,3,4),(0.492524364182756,
0.5,0.504719756176227),.UNSPECIFIED.);
#22990=B_SPLINE_CURVE_WITH_KNOTS('',3,(#133643,#133644,#133645,#133646,
#133647,#133648),.UNSPECIFIED.,.F.,.F.,(4,2,4),(0.,0.0126505779800128,0.0253014145110505),
 .UNSPECIFIED.);
#22991=B_SPLINE_CURVE_WITH_KNOTS('',3,(#133655,#133656,#133657,#133658,
#133659,#133660,#133661),.UNSPECIFIED.,.F.,.F.,(4,3,4),(0.49252436419132,
0.5,0.504719756176227),.UNSPECIFIED.);
#22992=B_SPLINE_CURVE_WITH_KNOTS('',3,(#133682,#133683,#133684,#133685,
#133686,#133687),.UNSPECIFIED.,.F.,.F.,(4,2,4),(0.,0.0126505794608813,0.0253014205743486),
 .UNSPECIFIED.);
#22993=B_SPLINE_CURVE_WITH_KNOTS('',3,(#133694,#133695,#133696,#133697,
#133698,#133699,#133700),.UNSPECIFIED.,.F.,.F.,(4,3,4),(0.492524364189435,
0.5,0.504719756176226),.UNSPECIFIED.);
#22994=B_SPLINE_CURVE_WITH_KNOTS('',3,(#133721,#133722,#133723,#133724,
#133725,#133726),.UNSPECIFIED.,.F.,.F.,(4,2,4),(0.,0.0126505804869144,0.0253014248256905),
 .UNSPECIFIED.);
#22995=B_SPLINE_CURVE_WITH_KNOTS('',3,(#133733,#133734,#133735,#133736,
#133737,#133738,#133739),.UNSPECIFIED.,.F.,.F.,(4,3,4),(0.492524364190348,
0.5,0.504719756176226),.UNSPECIFIED.);
#22996=B_SPLINE_CURVE_WITH_KNOTS('',3,(#133761,#133762,#133763,#133764,
#133765,#133766),.UNSPECIFIED.,.F.,.F.,(4,2,4),(-0.025304064498856,-0.0126521398388827,
-4.2125573862517E-11),.UNSPECIFIED.);
#22997=B_SPLINE_CURVE_WITH_KNOTS('',3,(#133790,#133791,#133792,#133793,
#133794,#133795),.UNSPECIFIED.,.F.,.F.,(4,2,4),(-0.0253040630374336,-0.0126521397986007,
-4.20119217192649E-11),.UNSPECIFIED.);
#22998=B_SPLINE_CURVE_WITH_KNOTS('',3,(#133819,#133820,#133821,#133822,
#133823,#133824),.UNSPECIFIED.,.F.,.F.,(4,2,4),(-0.0253040694676751,-0.0126521398389519,
-4.19704826448708E-11),.UNSPECIFIED.);
#22999=B_SPLINE_CURVE_WITH_KNOTS('',3,(#133848,#133849,#133850,#133851,
#133852,#133853),.UNSPECIFIED.,.F.,.F.,(4,2,4),(-0.0253040643721042,-0.0126521398535919,
-4.26806090469967E-11),.UNSPECIFIED.);
#23000=B_SPLINE_CURVE_WITH_KNOTS('',3,(#133877,#133878,#133879,#133880,
#133881,#133882),.UNSPECIFIED.,.F.,.F.,(4,2,4),(-0.0253040634165168,-0.0126521398236705,
-4.2208906508856E-11),.UNSPECIFIED.);
#23001=B_SPLINE_CURVE_WITH_KNOTS('',3,(#133906,#133907,#133908,#133909,
#133910,#133911),.UNSPECIFIED.,.F.,.F.,(4,2,4),(-0.0253040638021277,-0.0126521398274489,
-4.2573208847152E-11),.UNSPECIFIED.);
#23002=B_SPLINE_CURVE_WITH_KNOTS('',3,(#133935,#133936,#133937,#133938,
#133939,#133940),.UNSPECIFIED.,.F.,.F.,(4,2,4),(-0.0253040643923574,-0.0126521398266015,
-4.24393506448517E-11),.UNSPECIFIED.);
#23003=B_SPLINE_CURVE_WITH_KNOTS('',3,(#133964,#133965,#133966,#133967,
#133968,#133969),.UNSPECIFIED.,.F.,.F.,(4,2,4),(-0.0253040634154255,-0.0126521398084239,
-4.14864566311568E-11),.UNSPECIFIED.);
#23004=B_SPLINE_CURVE_WITH_KNOTS('',3,(#133993,#133994,#133995,#133996,
#133997,#133998),.UNSPECIFIED.,.F.,.F.,(4,2,4),(-0.0253040606038705,-0.0126521398219097,
-4.27034241301527E-11),.UNSPECIFIED.);
#23005=B_SPLINE_CURVE_WITH_KNOTS('',3,(#134022,#134023,#134024,#134025,
#134026,#134027),.UNSPECIFIED.,.F.,.F.,(4,2,4),(-0.0253040613299487,-0.0126521397910629,
-4.1742501816211E-11),.UNSPECIFIED.);
#23006=B_SPLINE_CURVE_WITH_KNOTS('',3,(#134051,#134052,#134053,#134054,
#134055,#134056),.UNSPECIFIED.,.F.,.F.,(4,2,4),(-0.025304066853621,-0.0126521398258534,
-4.13601410065301E-11),.UNSPECIFIED.);
#23007=B_SPLINE_CURVE_WITH_KNOTS('',3,(#134080,#134081,#134082,#134083,
#134084,#134085),.UNSPECIFIED.,.F.,.F.,(4,2,4),(-0.0253040666533286,-0.0126521398324811,
-4.16749482146095E-11),.UNSPECIFIED.);
#23008=B_SPLINE_CURVE_WITH_KNOTS('',3,(#134109,#134110,#134111,#134112,
#134113,#134114),.UNSPECIFIED.,.F.,.F.,(4,2,4),(-0.0253040634792013,-0.0126521398329723,
-4.27786313317302E-11),.UNSPECIFIED.);
#23009=B_SPLINE_CURVE_WITH_KNOTS('',3,(#134138,#134139,#134140,#134141,
#134142,#134143),.UNSPECIFIED.,.F.,.F.,(4,2,4),(-0.0253040635443814,-0.012652139804696,
-4.21150510299118E-11),.UNSPECIFIED.);
#23010=B_SPLINE_CURVE_WITH_KNOTS('',3,(#134167,#134168,#134169,#134170,
#134171,#134172),.UNSPECIFIED.,.F.,.F.,(4,2,4),(-0.0253040652094674,-0.0126521398118821,
-4.18545927083347E-11),.UNSPECIFIED.);
#23011=B_SPLINE_CURVE_WITH_KNOTS('',3,(#134196,#134197,#134198,#134199,
#134200,#134201),.UNSPECIFIED.,.F.,.F.,(4,2,4),(-0.0253040622867192,-0.0126521398070244,
-4.19272325191677E-11),.UNSPECIFIED.);
#23012=B_SPLINE_CURVE_WITH_KNOTS('',3,(#134225,#134226,#134227,#134228,
#134229,#134230),.UNSPECIFIED.,.F.,.F.,(4,2,4),(-0.0253040666146288,-0.0126521398295065,
-4.18443925342959E-11),.UNSPECIFIED.);
#23013=B_SPLINE_CURVE_WITH_KNOTS('',3,(#134254,#134255,#134256,#134257,
#134258,#134259),.UNSPECIFIED.,.F.,.F.,(4,2,4),(-0.02530406558539,-0.0126521398311914,
-4.21956844465221E-11),.UNSPECIFIED.);
#23014=B_SPLINE_CURVE_WITH_KNOTS('',3,(#134283,#134284,#134285,#134286,
#134287,#134288),.UNSPECIFIED.,.F.,.F.,(4,2,4),(-0.0253040616874405,-0.0126521398383703,
-4.3402618304933E-11),.UNSPECIFIED.);
#23015=B_SPLINE_CURVE_WITH_KNOTS('',3,(#134312,#134313,#134314,#134315,
#134316,#134317),.UNSPECIFIED.,.F.,.F.,(4,2,4),(-0.0253040610757602,-0.0126521398054598,
-4.21142877515823E-11),.UNSPECIFIED.);
#23016=B_SPLINE_CURVE_WITH_KNOTS('',3,(#134341,#134342,#134343,#134344,
#134345,#134346),.UNSPECIFIED.,.F.,.F.,(4,2,4),(-0.0253040624336241,-0.0126521398363262,
-4.2850282350182E-11),.UNSPECIFIED.);
#23017=B_SPLINE_CURVE_WITH_KNOTS('',3,(#134370,#134371,#134372,#134373,
#134374,#134375),.UNSPECIFIED.,.F.,.F.,(4,2,4),(-0.0253040617305736,-0.0126521398066379,
-4.31877381079637E-11),.UNSPECIFIED.);
#23018=B_SPLINE_CURVE_WITH_KNOTS('',3,(#134399,#134400,#134401,#134402,
#134403,#134404),.UNSPECIFIED.,.F.,.F.,(4,2,4),(-0.025304059734234,-0.0126521397823564,
-4.21624471447224E-11),.UNSPECIFIED.);
#23019=B_SPLINE_CURVE_WITH_KNOTS('',3,(#134428,#134429,#134430,#134431,
#134432,#134433),.UNSPECIFIED.,.F.,.F.,(4,2,4),(-0.0253040664569554,-0.0126521398563623,
-4.28707382094107E-11),.UNSPECIFIED.);
#23020=B_SPLINE_CURVE_WITH_KNOTS('',3,(#134457,#134458,#134459,#134460,
#134461,#134462),.UNSPECIFIED.,.F.,.F.,(4,2,4),(-0.025304062021989,-0.0126521398169023,
-4.14917475377585E-11),.UNSPECIFIED.);
#23021=B_SPLINE_CURVE_WITH_KNOTS('',3,(#134486,#134487,#134488,#134489,
#134490,#134491),.UNSPECIFIED.,.F.,.F.,(4,2,4),(-0.0253040667762494,-0.0126521398634984,
-4.26520728458168E-11),.UNSPECIFIED.);
#23022=B_SPLINE_CURVE_WITH_KNOTS('',3,(#134515,#134516,#134517,#134518,
#134519,#134520),.UNSPECIFIED.,.F.,.F.,(4,2,4),(-0.025304062706261,-0.0126521398103911,
-4.19324540368304E-11),.UNSPECIFIED.);
#23023=B_SPLINE_CURVE_WITH_KNOTS('',3,(#134544,#134545,#134546,#134547,
#134548,#134549),.UNSPECIFIED.,.F.,.F.,(4,2,4),(-0.0253040678335757,-0.0126521398507726,
-4.24169657731177E-11),.UNSPECIFIED.);
#23024=B_SPLINE_CURVE_WITH_KNOTS('',3,(#134573,#134574,#134575,#134576,
#134577,#134578),.UNSPECIFIED.,.F.,.F.,(4,2,4),(-0.0253040639899681,-0.0126521397979972,
-4.20035950465802E-11),.UNSPECIFIED.);
#23025=B_SPLINE_CURVE_WITH_KNOTS('',3,(#134604,#134605,#134606,#134607,
#134608,#134609,#134610,#134611,#134612,#134613),.UNSPECIFIED.,.F.,.F.,
(4,3,3,4),(4.14193967595349E-14,8.70530734855011E-5,0.000170036649813278,
0.000253022525483205),.UNSPECIFIED.);
#23026=B_SPLINE_CURVE_WITH_KNOTS('',3,(#134628,#134629,#134630,#134631,
#134632,#134633,#134634,#134635,#134636,#134637),.UNSPECIFIED.,.F.,.F.,
(4,3,3,4),(0.211606869610061,0.221412979786492,0.226204530183524,0.228987659497871),
 .UNSPECIFIED.);
#23027=B_SPLINE_CURVE_WITH_KNOTS('',3,(#134650,#134651,#134652,#134653,
#134654,#134655,#134656,#134657,#134658,#134659),.UNSPECIFIED.,.F.,.F.,
(4,3,3,4),(8.73864678274336E-14,8.70530734589771E-5,0.000170036649623857,
0.000253022525131198),.UNSPECIFIED.);
#23028=B_SPLINE_CURVE_WITH_KNOTS('',3,(#134674,#134675,#134676,#134677,
#134678,#134679,#134680,#134681,#134682,#134683),.UNSPECIFIED.,.F.,.F.,
(4,3,3,4),(0.211606869614525,0.221412980312189,0.226204530183508,0.228987659512711),
 .UNSPECIFIED.);
#23029=B_SPLINE_CURVE_WITH_KNOTS('',3,(#134696,#134697,#134698,#134699,
#134700,#134701,#134702,#134703,#134704,#134705),.UNSPECIFIED.,.F.,.F.,
(4,3,3,4),(8.03981756062997E-15,8.70530736309221E-5,0.000170036649877014,
0.000253022525465094),.UNSPECIFIED.);
#23030=B_SPLINE_CURVE_WITH_KNOTS('',3,(#134720,#134721,#134722,#134723,
#134724,#134725,#134726,#134727,#134728,#134729),.UNSPECIFIED.,.F.,.F.,
(4,3,3,4),(0.211606869609531,0.221412979024587,0.2262045301835,0.228987659519257),
 .UNSPECIFIED.);
#23031=B_SPLINE_CURVE_WITH_KNOTS('',3,(#134742,#134743,#134744,#134745,
#134746,#134747,#134748,#134749,#134750,#134751),.UNSPECIFIED.,.F.,.F.,
(4,3,3,4),(7.79800256787147E-14,8.70530734703506E-5,0.000170036649594596,
0.000253022525060469),.UNSPECIFIED.);
#23032=B_SPLINE_CURVE_WITH_KNOTS('',3,(#134766,#134767,#134768,#134769,
#134770,#134771,#134772,#134773,#134774,#134775),.UNSPECIFIED.,.F.,.F.,
(4,3,3,4),(0.211606869610436,0.221412979506795,0.226204530183523,0.228987659511922),
 .UNSPECIFIED.);
#23033=B_SPLINE_CURVE_WITH_KNOTS('',3,(#134788,#134789,#134790,#134791,
#134792,#134793,#134794,#134795,#134796,#134797),.UNSPECIFIED.,.F.,.F.,
(4,3,3,4),(5.37189951081576E-14,8.70530735283743E-5,0.000170036649708885,
0.000253022525231511),.UNSPECIFIED.);
#23034=B_SPLINE_CURVE_WITH_KNOTS('',3,(#134812,#134813,#134814,#134815,
#134816,#134817,#134818,#134819,#134820,#134821),.UNSPECIFIED.,.F.,.F.,
(4,3,3,4),(0.211606869618575,0.221412979552959,0.226204530183407,0.228987659520732),
 .UNSPECIFIED.);
#23035=B_SPLINE_CURVE_WITH_KNOTS('',3,(#134834,#134835,#134836,#134837,
#134838,#134839,#134840,#134841,#134842,#134843),.UNSPECIFIED.,.F.,.F.,
(4,3,3,4),(1.31873644434942E-13,8.7053073591002E-5,0.000170036649834339,
0.000253022525419973),.UNSPECIFIED.);
#23036=B_SPLINE_CURVE_WITH_KNOTS('',3,(#134858,#134859,#134860,#134861,
#134862,#134863,#134864,#134865,#134866,#134867,#134868,#134869,#134870,
#134871),.UNSPECIFIED.,.F.,.F.,(4,2,2,2,2,2,4),(9.99263316600448E-7,0.00392100953657802,
0.00802861323508025,0.0162407021656379,0.0326517370626527,0.0654159013494179,
0.13074836471509),.UNSPECIFIED.);
#23037=B_SPLINE_CURVE_WITH_KNOTS('',3,(#134884,#134885,#134886,#134887,
#134888,#134889,#134890,#134891,#134892,#134893),.UNSPECIFIED.,.F.,.F.,
(4,3,3,4),(7.89927548210784E-14,8.70530731075762E-5,0.000170036648965722,
0.0002530225241661),.UNSPECIFIED.);
#23038=B_SPLINE_CURVE_WITH_KNOTS('',3,(#134908,#134909,#134910,#134911,
#134912,#134913,#134914,#134915,#134916,#134917),.UNSPECIFIED.,.F.,.F.,
(4,3,3,4),(0.211606869614502,0.221412981431605,0.226204530183495,0.228987659498062),
 .UNSPECIFIED.);
#23039=B_SPLINE_CURVE_WITH_KNOTS('',3,(#134930,#134931,#134932,#134933,
#134934,#134935,#134936,#134937,#134938,#134939),.UNSPECIFIED.,.F.,.F.,
(4,3,3,4),(2.52334893766153E-14,8.70530732793856E-5,0.000170036649550745,
0.000253022525164497),.UNSPECIFIED.);
#23040=B_SPLINE_CURVE_WITH_KNOTS('',3,(#134954,#134955,#134956,#134957,
#134958,#134959,#134960,#134961,#134962,#134963),.UNSPECIFIED.,.F.,.F.,
(4,3,3,4),(0.211606869621102,0.221412977824722,0.226204530183524,0.228987659510322),
 .UNSPECIFIED.);
#23041=B_SPLINE_CURVE_WITH_KNOTS('',3,(#134976,#134977,#134978,#134979,
#134980,#134981,#134982,#134983,#134984,#134985),.UNSPECIFIED.,.F.,.F.,
(4,3,3,4),(7.50943469913966E-14,8.70530731548489E-5,0.00017003664908509,
0.000253022524357588),.UNSPECIFIED.);
#23042=B_SPLINE_CURVE_WITH_KNOTS('',3,(#135000,#135001,#135002,#135003,
#135004,#135005,#135006,#135007,#135008,#135009),.UNSPECIFIED.,.F.,.F.,
(4,3,3,4),(0.211606870032462,0.22141297801983,0.226204530183524,0.228987659635174),
 .UNSPECIFIED.);
#23043=B_SPLINE_CURVE_WITH_KNOTS('',3,(#135022,#135023,#135024,#135025,
#135026,#135027,#135028,#135029,#135030,#135031),.UNSPECIFIED.,.F.,.F.,
(4,3,3,4),(9.02311911813612E-14,8.70530732466921E-5,0.000170036649065836,
0.000253022524226805),.UNSPECIFIED.);
#23044=B_SPLINE_CURVE_WITH_KNOTS('',3,(#135046,#135047,#135048,#135049,
#135050,#135051,#135052,#135053,#135054,#135055),.UNSPECIFIED.,.F.,.F.,
(4,3,3,4),(0.211606869604561,0.221412978253218,0.22620453018352,0.228987659509309),
 .UNSPECIFIED.);
#23045=B_SPLINE_CURVE_WITH_KNOTS('',3,(#135068,#135069,#135070,#135071,
#135072,#135073,#135074,#135075,#135076,#135077),.UNSPECIFIED.,.F.,.F.,
(4,3,3,4),(1.07741326354794E-13,8.70530734410574E-5,0.000170036649714572,
0.000253022525330184),.UNSPECIFIED.);
#23046=B_SPLINE_CURVE_WITH_KNOTS('',3,(#135092,#135093,#135094,#135095,
#135096,#135097,#135098,#135099,#135100,#135101),.UNSPECIFIED.,.F.,.F.,
(4,3,3,4),(0.211606869612044,0.221412977691357,0.226204530183524,0.228987659517864),
 .UNSPECIFIED.);
#23047=B_SPLINE_CURVE_WITH_KNOTS('',3,(#135114,#135115,#135116,#135117,
#135118,#135119,#135120,#135121,#135122,#135123),.UNSPECIFIED.,.F.,.F.,
(4,3,3,4),(1.09031513920967E-13,8.70530732165772E-5,0.000170036649139832,
0.000253022524405007),.UNSPECIFIED.);
#23048=B_SPLINE_CURVE_WITH_KNOTS('',3,(#135138,#135139,#135140,#135141,
#135142,#135143,#135144,#135145,#135146,#135147),.UNSPECIFIED.,.F.,.F.,
(4,3,3,4),(0.211606870045396,0.221412978124601,0.226204530183484,0.228987659635174),
 .UNSPECIFIED.);
#23049=B_SPLINE_CURVE_WITH_KNOTS('',3,(#135160,#135161,#135162,#135163,
#135164,#135165,#135166,#135167,#135168,#135169),.UNSPECIFIED.,.F.,.F.,
(4,3,3,4),(6.03891784362884E-14,8.70530729984545E-5,0.000170036648893098,
0.00025302252412988),.UNSPECIFIED.);
#23050=B_SPLINE_CURVE_WITH_KNOTS('',3,(#135184,#135185,#135186,#135187,
#135188,#135189,#135190,#135191,#135192,#135193,#135194,#135195,#135196,
#135197),.UNSPECIFIED.,.F.,.F.,(4,2,2,2,2,2,4),(9.99274182381302E-7,0.00392100953236448,
0.00802861321169121,0.0162407021070139,0.0326517369455817,0.0654158886697625,
0.130748337459387),.UNSPECIFIED.);
#23051=B_SPLINE_CURVE_WITH_KNOTS('',3,(#135210,#135211,#135212,#135213,
#135214,#135215,#135216,#135217,#135218,#135219),.UNSPECIFIED.,.F.,.F.,
(4,3,3,4),(3.67379430042663E-14,8.70530734914654E-5,0.000170036649570622,
0.000253022524992313),.UNSPECIFIED.);
#23052=B_SPLINE_CURVE_WITH_KNOTS('',3,(#135234,#135235,#135236,#135237,
#135238,#135239,#135240,#135241,#135242,#135243,#135244,#135245,#135246,
#135247),.UNSPECIFIED.,.F.,.F.,(4,2,2,2,2,2,4),(9.99256961840177E-7,0.00392100965143877,
0.00802861351822096,0.0162407027811937,0.0326517383265419,0.0654159021312143,
0.130748376681168),.UNSPECIFIED.);
#23053=B_SPLINE_CURVE_WITH_KNOTS('',3,(#135260,#135261,#135262,#135263,
#135264,#135265,#135266,#135267,#135268,#135269),.UNSPECIFIED.,.F.,.F.,
(4,3,3,4),(1.57387654128723E-13,8.70530729486441E-5,0.000170036648862656,
0.000253022524119109),.UNSPECIFIED.);
#23054=B_SPLINE_CURVE_WITH_KNOTS('',3,(#135284,#135285,#135286,#135287,
#135288,#135289,#135290,#135291,#135292,#135293,#135294,#135295,#135296,
#135297),.UNSPECIFIED.,.F.,.F.,(4,2,2,2,2,2,4),(9.99262507793807E-7,0.00392100954195238,
0.00802861324845085,0.016240702191923,0.0326517371002704,0.0654158952120646,
0.130748362235185),.UNSPECIFIED.);
#23055=B_SPLINE_CURVE_WITH_KNOTS('',3,(#135310,#135311,#135312,#135313,
#135314,#135315,#135316,#135317,#135318,#135319),.UNSPECIFIED.,.F.,.F.,
(4,3,3,4),(1.22918305753956E-13,8.70530733818197E-5,0.000170036649366911,
0.000253022524693734),.UNSPECIFIED.);
#23056=B_SPLINE_CURVE_WITH_KNOTS('',3,(#135334,#135335,#135336,#135337,
#135338,#135339,#135340,#135341,#135342,#135343),.UNSPECIFIED.,.F.,.F.,
(4,3,3,4),(0.211606869609805,0.221412978520094,0.226204530183364,0.228987659522938),
 .UNSPECIFIED.);
#23057=B_SPLINE_CURVE_WITH_KNOTS('',3,(#135356,#135357,#135358,#135359,
#135360,#135361,#135362,#135363,#135364,#135365),.UNSPECIFIED.,.F.,.F.,
(4,3,3,4),(9.87657324158844E-14,8.70530733720858E-5,0.000170036649521387,
0.000253022525013159),.UNSPECIFIED.);
#23058=B_SPLINE_CURVE_WITH_KNOTS('',3,(#135380,#135381,#135382,#135383,
#135384,#135385,#135386,#135387,#135388,#135389),.UNSPECIFIED.,.F.,.F.,
(4,3,3,4),(0.211606870036805,0.221412975969717,0.226204530183423,0.228987659635174),
 .UNSPECIFIED.);
#23059=B_SPLINE_CURVE_WITH_KNOTS('',3,(#135402,#135403,#135404,#135405,
#135406,#135407,#135408,#135409,#135410,#135411),.UNSPECIFIED.,.F.,.F.,
(4,3,3,4),(6.10802431102158E-14,8.7053073275896E-5,0.000170036649311064,
0.00025302252468842),.UNSPECIFIED.);
#23060=B_SPLINE_CURVE_WITH_KNOTS('',3,(#135426,#135427,#135428,#135429,
#135430,#135431,#135432,#135433,#135434,#135435),.UNSPECIFIED.,.F.,.F.,
(4,3,3,4),(0.211606869622254,0.221412979041746,0.226204530183396,0.22898765948021),
 .UNSPECIFIED.);
#23061=B_SPLINE_CURVE_WITH_KNOTS('',3,(#135448,#135449,#135450,#135451,
#135452,#135453,#135454,#135455,#135456,#135457),.UNSPECIFIED.,.F.,.F.,
(4,3,3,4),(1.03129267188451E-13,8.7053073632608E-5,0.00017003664957889,
0.000253022524867124),.UNSPECIFIED.);
#23062=B_SPLINE_CURVE_WITH_KNOTS('',3,(#135472,#135473,#135474,#135475,
#135476,#135477,#135478,#135479,#135480,#135481),.UNSPECIFIED.,.F.,.F.,
(4,3,3,4),(0.211606869619466,0.221412978868105,0.226204530183133,0.228987659519068),
 .UNSPECIFIED.);
#23063=B_SPLINE_CURVE_WITH_KNOTS('',3,(#135494,#135495,#135496,#135497,
#135498,#135499,#135500,#135501,#135502,#135503),.UNSPECIFIED.,.F.,.F.,
(4,3,3,4),(2.08121007347066E-14,8.7053073146988E-5,0.000170036648983739,
0.000253022524162919),.UNSPECIFIED.);
#23064=B_SPLINE_CURVE_WITH_KNOTS('',3,(#135518,#135519,#135520,#135521,
#135522,#135523,#135524,#135525,#135526,#135527),.UNSPECIFIED.,.F.,.F.,
(4,3,3,4),(0.211606870038675,0.221412976851843,0.226204530183384,0.228987659635175),
 .UNSPECIFIED.);
#23065=B_SPLINE_CURVE_WITH_KNOTS('',3,(#135540,#135541,#135542,#135543,
#135544,#135545,#135546,#135547,#135548,#135549),.UNSPECIFIED.,.F.,.F.,
(4,3,3,4),(5.5757338411683E-14,8.70530736151624E-5,0.00017003664991911,
0.000253022525565324),.UNSPECIFIED.);
#23066=B_SPLINE_CURVE_WITH_KNOTS('',3,(#135564,#135565,#135566,#135567,
#135568,#135569,#135570,#135571,#135572,#135573),.UNSPECIFIED.,.F.,.F.,
(4,3,3,4),(0.211606869613814,0.221412976950775,0.22620453018352,0.228987659505786),
 .UNSPECIFIED.);
#23067=B_SPLINE_CURVE_WITH_KNOTS('',3,(#135586,#135587,#135588,#135589,
#135590,#135591,#135592,#135593,#135594,#135595),.UNSPECIFIED.,.F.,.F.,
(4,3,3,4),(6.46825384166277E-14,8.7053073213682E-5,0.000170036649169692,
0.000253022524468235),.UNSPECIFIED.);
#23068=B_SPLINE_CURVE_WITH_KNOTS('',3,(#135610,#135611,#135612,#135613,
#135614,#135615,#135616,#135617,#135618,#135619),.UNSPECIFIED.,.F.,.F.,
(4,3,3,4),(0.211606869605571,0.221412978487561,0.226204530183522,0.228987659505563),
 .UNSPECIFIED.);
#23069=B_SPLINE_CURVE_WITH_KNOTS('',3,(#135632,#135633,#135634,#135635,
#135636,#135637,#135638,#135639,#135640,#135641),.UNSPECIFIED.,.F.,.F.,
(4,3,3,4),(1.25934867797587E-13,8.70530732380585E-5,0.00017003664904369,
0.000253022524191407),.UNSPECIFIED.);
#23070=B_SPLINE_CURVE_WITH_KNOTS('',3,(#135656,#135657,#135658,#135659,
#135660,#135661,#135662,#135663,#135664,#135665),.UNSPECIFIED.,.F.,.F.,
(4,3,3,4),(0.211606870056587,0.221412979815329,0.226204530183526,0.228987659635175),
 .UNSPECIFIED.);
#23071=B_SPLINE_CURVE_WITH_KNOTS('',3,(#135678,#135679,#135680,#135681,
#135682,#135683,#135684,#135685,#135686,#135687),.UNSPECIFIED.,.F.,.F.,
(4,3,3,4),(8.80606518148291E-15,8.70530734448549E-5,0.000170036649791158,
0.000253022525475898),.UNSPECIFIED.);
#23072=B_SPLINE_CURVE_WITH_KNOTS('',3,(#135702,#135703,#135704,#135705,
#135706,#135707,#135708,#135709,#135710,#135711),.UNSPECIFIED.,.F.,.F.,
(4,3,3,4),(0.211606869615,0.221412981214008,0.226204530183526,0.228987659511592),
 .UNSPECIFIED.);
#23073=B_SPLINE_CURVE_WITH_KNOTS('',3,(#135724,#135725,#135726,#135727,
#135728,#135729,#135730,#135731,#135732,#135733),.UNSPECIFIED.,.F.,.F.,
(4,3,3,4),(1.01634978089741E-13,8.70530731190007E-5,0.000170036648882755,
0.000253022523989102),.UNSPECIFIED.);
#23074=B_SPLINE_CURVE_WITH_KNOTS('',3,(#135748,#135749,#135750,#135751,
#135752,#135753,#135754,#135755,#135756,#135757),.UNSPECIFIED.,.F.,.F.,
(4,3,3,4),(0.21160686962461,0.221412977210515,0.226204530183525,0.228987659495652),
 .UNSPECIFIED.);
#23075=B_SPLINE_CURVE_WITH_KNOTS('',3,(#135770,#135771,#135772,#135773,
#135774,#135775,#135776,#135777,#135778,#135779),.UNSPECIFIED.,.F.,.F.,
(4,3,3,4),(8.51741288654366E-14,8.70530733732294E-5,0.000170036649691492,
0.000253022525351441),.UNSPECIFIED.);
#23076=B_SPLINE_CURVE_WITH_KNOTS('',3,(#135794,#135795,#135796,#135797,
#135798,#135799,#135800,#135801,#135802,#135803),.UNSPECIFIED.,.F.,.F.,
(4,3,3,4),(0.211606870017552,0.221412978920659,0.226204530183525,0.228987659635174),
 .UNSPECIFIED.);
#23077=B_SPLINE_CURVE_WITH_KNOTS('',3,(#135816,#135817,#135818,#135819,
#135820,#135821,#135822,#135823,#135824,#135825),.UNSPECIFIED.,.F.,.F.,
(4,3,3,4),(9.67597096038106E-14,8.70530734827708E-5,0.000170036649712742,
0.000253022525284123),.UNSPECIFIED.);
#23078=B_SPLINE_CURVE_WITH_KNOTS('',3,(#135840,#135841,#135842,#135843,
#135844,#135845,#135846,#135847,#135848,#135849),.UNSPECIFIED.,.F.,.F.,
(4,3,3,4),(0.211606869611342,0.221412977795872,0.226204530183296,0.228987659507632),
 .UNSPECIFIED.);
#23079=B_SPLINE_CURVE_WITH_KNOTS('',3,(#135862,#135863,#135864,#135865,
#135866,#135867,#135868,#135869,#135870,#135871),.UNSPECIFIED.,.F.,.F.,
(4,3,3,4),(9.87701739216603E-14,8.70530730923315E-5,0.000170036649017183,
0.000253022524284285),.UNSPECIFIED.);
#23080=B_SPLINE_CURVE_WITH_KNOTS('',3,(#135886,#135887,#135888,#135889,
#135890,#135891,#135892,#135893,#135894,#135895),.UNSPECIFIED.,.F.,.F.,
(4,3,3,4),(0.211606869614618,0.221412977874128,0.226204530183525,0.228987659495887),
 .UNSPECIFIED.);
#23081=B_SPLINE_CURVE_WITH_KNOTS('',3,(#135908,#135909,#135910,#135911,
#135912,#135913,#135914,#135915,#135916,#135917),.UNSPECIFIED.,.F.,.F.,
(4,3,3,4),(1.02970012907908E-13,8.70530731785482E-5,0.000170036649084164,
0.000253022524331985),.UNSPECIFIED.);
#23082=B_SPLINE_CURVE_WITH_KNOTS('',3,(#135932,#135933,#135934,#135935,
#135936,#135937,#135938,#135939,#135940,#135941,#135942,#135943,#135944,
#135945),.UNSPECIFIED.,.F.,.F.,(4,2,2,2,2,2,4),(9.99231836108335E-7,0.00392100953658189,
0.00802861330453663,0.0162407023730482,0.032651737543804,0.0654159064689534,
0.130748385933526),.UNSPECIFIED.);
#23083=B_SPLINE_CURVE_WITH_KNOTS('',3,(#135958,#135959,#135960,#135961,
#135962,#135963,#135964,#135965,#135966,#135967),.UNSPECIFIED.,.F.,.F.,
(4,3,3,4),(2.23301994145838E-13,8.70609203873829E-5,0.00017004098563854,
0.000253023205833107),.UNSPECIFIED.);
#23084=B_SPLINE_CURVE_WITH_KNOTS('',3,(#135982,#135983,#135984,#135985,
#135986,#135987,#135988,#135989,#135990,#135991,#135992,#135993,#135994,
#135995),.UNSPECIFIED.,.F.,.F.,(4,2,2,2,2,2,4),(9.66170382949012E-7,0.00392697974081771,
0.00804085973309614,0.0162655707091348,0.0327021207330737,0.065518343067229,
0.130949505770759),.UNSPECIFIED.);
#23085=B_SPLINE_CURVE_WITH_KNOTS('',3,(#136008,#136009,#136010,#136011,
#136012,#136013,#136014,#136015,#136016,#136017),.UNSPECIFIED.,.F.,.F.,
(4,3,3,4),(1.54112774829538E-13,8.70609205573687E-5,0.000170040985736614,
0.000253023205859177),.UNSPECIFIED.);
#23086=B_SPLINE_CURVE_WITH_KNOTS('',3,(#136032,#136033,#136034,#136035,
#136036,#136037,#136038,#136039,#136040,#136041),.UNSPECIFIED.,.F.,.F.,
(4,3,3,4),(0.556212830500469,0.566018334268703,0.571428571428571,0.573654350170116),
 .UNSPECIFIED.);
#23087=B_SPLINE_CURVE_WITH_KNOTS('',3,(#136054,#136055,#136056,#136057,
#136058,#136059,#136060,#136061,#136062,#136063),.UNSPECIFIED.,.F.,.F.,
(4,3,3,4),(2.31230172025941E-13,8.70609204481204E-5,0.00017004098573502,
0.00025302320596535),.UNSPECIFIED.);
#23088=B_SPLINE_CURVE_WITH_KNOTS('',3,(#136078,#136079,#136080,#136081,
#136082,#136083,#136084,#136085,#136086,#136087,#136088,#136089,#136090,
#136091),.UNSPECIFIED.,.F.,.F.,(4,2,2,2,2,2,4),(9.66208308196074E-7,0.00392697967644637,
0.00804085952878198,0.0162655702222953,0.0327021196697788,0.0655183472628571,
0.130949503112459),.UNSPECIFIED.);
#23089=B_SPLINE_CURVE_WITH_KNOTS('',3,(#136104,#136105,#136106,#136107,
#136108,#136109,#136110,#136111,#136112,#136113,#136114,#136115,#136116),
 .UNSPECIFIED.,.F.,.F.,(4,3,3,3,4),(9.22977705889797E-14,8.70609205457749E-5,
0.000149888113578299,0.00017004098589941,0.000253023206195647),
 .UNSPECIFIED.);
#23090=B_SPLINE_CURVE_WITH_KNOTS('',3,(#136131,#136132,#136133,#136134,
#136135,#136136,#136137,#136138,#136139,#136140),.UNSPECIFIED.,.F.,.F.,
(4,3,3,4),(0.556212830497425,0.566018335391702,0.571428571428571,0.573654350184794),
 .UNSPECIFIED.);
#23091=B_SPLINE_CURVE_WITH_KNOTS('',3,(#136153,#136154,#136155,#136156,
#136157,#136158,#136159,#136160,#136161,#136162),.UNSPECIFIED.,.F.,.F.,
(4,3,3,4),(1.21696510425184E-13,8.70609206928594E-5,0.000170040985934045,
0.000253023206118154),.UNSPECIFIED.);
#23092=B_SPLINE_CURVE_WITH_KNOTS('',3,(#136177,#136178,#136179,#136180,
#136181,#136182,#136183,#136184,#136185,#136186,#136187,#136188,#136189,
#136190),.UNSPECIFIED.,.F.,.F.,(4,2,2,2,2,2,4),(9.66228217625918E-7,0.00392697956919349,
0.00804085924933738,0.0162655695995458,0.0327021183655822,0.065518345398006,
0.130949516846548),.UNSPECIFIED.);
#23093=B_SPLINE_CURVE_WITH_KNOTS('',3,(#136203,#136204,#136205,#136206,
#136207,#136208,#136209,#136210,#136211,#136212),.UNSPECIFIED.,.F.,.F.,
(4,3,3,4),(1.83368163365468E-13,8.70609205947636E-5,0.000170040985795044,
0.000253023205937427),.UNSPECIFIED.);
#23094=B_SPLINE_CURVE_WITH_KNOTS('',3,(#136227,#136228,#136229,#136230,
#136231,#136232,#136233,#136234,#136235,#136236),.UNSPECIFIED.,.F.,.F.,
(4,3,3,4),(0.556212830502335,0.566018335768767,0.571428571428571,0.57365435021991),
 .UNSPECIFIED.);
#23095=B_SPLINE_CURVE_WITH_KNOTS('',3,(#136249,#136250,#136251,#136252,
#136253,#136254,#136255,#136256,#136257,#136258),.UNSPECIFIED.,.F.,.F.,
(4,3,3,4),(2.19221044078209E-13,8.70609204363992E-5,0.000170040985578205,
0.000253023205662227),.UNSPECIFIED.);
#23096=B_SPLINE_CURVE_WITH_KNOTS('',3,(#136273,#136274,#136275,#136276,
#136277,#136278,#136279,#136280,#136281,#136282,#136283,#136284,#136285,
#136286),.UNSPECIFIED.,.F.,.F.,(4,2,2,2,2,2,4),(9.66236086782783E-7,0.00392697943596319,
0.00804085891948424,0.0162655688791268,0.0327021168735546,0.0655183394151674,
0.130949508120157),.UNSPECIFIED.);
#23097=B_SPLINE_CURVE_WITH_KNOTS('',3,(#136299,#136300,#136301,#136302,
#136303,#136304,#136305,#136306,#136307,#136308),.UNSPECIFIED.,.F.,.F.,
(4,3,3,4),(1.68080143162128E-13,8.70609204517327E-5,0.000170040985610495,
0.000253023205711627),.UNSPECIFIED.);
#23098=B_SPLINE_CURVE_WITH_KNOTS('',3,(#136323,#136324,#136325,#136326,
#136327,#136328,#136329,#136330,#136331,#136332),.UNSPECIFIED.,.F.,.F.,
(4,3,3,4),(0.556212830495103,0.566018336597087,0.571428571428571,0.573654350166826),
 .UNSPECIFIED.);
#23099=B_SPLINE_CURVE_WITH_KNOTS('',3,(#136345,#136346,#136347,#136348,
#136349,#136350,#136351,#136352,#136353,#136354),.UNSPECIFIED.,.F.,.F.,
(4,3,3,4),(1.34197132127504E-13,8.7060920586027E-5,0.00017004098587252,
0.000253023206102087),.UNSPECIFIED.);
#23100=B_SPLINE_CURVE_WITH_KNOTS('',3,(#136369,#136370,#136371,#136372,
#136373,#136374,#136375,#136376,#136377,#136378),.UNSPECIFIED.,.F.,.F.,
(4,3,3,4),(0.556212830497077,0.566018336499488,0.571428571428571,0.573654350165251),
 .UNSPECIFIED.);
#23101=B_SPLINE_CURVE_WITH_KNOTS('',3,(#136391,#136392,#136393,#136394,
#136395,#136396,#136397,#136398,#136399,#136400),.UNSPECIFIED.,.F.,.F.,
(4,3,3,4),(2.08605666433404E-13,8.70609206450327E-5,0.000170040985681761,
0.000253023205661205),.UNSPECIFIED.);
#23102=B_SPLINE_CURVE_WITH_KNOTS('',3,(#136415,#136416,#136417,#136418,
#136419,#136420,#136421,#136422,#136423,#136424,#136425,#136426,#136427,
#136428),.UNSPECIFIED.,.F.,.F.,(4,2,2,2,2,2,4),(9.66229434957699E-7,0.00392697962088967,
0.00804085935796308,0.0162655698264246,0.0327021188437879,0.065518347343508,
0.130949526287197),.UNSPECIFIED.);
#23103=B_SPLINE_CURVE_WITH_KNOTS('',3,(#136441,#136442,#136443,#136444,
#136445,#136446,#136447,#136448,#136449,#136450),.UNSPECIFIED.,.F.,.F.,
(4,3,3,4),(8.45001259843959E-14,8.70609204120089E-5,0.000170040985741675,
0.000253023206012994),.UNSPECIFIED.);
#23104=B_SPLINE_CURVE_WITH_KNOTS('',3,(#136482,#136483,#136484,#136485,
#136486,#136487,#136488,#136489,#136490,#136491),.UNSPECIFIED.,.F.,.F.,
(4,3,3,4),(1.51987334395212E-13,8.70609206640265E-5,0.000170040985730083,
0.000253023205738738),.UNSPECIFIED.);
#23105=B_SPLINE_CURVE_WITH_KNOTS('',3,(#136523,#136524,#136525,#136526,
#136527,#136528,#136529,#136530,#136531,#136532),.UNSPECIFIED.,.F.,.F.,
(4,3,3,4),(2.21373845505911E-13,8.7060920434661E-5,0.000170040985496251,
0.000253023205500094),.UNSPECIFIED.);
#23106=B_SPLINE_CURVE_WITH_KNOTS('',3,(#136547,#136548,#136549,#136550,
#136551,#136552,#136553,#136554,#136555,#136556),.UNSPECIFIED.,.F.,.F.,
(4,3,3,4),(0.556212830498472,0.566018335338913,0.571428571428571,0.573654350176112),
 .UNSPECIFIED.);
#23107=B_SPLINE_CURVE_WITH_KNOTS('',3,(#136569,#136570,#136571,#136572,
#136573,#136574,#136575,#136576,#136577,#136578),.UNSPECIFIED.,.F.,.F.,
(4,3,3,4),(1.17323887739643E-13,8.70609205778466E-5,0.000170040985778564,
0.000253023205922772),.UNSPECIFIED.);
#23108=B_SPLINE_CURVE_WITH_KNOTS('',3,(#136593,#136594,#136595,#136596,
#136597,#136598,#136599,#136600,#136601,#136602,#136603,#136604,#136605,
#136606),.UNSPECIFIED.,.F.,.F.,(4,2,2,2,2,2,4),(9.66258725593663E-7,0.00392697940720579,
0.00804085883290391,0.0162655686774062,0.0327021164455095,0.0655183366867418,
0.130949485166268),.UNSPECIFIED.);
#23109=B_SPLINE_CURVE_WITH_KNOTS('',3,(#136619,#136620,#136621,#136622,
#136623,#136624,#136625,#136626,#136627,#136628),.UNSPECIFIED.,.F.,.F.,
(4,3,3,4),(9.6474942780677E-14,8.70609207631378E-5,0.000170040985962259,
0.000253023206105505),.UNSPECIFIED.);
#23110=B_SPLINE_CURVE_WITH_KNOTS('',3,(#136643,#136644,#136645,#136646,
#136647,#136648,#136649,#136650,#136651,#136652),.UNSPECIFIED.,.F.,.F.,
(4,3,3,4),(0.556212830494827,0.566018337704693,0.571428571428571,0.573654350156748),
 .UNSPECIFIED.);
#23111=B_SPLINE_CURVE_WITH_KNOTS('',3,(#136665,#136666,#136667,#136668,
#136669,#136670,#136671,#136672,#136673,#136674,#136675,#136676,#136677),
 .UNSPECIFIED.,.F.,.F.,(4,3,3,3,4),(1.69396119959038E-13,8.70609205411585E-5,
0.00014988811322635,0.000170040985712469,0.000253023205827122),
 .UNSPECIFIED.);
#23112=B_SPLINE_CURVE_WITH_KNOTS('',3,(#136709,#136710,#136711,#136712,
#136713,#136714,#136715,#136716,#136717,#136718),.UNSPECIFIED.,.F.,.F.,
(4,3,3,4),(2.53759373651446E-13,8.70609204134188E-5,0.00017004098566721,
0.000253023205863598),.UNSPECIFIED.);
#23113=B_SPLINE_CURVE_WITH_KNOTS('',3,(#136733,#136734,#136735,#136736,
#136737,#136738,#136739,#136740,#136741,#136742,#136743,#136744,#136745,
#136746),.UNSPECIFIED.,.F.,.F.,(4,2,2,2,2,2,4),(9.66185494312226E-7,0.00392697955586284,
0.00804085929090517,0.0162655697528746,0.0327021187492143,0.0655183447212016,
0.130949516658934),.UNSPECIFIED.);
#23114=B_SPLINE_CURVE_WITH_KNOTS('',3,(#136759,#136760,#136761,#136762,
#136763,#136764,#136765,#136766,#136767,#136768),.UNSPECIFIED.,.F.,.F.,
(4,3,3,4),(1.35512089641325E-13,8.70609204684551E-5,0.00017004098566191,
0.000253023205798563),.UNSPECIFIED.);
#23115=B_SPLINE_CURVE_WITH_KNOTS('',3,(#136800,#136801,#136802,#136803,
#136804,#136805,#136806,#136807,#136808,#136809),.UNSPECIFIED.,.F.,.F.,
(4,3,3,4),(1.92969421757801E-13,8.7060920517829E-5,0.000170040985827322,
0.00025302320608008),.UNSPECIFIED.);
#23116=B_SPLINE_CURVE_WITH_KNOTS('',3,(#136824,#136825,#136826,#136827,
#136828,#136829,#136830,#136831,#136832,#136833,#136834,#136835,#136836,
#136837),.UNSPECIFIED.,.F.,.F.,(4,2,2,2,2,2,4),(9.66178287892415E-7,0.00392697957748608,
0.0080408593582245,0.0162655699127301,0.0327021190987407,0.0655183508972541,
0.130949528205721),.UNSPECIFIED.);
#23117=B_SPLINE_CURVE_WITH_KNOTS('',3,(#136850,#136851,#136852,#136853,
#136854,#136855,#136856,#136857,#136858,#136859,#136860,#136861,#136862),
 .UNSPECIFIED.,.F.,.F.,(4,3,3,3,4),(8.40873567267271E-14,8.70609204912656E-5,
0.000149888113153304,0.000170040985908062,0.000253023206266478),
 .UNSPECIFIED.);
#23118=B_SPLINE_CURVE_WITH_KNOTS('',3,(#136877,#136878,#136879,#136880,
#136881,#136882,#136883,#136884,#136885,#136886),.UNSPECIFIED.,.F.,.F.,
(4,3,3,4),(0.556212830496238,0.566018336002845,0.571428571428571,0.573654350219912),
 .UNSPECIFIED.);
#23119=B_SPLINE_CURVE_WITH_KNOTS('',3,(#136899,#136900,#136901,#136902,
#136903,#136904,#136905,#136906,#136907,#136908,#136909,#136910,#136911),
 .UNSPECIFIED.,.F.,.F.,(4,3,3,3,4),(2.14110068371842E-13,8.70609204644119E-5,
0.00014988811341431,0.000170040985596898,0.00025302320567211),
 .UNSPECIFIED.);
#23120=B_SPLINE_CURVE_WITH_KNOTS('',3,(#136926,#136927,#136928,#136929,
#136930,#136931,#136932,#136933,#136934,#136935),.UNSPECIFIED.,.F.,.F.,
(4,3,3,4),(0.556212830493125,0.566018337095459,0.571428571428571,0.573654350190219),
 .UNSPECIFIED.);
#23121=B_SPLINE_CURVE_WITH_KNOTS('',3,(#136948,#136949,#136950,#136951,
#136952,#136953,#136954,#136955,#136956,#136957),.UNSPECIFIED.,.F.,.F.,
(4,3,3,4),(9.00758862279578E-14,8.70609204372189E-5,0.00017004098588756,
0.000253023206279836),.UNSPECIFIED.);
#23122=B_SPLINE_CURVE_WITH_KNOTS('',3,(#136972,#136973,#136974,#136975,
#136976,#136977,#136978,#136979,#136980,#136981,#136982,#136983,#136984,
#136985),.UNSPECIFIED.,.F.,.F.,(4,2,2,2,2,2,4),(9.66205425621697E-7,0.00392697955933081,
0.0080408592506326,0.0162655696235016,0.0327021184357382,0.0655183462173166,
0.130949515010481),.UNSPECIFIED.);
#23123=B_SPLINE_CURVE_WITH_KNOTS('',3,(#136998,#136999,#137000,#137001,
#137002,#137003,#137004,#137005,#137006,#137007),.UNSPECIFIED.,.F.,.F.,
(4,3,3,4),(9.05841708095265E-14,8.70609207349165E-5,0.000170040985889652,
0.000253023205987879),.UNSPECIFIED.);
#23124=B_SPLINE_CURVE_WITH_KNOTS('',3,(#137022,#137023,#137024,#137025,
#137026,#137027,#137028,#137029,#137030,#137031,#137032,#137033,#137034,
#137035),.UNSPECIFIED.,.F.,.F.,(4,2,2,2,2,2,4),(9.66222234121705E-7,0.0039269794756902,
0.00804085902143472,0.0162655691092118,0.0327021173752005,0.0655183417329978,
0.13094951369088),.UNSPECIFIED.);
#23125=B_SPLINE_CURVE_WITH_KNOTS('',3,(#137048,#137049,#137050,#137051,
#137052,#137053,#137054,#137055,#137056,#137057),.UNSPECIFIED.,.F.,.F.,
(4,3,3,4),(1.80010415397423E-13,8.70609205854221E-5,0.000170040985761325,
0.000253023205880155),.UNSPECIFIED.);
#23126=B_SPLINE_CURVE_WITH_KNOTS('',3,(#137089,#137090,#137091,#137092,
#137093,#137094,#137095,#137096,#137097,#137098),.UNSPECIFIED.,.F.,.F.,
(4,3,3,4),(1.78220905471141E-13,8.70609204854381E-5,0.000170040985755445,
0.00025302320596902),.UNSPECIFIED.);
#23127=B_SPLINE_CURVE_WITH_KNOTS('',3,(#137130,#137131,#137132,#137133,
#137134,#137135,#137136,#137137,#137138,#137139),.UNSPECIFIED.,.F.,.F.,
(4,3,3,4),(1.58771823130732E-13,8.706092047505E-5,0.000170040985667919,
0.000253023205802976),.UNSPECIFIED.);
#23128=B_SPLINE_CURVE_WITH_KNOTS('',3,(#137154,#137155,#137156,#137157,
#137158,#137159,#137160,#137161,#137162,#137163,#137164,#137165,#137166,
#137167),.UNSPECIFIED.,.F.,.F.,(4,2,2,2,2,2,4),(9.66239005217944E-7,0.00392697936493239,
0.00804085874914389,0.0162655685121116,0.0327021161219164,0.0655183394313766,
0.13094949754352),.UNSPECIFIED.);
#23129=B_SPLINE_CURVE_WITH_KNOTS('',3,(#137180,#137181,#137182,#137183,
#137184,#137185,#137186,#137187,#137188,#137189),.UNSPECIFIED.,.F.,.F.,
(4,3,3,4),(1.50946766794193E-13,8.70609205558374E-5,0.000170040985841153,
0.000253023206069007),.UNSPECIFIED.);
#23130=B_SPLINE_CURVE_WITH_KNOTS('',3,(#137221,#137222,#137223,#137224,
#137225,#137226,#137227,#137228,#137229,#137230),.UNSPECIFIED.,.F.,.F.,
(4,3,3,4),(1.65491426438259E-13,8.70609204190512E-5,0.000170040985661301,
0.000253023205846518),.UNSPECIFIED.);
#23131=B_SPLINE_CURVE_WITH_KNOTS('',3,(#137245,#137246,#137247,#137248,
#137249,#137250,#137251,#137252,#137253,#137254),.UNSPECIFIED.,.F.,.F.,
(4,3,3,4),(0.556212830497802,0.566018335697945,0.571428571428571,0.573654350193131),
 .UNSPECIFIED.);
#23132=B_SPLINE_CURVE_WITH_KNOTS('',3,(#137267,#137268,#137269,#137270,
#137271,#137272,#137273,#137274,#137275,#137276,#137277,#137278,#137279),
 .UNSPECIFIED.,.F.,.F.,(4,3,3,3,4),(1.70398673709338E-13,8.70609205616646E-5,
0.000149888113059747,0.000170040985758334,0.000253023205898846),
 .UNSPECIFIED.);
#23133=B_SPLINE_CURVE_WITH_KNOTS('',3,(#137294,#137295,#137296,#137297,
#137298,#137299,#137300,#137301,#137302,#137303,#137304,#137305,#137306,
#137307),.UNSPECIFIED.,.F.,.F.,(4,2,2,2,2,2,4),(9.66463546611146E-7,0.0039269796958211,
0.00804085923376171,0.0162655693016797,0.03270211751058,0.0655183395302705,
0.130949485085588),.UNSPECIFIED.);
#23134=B_SPLINE_CURVE_WITH_KNOTS('',3,(#137322,#137323,#137324,#137325,
#137326,#137327),.UNSPECIFIED.,.F.,.F.,(4,2,4),(-0.0252969421656862,-0.0126483573154483,
-1.73911152839823E-10),.UNSPECIFIED.);
#23135=B_SPLINE_CURVE_WITH_KNOTS('',3,(#137340,#137341,#137342,#137343,
#137344,#137345,#137346),.UNSPECIFIED.,.F.,.F.,(4,3,4),(0.211502584834065,
0.214285714285714,0.223668160746706),.UNSPECIFIED.);
#23136=B_SPLINE_CURVE_WITH_KNOTS('',3,(#137347,#137348,#137349,#137350,
#137351,#137352),.UNSPECIFIED.,.F.,.F.,(4,2,4),(9.42251804061677E-11,0.0126483643388585,
0.0252969714247671),.UNSPECIFIED.);
#23137=B_SPLINE_CURVE_WITH_KNOTS('',3,(#137383,#137384,#137385,#137386,
#137387,#137388,#137389),.UNSPECIFIED.,.F.,.F.,(4,3,4),(0.211502584834048,
0.214285714285714,0.22366816074129),.UNSPECIFIED.);
#23138=B_SPLINE_CURVE_WITH_KNOTS('',3,(#137390,#137391,#137392,#137393,
#137394,#137395),.UNSPECIFIED.,.F.,.F.,(4,2,4),(1.25234643137483E-10,0.0126483644130537,
0.0252969715703692),.UNSPECIFIED.);
#23139=B_SPLINE_CURVE_WITH_KNOTS('',3,(#137426,#137427,#137428,#137429,
#137430,#137431,#137432),.UNSPECIFIED.,.F.,.F.,(4,3,4),(0.21150258483404,
0.214285714285714,0.223668160746203),.UNSPECIFIED.);
#23140=B_SPLINE_CURVE_WITH_KNOTS('',3,(#137433,#137434,#137435,#137436,
#137437,#137438),.UNSPECIFIED.,.F.,.F.,(4,2,4),(1.42901220958907E-10,0.0126483641798076,
0.0252969707431301),.UNSPECIFIED.);
#23141=B_SPLINE_CURVE_WITH_KNOTS('',3,(#137469,#137470,#137471,#137472,
#137473,#137474,#137475),.UNSPECIFIED.,.F.,.F.,(4,3,4),(0.211502584834064,
0.214285714285714,0.223668160739962),.UNSPECIFIED.);
#23142=B_SPLINE_CURVE_WITH_KNOTS('',3,(#137476,#137477,#137478,#137479,
#137480,#137481),.UNSPECIFIED.,.F.,.F.,(4,2,4),(1.57040128483674E-10,0.0126483646230286,
0.0252969722387553),.UNSPECIFIED.);
#23143=B_SPLINE_CURVE_WITH_KNOTS('',3,(#137512,#137513,#137514,#137515,
#137516,#137517,#137518),.UNSPECIFIED.,.F.,.F.,(4,3,4),(0.211502584834063,
0.214285714285714,0.223668160743146),.UNSPECIFIED.);
#23144=B_SPLINE_CURVE_WITH_KNOTS('',3,(#137519,#137520,#137521,#137522,
#137523,#137524),.UNSPECIFIED.,.F.,.F.,(4,2,4),(1.52830003479099E-10,0.0126483646010041,
0.0252969722035216),.UNSPECIFIED.);
#23145=B_SPLINE_CURVE_WITH_KNOTS('',3,(#137555,#137556,#137557,#137558,
#137559,#137560,#137561),.UNSPECIFIED.,.F.,.F.,(4,3,4),(0.211502584834064,
0.214285714285714,0.223668160739557),.UNSPECIFIED.);
#23146=B_SPLINE_CURVE_WITH_KNOTS('',3,(#137562,#137563,#137564,#137565,
#137566,#137567),.UNSPECIFIED.,.F.,.F.,(4,2,4),(1.48807329848891E-10,0.0126483641904826,
0.0252969707513306),.UNSPECIFIED.);
#23147=B_SPLINE_CURVE_WITH_KNOTS('',3,(#137596,#137597,#137598,#137599,
#137600,#137601),.UNSPECIFIED.,.F.,.F.,(4,2,4),(1.81998596448827E-10,0.0126483575178079,
0.0252969430018216),.UNSPECIFIED.);
#23148=B_SPLINE_CURVE_WITH_KNOTS('',3,(#137626,#137627,#137628,#137629,
#137630,#137631,#137632),.UNSPECIFIED.,.F.,.F.,(4,3,4),(0.211502584834064,
0.214285714285714,0.223668160743121),.UNSPECIFIED.);
#23149=B_SPLINE_CURVE_WITH_KNOTS('',3,(#137633,#137634,#137635,#137636,
#137637,#137638),.UNSPECIFIED.,.F.,.F.,(4,2,4),(9.7444894850297E-11,0.0126483571249872,
0.0252969416070819),.UNSPECIFIED.);
#23150=B_SPLINE_CURVE_WITH_KNOTS('',3,(#137669,#137670,#137671,#137672,
#137673,#137674,#137675),.UNSPECIFIED.,.F.,.F.,(4,3,4),(0.211502584834064,
0.214285714285714,0.223668160737537),.UNSPECIFIED.);
#23151=B_SPLINE_CURVE_WITH_KNOTS('',3,(#137676,#137677,#137678,#137679,
#137680,#137681),.UNSPECIFIED.,.F.,.F.,(4,2,4),(1.68360222936878E-10,0.0126483646033732,
0.0252969722045489),.UNSPECIFIED.);
#23152=B_SPLINE_CURVE_WITH_KNOTS('',3,(#137712,#137713,#137714,#137715,
#137716,#137717,#137718),.UNSPECIFIED.,.F.,.F.,(4,3,4),(0.21150258483406,
0.214285714285714,0.223668160740989),.UNSPECIFIED.);
#23153=B_SPLINE_CURVE_WITH_KNOTS('',3,(#137719,#137720,#137721,#137722,
#137723,#137724),.UNSPECIFIED.,.F.,.F.,(4,2,4),(1.3435638487885E-10,0.0126483643087339,
0.0252969712788357),.UNSPECIFIED.);
#23154=B_SPLINE_CURVE_WITH_KNOTS('',3,(#137755,#137756,#137757,#137758,
#137759,#137760,#137761),.UNSPECIFIED.,.F.,.F.,(4,3,4),(0.211502584834064,
0.214285714285714,0.223668160735638),.UNSPECIFIED.);
#23155=B_SPLINE_CURVE_WITH_KNOTS('',3,(#137762,#137763,#137764,#137765,
#137766,#137767),.UNSPECIFIED.,.F.,.F.,(4,2,4),(1.03868961680616E-10,0.0126483570659925,
0.0252969412940665),.UNSPECIFIED.);
#23156=B_SPLINE_CURVE_WITH_KNOTS('',3,(#137798,#137799,#137800,#137801,
#137802,#137803,#137804),.UNSPECIFIED.,.F.,.F.,(4,3,4),(0.211502584834024,
0.214285714285714,0.223668160739353),.UNSPECIFIED.);
#23157=B_SPLINE_CURVE_WITH_KNOTS('',3,(#137805,#137806,#137807,#137808,
#137809,#137810),.UNSPECIFIED.,.F.,.F.,(4,2,4),(9.76223213263302E-11,0.0126483642710012,
0.0252969711027679),.UNSPECIFIED.);
#23158=B_SPLINE_CURVE_WITH_KNOTS('',3,(#137841,#137842,#137843,#137844,
#137845,#137846,#137847),.UNSPECIFIED.,.F.,.F.,(4,3,4),(0.211502584834064,
0.214285714285714,0.223668160736429),.UNSPECIFIED.);
#23159=B_SPLINE_CURVE_WITH_KNOTS('',3,(#137848,#137849,#137850,#137851,
#137852,#137853),.UNSPECIFIED.,.F.,.F.,(4,2,4),(1.53232547903038E-10,0.0126483575945804,
0.0252969433218694),.UNSPECIFIED.);
#23160=B_SPLINE_CURVE_WITH_KNOTS('',3,(#137884,#137885,#137886,#137887,
#137888,#137889,#137890),.UNSPECIFIED.,.F.,.F.,(4,3,4),(0.211502584834064,
0.214285714285714,0.223668160740088),.UNSPECIFIED.);
#23161=B_SPLINE_CURVE_WITH_KNOTS('',3,(#137891,#137892,#137893,#137894,
#137895,#137896),.UNSPECIFIED.,.F.,.F.,(4,2,4),(1.70742253820634E-10,0.0126483643594943,
0.0252969713224395),.UNSPECIFIED.);
#23162=B_SPLINE_CURVE_WITH_KNOTS('',3,(#137927,#137928,#137929,#137930,
#137931,#137932,#137933),.UNSPECIFIED.,.F.,.F.,(4,3,4),(0.211502584833965,
0.214285714285714,0.22366816073647),.UNSPECIFIED.);
#23163=B_SPLINE_CURVE_WITH_KNOTS('',3,(#137934,#137935,#137936,#137937,
#137938,#137939),.UNSPECIFIED.,.F.,.F.,(4,2,4),(1.17570601323076E-10,0.0126483643814668,
0.0252969715083944),.UNSPECIFIED.);
#23164=B_SPLINE_CURVE_WITH_KNOTS('',3,(#137970,#137971,#137972,#137973,
#137974,#137975,#137976),.UNSPECIFIED.,.F.,.F.,(4,3,4),(0.211502584833903,
0.214285714285714,0.223668160739684),.UNSPECIFIED.);
#23165=B_SPLINE_CURVE_WITH_KNOTS('',3,(#137977,#137978,#137979,#137980,
#137981,#137982),.UNSPECIFIED.,.F.,.F.,(4,2,4),(1.58595950739882E-10,0.0126483645926137,
0.0252969721769568),.UNSPECIFIED.);
#23166=B_SPLINE_CURVE_WITH_KNOTS('',3,(#138013,#138014,#138015,#138016,
#138017,#138018,#138019),.UNSPECIFIED.,.F.,.F.,(4,3,4),(0.211502584833963,
0.214285714285714,0.223668160739601),.UNSPECIFIED.);
#23167=B_SPLINE_CURVE_WITH_KNOTS('',3,(#138020,#138021,#138022,#138023,
#138024,#138025),.UNSPECIFIED.,.F.,.F.,(4,2,4),(1.37481879759042E-10,0.0126483642605855,
0.0252969710301908),.UNSPECIFIED.);
#23168=B_SPLINE_CURVE_WITH_KNOTS('',3,(#138056,#138057,#138058,#138059,
#138060,#138061,#138062),.UNSPECIFIED.,.F.,.F.,(4,3,4),(0.211502584833935,
0.214285714285714,0.223668160739935),.UNSPECIFIED.);
#23169=B_SPLINE_CURVE_WITH_KNOTS('',3,(#138063,#138064,#138065,#138066,
#138067,#138068),.UNSPECIFIED.,.F.,.F.,(4,2,4),(1.15062703877832E-10,0.0126483572960972,
0.0252969421882394),.UNSPECIFIED.);
#23170=B_SPLINE_CURVE_WITH_KNOTS('',3,(#138099,#138100,#138101,#138102,
#138103,#138104,#138105),.UNSPECIFIED.,.F.,.F.,(4,3,4),(0.211502584833671,
0.214285714285714,0.223668160740443),.UNSPECIFIED.);
#23171=B_SPLINE_CURVE_WITH_KNOTS('',3,(#138106,#138107,#138108,#138109,
#138110,#138111),.UNSPECIFIED.,.F.,.F.,(4,2,4),(1.65806997188092E-10,0.0126483573808185,
0.0252969424808111),.UNSPECIFIED.);
#23172=B_SPLINE_CURVE_WITH_KNOTS('',3,(#138142,#138143,#138144,#138145,
#138146,#138147,#138148),.UNSPECIFIED.,.F.,.F.,(4,3,4),(0.211502584833923,
0.214285714285714,0.223668160474533),.UNSPECIFIED.);
#23173=B_SPLINE_CURVE_WITH_KNOTS('',3,(#138149,#138150,#138151,#138152,
#138153,#138154),.UNSPECIFIED.,.F.,.F.,(4,2,4),(1.3364996508922E-10,0.0126483641814018,
0.0252969708486838),.UNSPECIFIED.);
#23174=B_SPLINE_CURVE_WITH_KNOTS('',3,(#138186,#138187,#138188,#138189,
#138190,#138191,#138192),.UNSPECIFIED.,.F.,.F.,(4,3,4),(0.21150258483406,
0.214285714285714,0.223668160737251),.UNSPECIFIED.);
#23175=B_SPLINE_CURVE_WITH_KNOTS('',3,(#138193,#138194,#138195,#138196,
#138197,#138198),.UNSPECIFIED.,.F.,.F.,(4,2,4),(1.65464212098833E-10,0.012648364586302,
0.0252969721645957),.UNSPECIFIED.);
#23176=B_SPLINE_CURVE_WITH_KNOTS('',3,(#138228,#138229,#138230,#138231,
#138232,#138233,#138234),.UNSPECIFIED.,.F.,.F.,(4,3,4),(0.211502584834061,
0.214285714285714,0.223668160736262),.UNSPECIFIED.);
#23177=B_SPLINE_CURVE_WITH_KNOTS('',3,(#138235,#138236,#138237,#138238,
#138239,#138240),.UNSPECIFIED.,.F.,.F.,(4,2,4),(7.5709302282454E-11,0.0126483643841512,
0.0252969716087726),.UNSPECIFIED.);
#23178=B_SPLINE_CURVE_WITH_KNOTS('',3,(#138271,#138272,#138273,#138274,
#138275,#138276,#138277),.UNSPECIFIED.,.F.,.F.,(4,3,4),(0.211502584834065,
0.214285714285714,0.223668160742396),.UNSPECIFIED.);
#23179=B_SPLINE_CURVE_WITH_KNOTS('',3,(#138278,#138279,#138280,#138281,
#138282,#138283),.UNSPECIFIED.,.F.,.F.,(4,2,4),(1.28302262445121E-10,0.0126483641874972,
0.0252969707835284),.UNSPECIFIED.);
#23180=B_SPLINE_CURVE_WITH_KNOTS('',3,(#138314,#138315,#138316,#138317,
#138318,#138319,#138320),.UNSPECIFIED.,.F.,.F.,(4,3,4),(0.211502584834065,
0.214285714285714,0.223668160739137),.UNSPECIFIED.);
#23181=B_SPLINE_CURVE_WITH_KNOTS('',3,(#138321,#138322,#138323,#138324,
#138325,#138326),.UNSPECIFIED.,.F.,.F.,(4,2,4),(1.21129596779304E-10,0.0126483571382297,
0.0252969415887335),.UNSPECIFIED.);
#23182=B_SPLINE_CURVE_WITH_KNOTS('',3,(#138357,#138358,#138359,#138360,
#138361,#138362,#138363),.UNSPECIFIED.,.F.,.F.,(4,3,4),(0.211502584834064,
0.214285714285714,0.223668160739874),.UNSPECIFIED.);
#23183=B_SPLINE_CURVE_WITH_KNOTS('',3,(#138364,#138365,#138366,#138367,
#138368,#138369),.UNSPECIFIED.,.F.,.F.,(4,2,4),(8.64124104036477E-11,0.0126483569711156,
0.0252969409241859),.UNSPECIFIED.);
#23184=B_SPLINE_CURVE_WITH_KNOTS('',3,(#138400,#138401,#138402,#138403,
#138404,#138405,#138406),.UNSPECIFIED.,.F.,.F.,(4,3,4),(0.211502584834065,
0.214285714285714,0.223668160739885),.UNSPECIFIED.);
#23185=B_SPLINE_CURVE_WITH_KNOTS('',3,(#138407,#138408,#138409,#138410,
#138411,#138412),.UNSPECIFIED.,.F.,.F.,(4,2,4),(2.07944688460402E-10,0.012648364645067,
0.02529697221805),.UNSPECIFIED.);
#23186=B_SPLINE_CURVE_WITH_KNOTS('',3,(#138443,#138444,#138445,#138446,
#138447,#138448,#138449),.UNSPECIFIED.,.F.,.F.,(4,3,4),(0.211502584834065,
0.214285714285714,0.223668160741145),.UNSPECIFIED.);
#23187=B_SPLINE_CURVE_WITH_KNOTS('',3,(#138450,#138451,#138452,#138453,
#138454,#138455),.UNSPECIFIED.,.F.,.F.,(4,2,4),(1.69193695001643E-10,0.0126483642077223,
0.0252969707648244),.UNSPECIFIED.);
#23188=B_SPLINE_CURVE_WITH_KNOTS('',3,(#138486,#138487,#138488,#138489,
#138490,#138491,#138492),.UNSPECIFIED.,.F.,.F.,(4,3,4),(0.211502584834065,
0.214285714285714,0.223668160742228),.UNSPECIFIED.);
#23189=B_SPLINE_CURVE_WITH_KNOTS('',3,(#138493,#138494,#138495,#138496,
#138497,#138498),.UNSPECIFIED.,.F.,.F.,(4,2,4),(4.48927338603257E-11,0.0126483642352892,
0.0252969711325811),.UNSPECIFIED.);
#23190=B_SPLINE_CURVE_WITH_KNOTS('',3,(#138522,#138523,#138524,#138525,
#138526,#138527,#138528),.UNSPECIFIED.,.F.,.F.,(4,3,4),(0.211502584834063,
0.214285714285714,0.223668160734462),.UNSPECIFIED.);
#23191=B_SPLINE_CURVE_WITH_KNOTS('',3,(#138551,#138552,#138553,#138554,
#138555,#138556),.UNSPECIFIED.,.F.,.F.,(4,2,4),(1.55326272845714E-12,0.0126511155057583,
0.0253019892655775),.UNSPECIFIED.);
#23192=B_SPLINE_CURVE_WITH_KNOTS('',3,(#138573,#138574,#138575,#138576,
#138577,#138578,#138579),.UNSPECIFIED.,.F.,.F.,(4,3,4),(0.556108173865714,
0.558333952657053,0.568296447146679),.UNSPECIFIED.);
#23193=B_SPLINE_CURVE_WITH_KNOTS('',3,(#138580,#138581,#138582,#138583,
#138584,#138585),.UNSPECIFIED.,.F.,.F.,(4,2,4),(-0.0253019896340801,-0.012651115732023,
-4.08147370067891E-11),.UNSPECIFIED.);
#23194=B_SPLINE_CURVE_WITH_KNOTS('',3,(#138616,#138617,#138618,#138619,
#138620,#138621,#138622),.UNSPECIFIED.,.F.,.F.,(4,3,4),(0.556108173865714,
0.558333952657053,0.568296447141869),.UNSPECIFIED.);
#23195=B_SPLINE_CURVE_WITH_KNOTS('',3,(#138623,#138624,#138625,#138626,
#138627,#138628),.UNSPECIFIED.,.F.,.F.,(4,2,4),(-0.0253019894957092,-0.0126511156236248,
-2.40536167372962E-11),.UNSPECIFIED.);
#23196=B_SPLINE_CURVE_WITH_KNOTS('',3,(#138659,#138660,#138661,#138662,
#138663,#138664,#138665),.UNSPECIFIED.,.F.,.F.,(4,3,4),(0.556108173865714,
0.558333952657053,0.568296447138677),.UNSPECIFIED.);
#23197=B_SPLINE_CURVE_WITH_KNOTS('',3,(#138666,#138667,#138668,#138669,
#138670,#138671),.UNSPECIFIED.,.F.,.F.,(4,2,4),(-0.0253019896232341,-0.0126511156790116,
-3.02607001956279E-11),.UNSPECIFIED.);
#23198=B_SPLINE_CURVE_WITH_KNOTS('',3,(#138702,#138703,#138704,#138705,
#138706,#138707,#138708),.UNSPECIFIED.,.F.,.F.,(4,3,4),(0.556108173865714,
0.558333952657053,0.568296447137058),.UNSPECIFIED.);
#23199=B_SPLINE_CURVE_WITH_KNOTS('',3,(#138709,#138710,#138711,#138712,
#138713,#138714),.UNSPECIFIED.,.F.,.F.,(4,2,4),(-0.0253019894885685,-0.0126511156165778,
-1.93016713723182E-11),.UNSPECIFIED.);
#23200=B_SPLINE_CURVE_WITH_KNOTS('',3,(#138745,#138746,#138747,#138748,
#138749,#138750,#138751),.UNSPECIFIED.,.F.,.F.,(4,3,4),(0.556108173865714,
0.558333952657053,0.568296447144668),.UNSPECIFIED.);
#23201=B_SPLINE_CURVE_WITH_KNOTS('',3,(#138752,#138753,#138754,#138755,
#138756,#138757),.UNSPECIFIED.,.F.,.F.,(4,2,4),(-0.02530198959003,-0.0126511156559188,
-1.74384499895819E-11),.UNSPECIFIED.);
#23202=B_SPLINE_CURVE_WITH_KNOTS('',3,(#138788,#138789,#138790,#138791,
#138792,#138793,#138794),.UNSPECIFIED.,.F.,.F.,(4,3,4),(0.556108173865714,
0.558333952657053,0.568296447144199),.UNSPECIFIED.);
#23203=B_SPLINE_CURVE_WITH_KNOTS('',3,(#138795,#138796,#138797,#138798,
#138799,#138800),.UNSPECIFIED.,.F.,.F.,(4,2,4),(-0.0253019895178097,-0.0126511156113887,
-1.91482177336333E-11),.UNSPECIFIED.);
#23204=B_SPLINE_CURVE_WITH_KNOTS('',3,(#138831,#138832,#138833,#138834,
#138835,#138836,#138837),.UNSPECIFIED.,.F.,.F.,(4,3,4),(0.556108173865714,
0.558333952657053,0.568296447147839),.UNSPECIFIED.);
#23205=B_SPLINE_CURVE_WITH_KNOTS('',3,(#138838,#138839,#138840,#138841,
#138842,#138843),.UNSPECIFIED.,.F.,.F.,(4,2,4),(-0.0253019896252546,-0.012651115666266,
-1.96323547696498E-11),.UNSPECIFIED.);
#23206=B_SPLINE_CURVE_WITH_KNOTS('',3,(#138874,#138875,#138876,#138877,
#138878,#138879,#138880),.UNSPECIFIED.,.F.,.F.,(4,3,4),(0.556108173865714,
0.558333952657053,0.568296447147786),.UNSPECIFIED.);
#23207=B_SPLINE_CURVE_WITH_KNOTS('',3,(#138881,#138882,#138883,#138884,
#138885,#138886),.UNSPECIFIED.,.F.,.F.,(4,2,4),(-0.0253019895396078,-0.0126511156269564,
-2.44738500299047E-11),.UNSPECIFIED.);
#23208=B_SPLINE_CURVE_WITH_KNOTS('',3,(#138917,#138918,#138919,#138920,
#138921,#138922,#138923),.UNSPECIFIED.,.F.,.F.,(4,3,4),(0.556108173865715,
0.558333952657054,0.568296447135626),.UNSPECIFIED.);
#23209=B_SPLINE_CURVE_WITH_KNOTS('',3,(#138924,#138925,#138926,#138927,
#138928,#138929),.UNSPECIFIED.,.F.,.F.,(4,2,4),(-0.0253019895314073,-0.012651115614323,
-3.54363170751437E-11),.UNSPECIFIED.);
#23210=B_SPLINE_CURVE_WITH_KNOTS('',3,(#138960,#138961,#138962,#138963,
#138964,#138965,#138966),.UNSPECIFIED.,.F.,.F.,(4,3,4),(0.556108173865715,
0.558333952657055,0.568296447138926),.UNSPECIFIED.);
#23211=B_SPLINE_CURVE_WITH_KNOTS('',3,(#138967,#138968,#138969,#138970,
#138971,#138972),.UNSPECIFIED.,.F.,.F.,(4,2,4),(-0.025301989606925,-0.0126511156406089,
-2.78329234659758E-11),.UNSPECIFIED.);
#23212=B_SPLINE_CURVE_WITH_KNOTS('',3,(#139003,#139004,#139005,#139006,
#139007,#139008,#139009),.UNSPECIFIED.,.F.,.F.,(4,3,4),(0.556108173865715,
0.558333952657055,0.568296447147264),.UNSPECIFIED.);
#23213=B_SPLINE_CURVE_WITH_KNOTS('',3,(#139010,#139011,#139012,#139013,
#139014,#139015),.UNSPECIFIED.,.F.,.F.,(4,2,4),(-0.0253019896476435,-0.0126511157227825,
-2.66785100955236E-11),.UNSPECIFIED.);
#23214=B_SPLINE_CURVE_WITH_KNOTS('',3,(#139046,#139047,#139048,#139049,
#139050,#139051,#139052),.UNSPECIFIED.,.F.,.F.,(4,3,4),(0.556108173865715,
0.558333952657055,0.56829644715269),.UNSPECIFIED.);
#23215=B_SPLINE_CURVE_WITH_KNOTS('',3,(#139053,#139054,#139055,#139056,
#139057,#139058),.UNSPECIFIED.,.F.,.F.,(4,2,4),(-0.0253019895519308,-0.0126511156492357,
-3.55825612030625E-11),.UNSPECIFIED.);
#23216=B_SPLINE_CURVE_WITH_KNOTS('',3,(#139089,#139090,#139091,#139092,
#139093,#139094,#139095),.UNSPECIFIED.,.F.,.F.,(4,3,4),(0.556108173865715,
0.558333952657055,0.568296447144007),.UNSPECIFIED.);
#23217=B_SPLINE_CURVE_WITH_KNOTS('',3,(#139096,#139097,#139098,#139099,
#139100,#139101),.UNSPECIFIED.,.F.,.F.,(4,2,4),(-0.025301989516701,-0.01265111561885,
-5.85913262352022E-12),.UNSPECIFIED.);
#23218=B_SPLINE_CURVE_WITH_KNOTS('',3,(#139130,#139131,#139132,#139133,
#139134,#139135),.UNSPECIFIED.,.F.,.F.,(4,2,4),(-0.0253019896278924,-0.0126511156474334,
0.),.UNSPECIFIED.);
#23219=B_SPLINE_CURVE_WITH_KNOTS('',3,(#139160,#139161,#139162,#139163,
#139164,#139165,#139166),.UNSPECIFIED.,.F.,.F.,(4,3,4),(0.556108173865715,
0.558333952657055,0.568296447138361),.UNSPECIFIED.);
#23220=B_SPLINE_CURVE_WITH_KNOTS('',3,(#139167,#139168,#139169,#139170,
#139171,#139172),.UNSPECIFIED.,.F.,.F.,(4,2,4),(-0.025301989496816,-0.0126511156321275,
-2.29995258949067E-11),.UNSPECIFIED.);
#23221=B_SPLINE_CURVE_WITH_KNOTS('',3,(#139203,#139204,#139205,#139206,
#139207,#139208,#139209),.UNSPECIFIED.,.F.,.F.,(4,3,4),(0.556108173865715,
0.558333952657055,0.56829644715017),.UNSPECIFIED.);
#23222=B_SPLINE_CURVE_WITH_KNOTS('',3,(#139210,#139211,#139212,#139213,
#139214,#139215),.UNSPECIFIED.,.F.,.F.,(4,2,4),(-0.0253019895418659,-0.0126511156530789,
-2.9359289305253E-11),.UNSPECIFIED.);
#23223=B_SPLINE_CURVE_WITH_KNOTS('',3,(#139246,#139247,#139248,#139249,
#139250,#139251,#139252),.UNSPECIFIED.,.F.,.F.,(4,3,4),(0.556108173865715,
0.558333952657055,0.568296447135577),.UNSPECIFIED.);
#23224=B_SPLINE_CURVE_WITH_KNOTS('',3,(#139253,#139254,#139255,#139256,
#139257,#139258),.UNSPECIFIED.,.F.,.F.,(4,2,4),(-0.0253019895837948,-0.0126511156586353,
-1.96183694289864E-11),.UNSPECIFIED.);
#23225=B_SPLINE_CURVE_WITH_KNOTS('',3,(#139289,#139290,#139291,#139292,
#139293,#139294,#139295),.UNSPECIFIED.,.F.,.F.,(4,3,4),(0.556108173865715,
0.558333952657055,0.568296447140135),.UNSPECIFIED.);
#23226=B_SPLINE_CURVE_WITH_KNOTS('',3,(#139296,#139297,#139298,#139299,
#139300,#139301),.UNSPECIFIED.,.F.,.F.,(4,2,4),(-0.0253019895221298,-0.0126511156124946,
-2.86418840034219E-11),.UNSPECIFIED.);
#23227=B_SPLINE_CURVE_WITH_KNOTS('',3,(#139332,#139333,#139334,#139335,
#139336,#139337,#139338),.UNSPECIFIED.,.F.,.F.,(4,3,4),(0.556108173865715,
0.558333952657055,0.568296447141357),.UNSPECIFIED.);
#23228=B_SPLINE_CURVE_WITH_KNOTS('',3,(#139339,#139340,#139341,#139342,
#139343,#139344),.UNSPECIFIED.,.F.,.F.,(4,2,4),(-0.0253019896253231,-0.0126511157,
-2.89356767713134E-11),.UNSPECIFIED.);
#23229=B_SPLINE_CURVE_WITH_KNOTS('',3,(#139375,#139376,#139377,#139378,
#139379,#139380,#139381),.UNSPECIFIED.,.F.,.F.,(4,3,4),(0.556108173865716,
0.558333952657057,0.568296447129919),.UNSPECIFIED.);
#23230=B_SPLINE_CURVE_WITH_KNOTS('',3,(#139382,#139383,#139384,#139385,
#139386,#139387),.UNSPECIFIED.,.F.,.F.,(4,2,4),(-0.0253019895356154,-0.0126511156254898,
-2.51503019799149E-11),.UNSPECIFIED.);
#23231=B_SPLINE_CURVE_WITH_KNOTS('',3,(#139418,#139419,#139420,#139421,
#139422,#139423,#139424),.UNSPECIFIED.,.F.,.F.,(4,3,4),(0.556108173865715,
0.558333952657055,0.568296447143907),.UNSPECIFIED.);
#23232=B_SPLINE_CURVE_WITH_KNOTS('',3,(#139425,#139426,#139427,#139428,
#139429,#139430),.UNSPECIFIED.,.F.,.F.,(4,2,4),(-0.0253019895393503,-0.0126511156383291,
-2.10483228069158E-11),.UNSPECIFIED.);
#23233=B_SPLINE_CURVE_WITH_KNOTS('',3,(#139461,#139462,#139463,#139464,
#139465,#139466,#139467),.UNSPECIFIED.,.F.,.F.,(4,3,4),(0.556108173865715,
0.558333952657055,0.568296447145893),.UNSPECIFIED.);
#23234=B_SPLINE_CURVE_WITH_KNOTS('',3,(#139468,#139469,#139470,#139471,
#139472,#139473),.UNSPECIFIED.,.F.,.F.,(4,2,4),(-0.025301989566972,-0.0126511156375726,
-1.20351853483136E-11),.UNSPECIFIED.);
#23235=B_SPLINE_CURVE_WITH_KNOTS('',3,(#139504,#139505,#139506,#139507,
#139508,#139509,#139510),.UNSPECIFIED.,.F.,.F.,(4,3,4),(0.556108173865715,
0.558333952657055,0.568296447143574),.UNSPECIFIED.);
#23236=B_SPLINE_CURVE_WITH_KNOTS('',3,(#139511,#139512,#139513,#139514,
#139515,#139516),.UNSPECIFIED.,.F.,.F.,(4,2,4),(-0.0253019895694301,-0.0126511156503794,
-6.77978506669064E-12),.UNSPECIFIED.);
#23237=B_SPLINE_CURVE_WITH_KNOTS('',3,(#139547,#139548,#139549,#139550,
#139551,#139552,#139553),.UNSPECIFIED.,.F.,.F.,(4,3,4),(0.556108173865716,
0.558333952657056,0.56829644714022),.UNSPECIFIED.);
#23238=B_SPLINE_CURVE_WITH_KNOTS('',3,(#139554,#139555,#139556,#139557,
#139558,#139559),.UNSPECIFIED.,.F.,.F.,(4,2,4),(-0.0253019895254194,-0.0126511155865999,
-2.44209027999709E-11),.UNSPECIFIED.);
#23239=B_SPLINE_CURVE_WITH_KNOTS('',3,(#139590,#139591,#139592,#139593,
#139594,#139595,#139596),.UNSPECIFIED.,.F.,.F.,(4,3,4),(0.556108173865715,
0.558333952657055,0.568296447128213),.UNSPECIFIED.);
#23240=B_SPLINE_CURVE_WITH_KNOTS('',3,(#139597,#139598,#139599,#139600,
#139601,#139602),.UNSPECIFIED.,.F.,.F.,(4,2,4),(-0.0253019895140171,-0.0126511156345661,
-1.57640844822282E-11),.UNSPECIFIED.);
#23241=B_SPLINE_CURVE_WITH_KNOTS('',3,(#139633,#139634,#139635,#139636,
#139637,#139638,#139639),.UNSPECIFIED.,.F.,.F.,(4,3,4),(0.556108173865715,
0.558333952657071,0.56829644714659),.UNSPECIFIED.);
#23242=B_SPLINE_CURVE_WITH_KNOTS('',3,(#139640,#139641,#139642,#139643,
#139644,#139645),.UNSPECIFIED.,.F.,.F.,(4,2,4),(-0.0253019896200955,-0.0126511156782531,
-1.58387990223385E-11),.UNSPECIFIED.);
#23243=B_SPLINE_CURVE_WITH_KNOTS('',3,(#139676,#139677,#139678,#139679,
#139680,#139681,#139682),.UNSPECIFIED.,.F.,.F.,(4,3,4),(0.556108173865714,
0.558333952657053,0.568296447152951),.UNSPECIFIED.);
#23244=B_SPLINE_CURVE_WITH_KNOTS('',3,(#139683,#139684,#139685,#139686,
#139687,#139688),.UNSPECIFIED.,.F.,.F.,(4,2,4),(-0.0253019895367723,-0.0126511156270699,
-2.72321817873511E-11),.UNSPECIFIED.);
#23245=B_SPLINE_CURVE_WITH_KNOTS('',3,(#139719,#139720,#139721,#139722,
#139723,#139724,#139725),.UNSPECIFIED.,.F.,.F.,(4,3,4),(0.556108173865714,
0.558333952657053,0.568296447150853),.UNSPECIFIED.);
#23246=B_SPLINE_CURVE_WITH_KNOTS('',3,(#139726,#139727,#139728,#139729,
#139730,#139731),.UNSPECIFIED.,.F.,.F.,(4,2,4),(-0.0253019894899887,-0.012651115619704,
-1.88235260711878E-11),.UNSPECIFIED.);
#23247=B_SPLINE_CURVE_WITH_KNOTS('',3,(#139751,#139752,#139753,#139754,
#139755,#139756,#139757),.UNSPECIFIED.,.F.,.F.,(4,3,4),(0.556108173865714,
0.558333952657053,0.568296447114548),.UNSPECIFIED.);
#23248=B_SPLINE_CURVE_WITH_KNOTS('',3,(#139784,#139785,#139786,#139787,
#139788,#139789),.UNSPECIFIED.,.F.,.F.,(4,2,4),(-0.0253032195848505,-0.0126517291919461,
0.),.UNSPECIFIED.);
#23249=B_SPLINE_CURVE_WITH_KNOTS('',3,(#139798,#139799,#139800,#139801,
#139802,#139803),.UNSPECIFIED.,.F.,.F.,(4,2,4),(0.,0.0126517048550591,0.0253031720944598),
 .UNSPECIFIED.);
#23250=B_SPLINE_CURVE_WITH_KNOTS('',3,(#139823,#139824,#139825,#139826,
#139827,#139828),.UNSPECIFIED.,.F.,.F.,(4,2,4),(4.38171128399974E-11,0.0126517292144799,
0.0253032373814633),.UNSPECIFIED.);
#23251=B_SPLINE_CURVE_WITH_KNOTS('',3,(#139848,#139849,#139850,#139851,
#139852,#139853),.UNSPECIFIED.,.F.,.F.,(4,2,4),(3.57814230103522E-11,0.0126517292120754,
0.0253032358787696),.UNSPECIFIED.);
#23252=B_SPLINE_CURVE_WITH_KNOTS('',3,(#139873,#139874,#139875,#139876,
#139877,#139878),.UNSPECIFIED.,.F.,.F.,(4,2,4),(1.2439987344094E-11,0.0126517291603593,
0.0253032288431388),.UNSPECIFIED.);
#23253=B_SPLINE_CURVE_WITH_KNOTS('',3,(#139898,#139899,#139900,#139901,
#139902,#139903),.UNSPECIFIED.,.F.,.F.,(4,2,4),(0.,0.0126517046604698,0.0253031780482239),
 .UNSPECIFIED.);
#23254=B_SPLINE_CURVE_WITH_KNOTS('',3,(#139923,#139924,#139925,#139926,
#139927,#139928),.UNSPECIFIED.,.F.,.F.,(4,2,4),(0.,0.0126517291322339,0.025303231857666),
 .UNSPECIFIED.);
#23255=B_SPLINE_CURVE_WITH_KNOTS('',3,(#139948,#139949,#139950,#139951,
#139952,#139953),.UNSPECIFIED.,.F.,.F.,(4,2,4),(0.,0.0126517291489857,0.0253032322180855),
 .UNSPECIFIED.);
#23256=B_SPLINE_CURVE_WITH_KNOTS('',3,(#139973,#139974,#139975,#139976,
#139977,#139978),.UNSPECIFIED.,.F.,.F.,(4,2,4),(3.64720174388672E-11,0.0126517292140638,
0.0253032332575142),.UNSPECIFIED.);
#23257=B_SPLINE_CURVE_WITH_KNOTS('',3,(#139998,#139999,#140000,#140001,
#140002,#140003),.UNSPECIFIED.,.F.,.F.,(4,2,4),(0.,0.0126517291501688,0.0253032315632285),
 .UNSPECIFIED.);
#23258=B_SPLINE_CURVE_WITH_KNOTS('',3,(#140023,#140024,#140025,#140026,
#140027,#140028),.UNSPECIFIED.,.F.,.F.,(4,2,4),(4.98468781855941E-11,0.0126517292310175,
0.0253032323234676),.UNSPECIFIED.);
#23259=B_SPLINE_CURVE_WITH_KNOTS('',3,(#140048,#140049,#140050,#140051,
#140052,#140053),.UNSPECIFIED.,.F.,.F.,(4,2,4),(1.78170881484123E-11,0.0126517291939891,
0.0253032393088991),.UNSPECIFIED.);
#23260=B_SPLINE_CURVE_WITH_KNOTS('',3,(#140073,#140074,#140075,#140076,
#140077,#140078),.UNSPECIFIED.,.F.,.F.,(4,2,4),(0.,0.012651729151704,0.0253032336443197),
 .UNSPECIFIED.);
#23261=B_SPLINE_CURVE_WITH_KNOTS('',3,(#140098,#140099,#140100,#140101,
#140102,#140103),.UNSPECIFIED.,.F.,.F.,(4,2,4),(1.29662877955301E-11,0.0126517291972145,
0.0253032338446115),.UNSPECIFIED.);
#23262=B_SPLINE_CURVE_WITH_KNOTS('',3,(#140123,#140124,#140125,#140126,
#140127,#140128),.UNSPECIFIED.,.F.,.F.,(4,2,4),(1.06872879746175E-11,0.0126517291668657,
0.0253032367900497),.UNSPECIFIED.);
#23263=B_SPLINE_CURVE_WITH_KNOTS('',3,(#140148,#140149,#140150,#140151,
#140152,#140153),.UNSPECIFIED.,.F.,.F.,(4,2,4),(0.,0.0126517291525847,0.0253032326082015),
 .UNSPECIFIED.);
#23264=B_SPLINE_CURVE_WITH_KNOTS('',3,(#140173,#140174,#140175,#140176,
#140177,#140178),.UNSPECIFIED.,.F.,.F.,(4,2,4),(0.,0.0126517291593631,0.0253032317143608),
 .UNSPECIFIED.);
#23265=B_SPLINE_CURVE_WITH_KNOTS('',3,(#140198,#140199,#140200,#140201,
#140202,#140203),.UNSPECIFIED.,.F.,.F.,(4,2,4),(0.,0.0126517291345216,0.025303232365844),
 .UNSPECIFIED.);
#23266=B_SPLINE_CURVE_WITH_KNOTS('',3,(#140223,#140224,#140225,#140226,
#140227,#140228),.UNSPECIFIED.,.F.,.F.,(4,2,4),(2.76890456237896E-11,0.0126517291812319,
0.0253032339729562),.UNSPECIFIED.);
#23267=B_SPLINE_CURVE_WITH_KNOTS('',3,(#140248,#140249,#140250,#140251,
#140252,#140253),.UNSPECIFIED.,.F.,.F.,(4,2,4),(0.,0.012651729178449,0.0253032365218916),
 .UNSPECIFIED.);
#23268=B_SPLINE_CURVE_WITH_KNOTS('',3,(#140273,#140274,#140275,#140276,
#140277,#140278),.UNSPECIFIED.,.F.,.F.,(4,2,4),(0.,0.0126517291320085,0.025303230810267),
 .UNSPECIFIED.);
#23269=B_SPLINE_CURVE_WITH_KNOTS('',3,(#140298,#140299,#140300,#140301,
#140302,#140303),.UNSPECIFIED.,.F.,.F.,(4,2,4),(1.74085481906006E-11,0.0126517291619092,
0.0253032334768344),.UNSPECIFIED.);
#23270=B_SPLINE_CURVE_WITH_KNOTS('',3,(#140323,#140324,#140325,#140326,
#140327,#140328),.UNSPECIFIED.,.F.,.F.,(4,2,4),(0.,0.0126517291613853,0.0253032329245391),
 .UNSPECIFIED.);
#23271=B_SPLINE_CURVE_WITH_KNOTS('',3,(#140348,#140349,#140350,#140351,
#140352,#140353),.UNSPECIFIED.,.F.,.F.,(4,2,4),(1.10512950735125E-11,0.0126517291598583,
0.0253032349922658),.UNSPECIFIED.);
#23272=B_SPLINE_CURVE_WITH_KNOTS('',3,(#140373,#140374,#140375,#140376,
#140377,#140378),.UNSPECIFIED.,.F.,.F.,(4,2,4),(0.,0.0126517291624426,0.025303233284192),
 .UNSPECIFIED.);
#23273=B_SPLINE_CURVE_WITH_KNOTS('',3,(#140398,#140399,#140400,#140401,
#140402,#140403),.UNSPECIFIED.,.F.,.F.,(4,2,4),(3.26902022083678E-11,0.0126517291872101,
0.0253032306372425),.UNSPECIFIED.);
#23274=B_SPLINE_CURVE_WITH_KNOTS('',3,(#140423,#140424,#140425,#140426,
#140427,#140428),.UNSPECIFIED.,.F.,.F.,(4,2,4),(5.06203466173173E-11,0.0126517292236369,
0.0253032369878863),.UNSPECIFIED.);
#23275=B_SPLINE_CURVE_WITH_KNOTS('',3,(#140448,#140449,#140450,#140451,
#140452,#140453),.UNSPECIFIED.,.F.,.F.,(4,2,4),(1.01410125554829E-11,0.0126517291529624,
0.0253032321074454),.UNSPECIFIED.);
#23276=B_SPLINE_CURVE_WITH_KNOTS('',3,(#140473,#140474,#140475,#140476,
#140477,#140478),.UNSPECIFIED.,.F.,.F.,(4,2,4),(0.,0.0126517291283134,0.0253032314766247),
 .UNSPECIFIED.);
#23277=B_SPLINE_CURVE_WITH_KNOTS('',3,(#140508,#140509,#140510,#140511,
#140512,#140513),.UNSPECIFIED.,.F.,.F.,(4,2,4),(-0.0257915092833096,-0.0126485466669513,
-2.19810107615626E-11),.UNSPECIFIED.);
#23278=B_SPLINE_CURVE_WITH_KNOTS('',3,(#140527,#140528,#140529,#140530,
#140531,#140532),.UNSPECIFIED.,.F.,.F.,(4,2,4),(2.70362522355475E-11,0.0126485466623622,
0.0257911586180436),.UNSPECIFIED.);
#23279=B_SPLINE_CURVE_WITH_KNOTS('',3,(#140556,#140557,#140558,#140559,
#140560,#140561),.UNSPECIFIED.,.F.,.F.,(4,2,4),(1.43542774964306E-11,0.0126485466751825,
0.025791424513763),.UNSPECIFIED.);
#23280=B_SPLINE_CURVE_WITH_KNOTS('',3,(#140585,#140586,#140587,#140588,
#140589,#140590),.UNSPECIFIED.,.F.,.F.,(4,2,4),(6.79797826907082E-11,0.0126485467551672,
0.0257912698313032),.UNSPECIFIED.);
#23281=B_SPLINE_CURVE_WITH_KNOTS('',3,(#140614,#140615,#140616,#140617,
#140618,#140619),.UNSPECIFIED.,.F.,.F.,(4,2,4),(3.16048530260618E-11,0.0126485466866181,
0.0257913915485856),.UNSPECIFIED.);
#23282=B_SPLINE_CURVE_WITH_KNOTS('',3,(#140648,#140649,#140650,#140651,
#140652,#140653),.UNSPECIFIED.,.F.,.F.,(4,2,4),(2.60113353670021E-11,0.0126485466803885,
0.025791354907496),.UNSPECIFIED.);
#23283=B_SPLINE_CURVE_WITH_KNOTS('',3,(#140677,#140678,#140679,#140680,
#140681,#140682),.UNSPECIFIED.,.F.,.F.,(4,2,4),(5.48323673168424E-11,0.0126485466970084,
0.0257912960282793),.UNSPECIFIED.);
#23284=B_SPLINE_CURVE_WITH_KNOTS('',3,(#140706,#140707,#140708,#140709,
#140710,#140711),.UNSPECIFIED.,.F.,.F.,(4,2,4),(5.26304401860954E-11,0.0126485467607656,
0.0257913064734023),.UNSPECIFIED.);
#23285=B_SPLINE_CURVE_WITH_KNOTS('',3,(#140735,#140736,#140737,#140738,
#140739,#140740),.UNSPECIFIED.,.F.,.F.,(4,2,4),(3.13430767661628E-11,0.0126485466847367,
0.0257914462712551),.UNSPECIFIED.);
#23286=B_SPLINE_CURVE_WITH_KNOTS('',3,(#140764,#140765,#140766,#140767,
#140768,#140769),.UNSPECIFIED.,.F.,.F.,(4,2,4),(3.72919687755852E-11,0.0126485466486127,
0.0257915212993866),.UNSPECIFIED.);
#23287=B_SPLINE_CURVE_WITH_KNOTS('',3,(#140793,#140794,#140795,#140796,
#140797,#140798),.UNSPECIFIED.,.F.,.F.,(4,2,4),(3.33686758784895E-11,0.0126485466185285,
0.0257914200237712),.UNSPECIFIED.);
#23288=B_SPLINE_CURVE_WITH_KNOTS('',3,(#140822,#140823,#140824,#140825,
#140826,#140827),.UNSPECIFIED.,.F.,.F.,(4,2,4),(1.92687878762538E-11,0.0126485466368729,
0.0257914335980706),.UNSPECIFIED.);
#23289=B_SPLINE_CURVE_WITH_KNOTS('',3,(#140851,#140852,#140853,#140854,
#140855,#140856),.UNSPECIFIED.,.F.,.F.,(4,2,4),(2.44340999839289E-11,0.0126485466797976,
0.025791423235164),.UNSPECIFIED.);
#23290=B_SPLINE_CURVE_WITH_KNOTS('',3,(#140880,#140881,#140882,#140883,
#140884,#140885),.UNSPECIFIED.,.F.,.F.,(4,2,4),(5.66736717316295E-11,0.0126485467389853,
0.0257913878277949),.UNSPECIFIED.);
#23291=B_SPLINE_CURVE_WITH_KNOTS('',3,(#140914,#140915,#140916,#140917,
#140918,#140919),.UNSPECIFIED.,.F.,.F.,(4,2,4),(0.,0.012648546623643,0.0257912485305581),
 .UNSPECIFIED.);
#23292=B_SPLINE_CURVE_WITH_KNOTS('',3,(#140943,#140944,#140945,#140946,
#140947,#140948),.UNSPECIFIED.,.F.,.F.,(4,2,4),(5.37728797176222E-11,0.0126485467320549,
0.0257913769744669),.UNSPECIFIED.);
#23293=B_SPLINE_CURVE_WITH_KNOTS('',3,(#140972,#140973,#140974,#140975,
#140976,#140977),.UNSPECIFIED.,.F.,.F.,(4,2,4),(0.,0.0126485466447246,0.0257914432668697),
 .UNSPECIFIED.);
#23294=B_SPLINE_CURVE_WITH_KNOTS('',3,(#141001,#141002,#141003,#141004,
#141005,#141006),.UNSPECIFIED.,.F.,.F.,(4,2,4),(4.69338058508619E-11,0.0126485467018863,
0.0257913835745087),.UNSPECIFIED.);
#23295=B_SPLINE_CURVE_WITH_KNOTS('',3,(#141035,#141036,#141037,#141038,
#141039,#141040),.UNSPECIFIED.,.F.,.F.,(4,2,4),(2.38219565115975E-11,0.012648546654904,
0.0257914732516701),.UNSPECIFIED.);
#23296=B_SPLINE_CURVE_WITH_KNOTS('',3,(#141064,#141065,#141066,#141067,
#141068,#141069),.UNSPECIFIED.,.F.,.F.,(4,2,4),(2.97326209195323E-11,0.0126485466848618,
0.0257915677794139),.UNSPECIFIED.);
#23297=B_SPLINE_CURVE_WITH_KNOTS('',3,(#141093,#141094,#141095,#141096,
#141097,#141098),.UNSPECIFIED.,.F.,.F.,(4,2,4),(2.79225229640744E-11,0.0126485466708951,
0.0257914238548662),.UNSPECIFIED.);
#23298=B_SPLINE_CURVE_WITH_KNOTS('',3,(#141122,#141123,#141124,#141125,
#141126,#141127),.UNSPECIFIED.,.F.,.F.,(4,2,4),(1.32799613034488E-11,0.0126485465903112,
0.0257914139200059),.UNSPECIFIED.);
#23299=B_SPLINE_CURVE_WITH_KNOTS('',3,(#141151,#141152,#141153,#141154,
#141155,#141156),.UNSPECIFIED.,.F.,.F.,(4,2,4),(3.26716219031941E-11,0.0126485466900674,
0.025791388788007),.UNSPECIFIED.);
#23300=B_SPLINE_CURVE_WITH_KNOTS('',3,(#141180,#141181,#141182,#141183,
#141184,#141185),.UNSPECIFIED.,.F.,.F.,(4,2,4),(6.80582916254403E-11,0.0126485467142699,
0.0257914144991197),.UNSPECIFIED.);
#23301=B_SPLINE_CURVE_WITH_KNOTS('',3,(#141214,#141215,#141216,#141217,
#141218,#141219),.UNSPECIFIED.,.F.,.F.,(4,2,4),(4.44473432394692E-11,0.0126485466600686,
0.0257912643856431),.UNSPECIFIED.);
#23302=B_SPLINE_CURVE_WITH_KNOTS('',3,(#141248,#141249,#141250,#141251,
#141252,#141253),.UNSPECIFIED.,.F.,.F.,(4,2,4),(3.6215316177288E-11,0.0126485466901811,
0.0257914329539347),.UNSPECIFIED.);
#23303=B_SPLINE_CURVE_WITH_KNOTS('',3,(#141277,#141278,#141279,#141280,
#141281,#141282),.UNSPECIFIED.,.F.,.F.,(4,2,4),(2.63012159668852E-11,0.0126485466618793,
0.0257914669865645),.UNSPECIFIED.);
#23304=B_SPLINE_CURVE_WITH_KNOTS('',3,(#141306,#141307,#141308,#141309,
#141310,#141311),.UNSPECIFIED.,.F.,.F.,(4,2,4),(4.52322623488674E-11,0.0126485467153518,
0.0257913545346247),.UNSPECIFIED.);
#23305=B_SPLINE_CURVE_WITH_KNOTS('',3,(#141335,#141336,#141337,#141338,
#141339,#141340),.UNSPECIFIED.,.F.,.F.,(4,2,4),(4.14734752956722E-11,0.0126485466677345,
0.0257914043426878),.UNSPECIFIED.);
#23306=B_SPLINE_CURVE_WITH_KNOTS('',3,(#141377,#141378,#141379,#141380,
#141381,#141382),.UNSPECIFIED.,.F.,.F.,(4,2,4),(-0.0252997150098972,-0.0126500317843385,
-9.10712679921821E-9),.UNSPECIFIED.);
#23307=B_SPLINE_CURVE_WITH_KNOTS('',3,(#141410,#141411,#141412,#141413,
#141414,#141415),.UNSPECIFIED.,.F.,.F.,(4,2,4),(-0.0252993192639046,-0.0126498730539567,
-9.07035945657553E-9),.UNSPECIFIED.);
#23308=B_SPLINE_CURVE_WITH_KNOTS('',3,(#141443,#141444,#141445,#141446,
#141447,#141448),.UNSPECIFIED.,.F.,.F.,(4,2,4),(-0.0252993221176286,-0.0126498617303957,
-9.08144366998376E-9),.UNSPECIFIED.);
#23309=B_SPLINE_CURVE_WITH_KNOTS('',3,(#141476,#141477,#141478,#141479,
#141480,#141481),.UNSPECIFIED.,.F.,.F.,(4,2,4),(-0.025299328104327,-0.0126498714243405,
-9.07123582152836E-9),.UNSPECIFIED.);
#23310=B_SPLINE_CURVE_WITH_KNOTS('',3,(#141509,#141510,#141511,#141512,
#141513,#141514),.UNSPECIFIED.,.F.,.F.,(4,2,4),(-0.025299338488532,-0.0126498691500846,
-9.07425860494082E-9),.UNSPECIFIED.);
#23311=B_SPLINE_CURVE_WITH_KNOTS('',3,(#141542,#141543,#141544,#141545,
#141546,#141547),.UNSPECIFIED.,.F.,.F.,(4,2,4),(-0.0252997272114458,-0.0126500317748764,
-9.10567698325648E-9),.UNSPECIFIED.);
#23312=B_SPLINE_CURVE_WITH_KNOTS('',3,(#141575,#141576,#141577,#141578,
#141579,#141580),.UNSPECIFIED.,.F.,.F.,(4,2,4),(-0.0252993471269051,-0.01264987588227,
-9.06701983285907E-9),.UNSPECIFIED.);
#23313=B_SPLINE_CURVE_WITH_KNOTS('',3,(#141608,#141609,#141610,#141611,
#141612,#141613),.UNSPECIFIED.,.F.,.F.,(4,2,4),(-0.0252993194291543,-0.0126498641945722,
-9.07929462515278E-9),.UNSPECIFIED.);
#23314=B_SPLINE_CURVE_WITH_KNOTS('',3,(#141641,#141642,#141643,#141644,
#141645,#141646),.UNSPECIFIED.,.F.,.F.,(4,2,4),(-0.0252993149765833,-0.0126498658638244,
-9.07693491550288E-9),.UNSPECIFIED.);
#23315=B_SPLINE_CURVE_WITH_KNOTS('',3,(#141674,#141675,#141676,#141677,
#141678,#141679),.UNSPECIFIED.,.F.,.F.,(4,2,4),(-0.0252997346785984,-0.0126500317266587,
-9.10414309565621E-9),.UNSPECIFIED.);
#23316=B_SPLINE_CURVE_WITH_KNOTS('',3,(#141707,#141708,#141709,#141710,
#141711,#141712),.UNSPECIFIED.,.F.,.F.,(4,2,4),(-0.0252993458238753,-0.0126498773505181,
-9.0656312422277E-9),.UNSPECIFIED.);
#23317=B_SPLINE_CURVE_WITH_KNOTS('',3,(#141740,#141741,#141742,#141743,
#141744,#141745),.UNSPECIFIED.,.F.,.F.,(4,2,4),(-0.0252993101823874,-0.0126498642958816,
-9.07914507464191E-9),.UNSPECIFIED.);
#23318=B_SPLINE_CURVE_WITH_KNOTS('',3,(#141773,#141774,#141775,#141776,
#141777,#141778),.UNSPECIFIED.,.F.,.F.,(4,2,4),(-0.0252993301983058,-0.0126498632692199,
-9.07977696154583E-9),.UNSPECIFIED.);
#23319=B_SPLINE_CURVE_WITH_KNOTS('',3,(#141806,#141807,#141808,#141809,
#141810,#141811),.UNSPECIFIED.,.F.,.F.,(4,2,4),(-0.0252993173610177,-0.012649865812899,
-9.07689320581162E-9),.UNSPECIFIED.);
#23320=B_SPLINE_CURVE_WITH_KNOTS('',3,(#141836,#141837,#141838,#141839,
#141840,#141841),.UNSPECIFIED.,.F.,.F.,(4,2,4),(-0.0252993161138789,-0.0126498661496497,
-9.07674461980701E-9),.UNSPECIFIED.);
#23321=B_SPLINE_CURVE_WITH_KNOTS('',3,(#141863,#141864,#141865,#141866,
#141867,#141868),.UNSPECIFIED.,.F.,.F.,(4,2,4),(-0.0252997344586295,-0.0126500317232582,
-9.10763827896566E-9),.UNSPECIFIED.);
#23322=B_SPLINE_CURVE_WITH_KNOTS('',3,(#141896,#141897,#141898,#141899,
#141900,#141901),.UNSPECIFIED.,.F.,.F.,(4,2,4),(-0.0252993204603601,-0.0126498639881955,
-9.07887972440014E-9),.UNSPECIFIED.);
#23323=B_SPLINE_CURVE_WITH_KNOTS('',3,(#141929,#141930,#141931,#141932,
#141933,#141934),.UNSPECIFIED.,.F.,.F.,(4,2,4),(-0.0252993253610345,-0.012649862213264,
-9.08052791293024E-9),.UNSPECIFIED.);
#23324=B_SPLINE_CURVE_WITH_KNOTS('',3,(#141962,#141963,#141964,#141965,
#141966,#141967),.UNSPECIFIED.,.F.,.F.,(4,2,4),(-0.0252992970947547,-0.0126498664943603,
-9.07626198851097E-9),.UNSPECIFIED.);
#23325=B_SPLINE_CURVE_WITH_KNOTS('',3,(#141995,#141996,#141997,#141998,
#141999,#142000),.UNSPECIFIED.,.F.,.F.,(4,2,4),(-0.0252992902045865,-0.0126498538085401,
-9.05754709082385E-9),.UNSPECIFIED.);
#23326=B_SPLINE_CURVE_WITH_KNOTS('',3,(#142029,#142030,#142031,#142032,
#142033,#142034),.UNSPECIFIED.,.F.,.F.,(4,2,4),(-0.025299728807157,-0.0126500317762664,
-9.11489488747419E-9),.UNSPECIFIED.);
#23327=B_SPLINE_CURVE_WITH_KNOTS('',3,(#142061,#142062,#142063,#142064,
#142065,#142066),.UNSPECIFIED.,.F.,.F.,(4,2,4),(-0.0252993271765603,-0.0126498623727777,
-9.0807460960407E-9),.UNSPECIFIED.);
#23328=B_SPLINE_CURVE_WITH_KNOTS('',3,(#142094,#142095,#142096,#142097,
#142098,#142099),.UNSPECIFIED.,.F.,.F.,(4,2,4),(-0.0252997271572641,-0.0126500317584131,
-9.10477810159294E-9),.UNSPECIFIED.);
#23329=B_SPLINE_CURVE_WITH_KNOTS('',3,(#142127,#142128,#142129,#142130,
#142131,#142132),.UNSPECIFIED.,.F.,.F.,(4,2,4),(-0.0252993045945163,-0.0126498634942832,
-9.07959531518121E-9),.UNSPECIFIED.);
#23330=B_SPLINE_CURVE_WITH_KNOTS('',3,(#142160,#142161,#142162,#142163,
#142164,#142165),.UNSPECIFIED.,.F.,.F.,(4,2,4),(-0.0252993278041195,-0.0126498659235352,
-9.07719203621649E-9),.UNSPECIFIED.);
#23331=B_SPLINE_CURVE_WITH_KNOTS('',3,(#142193,#142194,#142195,#142196,
#142197,#142198),.UNSPECIFIED.,.F.,.F.,(4,2,4),(-0.0252993190119561,-0.0126498640052631,
-9.0793093460162E-9),.UNSPECIFIED.);
#23332=B_SPLINE_CURVE_WITH_KNOTS('',3,(#142226,#142227,#142228,#142229,
#142230,#142231),.UNSPECIFIED.,.F.,.F.,(4,2,4),(-0.0252993234646114,-0.0126498667429259,
-9.07600854194168E-9),.UNSPECIFIED.);
#23333=B_SPLINE_CURVE_WITH_KNOTS('',3,(#142259,#142260,#142261,#142262,
#142263,#142264),.UNSPECIFIED.,.F.,.F.,(4,2,4),(-0.0252997144599162,-0.012650031762626,
-9.10456312425145E-9),.UNSPECIFIED.);
#23334=B_SPLINE_CURVE_WITH_KNOTS('',3,(#142292,#142293,#142294,#142295,
#142296,#142297),.UNSPECIFIED.,.F.,.F.,(4,2,4),(-0.0252993049756229,-0.0126498626584025,
-9.0801991724232E-9),.UNSPECIFIED.);
#23335=B_SPLINE_CURVE_WITH_KNOTS('',3,(#142330,#142331,#142332,#142333,
#142334,#142335),.UNSPECIFIED.,.F.,.F.,(4,2,4),(0.,0.0126483033528629,0.0252967254469703),
 .UNSPECIFIED.);
#23336=B_SPLINE_CURVE_WITH_KNOTS('',3,(#142371,#142372,#142373,#142374,
#142375,#142376),.UNSPECIFIED.,.F.,.F.,(4,2,4),(0.,0.0126483617678804,0.0252969654295701),
 .UNSPECIFIED.);
#23337=B_SPLINE_CURVE_WITH_KNOTS('',3,(#142412,#142413,#142414,#142415,
#142416,#142417),.UNSPECIFIED.,.F.,.F.,(4,2,4),(0.,0.0126482976272339,0.0252967020886337),
 .UNSPECIFIED.);
#23338=B_SPLINE_CURVE_WITH_KNOTS('',3,(#142453,#142454,#142455,#142456,
#142457,#142458),.UNSPECIFIED.,.F.,.F.,(4,2,4),(0.,0.0126483617612936,0.0252969765449637),
 .UNSPECIFIED.);
#23339=B_SPLINE_CURVE_WITH_KNOTS('',3,(#142494,#142495,#142496,#142497,
#142498,#142499),.UNSPECIFIED.,.F.,.F.,(4,2,4),(0.,0.0126483617791059,0.0252969761281077),
 .UNSPECIFIED.);
#23340=B_SPLINE_CURVE_WITH_KNOTS('',3,(#142535,#142536,#142537,#142538,
#142539,#142540),.UNSPECIFIED.,.F.,.F.,(4,2,4),(0.,0.0126483617559022,0.0252969652965633),
 .UNSPECIFIED.);
#23341=B_SPLINE_CURVE_WITH_KNOTS('',3,(#142576,#142577,#142578,#142579,
#142580,#142581),.UNSPECIFIED.,.F.,.F.,(4,2,4),(0.,0.0126483052677277,0.0252967333732343),
 .UNSPECIFIED.);
#23342=B_SPLINE_CURVE_WITH_KNOTS('',3,(#142617,#142618,#142619,#142620,
#142621,#142622),.UNSPECIFIED.,.F.,.F.,(4,2,4),(0.,0.0126482994530337,0.0252967093118385),
 .UNSPECIFIED.);
#23343=B_SPLINE_CURVE_WITH_KNOTS('',3,(#142658,#142659,#142660,#142661,
#142662,#142663),.UNSPECIFIED.,.F.,.F.,(4,2,4),(0.,0.0126483617643872,0.0252969765390469),
 .UNSPECIFIED.);
#23344=B_SPLINE_CURVE_WITH_KNOTS('',3,(#142699,#142700,#142701,#142702,
#142703,#142704),.UNSPECIFIED.,.F.,.F.,(4,2,4),(0.,0.0126482983272483,0.0252967047813038),
 .UNSPECIFIED.);
#23345=B_SPLINE_CURVE_WITH_KNOTS('',3,(#142740,#142741,#142742,#142743,
#142744,#142745),.UNSPECIFIED.,.F.,.F.,(4,2,4),(0.,0.0126483000717647,0.0252967121149593),
 .UNSPECIFIED.);
#23346=B_SPLINE_CURVE_WITH_KNOTS('',3,(#142781,#142782,#142783,#142784,
#142785,#142786),.UNSPECIFIED.,.F.,.F.,(4,2,4),(0.,0.0126483617690835,0.0252969653140276),
 .UNSPECIFIED.);
#23347=B_SPLINE_CURVE_WITH_KNOTS('',3,(#142822,#142823,#142824,#142825,
#142826,#142827),.UNSPECIFIED.,.F.,.F.,(4,2,4),(2.42740058061956E-11,0.0126483617583391,
0.0252969653213079),.UNSPECIFIED.);
#23348=B_SPLINE_CURVE_WITH_KNOTS('',3,(#142863,#142864,#142865,#142866,
#142867,#142868),.UNSPECIFIED.,.F.,.F.,(4,2,4),(0.,0.0126483617625851,0.0252969737117307),
 .UNSPECIFIED.);
#23349=B_SPLINE_CURVE_WITH_KNOTS('',3,(#142904,#142905,#142906,#142907,
#142908,#142909),.UNSPECIFIED.,.F.,.F.,(4,2,4),(0.,0.0126483617752743,0.0252969768202461),
 .UNSPECIFIED.);
#23350=B_SPLINE_CURVE_WITH_KNOTS('',3,(#142945,#142946,#142947,#142948,
#142949,#142950),.UNSPECIFIED.,.F.,.F.,(4,2,4),(0.,0.0126483617401393,0.025296965465005),
 .UNSPECIFIED.);
#23351=B_SPLINE_CURVE_WITH_KNOTS('',3,(#142986,#142987,#142988,#142989,
#142990,#142991),.UNSPECIFIED.,.F.,.F.,(4,2,4),(0.,0.012648298093685,0.0252967038543137),
 .UNSPECIFIED.);
#23352=B_SPLINE_CURVE_WITH_KNOTS('',3,(#143027,#143028,#143029,#143030,
#143031,#143032),.UNSPECIFIED.,.F.,.F.,(4,2,4),(0.,0.0126483024110683,0.0252967329236766),
 .UNSPECIFIED.);
#23353=B_SPLINE_CURVE_WITH_KNOTS('',3,(#143068,#143069,#143070,#143071,
#143072,#143073),.UNSPECIFIED.,.F.,.F.,(4,2,4),(1.9407486965572E-11,0.0126483617769253,
0.0252969745847458),.UNSPECIFIED.);
#23354=B_SPLINE_CURVE_WITH_KNOTS('',3,(#143109,#143110,#143111,#143112,
#143113,#143114),.UNSPECIFIED.,.F.,.F.,(4,2,4),(3.3601607052622E-11,0.012648308385465,
0.0252967460828744),.UNSPECIFIED.);
#23355=B_SPLINE_CURVE_WITH_KNOTS('',3,(#143150,#143151,#143152,#143153,
#143154,#143155),.UNSPECIFIED.,.F.,.F.,(4,2,4),(0.,0.0126483007561831,0.0252967254663462),
 .UNSPECIFIED.);
#23356=B_SPLINE_CURVE_WITH_KNOTS('',3,(#143188,#143189,#143190,#143191,
#143192,#143193),.UNSPECIFIED.,.F.,.F.,(4,2,4),(0.,0.0126482990716502,0.0252967077163187),
 .UNSPECIFIED.);
#23357=B_SPLINE_CURVE_WITH_KNOTS('',3,(#143223,#143224,#143225,#143226,
#143227,#143228),.UNSPECIFIED.,.F.,.F.,(4,2,4),(4.24920173066688E-11,0.0126483000002919,
0.025296722178295),.UNSPECIFIED.);
#23358=B_SPLINE_CURVE_WITH_KNOTS('',3,(#143264,#143265,#143266,#143267,
#143268,#143269),.UNSPECIFIED.,.F.,.F.,(4,2,4),(0.,0.0126482982349249,0.0252967043333024),
 .UNSPECIFIED.);
#23359=B_SPLINE_CURVE_WITH_KNOTS('',3,(#143305,#143306,#143307,#143308,
#143309,#143310),.UNSPECIFIED.,.F.,.F.,(4,2,4),(0.,0.0126483617896171,0.025296965364044),
 .UNSPECIFIED.);
#23360=B_SPLINE_CURVE_WITH_KNOTS('',3,(#143346,#143347,#143348,#143349,
#143350,#143351),.UNSPECIFIED.,.F.,.F.,(4,2,4),(0.,0.0126483617446494,0.0252969654514837),
 .UNSPECIFIED.);
#23361=B_SPLINE_CURVE_WITH_KNOTS('',3,(#143387,#143388,#143389,#143390,
#143391,#143392),.UNSPECIFIED.,.F.,.F.,(4,2,4),(0.,0.01264836176774,0.0252969653009797),
 .UNSPECIFIED.);
#23362=B_SPLINE_CURVE_WITH_KNOTS('',3,(#143428,#143429,#143430,#143431,
#143432,#143433),.UNSPECIFIED.,.F.,.F.,(4,2,4),(0.,0.012648361762527,0.0252969743405282),
 .UNSPECIFIED.);
#23363=B_SPLINE_CURVE_WITH_KNOTS('',3,(#143469,#143470,#143471,#143472,
#143473,#143474),.UNSPECIFIED.,.F.,.F.,(4,2,4),(3.26919061841809E-11,0.0126483617530401,
0.025296965503827),.UNSPECIFIED.);
#23364=B_SPLINE_CURVE_WITH_KNOTS('',3,(#143504,#143505,#143506,#143507,
#143508,#143509),.UNSPECIFIED.,.F.,.F.,(4,2,4),(-0.0253036322111694,-0.0126517037466635,
-1.82800663495186E-10),.UNSPECIFIED.);
#23365=B_SPLINE_CURVE_WITH_KNOTS('',3,(#143529,#143530,#143531,#143532,
#143533,#143534),.UNSPECIFIED.,.F.,.F.,(4,2,4),(-0.0253032917436892,-0.0126516212476504,
-6.7092234545818E-12),.UNSPECIFIED.);
#23366=B_SPLINE_CURVE_WITH_KNOTS('',3,(#143554,#143555,#143556,#143557,
#143558,#143559),.UNSPECIFIED.,.F.,.F.,(4,2,4),(-0.0253036321774632,-0.0126517036083302,
-2.09170042397844E-11),.UNSPECIFIED.);
#23367=B_SPLINE_CURVE_WITH_KNOTS('',3,(#143579,#143580,#143581,#143582,
#143583,#143584),.UNSPECIFIED.,.F.,.F.,(4,2,4),(-0.0253036321684814,-0.0126517036417179,
-1.15808182488131E-10),.UNSPECIFIED.);
#23368=B_SPLINE_CURVE_WITH_KNOTS('',3,(#143604,#143605,#143606,#143607,
#143608,#143609),.UNSPECIFIED.,.F.,.F.,(4,2,4),(-0.0253036321869942,-0.0126517036462115,
-1.10797839653065E-10),.UNSPECIFIED.);
#23369=B_SPLINE_CURVE_WITH_KNOTS('',3,(#143629,#143630,#143631,#143632,
#143633,#143634),.UNSPECIFIED.,.F.,.F.,(4,2,4),(-0.0253036322201411,-0.0126517037535042,
-1.90251512460771E-10),.UNSPECIFIED.);
#23370=B_SPLINE_CURVE_WITH_KNOTS('',3,(#143654,#143655,#143656,#143657,
#143658,#143659),.UNSPECIFIED.,.F.,.F.,(4,2,4),(-0.0253036322061587,-0.0126517037427219,
-1.93522909502919E-10),.UNSPECIFIED.);
#23371=B_SPLINE_CURVE_WITH_KNOTS('',3,(#143679,#143680,#143681,#143682,
#143683,#143684),.UNSPECIFIED.,.F.,.F.,(4,2,4),(-0.0253036321241486,-0.0126517036041792,
-9.10544729892937E-11),.UNSPECIFIED.);
#23372=B_SPLINE_CURVE_WITH_KNOTS('',3,(#143704,#143705,#143706,#143707,
#143708,#143709),.UNSPECIFIED.,.F.,.F.,(4,2,4),(-0.0253032837977553,-0.0126516193848244,
-1.11454907802955E-10),.UNSPECIFIED.);
#23373=B_SPLINE_CURVE_WITH_KNOTS('',3,(#143729,#143730,#143731,#143732,
#143733,#143734),.UNSPECIFIED.,.F.,.F.,(4,2,4),(-0.0253032936362909,-0.0126516217100339,
-6.41719316574196E-12),.UNSPECIFIED.);
#23374=B_SPLINE_CURVE_WITH_KNOTS('',3,(#143754,#143755,#143756,#143757,
#143758,#143759),.UNSPECIFIED.,.F.,.F.,(4,2,4),(-0.0253036321434187,-0.0126517035746939,
0.),.UNSPECIFIED.);
#23375=B_SPLINE_CURVE_WITH_KNOTS('',3,(#143779,#143780,#143781,#143782,
#143783,#143784),.UNSPECIFIED.,.F.,.F.,(4,2,4),(-0.0253032880541102,-0.0126516204139794,
-1.41031603062558E-10),.UNSPECIFIED.);
#23376=B_SPLINE_CURVE_WITH_KNOTS('',3,(#143804,#143805,#143806,#143807,
#143808,#143809),.UNSPECIFIED.,.F.,.F.,(4,2,4),(-0.0253036322200184,-0.0126517036652856,
-4.99830593581052E-11),.UNSPECIFIED.);
#23377=B_SPLINE_CURVE_WITH_KNOTS('',3,(#143829,#143830,#143831,#143832,
#143833,#143834),.UNSPECIFIED.,.F.,.F.,(4,2,4),(-0.0253036322039681,-0.012651703705871,
-1.54916319355936E-10),.UNSPECIFIED.);
#23378=B_SPLINE_CURVE_WITH_KNOTS('',3,(#143854,#143855,#143856,#143857,
#143858,#143859),.UNSPECIFIED.,.F.,.F.,(4,2,4),(-0.0253036299712287,-0.0126517025076815,
-2.78628856098528E-12),.UNSPECIFIED.);
#23379=B_SPLINE_CURVE_WITH_KNOTS('',3,(#143879,#143880,#143881,#143882,
#143883,#143884),.UNSPECIFIED.,.F.,.F.,(4,2,4),(-0.0253032960389127,-0.0126516223592375,
-1.19824782041089E-10),.UNSPECIFIED.);
#23380=B_SPLINE_CURVE_WITH_KNOTS('',3,(#143904,#143905,#143906,#143907,
#143908,#143909),.UNSPECIFIED.,.F.,.F.,(4,2,4),(-0.0253032498580712,-0.0126516111196444,
0.),.UNSPECIFIED.);
#23381=B_SPLINE_CURVE_WITH_KNOTS('',3,(#143929,#143930,#143931,#143932,
#143933,#143934),.UNSPECIFIED.,.F.,.F.,(4,2,4),(-0.0253032543198873,-0.012651612194739,
0.),.UNSPECIFIED.);
#23382=B_SPLINE_CURVE_WITH_KNOTS('',3,(#143954,#143955,#143956,#143957,
#143958,#143959),.UNSPECIFIED.,.F.,.F.,(4,2,4),(-0.0253036321462399,-0.0126517035856047,
-7.17744960687661E-12),.UNSPECIFIED.);
#23383=B_SPLINE_CURVE_WITH_KNOTS('',3,(#143979,#143980,#143981,#143982,
#143983,#143984),.UNSPECIFIED.,.F.,.F.,(4,2,4),(-0.0253032981944482,-0.0126516228680173,
-1.27145845935095E-10),.UNSPECIFIED.);
#23384=B_SPLINE_CURVE_WITH_KNOTS('',3,(#144004,#144005,#144006,#144007,
#144008,#144009),.UNSPECIFIED.,.F.,.F.,(4,2,4),(-0.0253032720073819,-0.0126516164724433,
0.),.UNSPECIFIED.);
#23385=B_SPLINE_CURVE_WITH_KNOTS('',3,(#144029,#144030,#144031,#144032,
#144033,#144034),.UNSPECIFIED.,.F.,.F.,(4,2,4),(-0.025303632136923,-0.012651703583944,
-8.44966457913543E-12),.UNSPECIFIED.);
#23386=B_SPLINE_CURVE_WITH_KNOTS('',3,(#144054,#144055,#144056,#144057,
#144058,#144059),.UNSPECIFIED.,.F.,.F.,(4,2,4),(-0.0253036321454915,-0.0126517036104632,
-1.04495596203735E-10),.UNSPECIFIED.);
#23387=B_SPLINE_CURVE_WITH_KNOTS('',3,(#144079,#144080,#144081,#144082,
#144083,#144084),.UNSPECIFIED.,.F.,.F.,(4,2,4),(-0.0253036321600805,-0.0126517035775229,
0.),.UNSPECIFIED.);
#23388=B_SPLINE_CURVE_WITH_KNOTS('',3,(#144104,#144105,#144106,#144107,
#144108,#144109),.UNSPECIFIED.,.F.,.F.,(4,2,4),(-0.0253036321591695,-0.0126517036265382,
-2.34760544337576E-11),.UNSPECIFIED.);
#23389=B_SPLINE_CURVE_WITH_KNOTS('',3,(#144129,#144130,#144131,#144132,
#144133,#144134),.UNSPECIFIED.,.F.,.F.,(4,2,4),(-0.0253036322011602,-0.0126517037454701,
-1.96367942739695E-10),.UNSPECIFIED.);
#23390=B_SPLINE_CURVE_WITH_KNOTS('',3,(#144154,#144155,#144156,#144157,
#144158,#144159),.UNSPECIFIED.,.F.,.F.,(4,2,4),(-0.0253036321964258,-0.0126517036155337,
-2.2322820675269E-11),.UNSPECIFIED.);
#23391=B_SPLINE_CURVE_WITH_KNOTS('',3,(#144179,#144180,#144181,#144182,
#144183,#144184),.UNSPECIFIED.,.F.,.F.,(4,2,4),(-0.0253032929844905,-0.0126516215735631,
-3.93026722278478E-11),.UNSPECIFIED.);
#23392=B_SPLINE_CURVE_WITH_KNOTS('',3,(#144204,#144205,#144206,#144207,
#144208,#144209),.UNSPECIFIED.,.F.,.F.,(4,2,4),(-0.0253036321980525,-0.0126517036572632,
-4.59963178656153E-11),.UNSPECIFIED.);
#23393=B_SPLINE_CURVE_WITH_KNOTS('',3,(#144229,#144230,#144231,#144232,
#144233,#144234),.UNSPECIFIED.,.F.,.F.,(4,2,4),(-0.0253028607889791,-0.0126513115894774,
-1.43257597451374E-9),.UNSPECIFIED.);
#23394=B_SPLINE_CURVE_WITH_KNOTS('',3,(#144250,#144251,#144252,#144253,
#144254,#144255),.UNSPECIFIED.,.F.,.F.,(4,2,4),(-0.0253028678808171,-0.0126513117178962,
-1.53780291972661E-9),.UNSPECIFIED.);
#23395=B_SPLINE_CURVE_WITH_KNOTS('',3,(#144271,#144272,#144273,#144274,
#144275,#144276),.UNSPECIFIED.,.F.,.F.,(4,2,4),(-0.0253028686448891,-0.012651311734525,
-1.57900790706544E-9),.UNSPECIFIED.);
#23396=B_SPLINE_CURVE_WITH_KNOTS('',3,(#144292,#144293,#144294,#144295,
#144296,#144297),.UNSPECIFIED.,.F.,.F.,(4,2,4),(-0.0253028608314155,-0.0126513117590326,
-1.57566134445508E-9),.UNSPECIFIED.);
#23397=B_SPLINE_CURVE_WITH_KNOTS('',3,(#144313,#144314,#144315,#144316,
#144317,#144318),.UNSPECIFIED.,.F.,.F.,(4,2,4),(-0.0253028679915641,-0.0126513116532287,
-1.47354626417462E-9),.UNSPECIFIED.);
#23398=B_SPLINE_CURVE_WITH_KNOTS('',3,(#144334,#144335,#144336,#144337,
#144338,#144339),.UNSPECIFIED.,.F.,.F.,(4,2,4),(-0.0253028685599515,-0.0126513116039704,
-1.43719535231068E-9),.UNSPECIFIED.);
#23399=B_SPLINE_CURVE_WITH_KNOTS('',3,(#144355,#144356,#144357,#144358,
#144359,#144360),.UNSPECIFIED.,.F.,.F.,(4,2,4),(-0.0253028676392111,-0.0126513116536948,
-1.4995063558898E-9),.UNSPECIFIED.);
#23400=B_SPLINE_CURVE_WITH_KNOTS('',3,(#144376,#144377,#144378,#144379,
#144380,#144381),.UNSPECIFIED.,.F.,.F.,(4,2,4),(-0.0253028684857489,-0.0126513116569664,
-1.46742496279217E-9),.UNSPECIFIED.);
#23401=B_SPLINE_CURVE_WITH_KNOTS('',3,(#144397,#144398,#144399,#144400,
#144401,#144402),.UNSPECIFIED.,.F.,.F.,(4,2,4),(-0.0253028680664795,-0.0126513116285446,
-1.47392072158414E-9),.UNSPECIFIED.);
#23402=B_SPLINE_CURVE_WITH_KNOTS('',3,(#144418,#144419,#144420,#144421,
#144422,#144423),.UNSPECIFIED.,.F.,.F.,(4,2,4),(-0.0253028674744424,-0.0126513116179339,
-1.4976289791635E-9),.UNSPECIFIED.);
#23403=B_SPLINE_CURVE_WITH_KNOTS('',3,(#144439,#144440,#144441,#144442,
#144443,#144444),.UNSPECIFIED.,.F.,.F.,(4,2,4),(-0.0253028608153995,-0.012651311643751,
-1.49117444087077E-9),.UNSPECIFIED.);
#23404=B_SPLINE_CURVE_WITH_KNOTS('',3,(#144460,#144461,#144462,#144463,
#144464,#144465),.UNSPECIFIED.,.F.,.F.,(4,2,4),(-0.0253028688025471,-0.012651311694285,
-1.5592264354658E-9),.UNSPECIFIED.);
#23405=B_SPLINE_CURVE_WITH_KNOTS('',3,(#144481,#144482,#144483,#144484,
#144485,#144486),.UNSPECIFIED.,.F.,.F.,(4,2,4),(-0.0253028685614985,-0.0126513116925499,
-1.51033512779675E-9),.UNSPECIFIED.);
#23406=B_SPLINE_CURVE_WITH_KNOTS('',3,(#144502,#144503,#144504,#144505,
#144506,#144507),.UNSPECIFIED.,.F.,.F.,(4,2,4),(-0.0253028684579291,-0.0126513116076864,
-1.46460564856565E-9),.UNSPECIFIED.);
#23407=B_SPLINE_CURVE_WITH_KNOTS('',3,(#144523,#144524,#144525,#144526,
#144527,#144528),.UNSPECIFIED.,.F.,.F.,(4,2,4),(-0.0253028607761515,-0.0126513116250043,
-1.47685470450187E-9),.UNSPECIFIED.);
#23408=B_SPLINE_CURVE_WITH_KNOTS('',3,(#144544,#144545,#144546,#144547,
#144548,#144549),.UNSPECIFIED.,.F.,.F.,(4,2,4),(-0.0253028685031401,-0.0126513115444502,
-1.40921434937935E-9),.UNSPECIFIED.);
#23409=B_SPLINE_CURVE_WITH_KNOTS('',3,(#144565,#144566,#144567,#144568,
#144569,#144570),.UNSPECIFIED.,.F.,.F.,(4,2,4),(-0.0253028690751082,-0.0126513117151343,
-1.54119479678361E-9),.UNSPECIFIED.);
#23410=B_SPLINE_CURVE_WITH_KNOTS('',3,(#144586,#144587,#144588,#144589,
#144590,#144591),.UNSPECIFIED.,.F.,.F.,(4,2,4),(-0.0253028693983055,-0.0126513115448918,
-1.40235656073684E-9),.UNSPECIFIED.);
#23411=B_SPLINE_CURVE_WITH_KNOTS('',3,(#144607,#144608,#144609,#144610,
#144611,#144612),.UNSPECIFIED.,.F.,.F.,(4,2,4),(-0.0253028676030852,-0.0126513117658921,
-1.59613115432999E-9),.UNSPECIFIED.);
#23412=B_SPLINE_CURVE_WITH_KNOTS('',3,(#144628,#144629,#144630,#144631,
#144632,#144633),.UNSPECIFIED.,.F.,.F.,(4,2,4),(-0.0253028678921412,-0.0126513117315833,
-1.53634311175765E-9),.UNSPECIFIED.);
#23413=B_SPLINE_CURVE_WITH_KNOTS('',3,(#144649,#144650,#144651,#144652,
#144653,#144654),.UNSPECIFIED.,.F.,.F.,(4,2,4),(-0.0253028607407018,-0.0126513115927762,
-1.45961178560361E-9),.UNSPECIFIED.);
#23414=B_SPLINE_CURVE_WITH_KNOTS('',3,(#144670,#144671,#144672,#144673,
#144674,#144675),.UNSPECIFIED.,.F.,.F.,(4,2,4),(-0.0253028677288099,-0.0126513116203026,
-1.49586819667147E-9),.UNSPECIFIED.);
#23415=B_SPLINE_CURVE_WITH_KNOTS('',3,(#144691,#144692,#144693,#144694,
#144695,#144696),.UNSPECIFIED.,.F.,.F.,(4,2,4),(-0.0253028677262056,-0.0126513116265939,
-1.50229979151151E-9),.UNSPECIFIED.);
#23416=B_SPLINE_CURVE_WITH_KNOTS('',3,(#144712,#144713,#144714,#144715,
#144716,#144717),.UNSPECIFIED.,.F.,.F.,(4,2,4),(-0.0253028607760877,-0.0126513115295272,
-1.38452104295195E-9),.UNSPECIFIED.);
#23417=B_SPLINE_CURVE_WITH_KNOTS('',3,(#144733,#144734,#144735,#144736,
#144737,#144738),.UNSPECIFIED.,.F.,.F.,(4,2,4),(-0.0253028684626624,-0.012651311551332,
-1.42760715055035E-9),.UNSPECIFIED.);
#23418=B_SPLINE_CURVE_WITH_KNOTS('',3,(#144754,#144755,#144756,#144757,
#144758,#144759),.UNSPECIFIED.,.F.,.F.,(4,2,4),(-0.0253028607935486,-0.0126513115878577,
-1.42838934777401E-9),.UNSPECIFIED.);
#23419=B_SPLINE_CURVE_WITH_KNOTS('',3,(#144775,#144776,#144777,#144778,
#144779,#144780),.UNSPECIFIED.,.F.,.F.,(4,2,4),(-0.0253028607669744,-0.0126513116157709,
-1.47254117580098E-9),.UNSPECIFIED.);
#23420=B_SPLINE_CURVE_WITH_KNOTS('',3,(#144796,#144797,#144798,#144799,
#144800,#144801),.UNSPECIFIED.,.F.,.F.,(4,2,4),(-0.0253028683470321,-0.0126513117988463,
-1.62334940975728E-9),.UNSPECIFIED.);
#23421=B_SPLINE_CURVE_WITH_KNOTS('',3,(#144817,#144818,#144819,#144820,
#144821,#144822),.UNSPECIFIED.,.F.,.F.,(4,2,4),(-0.0253028608496447,-0.0126513116279292,
-1.4460164489416E-9),.UNSPECIFIED.);
#23422=B_SPLINE_CURVE_WITH_KNOTS('',3,(#144840,#144841,#144842,#144843,
#144844,#144845),.UNSPECIFIED.,.F.,.F.,(4,2,4),(-0.0253042129381971,-0.0126519919856879,
0.),.UNSPECIFIED.);
#23423=B_SPLINE_CURVE_WITH_KNOTS('',3,(#144855,#144856,#144857,#144858,
#144859,#144860),.UNSPECIFIED.,.F.,.F.,(4,2,4),(0.,0.0126519843067729,0.0253041804503512),
 .UNSPECIFIED.);
#23424=B_SPLINE_CURVE_WITH_KNOTS('',3,(#144884,#144885,#144886,#144887,
#144888,#144889),.UNSPECIFIED.,.F.,.F.,(4,2,4),(0.,0.0126519865865287,0.0253041900617945),
 .UNSPECIFIED.);
#23425=B_SPLINE_CURVE_WITH_KNOTS('',3,(#144913,#144914,#144915,#144916,
#144917,#144918),.UNSPECIFIED.,.F.,.F.,(4,2,4),(0.,0.0126519847777877,0.0253041824957834),
 .UNSPECIFIED.);
#23426=B_SPLINE_CURVE_WITH_KNOTS('',3,(#144942,#144943,#144944,#144945,
#144946,#144947),.UNSPECIFIED.,.F.,.F.,(4,2,4),(0.,0.0126519869389596,0.025304191433575),
 .UNSPECIFIED.);
#23427=B_SPLINE_CURVE_WITH_KNOTS('',3,(#144971,#144972,#144973,#144974,
#144975,#144976),.UNSPECIFIED.,.F.,.F.,(4,2,4),(0.,0.0126519849592999,0.025304183155069),
 .UNSPECIFIED.);
#23428=B_SPLINE_CURVE_WITH_KNOTS('',3,(#145000,#145001,#145002,#145003,
#145004,#145005),.UNSPECIFIED.,.F.,.F.,(4,2,4),(0.,0.0126519878879565,0.0253041955637346),
 .UNSPECIFIED.);
#23429=B_SPLINE_CURVE_WITH_KNOTS('',3,(#145026,#145027,#145028,#145029,
#145030,#145031),.UNSPECIFIED.,.F.,.F.,(4,2,4),(0.,0.0126519870093447,0.025304191879591),
 .UNSPECIFIED.);
#23430=B_SPLINE_CURVE_WITH_KNOTS('',3,(#145049,#145050,#145051,#145052,
#145053,#145054),.UNSPECIFIED.,.F.,.F.,(4,2,4),(0.,0.012651986717139,0.0253041906799449),
 .UNSPECIFIED.);
#23431=B_SPLINE_CURVE_WITH_KNOTS('',3,(#145078,#145079,#145080,#145081,
#145082,#145083),.UNSPECIFIED.,.F.,.F.,(4,2,4),(0.,0.0126519873096693,0.0253041931288259),
 .UNSPECIFIED.);
#23432=B_SPLINE_CURVE_WITH_KNOTS('',3,(#145107,#145108,#145109,#145110,
#145111,#145112),.UNSPECIFIED.,.F.,.F.,(4,2,4),(0.,0.0126519870612146,0.0253041921126481),
 .UNSPECIFIED.);
#23433=B_SPLINE_CURVE_WITH_KNOTS('',3,(#145136,#145137,#145138,#145139,
#145140,#145141),.UNSPECIFIED.,.F.,.F.,(4,2,4),(0.,0.0126519852924514,0.0253041846331273),
 .UNSPECIFIED.);
#23434=B_SPLINE_CURVE_WITH_KNOTS('',3,(#145165,#145166,#145167,#145168,
#145169,#145170),.UNSPECIFIED.,.F.,.F.,(4,2,4),(0.,0.0126519848460903,0.0253041826856367),
 .UNSPECIFIED.);
#23435=B_SPLINE_CURVE_WITH_KNOTS('',3,(#145194,#145195,#145196,#145197,
#145198,#145199),.UNSPECIFIED.,.F.,.F.,(4,2,4),(0.,0.0126519867876667,0.0253041908553758),
 .UNSPECIFIED.);
#23436=B_SPLINE_CURVE_WITH_KNOTS('',3,(#145223,#145224,#145225,#145226,
#145227,#145228),.UNSPECIFIED.,.F.,.F.,(4,2,4),(0.,0.0126519854542322,0.0253041852847222),
 .UNSPECIFIED.);
#23437=B_SPLINE_CURVE_WITH_KNOTS('',3,(#145252,#145253,#145254,#145255,
#145256,#145257),.UNSPECIFIED.,.F.,.F.,(4,2,4),(0.,0.0126519862176949,0.0253041884552269),
 .UNSPECIFIED.);
#23438=B_SPLINE_CURVE_WITH_KNOTS('',3,(#145281,#145282,#145283,#145284,
#145285,#145286),.UNSPECIFIED.,.F.,.F.,(4,2,4),(0.,0.0126519862606805,0.0253041886986062),
 .UNSPECIFIED.);
#23439=B_SPLINE_CURVE_WITH_KNOTS('',3,(#145310,#145311,#145312,#145313,
#145314,#145315),.UNSPECIFIED.,.F.,.F.,(4,2,4),(0.,0.0126519848133697,0.0253041826121683),
 .UNSPECIFIED.);
#23440=B_SPLINE_CURVE_WITH_KNOTS('',3,(#145339,#145340,#145341,#145342,
#145343,#145344),.UNSPECIFIED.,.F.,.F.,(4,2,4),(0.,0.0126519847288218,0.0253041821993781),
 .UNSPECIFIED.);
#23441=B_SPLINE_CURVE_WITH_KNOTS('',3,(#145368,#145369,#145370,#145371,
#145372,#145373),.UNSPECIFIED.,.F.,.F.,(4,2,4),(0.,0.0126519871577642,0.0253041925457795),
 .UNSPECIFIED.);
#23442=B_SPLINE_CURVE_WITH_KNOTS('',3,(#145398,#145399,#145400,#145401,
#145402,#145403),.UNSPECIFIED.,.F.,.F.,(4,2,4),(0.,0.0126519875408859,0.0253041941268785),
 .UNSPECIFIED.);
#23443=B_SPLINE_CURVE_WITH_KNOTS('',3,(#145426,#145427,#145428,#145429,
#145430,#145431),.UNSPECIFIED.,.F.,.F.,(4,2,4),(0.,0.0126519862827976,0.0253041887203517),
 .UNSPECIFIED.);
#23444=B_SPLINE_CURVE_WITH_KNOTS('',3,(#145455,#145456,#145457,#145458,
#145459,#145460),.UNSPECIFIED.,.F.,.F.,(4,2,4),(0.,0.012651985852953,0.0253041869280763),
 .UNSPECIFIED.);
#23445=B_SPLINE_CURVE_WITH_KNOTS('',3,(#145484,#145485,#145486,#145487,
#145488,#145489),.UNSPECIFIED.,.F.,.F.,(4,2,4),(0.,0.0126519861145527,0.0253041880659203),
 .UNSPECIFIED.);
#23446=B_SPLINE_CURVE_WITH_KNOTS('',3,(#145513,#145514,#145515,#145516,
#145517,#145518),.UNSPECIFIED.,.F.,.F.,(4,2,4),(0.,0.0126519863202011,0.0253041888160825),
 .UNSPECIFIED.);
#23447=B_SPLINE_CURVE_WITH_KNOTS('',3,(#145542,#145543,#145544,#145545,
#145546,#145547),.UNSPECIFIED.,.F.,.F.,(4,2,4),(0.,0.0126519859054325,0.0253041871291788),
 .UNSPECIFIED.);
#23448=B_SPLINE_CURVE_WITH_KNOTS('',3,(#145571,#145572,#145573,#145574,
#145575,#145576),.UNSPECIFIED.,.F.,.F.,(4,2,4),(0.,0.0126519835229689,0.0253041772181617),
 .UNSPECIFIED.);
#23449=B_SPLINE_CURVE_WITH_KNOTS('',3,(#145600,#145601,#145602,#145603,
#145604,#145605),.UNSPECIFIED.,.F.,.F.,(4,2,4),(0.,0.0126519864390143,0.0253041893892579),
 .UNSPECIFIED.);
#23450=B_SPLINE_CURVE_WITH_KNOTS('',3,(#145629,#145630,#145631,#145632,
#145633,#145634),.UNSPECIFIED.,.F.,.F.,(4,2,4),(0.,0.0126519858357069,0.025304186822954),
 .UNSPECIFIED.);
#23451=B_SPLINE_CURVE_WITH_KNOTS('',3,(#145669,#145670,#145671,#145672,
#145673,#145674),.UNSPECIFIED.,.F.,.F.,(4,2,4),(-0.0252989398056719,-0.0126493213074638,
0.),.UNSPECIFIED.);
#23452=B_SPLINE_CURVE_WITH_KNOTS('',3,(#145692,#145693,#145694,#145695,
#145696,#145697),.UNSPECIFIED.,.F.,.F.,(4,2,4),(0.,0.012649316395125,0.0252988129119735),
 .UNSPECIFIED.);
#23453=B_SPLINE_CURVE_WITH_KNOTS('',3,(#145725,#145726,#145727,#145728,
#145729,#145730),.UNSPECIFIED.,.F.,.F.,(4,2,4),(0.,0.0126493159533226,0.0252988074100563),
 .UNSPECIFIED.);
#23454=B_SPLINE_CURVE_WITH_KNOTS('',3,(#145758,#145759,#145760,#145761,
#145762,#145763),.UNSPECIFIED.,.F.,.F.,(4,2,4),(0.,0.012649321310377,0.0252988283293789),
 .UNSPECIFIED.);
#23455=B_SPLINE_CURVE_WITH_KNOTS('',3,(#145791,#145792,#145793,#145794,
#145795,#145796),.UNSPECIFIED.,.F.,.F.,(4,2,4),(0.,0.0126493158064216,0.0252988080156246),
 .UNSPECIFIED.);
#23456=B_SPLINE_CURVE_WITH_KNOTS('',3,(#145824,#145825,#145826,#145827,
#145828,#145829),.UNSPECIFIED.,.F.,.F.,(4,2,4),(0.,0.0126493154719441,0.0252988076384874),
 .UNSPECIFIED.);
#23457=B_SPLINE_CURVE_WITH_KNOTS('',3,(#145857,#145858,#145859,#145860,
#145861,#145862),.UNSPECIFIED.,.F.,.F.,(4,2,4),(0.,0.0126493163036998,0.0252988096871266),
 .UNSPECIFIED.);
#23458=B_SPLINE_CURVE_WITH_KNOTS('',3,(#145890,#145891,#145892,#145893,
#145894,#145895),.UNSPECIFIED.,.F.,.F.,(4,2,4),(0.,0.0126493213088601,0.0252988339968301),
 .UNSPECIFIED.);
#23459=B_SPLINE_CURVE_WITH_KNOTS('',3,(#145923,#145924,#145925,#145926,
#145927,#145928),.UNSPECIFIED.,.F.,.F.,(4,2,4),(0.,0.0126493212450843,0.0252988321670426),
 .UNSPECIFIED.);
#23460=B_SPLINE_CURVE_WITH_KNOTS('',3,(#145956,#145957,#145958,#145959,
#145960,#145961),.UNSPECIFIED.,.F.,.F.,(4,2,4),(0.,0.0126493164888677,0.0252988100939839),
 .UNSPECIFIED.);
#23461=B_SPLINE_CURVE_WITH_KNOTS('',3,(#145989,#145990,#145991,#145992,
#145993,#145994),.UNSPECIFIED.,.F.,.F.,(4,2,4),(0.,0.0126493167066686,0.0252988109105679),
 .UNSPECIFIED.);
#23462=B_SPLINE_CURVE_WITH_KNOTS('',3,(#146022,#146023,#146024,#146025,
#146026,#146027),.UNSPECIFIED.,.F.,.F.,(4,2,4),(0.,0.0126493212346032,0.025298829133827),
 .UNSPECIFIED.);
#23463=B_SPLINE_CURVE_WITH_KNOTS('',3,(#146055,#146056,#146057,#146058,
#146059,#146060),.UNSPECIFIED.,.F.,.F.,(4,2,4),(0.,0.0126493159995195,0.0252988104878458),
 .UNSPECIFIED.);
#23464=B_SPLINE_CURVE_WITH_KNOTS('',3,(#146088,#146089,#146090,#146091,
#146092,#146093),.UNSPECIFIED.,.F.,.F.,(4,2,4),(0.,0.0126493213102731,0.0252988320787696),
 .UNSPECIFIED.);
#23465=B_SPLINE_CURVE_WITH_KNOTS('',3,(#146118,#146119,#146120,#146121,
#146122,#146123),.UNSPECIFIED.,.F.,.F.,(4,2,4),(0.,0.0126493213088555,0.0252988287166666),
 .UNSPECIFIED.);
#23466=B_SPLINE_CURVE_WITH_KNOTS('',3,(#146145,#146146,#146147,#146148,
#146149,#146150),.UNSPECIFIED.,.F.,.F.,(4,2,4),(0.,0.0126493211988361,0.0252988317094231),
 .UNSPECIFIED.);
#23467=B_SPLINE_CURVE_WITH_KNOTS('',3,(#146178,#146179,#146180,#146181,
#146182,#146183),.UNSPECIFIED.,.F.,.F.,(4,2,4),(0.,0.012649321215418,0.0252988292224408),
 .UNSPECIFIED.);
#23468=B_SPLINE_CURVE_WITH_KNOTS('',3,(#146211,#146212,#146213,#146214,
#146215,#146216),.UNSPECIFIED.,.F.,.F.,(4,2,4),(0.,0.0126493160353129,0.0252988086035777),
 .UNSPECIFIED.);
#23469=B_SPLINE_CURVE_WITH_KNOTS('',3,(#146244,#146245,#146246,#146247,
#146248,#146249),.UNSPECIFIED.,.F.,.F.,(4,2,4),(0.,0.0126493212877845,0.0252988315664183),
 .UNSPECIFIED.);
#23470=B_SPLINE_CURVE_WITH_KNOTS('',3,(#146277,#146278,#146279,#146280,
#146281,#146282),.UNSPECIFIED.,.F.,.F.,(4,2,4),(0.,0.0126493212849581,0.0252988352832389),
 .UNSPECIFIED.);
#23471=B_SPLINE_CURVE_WITH_KNOTS('',3,(#146310,#146311,#146312,#146313,
#146314,#146315),.UNSPECIFIED.,.F.,.F.,(4,2,4),(0.,0.012649316194881,0.0252988129351232),
 .UNSPECIFIED.);
#23472=B_SPLINE_CURVE_WITH_KNOTS('',3,(#146343,#146344,#146345,#146346,
#146347,#146348),.UNSPECIFIED.,.F.,.F.,(4,2,4),(0.,0.0126493167128799,0.025298817624995),
 .UNSPECIFIED.);
#23473=B_SPLINE_CURVE_WITH_KNOTS('',3,(#146376,#146377,#146378,#146379,
#146380,#146381),.UNSPECIFIED.,.F.,.F.,(4,2,4),(0.,0.0126493213076427,0.0252988335485302),
 .UNSPECIFIED.);
#23474=B_SPLINE_CURVE_WITH_KNOTS('',3,(#146409,#146410,#146411,#146412,
#146413,#146414),.UNSPECIFIED.,.F.,.F.,(4,2,4),(0.,0.0126493213070669,0.025298828284289),
 .UNSPECIFIED.);
#23475=B_SPLINE_CURVE_WITH_KNOTS('',3,(#146442,#146443,#146444,#146445,
#146446,#146447),.UNSPECIFIED.,.F.,.F.,(4,2,4),(0.,0.0126493165134168,0.0252988152984364),
 .UNSPECIFIED.);
#23476=B_SPLINE_CURVE_WITH_KNOTS('',3,(#146475,#146476,#146477,#146478,
#146479,#146480),.UNSPECIFIED.,.F.,.F.,(4,2,4),(0.,0.0126493159700643,0.025298809661145),
 .UNSPECIFIED.);
#23477=B_SPLINE_CURVE_WITH_KNOTS('',3,(#146508,#146509,#146510,#146511,
#146512,#146513),.UNSPECIFIED.,.F.,.F.,(4,2,4),(0.,0.0126493213142762,0.0252988279997388),
 .UNSPECIFIED.);
#23478=B_SPLINE_CURVE_WITH_KNOTS('',3,(#146541,#146542,#146543,#146544,
#146545,#146546),.UNSPECIFIED.,.F.,.F.,(4,2,4),(0.,0.0126493162481951,0.0252988083212156),
 .UNSPECIFIED.);
#23479=B_SPLINE_CURVE_WITH_KNOTS('',3,(#146574,#146575,#146576,#146577,
#146578,#146579),.UNSPECIFIED.,.F.,.F.,(4,2,4),(0.,0.0126493163255192,0.0252988106377532),
 .UNSPECIFIED.);
#23480=B_SPLINE_CURVE_WITH_KNOTS('',3,(#146622,#146623,#146624,#146625,
#146626,#146627,#146628,#146629,#146630,#146631,#146632,#146633,#146634),
 .UNSPECIFIED.,.F.,.F.,(4,3,3,3,4),(0.,8.70610642392342E-5,0.00010313475499915,
0.000170041092769086,0.000253022912732791),.UNSPECIFIED.);
#23481=B_SPLINE_CURVE_WITH_KNOTS('',3,(#146650,#146651,#146652,#146653,
#146654,#146655,#146656,#146657,#146658,#146659),.UNSPECIFIED.,.F.,.F.,
(4,3,3,4),(0.556108173894251,0.558333952657053,0.568139465476172,0.573549700889344),
 .UNSPECIFIED.);
#23482=B_SPLINE_CURVE_WITH_KNOTS('',3,(#146660,#146661,#146662,#146663,
#146664,#146665,#146666,#146667,#146668,#146669),.UNSPECIFIED.,.F.,.F.,
(4,3,3,4),(1.69231154865856E-13,8.70609204190528E-5,0.000170040985661312,
0.000253023205846536),.UNSPECIFIED.);
#23483=B_SPLINE_CURVE_WITH_KNOTS('',3,(#146701,#146702,#146703,#146704,
#146705,#146706,#146707,#146708,#146709,#146710),.UNSPECIFIED.,.F.,.F.,
(4,3,3,4),(1.54680663374548E-13,8.70609205558343E-5,0.000170040985841156,
0.000253023206069013),.UNSPECIFIED.);
#23484=B_SPLINE_CURVE_WITH_KNOTS('',3,(#146737,#146738,#146739,#146740,
#146741,#146742,#146743,#146744,#146745,#146746,#146747,#146748,#146749,
#146750),.UNSPECIFIED.,.F.,.F.,(4,2,2,2,2,2,4),(3.17115822501972E-10,0.0399756457172238,
0.0600249637123924,0.0700670077817768,0.0750919619185494,0.0776053703943144,
0.080004019688016),.UNSPECIFIED.);
#23485=B_SPLINE_CURVE_WITH_KNOTS('',3,(#146751,#146752,#146753,#146754,
#146755,#146756,#146757,#146758,#146759,#146760),.UNSPECIFIED.,.F.,.F.,
(4,3,3,4),(1.61821296805164E-13,8.70609204750516E-5,0.000170040985668408,
0.000253023205803955),.UNSPECIFIED.);
#23486=B_SPLINE_CURVE_WITH_KNOTS('',3,(#146792,#146793,#146794,#146795,
#146796,#146797,#146798,#146799,#146800,#146801),.UNSPECIFIED.,.F.,.F.,
(4,3,3,4),(1.8179717827368E-13,8.70609204854375E-5,0.000170040985755457,
0.000253023205969049),.UNSPECIFIED.);
#23487=B_SPLINE_CURVE_WITH_KNOTS('',3,(#146833,#146834,#146835,#146836,
#146837,#146838,#146839,#146840,#146841,#146842),.UNSPECIFIED.,.F.,.F.,
(4,3,3,4),(1.82791368656842E-13,8.70609205854241E-5,0.000170040985761326,
0.000253023205880162),.UNSPECIFIED.);
#23488=B_SPLINE_CURVE_WITH_KNOTS('',3,(#146869,#146870,#146871,#146872,
#146873,#146874,#146875,#146876,#146877,#146878,#146879,#146880,#146881,
#146882),.UNSPECIFIED.,.F.,.F.,(4,2,2,2,2,2,4),(3.25736694958069E-10,0.0399756350505435,
0.060024947723225,0.070066996420522,0.0750919528708576,0.0776053625034702,
0.0800040128963778),.UNSPECIFIED.);
#23489=B_SPLINE_CURVE_WITH_KNOTS('',3,(#146883,#146884,#146885,#146886,
#146887,#146888,#146889,#146890,#146891,#146892),.UNSPECIFIED.,.F.,.F.,
(4,3,3,4),(9.38154535606092E-14,8.70609207349159E-5,0.00017004098588965,
0.000253023205987876),.UNSPECIFIED.);
#23490=B_SPLINE_CURVE_WITH_KNOTS('',3,(#146919,#146920,#146921,#146922,
#146923,#146924,#146925,#146926,#146927,#146928,#146929,#146930,#146931,
#146932),.UNSPECIFIED.,.F.,.F.,(4,2,2,2,2,2,4),(3.42543828201874E-10,0.0399756356949133,
0.0600249478091022,0.0700669878091456,0.0750919399147613,0.077605347375955,
0.0800039956845119),.UNSPECIFIED.);
#23491=B_SPLINE_CURVE_WITH_KNOTS('',3,(#146933,#146934,#146935,#146936,
#146937,#146938,#146939,#146940,#146941,#146942),.UNSPECIFIED.,.F.,.F.,
(4,3,3,4),(9.32267848327091E-14,8.70609204372164E-5,0.000170040985887543,
0.000253023206279809),.UNSPECIFIED.);
#23492=B_SPLINE_CURVE_WITH_KNOTS('',3,(#146969,#146970,#146971,#146972,
#146973,#146974,#146975,#146976,#146977,#146978),.UNSPECIFIED.,.F.,.F.,
(4,3,3,4),(0.556108173897008,0.558333952657056,0.568139434940753,0.57354970089104),
 .UNSPECIFIED.);
#23493=B_SPLINE_CURVE_WITH_KNOTS('',3,(#146979,#146980,#146981,#146982,
#146983,#146984,#146985,#146986,#146987,#146988,#146989,#146990,#146991),
 .UNSPECIFIED.,.F.,.F.,(4,3,3,3,4),(2.17783596318746E-13,8.70609204643982E-5,
0.000149888113335004,0.000170040985596686,0.000253023205671698),
 .UNSPECIFIED.);
#23494=B_SPLINE_CURVE_WITH_KNOTS('',3,(#147018,#147019,#147020,#147021,
#147022,#147023,#147024,#147025,#147026,#147027),.UNSPECIFIED.,.F.,.F.,
(4,3,3,4),(0.556108173865716,0.558333952657056,0.568139432990237,0.573549700892214),
 .UNSPECIFIED.);
#23495=B_SPLINE_CURVE_WITH_KNOTS('',3,(#147028,#147029,#147030,#147031,
#147032,#147033,#147034,#147035,#147036,#147037,#147038,#147039,#147040),
 .UNSPECIFIED.,.F.,.F.,(4,3,3,3,4),(8.71190282254634E-14,8.70609204912651E-5,
0.000149888113153294,0.000170040985908022,0.000253023206266396),
 .UNSPECIFIED.);
#23496=B_SPLINE_CURVE_WITH_KNOTS('',3,(#147067,#147068,#147069,#147070,
#147071,#147072,#147073,#147074,#147075,#147076,#147077,#147078,#147079,
#147080),.UNSPECIFIED.,.F.,.F.,(4,2,2,2,2,2,4),(2.72062316739559E-10,0.0399756540412885,
0.0600249697811288,0.0700669995408656,0.075091946519025,0.0776053514146817,
0.080003997248157),.UNSPECIFIED.);
#23497=B_SPLINE_CURVE_WITH_KNOTS('',3,(#147081,#147082,#147083,#147084,
#147085,#147086,#147087,#147088,#147089,#147090),.UNSPECIFIED.,.F.,.F.,
(4,3,3,4),(1.96283630672745E-13,8.7060920517827E-5,0.000170040985827293,
0.000253023206080021),.UNSPECIFIED.);
#23498=B_SPLINE_CURVE_WITH_KNOTS('',3,(#147122,#147123,#147124,#147125,
#147126,#147127,#147128,#147129,#147130,#147131),.UNSPECIFIED.,.F.,.F.,
(4,3,3,4),(1.38795067579082E-13,8.7060920468453E-5,0.000170040985661875,
0.000253023205798495),.UNSPECIFIED.);
#23499=B_SPLINE_CURVE_WITH_KNOTS('',3,(#147158,#147159,#147160,#147161,
#147162,#147163,#147164,#147165,#147166,#147167,#147168,#147169,#147170,
#147171),.UNSPECIFIED.,.F.,.F.,(4,2,2,2,2,2,4),(2.7352003332601E-10,0.0399756335387596,
0.0600249433548185,0.0700669840178637,0.0750919364533658,0.0776053440791422,
0.0800039925289707),.UNSPECIFIED.);
#23500=B_SPLINE_CURVE_WITH_KNOTS('',3,(#147172,#147173,#147174,#147175,
#147176,#147177,#147178,#147179,#147180,#147181),.UNSPECIFIED.,.F.,.F.,
(4,3,3,4),(2.56474145581824E-13,8.70609204134192E-5,0.000170040985667171,
0.000253023205863517),.UNSPECIFIED.);
#23501=B_SPLINE_CURVE_WITH_KNOTS('',3,(#147213,#147214,#147215,#147216,
#147217,#147218,#147219,#147220,#147221,#147222,#147223,#147224,#147225),
 .UNSPECIFIED.,.F.,.F.,(4,3,3,3,4),(1.72563598568684E-13,8.70609205411575E-5,
0.00014988811322632,0.000170040985712443,0.00025302320582707),
 .UNSPECIFIED.);
#23502=B_SPLINE_CURVE_WITH_KNOTS('',3,(#147252,#147253,#147254,#147255,
#147256,#147257,#147258,#147259,#147260,#147261),.UNSPECIFIED.,.F.,.F.,
(4,3,3,4),(0.556108173930173,0.558333952657056,0.568139440253929,0.573549700889268),
 .UNSPECIFIED.);
#23503=B_SPLINE_CURVE_WITH_KNOTS('',3,(#147262,#147263,#147264,#147265,
#147266,#147267,#147268,#147269,#147270,#147271),.UNSPECIFIED.,.F.,.F.,
(4,3,3,4),(9.95524747780889E-14,8.70609207631359E-5,0.000170040985962216,
0.000253023206105423),.UNSPECIFIED.);
#23504=B_SPLINE_CURVE_WITH_KNOTS('',3,(#147298,#147299,#147300,#147301,
#147302,#147303,#147304,#147305,#147306,#147307,#147308,#147309,#147310,
#147311),.UNSPECIFIED.,.F.,.F.,(4,2,2,2,2,2,4),(2.08407129104266E-10,0.0399756526762724,
0.0600249688922645,0.0700670003688512,0.0750919482058424,0.0776053535310304,
0.0800039998029628),.UNSPECIFIED.);
#23505=B_SPLINE_CURVE_WITH_KNOTS('',3,(#147312,#147313,#147314,#147315,
#147316,#147317,#147318,#147319,#147320,#147321),.UNSPECIFIED.,.F.,.F.,
(4,3,3,4),(1.10306306544097E-13,8.70609205778296E-5,0.00017004098578854,
0.000253023205942734),.UNSPECIFIED.);
#23506=B_SPLINE_CURVE_WITH_KNOTS('',3,(#147348,#147349,#147350,#147351,
#147352,#147353,#147354,#147355,#147356,#147357),.UNSPECIFIED.,.F.,.F.,
(4,3,3,4),(0.556108173910857,0.558333952657056,0.568139440135517,0.573549700893365),
 .UNSPECIFIED.);
#23507=B_SPLINE_CURVE_WITH_KNOTS('',3,(#147358,#147359,#147360,#147361,
#147362,#147363,#147364,#147365,#147366,#147367),.UNSPECIFIED.,.F.,.F.,
(4,3,3,4),(2.24448260341437E-13,8.70609204346609E-5,0.000170040985496222,
0.000253023205500031),.UNSPECIFIED.);
#23508=B_SPLINE_CURVE_WITH_KNOTS('',3,(#147399,#147400,#147401,#147402,
#147403,#147404,#147405,#147406,#147407,#147408),.UNSPECIFIED.,.F.,.F.,
(4,3,3,4),(1.55289471312465E-13,8.70609206640267E-5,0.000170040985730055,
0.00025302320573868),.UNSPECIFIED.);
#23509=B_SPLINE_CURVE_WITH_KNOTS('',3,(#147435,#147436,#147437,#147438,
#147439,#147440,#147441,#147442,#147443,#147444),.UNSPECIFIED.,.F.,.F.,
(4,3,3,4),(0.556108173913933,0.558333952657056,0.568139463253051,0.573549700879883),
 .UNSPECIFIED.);
#23510=B_SPLINE_CURVE_WITH_KNOTS('',3,(#147445,#147446,#147447,#147448,
#147449,#147450,#147451,#147452,#147453,#147454),.UNSPECIFIED.,.F.,.F.,
(4,3,3,4),(8.75431270138763E-14,8.70609204120076E-5,0.000170040985741647,
0.000253023206012933),.UNSPECIFIED.);
#23511=B_SPLINE_CURVE_WITH_KNOTS('',3,(#147481,#147482,#147483,#147484,
#147485,#147486,#147487,#147488,#147489,#147490,#147491,#147492,#147493,
#147494),.UNSPECIFIED.,.F.,.F.,(4,2,2,2,2,2,4),(2.99556102725697E-10,0.0399756352567531,
0.0600249465583133,0.070066989855618,0.0750919436067488,0.0776053518899977,
0.0800040009606207),.UNSPECIFIED.);
#23512=B_SPLINE_CURVE_WITH_KNOTS('',3,(#147495,#147496,#147497,#147498,
#147499,#147500,#147501,#147502,#147503,#147504),.UNSPECIFIED.,.F.,.F.,
(4,3,3,4),(2.11907265441818E-13,8.70609206450316E-5,0.000170040985681721,
0.000253023205661128),.UNSPECIFIED.);
#23513=B_SPLINE_CURVE_WITH_KNOTS('',3,(#147531,#147532,#147533,#147534,
#147535,#147536,#147537,#147538,#147539,#147540),.UNSPECIFIED.,.F.,.F.,
(4,3,3,4),(0.556108173921688,0.558333952657057,0.568139461882756,0.573549700889244),
 .UNSPECIFIED.);
#23514=B_SPLINE_CURVE_WITH_KNOTS('',3,(#147541,#147542,#147543,#147544,
#147545,#147546,#147547,#147548,#147549,#147550),.UNSPECIFIED.,.F.,.F.,
(4,3,3,4),(1.37524544768384E-13,8.70609205860296E-5,0.000170040985872499,
0.000253023206102047),.UNSPECIFIED.);
#23515=B_SPLINE_CURVE_WITH_KNOTS('',3,(#147577,#147578,#147579,#147580,
#147581,#147582,#147583,#147584,#147585,#147586),.UNSPECIFIED.,.F.,.F.,
(4,3,3,4),(0.556108173920208,0.558333952657064,0.568139457501484,0.573549700896862),
 .UNSPECIFIED.);
#23516=B_SPLINE_CURVE_WITH_KNOTS('',3,(#147587,#147588,#147589,#147590,
#147591,#147592,#147593,#147594,#147595,#147596),.UNSPECIFIED.,.F.,.F.,
(4,3,3,4),(1.71159403601284E-13,8.70609204517324E-5,0.000170040985610444,
0.000253023205711528),.UNSPECIFIED.);
#23517=B_SPLINE_CURVE_WITH_KNOTS('',3,(#147623,#147624,#147625,#147626,
#147627,#147628,#147629,#147630,#147631,#147632,#147633,#147634,#147635,
#147636),.UNSPECIFIED.,.F.,.F.,(4,2,2,2,2,2,4),(3.15293603599107E-10,0.0399756318238306,
0.0600249397363027,0.0700669805933937,0.075091933125416,0.0776053407993536,
0.0800039893127443),.UNSPECIFIED.);
#23518=B_SPLINE_CURVE_WITH_KNOTS('',3,(#147637,#147638,#147639,#147640,
#147641,#147642,#147643,#147644,#147645,#147646),.UNSPECIFIED.,.F.,.F.,
(4,3,3,4),(2.22592601224058E-13,8.70609204363956E-5,0.000170040985578146,
0.000253023205662112),.UNSPECIFIED.);
#23519=B_SPLINE_CURVE_WITH_KNOTS('',3,(#147673,#147674,#147675,#147676,
#147677,#147678,#147679,#147680,#147681,#147682),.UNSPECIFIED.,.F.,.F.,
(4,3,3,4),(0.556108173873244,0.558333952657066,0.568139478039504,0.573549700885696),
 .UNSPECIFIED.);
#23520=B_SPLINE_CURVE_WITH_KNOTS('',3,(#147683,#147684,#147685,#147686,
#147687,#147688,#147689,#147690,#147691,#147692),.UNSPECIFIED.,.F.,.F.,
(4,3,3,4),(1.86698732542565E-13,8.70609205947636E-5,0.000170040985794769,
0.000253023205936877),.UNSPECIFIED.);
#23521=B_SPLINE_CURVE_WITH_KNOTS('',3,(#147719,#147720,#147721,#147722,
#147723,#147724,#147725,#147726,#147727,#147728,#147729,#147730,#147731,
#147732),.UNSPECIFIED.,.F.,.F.,(4,2,2,2,2,2,4),(2.73861150635604E-10,0.0399756418181266,
0.0600249547070785,0.0700669927695654,0.0750919439059226,0.0776053508825574,
0.0800039986914438),.UNSPECIFIED.);
#23522=B_SPLINE_CURVE_WITH_KNOTS('',3,(#147733,#147734,#147735,#147736,
#147737,#147738,#147739,#147740,#147741,#147742),.UNSPECIFIED.,.F.,.F.,
(4,3,3,4),(1.25089518386443E-13,8.70609206928586E-5,0.000170040985933957,
0.000253023206117974),.UNSPECIFIED.);
#23523=B_SPLINE_CURVE_WITH_KNOTS('',3,(#147769,#147770,#147771,#147772,
#147773,#147774,#147775,#147776,#147777,#147778),.UNSPECIFIED.,.F.,.F.,
(4,3,3,4),(0.556108173902585,0.558333952657053,0.568139480300036,0.573549700888651),
 .UNSPECIFIED.);
#23524=B_SPLINE_CURVE_WITH_KNOTS('',3,(#147779,#147780,#147781,#147782,
#147783,#147784,#147785,#147786,#147787,#147788,#147789,#147790,#147791),
 .UNSPECIFIED.,.F.,.F.,(4,3,3,3,4),(9.56422294869686E-14,8.70609205457756E-5,
0.000149888113578247,0.00017004098589937,0.000253023206195566),
 .UNSPECIFIED.);
#23525=B_SPLINE_CURVE_WITH_KNOTS('',3,(#147818,#147819,#147820,#147821,
#147822,#147823,#147824,#147825,#147826,#147827,#147828,#147829,#147830,
#147831),.UNSPECIFIED.,.F.,.F.,(4,2,2,2,2,2,4),(2.38543663118769E-10,0.03997565913649,
0.0600249813095576,0.0700670156573217,0.0750919649363173,0.077605370984128,
0.0800040179180761),.UNSPECIFIED.);
#23526=B_SPLINE_CURVE_WITH_KNOTS('',3,(#147832,#147833,#147834,#147835,
#147836,#147837,#147838,#147839,#147840,#147841),.UNSPECIFIED.,.F.,.F.,
(4,3,3,4),(2.3455914248856E-13,8.70609204481195E-5,0.000170040985735005,
0.000253023205965325),.UNSPECIFIED.);
#23527=B_SPLINE_CURVE_WITH_KNOTS('',3,(#147868,#147869,#147870,#147871,
#147872,#147873,#147874,#147875,#147876,#147877),.UNSPECIFIED.,.F.,.F.,
(4,3,3,4),(0.556108173916858,0.558333952657053,0.5681394446842,0.57354970088037),
 .UNSPECIFIED.);
#23528=B_SPLINE_CURVE_WITH_KNOTS('',3,(#147878,#147879,#147880,#147881,
#147882,#147883,#147884,#147885,#147886,#147887),.UNSPECIFIED.,.F.,.F.,
(4,3,3,4),(1.57842903223202E-13,8.70609205573698E-5,0.000170040985736597,
0.000253023205859146),.UNSPECIFIED.);
#23529=B_SPLINE_CURVE_WITH_KNOTS('',3,(#147914,#147915,#147916,#147917,
#147918,#147919,#147920,#147921,#147922,#147923,#147924,#147925,#147926,
#147927),.UNSPECIFIED.,.F.,.F.,(4,2,2,2,2,2,4),(2.49802435109874E-10,0.0399756361689207,
0.0600249451800575,0.0700669820430787,0.0750919325770055,0.0776053392515876,
0.0800039867512925),.UNSPECIFIED.);
#23530=B_SPLINE_CURVE_WITH_KNOTS('',3,(#147928,#147929,#147930,#147931,
#147932,#147933,#147934,#147935,#147936,#147937),.UNSPECIFIED.,.F.,.F.,
(4,3,3,4),(2.27093858578823E-13,8.7060920387382E-5,0.000170040985638493,
0.000253023205833007),.UNSPECIFIED.);
#23531=B_SPLINE_CURVE_WITH_KNOTS('',3,(#147963,#147964,#147965,#147966,
#147967,#147968,#147969,#147970,#147971,#147972,#147973,#147974,#147975,
#147976),.UNSPECIFIED.,.F.,.F.,(4,2,2,2,2,2,4),(1.87595803499913E-10,0.0399756516265179,
0.0600249695553755,0.0700670019266469,0.0750919502131022,0.0776053557636566,
0.0800040022491232),.UNSPECIFIED.);
#23532=B_SPLINE_CURVE_WITH_KNOTS('',3,(#147984,#147985,#147986,#147987,
#147988,#147989),.UNSPECIFIED.,.F.,.F.,(4,2,4),(0.,0.0126518799230764,0.0253039866726396),
 .UNSPECIFIED.);
#23533=B_SPLINE_CURVE_WITH_KNOTS('',3,(#148003,#148004,#148005,#148006,
#148007,#148008),.UNSPECIFIED.,.F.,.F.,(4,2,4),(-0.0253039870735502,-0.0126518801554942,
-4.4945748511882E-11),.UNSPECIFIED.);
#23534=B_SPLINE_CURVE_WITH_KNOTS('',3,(#148028,#148029,#148030,#148031,
#148032,#148033),.UNSPECIFIED.,.F.,.F.,(4,2,4),(-0.025303988212384,-0.0126518801493775,
-6.78167313972189E-11),.UNSPECIFIED.);
#23535=B_SPLINE_CURVE_WITH_KNOTS('',3,(#148053,#148054,#148055,#148056,
#148057,#148058),.UNSPECIFIED.,.F.,.F.,(4,2,4),(-0.0253039877294629,-0.0126518801101943,
0.),.UNSPECIFIED.);
#23536=B_SPLINE_CURVE_WITH_KNOTS('',3,(#148078,#148079,#148080,#148081,
#148082,#148083),.UNSPECIFIED.,.F.,.F.,(4,2,4),(-0.0253039877142318,-0.0126518802515817,
-1.27645775893637E-10),.UNSPECIFIED.);
#23537=B_SPLINE_CURVE_WITH_KNOTS('',3,(#148103,#148104,#148105,#148106,
#148107,#148108),.UNSPECIFIED.,.F.,.F.,(4,2,4),(-0.0253039881409112,-0.012651880135877,
-6.53908663328373E-11),.UNSPECIFIED.);
#23538=B_SPLINE_CURVE_WITH_KNOTS('',3,(#148128,#148129,#148130,#148131,
#148132,#148133),.UNSPECIFIED.,.F.,.F.,(4,2,4),(-0.0253039874124978,-0.0126518802797077,
-1.45539209156498E-10),.UNSPECIFIED.);
#23539=B_SPLINE_CURVE_WITH_KNOTS('',3,(#148153,#148154,#148155,#148156,
#148157,#148158),.UNSPECIFIED.,.F.,.F.,(4,2,4),(-0.025303987819935,-0.0126518802163937,
-9.41260888676076E-11),.UNSPECIFIED.);
#23540=B_SPLINE_CURVE_WITH_KNOTS('',3,(#148178,#148179,#148180,#148181,
#148182,#148183),.UNSPECIFIED.,.F.,.F.,(4,2,4),(-0.025303987005773,-0.0126518802269383,
-8.98671033422449E-11),.UNSPECIFIED.);
#23541=B_SPLINE_CURVE_WITH_KNOTS('',3,(#148203,#148204,#148205,#148206,
#148207,#148208),.UNSPECIFIED.,.F.,.F.,(4,2,4),(-0.0253039876388824,-0.0126518800737849,
0.),.UNSPECIFIED.);
#23542=B_SPLINE_CURVE_WITH_KNOTS('',3,(#148228,#148229,#148230,#148231,
#148232,#148233),.UNSPECIFIED.,.F.,.F.,(4,2,4),(-0.0253039873540886,-0.0126518801299279,
-2.55819705696769E-11),.UNSPECIFIED.);
#23543=B_SPLINE_CURVE_WITH_KNOTS('',3,(#148253,#148254,#148255,#148256,
#148257,#148258),.UNSPECIFIED.,.F.,.F.,(4,2,4),(-0.0253039877440053,-0.0126518801932579,
-6.41805636414361E-11),.UNSPECIFIED.);
#23544=B_SPLINE_CURVE_WITH_KNOTS('',3,(#148278,#148279,#148280,#148281,
#148282,#148283),.UNSPECIFIED.,.F.,.F.,(4,2,4),(-0.025303988161419,-0.0126518802705622,
-1.48159921831148E-10),.UNSPECIFIED.);
#23545=B_SPLINE_CURVE_WITH_KNOTS('',3,(#148303,#148304,#148305,#148306,
#148307,#148308),.UNSPECIFIED.,.F.,.F.,(4,2,4),(-0.0253039868057278,-0.0126518802510195,
-1.43891034504184E-10),.UNSPECIFIED.);
#23546=B_SPLINE_CURVE_WITH_KNOTS('',3,(#148328,#148329,#148330,#148331,
#148332,#148333),.UNSPECIFIED.,.F.,.F.,(4,2,4),(-0.0253039861773998,-0.0126518792406827,
-1.25047541765788E-12),.UNSPECIFIED.);
#23547=B_SPLINE_CURVE_WITH_KNOTS('',3,(#148353,#148354,#148355,#148356,
#148357,#148358),.UNSPECIFIED.,.F.,.F.,(4,2,4),(-0.0253039872355756,-0.012651880214651,
-8.66837955582067E-11),.UNSPECIFIED.);
#23548=B_SPLINE_CURVE_WITH_KNOTS('',3,(#148378,#148379,#148380,#148381,
#148382,#148383),.UNSPECIFIED.,.F.,.F.,(4,2,4),(-0.025303986926397,-0.0126518801426057,
-3.96025053028826E-11),.UNSPECIFIED.);
#23549=B_SPLINE_CURVE_WITH_KNOTS('',3,(#148403,#148404,#148405,#148406,
#148407,#148408),.UNSPECIFIED.,.F.,.F.,(4,2,4),(-0.0253039871076078,-0.0126518802996017,
-1.54504083138551E-10),.UNSPECIFIED.);
#23550=B_SPLINE_CURVE_WITH_KNOTS('',3,(#148428,#148429,#148430,#148431,
#148432,#148433),.UNSPECIFIED.,.F.,.F.,(4,2,4),(-0.0253039881080807,-0.012651880317787,
-1.8657949837908E-10),.UNSPECIFIED.);
#23551=B_SPLINE_CURVE_WITH_KNOTS('',3,(#148453,#148454,#148455,#148456,
#148457,#148458),.UNSPECIFIED.,.F.,.F.,(4,2,4),(-0.0253039878268396,-0.012651880171774,
-5.62077259735894E-11),.UNSPECIFIED.);
#23552=B_SPLINE_CURVE_WITH_KNOTS('',3,(#148478,#148479,#148480,#148481,
#148482,#148483),.UNSPECIFIED.,.F.,.F.,(4,2,4),(-0.0253039875227548,-0.012651880215428,
-9.63703908340996E-11),.UNSPECIFIED.);
#23553=B_SPLINE_CURVE_WITH_KNOTS('',3,(#148503,#148504,#148505,#148506,
#148507,#148508),.UNSPECIFIED.,.F.,.F.,(4,2,4),(-0.0253039869108518,-0.0126518801654752,
-5.19251655561881E-11),.UNSPECIFIED.);
#23554=B_SPLINE_CURVE_WITH_KNOTS('',3,(#148528,#148529,#148530,#148531,
#148532,#148533),.UNSPECIFIED.,.F.,.F.,(4,2,4),(-0.0253039878151877,-0.0126518800924445,
0.),.UNSPECIFIED.);
#23555=B_SPLINE_CURVE_WITH_KNOTS('',3,(#148553,#148554,#148555,#148556,
#148557,#148558),.UNSPECIFIED.,.F.,.F.,(4,2,4),(-0.0253039878504019,-0.0126518801601293,
-8.34110037983837E-11),.UNSPECIFIED.);
#23556=B_SPLINE_CURVE_WITH_KNOTS('',3,(#148578,#148579,#148580,#148581,
#148582,#148583),.UNSPECIFIED.,.F.,.F.,(4,2,4),(-0.0253039876310961,-0.0126518802884517,
-1.63184913498648E-10),.UNSPECIFIED.);
#23557=B_SPLINE_CURVE_WITH_KNOTS('',3,(#148603,#148604,#148605,#148606,
#148607,#148608),.UNSPECIFIED.,.F.,.F.,(4,2,4),(-0.0253039877773045,-0.012651880230267,
-8.69090979738196E-11),.UNSPECIFIED.);
#23558=B_SPLINE_CURVE_WITH_KNOTS('',3,(#148628,#148629,#148630,#148631,
#148632,#148633),.UNSPECIFIED.,.F.,.F.,(4,2,4),(-0.025303986895663,-0.0126518801777525,
-8.87840599650414E-11),.UNSPECIFIED.);
#23559=B_SPLINE_CURVE_WITH_KNOTS('',3,(#148653,#148654,#148655,#148656,
#148657,#148658),.UNSPECIFIED.,.F.,.F.,(4,2,4),(-0.0253039879972589,-0.0126518801718497,
-6.59172473549408E-11),.UNSPECIFIED.);
#23560=B_SPLINE_CURVE_WITH_KNOTS('',3,(#148678,#148679,#148680,#148681,
#148682,#148683),.UNSPECIFIED.,.F.,.F.,(4,2,4),(-0.0253039869494593,-0.0126518802187377,
-1.08653201019715E-10),.UNSPECIFIED.);
#23561=B_SPLINE_CURVE_WITH_KNOTS('',3,(#148715,#148716,#148717,#148718,
#148719,#148720),.UNSPECIFIED.,.F.,.F.,(4,2,4),(1.2316114164264E-10,0.012650972362086,
0.0253021873423967),.UNSPECIFIED.);
#23562=B_SPLINE_CURVE_WITH_KNOTS('',3,(#148727,#148728,#148729,#148730,
#148731,#148732,#148733),.UNSPECIFIED.,.F.,.F.,(4,3,4),(0.561466076967393,
0.571428571428571,0.57365435021991),.UNSPECIFIED.);
#23563=B_SPLINE_CURVE_WITH_KNOTS('',3,(#148758,#148759,#148760,#148761,
#148762,#148763),.UNSPECIFIED.,.F.,.F.,(4,2,4),(0.,0.012650972319385,0.0253021873649507),
 .UNSPECIFIED.);
#23564=B_SPLINE_CURVE_WITH_KNOTS('',3,(#148770,#148771,#148772,#148773,
#148774,#148775,#148776),.UNSPECIFIED.,.F.,.F.,(4,3,4),(0.561466076966358,
0.571428571428571,0.57365435021991),.UNSPECIFIED.);
#23565=B_SPLINE_CURVE_WITH_KNOTS('',3,(#148801,#148802,#148803,#148804,
#148805,#148806),.UNSPECIFIED.,.F.,.F.,(4,2,4),(0.,0.012650972315468,0.025302187363785),
 .UNSPECIFIED.);
#23566=B_SPLINE_CURVE_WITH_KNOTS('',3,(#148813,#148814,#148815,#148816,
#148817,#148818,#148819),.UNSPECIFIED.,.F.,.F.,(4,3,4),(0.561466076969539,
0.571428571428571,0.573654350219911),.UNSPECIFIED.);
#23567=B_SPLINE_CURVE_WITH_KNOTS('',3,(#148844,#148845,#148846,#148847,
#148848,#148849),.UNSPECIFIED.,.F.,.F.,(4,2,4),(9.04688586768257E-11,0.0126509723542132,
0.0253021873590814),.UNSPECIFIED.);
#23568=B_SPLINE_CURVE_WITH_KNOTS('',3,(#148856,#148857,#148858,#148859,
#148860,#148861,#148862),.UNSPECIFIED.,.F.,.F.,(4,3,4),(0.561466076978747,
0.571428571428571,0.573654350219911),.UNSPECIFIED.);
#23569=B_SPLINE_CURVE_WITH_KNOTS('',3,(#148887,#148888,#148889,#148890,
#148891,#148892),.UNSPECIFIED.,.F.,.F.,(4,2,4),(1.55063105361005E-10,0.0126509724789961,
0.0253021874395334),.UNSPECIFIED.);
#23570=B_SPLINE_CURVE_WITH_KNOTS('',3,(#148899,#148900,#148901,#148902,
#148903,#148904,#148905),.UNSPECIFIED.,.F.,.F.,(4,3,4),(0.561466076972735,
0.571428571428571,0.573654350219911),.UNSPECIFIED.);
#23571=B_SPLINE_CURVE_WITH_KNOTS('',3,(#148930,#148931,#148932,#148933,
#148934,#148935),.UNSPECIFIED.,.F.,.F.,(4,2,4),(1.18014507066057E-10,0.0126509723379533,
0.0253021873193351),.UNSPECIFIED.);
#23572=B_SPLINE_CURVE_WITH_KNOTS('',3,(#148942,#148943,#148944,#148945,
#148946,#148947,#148948),.UNSPECIFIED.,.F.,.F.,(4,3,4),(0.561466076971035,
0.571428571428571,0.573654350219911),.UNSPECIFIED.);
#23573=B_SPLINE_CURVE_WITH_KNOTS('',3,(#148973,#148974,#148975,#148976,
#148977,#148978),.UNSPECIFIED.,.F.,.F.,(4,2,4),(1.33608236322443E-10,0.0126509723640742,
0.0253021873406959),.UNSPECIFIED.);
#23574=B_SPLINE_CURVE_WITH_KNOTS('',3,(#148985,#148986,#148987,#148988,
#148989,#148990,#148991),.UNSPECIFIED.,.F.,.F.,(4,3,4),(0.561466076969876,
0.571428571428571,0.573654350219911),.UNSPECIFIED.);
#23575=B_SPLINE_CURVE_WITH_KNOTS('',3,(#149016,#149017,#149018,#149019,
#149020,#149021),.UNSPECIFIED.,.F.,.F.,(4,2,4),(8.75960167674949E-11,0.012650972335585,
0.025302187348281),.UNSPECIFIED.);
#23576=B_SPLINE_CURVE_WITH_KNOTS('',3,(#149028,#149029,#149030,#149031,
#149032,#149033,#149034),.UNSPECIFIED.,.F.,.F.,(4,3,4),(0.561466076970862,
0.571428571428571,0.573654350219911),.UNSPECIFIED.);
#23577=B_SPLINE_CURVE_WITH_KNOTS('',3,(#149059,#149060,#149061,#149062,
#149063,#149064),.UNSPECIFIED.,.F.,.F.,(4,2,4),(1.13250179511007E-10,0.0126509723673497,
0.0253021873796661),.UNSPECIFIED.);
#23578=B_SPLINE_CURVE_WITH_KNOTS('',3,(#149071,#149072,#149073,#149074,
#149075,#149076,#149077),.UNSPECIFIED.,.F.,.F.,(4,3,4),(0.561466076977858,
0.571428571428571,0.573654350219911),.UNSPECIFIED.);
#23579=B_SPLINE_CURVE_WITH_KNOTS('',3,(#149102,#149103,#149104,#149105,
#149106,#149107),.UNSPECIFIED.,.F.,.F.,(4,2,4),(3.19290848309924E-11,0.012650984626482,
0.0253022387208064),.UNSPECIFIED.);
#23580=B_SPLINE_CURVE_WITH_KNOTS('',3,(#149114,#149115,#149116,#149117,
#149118,#149119,#149120),.UNSPECIFIED.,.F.,.F.,(4,3,4),(0.561466076972143,
0.571428571428571,0.573654350219912),.UNSPECIFIED.);
#23581=B_SPLINE_CURVE_WITH_KNOTS('',3,(#149145,#149146,#149147,#149148,
#149149,#149150),.UNSPECIFIED.,.F.,.F.,(4,2,4),(3.90657541139824E-11,0.0126509723622263,
0.0253021873944465),.UNSPECIFIED.);
#23582=B_SPLINE_CURVE_WITH_KNOTS('',3,(#149157,#149158,#149159,#149160,
#149161,#149162,#149163),.UNSPECIFIED.,.F.,.F.,(4,3,4),(0.561466076972731,
0.571428571428571,0.573654350219911),.UNSPECIFIED.);
#23583=B_SPLINE_CURVE_WITH_KNOTS('',3,(#149188,#149189,#149190,#149191,
#149192,#149193),.UNSPECIFIED.,.F.,.F.,(4,2,4),(1.43287852277096E-10,0.0126509723742098,
0.0253021873653449),.UNSPECIFIED.);
#23584=B_SPLINE_CURVE_WITH_KNOTS('',3,(#149200,#149201,#149202,#149203,
#149204,#149205,#149206),.UNSPECIFIED.,.F.,.F.,(4,3,4),(0.561466076975045,
0.571428571428571,0.573654350219911),.UNSPECIFIED.);
#23585=B_SPLINE_CURVE_WITH_KNOTS('',3,(#149231,#149232,#149233,#149234,
#149235,#149236),.UNSPECIFIED.,.F.,.F.,(4,2,4),(6.13476290471813E-12,0.012650972297768,
0.0253021873857862),.UNSPECIFIED.);
#23586=B_SPLINE_CURVE_WITH_KNOTS('',3,(#149243,#149244,#149245,#149246,
#149247,#149248,#149249),.UNSPECIFIED.,.F.,.F.,(4,3,4),(0.561466076967729,
0.571428571428571,0.573654350219911),.UNSPECIFIED.);
#23587=B_SPLINE_CURVE_WITH_KNOTS('',3,(#149274,#149275,#149276,#149277,
#149278,#149279),.UNSPECIFIED.,.F.,.F.,(4,2,4),(1.30084725401937E-10,0.0126509853979978,
0.0253022417622605),.UNSPECIFIED.);
#23588=B_SPLINE_CURVE_WITH_KNOTS('',3,(#149286,#149287,#149288,#149289,
#149290,#149291,#149292),.UNSPECIFIED.,.F.,.F.,(4,3,4),(0.561466076973636,
0.571428571428571,0.573654350219912),.UNSPECIFIED.);
#23589=B_SPLINE_CURVE_WITH_KNOTS('',3,(#149314,#149315,#149316,#149317,
#149318,#149319),.UNSPECIFIED.,.F.,.F.,(4,2,4),(5.6077424021607E-11,0.0126509723730836,
0.0253021874161603),.UNSPECIFIED.);
#23590=B_SPLINE_CURVE_WITH_KNOTS('',3,(#149345,#149346,#149347,#149348,
#149349,#149350),.UNSPECIFIED.,.F.,.F.,(4,2,4),(9.5934436762368E-11,0.0126509723665809,
0.0253021873569743),.UNSPECIFIED.);
#23591=B_SPLINE_CURVE_WITH_KNOTS('',3,(#149357,#149358,#149359,#149360,
#149361,#149362,#149363),.UNSPECIFIED.,.F.,.F.,(4,3,4),(0.561466076970824,
0.571428571428571,0.573654350219912),.UNSPECIFIED.);
#23592=B_SPLINE_CURVE_WITH_KNOTS('',3,(#149388,#149389,#149390,#149391,
#149392,#149393),.UNSPECIFIED.,.F.,.F.,(4,2,4),(0.,0.012650972289366,0.025302187368722),
 .UNSPECIFIED.);
#23593=B_SPLINE_CURVE_WITH_KNOTS('',3,(#149400,#149401,#149402,#149403,
#149404,#149405,#149406),.UNSPECIFIED.,.F.,.F.,(4,3,4),(0.561466076966466,
0.571428571428571,0.573654350219911),.UNSPECIFIED.);
#23594=B_SPLINE_CURVE_WITH_KNOTS('',3,(#149431,#149432,#149433,#149434,
#149435,#149436),.UNSPECIFIED.,.F.,.F.,(4,2,4),(2.03238081656241E-11,0.0126509859875903,
0.025302244503775),.UNSPECIFIED.);
#23595=B_SPLINE_CURVE_WITH_KNOTS('',3,(#149443,#149444,#149445,#149446,
#149447,#149448,#149449),.UNSPECIFIED.,.F.,.F.,(4,3,4),(0.561466076969195,
0.571428571428571,0.573654350219911),.UNSPECIFIED.);
#23596=B_SPLINE_CURVE_WITH_KNOTS('',3,(#149474,#149475,#149476,#149477,
#149478,#149479),.UNSPECIFIED.,.F.,.F.,(4,2,4),(7.54818598705809E-11,0.0126509724217488,
0.0253021872329842),.UNSPECIFIED.);
#23597=B_SPLINE_CURVE_WITH_KNOTS('',3,(#149492,#149493,#149494,#149495,
#149496,#149497,#149498),.UNSPECIFIED.,.F.,.F.,(4,3,4),(0.561466077,0.571428571428571,
0.573654350219911),.UNSPECIFIED.);
#23598=B_SPLINE_CURVE_WITH_KNOTS('',3,(#149518,#149519,#149520,#149521,
#149522,#149523),.UNSPECIFIED.,.F.,.F.,(4,2,4),(1.59968285071419E-10,0.0126509724314883,
0.0253021874246143),.UNSPECIFIED.);
#23599=B_SPLINE_CURVE_WITH_KNOTS('',3,(#149526,#149527,#149528,#149529,
#149530,#149531,#149532),.UNSPECIFIED.,.F.,.F.,(4,3,4),(0.561466076974998,
0.571428571428571,0.573654350219913),.UNSPECIFIED.);
#23600=B_SPLINE_CURVE_WITH_KNOTS('',3,(#149560,#149561,#149562,#149563,
#149564,#149565),.UNSPECIFIED.,.F.,.F.,(4,2,4),(0.,0.0126509723220439,0.0253021873975209),
 .UNSPECIFIED.);
#23601=B_SPLINE_CURVE_WITH_KNOTS('',3,(#149572,#149573,#149574,#149575,
#149576,#149577,#149578),.UNSPECIFIED.,.F.,.F.,(4,3,4),(0.561466076968925,
0.571428571428571,0.573654350219921),.UNSPECIFIED.);
#23602=B_SPLINE_CURVE_WITH_KNOTS('',3,(#149603,#149604,#149605,#149606,
#149607,#149608),.UNSPECIFIED.,.F.,.F.,(4,2,4),(3.40001431064816E-11,0.0126509723440331,
0.0253021873749516),.UNSPECIFIED.);
#23603=B_SPLINE_CURVE_WITH_KNOTS('',3,(#149615,#149616,#149617,#149618,
#149619,#149620,#149621),.UNSPECIFIED.,.F.,.F.,(4,3,4),(0.561466076968893,
0.571428571428571,0.57365435021992),.UNSPECIFIED.);
#23604=B_SPLINE_CURVE_WITH_KNOTS('',3,(#149646,#149647,#149648,#149649,
#149650,#149651),.UNSPECIFIED.,.F.,.F.,(4,2,4),(1.61417479377113E-10,0.0126509724299645,
0.025302187398691),.UNSPECIFIED.);
#23605=B_SPLINE_CURVE_WITH_KNOTS('',3,(#149658,#149659,#149660,#149661,
#149662,#149663,#149664),.UNSPECIFIED.,.F.,.F.,(4,3,4),(0.561466076970706,
0.571428571428571,0.573654350219922),.UNSPECIFIED.);
#23606=B_SPLINE_CURVE_WITH_KNOTS('',3,(#149689,#149690,#149691,#149692,
#149693,#149694),.UNSPECIFIED.,.F.,.F.,(4,2,4),(1.72077501315142E-11,0.0126509723056168,
0.0253021873602548),.UNSPECIFIED.);
#23607=B_SPLINE_CURVE_WITH_KNOTS('',3,(#149701,#149702,#149703,#149704,
#149705,#149706,#149707),.UNSPECIFIED.,.F.,.F.,(4,3,4),(0.561466076970486,
0.571428571428571,0.57365435021991),.UNSPECIFIED.);
#23608=B_SPLINE_CURVE_WITH_KNOTS('',3,(#149732,#149733,#149734,#149735,
#149736,#149737),.UNSPECIFIED.,.F.,.F.,(4,2,4),(0.,0.0126509722816313,0.0253021873170131),
 .UNSPECIFIED.);
#23609=B_SPLINE_CURVE_WITH_KNOTS('',3,(#149744,#149745,#149746,#149747,
#149748,#149749,#149750),.UNSPECIFIED.,.F.,.F.,(4,3,4),(0.561466076974285,
0.571428571428571,0.57365435021991),.UNSPECIFIED.);
#23610=B_SPLINE_CURVE_WITH_KNOTS('',3,(#149775,#149776,#149777,#149778,
#149779,#149780),.UNSPECIFIED.,.F.,.F.,(4,2,4),(1.75845480016369E-10,0.0126509724250738,
0.0253021874139565),.UNSPECIFIED.);
#23611=B_SPLINE_CURVE_WITH_KNOTS('',3,(#149787,#149788,#149789,#149790,
#149791,#149792,#149793),.UNSPECIFIED.,.F.,.F.,(4,3,4),(0.561466076973471,
0.571428571428571,0.57365435021991),.UNSPECIFIED.);
#23612=B_SPLINE_CURVE_WITH_KNOTS('',3,(#149818,#149819,#149820,#149821,
#149822,#149823),.UNSPECIFIED.,.F.,.F.,(4,2,4),(2.3529783390845E-11,0.0126509723223139,
0.0253021873783273),.UNSPECIFIED.);
#23613=B_SPLINE_CURVE_WITH_KNOTS('',3,(#149830,#149831,#149832,#149833,
#149834,#149835,#149836),.UNSPECIFIED.,.F.,.F.,(4,3,4),(0.561466076971879,
0.571428571428571,0.57365435021991),.UNSPECIFIED.);
#23614=B_SPLINE_CURVE_WITH_KNOTS('',3,(#149861,#149862,#149863,#149864,
#149865,#149866),.UNSPECIFIED.,.F.,.F.,(4,2,4),(4.81522774177321E-11,0.0126509851968905,
0.0253022411313395),.UNSPECIFIED.);
#23615=B_SPLINE_CURVE_WITH_KNOTS('',3,(#149873,#149874,#149875,#149876,
#149877,#149878,#149879),.UNSPECIFIED.,.F.,.F.,(4,3,4),(0.561466076969465,
0.571428571428571,0.57365435021991),.UNSPECIFIED.);
#23616=B_SPLINE_CURVE_WITH_KNOTS('',3,(#149904,#149905,#149906,#149907,
#149908,#149909),.UNSPECIFIED.,.F.,.F.,(4,2,4),(0.,0.0126509722877906,0.0253021873372228),
 .UNSPECIFIED.);
#23617=B_SPLINE_CURVE_WITH_KNOTS('',3,(#149916,#149917,#149918,#149919,
#149920,#149921,#149922),.UNSPECIFIED.,.F.,.F.,(4,3,4),(0.561466076971086,
0.571428571428571,0.57365435021991),.UNSPECIFIED.);
#23618=B_SPLINE_CURVE_WITH_KNOTS('',3,(#149948,#149949,#149950,#149951,
#149952,#149953),.UNSPECIFIED.,.F.,.F.,(4,2,4),(-0.0253038285839127,-0.0126520268760324,
0.),.UNSPECIFIED.);
#23619=B_SPLINE_CURVE_WITH_KNOTS('',3,(#149987,#149988,#149989,#149990,
#149991,#149992),.UNSPECIFIED.,.F.,.F.,(4,2,4),(-0.0253038286551005,-0.012652026917456,
0.),.UNSPECIFIED.);
#23620=B_SPLINE_CURVE_WITH_KNOTS('',3,(#150026,#150027,#150028,#150029,
#150030,#150031),.UNSPECIFIED.,.F.,.F.,(4,2,4),(-0.0253038285468146,-0.0126520268079982,
0.),.UNSPECIFIED.);
#23621=B_SPLINE_CURVE_WITH_KNOTS('',3,(#150065,#150066,#150067,#150068,
#150069,#150070),.UNSPECIFIED.,.F.,.F.,(4,2,4),(-0.0253038284106424,-0.0126520267846328,
-1.9438166354302E-11),.UNSPECIFIED.);
#23622=B_SPLINE_CURVE_WITH_KNOTS('',3,(#150104,#150105,#150106,#150107,
#150108,#150109),.UNSPECIFIED.,.F.,.F.,(4,2,4),(-0.0253038285523641,-0.0126520269075616,
-8.06536434860838E-12),.UNSPECIFIED.);
#23623=B_SPLINE_CURVE_WITH_KNOTS('',3,(#150143,#150144,#150145,#150146,
#150147,#150148),.UNSPECIFIED.,.F.,.F.,(4,2,4),(-0.0253038285807823,-0.012652026911929,
0.),.UNSPECIFIED.);
#23624=B_SPLINE_CURVE_WITH_KNOTS('',3,(#150182,#150183,#150184,#150185,
#150186,#150187),.UNSPECIFIED.,.F.,.F.,(4,2,4),(-0.0253038286017608,-0.0126520268893115,
0.),.UNSPECIFIED.);
#23625=B_SPLINE_CURVE_WITH_KNOTS('',3,(#150221,#150222,#150223,#150224,
#150225,#150226),.UNSPECIFIED.,.F.,.F.,(4,2,4),(-0.0253038285628698,-0.0126520269487189,
-1.01505019667325E-11),.UNSPECIFIED.);
#23626=B_SPLINE_CURVE_WITH_KNOTS('',3,(#150260,#150261,#150262,#150263,
#150264,#150265),.UNSPECIFIED.,.F.,.F.,(4,2,4),(-0.0253038284600093,-0.0126520268733603,
-1.30362942662998E-11),.UNSPECIFIED.);
#23627=B_SPLINE_CURVE_WITH_KNOTS('',3,(#150299,#150300,#150301,#150302,
#150303,#150304),.UNSPECIFIED.,.F.,.F.,(4,2,4),(-0.0253038285157797,-0.0126520268380531,
0.),.UNSPECIFIED.);
#23628=B_SPLINE_CURVE_WITH_KNOTS('',3,(#150338,#150339,#150340,#150341,
#150342,#150343),.UNSPECIFIED.,.F.,.F.,(4,2,4),(-0.025303828580961,-0.0126520268888839,
-3.22808793584706E-12),.UNSPECIFIED.);
#23629=B_SPLINE_CURVE_WITH_KNOTS('',3,(#150377,#150378,#150379,#150380,
#150381,#150382),.UNSPECIFIED.,.F.,.F.,(4,2,4),(-0.0253038285191941,-0.0126520268349931,
0.),.UNSPECIFIED.);
#23630=B_SPLINE_CURVE_WITH_KNOTS('',3,(#150416,#150417,#150418,#150419,
#150420,#150421),.UNSPECIFIED.,.F.,.F.,(4,2,4),(-0.025303828506458,-0.0126520269004065,
-1.72773739759435E-11),.UNSPECIFIED.);
#23631=B_SPLINE_CURVE_WITH_KNOTS('',3,(#150455,#150456,#150457,#150458,
#150459,#150460),.UNSPECIFIED.,.F.,.F.,(4,2,4),(-0.0253038286343293,-0.0126520268567648,
0.),.UNSPECIFIED.);
#23632=B_SPLINE_CURVE_WITH_KNOTS('',3,(#150494,#150495,#150496,#150497,
#150498,#150499),.UNSPECIFIED.,.F.,.F.,(4,2,4),(-0.0253038285556593,-0.0126520268415039,
0.),.UNSPECIFIED.);
#23633=B_SPLINE_CURVE_WITH_KNOTS('',3,(#150533,#150534,#150535,#150536,
#150537,#150538),.UNSPECIFIED.,.F.,.F.,(4,2,4),(-0.025303828616761,-0.0126520269208739,
0.),.UNSPECIFIED.);
#23634=B_SPLINE_CURVE_WITH_KNOTS('',3,(#150572,#150573,#150574,#150575,
#150576,#150577),.UNSPECIFIED.,.F.,.F.,(4,2,4),(-0.0253038284604553,-0.0126520268848923,
-1.02886171804428E-11),.UNSPECIFIED.);
#23635=B_SPLINE_CURVE_WITH_KNOTS('',3,(#150611,#150612,#150613,#150614,
#150615,#150616),.UNSPECIFIED.,.F.,.F.,(4,2,4),(-0.0253038286149417,-0.0126520269606899,
-3.53035656264211E-12),.UNSPECIFIED.);
#23636=B_SPLINE_CURVE_WITH_KNOTS('',3,(#150650,#150651,#150652,#150653,
#150654,#150655),.UNSPECIFIED.,.F.,.F.,(4,2,4),(-0.0253038284892162,-0.0126520268129704,
-2.58471022362983E-12),.UNSPECIFIED.);
#23637=B_SPLINE_CURVE_WITH_KNOTS('',3,(#150689,#150690,#150691,#150692,
#150693,#150694),.UNSPECIFIED.,.F.,.F.,(4,2,4),(-0.0253038284441624,-0.0126520268794058,
-1.13759314468442E-11),.UNSPECIFIED.);
#23638=B_SPLINE_CURVE_WITH_KNOTS('',3,(#150728,#150729,#150730,#150731,
#150732,#150733),.UNSPECIFIED.,.F.,.F.,(4,2,4),(-0.0253038285376909,-0.0126520268358134,
0.),.UNSPECIFIED.);
#23639=B_SPLINE_CURVE_WITH_KNOTS('',3,(#150764,#150765,#150766,#150767,
#150768,#150769),.UNSPECIFIED.,.F.,.F.,(4,2,4),(-0.0253038285032559,-0.0126520268449107,
-7.70856642406947E-12),.UNSPECIFIED.);
#23640=B_SPLINE_CURVE_WITH_KNOTS('',3,(#150791,#150792,#150793,#150794,
#150795,#150796),.UNSPECIFIED.,.F.,.F.,(4,2,4),(-0.0253038286446529,-0.0126520268985584,
0.),.UNSPECIFIED.);
#23641=B_SPLINE_CURVE_WITH_KNOTS('',3,(#150830,#150831,#150832,#150833,
#150834,#150835),.UNSPECIFIED.,.F.,.F.,(4,2,4),(-0.0253038286142863,-0.012652026982915,
-1.52916915241441E-12),.UNSPECIFIED.);
#23642=B_SPLINE_CURVE_WITH_KNOTS('',3,(#150869,#150870,#150871,#150872,
#150873,#150874),.UNSPECIFIED.,.F.,.F.,(4,2,4),(-0.0253038286058837,-0.0126520269289845,
0.),.UNSPECIFIED.);
#23643=B_SPLINE_CURVE_WITH_KNOTS('',3,(#150908,#150909,#150910,#150911,
#150912,#150913),.UNSPECIFIED.,.F.,.F.,(4,2,4),(-0.0253038285954271,-0.0126520269217119,
-3.19100648682458E-12),.UNSPECIFIED.);
#23644=B_SPLINE_CURVE_WITH_KNOTS('',3,(#150947,#150948,#150949,#150950,
#150951,#150952),.UNSPECIFIED.,.F.,.F.,(4,2,4),(-0.025303828457649,-0.0126520268415871,
-1.61810773113835E-11),.UNSPECIFIED.);
#23645=B_SPLINE_CURVE_WITH_KNOTS('',3,(#150986,#150987,#150988,#150989,
#150990,#150991),.UNSPECIFIED.,.F.,.F.,(4,2,4),(-0.0253038285087455,-0.0126520267988281,
0.),.UNSPECIFIED.);
#23646=B_SPLINE_CURVE_WITH_KNOTS('',3,(#151025,#151026,#151027,#151028,
#151029,#151030),.UNSPECIFIED.,.F.,.F.,(4,2,4),(-0.0253038285970617,-0.0126520269741822,
-1.24514287769273E-11),.UNSPECIFIED.);
#23647=B_SPLINE_CURVE_WITH_KNOTS('',3,(#151062,#151063,#151064,#151065,
#151066,#151067),.UNSPECIFIED.,.F.,.F.,(4,2,4),(-0.0240533908522633,-0.0122571958022784,
0.),.UNSPECIFIED.);
#23648=B_SPLINE_CURVE_WITH_KNOTS('',3,(#151091,#151092,#151093,#151094,
#151095,#151096),.UNSPECIFIED.,.F.,.F.,(4,2,4),(-0.0240535314783445,-0.0122572446394088,
0.),.UNSPECIFIED.);
#23649=B_SPLINE_CURVE_WITH_KNOTS('',3,(#151120,#151121,#151122,#151123,
#151124,#151125),.UNSPECIFIED.,.F.,.F.,(4,2,4),(-0.0240532016237181,-0.0122571280238569,
0.),.UNSPECIFIED.);
#23650=B_SPLINE_CURVE_WITH_KNOTS('',3,(#151149,#151150,#151151,#151152,
#151153,#151154),.UNSPECIFIED.,.F.,.F.,(4,2,4),(-0.0240533156711824,-0.0122571705517197,
0.),.UNSPECIFIED.);
#23651=B_SPLINE_CURVE_WITH_KNOTS('',3,(#151183,#151184,#151185,#151186,
#151187,#151188),.UNSPECIFIED.,.F.,.F.,(4,2,4),(-0.0240537809878963,-0.0122573306077586,
0.),.UNSPECIFIED.);
#23652=B_SPLINE_CURVE_WITH_KNOTS('',3,(#151217,#151218,#151219,#151220,
#151221,#151222),.UNSPECIFIED.,.F.,.F.,(4,2,4),(-0.024053361759142,-0.0122571855913509,
0.),.UNSPECIFIED.);
#23653=B_SPLINE_CURVE_WITH_KNOTS('',3,(#151246,#151247,#151248,#151249,
#151250,#151251),.UNSPECIFIED.,.F.,.F.,(4,2,4),(-0.0240534328364565,-0.0122572100588516,
0.),.UNSPECIFIED.);
#23654=B_SPLINE_CURVE_WITH_KNOTS('',3,(#151275,#151276,#151277,#151278,
#151279,#151280),.UNSPECIFIED.,.F.,.F.,(4,2,4),(-0.0240533728250536,-0.0122571910559405,
0.),.UNSPECIFIED.);
#23655=B_SPLINE_CURVE_WITH_KNOTS('',3,(#151304,#151305,#151306,#151307,
#151308,#151309),.UNSPECIFIED.,.F.,.F.,(4,2,4),(-0.0240533442755893,-0.0122571809828921,
0.),.UNSPECIFIED.);
#23656=B_SPLINE_CURVE_WITH_KNOTS('',3,(#151333,#151334,#151335,#151336,
#151337,#151338),.UNSPECIFIED.,.F.,.F.,(4,2,4),(-0.0240529243109103,-0.012257032788197,
0.),.UNSPECIFIED.);
#23657=B_SPLINE_CURVE_WITH_KNOTS('',3,(#151362,#151363,#151364,#151365,
#151366,#151367),.UNSPECIFIED.,.F.,.F.,(4,2,4),(-0.0240532082872642,-0.0122571342903452,
0.),.UNSPECIFIED.);
#23658=B_SPLINE_CURVE_WITH_KNOTS('',3,(#151396,#151397,#151398,#151399,
#151400,#151401),.UNSPECIFIED.,.F.,.F.,(4,2,4),(-0.0240534422631641,-0.0122572124745634,
0.),.UNSPECIFIED.);
#23659=B_SPLINE_CURVE_WITH_KNOTS('',3,(#151425,#151426,#151427,#151428,
#151429,#151430),.UNSPECIFIED.,.F.,.F.,(4,2,4),(-0.0240532828403448,-0.0122571585650213,
0.),.UNSPECIFIED.);
#23660=B_SPLINE_CURVE_WITH_KNOTS('',3,(#151454,#151455,#151456,#151457,
#151458,#151459),.UNSPECIFIED.,.F.,.F.,(4,2,4),(-0.0240534794813553,-0.0122572283945417,
0.),.UNSPECIFIED.);
#23661=B_SPLINE_CURVE_WITH_KNOTS('',3,(#151483,#151484,#151485,#151486,
#151487,#151488),.UNSPECIFIED.,.F.,.F.,(4,2,4),(-0.02405383490832,-0.012257350841524,
0.),.UNSPECIFIED.);
#23662=B_SPLINE_CURVE_WITH_KNOTS('',3,(#151517,#151518,#151519,#151520,
#151521,#151522),.UNSPECIFIED.,.F.,.F.,(4,2,4),(-0.0240530169280848,-0.0122570654448755,
0.),.UNSPECIFIED.);
#23663=B_SPLINE_CURVE_WITH_KNOTS('',3,(#151546,#151547,#151548,#151549,
#151550,#151551),.UNSPECIFIED.,.F.,.F.,(4,2,4),(-0.0240533479705919,-0.0122571825715407,
0.),.UNSPECIFIED.);
#23664=B_SPLINE_CURVE_WITH_KNOTS('',3,(#151575,#151576,#151577,#151578,
#151579,#151580),.UNSPECIFIED.,.F.,.F.,(4,2,4),(-0.024053311848544,-0.0122571689410321,
0.),.UNSPECIFIED.);
#23665=B_SPLINE_CURVE_WITH_KNOTS('',3,(#151604,#151605,#151606,#151607,
#151608,#151609),.UNSPECIFIED.,.F.,.F.,(4,2,4),(-0.0240533439257344,-0.012257179103354,
0.),.UNSPECIFIED.);
#23666=B_SPLINE_CURVE_WITH_KNOTS('',3,(#151633,#151634,#151635,#151636,
#151637,#151638),.UNSPECIFIED.,.F.,.F.,(4,2,4),(-0.0240530635024099,-0.0122570824968178,
0.),.UNSPECIFIED.);
#23667=B_SPLINE_CURVE_WITH_KNOTS('',3,(#151662,#151663,#151664,#151665,
#151666,#151667),.UNSPECIFIED.,.F.,.F.,(4,2,4),(-0.024053273040655,-0.0122571549226549,
0.),.UNSPECIFIED.);
#23668=B_SPLINE_CURVE_WITH_KNOTS('',3,(#151691,#151692,#151693,#151694,
#151695,#151696),.UNSPECIFIED.,.F.,.F.,(4,2,4),(-0.0240536699122217,-0.0122572931629393,
0.),.UNSPECIFIED.);
#23669=B_SPLINE_CURVE_WITH_KNOTS('',3,(#151720,#151721,#151722,#151723,
#151724,#151725),.UNSPECIFIED.,.F.,.F.,(4,2,4),(-0.0240536981873685,-0.0122573028539489,
0.),.UNSPECIFIED.);
#23670=B_SPLINE_CURVE_WITH_KNOTS('',3,(#151749,#151750,#151751,#151752,
#151753,#151754),.UNSPECIFIED.,.F.,.F.,(4,2,4),(-0.024053529185018,-0.0122572436632474,
0.),.UNSPECIFIED.);
#23671=B_SPLINE_CURVE_WITH_KNOTS('',3,(#151783,#151784,#151785,#151786,
#151787,#151788),.UNSPECIFIED.,.F.,.F.,(4,2,4),(-0.0240534288870408,-0.0122572093109304,
0.),.UNSPECIFIED.);
#23672=B_SPLINE_CURVE_WITH_KNOTS('',3,(#151812,#151813,#151814,#151815,
#151816,#151817),.UNSPECIFIED.,.F.,.F.,(4,2,4),(-0.0240537713625275,-0.0122573281131518,
0.),.UNSPECIFIED.);
#23673=B_SPLINE_CURVE_WITH_KNOTS('',3,(#151841,#151842,#151843,#151844,
#151845,#151846),.UNSPECIFIED.,.F.,.F.,(4,2,4),(-0.0240533351661113,-0.0122571766305564,
0.),.UNSPECIFIED.);
#23674=B_SPLINE_CURVE_WITH_KNOTS('',3,(#151870,#151871,#151872,#151873,
#151874,#151875),.UNSPECIFIED.,.F.,.F.,(4,2,4),(-0.024054081148553,-0.0122574351715113,
0.),.UNSPECIFIED.);
#23675=B_SPLINE_CURVE_WITH_KNOTS('',3,(#151899,#151900,#151901,#151902,
#151903,#151904),.UNSPECIFIED.,.F.,.F.,(4,2,4),(-0.0240530980436435,-0.0122570945679079,
0.),.UNSPECIFIED.);
#23676=B_SPLINE_CURVE_WITH_KNOTS('',3,(#152515,#152516,#152517,#152518,
#152519,#152520),.UNSPECIFIED.,.F.,.F.,(4,2,4),(3.48126610442943E-11,0.0126485446413335,
0.025296968417101),.UNSPECIFIED.);
#23677=B_SPLINE_CURVE_WITH_KNOTS('',3,(#152538,#152539,#152540,#152541,
#152542,#152543),.UNSPECIFIED.,.F.,.F.,(4,2,4),(-0.0252968472729343,-0.0126485446090834,
-2.17366402655017E-11),.UNSPECIFIED.);
#23678=B_SPLINE_CURVE_WITH_KNOTS('',3,(#152579,#152580,#152581,#152582,
#152583,#152584),.UNSPECIFIED.,.F.,.F.,(4,2,4),(-0.0252968473826894,-0.0126485446000957,
-2.0234428715904E-11),.UNSPECIFIED.);
#23679=B_SPLINE_CURVE_WITH_KNOTS('',3,(#152620,#152621,#152622,#152623,
#152624,#152625),.UNSPECIFIED.,.F.,.F.,(4,2,4),(-0.0252968472290505,-0.0126485446178443,
-1.42757888843548E-11),.UNSPECIFIED.);
#23680=B_SPLINE_CURVE_WITH_KNOTS('',3,(#152661,#152662,#152663,#152664,
#152665,#152666),.UNSPECIFIED.,.F.,.F.,(4,2,4),(-0.0252968474456481,-0.0126485446475364,
-3.50366680113012E-11),.UNSPECIFIED.);
#23681=B_SPLINE_CURVE_WITH_KNOTS('',3,(#152702,#152703,#152704,#152705,
#152706,#152707),.UNSPECIFIED.,.F.,.F.,(4,2,4),(-0.0252969813766171,-0.0126485446434368,
-3.20461539249361E-11),.UNSPECIFIED.);
#23682=B_SPLINE_CURVE_WITH_KNOTS('',3,(#152743,#152744,#152745,#152746,
#152747,#152748),.UNSPECIFIED.,.F.,.F.,(4,2,4),(-0.0252969778573368,-0.0126485446281753,
-2.83896205155454E-11),.UNSPECIFIED.);
#23683=B_SPLINE_CURVE_WITH_KNOTS('',3,(#152781,#152782,#152783,#152784,
#152785,#152786),.UNSPECIFIED.,.F.,.F.,(4,2,4),(-0.0252969796412403,-0.0126485446363986,
-3.44679423891492E-11),.UNSPECIFIED.);
#23684=B_SPLINE_CURVE_WITH_KNOTS('',3,(#152816,#152817,#152818,#152819,
#152820,#152821),.UNSPECIFIED.,.F.,.F.,(4,2,4),(-0.0252969759465009,-0.0126485445986618,
0.),.UNSPECIFIED.);
#23685=B_SPLINE_CURVE_WITH_KNOTS('',3,(#152857,#152858,#152859,#152860,
#152861,#152862),.UNSPECIFIED.,.F.,.F.,(4,2,4),(-0.0252969599122676,-0.0126485446559965,
-2.64061897348178E-11),.UNSPECIFIED.);
#23686=B_SPLINE_CURVE_WITH_KNOTS('',3,(#152898,#152899,#152900,#152901,
#152902,#152903),.UNSPECIFIED.,.F.,.F.,(4,2,4),(-0.0252968474027855,-0.0126485446051056,
0.),.UNSPECIFIED.);
#23687=B_SPLINE_CURVE_WITH_KNOTS('',3,(#152939,#152940,#152941,#152942,
#152943,#152944),.UNSPECIFIED.,.F.,.F.,(4,2,4),(-0.0252969724871208,-0.0126485446152108,
0.),.UNSPECIFIED.);
#23688=B_SPLINE_CURVE_WITH_KNOTS('',3,(#152980,#152981,#152982,#152983,
#152984,#152985),.UNSPECIFIED.,.F.,.F.,(4,2,4),(-0.0252969815801744,-0.0126485446478389,
-3.94803981174086E-11),.UNSPECIFIED.);
#23689=B_SPLINE_CURVE_WITH_KNOTS('',3,(#153021,#153022,#153023,#153024,
#153025,#153026),.UNSPECIFIED.,.F.,.F.,(4,2,4),(-0.0252968472773642,-0.0126485446695086,
-5.66388602685208E-11),.UNSPECIFIED.);
#23690=B_SPLINE_CURVE_WITH_KNOTS('',3,(#153062,#153063,#153064,#153065,
#153066,#153067),.UNSPECIFIED.,.F.,.F.,(4,2,4),(-0.0252968473121451,-0.0126485446154412,
-1.1150868423071E-11),.UNSPECIFIED.);
#23691=B_SPLINE_CURVE_WITH_KNOTS('',3,(#153103,#153104,#153105,#153106,
#153107,#153108),.UNSPECIFIED.,.F.,.F.,(4,2,4),(-0.025296847243463,-0.0126485446122804,
-1.33509418798194E-11),.UNSPECIFIED.);
#23692=B_SPLINE_CURVE_WITH_KNOTS('',3,(#153144,#153145,#153146,#153147,
#153148,#153149),.UNSPECIFIED.,.F.,.F.,(4,2,4),(-0.0252968474367496,-0.0126485446764713,
-6.67833600920265E-11),.UNSPECIFIED.);
#23693=B_SPLINE_CURVE_WITH_KNOTS('',3,(#153185,#153186,#153187,#153188,
#153189,#153190),.UNSPECIFIED.,.F.,.F.,(4,2,4),(-0.0252968473967678,-0.0126485446111826,
-2.20091098124264E-11),.UNSPECIFIED.);
#23694=B_SPLINE_CURVE_WITH_KNOTS('',3,(#153226,#153227,#153228,#153229,
#153230,#153231),.UNSPECIFIED.,.F.,.F.,(4,2,4),(-0.025296977282385,-0.0126485447145659,
-8.45704270502345E-11),.UNSPECIFIED.);
#23695=B_SPLINE_CURVE_WITH_KNOTS('',3,(#153268,#153269,#153270,#153271,
#153272,#153273),.UNSPECIFIED.,.F.,.F.,(4,2,4),(-0.0252969810914952,-0.0126485446316171,
-2.47067262482137E-11),.UNSPECIFIED.);
#23696=B_SPLINE_CURVE_WITH_KNOTS('',3,(#153308,#153309,#153310,#153311,
#153312,#153313),.UNSPECIFIED.,.F.,.F.,(4,2,4),(-0.0252968472556989,-0.0126485446070453,
0.),.UNSPECIFIED.);
#23697=B_SPLINE_CURVE_WITH_KNOTS('',3,(#153349,#153350,#153351,#153352,
#153353,#153354),.UNSPECIFIED.,.F.,.F.,(4,2,4),(-0.0252969788338113,-0.0126485446612997,
-3.58097579367112E-11),.UNSPECIFIED.);
#23698=B_SPLINE_CURVE_WITH_KNOTS('',3,(#153390,#153391,#153392,#153393,
#153394,#153395),.UNSPECIFIED.,.F.,.F.,(4,2,4),(-0.0252969664419228,-0.012648544666138,
-3.73045691559604E-11),.UNSPECIFIED.);
#23699=B_SPLINE_CURVE_WITH_KNOTS('',3,(#153431,#153432,#153433,#153434,
#153435,#153436),.UNSPECIFIED.,.F.,.F.,(4,2,4),(-0.0252968473797348,-0.0126485446073801,
-2.24880981891662E-11),.UNSPECIFIED.);
#23700=B_SPLINE_CURVE_WITH_KNOTS('',3,(#153472,#153473,#153474,#153475,
#153476,#153477),.UNSPECIFIED.,.F.,.F.,(4,2,4),(-0.0252968473839868,-0.0126485445770089,
0.),.UNSPECIFIED.);
#23701=B_SPLINE_CURVE_WITH_KNOTS('',3,(#153513,#153514,#153515,#153516,
#153517,#153518),.UNSPECIFIED.,.F.,.F.,(4,2,4),(-0.0252968472873195,-0.0126485445945012,
-1.47688701546134E-11),.UNSPECIFIED.);
#23702=B_SPLINE_CURVE_WITH_KNOTS('',3,(#153554,#153555,#153556,#153557,
#153558,#153559),.UNSPECIFIED.,.F.,.F.,(4,2,4),(-0.0252969824708076,-0.0126485446988715,
-7.00456255497972E-11),.UNSPECIFIED.);
#23703=B_SPLINE_CURVE_WITH_KNOTS('',3,(#153595,#153596,#153597,#153598,
#153599,#153600),.UNSPECIFIED.,.F.,.F.,(4,2,4),(-0.0252968472865847,-0.0126485446264394,
-2.50634790699422E-11),.UNSPECIFIED.);
#23704=B_SPLINE_CURVE_WITH_KNOTS('',3,(#153636,#153637,#153638,#153639,
#153640,#153641),.UNSPECIFIED.,.F.,.F.,(4,2,4),(-0.0252969705196494,-0.012648544669824,
-3.72970924977789E-11),.UNSPECIFIED.);
#23705=B_SPLINE_CURVE_WITH_KNOTS('',3,(#153691,#153692,#153693,#153694,
#153695,#153696),.UNSPECIFIED.,.F.,.F.,(4,2,4),(0.,0.0141859771214826,0.0270902355424121),
 .UNSPECIFIED.);
#23706=B_SPLINE_CURVE_WITH_KNOTS('',3,(#153698,#153699,#153700,#153701,
#153702,#153703),.UNSPECIFIED.,.F.,.F.,(4,2,4),(0.000841213375608474,0.0328420548602157,
0.0646443104438985),.UNSPECIFIED.);
#23707=B_SPLINE_CURVE_WITH_KNOTS('',3,(#153717,#153718,#153719,#153720,
#153721,#153722),.UNSPECIFIED.,.F.,.F.,(4,2,4),(0.,0.0322203315702454,0.0646290661358398),
 .UNSPECIFIED.);
#23708=B_SPLINE_CURVE_WITH_KNOTS('',3,(#153723,#153724,#153725,#153726,
#153727,#153728),.UNSPECIFIED.,.F.,.F.,(4,2,4),(-0.0270903064616207,-0.014186058870529,
0.),.UNSPECIFIED.);
#23709=B_SPLINE_CURVE_WITH_KNOTS('',3,(#153731,#153732,#153733,#153734,
#153735,#153736,#153737,#153738),.UNSPECIFIED.,.F.,.F.,(4,2,2,4),(1.00000000424066E-6,
0.032117316005638,0.0481218021713528,0.0656773383786918),.UNSPECIFIED.);
#23710=B_SPLINE_CURVE_WITH_KNOTS('',3,(#153740,#153741,#153742,#153743,
#153744,#153745,#153746,#153747),.UNSPECIFIED.,.F.,.F.,(4,2,2,4),(1.00008813714387E-6,
0.0149899305188782,0.0288003387031098,0.056524442103007),.UNSPECIFIED.);
#23711=B_SPLINE_CURVE_WITH_KNOTS('',3,(#153748,#153749,#153750,#153751,
#153752,#153753),.UNSPECIFIED.,.F.,.F.,(4,2,4),(0.000841212496343715,0.0328420540155859,
0.0646443074565014),.UNSPECIFIED.);
#23712=B_SPLINE_CURVE_WITH_KNOTS('',3,(#153776,#153777,#153778,#153779,
#153780,#153781),.UNSPECIFIED.,.F.,.F.,(4,2,4),(0.,0.0322203314085649,0.0646290655094404),
 .UNSPECIFIED.);
#23713=B_SPLINE_CURVE_WITH_KNOTS('',3,(#153782,#153783,#153784,#153785,
#153786,#153787),.UNSPECIFIED.,.F.,.F.,(4,2,4),(-0.0270903064315289,-0.0141860587887412,
0.),.UNSPECIFIED.);
#23714=B_SPLINE_CURVE_WITH_KNOTS('',3,(#153790,#153791,#153792,#153793,
#153794,#153795,#153796,#153797),.UNSPECIFIED.,.F.,.F.,(4,2,2,4),(1.00000000422679E-6,
0.0321173159964771,0.0481218021303975,0.0656773382668063),.UNSPECIFIED.);
#23715=B_SPLINE_CURVE_WITH_KNOTS('',3,(#153799,#153800,#153801,#153802,
#153803,#153804,#153805,#153806),.UNSPECIFIED.,.F.,.F.,(4,2,2,4),(1.00015504287392E-6,
0.0149898933241323,0.028800226478695,0.0565241789207558),.UNSPECIFIED.);
#23716=B_SPLINE_CURVE_WITH_KNOTS('',3,(#153807,#153808,#153809,#153810,
#153811,#153812),.UNSPECIFIED.,.F.,.F.,(4,2,4),(0.000841212499847193,0.0328420540711237,
0.0646443098284148),.UNSPECIFIED.);
#23717=B_SPLINE_CURVE_WITH_KNOTS('',3,(#153835,#153836,#153837,#153838,
#153839,#153840),.UNSPECIFIED.,.F.,.F.,(4,2,4),(0.,0.0322203310170438,0.0646290639830013),
 .UNSPECIFIED.);
#23718=B_SPLINE_CURVE_WITH_KNOTS('',3,(#153841,#153842,#153843,#153844,
#153845,#153846),.UNSPECIFIED.,.F.,.F.,(4,2,4),(-0.0270903065350147,-0.0141860589225805,
0.),.UNSPECIFIED.);
#23719=B_SPLINE_CURVE_WITH_KNOTS('',3,(#153849,#153850,#153851,#153852,
#153853,#153854,#153855,#153856),.UNSPECIFIED.,.F.,.F.,(4,2,2,4),(1.00000000426148E-6,
0.0321173161023142,0.0481218022823433,0.0656773384116248),.UNSPECIFIED.);
#23720=B_SPLINE_CURVE_WITH_KNOTS('',3,(#153858,#153859,#153860,#153861,
#153862,#153863,#153864,#153865),.UNSPECIFIED.,.F.,.F.,(4,2,2,4),(1.00011528535774E-6,
0.014989896815884,0.0288002355221683,0.0565241993123861),.UNSPECIFIED.);
#23721=B_SPLINE_CURVE_WITH_KNOTS('',3,(#153866,#153867,#153868,#153869,
#153870,#153871),.UNSPECIFIED.,.F.,.F.,(4,2,4),(0.000841212480934865,0.032842054020484,
0.0646443080313221),.UNSPECIFIED.);
#23722=B_SPLINE_CURVE_WITH_KNOTS('',3,(#153894,#153895,#153896,#153897,
#153898,#153899),.UNSPECIFIED.,.F.,.F.,(4,2,4),(0.,0.0322203315669168,0.0646290661501098),
 .UNSPECIFIED.);
#23723=B_SPLINE_CURVE_WITH_KNOTS('',3,(#153900,#153901,#153902,#153903,
#153904,#153905),.UNSPECIFIED.,.F.,.F.,(4,2,4),(-0.0270903064252968,-0.0141860587916916,
0.),.UNSPECIFIED.);
#23724=B_SPLINE_CURVE_WITH_KNOTS('',3,(#153908,#153909,#153910,#153911,
#153912,#153913,#153914,#153915),.UNSPECIFIED.,.F.,.F.,(4,2,2,4),(1.00000000436556E-6,
0.0321173160280198,0.0481218021977914,0.0656773383565895),.UNSPECIFIED.);
#23725=B_SPLINE_CURVE_WITH_KNOTS('',3,(#153917,#153918,#153919,#153920,
#153921,#153922,#153923,#153924),.UNSPECIFIED.,.F.,.F.,(4,2,2,4),(1.00011613791014E-6,
0.0149899423335993,0.0288003757402801,0.0565245295965229),.UNSPECIFIED.);
#23726=B_SPLINE_CURVE_WITH_KNOTS('',3,(#153925,#153926,#153927,#153928,
#153929,#153930),.UNSPECIFIED.,.F.,.F.,(4,2,4),(0.00084121251482112,0.0328420540437307,
0.0646443075511192),.UNSPECIFIED.);
#23727=B_SPLINE_CURVE_WITH_KNOTS('',3,(#153953,#153954,#153955,#153956,
#153957,#153958),.UNSPECIFIED.,.F.,.F.,(4,2,4),(0.,0.0322203311065635,0.0646290643975586),
 .UNSPECIFIED.);
#23728=B_SPLINE_CURVE_WITH_KNOTS('',3,(#153959,#153960,#153961,#153962,
#153963,#153964),.UNSPECIFIED.,.F.,.F.,(4,2,4),(-0.0270903064149145,-0.0141860587690414,
0.),.UNSPECIFIED.);
#23729=B_SPLINE_CURVE_WITH_KNOTS('',3,(#153967,#153968,#153969,#153970,
#153971,#153972,#153973,#153974),.UNSPECIFIED.,.F.,.F.,(4,2,2,4),(1.00000000421291E-6,
0.0321173160083687,0.0481218021505993,0.0656773382163755),.UNSPECIFIED.);
#23730=B_SPLINE_CURVE_WITH_KNOTS('',3,(#153976,#153977,#153978,#153979,
#153980,#153981,#153982,#153983),.UNSPECIFIED.,.F.,.F.,(4,2,2,4),(1.0001428935229E-6,
0.0149898839800048,0.0288001961576573,0.0565241066066853),.UNSPECIFIED.);
#23731=B_SPLINE_CURVE_WITH_KNOTS('',3,(#153984,#153985,#153986,#153987,
#153988,#153989),.UNSPECIFIED.,.F.,.F.,(4,2,4),(0.000841212502526919,0.0328420540695526,
0.0646443094065842),.UNSPECIFIED.);
#23732=B_SPLINE_CURVE_WITH_KNOTS('',3,(#154012,#154013,#154014,#154015,
#154016,#154017),.UNSPECIFIED.,.F.,.F.,(4,2,4),(0.,0.0322203309313174,0.0646290637295966),
 .UNSPECIFIED.);
#23733=B_SPLINE_CURVE_WITH_KNOTS('',3,(#154018,#154019,#154020,#154021,
#154022,#154023),.UNSPECIFIED.,.F.,.F.,(4,2,4),(-0.0270903064312433,-0.0141860588372105,
0.),.UNSPECIFIED.);
#23734=B_SPLINE_CURVE_WITH_KNOTS('',3,(#154026,#154027,#154028,#154029,
#154030,#154031,#154032,#154033),.UNSPECIFIED.,.F.,.F.,(4,2,2,4),(1.00000000408107E-6,
0.0321173160914473,0.0481218022691526,0.06567733839924),.UNSPECIFIED.);
#23735=B_SPLINE_CURVE_WITH_KNOTS('',3,(#154035,#154036,#154037,#154038,
#154039,#154040,#154041,#154042),.UNSPECIFIED.,.F.,.F.,(4,2,2,4),(1.00014860399301E-6,
0.0149899446057504,0.0288003809775306,0.0565245409726297),.UNSPECIFIED.);
#23736=B_SPLINE_CURVE_WITH_KNOTS('',3,(#154043,#154044,#154045,#154046,
#154047,#154048),.UNSPECIFIED.,.F.,.F.,(4,2,4),(0.000841212512306117,0.0328420540410832,
0.0646443079873795),.UNSPECIFIED.);
#23737=B_SPLINE_CURVE_WITH_KNOTS('',3,(#154071,#154072,#154073,#154074,
#154075,#154076),.UNSPECIFIED.,.F.,.F.,(4,2,4),(0.,0.0322203316998426,0.0646290664672489),
 .UNSPECIFIED.);
#23738=B_SPLINE_CURVE_WITH_KNOTS('',3,(#154077,#154078,#154079,#154080,
#154081,#154082),.UNSPECIFIED.,.F.,.F.,(4,2,4),(-0.0270903064584401,-0.0141860588669718,
0.),.UNSPECIFIED.);
#23739=B_SPLINE_CURVE_WITH_KNOTS('',3,(#154085,#154086,#154087,#154088,
#154089,#154090,#154091,#154092),.UNSPECIFIED.,.F.,.F.,(4,2,2,4),(1.00000000417821E-6,
0.0321173160331573,0.0481218022107658,0.0656773383904979),.UNSPECIFIED.);
#23740=B_SPLINE_CURVE_WITH_KNOTS('',3,(#154094,#154095,#154096,#154097,
#154098,#154099,#154100,#154101),.UNSPECIFIED.,.F.,.F.,(4,2,2,4),(1.00017459187543E-6,
0.0149899208702244,0.0288003107957597,0.0565243773111484),.UNSPECIFIED.);
#23741=B_SPLINE_CURVE_WITH_KNOTS('',3,(#154102,#154103,#154104,#154105,
#154106,#154107),.UNSPECIFIED.,.F.,.F.,(4,2,4),(0.000841212498535907,0.0328420540394922,
0.0646443082333259),.UNSPECIFIED.);
#23742=B_SPLINE_CURVE_WITH_KNOTS('',3,(#154130,#154131,#154132,#154133,
#154134,#154135),.UNSPECIFIED.,.F.,.F.,(4,2,4),(0.,0.0322203315803248,0.0646290661264063),
 .UNSPECIFIED.);
#23743=B_SPLINE_CURVE_WITH_KNOTS('',3,(#154136,#154137,#154138,#154139,
#154140,#154141),.UNSPECIFIED.,.F.,.F.,(4,2,4),(-0.0270903065107537,-0.0141860588988156,
0.),.UNSPECIFIED.);
#23744=B_SPLINE_CURVE_WITH_KNOTS('',3,(#154144,#154145,#154146,#154147,
#154148,#154149,#154150,#154151),.UNSPECIFIED.,.F.,.F.,(4,2,2,4),(1.00000000423373E-6,
0.0321173160269704,0.048121802160199,0.0656773383201519),.UNSPECIFIED.);
#23745=B_SPLINE_CURVE_WITH_KNOTS('',3,(#154153,#154154,#154155,#154156,
#154157,#154158,#154159,#154160),.UNSPECIFIED.,.F.,.F.,(4,2,2,4),(1.00013892581745E-6,
0.0149899181546202,0.0288003020884492,0.0565243566919721),.UNSPECIFIED.);
#23746=B_SPLINE_CURVE_WITH_KNOTS('',3,(#154161,#154162,#154163,#154164,
#154165,#154166),.UNSPECIFIED.,.F.,.F.,(4,2,4),(0.000841212508110519,0.0328420540551423,
0.0646443085644263),.UNSPECIFIED.);
#23747=B_SPLINE_CURVE_WITH_KNOTS('',3,(#154189,#154190,#154191,#154192,
#154193,#154194),.UNSPECIFIED.,.F.,.F.,(4,2,4),(0.,0.0322203310983203,0.0646290643108364),
 .UNSPECIFIED.);
#23748=B_SPLINE_CURVE_WITH_KNOTS('',3,(#154195,#154196,#154197,#154198,
#154199,#154200),.UNSPECIFIED.,.F.,.F.,(4,2,4),(-0.0270903065126501,-0.0141860589068631,
0.),.UNSPECIFIED.);
#23749=B_SPLINE_CURVE_WITH_KNOTS('',3,(#154203,#154204,#154205,#154206,
#154207,#154208,#154209,#154210),.UNSPECIFIED.,.F.,.F.,(4,2,2,4),(1.00000000422679E-6,
0.0321173160957739,0.0481218023156141,0.0656773385260134),.UNSPECIFIED.);
#23750=B_SPLINE_CURVE_WITH_KNOTS('',3,(#154212,#154213,#154214,#154215,
#154216,#154217,#154218,#154219),.UNSPECIFIED.,.F.,.F.,(4,2,2,4),(1.00012353586113E-6,
0.0149899334156635,0.0288003481710984,0.0565244646056971),.UNSPECIFIED.);
#23751=B_SPLINE_CURVE_WITH_KNOTS('',3,(#154220,#154221,#154222,#154223,
#154224,#154225),.UNSPECIFIED.,.F.,.F.,(4,2,4),(0.000841212516248009,0.0328420540304007,
0.0646443083551271),.UNSPECIFIED.);
#23752=B_SPLINE_CURVE_WITH_KNOTS('',3,(#154248,#154249,#154250,#154251,
#154252,#154253),.UNSPECIFIED.,.F.,.F.,(4,2,4),(0.,0.0322203320530467,0.0646290679305432),
 .UNSPECIFIED.);
#23753=B_SPLINE_CURVE_WITH_KNOTS('',3,(#154254,#154255,#154256,#154257,
#154258,#154259),.UNSPECIFIED.,.F.,.F.,(4,2,4),(-0.0270903065054314,-0.0141860589103654,
0.),.UNSPECIFIED.);
#23754=B_SPLINE_CURVE_WITH_KNOTS('',3,(#154262,#154263,#154264,#154265,
#154266,#154267,#154268,#154269),.UNSPECIFIED.,.F.,.F.,(4,2,2,4),(1.00000000442801E-6,
0.032117316028803,0.0481218021765062,0.0656773384184277),.UNSPECIFIED.);
#23755=B_SPLINE_CURVE_WITH_KNOTS('',3,(#154271,#154272,#154273,#154274,
#154275,#154276,#154277,#154278),.UNSPECIFIED.,.F.,.F.,(4,2,2,4),(1.00016980558116E-6,
0.014989959175291,0.0288004270714822,0.0565246501588951),.UNSPECIFIED.);
#23756=B_SPLINE_CURVE_WITH_KNOTS('',3,(#154279,#154280,#154281,#154282,
#154283,#154284),.UNSPECIFIED.,.F.,.F.,(4,2,4),(0.000841212498799183,0.0328420540437319,
0.064644307927571),.UNSPECIFIED.);
#23757=B_SPLINE_CURVE_WITH_KNOTS('',3,(#154307,#154308,#154309,#154310,
#154311,#154312),.UNSPECIFIED.,.F.,.F.,(4,2,4),(0.,0.0322203314745356,0.0646290658004266),
 .UNSPECIFIED.);
#23758=B_SPLINE_CURVE_WITH_KNOTS('',3,(#154313,#154314,#154315,#154316,
#154317,#154318),.UNSPECIFIED.,.F.,.F.,(4,2,4),(-0.0270903064921837,-0.0141860588757323,
0.),.UNSPECIFIED.);
#23759=B_SPLINE_CURVE_WITH_KNOTS('',3,(#154321,#154322,#154323,#154324,
#154325,#154326,#154327,#154328),.UNSPECIFIED.,.F.,.F.,(4,2,2,4),(1.00000000403944E-6,
0.0321173159942312,0.0481218021528757,0.0656773383460366),.UNSPECIFIED.);
#23760=B_SPLINE_CURVE_WITH_KNOTS('',3,(#154330,#154331,#154332,#154333,
#154334,#154335,#154336,#154337),.UNSPECIFIED.,.F.,.F.,(4,2,2,4),(1.00021693869851E-6,
0.0149899233812258,0.0288003179063593,0.0565243937091347),.UNSPECIFIED.);
#23761=B_SPLINE_CURVE_WITH_KNOTS('',3,(#154338,#154339,#154340,#154341,
#154342,#154343),.UNSPECIFIED.,.F.,.F.,(4,2,4),(0.000841212519676827,0.0328420540777682,
0.0646443087952493),.UNSPECIFIED.);
#23762=B_SPLINE_CURVE_WITH_KNOTS('',3,(#154366,#154367,#154368,#154369,
#154370,#154371),.UNSPECIFIED.,.F.,.F.,(4,2,4),(0.,0.032220330961457,0.0646290638718947),
 .UNSPECIFIED.);
#23763=B_SPLINE_CURVE_WITH_KNOTS('',3,(#154372,#154373,#154374,#154375,
#154376,#154377),.UNSPECIFIED.,.F.,.F.,(4,2,4),(-0.0270903064237865,-0.0141860588161846,
0.),.UNSPECIFIED.);
#23764=B_SPLINE_CURVE_WITH_KNOTS('',3,(#154380,#154381,#154382,#154383,
#154384,#154385,#154386,#154387),.UNSPECIFIED.,.F.,.F.,(4,2,2,4),(1.00000000397005E-6,
0.0321173160729806,0.0481218022715349,0.0656773384478732),.UNSPECIFIED.);
#23765=B_SPLINE_CURVE_WITH_KNOTS('',3,(#154389,#154390,#154391,#154392,
#154393,#154394,#154395,#154396),.UNSPECIFIED.,.F.,.F.,(4,2,2,4),(1.00015850917621E-6,
0.0149899557945825,0.0288004171433498,0.0565246271762989),.UNSPECIFIED.);
#23766=B_SPLINE_CURVE_WITH_KNOTS('',3,(#154397,#154398,#154399,#154400,
#154401,#154402),.UNSPECIFIED.,.F.,.F.,(4,2,4),(0.000841212520024779,0.0328420540605427,
0.0646443083686256),.UNSPECIFIED.);
#23767=B_SPLINE_CURVE_WITH_KNOTS('',3,(#154425,#154426,#154427,#154428,
#154429,#154430),.UNSPECIFIED.,.F.,.F.,(4,2,4),(0.,0.0322203316707932,0.0646290665533952),
 .UNSPECIFIED.);
#23768=B_SPLINE_CURVE_WITH_KNOTS('',3,(#154431,#154432,#154433,#154434,
#154435,#154436),.UNSPECIFIED.,.F.,.F.,(4,2,4),(-0.0270903063691943,-0.0141860587297742,
0.),.UNSPECIFIED.);
#23769=B_SPLINE_CURVE_WITH_KNOTS('',3,(#154439,#154440,#154441,#154442,
#154443,#154444,#154445,#154446),.UNSPECIFIED.,.F.,.F.,(4,2,2,4),(1.00000000397699E-6,
0.0321173160397508,0.0481218022104113,0.0656773383873906),.UNSPECIFIED.);
#23770=B_SPLINE_CURVE_WITH_KNOTS('',3,(#154448,#154449,#154450,#154451,
#154452,#154453,#154454,#154455),.UNSPECIFIED.,.F.,.F.,(4,2,2,4),(1.00009241193544E-6,
0.0149899114490231,0.0288002806104871,0.0565243055933151),.UNSPECIFIED.);
#23771=B_SPLINE_CURVE_WITH_KNOTS('',3,(#154456,#154457,#154458,#154459,
#154460,#154461),.UNSPECIFIED.,.F.,.F.,(4,2,4),(0.000841212507969122,0.0328420540427537,
0.0646443075038919),.UNSPECIFIED.);
#23772=B_SPLINE_CURVE_WITH_KNOTS('',3,(#154482,#154483,#154484,#154485,
#154486,#154487),.UNSPECIFIED.,.F.,.F.,(4,2,4),(-0.027090306535355,-0.0141860588953685,
0.),.UNSPECIFIED.);
#23773=B_SPLINE_CURVE_WITH_KNOTS('',3,(#154510,#154511,#154512,#154513,
#154514,#154515),.UNSPECIFIED.,.F.,.F.,(4,2,4),(0.,0.0322203315533029,0.0646290660316353),
 .UNSPECIFIED.);
#23774=B_SPLINE_CURVE_WITH_KNOTS('',3,(#154516,#154517,#154518,#154519,
#154520,#154521),.UNSPECIFIED.,.F.,.F.,(4,2,4),(-0.0270903064994476,-0.0141860588902063,
0.),.UNSPECIFIED.);
#23775=B_SPLINE_CURVE_WITH_KNOTS('',3,(#154524,#154525,#154526,#154527,
#154528,#154529,#154530,#154531),.UNSPECIFIED.,.F.,.F.,(4,2,2,4),(1.00000000449046E-6,
0.0321173160115672,0.0481218021634407,0.0656773383366627),.UNSPECIFIED.);
#23776=B_SPLINE_CURVE_WITH_KNOTS('',3,(#154533,#154534,#154535,#154536,
#154537,#154538,#154539,#154540),.UNSPECIFIED.,.F.,.F.,(4,2,2,4),(1.00012267353931E-6,
0.0149899195388564,0.0288003053841497,0.0565243637255748),.UNSPECIFIED.);
#23777=B_SPLINE_CURVE_WITH_KNOTS('',3,(#154541,#154542,#154543,#154544,
#154545,#154546),.UNSPECIFIED.,.F.,.F.,(4,2,4),(0.000841212515697555,0.0328420540675755,
0.0646443081941838),.UNSPECIFIED.);
#23778=B_SPLINE_CURVE_WITH_KNOTS('',3,(#154569,#154570,#154571,#154572,
#154573,#154574),.UNSPECIFIED.,.F.,.F.,(4,2,4),(0.,0.0322203311701331,0.0646290645652637),
 .UNSPECIFIED.);
#23779=B_SPLINE_CURVE_WITH_KNOTS('',3,(#154575,#154576,#154577,#154578,
#154579,#154580),.UNSPECIFIED.,.F.,.F.,(4,2,4),(-0.0270903064750334,-0.0141860588293611,
0.),.UNSPECIFIED.);
#23780=B_SPLINE_CURVE_WITH_KNOTS('',3,(#154583,#154584,#154585,#154586,
#154587,#154588,#154589,#154590),.UNSPECIFIED.,.F.,.F.,(4,2,2,4),(1.00000000401862E-6,
0.0321173161163047,0.048121802319759,0.0656773384844766),.UNSPECIFIED.);
#23781=B_SPLINE_CURVE_WITH_KNOTS('',3,(#154592,#154593,#154594,#154595,
#154596,#154597,#154598,#154599),.UNSPECIFIED.,.F.,.F.,(4,2,2,4),(1.00012621567518E-6,
0.0149899307663365,0.028800340737718,0.0565244474880159),.UNSPECIFIED.);
#23782=B_SPLINE_CURVE_WITH_KNOTS('',3,(#154600,#154601,#154602,#154603,
#154604,#154605),.UNSPECIFIED.,.F.,.F.,(4,2,4),(0.000841212510412574,0.0328420540605121,
0.06464430886662),.UNSPECIFIED.);
#23783=B_SPLINE_CURVE_WITH_KNOTS('',3,(#154628,#154629,#154630,#154631,
#154632,#154633),.UNSPECIFIED.,.F.,.F.,(4,2,4),(0.,0.0322203316658832,0.0646290665311863),
 .UNSPECIFIED.);
#23784=B_SPLINE_CURVE_WITH_KNOTS('',3,(#154634,#154635,#154636,#154637,
#154638,#154639),.UNSPECIFIED.,.F.,.F.,(4,2,4),(-0.0270903064362176,-0.0141860588055876,
0.),.UNSPECIFIED.);
#23785=B_SPLINE_CURVE_WITH_KNOTS('',3,(#154642,#154643,#154644,#154645,
#154646,#154647,#154648,#154649),.UNSPECIFIED.,.F.,.F.,(4,2,2,4),(1.00000000410883E-6,
0.0321173160026744,0.0481218021569424,0.0656773383825617),.UNSPECIFIED.);
#23786=B_SPLINE_CURVE_WITH_KNOTS('',3,(#154651,#154652,#154653,#154654,
#154655,#154656,#154657,#154658),.UNSPECIFIED.,.F.,.F.,(4,2,2,4),(1.00011248478266E-6,
0.0149899105681496,0.028800278824881,0.056524301870037),.UNSPECIFIED.);
#23787=B_SPLINE_CURVE_WITH_KNOTS('',3,(#154659,#154660,#154661,#154662,
#154663,#154664),.UNSPECIFIED.,.F.,.F.,(4,2,4),(0.000841212512084421,0.0328420540328582,
0.0646443087371659),.UNSPECIFIED.);
#23788=B_SPLINE_CURVE_WITH_KNOTS('',3,(#154687,#154688,#154689,#154690,
#154691,#154692),.UNSPECIFIED.,.F.,.F.,(4,2,4),(0.,0.032220331299064,0.0646290651252309),
 .UNSPECIFIED.);
#23789=B_SPLINE_CURVE_WITH_KNOTS('',3,(#154693,#154694,#154695,#154696,
#154697,#154698),.UNSPECIFIED.,.F.,.F.,(4,2,4),(-0.0270903064032475,-0.0141860587633634,
0.),.UNSPECIFIED.);
#23790=B_SPLINE_CURVE_WITH_KNOTS('',3,(#154701,#154702,#154703,#154704,
#154705,#154706,#154707,#154708),.UNSPECIFIED.,.F.,.F.,(4,2,2,4),(1.00000000391454E-6,
0.0321173160046967,0.0481218021440837,0.0656773382680278),.UNSPECIFIED.);
#23791=B_SPLINE_CURVE_WITH_KNOTS('',3,(#154710,#154711,#154712,#154713,
#154714,#154715,#154716,#154717),.UNSPECIFIED.,.F.,.F.,(4,2,2,4),(1.00012376496616E-6,
0.0149899403925003,0.0288003683844058,0.0565245115545341),.UNSPECIFIED.);
#23792=B_SPLINE_CURVE_WITH_KNOTS('',3,(#154718,#154719,#154720,#154721,
#154722,#154723),.UNSPECIFIED.,.F.,.F.,(4,2,4),(0.00084121251706062,0.0328420540537706,
0.0646443079811129),.UNSPECIFIED.);
#23793=B_SPLINE_CURVE_WITH_KNOTS('',3,(#154746,#154747,#154748,#154749,
#154750,#154751),.UNSPECIFIED.,.F.,.F.,(4,2,4),(0.,0.0322203309785123,0.0646290639103093),
 .UNSPECIFIED.);
#23794=B_SPLINE_CURVE_WITH_KNOTS('',3,(#154752,#154753,#154754,#154755,
#154756,#154757),.UNSPECIFIED.,.F.,.F.,(4,2,4),(-0.0270903065056521,-0.0141860588741511,
0.),.UNSPECIFIED.);
#23795=B_SPLINE_CURVE_WITH_KNOTS('',3,(#154760,#154761,#154762,#154763,
#154764,#154765,#154766,#154767),.UNSPECIFIED.,.F.,.F.,(4,2,2,4),(1.00000000425454E-6,
0.0321173160975012,0.0481218022746217,0.065677338421128),.UNSPECIFIED.);
#23796=B_SPLINE_CURVE_WITH_KNOTS('',3,(#154769,#154770,#154771,#154772,
#154773,#154774,#154775,#154776),.UNSPECIFIED.,.F.,.F.,(4,2,2,4),(1.00015136715194E-6,
0.0149899861205894,0.02880050974179,0.0565248447377549),.UNSPECIFIED.);
#23797=B_SPLINE_CURVE_WITH_KNOTS('',3,(#154777,#154778,#154779,#154780,
#154781,#154782),.UNSPECIFIED.,.F.,.F.,(4,2,4),(0.000841212514893795,0.0328420540828173,
0.0646443082401466),.UNSPECIFIED.);
#23798=B_SPLINE_CURVE_WITH_KNOTS('',3,(#154805,#154806,#154807,#154808,
#154809,#154810),.UNSPECIFIED.,.F.,.F.,(4,2,4),(0.,0.0322203316164535,0.0646290663521486),
 .UNSPECIFIED.);
#23799=B_SPLINE_CURVE_WITH_KNOTS('',3,(#154811,#154812,#154813,#154814,
#154815,#154816),.UNSPECIFIED.,.F.,.F.,(4,2,4),(-0.027090306440936,-0.0141860588197551,
0.),.UNSPECIFIED.);
#23800=B_SPLINE_CURVE_WITH_KNOTS('',3,(#154819,#154820,#154821,#154822,
#154823,#154824,#154825,#154826),.UNSPECIFIED.,.F.,.F.,(4,2,2,4),(1.0000000041574E-6,
0.0321173160398495,0.0481218021954762,0.0656773384252558),.UNSPECIFIED.);
#23801=B_SPLINE_CURVE_WITH_KNOTS('',3,(#154828,#154829,#154830,#154831,
#154832,#154833,#154834,#154835),.UNSPECIFIED.,.F.,.F.,(4,2,2,4),(1.00008869019263E-6,
0.0149899304634008,0.0288003394410968,0.0565244443100335),.UNSPECIFIED.);
#23802=B_SPLINE_CURVE_WITH_KNOTS('',3,(#154836,#154837,#154838,#154839,
#154840,#154841),.UNSPECIFIED.,.F.,.F.,(4,2,4),(0.000841212512502353,0.0328420540374941,
0.0646443074408672),.UNSPECIFIED.);
#23803=B_SPLINE_CURVE_WITH_KNOTS('',3,(#154862,#154863,#154864,#154865,
#154866,#154867),.UNSPECIFIED.,.F.,.F.,(4,2,4),(-0.0270903064711485,-0.0141860588564947,
0.),.UNSPECIFIED.);
#23804=B_SPLINE_CURVE_WITH_KNOTS('',3,(#154890,#154891,#154892,#154893,
#154894,#154895),.UNSPECIFIED.,.F.,.F.,(4,2,4),(0.,0.032220331040302,0.0646290641347894),
 .UNSPECIFIED.);
#23805=B_SPLINE_CURVE_WITH_KNOTS('',3,(#154896,#154897,#154898,#154899,
#154900,#154901),.UNSPECIFIED.,.F.,.F.,(4,2,4),(-0.02709030651203,-0.0141860588716743,
0.),.UNSPECIFIED.);
#23806=B_SPLINE_CURVE_WITH_KNOTS('',3,(#154904,#154905,#154906,#154907,
#154908,#154909,#154910,#154911),.UNSPECIFIED.,.F.,.F.,(4,2,2,4),(9.9998998204146E-7,
0.0321173159898052,0.0481218021226243,0.0656773382297077),.UNSPECIFIED.);
#23807=B_SPLINE_CURVE_WITH_KNOTS('',3,(#154913,#154914,#154915,#154916,
#154917,#154918,#154919,#154920),.UNSPECIFIED.,.F.,.F.,(4,2,2,4),(1.00012131849139E-6,
0.0149901622886091,0.0288007887685852,0.0565244707711353),.UNSPECIFIED.);
#23808=B_SPLINE_CURVE_WITH_KNOTS('',3,(#154921,#154922,#154923,#154924,
#154925,#154926),.UNSPECIFIED.,.F.,.F.,(4,2,4),(0.00084121252107635,0.03284205406008,
0.0646443081956264),.UNSPECIFIED.);
#23809=B_SPLINE_CURVE_WITH_KNOTS('',3,(#154949,#154950,#154951,#154952,
#154953,#154954),.UNSPECIFIED.,.F.,.F.,(4,2,4),(0.,0.0322203319709312,0.0646290676419014),
 .UNSPECIFIED.);
#23810=B_SPLINE_CURVE_WITH_KNOTS('',3,(#154955,#154956,#154957,#154958,
#154959,#154960),.UNSPECIFIED.,.F.,.F.,(4,2,4),(-0.027090306419541,-0.0141860588100847,
0.),.UNSPECIFIED.);
#23811=B_SPLINE_CURVE_WITH_KNOTS('',3,(#154963,#154964,#154965,#154966,
#154967,#154968,#154969,#154970),.UNSPECIFIED.,.F.,.F.,(4,2,2,4),(1.00000000395617E-6,
0.0321173160087043,0.0481218021580067,0.0656773383989004),.UNSPECIFIED.);
#23812=B_SPLINE_CURVE_WITH_KNOTS('',3,(#154972,#154973,#154974,#154975,
#154976,#154977,#154978,#154979),.UNSPECIFIED.,.F.,.F.,(4,2,2,4),(1.00009951607972E-6,
0.0149899106455396,0.0288002790811247,0.0565243023502256),.UNSPECIFIED.);
#23813=B_SPLINE_CURVE_WITH_KNOTS('',3,(#154980,#154981,#154982,#154983,
#154984,#154985),.UNSPECIFIED.,.F.,.F.,(4,2,4),(0.000841212510310441,0.0328420540544761,
0.0646443082224731),.UNSPECIFIED.);
#23814=B_SPLINE_CURVE_WITH_KNOTS('',3,(#155008,#155009,#155010,#155011,
#155012,#155013),.UNSPECIFIED.,.F.,.F.,(4,2,4),(0.,0.0322203315633675,0.0646290661052855),
 .UNSPECIFIED.);
#23815=B_SPLINE_CURVE_WITH_KNOTS('',3,(#155014,#155015,#155016,#155017,
#155018,#155019),.UNSPECIFIED.,.F.,.F.,(4,2,4),(-0.0270903063858845,-0.0141860587941446,
0.),.UNSPECIFIED.);
#23816=B_SPLINE_CURVE_WITH_KNOTS('',3,(#155022,#155023,#155024,#155025,
#155026,#155027,#155028,#155029),.UNSPECIFIED.,.F.,.F.,(4,2,2,4),(1.00000000446965E-6,
0.0321173160234447,0.0481218021637841,0.0656773383422308),.UNSPECIFIED.);
#23817=B_SPLINE_CURVE_WITH_KNOTS('',3,(#155031,#155032,#155033,#155034,
#155035,#155036,#155037,#155038),.UNSPECIFIED.,.F.,.F.,(4,2,2,4),(1.00008421606349E-6,
0.0149899151239748,0.0288002930878146,0.0565243355189921),.UNSPECIFIED.);
#23818=B_SPLINE_CURVE_WITH_KNOTS('',3,(#155039,#155040,#155041,#155042,
#155043,#155044),.UNSPECIFIED.,.F.,.F.,(4,2,4),(0.000841212504543673,0.0328420540215709,
0.0646443077365915),.UNSPECIFIED.);
#23819=B_SPLINE_CURVE_WITH_KNOTS('',3,(#155067,#155068,#155069,#155070,
#155071,#155072),.UNSPECIFIED.,.F.,.F.,(4,2,4),(0.,0.0322203312992352,0.064629065097578),
 .UNSPECIFIED.);
#23820=B_SPLINE_CURVE_WITH_KNOTS('',3,(#155073,#155074,#155075,#155076,
#155077,#155078),.UNSPECIFIED.,.F.,.F.,(4,2,4),(-0.0270903065060037,-0.0141860588797379,
0.),.UNSPECIFIED.);
#23821=B_SPLINE_CURVE_WITH_KNOTS('',3,(#155081,#155082,#155083,#155084,
#155085,#155086,#155087,#155088),.UNSPECIFIED.,.F.,.F.,(4,2,2,4),(9.99989850218092E-7,
0.0321173160019981,0.0481218021363862,0.0656773382328053),.UNSPECIFIED.);
#23822=B_SPLINE_CURVE_WITH_KNOTS('',3,(#155090,#155091,#155092,#155093,
#155094,#155095,#155096,#155097),.UNSPECIFIED.,.F.,.F.,(4,2,2,4),(1.00014836394316E-6,
0.0149901114536482,0.0288006347456497,0.0565241094201872),.UNSPECIFIED.);
#23823=B_SPLINE_CURVE_WITH_KNOTS('',3,(#155098,#155099,#155100,#155101,
#155102,#155103),.UNSPECIFIED.,.F.,.F.,(4,2,4),(0.000841212522281091,0.0328420540517081,
0.0646443095449781),.UNSPECIFIED.);
#23824=B_SPLINE_CURVE_WITH_KNOTS('',3,(#155126,#155127,#155128,#155129,
#155130,#155131),.UNSPECIFIED.,.F.,.F.,(4,2,4),(0.,0.0322203308131721,0.064629063261788),
 .UNSPECIFIED.);
#23825=B_SPLINE_CURVE_WITH_KNOTS('',3,(#155132,#155133,#155134,#155135,
#155136,#155137),.UNSPECIFIED.,.F.,.F.,(4,2,4),(-0.0270903063886443,-0.0141860587785814,
0.),.UNSPECIFIED.);
#23826=B_SPLINE_CURVE_WITH_KNOTS('',3,(#155140,#155141,#155142,#155143,
#155144,#155145,#155146,#155147),.UNSPECIFIED.,.F.,.F.,(4,2,2,4),(1.00000000401168E-6,
0.0321173160581702,0.0481218022453477,0.0656773383503209),.UNSPECIFIED.);
#23827=B_SPLINE_CURVE_WITH_KNOTS('',3,(#155149,#155150,#155151,#155152,
#155153,#155154,#155155,#155156),.UNSPECIFIED.,.F.,.F.,(4,2,2,4),(1.00016934312906E-6,
0.0149899461668579,0.028800386619068,0.0565245547525933),.UNSPECIFIED.);
#23828=B_SPLINE_CURVE_WITH_KNOTS('',3,(#155157,#155158,#155159,#155160,
#155161,#155162),.UNSPECIFIED.,.F.,.F.,(4,2,4),(0.000841212503056033,0.0328420540648736,
0.0646443079179034),.UNSPECIFIED.);
#23829=B_SPLINE_CURVE_WITH_KNOTS('',3,(#155185,#155186,#155187,#155188,
#155189,#155190),.UNSPECIFIED.,.F.,.F.,(4,2,4),(0.,0.0322203317246494,0.0646290666940337),
 .UNSPECIFIED.);
#23830=B_SPLINE_CURVE_WITH_KNOTS('',3,(#155191,#155192,#155193,#155194,
#155195,#155196),.UNSPECIFIED.,.F.,.F.,(4,2,4),(-0.0270903064677105,-0.014186058827064,
0.),.UNSPECIFIED.);
#23831=B_SPLINE_CURVE_WITH_KNOTS('',3,(#155199,#155200,#155201,#155202,
#155203,#155204,#155205,#155206),.UNSPECIFIED.,.F.,.F.,(4,2,2,4),(1.00000000416434E-6,
0.032117316012009,0.048121802177314,0.0656773384064538),.UNSPECIFIED.);
#23832=B_SPLINE_CURVE_WITH_KNOTS('',3,(#155208,#155209,#155210,#155211,
#155212,#155213,#155214,#155215),.UNSPECIFIED.,.F.,.F.,(4,2,2,4),(1.00010778408823E-6,
0.0149898884705105,0.028800211788248,0.0565241445861282),.UNSPECIFIED.);
#23833=B_SPLINE_CURVE_WITH_KNOTS('',3,(#155216,#155217,#155218,#155219,
#155220,#155221),.UNSPECIFIED.,.F.,.F.,(4,2,4),(0.000841212508163703,0.0328420540409334,
0.0646443086155899),.UNSPECIFIED.);
#23834=B_SPLINE_CURVE_WITH_KNOTS('',3,(#155244,#155245,#155246,#155247,
#155248,#155249),.UNSPECIFIED.,.F.,.F.,(4,2,4),(0.,0.0322203309557638,0.0646290638560515),
 .UNSPECIFIED.);
#23835=B_SPLINE_CURVE_WITH_KNOTS('',3,(#155250,#155251,#155252,#155253,
#155254,#155255),.UNSPECIFIED.,.F.,.F.,(4,2,4),(-0.0270903064294424,-0.0141860588345496,
0.),.UNSPECIFIED.);
#23836=B_SPLINE_CURVE_WITH_KNOTS('',3,(#155258,#155259,#155260,#155261,
#155262,#155263,#155264,#155265),.UNSPECIFIED.,.F.,.F.,(4,2,2,4),(1.00000000420597E-6,
0.0321173159670649,0.048121802089453,0.0656773381295942),.UNSPECIFIED.);
#23837=B_SPLINE_CURVE_WITH_KNOTS('',3,(#155267,#155268,#155269,#155270,
#155271,#155272,#155273,#155274),.UNSPECIFIED.,.F.,.F.,(4,2,2,4),(1.00012040405606E-6,
0.0149899472299666,0.028800390838345,0.056524565189487),.UNSPECIFIED.);
#23838=B_SPLINE_CURVE_WITH_KNOTS('',3,(#155275,#155276,#155277,#155278,
#155279,#155280),.UNSPECIFIED.,.F.,.F.,(4,2,4),(0.000841212507813186,0.0328420540587639,
0.0646443079539742),.UNSPECIFIED.);
#23839=B_SPLINE_CURVE_WITH_KNOTS('',3,(#155293,#155294,#155295,#155296,
#155297,#155298),.UNSPECIFIED.,.F.,.F.,(4,2,4),(0.,0.0322203302008996,0.0646290631014971),
 .UNSPECIFIED.);
#23840=B_SPLINE_CURVE_WITH_KNOTS('',3,(#155300,#155301,#155302,#155303,
#155304,#155305,#155306,#155307),.UNSPECIFIED.,.F.,.F.,(4,2,2,4),(1.00000000396311E-6,
0.0321173162056066,0.0481218402735079,0.0656773352685673),.UNSPECIFIED.);
#23841=B_SPLINE_CURVE_WITH_KNOTS('',3,(#155308,#155309,#155310,#155311,
#155312,#155313,#155314,#155315),.UNSPECIFIED.,.F.,.F.,(4,2,2,4),(1.00019596529798E-6,
0.0149905409355991,0.0288008434416931,0.056524563022755),.UNSPECIFIED.);
#23842=B_SPLINE_CURVE_WITH_KNOTS('',3,(#155334,#155335,#155336,#155337,
#155338,#155339),.UNSPECIFIED.,.F.,.F.,(4,2,4),(-0.0253026342524986,-0.0126514544652314,
-1.88668421163829E-11),.UNSPECIFIED.);
#23843=B_SPLINE_CURVE_WITH_KNOTS('',3,(#155348,#155349,#155350,#155351,
#155352,#155353),.UNSPECIFIED.,.F.,.F.,(4,2,4),(0.,0.0126514363600221,0.0253026263497453),
 .UNSPECIFIED.);
#23844=B_SPLINE_CURVE_WITH_KNOTS('',3,(#155369,#155370,#155371,#155372,
#155373,#155374),.UNSPECIFIED.,.F.,.F.,(4,2,4),(3.32128913797922E-11,0.0126514528097758,
0.025302666580165),.UNSPECIFIED.);
#23845=B_SPLINE_CURVE_WITH_KNOTS('',3,(#155390,#155391,#155392,#155393,
#155394,#155395),.UNSPECIFIED.,.F.,.F.,(4,2,4),(2.48238510840293E-11,0.0126514528557191,
0.0253026666422664),.UNSPECIFIED.);
#23846=B_SPLINE_CURVE_WITH_KNOTS('',3,(#155411,#155412,#155413,#155414,
#155415,#155416),.UNSPECIFIED.,.F.,.F.,(4,2,4),(0.,0.0126514361044767,0.0253026254261494),
 .UNSPECIFIED.);
#23847=B_SPLINE_CURVE_WITH_KNOTS('',3,(#155432,#155433,#155434,#155435,
#155436,#155437),.UNSPECIFIED.,.F.,.F.,(4,2,4),(1.78381052840366E-11,0.012651452890063,
0.0253026666624878),.UNSPECIFIED.);
#23848=B_SPLINE_CURVE_WITH_KNOTS('',3,(#155453,#155454,#155455,#155456,
#155457,#155458),.UNSPECIFIED.,.F.,.F.,(4,2,4),(0.,0.0126514377629713,0.0253026295575941),
 .UNSPECIFIED.);
#23849=B_SPLINE_CURVE_WITH_KNOTS('',3,(#155474,#155475,#155476,#155477,
#155478,#155479),.UNSPECIFIED.,.F.,.F.,(4,2,4),(0.,0.0126514375141281,0.0253026290465384),
 .UNSPECIFIED.);
#23850=B_SPLINE_CURVE_WITH_KNOTS('',3,(#155495,#155496,#155497,#155498,
#155499,#155500),.UNSPECIFIED.,.F.,.F.,(4,2,4),(1.86039915567488E-11,0.0126514527918854,
0.0253026665522429),.UNSPECIFIED.);
#23851=B_SPLINE_CURVE_WITH_KNOTS('',3,(#155516,#155517,#155518,#155519,
#155520,#155521),.UNSPECIFIED.,.F.,.F.,(4,2,4),(0.,0.0126514374178867,0.0253026288727294),
 .UNSPECIFIED.);
#23852=B_SPLINE_CURVE_WITH_KNOTS('',3,(#155537,#155538,#155539,#155540,
#155541,#155542),.UNSPECIFIED.,.F.,.F.,(4,2,4),(0.,0.0126514379132605,0.0253026301647806),
 .UNSPECIFIED.);
#23853=B_SPLINE_CURVE_WITH_KNOTS('',3,(#155558,#155559,#155560,#155561,
#155562,#155563),.UNSPECIFIED.,.F.,.F.,(4,2,4),(0.,0.0126514341354231,0.02530262056224),
 .UNSPECIFIED.);
#23854=B_SPLINE_CURVE_WITH_KNOTS('',3,(#155579,#155580,#155581,#155582,
#155583,#155584),.UNSPECIFIED.,.F.,.F.,(4,2,4),(0.,0.0126514348780394,0.025302622573186),
 .UNSPECIFIED.);
#23855=B_SPLINE_CURVE_WITH_KNOTS('',3,(#155600,#155601,#155602,#155603,
#155604,#155605),.UNSPECIFIED.,.F.,.F.,(4,2,4),(0.,0.0126514359812692,0.0253026251414924),
 .UNSPECIFIED.);
#23856=B_SPLINE_CURVE_WITH_KNOTS('',3,(#155621,#155622,#155623,#155624,
#155625,#155626),.UNSPECIFIED.,.F.,.F.,(4,2,4),(2.48627244145729E-11,0.0126514528013674,
0.0253026665766467),.UNSPECIFIED.);
#23857=B_SPLINE_CURVE_WITH_KNOTS('',3,(#155642,#155643,#155644,#155645,
#155646,#155647),.UNSPECIFIED.,.F.,.F.,(4,2,4),(0.,0.0126514360446639,0.0253026253845719),
 .UNSPECIFIED.);
#23858=B_SPLINE_CURVE_WITH_KNOTS('',3,(#155663,#155664,#155665,#155666,
#155667,#155668),.UNSPECIFIED.,.F.,.F.,(4,2,4),(0.,0.0126514360075886,0.0253026253307672),
 .UNSPECIFIED.);
#23859=B_SPLINE_CURVE_WITH_KNOTS('',3,(#155684,#155685,#155686,#155687,
#155688,#155689),.UNSPECIFIED.,.F.,.F.,(4,2,4),(0.,0.0126514352765847,0.0253026235823062),
 .UNSPECIFIED.);
#23860=B_SPLINE_CURVE_WITH_KNOTS('',3,(#155705,#155706,#155707,#155708,
#155709,#155710),.UNSPECIFIED.,.F.,.F.,(4,2,4),(9.20122805263892E-12,0.0126514528186731,
0.025302666610893),.UNSPECIFIED.);
#23861=B_SPLINE_CURVE_WITH_KNOTS('',3,(#155726,#155727,#155728,#155729,
#155730,#155731),.UNSPECIFIED.,.F.,.F.,(4,2,4),(0.,0.0126514380585315,0.0253026303831182),
 .UNSPECIFIED.);
#23862=B_SPLINE_CURVE_WITH_KNOTS('',3,(#155747,#155748,#155749,#155750,
#155751,#155752),.UNSPECIFIED.,.F.,.F.,(4,2,4),(0.,0.0126514369475504,0.0253026276141575),
 .UNSPECIFIED.);
#23863=B_SPLINE_CURVE_WITH_KNOTS('',3,(#155768,#155769,#155770,#155771,
#155772,#155773),.UNSPECIFIED.,.F.,.F.,(4,2,4),(0.,0.0126514362674318,0.0253026258987748),
 .UNSPECIFIED.);
#23864=B_SPLINE_CURVE_WITH_KNOTS('',3,(#155789,#155790,#155791,#155792,
#155793,#155794),.UNSPECIFIED.,.F.,.F.,(4,2,4),(0.,0.0126514378601925,0.0253026298921727),
 .UNSPECIFIED.);
#23865=B_SPLINE_CURVE_WITH_KNOTS('',3,(#155810,#155811,#155812,#155813,
#155814,#155815),.UNSPECIFIED.,.F.,.F.,(4,2,4),(0.,0.0126514360091151,0.0253026252315581),
 .UNSPECIFIED.);
#23866=B_SPLINE_CURVE_WITH_KNOTS('',3,(#155831,#155832,#155833,#155834,
#155835,#155836),.UNSPECIFIED.,.F.,.F.,(4,2,4),(0.,0.012651437241266,0.025302628328002),
 .UNSPECIFIED.);
#23867=B_SPLINE_CURVE_WITH_KNOTS('',3,(#155852,#155853,#155854,#155855,
#155856,#155857),.UNSPECIFIED.,.F.,.F.,(4,2,4),(2.1570000216242E-11,0.012651452719397,
0.0253026665300329),.UNSPECIFIED.);
#23868=B_SPLINE_CURVE_WITH_KNOTS('',3,(#155873,#155874,#155875,#155876,
#155877,#155878),.UNSPECIFIED.,.F.,.F.,(4,2,4),(0.,0.0126514357414824,0.025302624730698),
 .UNSPECIFIED.);
#23869=B_SPLINE_CURVE_WITH_KNOTS('',3,(#155894,#155895,#155896,#155897,
#155898,#155899),.UNSPECIFIED.,.F.,.F.,(4,2,4),(0.,0.0126514374648161,0.0253026289492822),
 .UNSPECIFIED.);
#23870=B_SPLINE_CURVE_WITH_KNOTS('',3,(#155915,#155916,#155917,#155918,
#155919,#155920),.UNSPECIFIED.,.F.,.F.,(4,2,4),(2.26557866084254E-11,0.0126514528474184,
0.0253026666314633),.UNSPECIFIED.);
#23871=B_SPLINE_CURVE_WITH_KNOTS('',3,(#155951,#155952,#155953,#155954),
 .UNSPECIFIED.,.F.,.F.,(4,4),(9.26470581739597E-13,6.28597141856272E-5),
 .UNSPECIFIED.);
#23872=B_SPLINE_CURVE_WITH_KNOTS('',3,(#155972,#155973,#155974,#155975),
 .UNSPECIFIED.,.F.,.F.,(4,4),(1.04766320724494E-15,6.28597156104803E-5),
 .UNSPECIFIED.);
#23873=B_SPLINE_CURVE_WITH_KNOTS('',3,(#156015,#156016,#156017,#156018),
 .UNSPECIFIED.,.F.,.F.,(4,4),(8.08906446880292E-14,6.28597156343113E-5),
 .UNSPECIFIED.);
#23874=B_SPLINE_CURVE_WITH_KNOTS('',3,(#156058,#156059,#156060,#156061),
 .UNSPECIFIED.,.F.,.F.,(4,4),(2.37774944269479E-13,6.2859613216331E-5),
 .UNSPECIFIED.);
#23875=B_SPLINE_CURVE_WITH_KNOTS('',3,(#156101,#156102,#156103,#156104),
 .UNSPECIFIED.,.F.,.F.,(4,4),(2.29518468417639E-13,6.2859715533947E-5),
 .UNSPECIFIED.);
#23876=B_SPLINE_CURVE_WITH_KNOTS('',3,(#156144,#156145,#156146,#156147),
 .UNSPECIFIED.,.F.,.F.,(4,4),(2.70866639842599E-13,6.28596134458986E-5),
 .UNSPECIFIED.);
#23877=B_SPLINE_CURVE_WITH_KNOTS('',3,(#156187,#156188,#156189,#156190),
 .UNSPECIFIED.,.F.,.F.,(4,4),(2.23807374264663E-13,6.28597151266788E-5),
 .UNSPECIFIED.);
#23878=B_SPLINE_CURVE_WITH_KNOTS('',3,(#156230,#156231,#156232,#156233),
 .UNSPECIFIED.,.F.,.F.,(4,4),(1.87272302703493E-13,6.28596136423573E-5),
 .UNSPECIFIED.);
#23879=B_SPLINE_CURVE_WITH_KNOTS('',3,(#156273,#156274,#156275,#156276),
 .UNSPECIFIED.,.F.,.F.,(4,4),(2.8724223760636E-13,6.2859715332009E-5),
 .UNSPECIFIED.);
#23880=B_SPLINE_CURVE_WITH_KNOTS('',3,(#156316,#156317,#156318,#156319),
 .UNSPECIFIED.,.F.,.F.,(4,4),(1.70751514793651E-13,6.28596134861198E-5),
 .UNSPECIFIED.);
#23881=B_SPLINE_CURVE_WITH_KNOTS('',3,(#156359,#156360,#156361,#156362),
 .UNSPECIFIED.,.F.,.F.,(4,4),(3.03042579258976E-13,6.28597151227342E-5),
 .UNSPECIFIED.);
#23882=B_SPLINE_CURVE_WITH_KNOTS('',3,(#156402,#156403,#156404,#156405),
 .UNSPECIFIED.,.F.,.F.,(4,4),(5.08657612240452E-14,6.28596135406422E-5),
 .UNSPECIFIED.);
#23883=B_SPLINE_CURVE_WITH_KNOTS('',3,(#156445,#156446,#156447,#156448),
 .UNSPECIFIED.,.F.,.F.,(4,4),(5.28446618968616E-14,6.28597154269528E-5),
 .UNSPECIFIED.);
#23884=B_SPLINE_CURVE_WITH_KNOTS('',3,(#156488,#156489,#156490,#156491),
 .UNSPECIFIED.,.F.,.F.,(4,4),(2.55677946032555E-14,6.28597154812872E-5),
 .UNSPECIFIED.);
#23885=B_SPLINE_CURVE_WITH_KNOTS('',3,(#156531,#156532,#156533,#156534),
 .UNSPECIFIED.,.F.,.F.,(4,4),(3.0550090682991E-14,6.28596141204512E-5),
 .UNSPECIFIED.);
#23886=B_SPLINE_CURVE_WITH_KNOTS('',3,(#156574,#156575,#156576,#156577),
 .UNSPECIFIED.,.F.,.F.,(4,4),(2.44665260015811E-13,6.28596133307425E-5),
 .UNSPECIFIED.);
#23887=B_SPLINE_CURVE_WITH_KNOTS('',3,(#156617,#156618,#156619,#156620),
 .UNSPECIFIED.,.F.,.F.,(4,4),(1.31704635813045E-13,6.28597154645398E-5),
 .UNSPECIFIED.);
#23888=B_SPLINE_CURVE_WITH_KNOTS('',3,(#156660,#156661,#156662,#156663),
 .UNSPECIFIED.,.F.,.F.,(4,4),(1.60877020579121E-13,6.28597156681893E-5),
 .UNSPECIFIED.);
#23889=B_SPLINE_CURVE_WITH_KNOTS('',3,(#156703,#156704,#156705,#156706),
 .UNSPECIFIED.,.F.,.F.,(4,4),(7.17404455169434E-14,6.28596139390678E-5),
 .UNSPECIFIED.);
#23890=B_SPLINE_CURVE_WITH_KNOTS('',3,(#156746,#156747,#156748,#156749),
 .UNSPECIFIED.,.F.,.F.,(4,4),(6.75749921739619E-14,6.28597156566878E-5),
 .UNSPECIFIED.);
#23891=B_SPLINE_CURVE_WITH_KNOTS('',3,(#156789,#156790,#156791,#156792),
 .UNSPECIFIED.,.F.,.F.,(4,4),(1.12746347172328E-13,6.28596136474964E-5),
 .UNSPECIFIED.);
#23892=B_SPLINE_CURVE_WITH_KNOTS('',3,(#156832,#156833,#156834,#156835),
 .UNSPECIFIED.,.F.,.F.,(4,4),(2.88340174742551E-13,6.28596130517667E-5),
 .UNSPECIFIED.);
#23893=B_SPLINE_CURVE_WITH_KNOTS('',3,(#156875,#156876,#156877,#156878),
 .UNSPECIFIED.,.F.,.F.,(4,4),(1.38583212404894E-13,6.28596135251862E-5),
 .UNSPECIFIED.);
#23894=B_SPLINE_CURVE_WITH_KNOTS('',3,(#156918,#156919,#156920,#156921),
 .UNSPECIFIED.,.F.,.F.,(4,4),(3.44119806752207E-14,6.28596138372693E-5),
 .UNSPECIFIED.);
#23895=B_SPLINE_CURVE_WITH_KNOTS('',3,(#156961,#156962,#156963,#156964),
 .UNSPECIFIED.,.F.,.F.,(4,4),(5.94610859549734E-14,6.28597152568138E-5),
 .UNSPECIFIED.);
#23896=B_SPLINE_CURVE_WITH_KNOTS('',3,(#157004,#157005,#157006,#157007),
 .UNSPECIFIED.,.F.,.F.,(4,4),(1.8601570951842E-15,6.28596138115333E-5),
 .UNSPECIFIED.);
#23897=B_SPLINE_CURVE_WITH_KNOTS('',3,(#157047,#157048,#157049,#157050),
 .UNSPECIFIED.,.F.,.F.,(4,4),(1.99004818569542E-13,6.28596133094018E-5),
 .UNSPECIFIED.);
#23898=B_SPLINE_CURVE_WITH_KNOTS('',3,(#157090,#157091,#157092,#157093),
 .UNSPECIFIED.,.F.,.F.,(4,4),(1.38126555594922E-13,6.28596131963104E-5),
 .UNSPECIFIED.);
#23899=B_SPLINE_CURVE_WITH_KNOTS('',3,(#157133,#157134,#157135,#157136),
 .UNSPECIFIED.,.F.,.F.,(4,4),(6.20789635911566E-14,6.28596134471087E-5),
 .UNSPECIFIED.);
#23900=B_SPLINE_CURVE_WITH_KNOTS('',3,(#157179,#157180,#157181,#157182,
#157183,#157184),.UNSPECIFIED.,.F.,.F.,(4,2,4),(-0.0252983210333844,-0.012649302700262,
0.),.UNSPECIFIED.);
#23901=B_SPLINE_CURVE_WITH_KNOTS('',3,(#157212,#157213,#157214,#157215,
#157216,#157217),.UNSPECIFIED.,.F.,.F.,(4,2,4),(-0.0252983259187359,-0.012649308870704,
0.),.UNSPECIFIED.);
#23902=B_SPLINE_CURVE_WITH_KNOTS('',3,(#157245,#157246,#157247,#157248,
#157249,#157250),.UNSPECIFIED.,.F.,.F.,(4,2,4),(-0.0252983452113512,-0.0126493122835931,
0.),.UNSPECIFIED.);
#23903=B_SPLINE_CURVE_WITH_KNOTS('',3,(#157278,#157279,#157280,#157281,
#157282,#157283),.UNSPECIFIED.,.F.,.F.,(4,2,4),(-0.0252983126265095,-0.012649303527495,
0.),.UNSPECIFIED.);
#23904=B_SPLINE_CURVE_WITH_KNOTS('',3,(#157311,#157312,#157313,#157314,
#157315,#157316),.UNSPECIFIED.,.F.,.F.,(4,2,4),(-0.0252983051684543,-0.0126493005082459,
0.),.UNSPECIFIED.);
#23905=B_SPLINE_CURVE_WITH_KNOTS('',3,(#157344,#157345,#157346,#157347,
#157348,#157349),.UNSPECIFIED.,.F.,.F.,(4,2,4),(-0.0252983420341862,-0.0126493154664923,
0.),.UNSPECIFIED.);
#23906=B_SPLINE_CURVE_WITH_KNOTS('',3,(#157377,#157378,#157379,#157380,
#157381,#157382),.UNSPECIFIED.,.F.,.F.,(4,2,4),(-0.0252983184795831,-0.012649301187786,
0.),.UNSPECIFIED.);
#23907=B_SPLINE_CURVE_WITH_KNOTS('',3,(#157410,#157411,#157412,#157413,
#157414,#157415),.UNSPECIFIED.,.F.,.F.,(4,2,4),(-0.0252987422513607,-0.0126494774106738,
-2.8633935500455E-11),.UNSPECIFIED.);
#23908=B_SPLINE_CURVE_WITH_KNOTS('',3,(#157443,#157444,#157445,#157446,
#157447,#157448),.UNSPECIFIED.,.F.,.F.,(4,2,4),(-0.0252983196287654,-0.0126493019768695,
0.),.UNSPECIFIED.);
#23909=B_SPLINE_CURVE_WITH_KNOTS('',3,(#157476,#157477,#157478,#157479,
#157480,#157481),.UNSPECIFIED.,.F.,.F.,(4,2,4),(-0.0252987422906831,-0.0126494774423558,
-3.53359529137176E-11),.UNSPECIFIED.);
#23910=B_SPLINE_CURVE_WITH_KNOTS('',3,(#157509,#157510,#157511,#157512,
#157513,#157514),.UNSPECIFIED.,.F.,.F.,(4,2,4),(-0.0252983427352373,-0.0126493112443732,
0.),.UNSPECIFIED.);
#23911=B_SPLINE_CURVE_WITH_KNOTS('',3,(#157542,#157543,#157544,#157545,
#157546,#157547),.UNSPECIFIED.,.F.,.F.,(4,2,4),(-0.0252983604613678,-0.0126493184035386,
0.),.UNSPECIFIED.);
#23912=B_SPLINE_CURVE_WITH_KNOTS('',3,(#157575,#157576,#157577,#157578,
#157579,#157580),.UNSPECIFIED.,.F.,.F.,(4,2,4),(-0.0252983388699996,-0.0126493141276362,
0.),.UNSPECIFIED.);
#23913=B_SPLINE_CURVE_WITH_KNOTS('',3,(#157608,#157609,#157610,#157611,
#157612,#157613),.UNSPECIFIED.,.F.,.F.,(4,2,4),(-0.0252983093340518,-0.0126493021520564,
0.),.UNSPECIFIED.);
#23914=B_SPLINE_CURVE_WITH_KNOTS('',3,(#157638,#157639,#157640,#157641,
#157642,#157643),.UNSPECIFIED.,.F.,.F.,(4,2,4),(-0.0252983343649174,-0.0126493123664179,
0.),.UNSPECIFIED.);
#23915=B_SPLINE_CURVE_WITH_KNOTS('',3,(#157665,#157666,#157667,#157668,
#157669,#157670),.UNSPECIFIED.,.F.,.F.,(4,2,4),(-0.0252983139448652,-0.012649299232769,
0.),.UNSPECIFIED.);
#23916=B_SPLINE_CURVE_WITH_KNOTS('',3,(#157698,#157699,#157700,#157701,
#157702,#157703),.UNSPECIFIED.,.F.,.F.,(4,2,4),(-0.0252983284278702,-0.0126493053945732,
0.),.UNSPECIFIED.);
#23917=B_SPLINE_CURVE_WITH_KNOTS('',3,(#157731,#157732,#157733,#157734,
#157735,#157736),.UNSPECIFIED.,.F.,.F.,(4,2,4),(-0.025298752822132,-0.0126494774032927,
-2.07888706249548E-11),.UNSPECIFIED.);
#23918=B_SPLINE_CURVE_WITH_KNOTS('',3,(#157765,#157766,#157767,#157768,
#157769,#157770),.UNSPECIFIED.,.F.,.F.,(4,2,4),(-0.0252983533956398,-0.0126493200194815,
0.),.UNSPECIFIED.);
#23919=B_SPLINE_CURVE_WITH_KNOTS('',3,(#157797,#157798,#157799,#157800,
#157801,#157802),.UNSPECIFIED.,.F.,.F.,(4,2,4),(-0.0252983451914397,-0.0126493126064348,
0.),.UNSPECIFIED.);
#23920=B_SPLINE_CURVE_WITH_KNOTS('',3,(#157830,#157831,#157832,#157833,
#157834,#157835),.UNSPECIFIED.,.F.,.F.,(4,2,4),(-0.025298337408984,-0.0126493088979085,
0.),.UNSPECIFIED.);
#23921=B_SPLINE_CURVE_WITH_KNOTS('',3,(#157863,#157864,#157865,#157866,
#157867,#157868),.UNSPECIFIED.,.F.,.F.,(4,2,4),(-0.0252983425361315,-0.0126493108082732,
0.),.UNSPECIFIED.);
#23922=B_SPLINE_CURVE_WITH_KNOTS('',3,(#157896,#157897,#157898,#157899,
#157900,#157901),.UNSPECIFIED.,.F.,.F.,(4,2,4),(-0.0252983214371618,-0.0126493028038431,
0.),.UNSPECIFIED.);
#23923=B_SPLINE_CURVE_WITH_KNOTS('',3,(#157929,#157930,#157931,#157932,
#157933,#157934),.UNSPECIFIED.,.F.,.F.,(4,2,4),(-0.0252983382857441,-0.0126493089336017,
0.),.UNSPECIFIED.);
#23924=B_SPLINE_CURVE_WITH_KNOTS('',3,(#157962,#157963,#157964,#157965,
#157966,#157967),.UNSPECIFIED.,.F.,.F.,(4,2,4),(-0.0252983296574141,-0.0126493057311267,
0.),.UNSPECIFIED.);
#23925=B_SPLINE_CURVE_WITH_KNOTS('',3,(#157995,#157996,#157997,#157998,
#157999,#158000),.UNSPECIFIED.,.F.,.F.,(4,2,4),(-0.0252983425115197,-0.0126493156571284,
0.),.UNSPECIFIED.);
#23926=B_SPLINE_CURVE_WITH_KNOTS('',3,(#158028,#158029,#158030,#158031,
#158032,#158033),.UNSPECIFIED.,.F.,.F.,(4,2,4),(-0.0252983434321303,-0.0126493159559477,
0.),.UNSPECIFIED.);
#23927=B_SPLINE_CURVE_WITH_KNOTS('',3,(#158061,#158062,#158063,#158064,
#158065,#158066),.UNSPECIFIED.,.F.,.F.,(4,2,4),(-0.025298310545057,-0.0126492984757903,
0.),.UNSPECIFIED.);
#23928=B_SPLINE_CURVE_WITH_KNOTS('',3,(#158094,#158095,#158096,#158097,
#158098,#158099),.UNSPECIFIED.,.F.,.F.,(4,2,4),(-0.0252982986313331,-0.0126492979062713,
0.),.UNSPECIFIED.);
#23929=B_SPLINE_CURVE_WITH_KNOTS('',3,(#158136,#158137,#158138,#158139,
#158140,#158141,#158142,#158143,#158144,#158145),.UNSPECIFIED.,.F.,.F.,
(4,3,3,4),(4.25990453213117E-13,1.58768505726012E-5,3.06163004638053E-5,
4.5355765246366E-5),.UNSPECIFIED.);
#23930=B_SPLINE_CURVE_WITH_KNOTS('',3,(#158156,#158157,#158158,#158159,
#158160,#158161,#158162),.UNSPECIFIED.,.F.,.F.,(4,3,4),(0.0665257480074743,
0.0687515042649955,0.0736118336323568),.UNSPECIFIED.);
#23931=B_SPLINE_CURVE_WITH_KNOTS('',3,(#158184,#158185,#158186,#158187,
#158188,#158189,#158190,#158191,#158192,#158193),.UNSPECIFIED.,.F.,.F.,
(4,3,3,4),(1.99141659217819E-11,5.49564847615335E-5,0.000106404139403314,
0.000157852343447398),.UNSPECIFIED.);
#23932=B_SPLINE_CURVE_WITH_KNOTS('',3,(#158222,#158223,#158224,#158225,
#158226,#158227,#158228,#158229,#158230,#158231),.UNSPECIFIED.,.F.,.F.,
(4,3,3,4),(5.32676466607925E-13,1.58768508861865E-5,3.06163005726345E-5,
4.53557651504358E-5),.UNSPECIFIED.);
#23933=B_SPLINE_CURVE_WITH_KNOTS('',3,(#158242,#158243,#158244,#158245,
#158246,#158247,#158248),.UNSPECIFIED.,.F.,.F.,(4,3,4),(0.0665257254736559,
0.0687515042649955,0.0736118336370433),.UNSPECIFIED.);
#23934=B_SPLINE_CURVE_WITH_KNOTS('',3,(#158270,#158271,#158272,#158273,
#158274,#158275,#158276,#158277,#158278,#158279),.UNSPECIFIED.,.F.,.F.,
(4,3,3,4),(1.93863144415546E-11,5.49564848580405E-5,0.000106404139411967,
0.000157852343337258),.UNSPECIFIED.);
#23935=B_SPLINE_CURVE_WITH_KNOTS('',3,(#158308,#158309,#158310,#158311,
#158312,#158313,#158314,#158315,#158316,#158317),.UNSPECIFIED.,.F.,.F.,
(4,3,3,4),(5.5731114037476E-13,1.58768507104624E-5,3.06163004400154E-5,
4.53557650609786E-5),.UNSPECIFIED.);
#23936=B_SPLINE_CURVE_WITH_KNOTS('',3,(#158328,#158329,#158330,#158331,
#158332,#158333),.UNSPECIFIED.,.F.,.F.,(4,2,4),(-0.0324724419097549,-0.0162483431540196,
0.),.UNSPECIFIED.);
#23937=B_SPLINE_CURVE_WITH_KNOTS('',3,(#158355,#158356,#158357,#158358,
#158359,#158360,#158361,#158362,#158363,#158364),.UNSPECIFIED.,.F.,.F.,
(4,3,3,4),(1.94550864791645E-11,5.49564847847185E-5,0.000106404139445542,
0.000157852343508583),.UNSPECIFIED.);
#23938=B_SPLINE_CURVE_WITH_KNOTS('',3,(#158393,#158394,#158395,#158396,
#158397,#158398,#158399,#158400,#158401,#158402),.UNSPECIFIED.,.F.,.F.,
(4,3,3,4),(3.76772541217172E-13,1.58768505800345E-5,3.06163003300456E-5,
4.53557649715249E-5),.UNSPECIFIED.);
#23939=B_SPLINE_CURVE_WITH_KNOTS('',3,(#158413,#158414,#158415,#158416,
#158417,#158418,#158419),.UNSPECIFIED.,.F.,.F.,(4,3,4),(0.0665257474100939,
0.068751504264996,0.0736118336454257),.UNSPECIFIED.);
#23940=B_SPLINE_CURVE_WITH_KNOTS('',3,(#158441,#158442,#158443,#158444,
#158445,#158446,#158447,#158448,#158449,#158450),.UNSPECIFIED.,.F.,.F.,
(4,3,3,4),(1.96446060032063E-11,5.4956484838752E-5,0.000106404139406406,
0.000157852343376373),.UNSPECIFIED.);
#23941=B_SPLINE_CURVE_WITH_KNOTS('',3,(#158479,#158480,#158481,#158482,
#158483,#158484,#158485,#158486,#158487,#158488),.UNSPECIFIED.,.F.,.F.,
(4,3,3,4),(4.86755894837992E-13,1.58768505748808E-5,3.0616300507068E-5,
4.5355765330689E-5),.UNSPECIFIED.);
#23942=B_SPLINE_CURVE_WITH_KNOTS('',3,(#158525,#158526,#158527,#158528,
#158529,#158530,#158531,#158532,#158533,#158534),.UNSPECIFIED.,.F.,.F.,
(4,3,3,4),(1.99724871658589E-11,5.49564846709833E-5,0.000106404139381309,
0.000157852343435992),.UNSPECIFIED.);
#23943=B_SPLINE_CURVE_WITH_KNOTS('',3,(#158563,#158564,#158565,#158566,
#158567,#158568,#158569,#158570,#158571,#158572),.UNSPECIFIED.,.F.,.F.,
(4,3,3,4),(4.33749804775174E-13,1.58768504673084E-5,3.06163003327111E-5,
4.53557650894788E-5),.UNSPECIFIED.);
#23944=B_SPLINE_CURVE_WITH_KNOTS('',3,(#158583,#158584,#158585,#158586,
#158587,#158588,#158589),.UNSPECIFIED.,.F.,.F.,(4,3,4),(0.0665257474078056,
0.0687515042649963,0.0736118336407646),.UNSPECIFIED.);
#23945=B_SPLINE_CURVE_WITH_KNOTS('',3,(#158611,#158612,#158613,#158614,
#158615,#158616,#158617,#158618,#158619,#158620),.UNSPECIFIED.,.F.,.F.,
(4,3,3,4),(1.97606791947156E-11,5.49564847358755E-5,0.000106404139427357,
0.000157852343477407),.UNSPECIFIED.);
#23946=B_SPLINE_CURVE_WITH_KNOTS('',3,(#158649,#158650,#158651,#158652,
#158653,#158654,#158655,#158656,#158657,#158658),.UNSPECIFIED.,.F.,.F.,
(4,3,3,4),(3.72492554887973E-13,1.58768508262691E-5,3.06163004955292E-5,
4.5355765056191E-5),.UNSPECIFIED.);
#23947=B_SPLINE_CURVE_WITH_KNOTS('',3,(#158669,#158670,#158671,#158672,
#158673,#158674),.UNSPECIFIED.,.F.,.F.,(4,2,4),(-0.0324734603942446,-0.0162498515535043,
-9.9933629731791E-7),.UNSPECIFIED.);
#23948=B_SPLINE_CURVE_WITH_KNOTS('',3,(#158696,#158697,#158698,#158699,
#158700,#158701,#158702,#158703,#158704,#158705),.UNSPECIFIED.,.F.,.F.,
(4,3,3,4),(1.93519675222046E-11,5.49564847880802E-5,0.000106404139355769,
0.000157852343325931),.UNSPECIFIED.);
#23949=B_SPLINE_CURVE_WITH_KNOTS('',3,(#158734,#158735,#158736,#158737,
#158738,#158739,#158740,#158741,#158742,#158743),.UNSPECIFIED.,.F.,.F.,
(4,3,3,4),(4.97103074448361E-13,1.58768506527717E-5,3.06163004425891E-5,
4.53557651237911E-5),.UNSPECIFIED.);
#23950=B_SPLINE_CURVE_WITH_KNOTS('',3,(#158754,#158755,#158756,#158757,
#158758,#158759,#158760),.UNSPECIFIED.,.F.,.F.,(4,3,4),(0.0665257474071759,
0.0687515042649955,0.0736118336741103),.UNSPECIFIED.);
#23951=B_SPLINE_CURVE_WITH_KNOTS('',3,(#158782,#158783,#158784,#158785,
#158786,#158787,#158788,#158789,#158790,#158791),.UNSPECIFIED.,.F.,.F.,
(4,3,3,4),(1.96923621175035E-11,5.49564847036435E-5,0.000106404139397447,
0.000157852343493646),.UNSPECIFIED.);
#23952=B_SPLINE_CURVE_WITH_KNOTS('',3,(#158820,#158821,#158822,#158823,
#158824,#158825,#158826,#158827,#158828,#158829),.UNSPECIFIED.,.F.,.F.,
(4,3,3,4),(4.23342436434571E-13,1.58768506365923E-5,3.06163005047287E-5,
4.5355765264208E-5),.UNSPECIFIED.);
#23953=B_SPLINE_CURVE_WITH_KNOTS('',3,(#158840,#158841,#158842,#158843,
#158844,#158845),.UNSPECIFIED.,.F.,.F.,(4,2,4),(-0.0324734273212292,-0.0162498395840204,
-9.99919512960357E-7),.UNSPECIFIED.);
#23954=B_SPLINE_CURVE_WITH_KNOTS('',3,(#158867,#158868,#158869,#158870,
#158871,#158872,#158873,#158874,#158875,#158876),.UNSPECIFIED.,.F.,.F.,
(4,3,3,4),(1.97891657315654E-11,5.49564847358851E-5,0.000106404139393166,
0.000157852343452837),.UNSPECIFIED.);
#23955=B_SPLINE_CURVE_WITH_KNOTS('',3,(#158905,#158906,#158907,#158908,
#158909,#158910,#158911,#158912,#158913,#158914),.UNSPECIFIED.,.F.,.F.,
(4,3,3,4),(4.45427133556455E-13,1.58768506679322E-5,3.06163004489602E-5,
4.53557651213399E-5),.UNSPECIFIED.);
#23956=B_SPLINE_CURVE_WITH_KNOTS('',3,(#158925,#158926,#158927,#158928,
#158929,#158930,#158931),.UNSPECIFIED.,.F.,.F.,(4,3,4),(0.066525747412771,
0.0687515042650049,0.0736118336413792),.UNSPECIFIED.);
#23957=B_SPLINE_CURVE_WITH_KNOTS('',3,(#158953,#158954,#158955,#158956,
#158957,#158958,#158959,#158960,#158961,#158962),.UNSPECIFIED.,.F.,.F.,
(4,3,3,4),(1.99079370166527E-11,5.49564848485402E-5,0.000106404139310357,
0.000157852343174584),.UNSPECIFIED.);
#23958=B_SPLINE_CURVE_WITH_KNOTS('',3,(#158991,#158992,#158993,#158994,
#158995,#158996,#158997,#158998,#158999,#159000),.UNSPECIFIED.,.F.,.F.,
(4,3,3,4),(4.10262871629452E-13,1.5876850659983E-5,3.06163003713765E-5,
4.53557649741511E-5),.UNSPECIFIED.);
#23959=B_SPLINE_CURVE_WITH_KNOTS('',3,(#159011,#159012,#159013,#159014,
#159015,#159016,#159017),.UNSPECIFIED.,.F.,.F.,(4,3,4),(0.0665257254736557,
0.0687515042650046,0.0736118336259733),.UNSPECIFIED.);
#23960=B_SPLINE_CURVE_WITH_KNOTS('',3,(#159039,#159040,#159041,#159042,
#159043,#159044,#159045,#159046,#159047,#159048),.UNSPECIFIED.,.F.,.F.,
(4,3,3,4),(1.96994503283381E-11,5.49564846894993E-5,0.000106404139458188,
0.000157852343520435),.UNSPECIFIED.);
#23961=B_SPLINE_CURVE_WITH_KNOTS('',3,(#159077,#159078,#159079,#159080,
#159081,#159082,#159083,#159084,#159085,#159086),.UNSPECIFIED.,.F.,.F.,
(4,3,3,4),(4.3756932208846E-13,1.58768506118317E-5,3.06163003591576E-5,
4.5355764997848E-5),.UNSPECIFIED.);
#23962=B_SPLINE_CURVE_WITH_KNOTS('',3,(#159097,#159098,#159099,#159100,
#159101,#159102,#159103),.UNSPECIFIED.,.F.,.F.,(4,3,4),(0.0665257474083367,
0.0687515042650054,0.0736118336568276),.UNSPECIFIED.);
#23963=B_SPLINE_CURVE_WITH_KNOTS('',3,(#159125,#159126,#159127,#159128,
#159129,#159130,#159131,#159132,#159133,#159134),.UNSPECIFIED.,.F.,.F.,
(4,3,3,4),(1.95026631094892E-11,5.49564847805335E-5,0.000106404139539567,
0.000157852343624086),.UNSPECIFIED.);
#23964=B_SPLINE_CURVE_WITH_KNOTS('',3,(#159163,#159164,#159165,#159166,
#159167,#159168,#159169,#159170,#159171,#159172),.UNSPECIFIED.,.F.,.F.,
(4,3,3,4),(5.72598080427875E-13,1.58768505648184E-5,3.0616300343596E-5,
4.53557650137651E-5),.UNSPECIFIED.);
#23965=B_SPLINE_CURVE_WITH_KNOTS('',3,(#159183,#159184,#159185,#159186,
#159187,#159188),.UNSPECIFIED.,.F.,.F.,(4,2,4),(-0.0324734452498497,-0.0162498432494454,
-1.00000000166633E-6),.UNSPECIFIED.);
#23966=B_SPLINE_CURVE_WITH_KNOTS('',3,(#159210,#159211,#159212,#159213,
#159214,#159215,#159216,#159217,#159218,#159219),.UNSPECIFIED.,.F.,.F.,
(4,3,3,4),(1.96990710543907E-11,5.49564848806438E-5,0.000106404139562349,
0.000157852343603431),.UNSPECIFIED.);
#23967=B_SPLINE_CURVE_WITH_KNOTS('',3,(#159248,#159249,#159250,#159251,
#159252,#159253,#159254,#159255,#159256,#159257),.UNSPECIFIED.,.F.,.F.,
(4,3,3,4),(5.42714613550798E-13,1.58768507853872E-5,3.0616300474766E-5,
4.53557650554828E-5),.UNSPECIFIED.);
#23968=B_SPLINE_CURVE_WITH_KNOTS('',3,(#159268,#159269,#159270,#159271,
#159272,#159273),.UNSPECIFIED.,.F.,.F.,(4,2,4),(-0.0324724759362906,-0.0162483528856071,
0.),.UNSPECIFIED.);
#23969=B_SPLINE_CURVE_WITH_KNOTS('',3,(#159295,#159296,#159297,#159298,
#159299,#159300,#159301,#159302,#159303,#159304),.UNSPECIFIED.,.F.,.F.,
(4,3,3,4),(1.91843530344647E-11,5.49564848028284E-5,0.000106404139357679,
0.000157852343315008),.UNSPECIFIED.);
#23970=B_SPLINE_CURVE_WITH_KNOTS('',3,(#159333,#159334,#159335,#159336,
#159337,#159338,#159339,#159340,#159341,#159342),.UNSPECIFIED.,.F.,.F.,
(4,3,3,4),(5.72877897171871E-13,1.58768507696157E-5,3.06163006409456E-5,
4.53557654036395E-5),.UNSPECIFIED.);
#23971=B_SPLINE_CURVE_WITH_KNOTS('',3,(#159353,#159354,#159355,#159356,
#159357,#159358,#159359),.UNSPECIFIED.,.F.,.F.,(4,3,4),(0.0665257474130942,
0.0687515042650042,0.0736118336272697),.UNSPECIFIED.);
#23972=B_SPLINE_CURVE_WITH_KNOTS('',3,(#159381,#159382,#159383,#159384,
#159385,#159386,#159387,#159388,#159389,#159390),.UNSPECIFIED.,.F.,.F.,
(4,3,3,4),(1.96992446166412E-11,5.49564845849989E-5,0.000106404139248683,
0.000157852343250848),.UNSPECIFIED.);
#23973=B_SPLINE_CURVE_WITH_KNOTS('',3,(#159419,#159420,#159421,#159422,
#159423,#159424,#159425,#159426,#159427,#159428),.UNSPECIFIED.,.F.,.F.,
(4,3,3,4),(4.06608505957668E-13,1.58768507642259E-5,3.06163004292337E-5,
4.53557649856869E-5),.UNSPECIFIED.);
#23974=B_SPLINE_CURVE_WITH_KNOTS('',3,(#159439,#159440,#159441,#159442,
#159443,#159444,#159445),.UNSPECIFIED.,.F.,.F.,(4,3,4),(0.0665257474083745,
0.0687515042650048,0.0736118336494111),.UNSPECIFIED.);
#23975=B_SPLINE_CURVE_WITH_KNOTS('',3,(#159467,#159468,#159469,#159470,
#159471,#159472,#159473,#159474,#159475,#159476),.UNSPECIFIED.,.F.,.F.,
(4,3,3,4),(2.00282565627927E-11,5.4956484612054E-5,0.000106404139237452,
0.000157852343260917),.UNSPECIFIED.);
#23976=B_SPLINE_CURVE_WITH_KNOTS('',3,(#159505,#159506,#159507,#159508,
#159509,#159510,#159511,#159512,#159513,#159514),.UNSPECIFIED.,.F.,.F.,
(4,3,3,4),(4.24635773281619E-13,1.58768508533791E-5,3.06163006130592E-5,
4.53557652642364E-5),.UNSPECIFIED.);
#23977=B_SPLINE_CURVE_WITH_KNOTS('',3,(#159525,#159526,#159527,#159528,
#159529,#159530),.UNSPECIFIED.,.F.,.F.,(4,2,4),(-0.0324724492216348,-0.0162483449368564,
0.),.UNSPECIFIED.);
#23978=B_SPLINE_CURVE_WITH_KNOTS('',3,(#159552,#159553,#159554,#159555,
#159556,#159557,#159558,#159559,#159560,#159561),.UNSPECIFIED.,.F.,.F.,
(4,3,3,4),(1.95510594782417E-11,5.49564846343817E-5,0.00010640413941878,
0.000157852343605449),.UNSPECIFIED.);
#23979=B_SPLINE_CURVE_WITH_KNOTS('',3,(#159590,#159591,#159592,#159593,
#159594,#159595,#159596,#159597,#159598,#159599),.UNSPECIFIED.,.F.,.F.,
(4,3,3,4),(5.34422429970871E-13,1.58768507156534E-5,3.06163005847287E-5,
4.5355765345147E-5),.UNSPECIFIED.);
#23980=B_SPLINE_CURVE_WITH_KNOTS('',3,(#159610,#159611,#159612,#159613,
#159614,#159615),.UNSPECIFIED.,.F.,.F.,(4,2,4),(-0.0324724718076845,-0.0162483528768924,
0.),.UNSPECIFIED.);
#23981=B_SPLINE_CURVE_WITH_KNOTS('',3,(#159637,#159638,#159639,#159640,
#159641,#159642,#159643,#159644,#159645,#159646),.UNSPECIFIED.,.F.,.F.,
(4,3,3,4),(1.93183891144322E-11,5.49564847063177E-5,0.000106404139517368,
0.000157852343710412),.UNSPECIFIED.);
#23982=B_SPLINE_CURVE_WITH_KNOTS('',3,(#159675,#159676,#159677,#159678,
#159679,#159680,#159681,#159682,#159683,#159684),.UNSPECIFIED.,.F.,.F.,
(4,3,3,4),(6.12267080355569E-13,1.58768507909601E-5,3.06163004936341E-5,
4.53557650877082E-5),.UNSPECIFIED.);
#23983=B_SPLINE_CURVE_WITH_KNOTS('',3,(#159695,#159696,#159697,#159698,
#159699,#159700,#159701),.UNSPECIFIED.,.F.,.F.,(4,3,4),(0.0665257474091276,
0.0687515042650037,0.0736118336651023),.UNSPECIFIED.);
#23984=B_SPLINE_CURVE_WITH_KNOTS('',3,(#159723,#159724,#159725,#159726,
#159727,#159728,#159729,#159730,#159731,#159732),.UNSPECIFIED.,.F.,.F.,
(4,3,3,4),(1.92577364666127E-11,5.49564845527144E-5,0.000106404139360879,
0.000157852343571467),.UNSPECIFIED.);
#23985=B_SPLINE_CURVE_WITH_KNOTS('',3,(#159761,#159762,#159763,#159764,
#159765,#159766,#159767,#159768,#159769,#159770),.UNSPECIFIED.,.F.,.F.,
(4,3,3,4),(5.30241697382471E-13,1.58768505423667E-5,3.06163004809113E-5,
4.53557653108321E-5),.UNSPECIFIED.);
#23986=B_SPLINE_CURVE_WITH_KNOTS('',3,(#159781,#159782,#159783,#159784,
#159785,#159786),.UNSPECIFIED.,.F.,.F.,(4,2,4),(-0.0324724440917989,-0.0162483453836653,
0.),.UNSPECIFIED.);
#23987=B_SPLINE_CURVE_WITH_KNOTS('',3,(#159808,#159809,#159810,#159811,
#159812,#159813,#159814,#159815,#159816,#159817),.UNSPECIFIED.,.F.,.F.,
(4,3,3,4),(1.96520139212204E-11,5.49564848592545E-5,0.000106404139585418,
0.000157852343532562),.UNSPECIFIED.);
#23988=B_SPLINE_CURVE_WITH_KNOTS('',3,(#159846,#159847,#159848,#159849,
#159850,#159851,#159852,#159853,#159854,#159855),.UNSPECIFIED.,.F.,.F.,
(4,3,3,4),(4.53878480879253E-13,1.58768507388306E-5,3.06163005119187E-5,
4.53557651763179E-5),.UNSPECIFIED.);
#23989=B_SPLINE_CURVE_WITH_KNOTS('',3,(#159866,#159867,#159868,#159869,
#159870,#159871,#159872),.UNSPECIFIED.,.F.,.F.,(4,3,4),(0.0665257474082937,
0.0687515042650046,0.0736118336483852),.UNSPECIFIED.);
#23990=B_SPLINE_CURVE_WITH_KNOTS('',3,(#159894,#159895,#159896,#159897,
#159898,#159899,#159900,#159901,#159902,#159903),.UNSPECIFIED.,.F.,.F.,
(4,3,3,4),(1.92866355622382E-11,5.49564847070356E-5,0.000106404139504483,
0.000157852343704383),.UNSPECIFIED.);
#23991=B_SPLINE_CURVE_WITH_KNOTS('',3,(#159932,#159933,#159934,#159935,
#159936,#159937,#159938,#159939,#159940,#159941),.UNSPECIFIED.,.F.,.F.,
(4,3,3,4),(3.60097101546029E-13,1.58768506767972E-5,3.06163003015025E-5,
4.53557648175994E-5),.UNSPECIFIED.);
#23992=B_SPLINE_CURVE_WITH_KNOTS('',3,(#159952,#159953,#159954,#159955,
#159956,#159957,#159958),.UNSPECIFIED.,.F.,.F.,(4,3,4),(0.0665257474088453,
0.0687515042650069,0.0736118336634073),.UNSPECIFIED.);
#23993=B_SPLINE_CURVE_WITH_KNOTS('',3,(#159980,#159981,#159982,#159983,
#159984,#159985,#159986,#159987,#159988,#159989),.UNSPECIFIED.,.F.,.F.,
(4,3,3,4),(1.975508753699E-11,5.49564846646962E-5,0.000106404139476724,
0.000157852343691029),.UNSPECIFIED.);
#23994=B_SPLINE_CURVE_WITH_KNOTS('',3,(#160018,#160019,#160020,#160021,
#160022,#160023,#160024,#160025,#160026,#160027),.UNSPECIFIED.,.F.,.F.,
(4,3,3,4),(3.55815629379808E-13,1.58768504837401E-5,3.06163004587416E-5,
4.53557653250738E-5),.UNSPECIFIED.);
#23995=B_SPLINE_CURVE_WITH_KNOTS('',3,(#160038,#160039,#160040,#160041,
#160042,#160043,#160044),.UNSPECIFIED.,.F.,.F.,(4,3,4),(0.0665257474135242,
0.0687515042650059,0.0736118336248754),.UNSPECIFIED.);
#23996=B_SPLINE_CURVE_WITH_KNOTS('',3,(#160066,#160067,#160068,#160069,
#160070,#160071,#160072,#160073,#160074,#160075),.UNSPECIFIED.,.F.,.F.,
(4,3,3,4),(1.94487369940343E-11,5.49564848072225E-5,0.000106404139452461,
0.000157852343430733),.UNSPECIFIED.);
#23997=B_SPLINE_CURVE_WITH_KNOTS('',3,(#160104,#160105,#160106,#160107,
#160108,#160109,#160110,#160111,#160112,#160113),.UNSPECIFIED.,.F.,.F.,
(4,3,3,4),(4.88112751114793E-13,1.58768508220155E-5,3.06163006345242E-5,
4.53557653383791E-5),.UNSPECIFIED.);
#23998=B_SPLINE_CURVE_WITH_KNOTS('',3,(#160124,#160125,#160126,#160127,
#160128,#160129,#160130),.UNSPECIFIED.,.F.,.F.,(4,3,4),(0.0665257474068711,
0.0687515042649959,0.0736118336610845),.UNSPECIFIED.);
#23999=B_SPLINE_CURVE_WITH_KNOTS('',3,(#160152,#160153,#160154,#160155,
#160156,#160157,#160158,#160159,#160160,#160161),.UNSPECIFIED.,.F.,.F.,
(4,3,3,4),(1.91069259613115E-11,5.4956484720837E-5,0.000106404139379998,
0.000157852343441449),.UNSPECIFIED.);
#24000=B_SPLINE_CURVE_WITH_KNOTS('',3,(#160190,#160191,#160192,#160193,
#160194,#160195,#160196,#160197,#160198,#160199),.UNSPECIFIED.,.F.,.F.,
(4,3,3,4),(3.43528304253375E-13,1.58768508327752E-5,3.0616300487357E-5,
4.53557650332359E-5),.UNSPECIFIED.);
#24001=B_SPLINE_CURVE_WITH_KNOTS('',3,(#160210,#160211,#160212,#160213,
#160214,#160215),.UNSPECIFIED.,.F.,.F.,(4,2,4),(-0.0324734447985545,-0.0162498503876316,
-1.00000000177736E-6),.UNSPECIFIED.);
#24002=B_SPLINE_CURVE_WITH_KNOTS('',3,(#160237,#160238,#160239,#160240,
#160241,#160242,#160243,#160244,#160245,#160246),.UNSPECIFIED.,.F.,.F.,
(4,3,3,4),(1.91966606562681E-11,5.49564846408601E-5,0.000106404139400499,
0.000157852343415483),.UNSPECIFIED.);
#24003=B_SPLINE_CURVE_WITH_KNOTS('',3,(#160275,#160276,#160277,#160278,
#160279,#160280,#160281,#160282,#160283,#160284),.UNSPECIFIED.,.F.,.F.,
(4,3,3,4),(4.80195844454561E-13,1.58768506961566E-5,3.06163005244348E-5,
4.53557652441286E-5),.UNSPECIFIED.);
#24004=B_SPLINE_CURVE_WITH_KNOTS('',3,(#160295,#160296,#160297,#160298,
#160299,#160300,#160301),.UNSPECIFIED.,.F.,.F.,(4,3,4),(0.0665257474126737,
0.0687515042649959,0.0736118336563353),.UNSPECIFIED.);
#24005=B_SPLINE_CURVE_WITH_KNOTS('',3,(#160323,#160324,#160325,#160326,
#160327,#160328,#160329,#160330,#160331,#160332),.UNSPECIFIED.,.F.,.F.,
(4,3,3,4),(1.95587395262878E-11,5.49564849813836E-5,0.000106404139413079,
0.00015785234324718),.UNSPECIFIED.);
#24006=B_SPLINE_CURVE_WITH_KNOTS('',3,(#160361,#160362,#160363,#160364,
#160365,#160366,#160367,#160368,#160369,#160370),.UNSPECIFIED.,.F.,.F.,
(4,3,3,4),(3.33037896955563E-13,1.5876850567122E-5,3.06163004445858E-5,
4.53557652134316E-5),.UNSPECIFIED.);
#24007=B_SPLINE_CURVE_WITH_KNOTS('',3,(#160381,#160382,#160383,#160384,
#160385,#160386,#160387),.UNSPECIFIED.,.F.,.F.,(4,3,4),(0.0665257474066404,
0.0687515042649958,0.0736118336459457),.UNSPECIFIED.);
#24008=B_SPLINE_CURVE_WITH_KNOTS('',3,(#160409,#160410,#160411,#160412,
#160413,#160414,#160415,#160416,#160417,#160418),.UNSPECIFIED.,.F.,.F.,
(4,3,3,4),(1.99075229772508E-11,5.49564847828955E-5,0.000106404139424612,
0.000157852343348),.UNSPECIFIED.);
#24009=B_SPLINE_CURVE_WITH_KNOTS('',3,(#160447,#160448,#160449,#160450,
#160451,#160452,#160453,#160454,#160455,#160456),.UNSPECIFIED.,.F.,.F.,
(4,3,3,4),(3.41414203172804E-13,1.58768505874591E-5,3.06163003339983E-5,
4.53557649719169E-5),.UNSPECIFIED.);
#24010=B_SPLINE_CURVE_WITH_KNOTS('',3,(#160467,#160468,#160469,#160470,
#160471,#160472,#160473),.UNSPECIFIED.,.F.,.F.,(4,3,4),(0.06652574740877,
0.068751504264996,0.0736118336476656),.UNSPECIFIED.);
#24011=B_SPLINE_CURVE_WITH_KNOTS('',3,(#160495,#160496,#160497,#160498,
#160499,#160500,#160501,#160502,#160503,#160504),.UNSPECIFIED.,.F.,.F.,
(4,3,3,4),(1.94484427579567E-11,5.49564846028534E-5,0.00010640413945402,
0.000157852343648001),.UNSPECIFIED.);
#24012=B_SPLINE_CURVE_WITH_KNOTS('',3,(#160533,#160534,#160535,#160536,
#160537,#160538,#160539,#160540,#160541,#160542),.UNSPECIFIED.,.F.,.F.,
(4,3,3,4),(4.15431761292954E-13,1.58768508092275E-5,3.06163004475716E-5,
4.5355764977311E-5),.UNSPECIFIED.);
#24013=B_SPLINE_CURVE_WITH_KNOTS('',3,(#160553,#160554,#160555,#160556,
#160557,#160558,#160559),.UNSPECIFIED.,.F.,.F.,(4,3,4),(0.0665257474138115,
0.0687515042649961,0.0736118336459126),.UNSPECIFIED.);
#24014=B_SPLINE_CURVE_WITH_KNOTS('',3,(#160581,#160582,#160583,#160584,
#160585,#160586,#160587,#160588,#160589,#160590),.UNSPECIFIED.,.F.,.F.,
(4,3,3,4),(1.96216466760054E-11,5.4956484902517E-5,0.000106404139425267,
0.000157852343253078),.UNSPECIFIED.);
#24015=B_SPLINE_CURVE_WITH_KNOTS('',3,(#160609,#160610,#160611,#160612,
#160613,#160614),.UNSPECIFIED.,.F.,.F.,(4,2,4),(3.50146860978608E-11,0.0126520282634591,
0.025303829872637),.UNSPECIFIED.);
#24016=B_SPLINE_CURVE_WITH_KNOTS('',3,(#160634,#160635,#160636,#160637,
#160638,#160639),.UNSPECIFIED.,.F.,.F.,(4,2,4),(0.,0.0126520258962633,0.025303824074642),
 .UNSPECIFIED.);
#24017=B_SPLINE_CURVE_WITH_KNOTS('',3,(#160659,#160660,#160661,#160662,
#160663,#160664),.UNSPECIFIED.,.F.,.F.,(4,2,4),(0.,0.0126520281025744,0.0253038295843138),
 .UNSPECIFIED.);
#24018=B_SPLINE_CURVE_WITH_KNOTS('',3,(#160684,#160685,#160686,#160687,
#160688,#160689),.UNSPECIFIED.,.F.,.F.,(4,2,4),(0.,0.0126520265670996,0.0253038257319735),
 .UNSPECIFIED.);
#24019=B_SPLINE_CURVE_WITH_KNOTS('',3,(#160709,#160710,#160711,#160712,
#160713,#160714),.UNSPECIFIED.,.F.,.F.,(4,2,4),(0.,0.0126520266851299,0.0253038261543005),
 .UNSPECIFIED.);
#24020=B_SPLINE_CURVE_WITH_KNOTS('',3,(#160734,#160735,#160736,#160737,
#160738,#160739),.UNSPECIFIED.,.F.,.F.,(4,2,4),(0.,0.012652026020123,0.0253038244493337),
 .UNSPECIFIED.);
#24021=B_SPLINE_CURVE_WITH_KNOTS('',3,(#160759,#160760,#160761,#160762,
#160763,#160764),.UNSPECIFIED.,.F.,.F.,(4,2,4),(0.,0.0126520262984874,0.0253038249916903),
 .UNSPECIFIED.);
#24022=B_SPLINE_CURVE_WITH_KNOTS('',3,(#160784,#160785,#160786,#160787,
#160788,#160789),.UNSPECIFIED.,.F.,.F.,(4,2,4),(0.,0.0126520282590167,0.025303829881957),
 .UNSPECIFIED.);
#24023=B_SPLINE_CURVE_WITH_KNOTS('',3,(#160809,#160810,#160811,#160812,
#160813,#160814),.UNSPECIFIED.,.F.,.F.,(4,2,4),(0.,0.0126520269368647,0.0253038266869163),
 .UNSPECIFIED.);
#24024=B_SPLINE_CURVE_WITH_KNOTS('',3,(#160834,#160835,#160836,#160837,
#160838,#160839),.UNSPECIFIED.,.F.,.F.,(4,2,4),(0.,0.0126520263342759,0.0253038251684596),
 .UNSPECIFIED.);
#24025=B_SPLINE_CURVE_WITH_KNOTS('',3,(#160859,#160860,#160861,#160862,
#160863,#160864),.UNSPECIFIED.,.F.,.F.,(4,2,4),(0.,0.0126520256408363,0.0253038236240611),
 .UNSPECIFIED.);
#24026=B_SPLINE_CURVE_WITH_KNOTS('',3,(#160884,#160885,#160886,#160887,
#160888,#160889),.UNSPECIFIED.,.F.,.F.,(4,2,4),(0.,0.012652027883969,0.0253038291064795),
 .UNSPECIFIED.);
#24027=B_SPLINE_CURVE_WITH_KNOTS('',3,(#160909,#160910,#160911,#160912,
#160913,#160914),.UNSPECIFIED.,.F.,.F.,(4,2,4),(2.283603133213E-11,0.0126520283107723,
0.0253038299118963),.UNSPECIFIED.);
#24028=B_SPLINE_CURVE_WITH_KNOTS('',3,(#160934,#160935,#160936,#160937,
#160938,#160939),.UNSPECIFIED.,.F.,.F.,(4,2,4),(0.,0.0126520276386329,0.0253038283858036),
 .UNSPECIFIED.);
#24029=B_SPLINE_CURVE_WITH_KNOTS('',3,(#160959,#160960,#160961,#160962,
#160963,#160964),.UNSPECIFIED.,.F.,.F.,(4,2,4),(1.73862291501938E-9,0.0126520270262746,
0.0253038246440909),.UNSPECIFIED.);
#24030=B_SPLINE_CURVE_WITH_KNOTS('',3,(#160984,#160985,#160986,#160987,
#160988,#160989),.UNSPECIFIED.,.F.,.F.,(4,2,4),(0.,0.0126520283246941,0.0253038302032181),
 .UNSPECIFIED.);
#24031=B_SPLINE_CURVE_WITH_KNOTS('',3,(#161009,#161010,#161011,#161012,
#161013,#161014),.UNSPECIFIED.,.F.,.F.,(4,2,4),(0.,0.0126520255277967,0.0253038232885518),
 .UNSPECIFIED.);
#24032=B_SPLINE_CURVE_WITH_KNOTS('',3,(#161034,#161035,#161036,#161037,
#161038,#161039),.UNSPECIFIED.,.F.,.F.,(4,2,4),(6.06839707590124E-13,0.0126520265612889,
0.02530382571351),.UNSPECIFIED.);
#24033=B_SPLINE_CURVE_WITH_KNOTS('',3,(#161059,#161060,#161061,#161062,
#161063,#161064),.UNSPECIFIED.,.F.,.F.,(4,2,4),(0.,0.0126520273330737,0.025303827547897),
 .UNSPECIFIED.);
#24034=B_SPLINE_CURVE_WITH_KNOTS('',3,(#161084,#161085,#161086,#161087,
#161088,#161089),.UNSPECIFIED.,.F.,.F.,(4,2,4),(0.,0.0126520266653492,0.0253038258407741),
 .UNSPECIFIED.);
#24035=B_SPLINE_CURVE_WITH_KNOTS('',3,(#161109,#161110,#161111,#161112,
#161113,#161114),.UNSPECIFIED.,.F.,.F.,(4,2,4),(1.70116744281899E-11,0.012652028270309,
0.0253038299189388),.UNSPECIFIED.);
#24036=B_SPLINE_CURVE_WITH_KNOTS('',3,(#161134,#161135,#161136,#161137,
#161138,#161139),.UNSPECIFIED.,.F.,.F.,(4,2,4),(0.,0.012652026346306,0.0253038252129835),
 .UNSPECIFIED.);
#24037=B_SPLINE_CURVE_WITH_KNOTS('',3,(#161159,#161160,#161161,#161162,
#161163,#161164),.UNSPECIFIED.,.F.,.F.,(4,2,4),(0.,0.0126520272288475,0.0253038274605735),
 .UNSPECIFIED.);
#24038=B_SPLINE_CURVE_WITH_KNOTS('',3,(#161184,#161185,#161186,#161187,
#161188,#161189),.UNSPECIFIED.,.F.,.F.,(4,2,4),(0.,0.0126520253434002,0.0253038227547039),
 .UNSPECIFIED.);
#24039=B_SPLINE_CURVE_WITH_KNOTS('',3,(#161209,#161210,#161211,#161212,
#161213,#161214),.UNSPECIFIED.,.F.,.F.,(4,2,4),(0.,0.0126520265495153,0.025303825763251),
 .UNSPECIFIED.);
#24040=B_SPLINE_CURVE_WITH_KNOTS('',3,(#161234,#161235,#161236,#161237,
#161238,#161239),.UNSPECIFIED.,.F.,.F.,(4,2,4),(0.,0.0126520265638083,0.0253038256562407),
 .UNSPECIFIED.);
#24041=B_SPLINE_CURVE_WITH_KNOTS('',3,(#161259,#161260,#161261,#161262,
#161263,#161264),.UNSPECIFIED.,.F.,.F.,(4,2,4),(0.,0.0126520252611529,0.0253038225702637),
 .UNSPECIFIED.);
#24042=B_SPLINE_CURVE_WITH_KNOTS('',3,(#161284,#161285,#161286,#161287,
#161288,#161289),.UNSPECIFIED.,.F.,.F.,(4,2,4),(0.,0.0126520278786851,0.0253038289796549),
 .UNSPECIFIED.);
#24043=B_SPLINE_CURVE_WITH_KNOTS('',3,(#161309,#161310,#161311,#161312,
#161313,#161314),.UNSPECIFIED.,.F.,.F.,(4,2,4),(0.,0.0126520284756542,0.0253038304784128),
 .UNSPECIFIED.);
#24044=B_SPLINE_CURVE_WITH_KNOTS('',3,(#161340,#161341,#161342,#161343,
#161344,#161345),.UNSPECIFIED.,.F.,.F.,(4,2,4),(-0.0253039879324086,-0.0126518800290025,
-1.10254964880152E-11),.UNSPECIFIED.);
#24045=B_SPLINE_CURVE_WITH_KNOTS('',3,(#161355,#161356,#161357,#161358,
#161359,#161360),.UNSPECIFIED.,.F.,.F.,(4,2,4),(1.52206643631891E-9,0.0126518815909643,
0.0253039868896389),.UNSPECIFIED.);
#24046=B_SPLINE_CURVE_WITH_KNOTS('',3,(#161394,#161395,#161396,#161397,
#161398,#161399),.UNSPECIFIED.,.F.,.F.,(4,2,4),(1.51612725093129E-9,0.0126518816134216,
0.025303986957009),.UNSPECIFIED.);
#24047=B_SPLINE_CURVE_WITH_KNOTS('',3,(#161433,#161434,#161435,#161436,
#161437,#161438),.UNSPECIFIED.,.F.,.F.,(4,2,4),(1.43547212827194E-9,0.0126518815341548,
0.0253039869610686),.UNSPECIFIED.);
#24048=B_SPLINE_CURVE_WITH_KNOTS('',3,(#161472,#161473,#161474,#161475,
#161476,#161477),.UNSPECIFIED.,.F.,.F.,(4,2,4),(1.40821217994557E-9,0.0126518814793586,
0.0253039869121775),.UNSPECIFIED.);
#24049=B_SPLINE_CURVE_WITH_KNOTS('',3,(#161511,#161512,#161513,#161514,
#161515,#161516),.UNSPECIFIED.,.F.,.F.,(4,2,4),(1.34058371660886E-9,0.0126518813899474,
0.0253039868784617),.UNSPECIFIED.);
#24050=B_SPLINE_CURVE_WITH_KNOTS('',3,(#161550,#161551,#161552,#161553,
#161554,#161555),.UNSPECIFIED.,.F.,.F.,(4,2,4),(1.50113469982618E-9,0.01265188158503,
0.0253039869826423),.UNSPECIFIED.);
#24051=B_SPLINE_CURVE_WITH_KNOTS('',3,(#161586,#161587,#161588,#161589,
#161590,#161591),.UNSPECIFIED.,.F.,.F.,(4,2,4),(1.50445324217149E-9,0.0126518816050577,
0.025303986954268),.UNSPECIFIED.);
#24052=B_SPLINE_CURVE_WITH_KNOTS('',3,(#161617,#161618,#161619,#161620,
#161621,#161622),.UNSPECIFIED.,.F.,.F.,(4,2,4),(1.52727531068401E-9,0.0126518816268682,
0.0253039869661077),.UNSPECIFIED.);
#24053=B_SPLINE_CURVE_WITH_KNOTS('',3,(#161656,#161657,#161658,#161659,
#161660,#161661),.UNSPECIFIED.,.F.,.F.,(4,2,4),(1.41870323249377E-9,0.012651881462905,
0.0253039868467572),.UNSPECIFIED.);
#24054=B_SPLINE_CURVE_WITH_KNOTS('',3,(#161695,#161696,#161697,#161698,
#161699,#161700),.UNSPECIFIED.,.F.,.F.,(4,2,4),(1.53232704557586E-9,0.012651881631661,
0.0253039869495135),.UNSPECIFIED.);
#24055=B_SPLINE_CURVE_WITH_KNOTS('',3,(#161734,#161735,#161736,#161737,
#161738,#161739),.UNSPECIFIED.,.F.,.F.,(4,2,4),(1.38628499338917E-9,0.0126518814663333,
0.0253039869324201),.UNSPECIFIED.);
#24056=B_SPLINE_CURVE_WITH_KNOTS('',3,(#161773,#161774,#161775,#161776,
#161777,#161778),.UNSPECIFIED.,.F.,.F.,(4,2,4),(1.43816896721697E-9,0.0126518814925827,
0.0253039868824678),.UNSPECIFIED.);
#24057=B_SPLINE_CURVE_WITH_KNOTS('',3,(#161812,#161813,#161814,#161815,
#161816,#161817),.UNSPECIFIED.,.F.,.F.,(4,2,4),(1.41531481175481E-9,0.0126518814869672,
0.0253039869094249),.UNSPECIFIED.);
#24058=B_SPLINE_CURVE_WITH_KNOTS('',3,(#161851,#161852,#161853,#161854,
#161855,#161856),.UNSPECIFIED.,.F.,.F.,(4,2,4),(1.50211413795707E-9,0.012651881579894,
0.0253039869249388),.UNSPECIFIED.);
#24059=B_SPLINE_CURVE_WITH_KNOTS('',3,(#161890,#161891,#161892,#161893,
#161894,#161895),.UNSPECIFIED.,.F.,.F.,(4,2,4),(1.4974251600475E-9,0.0126518815659028,
0.0253039869225986),.UNSPECIFIED.);
#24060=B_SPLINE_CURVE_WITH_KNOTS('',3,(#161929,#161930,#161931,#161932,
#161933,#161934),.UNSPECIFIED.,.F.,.F.,(4,2,4),(1.44629883447371E-9,0.0126518815283366,
0.0253039869307436),.UNSPECIFIED.);
#24061=B_SPLINE_CURVE_WITH_KNOTS('',3,(#161968,#161969,#161970,#161971,
#161972,#161973),.UNSPECIFIED.,.F.,.F.,(4,2,4),(1.47110006734065E-9,0.0126518815235758,
0.0253039868593664),.UNSPECIFIED.);
#24062=B_SPLINE_CURVE_WITH_KNOTS('',3,(#162008,#162009,#162010,#162011,
#162012,#162013),.UNSPECIFIED.,.F.,.F.,(4,2,4),(1.4826859213418E-9,0.0126518815996713,
0.0253039869934791),.UNSPECIFIED.);
#24063=B_SPLINE_CURVE_WITH_KNOTS('',3,(#162046,#162047,#162048,#162049,
#162050,#162051),.UNSPECIFIED.,.F.,.F.,(4,2,4),(1.51322869999487E-9,0.0126518816030172,
0.0253039869465037),.UNSPECIFIED.);
#24064=B_SPLINE_CURVE_WITH_KNOTS('',3,(#162085,#162086,#162087,#162088,
#162089,#162090),.UNSPECIFIED.,.F.,.F.,(4,2,4),(1.44312089558744E-9,0.0126518814908936,
0.0253039868677599),.UNSPECIFIED.);
#24065=B_SPLINE_CURVE_WITH_KNOTS('',3,(#162124,#162125,#162126,#162127,
#162128,#162129),.UNSPECIFIED.,.F.,.F.,(4,2,4),(1.38491957805618E-9,0.0126518814509472,
0.0253039869037668),.UNSPECIFIED.);
#24066=B_SPLINE_CURVE_WITH_KNOTS('',3,(#162163,#162164,#162165,#162166,
#162167,#162168),.UNSPECIFIED.,.F.,.F.,(4,2,4),(1.4442356085963E-9,0.012651881521997,
0.0253039869119498),.UNSPECIFIED.);
#24067=B_SPLINE_CURVE_WITH_KNOTS('',3,(#162202,#162203,#162204,#162205,
#162206,#162207),.UNSPECIFIED.,.F.,.F.,(4,2,4),(1.4282679182595E-9,0.0126518815081054,
0.0253039869290959),.UNSPECIFIED.);
#24068=B_SPLINE_CURVE_WITH_KNOTS('',3,(#162241,#162242,#162243,#162244,
#162245,#162246),.UNSPECIFIED.,.F.,.F.,(4,2,4),(1.45021697356858E-9,0.012651881537926,
0.0253039869495223),.UNSPECIFIED.);
#24069=B_SPLINE_CURVE_WITH_KNOTS('',3,(#162280,#162281,#162282,#162283,
#162284,#162285),.UNSPECIFIED.,.F.,.F.,(4,2,4),(1.57796420795521E-9,0.0126518816874471,
0.0253039869733485),.UNSPECIFIED.);
#24070=B_SPLINE_CURVE_WITH_KNOTS('',3,(#162319,#162320,#162321,#162322,
#162323,#162324),.UNSPECIFIED.,.F.,.F.,(4,2,4),(1.54977618130921E-9,0.0126518816622565,
0.0253039869718755),.UNSPECIFIED.);
#24071=B_SPLINE_CURVE_WITH_KNOTS('',3,(#162358,#162359,#162360,#162361,
#162362,#162363),.UNSPECIFIED.,.F.,.F.,(4,2,4),(1.41539846907942E-9,0.0126518814803473,
0.0253039869013059),.UNSPECIFIED.);
#24072=B_SPLINE_CURVE_WITH_KNOTS('',3,(#162397,#162398,#162399,#162400,
#162401,#162402),.UNSPECIFIED.,.F.,.F.,(4,2,4),(1.48230471024643E-9,0.0126518815759344,
0.0253039869544491),.UNSPECIFIED.);
#24073=B_SPLINE_CURVE_WITH_KNOTS('',3,(#163039,#163040,#163041,#163042,
#163043,#163044),.UNSPECIFIED.,.F.,.F.,(4,2,4),(0.,0.0318022370486529,0.0638030677158179),
 .UNSPECIFIED.);
#24074=B_SPLINE_CURVE_WITH_KNOTS('',3,(#163045,#163046,#163047,#163048,
#163049,#163050),.UNSPECIFIED.,.F.,.F.,(4,2,4),(8.7491300728103E-11,0.0129043685365852,
0.0270905602892694),.UNSPECIFIED.);
#24075=B_SPLINE_CURVE_WITH_KNOTS('',3,(#163054,#163055,#163056,#163057,
#163058,#163059,#163060,#163061),.UNSPECIFIED.,.F.,.F.,(4,2,2,4),(1.00010025441208E-6,
0.0146013173462511,0.0279117437094298,0.0546218077071897),.UNSPECIFIED.);
#24076=B_SPLINE_CURVE_WITH_KNOTS('',3,(#163062,#163063,#163064,#163065,
#163066,#163067),.UNSPECIFIED.,.F.,.F.,(4,2,4),(0.000862177893008277,0.0332709227757339,
0.0654912697583216),.UNSPECIFIED.);
#24077=B_SPLINE_CURVE_WITH_KNOTS('',3,(#163068,#163069,#163070,#163071,
#163072,#163073,#163074,#163075),.UNSPECIFIED.,.F.,.F.,(4,2,2,4),(1.00002233420631E-6,
0.0322596484018977,0.048328981802378,0.0657704349945425),.UNSPECIFIED.);
#24078=B_SPLINE_CURVE_WITH_KNOTS('',3,(#163098,#163099,#163100,#163101,
#163102,#163103),.UNSPECIFIED.,.F.,.F.,(4,2,4),(0.,0.0318022366302916,0.0638030661107383),
 .UNSPECIFIED.);
#24079=B_SPLINE_CURVE_WITH_KNOTS('',3,(#163104,#163105,#163106,#163107,
#163108,#163109),.UNSPECIFIED.,.F.,.F.,(4,2,4),(1.37609960883432E-10,0.0129043686339332,
0.0270905603810427),.UNSPECIFIED.);
#24080=B_SPLINE_CURVE_WITH_KNOTS('',3,(#163113,#163114,#163115,#163116,
#163117,#163118,#163119,#163120),.UNSPECIFIED.,.F.,.F.,(4,2,2,4),(1.00011427568223E-6,
0.014601317221349,0.0279117434743883,0.0546218072225535),.UNSPECIFIED.);
#24081=B_SPLINE_CURVE_WITH_KNOTS('',3,(#163121,#163122,#163123,#163124,
#163125,#163126),.UNSPECIFIED.,.F.,.F.,(4,2,4),(0.000862177877279032,0.0332709227985011,
0.0654912694116861),.UNSPECIFIED.);
#24082=B_SPLINE_CURVE_WITH_KNOTS('',3,(#163127,#163128,#163129,#163130,
#163131,#163132,#163133,#163134),.UNSPECIFIED.,.F.,.F.,(4,2,2,4),(1.00001041491299E-6,
0.0322596485585965,0.0483293807968369,0.0657704943362129),.UNSPECIFIED.);
#24083=B_SPLINE_CURVE_WITH_KNOTS('',3,(#163157,#163158,#163159,#163160,
#163161,#163162),.UNSPECIFIED.,.F.,.F.,(4,2,4),(0.,0.0318022365401368,0.0638030657211654),
 .UNSPECIFIED.);
#24084=B_SPLINE_CURVE_WITH_KNOTS('',3,(#163163,#163164,#163165,#163166,
#163167,#163168),.UNSPECIFIED.,.F.,.F.,(4,2,4),(1.56778555886997E-10,0.0129043686228877,
0.0270905603149191),.UNSPECIFIED.);
#24085=B_SPLINE_CURVE_WITH_KNOTS('',3,(#163172,#163173,#163174,#163175,
#163176,#163177,#163178,#163179),.UNSPECIFIED.,.F.,.F.,(4,2,2,4),(1.00005385785841E-6,
0.0146013173333266,0.0279117437159111,0.0546218077264354),.UNSPECIFIED.);
#24086=B_SPLINE_CURVE_WITH_KNOTS('',3,(#163180,#163181,#163182,#163183,
#163184,#163185),.UNSPECIFIED.,.F.,.F.,(4,2,4),(0.00086217789495907,0.0332709228025803,
0.0654912700336115),.UNSPECIFIED.);
#24087=B_SPLINE_CURVE_WITH_KNOTS('',3,(#163186,#163187,#163188,#163189,
#163190,#163191,#163192,#163193),.UNSPECIFIED.,.F.,.F.,(4,2,2,4),(1.00002524481216E-6,
0.0322596484594912,0.0483289818203511,0.0657704376678658),.UNSPECIFIED.);
#24088=B_SPLINE_CURVE_WITH_KNOTS('',3,(#163216,#163217,#163218,#163219,
#163220,#163221),.UNSPECIFIED.,.F.,.F.,(4,2,4),(0.,0.0318022368851196,0.0638030671062939),
 .UNSPECIFIED.);
#24089=B_SPLINE_CURVE_WITH_KNOTS('',3,(#163222,#163223,#163224,#163225,
#163226,#163227),.UNSPECIFIED.,.F.,.F.,(4,2,4),(6.96464037490181E-11,0.0129043685514154,
0.0270905603507981),.UNSPECIFIED.);
#24090=B_SPLINE_CURVE_WITH_KNOTS('',3,(#163231,#163232,#163233,#163234,
#163235,#163236,#163237,#163238),.UNSPECIFIED.,.F.,.F.,(4,2,2,4),(1.00000561038452E-6,
0.0146013174108614,0.0279117438241032,0.0546218079462628),.UNSPECIFIED.);
#24091=B_SPLINE_CURVE_WITH_KNOTS('',3,(#163239,#163240,#163241,#163242,
#163243,#163244),.UNSPECIFIED.,.F.,.F.,(4,2,4),(0.000862177865670856,0.0332709227848291,
0.0654912681350928),.UNSPECIFIED.);
#24092=B_SPLINE_CURVE_WITH_KNOTS('',3,(#163245,#163246,#163247,#163248,
#163249,#163250,#163251,#163252),.UNSPECIFIED.,.F.,.F.,(4,2,2,4),(1.00002366431758E-6,
0.032259648361095,0.0483289818685821,0.0657705256693144),.UNSPECIFIED.);
#24093=B_SPLINE_CURVE_WITH_KNOTS('',3,(#163275,#163276,#163277,#163278,
#163279,#163280),.UNSPECIFIED.,.F.,.F.,(4,2,4),(0.,0.0318022368256888,0.0638030668561903),
 .UNSPECIFIED.);
#24094=B_SPLINE_CURVE_WITH_KNOTS('',3,(#163281,#163282,#163283,#163284,
#163285,#163286),.UNSPECIFIED.,.F.,.F.,(4,2,4),(1.2210755509226E-10,0.0129043685695377,
0.0270905602832235),.UNSPECIFIED.);
#24095=B_SPLINE_CURVE_WITH_KNOTS('',3,(#163290,#163291,#163292,#163293,
#163294,#163295,#163296,#163297),.UNSPECIFIED.,.F.,.F.,(4,2,2,4),(1.00004953502741E-6,
0.0146013174148623,0.0279117438317188,0.0546218079602826),.UNSPECIFIED.);
#24096=B_SPLINE_CURVE_WITH_KNOTS('',3,(#163298,#163299,#163300,#163301,
#163302,#163303),.UNSPECIFIED.,.F.,.F.,(4,2,4),(0.000862177878398796,0.0332709228090972,
0.0654912687885388),.UNSPECIFIED.);
#24097=B_SPLINE_CURVE_WITH_KNOTS('',3,(#163304,#163305,#163306,#163307,
#163308,#163309,#163310,#163311),.UNSPECIFIED.,.F.,.F.,(4,2,2,4),(1.00001979611187E-6,
0.0322596483810105,0.048328981853273,0.0657704806604372),.UNSPECIFIED.);
#24098=B_SPLINE_CURVE_WITH_KNOTS('',3,(#163334,#163335,#163336,#163337,
#163338,#163339),.UNSPECIFIED.,.F.,.F.,(4,2,4),(0.,0.0318022366459589,0.0638030661171089),
 .UNSPECIFIED.);
#24099=B_SPLINE_CURVE_WITH_KNOTS('',3,(#163340,#163341,#163342,#163343,
#163344,#163345),.UNSPECIFIED.,.F.,.F.,(4,2,4),(1.3871504433622E-10,0.0129043686056305,
0.027090560316242),.UNSPECIFIED.);
#24100=B_SPLINE_CURVE_WITH_KNOTS('',3,(#163349,#163350,#163351,#163352,
#163353,#163354,#163355,#163356),.UNSPECIFIED.,.F.,.F.,(4,2,2,4),(1.00010651614903E-6,
0.014601317341088,0.0279117437055757,0.0546218077017514),.UNSPECIFIED.);
#24101=B_SPLINE_CURVE_WITH_KNOTS('',3,(#163357,#163358,#163359,#163360,
#163361,#163362),.UNSPECIFIED.,.F.,.F.,(4,2,4),(0.000862177886856545,0.0332709227980972,
0.0654912694331754),.UNSPECIFIED.);
#24102=B_SPLINE_CURVE_WITH_KNOTS('',3,(#163363,#163364,#163365,#163366,
#163367,#163368,#163369,#163370),.UNSPECIFIED.,.F.,.F.,(4,2,2,4),(1.00002623835471E-6,
0.0322596484247313,0.0483289819388386,0.0657704876040361),.UNSPECIFIED.);
#24103=B_SPLINE_CURVE_WITH_KNOTS('',3,(#163393,#163394,#163395,#163396,
#163397,#163398),.UNSPECIFIED.,.F.,.F.,(4,2,4),(0.,0.031802237071236,0.063803067841117),
 .UNSPECIFIED.);
#24104=B_SPLINE_CURVE_WITH_KNOTS('',3,(#163399,#163400,#163401,#163402,
#163403,#163404),.UNSPECIFIED.,.F.,.F.,(4,2,4),(8.97238040975725E-11,0.0129043685964079,
0.0270905603759876),.UNSPECIFIED.);
#24105=B_SPLINE_CURVE_WITH_KNOTS('',3,(#163408,#163409,#163410,#163411,
#163412,#163413,#163414,#163415),.UNSPECIFIED.,.F.,.F.,(4,2,2,4),(1.00002862386086E-6,
0.0146013173707883,0.0279117437374226,0.0546218077585137),.UNSPECIFIED.);
#24106=B_SPLINE_CURVE_WITH_KNOTS('',3,(#163416,#163417,#163418,#163419,
#163420,#163421),.UNSPECIFIED.,.F.,.F.,(4,2,4),(0.000862177885270482,0.0332709227980682,
0.0654912690986148),.UNSPECIFIED.);
#24107=B_SPLINE_CURVE_WITH_KNOTS('',3,(#163422,#163423,#163424,#163425,
#163426,#163427,#163428,#163429),.UNSPECIFIED.,.F.,.F.,(4,2,2,4),(1.00002356029572E-6,
0.0322596484060167,0.048328981827194,0.0657704543396389),.UNSPECIFIED.);
#24108=B_SPLINE_CURVE_WITH_KNOTS('',3,(#163452,#163453,#163454,#163455,
#163456,#163457),.UNSPECIFIED.,.F.,.F.,(4,2,4),(0.,0.0318022368265858,0.0638030668440867),
 .UNSPECIFIED.);
#24109=B_SPLINE_CURVE_WITH_KNOTS('',3,(#163458,#163459,#163460,#163461,
#163462,#163463),.UNSPECIFIED.,.F.,.F.,(4,2,4),(7.73312172257338E-11,0.0129043685463946,
0.0270905603278464),.UNSPECIFIED.);
#24110=B_SPLINE_CURVE_WITH_KNOTS('',3,(#163467,#163468,#163469,#163470,
#163471,#163472,#163473,#163474),.UNSPECIFIED.,.F.,.F.,(4,2,2,4),(1.00003343547171E-6,
0.0146013172580736,0.0279117435229017,0.0546218073061002),.UNSPECIFIED.);
#24111=B_SPLINE_CURVE_WITH_KNOTS('',3,(#163475,#163476,#163477,#163478,
#163479,#163480),.UNSPECIFIED.,.F.,.F.,(4,2,4),(0.000862177869507918,0.0332709228067202,
0.0654912684970968),.UNSPECIFIED.);
#24112=B_SPLINE_CURVE_WITH_KNOTS('',3,(#163481,#163482,#163483,#163484,
#163485,#163486,#163487,#163488),.UNSPECIFIED.,.F.,.F.,(4,2,2,4),(1.00000000542028E-6,
0.0322601579816196,0.048329645776346,0.0657704668609788),.UNSPECIFIED.);
#24113=B_SPLINE_CURVE_WITH_KNOTS('',3,(#163511,#163512,#163513,#163514,
#163515,#163516),.UNSPECIFIED.,.F.,.F.,(4,2,4),(0.,0.0318022366541384,0.0638030661905318),
 .UNSPECIFIED.);
#24114=B_SPLINE_CURVE_WITH_KNOTS('',3,(#163517,#163518,#163519,#163520,
#163521,#163522),.UNSPECIFIED.,.F.,.F.,(4,2,4),(1.12505063382816E-10,0.0129043685892822,
0.0270905603283878),.UNSPECIFIED.);
#24115=B_SPLINE_CURVE_WITH_KNOTS('',3,(#163526,#163527,#163528,#163529,
#163530,#163531,#163532,#163533),.UNSPECIFIED.,.F.,.F.,(4,2,2,4),(1.00012890021697E-6,
0.0146013173418215,0.0279117436722552,0.0546218076156347),.UNSPECIFIED.);
#24116=B_SPLINE_CURVE_WITH_KNOTS('',3,(#163534,#163535,#163536,#163537,
#163538,#163539),.UNSPECIFIED.,.F.,.F.,(4,2,4),(0.000862177889171675,0.0332709228033765,
0.0654912698035889),.UNSPECIFIED.);
#24117=B_SPLINE_CURVE_WITH_KNOTS('',3,(#163540,#163541,#163542,#163543,
#163544,#163545,#163546,#163547),.UNSPECIFIED.,.F.,.F.,(4,2,2,4),(1.00002679077808E-6,
0.0322596484275461,0.048328981818852,0.0657704591728584),.UNSPECIFIED.);
#24118=B_SPLINE_CURVE_WITH_KNOTS('',3,(#163570,#163571,#163572,#163573,
#163574,#163575),.UNSPECIFIED.,.F.,.F.,(4,2,4),(0.,0.0318022371744154,0.0638030681800889),
 .UNSPECIFIED.);
#24119=B_SPLINE_CURVE_WITH_KNOTS('',3,(#163576,#163577,#163578,#163579,
#163580,#163581),.UNSPECIFIED.,.F.,.F.,(4,2,4),(9.91423357346709E-11,0.0129043685986688,
0.0270905603679262),.UNSPECIFIED.);
#24120=B_SPLINE_CURVE_WITH_KNOTS('',3,(#163585,#163586,#163587,#163588,
#163589,#163590,#163591,#163592),.UNSPECIFIED.,.F.,.F.,(4,2,2,4),(1.00003733888782E-6,
0.0146013174139753,0.0279117438449331,0.0546218080025472),.UNSPECIFIED.);
#24121=B_SPLINE_CURVE_WITH_KNOTS('',3,(#163593,#163594,#163595,#163596,
#163597,#163598),.UNSPECIFIED.,.F.,.F.,(4,2,4),(0.000862177880280482,0.0332709227870337,
0.0654912695286052),.UNSPECIFIED.);
#24122=B_SPLINE_CURVE_WITH_KNOTS('',3,(#163599,#163600,#163601,#163602,
#163603,#163604,#163605,#163606),.UNSPECIFIED.,.F.,.F.,(4,2,2,4),(1.00002302923444E-6,
0.0322596484271033,0.0483289818283658,0.0657703792188617),.UNSPECIFIED.);
#24123=B_SPLINE_CURVE_WITH_KNOTS('',3,(#163629,#163630,#163631,#163632,
#163633,#163634),.UNSPECIFIED.,.F.,.F.,(4,2,4),(0.,0.0318022370000935,0.0638030675232337),
 .UNSPECIFIED.);
#24124=B_SPLINE_CURVE_WITH_KNOTS('',3,(#163635,#163636,#163637,#163638,
#163639,#163640),.UNSPECIFIED.,.F.,.F.,(4,2,4),(1.9267454212823E-10,0.0129043686879843,
0.0270905603704255),.UNSPECIFIED.);
#24125=B_SPLINE_CURVE_WITH_KNOTS('',3,(#163644,#163645,#163646,#163647,
#163648,#163649,#163650,#163651),.UNSPECIFIED.,.F.,.F.,(4,2,2,4),(1.0000842295421E-6,
0.0146013174557693,0.027911743968052,0.054621808273341),.UNSPECIFIED.);
#24126=B_SPLINE_CURVE_WITH_KNOTS('',3,(#163652,#163653,#163654,#163655,
#163656,#163657),.UNSPECIFIED.,.F.,.F.,(4,2,4),(0.000862177868208357,0.0332709228138138,
0.0654912705713705),.UNSPECIFIED.);
#24127=B_SPLINE_CURVE_WITH_KNOTS('',3,(#163658,#163659,#163660,#163661,
#163662,#163663,#163664,#163665),.UNSPECIFIED.,.F.,.F.,(4,2,2,4),(1.00002005209412E-6,
0.0322596484007827,0.0483289817025159,0.0657704465338113),.UNSPECIFIED.);
#24128=B_SPLINE_CURVE_WITH_KNOTS('',3,(#163688,#163689,#163690,#163691,
#163692,#163693),.UNSPECIFIED.,.F.,.F.,(4,2,4),(0.,0.0318022365057461,0.0638030656639669),
 .UNSPECIFIED.);
#24129=B_SPLINE_CURVE_WITH_KNOTS('',3,(#163694,#163695,#163696,#163697,
#163698,#163699),.UNSPECIFIED.,.F.,.F.,(4,2,4),(1.33958587895767E-10,0.0129043686200364,
0.0270905603446428),.UNSPECIFIED.);
#24130=B_SPLINE_CURVE_WITH_KNOTS('',3,(#163703,#163704,#163705,#163706,
#163707,#163708,#163709,#163710),.UNSPECIFIED.,.F.,.F.,(4,2,2,4),(1.00011780482097E-6,
0.0146013173060188,0.0279117436337659,0.0546218075428107),.UNSPECIFIED.);
#24131=B_SPLINE_CURVE_WITH_KNOTS('',3,(#163711,#163712,#163713,#163714,
#163715,#163716),.UNSPECIFIED.,.F.,.F.,(4,2,4),(0.000862177886576435,0.0332709227901183,
0.065491269651234),.UNSPECIFIED.);
#24132=B_SPLINE_CURVE_WITH_KNOTS('',3,(#163717,#163718,#163719,#163720,
#163721,#163722,#163723,#163724),.UNSPECIFIED.,.F.,.F.,(4,2,2,4),(1.00003164852966E-6,
0.0322596484125287,0.0483289818412921,0.0657704875195388),.UNSPECIFIED.);
#24133=B_SPLINE_CURVE_WITH_KNOTS('',3,(#163747,#163748,#163749,#163750,
#163751,#163752),.UNSPECIFIED.,.F.,.F.,(4,2,4),(0.,0.0318022371619141,0.0638030681403605),
 .UNSPECIFIED.);
#24134=B_SPLINE_CURVE_WITH_KNOTS('',3,(#163753,#163754,#163755,#163756,
#163757,#163758),.UNSPECIFIED.,.F.,.F.,(4,2,4),(1.31137303927657E-10,0.0129043686309504,
0.0270905603876553),.UNSPECIFIED.);
#24135=B_SPLINE_CURVE_WITH_KNOTS('',3,(#163762,#163763,#163764,#163765,
#163766,#163767,#163768,#163769),.UNSPECIFIED.,.F.,.F.,(4,2,2,4),(1.0000066045744E-6,
0.0146013173014613,0.0279117436224652,0.0546218075309517),.UNSPECIFIED.);
#24136=B_SPLINE_CURVE_WITH_KNOTS('',3,(#163770,#163771,#163772,#163773,
#163774,#163775),.UNSPECIFIED.,.F.,.F.,(4,2,4),(0.000862177872504536,0.0332709228002364,
0.0654912680611743),.UNSPECIFIED.);
#24137=B_SPLINE_CURVE_WITH_KNOTS('',3,(#163776,#163777,#163778,#163779,
#163780,#163781,#163782,#163783),.UNSPECIFIED.,.F.,.F.,(4,2,2,4),(1.00000000502476E-6,
0.0322601580199571,0.0483296459045163,0.0657704340761967),.UNSPECIFIED.);
#24138=B_SPLINE_CURVE_WITH_KNOTS('',3,(#163806,#163807,#163808,#163809,
#163810,#163811),.UNSPECIFIED.,.F.,.F.,(4,2,4),(0.,0.0318022370629207,0.0638030677192703),
 .UNSPECIFIED.);
#24139=B_SPLINE_CURVE_WITH_KNOTS('',3,(#163812,#163813,#163814,#163815,
#163816,#163817),.UNSPECIFIED.,.F.,.F.,(4,2,4),(4.43721061285751E-11,0.0129043685092561,
0.0270905603194748),.UNSPECIFIED.);
#24140=B_SPLINE_CURVE_WITH_KNOTS('',3,(#163821,#163822,#163823,#163824,
#163825,#163826,#163827,#163828),.UNSPECIFIED.,.F.,.F.,(4,2,2,4),(1.00005818709817E-6,
0.0146013174074703,0.0279117438604932,0.0546218080317429),.UNSPECIFIED.);
#24141=B_SPLINE_CURVE_WITH_KNOTS('',3,(#163829,#163830,#163831,#163832,
#163833,#163834),.UNSPECIFIED.,.F.,.F.,(4,2,4),(0.000862177872220941,0.0332709228215002,
0.0654912694033259),.UNSPECIFIED.);
#24142=B_SPLINE_CURVE_WITH_KNOTS('',3,(#163835,#163836,#163837,#163838,
#163839,#163840,#163841,#163842),.UNSPECIFIED.,.F.,.F.,(4,2,2,4),(1.0000220664601E-6,
0.0322596483992001,0.0483289818283565,0.0657704757709717),.UNSPECIFIED.);
#24143=B_SPLINE_CURVE_WITH_KNOTS('',3,(#163865,#163866,#163867,#163868,
#163869,#163870),.UNSPECIFIED.,.F.,.F.,(4,2,4),(0.,0.031802236674665,0.0638030662404222),
 .UNSPECIFIED.);
#24144=B_SPLINE_CURVE_WITH_KNOTS('',3,(#163871,#163872,#163873,#163874,
#163875,#163876),.UNSPECIFIED.,.F.,.F.,(4,2,4),(9.38720859421175E-11,0.0129043685919122,
0.0270905603839031),.UNSPECIFIED.);
#24145=B_SPLINE_CURVE_WITH_KNOTS('',3,(#163880,#163881,#163882,#163883,
#163884,#163885,#163886,#163887),.UNSPECIFIED.,.F.,.F.,(4,2,2,4),(1.00004272345226E-6,
0.0146013174276833,0.0279117439161975,0.0546218081690105),.UNSPECIFIED.);
#24146=B_SPLINE_CURVE_WITH_KNOTS('',3,(#163888,#163889,#163890,#163891,
#163892,#163893),.UNSPECIFIED.,.F.,.F.,(4,2,4),(0.000862177861840343,0.0332709228033376,
0.065491269533001),.UNSPECIFIED.);
#24147=B_SPLINE_CURVE_WITH_KNOTS('',3,(#163894,#163895,#163896,#163897,
#163898,#163899,#163900,#163901),.UNSPECIFIED.,.F.,.F.,(4,2,2,4),(1.00003187443489E-6,
0.0322596484212709,0.0483289818280934,0.0657704966481162),.UNSPECIFIED.);
#24148=B_SPLINE_CURVE_WITH_KNOTS('',3,(#163924,#163925,#163926,#163927,
#163928,#163929),.UNSPECIFIED.,.F.,.F.,(4,2,4),(0.,0.0318022372878971,0.0638030686367771),
 .UNSPECIFIED.);
#24149=B_SPLINE_CURVE_WITH_KNOTS('',3,(#163930,#163931,#163932,#163933,
#163934,#163935),.UNSPECIFIED.,.F.,.F.,(4,2,4),(2.19837355546419E-10,0.0129043687148192,
0.0270905603643064),.UNSPECIFIED.);
#24150=B_SPLINE_CURVE_WITH_KNOTS('',3,(#163939,#163940,#163941,#163942,
#163943,#163944,#163945,#163946),.UNSPECIFIED.,.F.,.F.,(4,2,2,4),(1.00004875114485E-6,
0.0146013172814568,0.0279117435857797,0.0546218074509637),.UNSPECIFIED.);
#24151=B_SPLINE_CURVE_WITH_KNOTS('',3,(#163947,#163948,#163949,#163950,
#163951,#163952),.UNSPECIFIED.,.F.,.F.,(4,2,4),(0.000862177878349837,0.033270922788406,
0.065491269431635),.UNSPECIFIED.);
#24152=B_SPLINE_CURVE_WITH_KNOTS('',3,(#163953,#163954,#163955,#163956,
#163957,#163958,#163959,#163960),.UNSPECIFIED.,.F.,.F.,(4,2,2,4),(1.00000000494149E-6,
0.0322601580319804,0.0483296458311714,0.065770462953049),.UNSPECIFIED.);
#24153=B_SPLINE_CURVE_WITH_KNOTS('',3,(#163983,#163984,#163985,#163986,
#163987,#163988),.UNSPECIFIED.,.F.,.F.,(4,2,4),(0.,0.0318022369064364,0.0638030671624213),
 .UNSPECIFIED.);
#24154=B_SPLINE_CURVE_WITH_KNOTS('',3,(#163989,#163990,#163991,#163992,
#163993,#163994),.UNSPECIFIED.,.F.,.F.,(4,2,4),(9.32625206027885E-11,0.0129043685655828,
0.0270905603109179),.UNSPECIFIED.);
#24155=B_SPLINE_CURVE_WITH_KNOTS('',3,(#163998,#163999,#164000,#164001,
#164002,#164003,#164004,#164005),.UNSPECIFIED.,.F.,.F.,(4,2,2,4),(1.00008320850672E-6,
0.0146013173354036,0.0279117437282217,0.0546218077522595),.UNSPECIFIED.);
#24156=B_SPLINE_CURVE_WITH_KNOTS('',3,(#164006,#164007,#164008,#164009,
#164010,#164011),.UNSPECIFIED.,.F.,.F.,(4,2,4),(0.000862177875794326,0.0332709228033271,
0.0654912704313143),.UNSPECIFIED.);
#24157=B_SPLINE_CURVE_WITH_KNOTS('',3,(#164012,#164013,#164014,#164015,
#164016,#164017,#164018,#164019),.UNSPECIFIED.,.F.,.F.,(4,2,2,4),(1.00002037827966E-6,
0.0322596484166018,0.048328981784968,0.0657704224707429),.UNSPECIFIED.);
#24158=B_SPLINE_CURVE_WITH_KNOTS('',3,(#164042,#164043,#164044,#164045,
#164046,#164047),.UNSPECIFIED.,.F.,.F.,(4,2,4),(0.,0.0318022367084148,0.0638030663573333),
 .UNSPECIFIED.);
#24159=B_SPLINE_CURVE_WITH_KNOTS('',3,(#164048,#164049,#164050,#164051,
#164052,#164053),.UNSPECIFIED.,.F.,.F.,(4,2,4),(7.39165248157004E-11,0.0129043685471262,
0.0270905603326953),.UNSPECIFIED.);
#24160=B_SPLINE_CURVE_WITH_KNOTS('',3,(#164056,#164057,#164058,#164059,
#164060,#164061,#164062,#164063),.UNSPECIFIED.,.F.,.F.,(4,2,2,4),(1.00001038055159E-6,
0.0322596485761878,0.0483293807899552,0.065770445007709),.UNSPECIFIED.);
#24161=B_SPLINE_CURVE_WITH_KNOTS('',3,(#164065,#164066,#164067,#164068,
#164069,#164070,#164071,#164072),.UNSPECIFIED.,.F.,.F.,(4,2,2,4),(1.00011510446344E-6,
0.0146013172123083,0.0279117434572996,0.0546218071857167),.UNSPECIFIED.);
#24162=B_SPLINE_CURVE_WITH_KNOTS('',3,(#164073,#164074,#164075,#164076,
#164077,#164078),.UNSPECIFIED.,.F.,.F.,(4,2,4),(0.000862177870731658,0.033270922780569,
0.065491269410436),.UNSPECIFIED.);
#24163=B_SPLINE_CURVE_WITH_KNOTS('',3,(#164101,#164102,#164103,#164104,
#164105,#164106),.UNSPECIFIED.,.F.,.F.,(4,2,4),(0.,0.0318022372306193,0.063803068414536),
 .UNSPECIFIED.);
#24164=B_SPLINE_CURVE_WITH_KNOTS('',3,(#164107,#164108,#164109,#164110,
#164111,#164112),.UNSPECIFIED.,.F.,.F.,(4,2,4),(1.92328310124429E-11,0.0129043684699768,
0.027090560300435),.UNSPECIFIED.);
#24165=B_SPLINE_CURVE_WITH_KNOTS('',3,(#164116,#164117,#164118,#164119,
#164120,#164121,#164122,#164123),.UNSPECIFIED.,.F.,.F.,(4,2,2,4),(1.00002463706826E-6,
0.0146013173736547,0.0279117437525558,0.0546218077972195),.UNSPECIFIED.);
#24166=B_SPLINE_CURVE_WITH_KNOTS('',3,(#164124,#164125,#164126,#164127,
#164128,#164129),.UNSPECIFIED.,.F.,.F.,(4,2,4),(0.000862177875615986,0.0332709227871561,
0.0654912687910421),.UNSPECIFIED.);
#24167=B_SPLINE_CURVE_WITH_KNOTS('',3,(#164130,#164131,#164132,#164133,
#164134,#164135,#164136,#164137),.UNSPECIFIED.,.F.,.F.,(4,2,2,4),(1.00002578894445E-6,
0.0322596484058082,0.0483289818206998,0.0657704182650545),.UNSPECIFIED.);
#24168=B_SPLINE_CURVE_WITH_KNOTS('',3,(#164160,#164161,#164162,#164163,
#164164,#164165),.UNSPECIFIED.,.F.,.F.,(4,2,4),(0.,0.0318022368777994,0.0638030670912566),
 .UNSPECIFIED.);
#24169=B_SPLINE_CURVE_WITH_KNOTS('',3,(#164166,#164167,#164168,#164169,
#164170,#164171),.UNSPECIFIED.,.F.,.F.,(4,2,4),(2.9932138542956E-11,0.012904368491281,
0.0270905603178472),.UNSPECIFIED.);
#24170=B_SPLINE_CURVE_WITH_KNOTS('',3,(#164175,#164176,#164177,#164178,
#164179,#164180,#164181,#164182),.UNSPECIFIED.,.F.,.F.,(4,2,2,4),(1.00006907438983E-6,
0.0146013172290565,0.0279117434657564,0.0546218071603638),.UNSPECIFIED.);
#24171=B_SPLINE_CURVE_WITH_KNOTS('',3,(#164183,#164184,#164185,#164186,
#164187,#164188),.UNSPECIFIED.,.F.,.F.,(4,2,4),(0.000862177872540946,0.03327092279438,
0.0654912686680073),.UNSPECIFIED.);
#24172=B_SPLINE_CURVE_WITH_KNOTS('',3,(#164189,#164190,#164191,#164192,
#164193,#164194,#164195,#164196),.UNSPECIFIED.,.F.,.F.,(4,2,2,4),(1.00002232148558E-6,
0.0322596483697194,0.0483289817513477,0.0657704552935119),.UNSPECIFIED.);
#24173=B_SPLINE_CURVE_WITH_KNOTS('',3,(#164219,#164220,#164221,#164222,
#164223,#164224),.UNSPECIFIED.,.F.,.F.,(4,2,4),(0.,0.0318022367095504,0.0638030663978886),
 .UNSPECIFIED.);
#24174=B_SPLINE_CURVE_WITH_KNOTS('',3,(#164225,#164226,#164227,#164228,
#164229,#164230),.UNSPECIFIED.,.F.,.F.,(4,2,4),(5.38220907370343E-11,0.0129043685342898,
0.0270905603303698),.UNSPECIFIED.);
#24175=B_SPLINE_CURVE_WITH_KNOTS('',3,(#164234,#164235,#164236,#164237,
#164238,#164239,#164240,#164241),.UNSPECIFIED.,.F.,.F.,(4,2,2,4),(1.00004428863022E-6,
0.014601317347221,0.0279117437015493,0.0546218077194452),.UNSPECIFIED.);
#24176=B_SPLINE_CURVE_WITH_KNOTS('',3,(#164242,#164243,#164244,#164245,
#164246,#164247),.UNSPECIFIED.,.F.,.F.,(4,2,4),(0.00086217787073894,0.0332709228103609,
0.0654912690057304),.UNSPECIFIED.);
#24177=B_SPLINE_CURVE_WITH_KNOTS('',3,(#164248,#164249,#164250,#164251,
#164252,#164253,#164254,#164255),.UNSPECIFIED.,.F.,.F.,(4,2,2,4),(1.00001042848546E-6,
0.0322596485825745,0.0483293807633492,0.0657704522279636),.UNSPECIFIED.);
#24178=B_SPLINE_CURVE_WITH_KNOTS('',3,(#164276,#164277,#164278,#164279,
#164280,#164281),.UNSPECIFIED.,.F.,.F.,(4,2,4),(6.02571216718838E-11,0.0129043685074554,
0.0270905602953015),.UNSPECIFIED.);
#24179=B_SPLINE_CURVE_WITH_KNOTS('',3,(#164304,#164305,#164306,#164307,
#164308,#164309),.UNSPECIFIED.,.F.,.F.,(4,2,4),(0.,0.0318022370128911,0.0638030676050469),
 .UNSPECIFIED.);
#24180=B_SPLINE_CURVE_WITH_KNOTS('',3,(#164310,#164311,#164312,#164313,
#164314,#164315),.UNSPECIFIED.,.F.,.F.,(4,2,4),(8.5531026078725E-11,0.0129043685353172,
0.0270905602920881),.UNSPECIFIED.);
#24181=B_SPLINE_CURVE_WITH_KNOTS('',3,(#164319,#164320,#164321,#164322,
#164323,#164324,#164325,#164326),.UNSPECIFIED.,.F.,.F.,(4,2,2,4),(1.00002113419786E-6,
0.0146013173396389,0.0279117436545904,0.0546218075733236),.UNSPECIFIED.);
#24182=B_SPLINE_CURVE_WITH_KNOTS('',3,(#164327,#164328,#164329,#164330,
#164331,#164332),.UNSPECIFIED.,.F.,.F.,(4,2,4),(0.000862177868521618,0.0332709227807087,
0.0654912686615231),.UNSPECIFIED.);
#24183=B_SPLINE_CURVE_WITH_KNOTS('',3,(#164333,#164334,#164335,#164336,
#164337,#164338,#164339,#164340),.UNSPECIFIED.,.F.,.F.,(4,2,2,4),(1.00002253887209E-6,
0.0322596484176829,0.0483289817265474,0.0657704408776146),.UNSPECIFIED.);
#24184=B_SPLINE_CURVE_WITH_KNOTS('',3,(#164363,#164364,#164365,#164366,
#164367,#164368),.UNSPECIFIED.,.F.,.F.,(4,2,4),(0.,0.0318022368415226,0.0638030668558906),
 .UNSPECIFIED.);
#24185=B_SPLINE_CURVE_WITH_KNOTS('',3,(#164369,#164370,#164371,#164372,
#164373,#164374),.UNSPECIFIED.,.F.,.F.,(4,2,4),(1.91828848464759E-10,0.012904368692585,
0.0270905603822096),.UNSPECIFIED.);
#24186=B_SPLINE_CURVE_WITH_KNOTS('',3,(#164378,#164379,#164380,#164381,
#164382,#164383,#164384,#164385),.UNSPECIFIED.,.F.,.F.,(4,2,2,4),(1.00013954231101E-6,
0.0146013174437899,0.0279117439331808,0.0546218081909757),.UNSPECIFIED.);
#24187=B_SPLINE_CURVE_WITH_KNOTS('',3,(#164386,#164387,#164388,#164389,
#164390,#164391),.UNSPECIFIED.,.F.,.F.,(4,2,4),(0.000862177870883951,0.0332709228008459,
0.0654912703454599),.UNSPECIFIED.);
#24188=B_SPLINE_CURVE_WITH_KNOTS('',3,(#164392,#164393,#164394,#164395,
#164396,#164397,#164398,#164399),.UNSPECIFIED.,.F.,.F.,(4,2,2,4),(1.00001951865821E-6,
0.032259648377015,0.0483289817988393,0.0657705274395779),.UNSPECIFIED.);
#24189=B_SPLINE_CURVE_WITH_KNOTS('',3,(#164422,#164423,#164424,#164425,
#164426,#164427),.UNSPECIFIED.,.F.,.F.,(4,2,4),(0.,0.0318022366633233,0.0638030661847201),
 .UNSPECIFIED.);
#24190=B_SPLINE_CURVE_WITH_KNOTS('',3,(#164428,#164429,#164430,#164431,
#164432,#164433),.UNSPECIFIED.,.F.,.F.,(4,2,4),(1.65661467333103E-10,0.0129043686548563,
0.027090560365806),.UNSPECIFIED.);
#24191=B_SPLINE_CURVE_WITH_KNOTS('',3,(#164437,#164438,#164439,#164440,
#164441,#164442,#164443,#164444),.UNSPECIFIED.,.F.,.F.,(4,2,2,4),(1.00011334763741E-6,
0.0146013173318975,0.0279117436952686,0.0546218076709802),.UNSPECIFIED.);
#24192=B_SPLINE_CURVE_WITH_KNOTS('',3,(#164445,#164446,#164447,#164448,
#164449,#164450),.UNSPECIFIED.,.F.,.F.,(4,2,4),(0.000862177869665458,0.0332709228033468,
0.065491269792743),.UNSPECIFIED.);
#24193=B_SPLINE_CURVE_WITH_KNOTS('',3,(#164451,#164452,#164453,#164454,
#164455,#164456,#164457,#164458),.UNSPECIFIED.,.F.,.F.,(4,2,2,4),(1.00002568413595E-6,
0.0322596484404524,0.0483289818696783,0.0657704422348949),.UNSPECIFIED.);
#24194=B_SPLINE_CURVE_WITH_KNOTS('',3,(#164481,#164482,#164483,#164484,
#164485,#164486),.UNSPECIFIED.,.F.,.F.,(4,2,4),(0.,0.0318022370202324,0.0638030676475271),
 .UNSPECIFIED.);
#24195=B_SPLINE_CURVE_WITH_KNOTS('',3,(#164487,#164488,#164489,#164490,
#164491,#164492),.UNSPECIFIED.,.F.,.F.,(4,2,4),(5.2106907920701E-11,0.0129043685230414,
0.0270905603348801),.UNSPECIFIED.);
#24196=B_SPLINE_CURVE_WITH_KNOTS('',3,(#164496,#164497,#164498,#164499,
#164500,#164501,#164502,#164503),.UNSPECIFIED.,.F.,.F.,(4,2,2,4),(1.00000774691514E-6,
0.0146013173767995,0.0279117437417889,0.0546218077665882),.UNSPECIFIED.);
#24197=B_SPLINE_CURVE_WITH_KNOTS('',3,(#164504,#164505,#164506,#164507,
#164508,#164509),.UNSPECIFIED.,.F.,.F.,(4,2,4),(0.000862177887326279,0.0332709227781763,
0.0654912681008252),.UNSPECIFIED.);
#24198=B_SPLINE_CURVE_WITH_KNOTS('',3,(#164510,#164511,#164512,#164513,
#164514,#164515,#164516,#164517),.UNSPECIFIED.,.F.,.F.,(4,2,2,4),(1.00002353000188E-6,
0.0322596483765172,0.048328981748336,0.0657705087336826),.UNSPECIFIED.);
#24199=B_SPLINE_CURVE_WITH_KNOTS('',3,(#164540,#164541,#164542,#164543,
#164544,#164545),.UNSPECIFIED.,.F.,.F.,(4,2,4),(0.,0.0318022367256598,0.0638030664722531),
 .UNSPECIFIED.);
#24200=B_SPLINE_CURVE_WITH_KNOTS('',3,(#164546,#164547,#164548,#164549,
#164550,#164551),.UNSPECIFIED.,.F.,.F.,(4,2,4),(2.01278360991408E-10,0.012904368702619,
0.0270905603865655),.UNSPECIFIED.);
#24201=B_SPLINE_CURVE_WITH_KNOTS('',3,(#164555,#164556,#164557,#164558,
#164559,#164560,#164561,#164562),.UNSPECIFIED.,.F.,.F.,(4,2,2,4),(1.00005471192477E-6,
0.0146013174139742,0.0279117438576769,0.0546218080280394),.UNSPECIFIED.);
#24202=B_SPLINE_CURVE_WITH_KNOTS('',3,(#164563,#164564,#164565,#164566,
#164567,#164568),.UNSPECIFIED.,.F.,.F.,(4,2,4),(0.000862177891690164,0.033270922795287,
0.0654912693810284),.UNSPECIFIED.);
#24203=B_SPLINE_CURVE_WITH_KNOTS('',3,(#164569,#164570,#164571,#164572,
#164573,#164574,#164575,#164576),.UNSPECIFIED.,.F.,.F.,(4,2,2,4),(1.00002005877465E-6,
0.0322596483563003,0.0483289818364804,0.0657705118953467),.UNSPECIFIED.);
#24204=B_SPLINE_CURVE_WITH_KNOTS('',3,(#164599,#164600,#164601,#164602,
#164603,#164604),.UNSPECIFIED.,.F.,.F.,(4,2,4),(0.,0.0318022365359491,0.0638030657623883),
 .UNSPECIFIED.);
#24205=B_SPLINE_CURVE_WITH_KNOTS('',3,(#164605,#164606,#164607,#164608,
#164609,#164610),.UNSPECIFIED.,.F.,.F.,(4,2,4),(6.90463637186275E-11,0.012904368517414,
0.0270905602824478),.UNSPECIFIED.);
#24206=B_SPLINE_CURVE_WITH_KNOTS('',3,(#164614,#164615,#164616,#164617,
#164618,#164619,#164620,#164621),.UNSPECIFIED.,.F.,.F.,(4,2,2,4),(1.0000568146761E-6,
0.0146013172773308,0.0279117435819077,0.0546218074276922),.UNSPECIFIED.);
#24207=B_SPLINE_CURVE_WITH_KNOTS('',3,(#164622,#164623,#164624,#164625,
#164626,#164627),.UNSPECIFIED.,.F.,.F.,(4,2,4),(0.000862177887123505,0.0332709228044832,
0.0654912698592312),.UNSPECIFIED.);
#24208=B_SPLINE_CURVE_WITH_KNOTS('',3,(#164628,#164629,#164630,#164631,
#164632,#164633,#164634,#164635),.UNSPECIFIED.,.F.,.F.,(4,2,2,4),(1.00002664962971E-6,
0.0322596484345612,0.0483289817571778,0.0657704600907545),.UNSPECIFIED.);
#24209=B_SPLINE_CURVE_WITH_KNOTS('',3,(#164656,#164657,#164658,#164659,
#164660,#164661),.UNSPECIFIED.,.F.,.F.,(4,2,4),(8.0445768736485E-11,0.0129043685387808,
0.0270905603068917),.UNSPECIFIED.);
#24210=B_SPLINE_CURVE_WITH_KNOTS('',3,(#164723,#164724,#164725,#164726),
 .UNSPECIFIED.,.F.,.F.,(4,4),(1.36901751880817E-13,6.28596797410394E-5),
 .UNSPECIFIED.);
#24211=B_SPLINE_CURVE_WITH_KNOTS('',3,(#164901,#164902,#164903,#164904),
 .UNSPECIFIED.,.F.,.F.,(4,4),(2.8990353702476E-13,6.28596796479073E-5),
 .UNSPECIFIED.);
#24212=B_SPLINE_CURVE_WITH_KNOTS('',3,(#165051,#165052,#165053,#165054),
 .UNSPECIFIED.,.F.,.F.,(4,4),(1.3060029988537E-13,6.28596799494453E-5),
 .UNSPECIFIED.);
#24213=B_SPLINE_CURVE_WITH_KNOTS('',3,(#165145,#165146,#165147,#165148),
 .UNSPECIFIED.,.F.,.F.,(4,4),(2.49597551107631E-14,6.28596800970493E-5),
 .UNSPECIFIED.);
#24214=B_SPLINE_CURVE_WITH_KNOTS('',3,(#165211,#165212,#165213,#165214),
 .UNSPECIFIED.,.F.,.F.,(4,4),(5.02345579122992E-14,6.28596800978433E-5),
 .UNSPECIFIED.);
#24215=B_SPLINE_CURVE_WITH_KNOTS('',3,(#165305,#165306,#165307,#165308),
 .UNSPECIFIED.,.F.,.F.,(4,4),(2.86656754501717E-13,6.28596799612116E-5),
 .UNSPECIFIED.);
#24216=B_SPLINE_CURVE_WITH_KNOTS('',3,(#165343,#165344,#165345,#165346),
 .UNSPECIFIED.,.F.,.F.,(4,4),(1.86594799180136E-13,6.28596801443001E-5),
 .UNSPECIFIED.);
#24217=B_SPLINE_CURVE_WITH_KNOTS('',3,(#165570,#165571,#165572,#165573,
#165574,#165575,#165576,#165577,#165578,#165579),.UNSPECIFIED.,.F.,.F.,
(4,3,3,4),(1.17787866773368E-13,5.49564749796463E-5,0.000106404128884424,
0.000157852343070985),.UNSPECIFIED.);
#24218=B_SPLINE_CURVE_WITH_KNOTS('',3,(#165591,#165592,#165593,#165594,
#165595,#165596,#165597),.UNSPECIFIED.,.F.,.F.,(4,3,4),(0.0665682422880065,
0.0687940209133699,0.073654350294286),.UNSPECIFIED.);
#24219=B_SPLINE_CURVE_WITH_KNOTS('',3,(#165608,#165609,#165610,#165611,
#165612,#165613,#165614,#165615,#165616,#165617),.UNSPECIFIED.,.F.,.F.,
(4,3,3,4),(0.,1.58768507494459E-5,3.06163175981273E-5,4.53557993402422E-5),
 .UNSPECIFIED.);
#24220=B_SPLINE_CURVE_WITH_KNOTS('',3,(#165646,#165647,#165648,#165649,
#165650,#165651,#165652,#165653,#165654,#165655),.UNSPECIFIED.,.F.,.F.,
(4,3,3,4),(1.94492182330635E-11,5.49564846028493E-5,0.000106404139457275,
0.00015785234352159),.UNSPECIFIED.);
#24221=B_SPLINE_CURVE_WITH_KNOTS('',3,(#165677,#165678,#165679,#165680,
#165681,#165682,#165683),.UNSPECIFIED.,.F.,.F.,(4,3,4),(0.0665682423510953,
0.0687940209135822,0.073654350296252),.UNSPECIFIED.);
#24222=B_SPLINE_CURVE_WITH_KNOTS('',3,(#165694,#165695,#165696,#165697,
#165698,#165699,#165700,#165701,#165702,#165703),.UNSPECIFIED.,.F.,.F.,
(4,3,3,4),(0.,1.58768505414901E-5,3.06163174087771E-5,4.53557990557712E-5),
 .UNSPECIFIED.);
#24223=B_SPLINE_CURVE_WITH_KNOTS('',3,(#165732,#165733,#165734,#165735,
#165736,#165737,#165738,#165739,#165740,#165741),.UNSPECIFIED.,.F.,.F.,
(4,3,3,4),(1.99083318270911E-11,5.49564847828966E-5,0.000106404139427877,
0.00015785234326692),.UNSPECIFIED.);
#24224=B_SPLINE_CURVE_WITH_KNOTS('',3,(#165763,#165764,#165765,#165766,
#165767,#165768,#165769),.UNSPECIFIED.,.F.,.F.,(4,3,4),(0.0665682422773013,
0.068794020913582,0.0736543502945316),.UNSPECIFIED.);
#24225=B_SPLINE_CURVE_WITH_KNOTS('',3,(#165780,#165781,#165782,#165783,
#165784,#165785,#165786,#165787,#165788,#165789),.UNSPECIFIED.,.F.,.F.,
(4,3,3,4),(0.,1.58768505056132E-5,3.06163174471421E-5,4.53557992820988E-5),
 .UNSPECIFIED.);
#24226=B_SPLINE_CURVE_WITH_KNOTS('',3,(#165818,#165819,#165820,#165821,
#165822,#165823,#165824,#165825,#165826,#165827),.UNSPECIFIED.,.F.,.F.,
(4,3,3,4),(1.95992847885823E-11,5.49564849740209E-5,0.00010640413939413,
0.000157852343216646),.UNSPECIFIED.);
#24227=B_SPLINE_CURVE_WITH_KNOTS('',3,(#165849,#165850,#165851,#165852,
#165853,#165854,#165855),.UNSPECIFIED.,.F.,.F.,(4,3,4),(0.0665682422879086,
0.0687940209135822,0.0736543503049214),.UNSPECIFIED.);
#24228=B_SPLINE_CURVE_WITH_KNOTS('',3,(#165866,#165867,#165868,#165869,
#165870,#165871,#165872,#165873,#165874,#165875),.UNSPECIFIED.,.F.,.F.,
(4,3,3,4),(0.,1.58768506377367E-5,3.06163175608296E-5,4.53557993773814E-5),
 .UNSPECIFIED.);
#24229=B_SPLINE_CURVE_WITH_KNOTS('',3,(#165904,#165905,#165906,#165907,
#165908,#165909,#165910,#165911,#165912,#165913),.UNSPECIFIED.,.F.,.F.,
(4,3,3,4),(1.9227260917741E-11,5.49564846408612E-5,0.000106404139395807,
0.000157852343431087),.UNSPECIFIED.);
#24230=B_SPLINE_CURVE_WITH_KNOTS('',3,(#165935,#165936,#165937,#165938,
#165939,#165940),.UNSPECIFIED.,.F.,.F.,(4,2,4),(0.,0.0162313728147786,0.032488015400969),
 .UNSPECIFIED.);
#24231=B_SPLINE_CURVE_WITH_KNOTS('',3,(#165951,#165952,#165953,#165954,
#165955,#165956,#165957,#165958,#165959,#165960),.UNSPECIFIED.,.F.,.F.,
(4,3,3,4),(0.,1.58768507540077E-5,3.06163175287554E-5,4.53557991708055E-5),
 .UNSPECIFIED.);
#24232=B_SPLINE_CURVE_WITH_KNOTS('',3,(#165989,#165990,#165991,#165992,
#165993,#165994,#165995,#165996,#165997,#165998),.UNSPECIFIED.,.F.,.F.,
(4,3,3,4),(1.91076604433025E-11,5.49564847134886E-5,0.000106404139369031,
0.000157852343374027),.UNSPECIFIED.);
#24233=B_SPLINE_CURVE_WITH_KNOTS('',3,(#166020,#166021,#166022,#166023,
#166024,#166025,#166026),.UNSPECIFIED.,.F.,.F.,(4,3,4),(0.066568242293216,
0.0687940209135806,0.0736543503096691),.UNSPECIFIED.);
#24234=B_SPLINE_CURVE_WITH_KNOTS('',3,(#166037,#166038,#166039,#166040,
#166041,#166042,#166043,#166044,#166045,#166046),.UNSPECIFIED.,.F.,.F.,
(4,3,3,4),(0.,1.58768507491376E-5,3.06163176585412E-5,4.53557994613311E-5),
 .UNSPECIFIED.);
#24235=B_SPLINE_CURVE_WITH_KNOTS('',3,(#166075,#166076,#166077,#166078,
#166079,#166080,#166081,#166082,#166083,#166084),.UNSPECIFIED.,.F.,.F.,
(4,3,3,4),(1.94512450953462E-11,5.49564848072227E-5,0.000106404139447775,
0.000157852343402473),.UNSPECIFIED.);
#24236=B_SPLINE_CURVE_WITH_KNOTS('',3,(#166106,#166107,#166108,#166109,
#166110,#166111,#166112),.UNSPECIFIED.,.F.,.F.,(4,3,4),(0.0665682422965139,
0.0687940209135805,0.0736543502734499),.UNSPECIFIED.);
#24237=B_SPLINE_CURVE_WITH_KNOTS('',3,(#166123,#166124,#166125,#166126,
#166127,#166128,#166129,#166130,#166131,#166132),.UNSPECIFIED.,.F.,.F.,
(4,3,3,4),(0.,1.58768504200603E-5,3.06163174679481E-5,4.53557994092083E-5),
 .UNSPECIFIED.);
#24238=B_SPLINE_CURVE_WITH_KNOTS('',3,(#166161,#166162,#166163,#166164,
#166165,#166166,#166167,#166168,#166169,#166170),.UNSPECIFIED.,.F.,.F.,
(4,3,3,4),(1.97540479541651E-11,5.49564846745727E-5,0.000106404139491155,
0.00015785234371001),.UNSPECIFIED.);
#24239=B_SPLINE_CURVE_WITH_KNOTS('',3,(#166192,#166193,#166194,#166195,
#166196,#166197,#166198),.UNSPECIFIED.,.F.,.F.,(4,3,4),(0.0665682423719981,
0.0687940209135804,0.0736543503119808),.UNSPECIFIED.);
#24240=B_SPLINE_CURVE_WITH_KNOTS('',3,(#166209,#166210,#166211,#166212,
#166213,#166214,#166215,#166216,#166217,#166218),.UNSPECIFIED.,.F.,.F.,
(4,3,3,4),(0.,1.58768505877374E-5,3.06163173724542E-5,4.53557990505977E-5),
 .UNSPECIFIED.);
#24241=B_SPLINE_CURVE_WITH_KNOTS('',3,(#166247,#166248,#166249,#166250,
#166251,#166252,#166253,#166254,#166255,#166256),.UNSPECIFIED.,.F.,.F.,
(4,3,3,4),(1.93035758031966E-11,5.49564846983035E-5,0.000106404139490847,
0.000157852343630075),.UNSPECIFIED.);
#24242=B_SPLINE_CURVE_WITH_KNOTS('',3,(#166278,#166279,#166280,#166281,
#166282,#166283,#166284),.UNSPECIFIED.,.F.,.F.,(4,3,4),(0.0665682422788486,
0.0687940209135805,0.073654350296961),.UNSPECIFIED.);
#24243=B_SPLINE_CURVE_WITH_KNOTS('',3,(#166295,#166296,#166297,#166298,
#166299,#166300,#166301,#166302,#166303,#166304),.UNSPECIFIED.,.F.,.F.,
(4,3,3,4),(0.,1.58768506651977E-5,3.06163175950794E-5,4.53557994183095E-5),
 .UNSPECIFIED.);
#24244=B_SPLINE_CURVE_WITH_KNOTS('',3,(#166333,#166334,#166335,#166336,
#166337,#166338,#166339,#166340,#166341,#166342),.UNSPECIFIED.,.F.,.F.,
(4,3,3,4),(1.96543653144358E-11,5.49564848592507E-5,0.000106404139588688,
0.000157852343493213),.UNSPECIFIED.);
#24245=B_SPLINE_CURVE_WITH_KNOTS('',3,(#166364,#166365,#166366,#166367,
#166368,#166369),.UNSPECIFIED.,.F.,.F.,(4,2,4),(0.,0.0162318631985632,0.0324879936074455),
 .UNSPECIFIED.);
#24246=B_SPLINE_CURVE_WITH_KNOTS('',3,(#166380,#166381,#166382,#166383,
#166384,#166385,#166386,#166387,#166388,#166389),.UNSPECIFIED.,.F.,.F.,
(4,3,3,4),(0.,1.58768504813884E-5,3.06163176465143E-5,4.53557997050518E-5),
 .UNSPECIFIED.);
#24247=B_SPLINE_CURVE_WITH_KNOTS('',3,(#166418,#166419,#166420,#166421,
#166422,#166423,#166424,#166425,#166426,#166427),.UNSPECIFIED.,.F.,.F.,
(4,3,3,4),(1.92583943969339E-11,5.49564845470167E-5,0.000106404139345154,
0.000157852343544874),.UNSPECIFIED.);
#24248=B_SPLINE_CURVE_WITH_KNOTS('',3,(#166449,#166450,#166451,#166452,
#166453,#166454,#166455),.UNSPECIFIED.,.F.,.F.,(4,3,4),(0.066568242289363,
0.0687940209135806,0.0736543503213074),.UNSPECIFIED.);
#24249=B_SPLINE_CURVE_WITH_KNOTS('',3,(#166466,#166467,#166468,#166469,
#166470,#166471,#166472,#166473,#166474,#166475),.UNSPECIFIED.,.F.,.F.,
(4,3,3,4),(0.,1.58768507441245E-5,3.06163177021733E-5,4.53557995536538E-5),
 .UNSPECIFIED.);
#24250=B_SPLINE_CURVE_WITH_KNOTS('',3,(#166504,#166505,#166506,#166507,
#166508,#166509,#166510,#166511,#166512,#166513),.UNSPECIFIED.,.F.,.F.,
(4,3,3,4),(1.93203317729608E-11,5.4956484706313E-5,0.000106404139520639,
0.000157852343600362),.UNSPECIFIED.);
#24251=B_SPLINE_CURVE_WITH_KNOTS('',3,(#166535,#166536,#166537,#166538,
#166539,#166540),.UNSPECIFIED.,.F.,.F.,(4,2,4),(0.,0.0162313587612594,0.0324879705789074),
 .UNSPECIFIED.);
#24252=B_SPLINE_CURVE_WITH_KNOTS('',3,(#166551,#166552,#166553,#166554,
#166555,#166556,#166557,#166558,#166559,#166560),.UNSPECIFIED.,.F.,.F.,
(4,3,3,4),(0.,1.58768506403926E-5,3.06163176425318E-5,4.53557995380538E-5),
 .UNSPECIFIED.);
#24253=B_SPLINE_CURVE_WITH_KNOTS('',3,(#166589,#166590,#166591,#166592,
#166593,#166594,#166595,#166596,#166597,#166598),.UNSPECIFIED.,.F.,.F.,
(4,3,3,4),(1.95534039607494E-11,5.49564846228906E-5,0.000106404139399807,
0.000157852343557442),.UNSPECIFIED.);
#24254=B_SPLINE_CURVE_WITH_KNOTS('',3,(#166620,#166621,#166622,#166623,
#166624,#166625),.UNSPECIFIED.,.F.,.F.,(4,2,4),(3.14562329816648E-10,0.0162313566854201,
0.0324879763496492),.UNSPECIFIED.);
#24255=B_SPLINE_CURVE_WITH_KNOTS('',3,(#166636,#166637,#166638,#166639,
#166640,#166641,#166642,#166643,#166644,#166645),.UNSPECIFIED.,.F.,.F.,
(4,3,3,4),(0.,1.58768507855502E-5,3.06163176193626E-5,4.53557993467085E-5),
 .UNSPECIFIED.);
#24256=B_SPLINE_CURVE_WITH_KNOTS('',3,(#166674,#166675,#166676,#166677,
#166678,#166679,#166680,#166681,#166682,#166683),.UNSPECIFIED.,.F.,.F.,
(4,3,3,4),(2.00303227837484E-11,5.49564846133499E-5,0.000106404139235265,
0.000157852343259419),.UNSPECIFIED.);
#24257=B_SPLINE_CURVE_WITH_KNOTS('',3,(#166705,#166706,#166707,#166708,
#166709,#166710,#166711),.UNSPECIFIED.,.F.,.F.,(4,3,4),(0.0665682422875406,
0.0687940209135808,0.0736543502979871),.UNSPECIFIED.);
#24258=B_SPLINE_CURVE_WITH_KNOTS('',3,(#166722,#166723,#166724,#166725,
#166726,#166727,#166728,#166729,#166730,#166731),.UNSPECIFIED.,.F.,.F.,
(4,3,3,4),(0.,1.58768507135064E-5,3.06163176365131E-5,4.5355799453002E-5),
 .UNSPECIFIED.);
#24259=B_SPLINE_CURVE_WITH_KNOTS('',3,(#166760,#166761,#166762,#166763,
#166764,#166765,#166766,#166767,#166768,#166769),.UNSPECIFIED.,.F.,.F.,
(4,3,3,4),(1.96999729795625E-11,5.49564845850009E-5,0.000106404139251949,
0.000157852343152646),.UNSPECIFIED.);
#24260=B_SPLINE_CURVE_WITH_KNOTS('',3,(#166791,#166792,#166793,#166794,
#166795,#166796,#166797),.UNSPECIFIED.,.F.,.F.,(4,3,4),(0.0665682423196876,
0.0687940209135806,0.0736543502758461),.UNSPECIFIED.);
#24261=B_SPLINE_CURVE_WITH_KNOTS('',3,(#166808,#166809,#166810,#166811,
#166812,#166813,#166814,#166815,#166816,#166817),.UNSPECIFIED.,.F.,.F.,
(4,3,3,4),(0.,1.58768506886893E-5,3.06163176410586E-5,4.53557994868356E-5),
 .UNSPECIFIED.);
#24262=B_SPLINE_CURVE_WITH_KNOTS('',3,(#166846,#166847,#166848,#166849,
#166850,#166851,#166852,#166853,#166854,#166855),.UNSPECIFIED.,.F.,.F.,
(4,3,3,4),(1.91599846899834E-11,5.49564847847627E-5,0.00010640413932454,
0.000157852343266793),.UNSPECIFIED.);
#24263=B_SPLINE_CURVE_WITH_KNOTS('',3,(#166877,#166878,#166879,#166880,
#166881,#166882),.UNSPECIFIED.,.F.,.F.,(4,2,4),(1.23551874885213E-10,0.0162313622636938,
0.032487982563608),.UNSPECIFIED.);
#24264=B_SPLINE_CURVE_WITH_KNOTS('',3,(#166893,#166894,#166895,#166896,
#166897,#166898,#166899,#166900,#166901,#166902),.UNSPECIFIED.,.F.,.F.,
(4,3,3,4),(0.,1.58768507290829E-5,3.06163176207548E-5,4.5355799405801E-5),
 .UNSPECIFIED.);
#24265=B_SPLINE_CURVE_WITH_KNOTS('',3,(#166931,#166932,#166933,#166934,
#166935,#166936,#166937,#166938,#166939,#166940),.UNSPECIFIED.,.F.,.F.,
(4,3,3,4),(1.96998203546808E-11,5.49564848806434E-5,0.000106404139564187,
0.000157852343588196),.UNSPECIFIED.);
#24266=B_SPLINE_CURVE_WITH_KNOTS('',3,(#166962,#166963,#166964,#166965,
#166966,#166967),.UNSPECIFIED.,.F.,.F.,(4,2,4),(0.,0.0162318638811279,0.0324879967796798),
 .UNSPECIFIED.);
#24267=B_SPLINE_CURVE_WITH_KNOTS('',3,(#166978,#166979,#166980,#166981,
#166982,#166983,#166984,#166985,#166986,#166987),.UNSPECIFIED.,.F.,.F.,
(4,3,3,4),(0.,1.58768505079052E-5,3.06163175682341E-5,4.53557995219932E-5),
 .UNSPECIFIED.);
#24268=B_SPLINE_CURVE_WITH_KNOTS('',3,(#167016,#167017,#167018,#167019,
#167020,#167021,#167022,#167023,#167024,#167025),.UNSPECIFIED.,.F.,.F.,
(4,3,3,4),(1.95048878554873E-11,5.4956484780533E-5,0.0001064041395414,0.000157852343523395),
 .UNSPECIFIED.);
#24269=B_SPLINE_CURVE_WITH_KNOTS('',3,(#167047,#167048,#167049,#167050,
#167051,#167052,#167053),.UNSPECIFIED.,.F.,.F.,(4,3,4),(0.0665682423833946,
0.068794020913582,0.0736543503054048),.UNSPECIFIED.);
#24270=B_SPLINE_CURVE_WITH_KNOTS('',3,(#167064,#167065,#167066,#167067,
#167068,#167069,#167070,#167071,#167072,#167073),.UNSPECIFIED.,.F.,.F.,
(4,3,3,4),(0.,1.5876850585908E-5,3.06163176069253E-5,4.53557993666698E-5),
 .UNSPECIFIED.);
#24271=B_SPLINE_CURVE_WITH_KNOTS('',3,(#167102,#167103,#167104,#167105,
#167106,#167107,#167108,#167109,#167110,#167111),.UNSPECIFIED.,.F.,.F.,
(4,3,3,4),(1.97016435778415E-11,5.49564846894979E-5,0.000106404139460024,
0.000157852343464582),.UNSPECIFIED.);
#24272=B_SPLINE_CURVE_WITH_KNOTS('',3,(#167133,#167134,#167135,#167136,
#167137,#167138,#167139),.UNSPECIFIED.,.F.,.F.,(4,3,4),(0.0665682421563453,
0.0687940209135813,0.0736543502745496),.UNSPECIFIED.);
#24273=B_SPLINE_CURVE_WITH_KNOTS('',3,(#167150,#167151,#167152,#167153,
#167154,#167155,#167156,#167157,#167158,#167159),.UNSPECIFIED.,.F.,.F.,
(4,3,3,4),(0.,1.58768505916532E-5,3.06163175413448E-5,4.53557993844558E-5),
 .UNSPECIFIED.);
#24274=B_SPLINE_CURVE_WITH_KNOTS('',3,(#167188,#167189,#167190,#167191,
#167192,#167193,#167194,#167195,#167196,#167197),.UNSPECIFIED.,.F.,.F.,
(4,3,3,4),(1.99325371145902E-11,5.49564848457451E-5,0.000106404139306774,
0.000157852343170209),.UNSPECIFIED.);
#24275=B_SPLINE_CURVE_WITH_KNOTS('',3,(#167219,#167220,#167221,#167222,
#167223,#167224,#167225),.UNSPECIFIED.,.F.,.F.,(4,3,4),(0.0665682423052219,
0.0687940209135831,0.0736543502899574),.UNSPECIFIED.);
#24276=B_SPLINE_CURVE_WITH_KNOTS('',3,(#167236,#167237,#167238,#167239,
#167240,#167241,#167242,#167243,#167244,#167245),.UNSPECIFIED.,.F.,.F.,
(4,3,3,4),(0.,1.58768506225724E-5,3.06163176219113E-5,4.53557994801334E-5),
 .UNSPECIFIED.);
#24277=B_SPLINE_CURVE_WITH_KNOTS('',3,(#167274,#167275,#167276,#167277,
#167278,#167279,#167280,#167281,#167282,#167283),.UNSPECIFIED.,.F.,.F.,
(4,3,3,4),(1.97900793505604E-11,5.49564847299566E-5,0.00010640413938352,
0.000157852343353258),.UNSPECIFIED.);
#24278=B_SPLINE_CURVE_WITH_KNOTS('',3,(#167305,#167306,#167307,#167308,
#167309,#167310),.UNSPECIFIED.,.F.,.F.,(4,2,4),(3.3528454241449E-10,0.0162318622754898,
0.0324879964841344),.UNSPECIFIED.);
#24279=B_SPLINE_CURVE_WITH_KNOTS('',3,(#167321,#167322,#167323,#167324,
#167325,#167326,#167327,#167328,#167329,#167330),.UNSPECIFIED.,.F.,.F.,
(4,3,3,4),(0.,1.58768505730015E-5,3.06163175841791E-5,4.53557994200099E-5),
 .UNSPECIFIED.);
#24280=B_SPLINE_CURVE_WITH_KNOTS('',3,(#167359,#167360,#167361,#167362,
#167363,#167364,#167365,#167366,#167367,#167368),.UNSPECIFIED.,.F.,.F.,
(4,3,3,4),(1.96951086378155E-11,5.49564846772444E-5,0.000106404139348174,
0.000157852343421498),.UNSPECIFIED.);
#24281=B_SPLINE_CURVE_WITH_KNOTS('',3,(#167390,#167391,#167392,#167393,
#167394,#167395,#167396),.UNSPECIFIED.,.F.,.F.,(4,3,4),(0.0665682423954821,
0.0687940209135814,0.0736543503169011),.UNSPECIFIED.);
#24282=B_SPLINE_CURVE_WITH_KNOTS('',3,(#167407,#167408,#167409,#167410,
#167411,#167412,#167413,#167414,#167415,#167416),.UNSPECIFIED.,.F.,.F.,
(4,3,3,4),(0.,1.5876850579189E-5,3.06163176024993E-5,4.53557995192418E-5),
 .UNSPECIFIED.);
#24283=B_SPLINE_CURVE_WITH_KNOTS('',3,(#167445,#167446,#167447,#167448,
#167449,#167450,#167451,#167452,#167453,#167454),.UNSPECIFIED.,.F.,.F.,
(4,3,3,4),(1.92477551805011E-11,5.49564847799471E-5,0.000106404139341856,
0.000157852343306238),.UNSPECIFIED.);
#24284=B_SPLINE_CURVE_WITH_KNOTS('',3,(#167476,#167477,#167478,#167479,
#167480,#167481),.UNSPECIFIED.,.F.,.F.,(4,2,4),(0.,0.0162313684470647,0.0324879996631388),
 .UNSPECIFIED.);
#24285=B_SPLINE_CURVE_WITH_KNOTS('',3,(#167492,#167493,#167494,#167495,
#167496,#167497,#167498,#167499,#167500,#167501),.UNSPECIFIED.,.F.,.F.,
(4,3,3,4),(0.,1.5876850785568E-5,3.0616317651021E-5,4.53557993820318E-5),
 .UNSPECIFIED.);
#24286=B_SPLINE_CURVE_WITH_KNOTS('',3,(#167530,#167531,#167532,#167533,
#167534,#167535,#167536,#167537,#167538,#167539),.UNSPECIFIED.,.F.,.F.,
(4,3,3,4),(1.98724445707963E-11,5.49564847358756E-5,0.000106404139421232,
0.000157852343488376),.UNSPECIFIED.);
#24287=B_SPLINE_CURVE_WITH_KNOTS('',3,(#167561,#167562,#167563,#167564,
#167565,#167566,#167567),.UNSPECIFIED.,.F.,.F.,(4,3,4),(0.0665682422866777,
0.068794020913583,0.0736543502893516),.UNSPECIFIED.);
#24288=B_SPLINE_CURVE_WITH_KNOTS('',3,(#167578,#167579,#167580,#167581,
#167582,#167583,#167584,#167585,#167586,#167587),.UNSPECIFIED.,.F.,.F.,
(4,3,3,4),(0.,1.58768503791903E-5,3.06163174838833E-5,4.53557994819831E-5),
 .UNSPECIFIED.);
#24289=B_SPLINE_CURVE_WITH_KNOTS('',3,(#167616,#167617,#167618,#167619,
#167620,#167621,#167622,#167623,#167624,#167625),.UNSPECIFIED.,.F.,.F.,
(4,3,3,4),(1.99724342327927E-11,5.49564846709836E-5,0.00010640413938314,
0.000157852343341814),.UNSPECIFIED.);
#24290=B_SPLINE_CURVE_WITH_KNOTS('',3,(#167662,#167663,#167664,#167665,
#167666,#167667,#167668,#167669,#167670,#167671),.UNSPECIFIED.,.F.,.F.,
(4,3,3,4),(0.,1.58768505326137E-5,3.06163176813787E-5,4.53557996601019E-5),
 .UNSPECIFIED.);
#24291=B_SPLINE_CURVE_WITH_KNOTS('',3,(#167700,#167701,#167702,#167703,
#167704,#167705,#167706,#167707,#167708,#167709),.UNSPECIFIED.,.F.,.F.,
(4,3,3,4),(1.96441694070615E-11,5.49564848245943E-5,0.000106404139380829,
0.00015785234333938),.UNSPECIFIED.);
#24292=B_SPLINE_CURVE_WITH_KNOTS('',3,(#167731,#167732,#167733,#167734,
#167735,#167736,#167737),.UNSPECIFIED.,.F.,.F.,(4,3,4),(0.0665682422879882,
0.0687940209135823,0.0736543502940118),.UNSPECIFIED.);
#24293=B_SPLINE_CURVE_WITH_KNOTS('',3,(#167748,#167749,#167750,#167751,
#167752,#167753,#167754,#167755,#167756,#167757),.UNSPECIFIED.,.F.,.F.,
(4,3,3,4),(0.,1.58768505197501E-5,3.06163174240148E-5,4.53557992217912E-5),
 .UNSPECIFIED.);
#24294=B_SPLINE_CURVE_WITH_KNOTS('',3,(#167786,#167787,#167788,#167789,
#167790,#167791,#167792,#167793,#167794,#167795),.UNSPECIFIED.,.F.,.F.,
(4,3,3,4),(1.94539174373277E-11,5.4956484797753E-5,0.000106404139464652,
0.000157852343533767),.UNSPECIFIED.);
#24295=B_SPLINE_CURVE_WITH_KNOTS('',3,(#167817,#167818,#167819,#167820,
#167821,#167822),.UNSPECIFIED.,.F.,.F.,(4,2,4),(0.,0.0162313678326357,0.0324880090349668),
 .UNSPECIFIED.);
#24296=B_SPLINE_CURVE_WITH_KNOTS('',3,(#167833,#167834,#167835,#167836,
#167837,#167838,#167839,#167840,#167841,#167842),.UNSPECIFIED.,.F.,.F.,
(4,3,3,4),(0.,1.58768506195949E-5,3.0616317499383E-5,4.53557992726239E-5),
 .UNSPECIFIED.);
#24297=B_SPLINE_CURVE_WITH_KNOTS('',3,(#167871,#167872,#167873,#167874,
#167875,#167876,#167877,#167878,#167879,#167880),.UNSPECIFIED.,.F.,.F.,
(4,3,3,4),(1.93866854359336E-11,5.49564848580382E-5,0.000106404139413798,
0.000157852343265456),.UNSPECIFIED.);
#24298=B_SPLINE_CURVE_WITH_KNOTS('',3,(#167902,#167903,#167904,#167905,
#167906,#167907,#167908),.UNSPECIFIED.,.F.,.F.,(4,3,4),(0.0665682421712998,
0.0687940209135817,0.0736543502856294),.UNSPECIFIED.);
#24299=B_SPLINE_CURVE_WITH_KNOTS('',3,(#167919,#167920,#167921,#167922,
#167923,#167924,#167925,#167926,#167927,#167928),.UNSPECIFIED.,.F.,.F.,
(4,3,3,4),(0.,1.58768508095443E-5,3.06163176188101E-5,4.53557993214627E-5),
 .UNSPECIFIED.);
#24300=B_SPLINE_CURVE_WITH_KNOTS('',3,(#167957,#167958,#167959,#167960,
#167961,#167962,#167963,#167964,#167965,#167966),.UNSPECIFIED.,.F.,.F.,
(4,3,3,4),(1.99132794969912E-11,5.49564847506683E-5,0.000106404139384107,
0.000157852343419854),.UNSPECIFIED.);
#24301=B_SPLINE_CURVE_WITH_KNOTS('',3,(#167988,#167989,#167990,#167991,
#167992,#167993,#167994),.UNSPECIFIED.,.F.,.F.,(4,3,4),(0.0665682422923062,
0.0687940209135823,0.0736543502809432),.UNSPECIFIED.);
#24302=B_SPLINE_CURVE_WITH_KNOTS('',3,(#168005,#168006,#168007,#168008,
#168009,#168010,#168011,#168012,#168013,#168014),.UNSPECIFIED.,.F.,.F.,
(4,3,3,4),(0.,1.58768505171131E-5,3.0616317600087E-5,4.53557995764553E-5),
 .UNSPECIFIED.);
#24303=B_SPLINE_CURVE_WITH_KNOTS('',3,(#168059,#168060,#168061,#168062),
 .UNSPECIFIED.,.F.,.F.,(4,4),(1.09971404256795,1.21244876000028),
 .UNSPECIFIED.);
#24304=B_SPLINE_CURVE_WITH_KNOTS('',3,(#168066,#168067,#168068,#168069),
 .UNSPECIFIED.,.F.,.F.,(4,4),(1.65787808514986,1.77061280261397),
 .UNSPECIFIED.);
#24305=B_SPLINE_CURVE_WITH_KNOTS('',3,(#168082,#168083,#168084,#168085),
 .UNSPECIFIED.,.F.,.F.,(4,4),(2.53487746522254,2.64761218276488),
 .UNSPECIFIED.);
#24306=B_SPLINE_CURVE_WITH_KNOTS('',3,(#168089,#168090,#168091,#168092),
 .UNSPECIFIED.,.F.,.F.,(4,4),(-2.64761218272936,-2.53487746528608),
 .UNSPECIFIED.);
#24307=B_SPLINE_CURVE_WITH_KNOTS('',3,(#168105,#168106,#168107,#168108,
#168109,#168110,#168111,#168112,#168113,#168114,#168115,#168116,#168117,
#168118),.UNSPECIFIED.,.F.,.F.,(4,2,2,2,2,2,4),(-3.61371859075551,-3.49762439616657,
-3.37604729441128,-3.254470192656,-3.13289309090071,-3.01131598914542,-2.89522179460579),
 .UNSPECIFIED.);
#24308=B_SPLINE_CURVE_WITH_KNOTS('',3,(#168120,#168121,#168122,#168123,
#168124,#168125),.UNSPECIFIED.,.F.,.F.,(4,2,4),(-0.505642410187432,-0.432426511837419,
-0.363335115211808),.UNSPECIFIED.);
#24309=B_SPLINE_CURVE_WITH_KNOTS('',3,(#168130,#168131,#168132,#168133,
#168134,#168135),.UNSPECIFIED.,.F.,.F.,(4,2,4),(-1.44175006264287,-1.37265866586429,
-1.29944276755287),.UNSPECIFIED.);
#24310=B_SPLINE_CURVE_WITH_KNOTS('',3,(#168144,#168145,#168146,#168147,
#168148,#168149),.UNSPECIFIED.,.F.,.F.,(4,2,4),(1.30070391833721,1.41679560118766,
1.44118086035152),.UNSPECIFIED.);
#24311=B_SPLINE_CURVE_WITH_KNOTS('',3,(#168155,#168156,#168157,#168158,
#168159,#168160,#168161,#168162),.UNSPECIFIED.,.F.,.F.,(4,2,2,4),(-3.254470192656,
-3.13289309090071,-3.01131598914542,-2.89522179462825),.UNSPECIFIED.);
#24312=B_SPLINE_CURVE_WITH_KNOTS('',3,(#168164,#168165,#168166,#168167,
#168168,#168169,#168170,#168171),.UNSPECIFIED.,.F.,.F.,(4,2,2,4),(-3.61371859064193,
-3.49762439616657,-3.37604729441128,-3.254470192656),.UNSPECIFIED.);
#24313=B_SPLINE_CURVE_WITH_KNOTS('',3,(#168180,#168181,#168182,#168183,
#168184,#168185),.UNSPECIFIED.,.F.,.F.,(4,2,4),(0.36333511511172,0.43242651183742,
0.505642410213935),.UNSPECIFIED.);
#24314=B_SPLINE_CURVE_WITH_KNOTS('',3,(#168200,#168201,#168202,#168203,
#168204,#168205,#168206,#168207,#168208,#168209,#168210,#168211,#168212,
#168213,#168214,#168215,#168216,#168217,#168218,#168219,#168220,#168221,
#168222,#168223,#168224,#168225,#168226,#168227,#168228,#168229,#168230,
#168231,#168232,#168233,#168234,#168235,#168236,#168237,#168238,#168239,
#168240,#168241,#168242),.UNSPECIFIED.,.F.,.F.,(4,3,3,3,3,3,3,3,3,3,3,3,
3,3,4),(0.499343871841187,0.549093604143059,0.599465023228859,0.62450790388089,
0.689718293200921,0.749671935920592,0.758683676198281,0.765317439925555,
0.780962943930518,0.812253951940444,0.874835967960296,0.890796391310028,
0.906126975970222,0.959821021734887,1.),.UNSPECIFIED.);
#24315=B_SPLINE_CURVE_WITH_KNOTS('',3,(#168243,#168244,#168245,#168246,
#168247,#168248,#168249,#168250,#168251,#168252,#168253,#168254,#168255,
#168256,#168257,#168258,#168259,#168260,#168261,#168262,#168263,#168264,
#168265,#168266,#168267,#168268,#168269,#168270,#168271,#168272,#168273,
#168274,#168275,#168276,#168277,#168278,#168279,#168280,#168281,#168282,
#168283,#168284,#168285,#168286,#168287,#168288),.UNSPECIFIED.,.F.,.F.,
(4,3,3,3,3,3,3,3,3,3,3,3,3,3,3,4),(0.,0.0539371583026244,0.106650915602551,
0.124835967960296,0.140821762748041,0.15604495995037,0.214914746357673,
0.249671935920592,0.255809368181488,0.25747418391811,0.265276431915629,
0.280880927910666,0.312089919900741,0.374507903880889,0.438618517613949,
0.499343871841187),.UNSPECIFIED.);
#24316=B_SPLINE_CURVE_WITH_KNOTS('',3,(#168292,#168293,#168294,#168295,
#168296,#168297,#168298,#168299,#168300,#168301,#168302,#168303,#168304,
#168305,#168306,#168307,#168308,#168309,#168310,#168311,#168312,#168313,
#168314,#168315,#168316,#168317,#168318,#168319,#168320,#168321,#168322,
#168323,#168324,#168325,#168326,#168327,#168328,#168329,#168330,#168331,
#168332,#168333,#168334),.UNSPECIFIED.,.F.,.F.,(4,3,3,3,3,3,3,3,3,3,3,3,
3,3,4),(0.499343871841254,0.54909365836049,0.599465134382744,0.62450790388094,
0.689718289747475,0.749671935920627,0.758683679203924,0.765317439925588,
0.780962943930549,0.812253951940471,0.874835967960314,0.890796399632331,
0.906126975970235,0.959821023994028,1.),.UNSPECIFIED.);
#24317=B_SPLINE_CURVE_WITH_KNOTS('',3,(#168336,#168337,#168338,#168339,
#168340,#168341,#168342,#168343,#168344,#168345,#168346,#168347,#168348,
#168349,#168350,#168351,#168352,#168353,#168354,#168355,#168356,#168357,
#168358,#168359,#168360,#168361,#168362,#168363,#168364,#168365,#168366,
#168367,#168368,#168369,#168370,#168371,#168372,#168373,#168374,#168375,
#168376,#168377,#168378,#168379,#168380,#168381),.UNSPECIFIED.,.F.,.F.,
(4,3,3,3,3,3,3,3,3,3,3,3,3,3,3,4),(0.,0.0539371583336762,0.10665091566333,
0.124835967960314,0.140821762714439,0.156044959950392,0.214914746428806,
0.249671935920627,0.255809368181394,0.257474183918147,0.265276431915666,
0.280880927910705,0.312089919900784,0.37450790388094,0.438618517375844,
0.499343871841254),.UNSPECIFIED.);
#24318=B_SPLINE_CURVE_WITH_KNOTS('',3,(#168405,#168406,#168407,#168408,
#168409,#168410,#168411,#168412,#168413,#168414),.UNSPECIFIED.,.F.,.F.,
(4,2,2,2,4),(9.99999999599415E-7,0.199896964270254,0.396819956928882,0.593738515946119,
0.793630665235622),.UNSPECIFIED.);
#24319=B_SPLINE_CURVE_WITH_KNOTS('',3,(#168418,#168419,#168420,#168421,
#168422,#168423,#168424,#168425,#168426,#168427),.UNSPECIFIED.,.F.,.F.,
(4,2,2,2,4),(1.0000000102557E-6,0.212494298875736,0.396821009247289,0.581148812864389,
0.793634316910742),.UNSPECIFIED.);
#24320=B_SPLINE_CURVE_WITH_KNOTS('',3,(#168438,#168439,#168440,#168441,
#168442,#168443),.UNSPECIFIED.,.F.,.F.,(4,2,4),(3.14399518292747E-10,0.174984677416615,
0.304359067388048),.UNSPECIFIED.);
#24321=B_SPLINE_CURVE_WITH_KNOTS('',3,(#168451,#168452,#168453,#168454,
#168455,#168456),.UNSPECIFIED.,.F.,.F.,(4,2,4),(0.000105555394099198,0.130107181442079,
0.280405013941638),.UNSPECIFIED.);
#24322=B_SPLINE_CURVE_WITH_KNOTS('',3,(#168459,#168460,#168461,#168462,
#168463,#168464,#168465,#168466,#168467,#168468,#168469,#168470,#168471,
#168472,#168473,#168474,#168475,#168476,#168477,#168478,#168479,#168480,
#168481,#168482,#168483,#168484,#168485,#168486,#168487,#168488,#168489,
#168490,#168491,#168492,#168493,#168494,#168495,#168496,#168497,#168498,
#168499,#168500,#168501,#168502,#168503,#168504,#168505,#168506,#168507,
#168508,#168509,#168510),.UNSPECIFIED.,.F.,.F.,(4,2,2,2,2,2,2,2,2,2,2,2,
2,2,2,2,2,2,2,2,2,2,2,2,2,4),(0.,0.0256250094143976,0.0414375088162371,
0.0493437585171568,0.053296883367617,0.0552734457928468,0.0562617270054617,
0.056755867611765,0.0572500082180766,0.120500005825418,0.247000001040109,
0.373499996254801,0.43674999386215,0.499999991469491,0.626499986684183,
0.689749984291532,0.752999981898873,0.879499977113565,0.942749974720914,
0.943738255933529,0.944726537146144,0.946703099571374,0.950656224421834,
0.958562474122746,0.974374973524585,0.999999995455179),.UNSPECIFIED.);
#24323=B_SPLINE_CURVE_WITH_KNOTS('',3,(#168520,#168521,#168522,#168523,
#168524,#168525,#168526,#168527,#168528,#168529),.UNSPECIFIED.,.F.,.F.,
(4,2,2,2,4),(-0.381457606174089,-0.304035109378442,-0.190979808271481,-0.0912225470703838,
-1.00000006925116E-6),.UNSPECIFIED.);
#24324=B_SPLINE_CURVE_WITH_KNOTS('',3,(#168533,#168534,#168535,#168536,
#168537,#168538,#168539,#168540,#168541,#168542,#168543,#168544,#168545,
#168546,#168547,#168548,#168549,#168550,#168551,#168552,#168553,#168554,
#168555,#168556,#168557,#168558,#168559,#168560,#168561,#168562,#168563,
#168564,#168565,#168566,#168567,#168568,#168569,#168570,#168571,#168572,
#168573,#168574,#168575,#168576,#168577,#168578,#168579,#168580,#168581,
#168582,#168583,#168584,#168585,#168586,#168587,#168588,#168589,#168590,
#168591,#168592,#168593,#168594,#168595,#168596,#168597,#168598,#168599,
#168600,#168601,#168602,#168603,#168604,#168605,#168606,#168607,#168608,
#168609,#168610,#168611,#168612,#168613,#168614,#168615,#168616,#168617,
#168618,#168619,#168620,#168621,#168622,#168623,#168624,#168625,#168626,
#168627,#168628,#168629,#168630,#168631,#168632,#168633,#168634,#168635,
#168636,#168637,#168638,#168639,#168640,#168641),.UNSPECIFIED.,.F.,.F.,
(4,3,3,3,3,3,3,3,3,3,3,3,3,3,3,3,3,3,3,3,3,3,3,3,3,3,3,3,3,3,3,3,3,3,3,
3,4),(0.,0.000877428960298162,0.00182186904808312,0.00560425316389786,0.00749819548399555,
0.00939395278983934,0.0246236265420485,0.0553976406888011,0.10510590613333,
0.117953721761098,0.16822163443711,0.218581997077039,0.244710640454446,
0.25,0.350381617416015,0.448693290958287,0.484375,0.498632474707576,0.49999999286025,
0.50105084551746,0.601647811048279,0.624999999999999,0.725405038227879,
0.746093749999999,0.749999999999999,0.753208507973121,0.875,0.883895257725269,
0.918382175878415,0.946288347314178,0.976389806038248,0.991048440539466,
0.99286064175195,0.994668244628355,0.998269520917499,0.999166914580596,
0.999999987137999),.UNSPECIFIED.);
#24325=B_SPLINE_CURVE_WITH_KNOTS('',3,(#168644,#168645,#168646,#168647,
#168648,#168649,#168650,#168651,#168652,#168653),.UNSPECIFIED.,.F.,.F.,
(4,2,2,2,4),(-0.381485937812174,-0.290460031477783,-0.190961318136168,-0.0775891327103021,
-1.00000005109901E-6),.UNSPECIFIED.);
#24326=B_SPLINE_CURVE_WITH_KNOTS('',3,(#168657,#168658,#168659,#168660,
#168661,#168662,#168663,#168664,#168665,#168666),.UNSPECIFIED.,.F.,.F.,
(4,2,2,2,4),(1.00000006872122E-6,0.0915138874962241,0.190511167453547,0.301327535855596,
0.381447321977382),.UNSPECIFIED.);
#24327=B_SPLINE_CURVE_WITH_KNOTS('',3,(#168670,#168671,#168672,#168673,
#168674,#168675,#168676,#168677,#168678,#168679),.UNSPECIFIED.,.F.,.F.,
(4,2,2,2,4),(1.00000005224979E-6,0.0799606858619584,0.19048250138979,0.289749093438666,
0.381474629767968),.UNSPECIFIED.);
#24328=B_SPLINE_CURVE_WITH_KNOTS('',3,(#168832,#168833,#168834,#168835,
#168836,#168837,#168838,#168839,#168840,#168841,#168842,#168843,#168844,
#168845,#168846,#168847,#168848,#168849,#168850,#168851,#168852,#168853,
#168854,#168855,#168856,#168857,#168858,#168859,#168860,#168861,#168862,
#168863,#168864,#168865,#168866,#168867,#168868,#168869,#168870,#168871,
#168872,#168873,#168874,#168875,#168876,#168877,#168878,#168879,#168880,
#168881,#168882,#168883,#168884,#168885,#168886,#168887,#168888,#168889,
#168890,#168891,#168892,#168893,#168894,#168895,#168896,#168897,#168898,
#168899,#168900,#168901),.UNSPECIFIED.,.F.,.F.,(4,3,3,3,3,3,3,3,3,3,3,3,
3,3,3,3,3,3,3,3,3,3,3,4),(0.,0.000547902305461683,0.00249435877321915,0.0180971390547113,
0.0494623915149704,0.112771098950549,0.184521296536466,0.241157246478698,
0.313497254092451,0.385778846725024,0.457780221042424,0.5,0.500001064694345,
0.572039858897225,0.644277278226495,0.716628202259504,0.758843661753893,
0.830600495604986,0.887229062947173,0.950537595516011,0.981902833679206,
0.99750562749206,0.999452086664773,1.),.UNSPECIFIED.);
#24329=B_SPLINE_CURVE_WITH_KNOTS('',3,(#168902,#168903,#168904,#168905,
#168906,#168907),.UNSPECIFIED.,.F.,.F.,(4,2,4),(-0.146653736581323,-0.073340873363055,
-2.14074661886166E-8),.UNSPECIFIED.);
#24330=B_SPLINE_CURVE_WITH_KNOTS('',3,(#168908,#168909,#168910,#168911,
#168912,#168913),.UNSPECIFIED.,.F.,.F.,(4,2,4),(2.14415571569341E-8,0.0733336158677515,
0.146653733111165),.UNSPECIFIED.);
#24331=B_SPLINE_CURVE_WITH_KNOTS('',3,(#169034,#169035,#169036,#169037),
 .UNSPECIFIED.,.F.,.F.,(4,4),(0.,0.00231659945791558),.UNSPECIFIED.);
#24332=B_SPLINE_CURVE_WITH_KNOTS('',3,(#169039,#169040,#169041,#169042,
#169043,#169044),.UNSPECIFIED.,.F.,.F.,(4,2,4),(3.0808796214308E-11,0.603462743313919,
1.20583125094992),.UNSPECIFIED.);
#24333=B_SPLINE_CURVE_WITH_KNOTS('',3,(#169046,#169047,#169048,#169049),
 .UNSPECIFIED.,.F.,.F.,(4,4),(0.,0.00231659459060812),.UNSPECIFIED.);
#24334=B_SPLINE_CURVE_WITH_KNOTS('',3,(#169050,#169051,#169052,#169053,
#169054,#169055,#169056,#169057,#169058,#169059,#169060,#169061,#169062,
#169063,#169064,#169065,#169066,#169067,#169068,#169069,#169070,#169071,
#169072,#169073,#169074,#169075,#169076,#169077,#169078,#169079,#169080,
#169081,#169082,#169083,#169084,#169085,#169086,#169087,#169088,#169089,
#169090,#169091,#169092,#169093,#169094,#169095,#169096,#169097,#169098,
#169099,#169100,#169101,#169102,#169103,#169104,#169105,#169106,#169107,
#169108,#169109,#169110,#169111,#169112,#169113,#169114,#169115,#169116,
#169117,#169118,#169119,#169120,#169121,#169122,#169123,#169124,#169125,
#169126,#169127,#169128,#169129,#169130,#169131,#169132,#169133,#169134,
#169135,#169136,#169137,#169138,#169139,#169140,#169141,#169142,#169143,
#169144,#169145,#169146,#169147,#169148,#169149,#169150,#169151,#169152,
#169153,#169154,#169155,#169156,#169157,#169158,#169159,#169160,#169161,
#169162,#169163,#169164,#169165,#169166,#169167,#169168,#169169,#169170),
 .UNSPECIFIED.,.F.,.F.,(4,3,3,3,3,3,3,3,3,3,3,3,3,3,3,3,3,3,3,3,3,3,3,3,
3,3,3,3,3,3,3,3,3,3,3,3,3,3,3,3,4),(0.,0.00042823575704742,0.000953028677821348,
0.0296649831518755,0.0591239226216254,0.0715449679712171,0.101238290723875,
0.124999999999999,0.214939059133572,0.246093749999998,0.249999999999998,
0.32793420327691,0.364178809141005,0.374999999999999,0.426885162186684,
0.434050718234393,0.4375,0.46875,0.484375,0.492187500000001,0.496093750000001,
0.498046875000001,0.500000000000001,0.500100116785369,0.582767577315675,
0.625000000000002,0.648830863552705,0.699553986074555,0.716893346557216,
0.738137016722508,0.742187500000003,0.746093750000003,0.750000000000003,
0.785581258945703,0.826685989965252,0.86775510100022,0.908405445427098,
0.930378240366883,0.969699336603254,0.999108385391882,1.),.UNSPECIFIED.);
#24335=B_SPLINE_CURVE_WITH_KNOTS('',3,(#169262,#169263,#169264,#169265),
 .UNSPECIFIED.,.F.,.F.,(4,4),(0.,0.026268696648067),.UNSPECIFIED.);
#24336=B_SPLINE_CURVE_WITH_KNOTS('',3,(#169266,#169267,#169268,#169269),
 .UNSPECIFIED.,.F.,.F.,(4,4),(0.,0.0262686966482326),.UNSPECIFIED.);
#24337=B_SPLINE_CURVE_WITH_KNOTS('',3,(#169493,#169494,#169495,#169496,
#169497,#169498,#169499,#169500,#169501,#169502,#169503,#169504),
 .UNSPECIFIED.,.F.,.F.,(4,2,2,2,2,4),(-0.358600614497163,-0.336590698464702,
-0.314434291168697,-0.269758529940321,-0.179530499588331,0.),
 .UNSPECIFIED.);
#24338=B_SPLINE_CURVE_WITH_KNOTS('',3,(#169506,#169507,#169508,#169509,
#169510,#169511,#169512,#169513,#169514,#169515,#169516,#169517),
 .UNSPECIFIED.,.F.,.F.,(4,2,2,2,2,4),(-0.358600621348355,-0.336590661936306,
-0.314434253593136,-0.269758494188564,-0.179530484335802,0.),
 .UNSPECIFIED.);
#24339=B_SPLINE_CURVE_WITH_KNOTS('',3,(#169518,#169519,#169520,#169521,
#169522,#169523,#169524,#169525,#169526,#169527,#169528,#169529,#169530,
#169531,#169532,#169533,#169534,#169535,#169536,#169537,#169538,#169539,
#169540,#169541,#169542,#169543,#169544,#169545,#169546,#169547,#169548,
#169549,#169550,#169551,#169552,#169553,#169554,#169555,#169556,#169557,
#169558,#169559,#169560,#169561,#169562,#169563,#169564,#169565,#169566,
#169567,#169568,#169569,#169570,#169571,#169572,#169573,#169574,#169575,
#169576,#169577,#169578,#169579,#169580,#169581,#169582,#169583,#169584,
#169585,#169586,#169587,#169588,#169589,#169590,#169591,#169592,#169593,
#169594,#169595,#169596,#169597,#169598,#169599,#169600,#169601,#169602,
#169603,#169604,#169605,#169606,#169607,#169608,#169609,#169610,#169611),
 .UNSPECIFIED.,.F.,.F.,(4,3,3,3,3,3,3,3,3,3,3,3,3,3,3,3,3,3,3,3,3,3,3,3,
3,3,3,3,3,3,3,4),(7.07383405333801E-9,0.000185481200514374,0.00209789788204644,
0.00593407499601808,0.0371456031055623,0.0774279743208184,0.101927509204789,
0.142817818939058,0.168586675415445,0.20952907741012,0.235207511954171,
0.25,0.300771028306561,0.366577698048115,0.438379241599273,0.499951864993755,
0.5,0.578342126744578,0.633450287347176,0.699317094696975,0.75,0.764868961176406,
0.80547318591929,0.831490470403233,0.872074648468611,0.898160396314077,
0.938061990284187,0.962902096319114,0.994062344852343,0.997890509989055,
0.999798786687148,0.999999999553271),.UNSPECIFIED.);
#24340=B_SPLINE_CURVE_WITH_KNOTS('',3,(#169685,#169686,#169687,#169688),
 .UNSPECIFIED.,.F.,.F.,(4,4),(-0.931540742513151,-1.04317168914391E-10),
 .UNSPECIFIED.);
#24341=B_SPLINE_CURVE_WITH_KNOTS('',3,(#169691,#169692,#169693,#169694),
 .UNSPECIFIED.,.F.,.F.,(4,4),(-0.931540739806317,-1.04317110474898E-10),
 .UNSPECIFIED.);
#24342=B_SPLINE_CURVE_WITH_KNOTS('',3,(#169851,#169852,#169853,#169854,
#169855,#169856,#169857,#169858,#169859,#169860),.UNSPECIFIED.,.F.,.F.,
(4,2,2,2,4),(0.,0.133115171967196,0.274762912401081,0.416400475291265,0.54980469291253),
 .UNSPECIFIED.);
#24343=B_SPLINE_CURVE_WITH_KNOTS('',3,(#169861,#169862,#169863,#169864,
#169865,#169866,#169867,#169868,#169869,#169870),.UNSPECIFIED.,.F.,.F.,
(4,2,2,2,4),(0.,0.133115213677724,0.27476292019439,0.416400641733826,0.549804817426638),
 .UNSPECIFIED.);
#24344=B_SPLINE_CURVE_WITH_KNOTS('',3,(#169882,#169883,#169884,#169885),
 .UNSPECIFIED.,.F.,.F.,(4,4),(2.03287907341032E-19,0.0122388605934849),
 .UNSPECIFIED.);
#24345=B_SPLINE_CURVE_WITH_KNOTS('',3,(#169887,#169888,#169889,#169890),
 .UNSPECIFIED.,.F.,.F.,(4,4),(0.,0.0122414931162063),.UNSPECIFIED.);
#24346=B_SPLINE_CURVE_WITH_KNOTS('',3,(#169953,#169954,#169955,#169956,
#169957,#169958,#169959,#169960,#169961,#169962),.UNSPECIFIED.,.F.,.F.,
(4,2,2,2,4),(1.0000000459831E-6,0.156718909328961,0.329756212037607,0.502919854676326,
0.659729926439619),.UNSPECIFIED.);
#24347=B_SPLINE_CURVE_WITH_KNOTS('',3,(#169973,#169974,#169975,#169976,
#169977,#169978,#169979,#169980,#169981,#169982,#169983,#169984,#169985,
#169986,#169987,#169988,#169989,#169990),.UNSPECIFIED.,.F.,.F.,(4,2,2,2,
2,2,2,2,4),(-0.772891272014126,-0.711371011943309,-0.647238677062543,-0.582315553959231,
-0.517392430855918,-0.452469307752605,-0.387546184649291,-0.323413849768526,
-0.261893589697701),.UNSPECIFIED.);
#24348=B_SPLINE_CURVE_WITH_KNOTS('',3,(#169995,#169996,#169997,#169998),
 .UNSPECIFIED.,.F.,.F.,(4,4),(-0.261893589697701,-0.25928151488776),
 .UNSPECIFIED.);
#24349=B_SPLINE_CURVE_WITH_KNOTS('',3,(#169999,#170000,#170001,#170002,
#170003,#170004,#170005,#170006,#170007,#170008,#170009,#170010,#170011,
#170012,#170013,#170014,#170015,#170016,#170017,#170018,#170019),
 .UNSPECIFIED.,.F.,.F.,(4,2,2,2,3,2,2,2,2,4),(-0.25928151488776,-0.194741358681164,
-0.130201202474569,-0.0651006012372844,0.,0.0651006012372838,0.130201202474568,
0.194741358681163,0.259281514887759,0.261893589697708),.UNSPECIFIED.);
#24350=B_SPLINE_CURVE_WITH_KNOTS('',3,(#170022,#170023,#170024,#170025,
#170026,#170027,#170028,#170029,#170030,#170031),.UNSPECIFIED.,.F.,.F.,
(4,2,2,2,4),(-0.772891272014128,-0.711371011943309,-0.647238677062543,-0.58231555395923,
-0.517392430855917),.UNSPECIFIED.);
#24351=B_SPLINE_CURVE_WITH_KNOTS('',3,(#170032,#170033,#170034,#170035,
#170036,#170037,#170038,#170039,#170040,#170041,#170042,#170043,#170044,
#170045,#170046,#170047,#170048,#170049,#170050,#170051,#170052,#170053,
#170054,#170055,#170056,#170057,#170058,#170059,#170060),.UNSPECIFIED.,
 .F.,.F.,(4,2,2,2,2,2,2,2,3,2,2,2,2,4),(-0.517392430855917,-0.452469307752604,
-0.38754618464929,-0.323413849768524,-0.259281514887758,-0.194741358681163,
-0.130201202474568,-0.0651006012372838,0.,0.0651694580098041,0.130338916019608,
0.194810907043524,0.25928289806744,0.261894972877388),.UNSPECIFIED.);
#24352=B_SPLINE_CURVE_WITH_KNOTS('',3,(#170120,#170121,#170122,#170123),
 .UNSPECIFIED.,.F.,.F.,(4,4),(1.31298214335883,1.31559438320612),
 .UNSPECIFIED.);
#24353=B_SPLINE_CURVE_WITH_KNOTS('',3,(#170125,#170126,#170127,#170128,
#170129,#170130,#170131,#170132,#170133,#170134,#170135,#170136,#170137,
#170138,#170139,#170140,#170141,#170142,#170143,#170144),.UNSPECIFIED.,
 .F.,.F.,(4,2,2,2,2,2,2,2,2,4),(1.31559438320612,1.3812434679175,1.44689255262887,
1.5131731285367,1.57945370444452,1.64573428035235,1.71201485626017,1.77766394097155,
1.84331302568292,1.84592524876208),.UNSPECIFIED.);
#24354=B_SPLINE_CURVE_WITH_KNOTS('',3,(#170148,#170149,#170150,#170151,
#170152,#170153,#170154,#170155,#170156,#170157,#170158,#170159,#170160,
#170161,#170162,#170163,#170164,#170165,#170166),.UNSPECIFIED.,.F.,.F.,
(4,2,2,2,3,2,2,2,4),(0.792955713409892,0.85556854154341,0.920793592756085,
0.986881564054135,1.05296953535218,1.11898939802791,1.18500926070363,1.25030182195487,
1.31298214335883),.UNSPECIFIED.);
#24355=B_SPLINE_CURVE_WITH_KNOTS('',3,(#170169,#170170,#170171,#170172),
 .UNSPECIFIED.,.F.,.F.,(4,4),(1.84331422285043,1.84592646269772),
 .UNSPECIFIED.);
#24356=B_SPLINE_CURVE_WITH_KNOTS('',3,(#170173,#170174,#170175,#170176,
#170177,#170178,#170179,#170180,#170181,#170182,#170183,#170184,#170185,
#170186,#170187,#170188,#170189,#170190,#170191,#170192,#170193,#170194,
#170195,#170196,#170197,#170198,#170199,#170200,#170201,#170202,#170203,
#170204,#170205,#170206,#170207),.UNSPECIFIED.,.F.,.F.,(4,2,2,2,3,2,2,2,
2,2,2,2,2,2,2,2,4),(0.792956927345539,0.855637248749495,0.920929810000743,
0.986949672676464,1.05296953535218,1.11905750665023,1.18514547794829,1.25037052916096,
1.31559558037363,1.38124466508501,1.44689374979638,1.51317432570421,1.57945490161203,
1.64573547751986,1.71201605342768,1.77766513813906,1.84331422285043),
 .UNSPECIFIED.);
#24357=LINE('',#92440,#26445);
#24358=LINE('',#93591,#26446);
#24359=LINE('',#93608,#26447);
#24360=LINE('',#93626,#26448);
#24361=LINE('',#93633,#26449);
#24362=LINE('',#93638,#26450);
#24363=LINE('',#94169,#26451);
#24364=LINE('',#95591,#26452);
#24365=LINE('',#95626,#26453);
#24366=LINE('',#95646,#26454);
#24367=LINE('',#95674,#26455);
#24368=LINE('',#95694,#26456);
#24369=LINE('',#95722,#26457);
#24370=LINE('',#95742,#26458);
#24371=LINE('',#95770,#26459);
#24372=LINE('',#95790,#26460);
#24373=LINE('',#95818,#26461);
#24374=LINE('',#95838,#26462);
#24375=LINE('',#95866,#26463);
#24376=LINE('',#95886,#26464);
#24377=LINE('',#95911,#26465);
#24378=LINE('',#95919,#26466);
#24379=LINE('',#95947,#26467);
#24380=LINE('',#95967,#26468);
#24381=LINE('',#95995,#26469);
#24382=LINE('',#96015,#26470);
#24383=LINE('',#96043,#26471);
#24384=LINE('',#96063,#26472);
#24385=LINE('',#96091,#26473);
#24386=LINE('',#96111,#26474);
#24387=LINE('',#96139,#26475);
#24388=LINE('',#96159,#26476);
#24389=LINE('',#96187,#26477);
#24390=LINE('',#96207,#26478);
#24391=LINE('',#96235,#26479);
#24392=LINE('',#96255,#26480);
#24393=LINE('',#96283,#26481);
#24394=LINE('',#96303,#26482);
#24395=LINE('',#96331,#26483);
#24396=LINE('',#96351,#26484);
#24397=LINE('',#96379,#26485);
#24398=LINE('',#96399,#26486);
#24399=LINE('',#96427,#26487);
#24400=LINE('',#96447,#26488);
#24401=LINE('',#96475,#26489);
#24402=LINE('',#96495,#26490);
#24403=LINE('',#96523,#26491);
#24404=LINE('',#96543,#26492);
#24405=LINE('',#96571,#26493);
#24406=LINE('',#96591,#26494);
#24407=LINE('',#96619,#26495);
#24408=LINE('',#96639,#26496);
#24409=LINE('',#96667,#26497);
#24410=LINE('',#96687,#26498);
#24411=LINE('',#96715,#26499);
#24412=LINE('',#96735,#26500);
#24413=LINE('',#96763,#26501);
#24414=LINE('',#96773,#26502);
#24415=LINE('',#96811,#26503);
#24416=LINE('',#96832,#26504);
#24417=LINE('',#96859,#26505);
#24418=LINE('',#96879,#26506);
#24419=LINE('',#96907,#26507);
#24420=LINE('',#96927,#26508);
#24421=LINE('',#96957,#26509);
#24422=LINE('',#96977,#26510);
#24423=LINE('',#96988,#26511);
#24424=LINE('',#97009,#26512);
#24425=LINE('',#97024,#26513);
#24426=LINE('',#97045,#26514);
#24427=LINE('',#97060,#26515);
#24428=LINE('',#97081,#26516);
#24429=LINE('',#97096,#26517);
#24430=LINE('',#97117,#26518);
#24431=LINE('',#97132,#26519);
#24432=LINE('',#97153,#26520);
#24433=LINE('',#97168,#26521);
#24434=LINE('',#97189,#26522);
#24435=LINE('',#97204,#26523);
#24436=LINE('',#97225,#26524);
#24437=LINE('',#97240,#26525);
#24438=LINE('',#97261,#26526);
#24439=LINE('',#97276,#26527);
#24440=LINE('',#97297,#26528);
#24441=LINE('',#97312,#26529);
#24442=LINE('',#97333,#26530);
#24443=LINE('',#97348,#26531);
#24444=LINE('',#97369,#26532);
#24445=LINE('',#97384,#26533);
#24446=LINE('',#97405,#26534);
#24447=LINE('',#97420,#26535);
#24448=LINE('',#97441,#26536);
#24449=LINE('',#97455,#26537);
#24450=LINE('',#97472,#26538);
#24451=LINE('',#97483,#26539);
#24452=LINE('',#97504,#26540);
#24453=LINE('',#97519,#26541);
#24454=LINE('',#97540,#26542);
#24455=LINE('',#97555,#26543);
#24456=LINE('',#97576,#26544);
#24457=LINE('',#97591,#26545);
#24458=LINE('',#97612,#26546);
#24459=LINE('',#97627,#26547);
#24460=LINE('',#97648,#26548);
#24461=LINE('',#97663,#26549);
#24462=LINE('',#97684,#26550);
#24463=LINE('',#97699,#26551);
#24464=LINE('',#97720,#26552);
#24465=LINE('',#97735,#26553);
#24466=LINE('',#97756,#26554);
#24467=LINE('',#97771,#26555);
#24468=LINE('',#97792,#26556);
#24469=LINE('',#97807,#26557);
#24470=LINE('',#97828,#26558);
#24471=LINE('',#97843,#26559);
#24472=LINE('',#97864,#26560);
#24473=LINE('',#97879,#26561);
#24474=LINE('',#97900,#26562);
#24475=LINE('',#97915,#26563);
#24476=LINE('',#97936,#26564);
#24477=LINE('',#97951,#26565);
#24478=LINE('',#97972,#26566);
#24479=LINE('',#97992,#26567);
#24480=LINE('',#99706,#26568);
#24481=LINE('',#99739,#26569);
#24482=LINE('',#99755,#26570);
#24483=LINE('',#99788,#26571);
#24484=LINE('',#99804,#26572);
#24485=LINE('',#99837,#26573);
#24486=LINE('',#99853,#26574);
#24487=LINE('',#99886,#26575);
#24488=LINE('',#99902,#26576);
#24489=LINE('',#99935,#26577);
#24490=LINE('',#99951,#26578);
#24491=LINE('',#99984,#26579);
#24492=LINE('',#100000,#26580);
#24493=LINE('',#100033,#26581);
#24494=LINE('',#100049,#26582);
#24495=LINE('',#100082,#26583);
#24496=LINE('',#100098,#26584);
#24497=LINE('',#100131,#26585);
#24498=LINE('',#100147,#26586);
#24499=LINE('',#100180,#26587);
#24500=LINE('',#100196,#26588);
#24501=LINE('',#100229,#26589);
#24502=LINE('',#100245,#26590);
#24503=LINE('',#100278,#26591);
#24504=LINE('',#100294,#26592);
#24505=LINE('',#100327,#26593);
#24506=LINE('',#100343,#26594);
#24507=LINE('',#100376,#26595);
#24508=LINE('',#100389,#26596);
#24509=LINE('',#100404,#26597);
#24510=LINE('',#100420,#26598);
#24511=LINE('',#100453,#26599);
#24512=LINE('',#100469,#26600);
#24513=LINE('',#100502,#26601);
#24514=LINE('',#100518,#26602);
#24515=LINE('',#100551,#26603);
#24516=LINE('',#100567,#26604);
#24517=LINE('',#100600,#26605);
#24518=LINE('',#100616,#26606);
#24519=LINE('',#100649,#26607);
#24520=LINE('',#100665,#26608);
#24521=LINE('',#100698,#26609);
#24522=LINE('',#100714,#26610);
#24523=LINE('',#100747,#26611);
#24524=LINE('',#100763,#26612);
#24525=LINE('',#100796,#26613);
#24526=LINE('',#100812,#26614);
#24527=LINE('',#100845,#26615);
#24528=LINE('',#100861,#26616);
#24529=LINE('',#100884,#26617);
#24530=LINE('',#100902,#26618);
#24531=LINE('',#100943,#26619);
#24532=LINE('',#100959,#26620);
#24533=LINE('',#100992,#26621);
#24534=LINE('',#101008,#26622);
#24535=LINE('',#101041,#26623);
#24536=LINE('',#101057,#26624);
#24537=LINE('',#101090,#26625);
#24538=LINE('',#101102,#26626);
#24539=LINE('',#101123,#26627);
#24540=LINE('',#101143,#26628);
#24541=LINE('',#101164,#26629);
#24542=LINE('',#101184,#26630);
#24543=LINE('',#101205,#26631);
#24544=LINE('',#101225,#26632);
#24545=LINE('',#101246,#26633);
#24546=LINE('',#101266,#26634);
#24547=LINE('',#101287,#26635);
#24548=LINE('',#101307,#26636);
#24549=LINE('',#101328,#26637);
#24550=LINE('',#101348,#26638);
#24551=LINE('',#101369,#26639);
#24552=LINE('',#101389,#26640);
#24553=LINE('',#101410,#26641);
#24554=LINE('',#101430,#26642);
#24555=LINE('',#101451,#26643);
#24556=LINE('',#101471,#26644);
#24557=LINE('',#101492,#26645);
#24558=LINE('',#101512,#26646);
#24559=LINE('',#101533,#26647);
#24560=LINE('',#101553,#26648);
#24561=LINE('',#101574,#26649);
#24562=LINE('',#101594,#26650);
#24563=LINE('',#101615,#26651);
#24564=LINE('',#101635,#26652);
#24565=LINE('',#101656,#26653);
#24566=LINE('',#101676,#26654);
#24567=LINE('',#101697,#26655);
#24568=LINE('',#101717,#26656);
#24569=LINE('',#101738,#26657);
#24570=LINE('',#101758,#26658);
#24571=LINE('',#101779,#26659);
#24572=LINE('',#101799,#26660);
#24573=LINE('',#101820,#26661);
#24574=LINE('',#101840,#26662);
#24575=LINE('',#101861,#26663);
#24576=LINE('',#101881,#26664);
#24577=LINE('',#101902,#26665);
#24578=LINE('',#101922,#26666);
#24579=LINE('',#101943,#26667);
#24580=LINE('',#101962,#26668);
#24581=LINE('',#101979,#26669);
#24582=LINE('',#101991,#26670);
#24583=LINE('',#102012,#26671);
#24584=LINE('',#102032,#26672);
#24585=LINE('',#102053,#26673);
#24586=LINE('',#102073,#26674);
#24587=LINE('',#102094,#26675);
#24588=LINE('',#102114,#26676);
#24589=LINE('',#102135,#26677);
#24590=LINE('',#102155,#26678);
#24591=LINE('',#102176,#26679);
#24592=LINE('',#102196,#26680);
#24593=LINE('',#102217,#26681);
#24594=LINE('',#102237,#26682);
#24595=LINE('',#102258,#26683);
#24596=LINE('',#104190,#26684);
#24597=LINE('',#104226,#26685);
#24598=LINE('',#104239,#26686);
#24599=LINE('',#104269,#26687);
#24600=LINE('',#104282,#26688);
#24601=LINE('',#104312,#26689);
#24602=LINE('',#104325,#26690);
#24603=LINE('',#104355,#26691);
#24604=LINE('',#104368,#26692);
#24605=LINE('',#104398,#26693);
#24606=LINE('',#104411,#26694);
#24607=LINE('',#104441,#26695);
#24608=LINE('',#104454,#26696);
#24609=LINE('',#104475,#26697);
#24610=LINE('',#104482,#26698);
#24611=LINE('',#104512,#26699);
#24612=LINE('',#104525,#26700);
#24613=LINE('',#104555,#26701);
#24614=LINE('',#104568,#26702);
#24615=LINE('',#104598,#26703);
#24616=LINE('',#104611,#26704);
#24617=LINE('',#104641,#26705);
#24618=LINE('',#104654,#26706);
#24619=LINE('',#104684,#26707);
#24620=LINE('',#104697,#26708);
#24621=LINE('',#104727,#26709);
#24622=LINE('',#104740,#26710);
#24623=LINE('',#104770,#26711);
#24624=LINE('',#104783,#26712);
#24625=LINE('',#104813,#26713);
#24626=LINE('',#104826,#26714);
#24627=LINE('',#104856,#26715);
#24628=LINE('',#104869,#26716);
#24629=LINE('',#104899,#26717);
#24630=LINE('',#104912,#26718);
#24631=LINE('',#104942,#26719);
#24632=LINE('',#104955,#26720);
#24633=LINE('',#104985,#26721);
#24634=LINE('',#104998,#26722);
#24635=LINE('',#105028,#26723);
#24636=LINE('',#105041,#26724);
#24637=LINE('',#105071,#26725);
#24638=LINE('',#105084,#26726);
#24639=LINE('',#105114,#26727);
#24640=LINE('',#105127,#26728);
#24641=LINE('',#105157,#26729);
#24642=LINE('',#105170,#26730);
#24643=LINE('',#105200,#26731);
#24644=LINE('',#105209,#26732);
#24645=LINE('',#105229,#26733);
#24646=LINE('',#105256,#26734);
#24647=LINE('',#105286,#26735);
#24648=LINE('',#105299,#26736);
#24649=LINE('',#105329,#26737);
#24650=LINE('',#105342,#26738);
#24651=LINE('',#105372,#26739);
#24652=LINE('',#105385,#26740);
#24653=LINE('',#105412,#26741);
#24654=LINE('',#105432,#26742);
#24655=LINE('',#105448,#26743);
#24656=LINE('',#105475,#26744);
#24657=LINE('',#105495,#26745);
#24658=LINE('',#105522,#26746);
#24659=LINE('',#105542,#26747);
#24660=LINE('',#105569,#26748);
#24661=LINE('',#105589,#26749);
#24662=LINE('',#105616,#26750);
#24663=LINE('',#105636,#26751);
#24664=LINE('',#105663,#26752);
#24665=LINE('',#105683,#26753);
#24666=LINE('',#105710,#26754);
#24667=LINE('',#105730,#26755);
#24668=LINE('',#105757,#26756);
#24669=LINE('',#105777,#26757);
#24670=LINE('',#105804,#26758);
#24671=LINE('',#105824,#26759);
#24672=LINE('',#105851,#26760);
#24673=LINE('',#105871,#26761);
#24674=LINE('',#105898,#26762);
#24675=LINE('',#105918,#26763);
#24676=LINE('',#105945,#26764);
#24677=LINE('',#105965,#26765);
#24678=LINE('',#105992,#26766);
#24679=LINE('',#106012,#26767);
#24680=LINE('',#106039,#26768);
#24681=LINE('',#106058,#26769);
#24682=LINE('',#106075,#26770);
#24683=LINE('',#106091,#26771);
#24684=LINE('',#106118,#26772);
#24685=LINE('',#106138,#26773);
#24686=LINE('',#106165,#26774);
#24687=LINE('',#106185,#26775);
#24688=LINE('',#106212,#26776);
#24689=LINE('',#106232,#26777);
#24690=LINE('',#106259,#26778);
#24691=LINE('',#106279,#26779);
#24692=LINE('',#106306,#26780);
#24693=LINE('',#106326,#26781);
#24694=LINE('',#106353,#26782);
#24695=LINE('',#106373,#26783);
#24696=LINE('',#106400,#26784);
#24697=LINE('',#106420,#26785);
#24698=LINE('',#106447,#26786);
#24699=LINE('',#106467,#26787);
#24700=LINE('',#106494,#26788);
#24701=LINE('',#106514,#26789);
#24702=LINE('',#106541,#26790);
#24703=LINE('',#106561,#26791);
#24704=LINE('',#106588,#26792);
#24705=LINE('',#106608,#26793);
#24706=LINE('',#106635,#26794);
#24707=LINE('',#106655,#26795);
#24708=LINE('',#106682,#26796);
#24709=LINE('',#106702,#26797);
#24710=LINE('',#106729,#26798);
#24711=LINE('',#106760,#26799);
#24712=LINE('',#108631,#26800);
#24713=LINE('',#108647,#26801);
#24714=LINE('',#108667,#26802);
#24715=LINE('',#108683,#26803);
#24716=LINE('',#108703,#26804);
#24717=LINE('',#108719,#26805);
#24718=LINE('',#108739,#26806);
#24719=LINE('',#108755,#26807);
#24720=LINE('',#108775,#26808);
#24721=LINE('',#108791,#26809);
#24722=LINE('',#108811,#26810);
#24723=LINE('',#108827,#26811);
#24724=LINE('',#108847,#26812);
#24725=LINE('',#108863,#26813);
#24726=LINE('',#108883,#26814);
#24727=LINE('',#108899,#26815);
#24728=LINE('',#108919,#26816);
#24729=LINE('',#108935,#26817);
#24730=LINE('',#108955,#26818);
#24731=LINE('',#108971,#26819);
#24732=LINE('',#108991,#26820);
#24733=LINE('',#109007,#26821);
#24734=LINE('',#109027,#26822);
#24735=LINE('',#109043,#26823);
#24736=LINE('',#109063,#26824);
#24737=LINE('',#109079,#26825);
#24738=LINE('',#109099,#26826);
#24739=LINE('',#109115,#26827);
#24740=LINE('',#109132,#26828);
#24741=LINE('',#109142,#26829);
#24742=LINE('',#109162,#26830);
#24743=LINE('',#109178,#26831);
#24744=LINE('',#109198,#26832);
#24745=LINE('',#109214,#26833);
#24746=LINE('',#109234,#26834);
#24747=LINE('',#109250,#26835);
#24748=LINE('',#109270,#26836);
#24749=LINE('',#109286,#26837);
#24750=LINE('',#109306,#26838);
#24751=LINE('',#109322,#26839);
#24752=LINE('',#109342,#26840);
#24753=LINE('',#109358,#26841);
#24754=LINE('',#109378,#26842);
#24755=LINE('',#109394,#26843);
#24756=LINE('',#109414,#26844);
#24757=LINE('',#109430,#26845);
#24758=LINE('',#109450,#26846);
#24759=LINE('',#109462,#26847);
#24760=LINE('',#109478,#26848);
#24761=LINE('',#109502,#26849);
#24762=LINE('',#109522,#26850);
#24763=LINE('',#109538,#26851);
#24764=LINE('',#109558,#26852);
#24765=LINE('',#109574,#26853);
#24766=LINE('',#109594,#26854);
#24767=LINE('',#109610,#26855);
#24768=LINE('',#109630,#26856);
#24769=LINE('',#109646,#26857);
#24770=LINE('',#109654,#26858);
#24771=LINE('',#109685,#26859);
#24772=LINE('',#109697,#26860);
#24773=LINE('',#109728,#26861);
#24774=LINE('',#109740,#26862);
#24775=LINE('',#109771,#26863);
#24776=LINE('',#109783,#26864);
#24777=LINE('',#109814,#26865);
#24778=LINE('',#109826,#26866);
#24779=LINE('',#109857,#26867);
#24780=LINE('',#109869,#26868);
#24781=LINE('',#109900,#26869);
#24782=LINE('',#109912,#26870);
#24783=LINE('',#109943,#26871);
#24784=LINE('',#109955,#26872);
#24785=LINE('',#109986,#26873);
#24786=LINE('',#109998,#26874);
#24787=LINE('',#110029,#26875);
#24788=LINE('',#110041,#26876);
#24789=LINE('',#110072,#26877);
#24790=LINE('',#110084,#26878);
#24791=LINE('',#110115,#26879);
#24792=LINE('',#110127,#26880);
#24793=LINE('',#110158,#26881);
#24794=LINE('',#110170,#26882);
#24795=LINE('',#110201,#26883);
#24796=LINE('',#110213,#26884);
#24797=LINE('',#110244,#26885);
#24798=LINE('',#110256,#26886);
#24799=LINE('',#110287,#26887);
#24800=LINE('',#110299,#26888);
#24801=LINE('',#110330,#26889);
#24802=LINE('',#110342,#26890);
#24803=LINE('',#110373,#26891);
#24804=LINE('',#110385,#26892);
#24805=LINE('',#110416,#26893);
#24806=LINE('',#110428,#26894);
#24807=LINE('',#110459,#26895);
#24808=LINE('',#110471,#26896);
#24809=LINE('',#110502,#26897);
#24810=LINE('',#110514,#26898);
#24811=LINE('',#110545,#26899);
#24812=LINE('',#110557,#26900);
#24813=LINE('',#110588,#26901);
#24814=LINE('',#110600,#26902);
#24815=LINE('',#110631,#26903);
#24816=LINE('',#110643,#26904);
#24817=LINE('',#110674,#26905);
#24818=LINE('',#110686,#26906);
#24819=LINE('',#110717,#26907);
#24820=LINE('',#110729,#26908);
#24821=LINE('',#110760,#26909);
#24822=LINE('',#110772,#26910);
#24823=LINE('',#110803,#26911);
#24824=LINE('',#110815,#26912);
#24825=LINE('',#110846,#26913);
#24826=LINE('',#110858,#26914);
#24827=LINE('',#110889,#26915);
#24828=LINE('',#112357,#26916);
#24829=LINE('',#112383,#26917);
#24830=LINE('',#112409,#26918);
#24831=LINE('',#112429,#26919);
#24832=LINE('',#112455,#26920);
#24833=LINE('',#112475,#26921);
#24834=LINE('',#112501,#26922);
#24835=LINE('',#112521,#26923);
#24836=LINE('',#112547,#26924);
#24837=LINE('',#112567,#26925);
#24838=LINE('',#112593,#26926);
#24839=LINE('',#112613,#26927);
#24840=LINE('',#112639,#26928);
#24841=LINE('',#112656,#26929);
#24842=LINE('',#112667,#26930);
#24843=LINE('',#112687,#26931);
#24844=LINE('',#112713,#26932);
#24845=LINE('',#112733,#26933);
#24846=LINE('',#112759,#26934);
#24847=LINE('',#112779,#26935);
#24848=LINE('',#112805,#26936);
#24849=LINE('',#112825,#26937);
#24850=LINE('',#112851,#26938);
#24851=LINE('',#112871,#26939);
#24852=LINE('',#112897,#26940);
#24853=LINE('',#112917,#26941);
#24854=LINE('',#112943,#26942);
#24855=LINE('',#112963,#26943);
#24856=LINE('',#112989,#26944);
#24857=LINE('',#113009,#26945);
#24858=LINE('',#113035,#26946);
#24859=LINE('',#113055,#26947);
#24860=LINE('',#113081,#26948);
#24861=LINE('',#113101,#26949);
#24862=LINE('',#113127,#26950);
#24863=LINE('',#113147,#26951);
#24864=LINE('',#113173,#26952);
#24865=LINE('',#113193,#26953);
#24866=LINE('',#113219,#26954);
#24867=LINE('',#113239,#26955);
#24868=LINE('',#113265,#26956);
#24869=LINE('',#113285,#26957);
#24870=LINE('',#113311,#26958);
#24871=LINE('',#113331,#26959);
#24872=LINE('',#113357,#26960);
#24873=LINE('',#113377,#26961);
#24874=LINE('',#113390,#26962);
#24875=LINE('',#113415,#26963);
#24876=LINE('',#113449,#26964);
#24877=LINE('',#113469,#26965);
#24878=LINE('',#113495,#26966);
#24879=LINE('',#113515,#26967);
#24880=LINE('',#113541,#26968);
#24881=LINE('',#113561,#26969);
#24882=LINE('',#113587,#26970);
#24883=LINE('',#113607,#26971);
#24884=LINE('',#113633,#26972);
#24885=LINE('',#113659,#26973);
#24886=LINE('',#113673,#26974);
#24887=LINE('',#113687,#26975);
#24888=LINE('',#113708,#26976);
#24889=LINE('',#113720,#26977);
#24890=LINE('',#113741,#26978);
#24891=LINE('',#113753,#26979);
#24892=LINE('',#113774,#26980);
#24893=LINE('',#113786,#26981);
#24894=LINE('',#113807,#26982);
#24895=LINE('',#113819,#26983);
#24896=LINE('',#113840,#26984);
#24897=LINE('',#113852,#26985);
#24898=LINE('',#113873,#26986);
#24899=LINE('',#113885,#26987);
#24900=LINE('',#113906,#26988);
#24901=LINE('',#113918,#26989);
#24902=LINE('',#113939,#26990);
#24903=LINE('',#113951,#26991);
#24904=LINE('',#113972,#26992);
#24905=LINE('',#113984,#26993);
#24906=LINE('',#114005,#26994);
#24907=LINE('',#114017,#26995);
#24908=LINE('',#114038,#26996);
#24909=LINE('',#114050,#26997);
#24910=LINE('',#114071,#26998);
#24911=LINE('',#114083,#26999);
#24912=LINE('',#114104,#27000);
#24913=LINE('',#114115,#27001);
#24914=LINE('',#114132,#27002);
#24915=LINE('',#114140,#27003);
#24916=LINE('',#114161,#27004);
#24917=LINE('',#114173,#27005);
#24918=LINE('',#114194,#27006);
#24919=LINE('',#114206,#27007);
#24920=LINE('',#114227,#27008);
#24921=LINE('',#114239,#27009);
#24922=LINE('',#114260,#27010);
#24923=LINE('',#114272,#27011);
#24924=LINE('',#114293,#27012);
#24925=LINE('',#114305,#27013);
#24926=LINE('',#114326,#27014);
#24927=LINE('',#114338,#27015);
#24928=LINE('',#114359,#27016);
#24929=LINE('',#114371,#27017);
#24930=LINE('',#114392,#27018);
#24931=LINE('',#114404,#27019);
#24932=LINE('',#114425,#27020);
#24933=LINE('',#114437,#27021);
#24934=LINE('',#114458,#27022);
#24935=LINE('',#114470,#27023);
#24936=LINE('',#114491,#27024);
#24937=LINE('',#114503,#27025);
#24938=LINE('',#114524,#27026);
#24939=LINE('',#114536,#27027);
#24940=LINE('',#114557,#27028);
#24941=LINE('',#114569,#27029);
#24942=LINE('',#114590,#27030);
#24943=LINE('',#114607,#27031);
#24944=LINE('',#116251,#27032);
#24945=LINE('',#116278,#27033);
#24946=LINE('',#116298,#27034);
#24947=LINE('',#116325,#27035);
#24948=LINE('',#116345,#27036);
#24949=LINE('',#116372,#27037);
#24950=LINE('',#116392,#27038);
#24951=LINE('',#116419,#27039);
#24952=LINE('',#116439,#27040);
#24953=LINE('',#116466,#27041);
#24954=LINE('',#116486,#27042);
#24955=LINE('',#116513,#27043);
#24956=LINE('',#116533,#27044);
#24957=LINE('',#116560,#27045);
#24958=LINE('',#116580,#27046);
#24959=LINE('',#116607,#27047);
#24960=LINE('',#116627,#27048);
#24961=LINE('',#116654,#27049);
#24962=LINE('',#116674,#27050);
#24963=LINE('',#116701,#27051);
#24964=LINE('',#116721,#27052);
#24965=LINE('',#116748,#27053);
#24966=LINE('',#116768,#27054);
#24967=LINE('',#116795,#27055);
#24968=LINE('',#116815,#27056);
#24969=LINE('',#116842,#27057);
#24970=LINE('',#116862,#27058);
#24971=LINE('',#116889,#27059);
#24972=LINE('',#116906,#27060);
#24973=LINE('',#116921,#27061);
#24974=LINE('',#116941,#27062);
#24975=LINE('',#116968,#27063);
#24976=LINE('',#116988,#27064);
#24977=LINE('',#117015,#27065);
#24978=LINE('',#117035,#27066);
#24979=LINE('',#117062,#27067);
#24980=LINE('',#117082,#27068);
#24981=LINE('',#117109,#27069);
#24982=LINE('',#117129,#27070);
#24983=LINE('',#117156,#27071);
#24984=LINE('',#117176,#27072);
#24985=LINE('',#117203,#27073);
#24986=LINE('',#117223,#27074);
#24987=LINE('',#117250,#27075);
#24988=LINE('',#117270,#27076);
#24989=LINE('',#117293,#27077);
#24990=LINE('',#117309,#27078);
#24991=LINE('',#117344,#27079);
#24992=LINE('',#117364,#27080);
#24993=LINE('',#117391,#27081);
#24994=LINE('',#117411,#27082);
#24995=LINE('',#117438,#27083);
#24996=LINE('',#117458,#27084);
#24997=LINE('',#117485,#27085);
#24998=LINE('',#117505,#27086);
#24999=LINE('',#117532,#27087);
#25000=LINE('',#117552,#27088);
#25001=LINE('',#117579,#27089);
#25002=LINE('',#117591,#27090);
#25003=LINE('',#117612,#27091);
#25004=LINE('',#117628,#27092);
#25005=LINE('',#117649,#27093);
#25006=LINE('',#117665,#27094);
#25007=LINE('',#117686,#27095);
#25008=LINE('',#117702,#27096);
#25009=LINE('',#117723,#27097);
#25010=LINE('',#117739,#27098);
#25011=LINE('',#117760,#27099);
#25012=LINE('',#117776,#27100);
#25013=LINE('',#117797,#27101);
#25014=LINE('',#117813,#27102);
#25015=LINE('',#117834,#27103);
#25016=LINE('',#117850,#27104);
#25017=LINE('',#117871,#27105);
#25018=LINE('',#117887,#27106);
#25019=LINE('',#117908,#27107);
#25020=LINE('',#117924,#27108);
#25021=LINE('',#117945,#27109);
#25022=LINE('',#117961,#27110);
#25023=LINE('',#117982,#27111);
#25024=LINE('',#117998,#27112);
#25025=LINE('',#118019,#27113);
#25026=LINE('',#118035,#27114);
#25027=LINE('',#118056,#27115);
#25028=LINE('',#118072,#27116);
#25029=LINE('',#118093,#27117);
#25030=LINE('',#118109,#27118);
#25031=LINE('',#118130,#27119);
#25032=LINE('',#118146,#27120);
#25033=LINE('',#118167,#27121);
#25034=LINE('',#118183,#27122);
#25035=LINE('',#118204,#27123);
#25036=LINE('',#118220,#27124);
#25037=LINE('',#118241,#27125);
#25038=LINE('',#118257,#27126);
#25039=LINE('',#118278,#27127);
#25040=LINE('',#118294,#27128);
#25041=LINE('',#118315,#27129);
#25042=LINE('',#118331,#27130);
#25043=LINE('',#118352,#27131);
#25044=LINE('',#118367,#27132);
#25045=LINE('',#118384,#27133);
#25046=LINE('',#118396,#27134);
#25047=LINE('',#118417,#27135);
#25048=LINE('',#118433,#27136);
#25049=LINE('',#118454,#27137);
#25050=LINE('',#118470,#27138);
#25051=LINE('',#118491,#27139);
#25052=LINE('',#118507,#27140);
#25053=LINE('',#118528,#27141);
#25054=LINE('',#118544,#27142);
#25055=LINE('',#118565,#27143);
#25056=LINE('',#118581,#27144);
#25057=LINE('',#118602,#27145);
#25058=LINE('',#118618,#27146);
#25059=LINE('',#118639,#27147);
#25060=LINE('',#120741,#27148);
#25061=LINE('',#120777,#27149);
#25062=LINE('',#120790,#27150);
#25063=LINE('',#120820,#27151);
#25064=LINE('',#120833,#27152);
#25065=LINE('',#120863,#27153);
#25066=LINE('',#120876,#27154);
#25067=LINE('',#120906,#27155);
#25068=LINE('',#120919,#27156);
#25069=LINE('',#120949,#27157);
#25070=LINE('',#120962,#27158);
#25071=LINE('',#120992,#27159);
#25072=LINE('',#121005,#27160);
#25073=LINE('',#121026,#27161);
#25074=LINE('',#121033,#27162);
#25075=LINE('',#121063,#27163);
#25076=LINE('',#121076,#27164);
#25077=LINE('',#121106,#27165);
#25078=LINE('',#121119,#27166);
#25079=LINE('',#121149,#27167);
#25080=LINE('',#121162,#27168);
#25081=LINE('',#121192,#27169);
#25082=LINE('',#121205,#27170);
#25083=LINE('',#121235,#27171);
#25084=LINE('',#121248,#27172);
#25085=LINE('',#121278,#27173);
#25086=LINE('',#121291,#27174);
#25087=LINE('',#121321,#27175);
#25088=LINE('',#121334,#27176);
#25089=LINE('',#121364,#27177);
#25090=LINE('',#121377,#27178);
#25091=LINE('',#121407,#27179);
#25092=LINE('',#121420,#27180);
#25093=LINE('',#121450,#27181);
#25094=LINE('',#121463,#27182);
#25095=LINE('',#121493,#27183);
#25096=LINE('',#121506,#27184);
#25097=LINE('',#121536,#27185);
#25098=LINE('',#121549,#27186);
#25099=LINE('',#121579,#27187);
#25100=LINE('',#121592,#27188);
#25101=LINE('',#121622,#27189);
#25102=LINE('',#121635,#27190);
#25103=LINE('',#121665,#27191);
#25104=LINE('',#121674,#27192);
#25105=LINE('',#121694,#27193);
#25106=LINE('',#121721,#27194);
#25107=LINE('',#121751,#27195);
#25108=LINE('',#121764,#27196);
#25109=LINE('',#121794,#27197);
#25110=LINE('',#121807,#27198);
#25111=LINE('',#121837,#27199);
#25112=LINE('',#121850,#27200);
#25113=LINE('',#121880,#27201);
#25114=LINE('',#121893,#27202);
#25115=LINE('',#121923,#27203);
#25116=LINE('',#121936,#27204);
#25117=LINE('',#121963,#27205);
#25118=LINE('',#121979,#27206);
#25119=LINE('',#121991,#27207);
#25120=LINE('',#122014,#27208);
#25121=LINE('',#122030,#27209);
#25122=LINE('',#122053,#27210);
#25123=LINE('',#122069,#27211);
#25124=LINE('',#122092,#27212);
#25125=LINE('',#122108,#27213);
#25126=LINE('',#122131,#27214);
#25127=LINE('',#122147,#27215);
#25128=LINE('',#122170,#27216);
#25129=LINE('',#122186,#27217);
#25130=LINE('',#122209,#27218);
#25131=LINE('',#122225,#27219);
#25132=LINE('',#122248,#27220);
#25133=LINE('',#122264,#27221);
#25134=LINE('',#122287,#27222);
#25135=LINE('',#122303,#27223);
#25136=LINE('',#122326,#27224);
#25137=LINE('',#122342,#27225);
#25138=LINE('',#122365,#27226);
#25139=LINE('',#122381,#27227);
#25140=LINE('',#122404,#27228);
#25141=LINE('',#122420,#27229);
#25142=LINE('',#122443,#27230);
#25143=LINE('',#122459,#27231);
#25144=LINE('',#122482,#27232);
#25145=LINE('',#122497,#27233);
#25146=LINE('',#122510,#27234);
#25147=LINE('',#122522,#27235);
#25148=LINE('',#122545,#27236);
#25149=LINE('',#122561,#27237);
#25150=LINE('',#122584,#27238);
#25151=LINE('',#122600,#27239);
#25152=LINE('',#122623,#27240);
#25153=LINE('',#122639,#27241);
#25154=LINE('',#122662,#27242);
#25155=LINE('',#122678,#27243);
#25156=LINE('',#122701,#27244);
#25157=LINE('',#122717,#27245);
#25158=LINE('',#122740,#27246);
#25159=LINE('',#122756,#27247);
#25160=LINE('',#122779,#27248);
#25161=LINE('',#122795,#27249);
#25162=LINE('',#122818,#27250);
#25163=LINE('',#122834,#27251);
#25164=LINE('',#122857,#27252);
#25165=LINE('',#122873,#27253);
#25166=LINE('',#122896,#27254);
#25167=LINE('',#122912,#27255);
#25168=LINE('',#122935,#27256);
#25169=LINE('',#122951,#27257);
#25170=LINE('',#122974,#27258);
#25171=LINE('',#122990,#27259);
#25172=LINE('',#123013,#27260);
#25173=LINE('',#123029,#27261);
#25174=LINE('',#123052,#27262);
#25175=LINE('',#123079,#27263);
#25176=LINE('',#125098,#27264);
#25177=LINE('',#125111,#27265);
#25178=LINE('',#125131,#27266);
#25179=LINE('',#125144,#27267);
#25180=LINE('',#125164,#27268);
#25181=LINE('',#125177,#27269);
#25182=LINE('',#125197,#27270);
#25183=LINE('',#125210,#27271);
#25184=LINE('',#125230,#27272);
#25185=LINE('',#125243,#27273);
#25186=LINE('',#125263,#27274);
#25187=LINE('',#125276,#27275);
#25188=LINE('',#125296,#27276);
#25189=LINE('',#125309,#27277);
#25190=LINE('',#125329,#27278);
#25191=LINE('',#125342,#27279);
#25192=LINE('',#125362,#27280);
#25193=LINE('',#125375,#27281);
#25194=LINE('',#125395,#27282);
#25195=LINE('',#125408,#27283);
#25196=LINE('',#125428,#27284);
#25197=LINE('',#125441,#27285);
#25198=LINE('',#125461,#27286);
#25199=LINE('',#125474,#27287);
#25200=LINE('',#125494,#27288);
#25201=LINE('',#125507,#27289);
#25202=LINE('',#125527,#27290);
#25203=LINE('',#125540,#27291);
#25204=LINE('',#125557,#27292);
#25205=LINE('',#125564,#27293);
#25206=LINE('',#125584,#27294);
#25207=LINE('',#125597,#27295);
#25208=LINE('',#125617,#27296);
#25209=LINE('',#125630,#27297);
#25210=LINE('',#125650,#27298);
#25211=LINE('',#125663,#27299);
#25212=LINE('',#125683,#27300);
#25213=LINE('',#125696,#27301);
#25214=LINE('',#125716,#27302);
#25215=LINE('',#125729,#27303);
#25216=LINE('',#125749,#27304);
#25217=LINE('',#125762,#27305);
#25218=LINE('',#125782,#27306);
#25219=LINE('',#125791,#27307);
#25220=LINE('',#125807,#27308);
#25221=LINE('',#125828,#27309);
#25222=LINE('',#125848,#27310);
#25223=LINE('',#125861,#27311);
#25224=LINE('',#125881,#27312);
#25225=LINE('',#125894,#27313);
#25226=LINE('',#125914,#27314);
#25227=LINE('',#125927,#27315);
#25228=LINE('',#125947,#27316);
#25229=LINE('',#125960,#27317);
#25230=LINE('',#125980,#27318);
#25231=LINE('',#125993,#27319);
#25232=LINE('',#126013,#27320);
#25233=LINE('',#126026,#27321);
#25234=LINE('',#126038,#27322);
#25235=LINE('',#126065,#27323);
#25236=LINE('',#126081,#27324);
#25237=LINE('',#126108,#27325);
#25238=LINE('',#126124,#27326);
#25239=LINE('',#126151,#27327);
#25240=LINE('',#126167,#27328);
#25241=LINE('',#126194,#27329);
#25242=LINE('',#126210,#27330);
#25243=LINE('',#126237,#27331);
#25244=LINE('',#126253,#27332);
#25245=LINE('',#126280,#27333);
#25246=LINE('',#126296,#27334);
#25247=LINE('',#126323,#27335);
#25248=LINE('',#126339,#27336);
#25249=LINE('',#126366,#27337);
#25250=LINE('',#126382,#27338);
#25251=LINE('',#126409,#27339);
#25252=LINE('',#126425,#27340);
#25253=LINE('',#126452,#27341);
#25254=LINE('',#126468,#27342);
#25255=LINE('',#126495,#27343);
#25256=LINE('',#126511,#27344);
#25257=LINE('',#126538,#27345);
#25258=LINE('',#126554,#27346);
#25259=LINE('',#126581,#27347);
#25260=LINE('',#126597,#27348);
#25261=LINE('',#126624,#27349);
#25262=LINE('',#126640,#27350);
#25263=LINE('',#126667,#27351);
#25264=LINE('',#126683,#27352);
#25265=LINE('',#126710,#27353);
#25266=LINE('',#126726,#27354);
#25267=LINE('',#126753,#27355);
#25268=LINE('',#126769,#27356);
#25269=LINE('',#126796,#27357);
#25270=LINE('',#126812,#27358);
#25271=LINE('',#126839,#27359);
#25272=LINE('',#126855,#27360);
#25273=LINE('',#126882,#27361);
#25274=LINE('',#126898,#27362);
#25275=LINE('',#126925,#27363);
#25276=LINE('',#126940,#27364);
#25277=LINE('',#126957,#27365);
#25278=LINE('',#126969,#27366);
#25279=LINE('',#126996,#27367);
#25280=LINE('',#127012,#27368);
#25281=LINE('',#127039,#27369);
#25282=LINE('',#127055,#27370);
#25283=LINE('',#127082,#27371);
#25284=LINE('',#127098,#27372);
#25285=LINE('',#127125,#27373);
#25286=LINE('',#127141,#27374);
#25287=LINE('',#127168,#27375);
#25288=LINE('',#127184,#27376);
#25289=LINE('',#127211,#27377);
#25290=LINE('',#127227,#27378);
#25291=LINE('',#127254,#27379);
#25292=LINE('',#128722,#27380);
#25293=LINE('',#128748,#27381);
#25294=LINE('',#128765,#27382);
#25295=LINE('',#128785,#27383);
#25296=LINE('',#128802,#27384);
#25297=LINE('',#128822,#27385);
#25298=LINE('',#128839,#27386);
#25299=LINE('',#128859,#27387);
#25300=LINE('',#128876,#27388);
#25301=LINE('',#128896,#27389);
#25302=LINE('',#128913,#27390);
#25303=LINE('',#128933,#27391);
#25304=LINE('',#128950,#27392);
#25305=LINE('',#128967,#27393);
#25306=LINE('',#128978,#27394);
#25307=LINE('',#128998,#27395);
#25308=LINE('',#129015,#27396);
#25309=LINE('',#129035,#27397);
#25310=LINE('',#129052,#27398);
#25311=LINE('',#129072,#27399);
#25312=LINE('',#129089,#27400);
#25313=LINE('',#129109,#27401);
#25314=LINE('',#129126,#27402);
#25315=LINE('',#129146,#27403);
#25316=LINE('',#129163,#27404);
#25317=LINE('',#129183,#27405);
#25318=LINE('',#129200,#27406);
#25319=LINE('',#129220,#27407);
#25320=LINE('',#129237,#27408);
#25321=LINE('',#129257,#27409);
#25322=LINE('',#129274,#27410);
#25323=LINE('',#129294,#27411);
#25324=LINE('',#129311,#27412);
#25325=LINE('',#129331,#27413);
#25326=LINE('',#129348,#27414);
#25327=LINE('',#129368,#27415);
#25328=LINE('',#129385,#27416);
#25329=LINE('',#129405,#27417);
#25330=LINE('',#129422,#27418);
#25331=LINE('',#129442,#27419);
#25332=LINE('',#129459,#27420);
#25333=LINE('',#129479,#27421);
#25334=LINE('',#129492,#27422);
#25335=LINE('',#129508,#27423);
#25336=LINE('',#129533,#27424);
#25337=LINE('',#129553,#27425);
#25338=LINE('',#129570,#27426);
#25339=LINE('',#129590,#27427);
#25340=LINE('',#129607,#27428);
#25341=LINE('',#129627,#27429);
#25342=LINE('',#129644,#27430);
#25343=LINE('',#129664,#27431);
#25344=LINE('',#129681,#27432);
#25345=LINE('',#129701,#27433);
#25346=LINE('',#129718,#27434);
#25347=LINE('',#129738,#27435);
#25348=LINE('',#129755,#27436);
#25349=LINE('',#129772,#27437);
#25350=LINE('',#129788,#27438);
#25351=LINE('',#129800,#27439);
#25352=LINE('',#129817,#27440);
#25353=LINE('',#129833,#27441);
#25354=LINE('',#129850,#27442);
#25355=LINE('',#129866,#27443);
#25356=LINE('',#129883,#27444);
#25357=LINE('',#129899,#27445);
#25358=LINE('',#129916,#27446);
#25359=LINE('',#129932,#27447);
#25360=LINE('',#129949,#27448);
#25361=LINE('',#129965,#27449);
#25362=LINE('',#129982,#27450);
#25363=LINE('',#129998,#27451);
#25364=LINE('',#130015,#27452);
#25365=LINE('',#130031,#27453);
#25366=LINE('',#130048,#27454);
#25367=LINE('',#130064,#27455);
#25368=LINE('',#130081,#27456);
#25369=LINE('',#130097,#27457);
#25370=LINE('',#130114,#27458);
#25371=LINE('',#130130,#27459);
#25372=LINE('',#130147,#27460);
#25373=LINE('',#130163,#27461);
#25374=LINE('',#130180,#27462);
#25375=LINE('',#130196,#27463);
#25376=LINE('',#130213,#27464);
#25377=LINE('',#130228,#27465);
#25378=LINE('',#130241,#27466);
#25379=LINE('',#130253,#27467);
#25380=LINE('',#130270,#27468);
#25381=LINE('',#130286,#27469);
#25382=LINE('',#130303,#27470);
#25383=LINE('',#130319,#27471);
#25384=LINE('',#130336,#27472);
#25385=LINE('',#130352,#27473);
#25386=LINE('',#130369,#27474);
#25387=LINE('',#130385,#27475);
#25388=LINE('',#130402,#27476);
#25389=LINE('',#130418,#27477);
#25390=LINE('',#130435,#27478);
#25391=LINE('',#130451,#27479);
#25392=LINE('',#130468,#27480);
#25393=LINE('',#130484,#27481);
#25394=LINE('',#130501,#27482);
#25395=LINE('',#130517,#27483);
#25396=LINE('',#130534,#27484);
#25397=LINE('',#130550,#27485);
#25398=LINE('',#130567,#27486);
#25399=LINE('',#130583,#27487);
#25400=LINE('',#130600,#27488);
#25401=LINE('',#130616,#27489);
#25402=LINE('',#130633,#27490);
#25403=LINE('',#130649,#27491);
#25404=LINE('',#130666,#27492);
#25405=LINE('',#130682,#27493);
#25406=LINE('',#130699,#27494);
#25407=LINE('',#130720,#27495);
#25408=LINE('',#132652,#27496);
#25409=LINE('',#132675,#27497);
#25410=LINE('',#132691,#27498);
#25411=LINE('',#132714,#27499);
#25412=LINE('',#132730,#27500);
#25413=LINE('',#132753,#27501);
#25414=LINE('',#132769,#27502);
#25415=LINE('',#132792,#27503);
#25416=LINE('',#132808,#27504);
#25417=LINE('',#132831,#27505);
#25418=LINE('',#132847,#27506);
#25419=LINE('',#132870,#27507);
#25420=LINE('',#132886,#27508);
#25421=LINE('',#132909,#27509);
#25422=LINE('',#132925,#27510);
#25423=LINE('',#132948,#27511);
#25424=LINE('',#132964,#27512);
#25425=LINE('',#132985,#27513);
#25426=LINE('',#133001,#27514);
#25427=LINE('',#133024,#27515);
#25428=LINE('',#133040,#27516);
#25429=LINE('',#133063,#27517);
#25430=LINE('',#133079,#27518);
#25431=LINE('',#133102,#27519);
#25432=LINE('',#133118,#27520);
#25433=LINE('',#133141,#27521);
#25434=LINE('',#133157,#27522);
#25435=LINE('',#133180,#27523);
#25436=LINE('',#133193,#27524);
#25437=LINE('',#133204,#27525);
#25438=LINE('',#133220,#27526);
#25439=LINE('',#133243,#27527);
#25440=LINE('',#133259,#27528);
#25441=LINE('',#133282,#27529);
#25442=LINE('',#133298,#27530);
#25443=LINE('',#133321,#27531);
#25444=LINE('',#133337,#27532);
#25445=LINE('',#133360,#27533);
#25446=LINE('',#133376,#27534);
#25447=LINE('',#133399,#27535);
#25448=LINE('',#133415,#27536);
#25449=LINE('',#133434,#27537);
#25450=LINE('',#133446,#27538);
#25451=LINE('',#133477,#27539);
#25452=LINE('',#133493,#27540);
#25453=LINE('',#133516,#27541);
#25454=LINE('',#133532,#27542);
#25455=LINE('',#133555,#27543);
#25456=LINE('',#133571,#27544);
#25457=LINE('',#133594,#27545);
#25458=LINE('',#133610,#27546);
#25459=LINE('',#133633,#27547);
#25460=LINE('',#133649,#27548);
#25461=LINE('',#133672,#27549);
#25462=LINE('',#133688,#27550);
#25463=LINE('',#133711,#27551);
#25464=LINE('',#133727,#27552);
#25465=LINE('',#133750,#27553);
#25466=LINE('',#133758,#27554);
#25467=LINE('',#133775,#27555);
#25468=LINE('',#133787,#27556);
#25469=LINE('',#133804,#27557);
#25470=LINE('',#133816,#27558);
#25471=LINE('',#133833,#27559);
#25472=LINE('',#133845,#27560);
#25473=LINE('',#133862,#27561);
#25474=LINE('',#133874,#27562);
#25475=LINE('',#133891,#27563);
#25476=LINE('',#133903,#27564);
#25477=LINE('',#133920,#27565);
#25478=LINE('',#133932,#27566);
#25479=LINE('',#133949,#27567);
#25480=LINE('',#133961,#27568);
#25481=LINE('',#133978,#27569);
#25482=LINE('',#133990,#27570);
#25483=LINE('',#134007,#27571);
#25484=LINE('',#134019,#27572);
#25485=LINE('',#134036,#27573);
#25486=LINE('',#134048,#27574);
#25487=LINE('',#134065,#27575);
#25488=LINE('',#134077,#27576);
#25489=LINE('',#134094,#27577);
#25490=LINE('',#134106,#27578);
#25491=LINE('',#134123,#27579);
#25492=LINE('',#134135,#27580);
#25493=LINE('',#134152,#27581);
#25494=LINE('',#134164,#27582);
#25495=LINE('',#134181,#27583);
#25496=LINE('',#134193,#27584);
#25497=LINE('',#134210,#27585);
#25498=LINE('',#134222,#27586);
#25499=LINE('',#134239,#27587);
#25500=LINE('',#134251,#27588);
#25501=LINE('',#134268,#27589);
#25502=LINE('',#134280,#27590);
#25503=LINE('',#134297,#27591);
#25504=LINE('',#134309,#27592);
#25505=LINE('',#134326,#27593);
#25506=LINE('',#134338,#27594);
#25507=LINE('',#134355,#27595);
#25508=LINE('',#134367,#27596);
#25509=LINE('',#134384,#27597);
#25510=LINE('',#134396,#27598);
#25511=LINE('',#134413,#27599);
#25512=LINE('',#134425,#27600);
#25513=LINE('',#134442,#27601);
#25514=LINE('',#134454,#27602);
#25515=LINE('',#134471,#27603);
#25516=LINE('',#134483,#27604);
#25517=LINE('',#134500,#27605);
#25518=LINE('',#134512,#27606);
#25519=LINE('',#134529,#27607);
#25520=LINE('',#134541,#27608);
#25521=LINE('',#134558,#27609);
#25522=LINE('',#134570,#27610);
#25523=LINE('',#134587,#27611);
#25524=LINE('',#137321,#27612);
#25525=LINE('',#137353,#27613);
#25526=LINE('',#137370,#27614);
#25527=LINE('',#137396,#27615);
#25528=LINE('',#137413,#27616);
#25529=LINE('',#137439,#27617);
#25530=LINE('',#137456,#27618);
#25531=LINE('',#137482,#27619);
#25532=LINE('',#137499,#27620);
#25533=LINE('',#137525,#27621);
#25534=LINE('',#137542,#27622);
#25535=LINE('',#137568,#27623);
#25536=LINE('',#137585,#27624);
#25537=LINE('',#137602,#27625);
#25538=LINE('',#137613,#27626);
#25539=LINE('',#137639,#27627);
#25540=LINE('',#137656,#27628);
#25541=LINE('',#137682,#27629);
#25542=LINE('',#137699,#27630);
#25543=LINE('',#137725,#27631);
#25544=LINE('',#137742,#27632);
#25545=LINE('',#137768,#27633);
#25546=LINE('',#137785,#27634);
#25547=LINE('',#137811,#27635);
#25548=LINE('',#137828,#27636);
#25549=LINE('',#137854,#27637);
#25550=LINE('',#137871,#27638);
#25551=LINE('',#137897,#27639);
#25552=LINE('',#137914,#27640);
#25553=LINE('',#137940,#27641);
#25554=LINE('',#137957,#27642);
#25555=LINE('',#137983,#27643);
#25556=LINE('',#138000,#27644);
#25557=LINE('',#138026,#27645);
#25558=LINE('',#138043,#27646);
#25559=LINE('',#138069,#27647);
#25560=LINE('',#138086,#27648);
#25561=LINE('',#138112,#27649);
#25562=LINE('',#138129,#27650);
#25563=LINE('',#138155,#27651);
#25564=LINE('',#138168,#27652);
#25565=LINE('',#138184,#27653);
#25566=LINE('',#138215,#27654);
#25567=LINE('',#138241,#27655);
#25568=LINE('',#138258,#27656);
#25569=LINE('',#138284,#27657);
#25570=LINE('',#138301,#27658);
#25571=LINE('',#138327,#27659);
#25572=LINE('',#138344,#27660);
#25573=LINE('',#138370,#27661);
#25574=LINE('',#138387,#27662);
#25575=LINE('',#138413,#27663);
#25576=LINE('',#138430,#27664);
#25577=LINE('',#138456,#27665);
#25578=LINE('',#138473,#27666);
#25579=LINE('',#138499,#27667);
#25580=LINE('',#138516,#27668);
#25581=LINE('',#138539,#27669);
#25582=LINE('',#138559,#27670);
#25583=LINE('',#138571,#27671);
#25584=LINE('',#138598,#27672);
#25585=LINE('',#138614,#27673);
#25586=LINE('',#138641,#27674);
#25587=LINE('',#138657,#27675);
#25588=LINE('',#138684,#27676);
#25589=LINE('',#138700,#27677);
#25590=LINE('',#138727,#27678);
#25591=LINE('',#138743,#27679);
#25592=LINE('',#138770,#27680);
#25593=LINE('',#138786,#27681);
#25594=LINE('',#138813,#27682);
#25595=LINE('',#138829,#27683);
#25596=LINE('',#138856,#27684);
#25597=LINE('',#138872,#27685);
#25598=LINE('',#138899,#27686);
#25599=LINE('',#138915,#27687);
#25600=LINE('',#138942,#27688);
#25601=LINE('',#138958,#27689);
#25602=LINE('',#138985,#27690);
#25603=LINE('',#139001,#27691);
#25604=LINE('',#139028,#27692);
#25605=LINE('',#139044,#27693);
#25606=LINE('',#139071,#27694);
#25607=LINE('',#139087,#27695);
#25608=LINE('',#139114,#27696);
#25609=LINE('',#139129,#27697);
#25610=LINE('',#139146,#27698);
#25611=LINE('',#139158,#27699);
#25612=LINE('',#139185,#27700);
#25613=LINE('',#139201,#27701);
#25614=LINE('',#139228,#27702);
#25615=LINE('',#139244,#27703);
#25616=LINE('',#139271,#27704);
#25617=LINE('',#139287,#27705);
#25618=LINE('',#139314,#27706);
#25619=LINE('',#139330,#27707);
#25620=LINE('',#139357,#27708);
#25621=LINE('',#139373,#27709);
#25622=LINE('',#139400,#27710);
#25623=LINE('',#139416,#27711);
#25624=LINE('',#139443,#27712);
#25625=LINE('',#139459,#27713);
#25626=LINE('',#139486,#27714);
#25627=LINE('',#139502,#27715);
#25628=LINE('',#139529,#27716);
#25629=LINE('',#139545,#27717);
#25630=LINE('',#139572,#27718);
#25631=LINE('',#139588,#27719);
#25632=LINE('',#139615,#27720);
#25633=LINE('',#139631,#27721);
#25634=LINE('',#139658,#27722);
#25635=LINE('',#139674,#27723);
#25636=LINE('',#139701,#27724);
#25637=LINE('',#139717,#27725);
#25638=LINE('',#139744,#27726);
#25639=LINE('',#139771,#27727);
#25640=LINE('',#141383,#27728);
#25641=LINE('',#141400,#27729);
#25642=LINE('',#141416,#27730);
#25643=LINE('',#141433,#27731);
#25644=LINE('',#141449,#27732);
#25645=LINE('',#141466,#27733);
#25646=LINE('',#141482,#27734);
#25647=LINE('',#141499,#27735);
#25648=LINE('',#141515,#27736);
#25649=LINE('',#141532,#27737);
#25650=LINE('',#141548,#27738);
#25651=LINE('',#141565,#27739);
#25652=LINE('',#141581,#27740);
#25653=LINE('',#141598,#27741);
#25654=LINE('',#141614,#27742);
#25655=LINE('',#141631,#27743);
#25656=LINE('',#141647,#27744);
#25657=LINE('',#141664,#27745);
#25658=LINE('',#141680,#27746);
#25659=LINE('',#141697,#27747);
#25660=LINE('',#141713,#27748);
#25661=LINE('',#141730,#27749);
#25662=LINE('',#141746,#27750);
#25663=LINE('',#141763,#27751);
#25664=LINE('',#141779,#27752);
#25665=LINE('',#141796,#27753);
#25666=LINE('',#141812,#27754);
#25667=LINE('',#141829,#27755);
#25668=LINE('',#141842,#27756);
#25669=LINE('',#141853,#27757);
#25670=LINE('',#141869,#27758);
#25671=LINE('',#141886,#27759);
#25672=LINE('',#141902,#27760);
#25673=LINE('',#141919,#27761);
#25674=LINE('',#141935,#27762);
#25675=LINE('',#141952,#27763);
#25676=LINE('',#141968,#27764);
#25677=LINE('',#141985,#27765);
#25678=LINE('',#142001,#27766);
#25679=LINE('',#142014,#27767);
#25680=LINE('',#142026,#27768);
#25681=LINE('',#142051,#27769);
#25682=LINE('',#142067,#27770);
#25683=LINE('',#142084,#27771);
#25684=LINE('',#142100,#27772);
#25685=LINE('',#142117,#27773);
#25686=LINE('',#142133,#27774);
#25687=LINE('',#142150,#27775);
#25688=LINE('',#142166,#27776);
#25689=LINE('',#142183,#27777);
#25690=LINE('',#142199,#27778);
#25691=LINE('',#142216,#27779);
#25692=LINE('',#142232,#27780);
#25693=LINE('',#142249,#27781);
#25694=LINE('',#142265,#27782);
#25695=LINE('',#142282,#27783);
#25696=LINE('',#142298,#27784);
#25697=LINE('',#142315,#27785);
#25698=LINE('',#142327,#27786);
#25699=LINE('',#142352,#27787);
#25700=LINE('',#142368,#27788);
#25701=LINE('',#142393,#27789);
#25702=LINE('',#142409,#27790);
#25703=LINE('',#142434,#27791);
#25704=LINE('',#142450,#27792);
#25705=LINE('',#142475,#27793);
#25706=LINE('',#142491,#27794);
#25707=LINE('',#142516,#27795);
#25708=LINE('',#142532,#27796);
#25709=LINE('',#142557,#27797);
#25710=LINE('',#142573,#27798);
#25711=LINE('',#142598,#27799);
#25712=LINE('',#142614,#27800);
#25713=LINE('',#142639,#27801);
#25714=LINE('',#142655,#27802);
#25715=LINE('',#142680,#27803);
#25716=LINE('',#142696,#27804);
#25717=LINE('',#142721,#27805);
#25718=LINE('',#142737,#27806);
#25719=LINE('',#142762,#27807);
#25720=LINE('',#142778,#27808);
#25721=LINE('',#142803,#27809);
#25722=LINE('',#142819,#27810);
#25723=LINE('',#142844,#27811);
#25724=LINE('',#142860,#27812);
#25725=LINE('',#142885,#27813);
#25726=LINE('',#142901,#27814);
#25727=LINE('',#142926,#27815);
#25728=LINE('',#142942,#27816);
#25729=LINE('',#142967,#27817);
#25730=LINE('',#142983,#27818);
#25731=LINE('',#143008,#27819);
#25732=LINE('',#143024,#27820);
#25733=LINE('',#143049,#27821);
#25734=LINE('',#143065,#27822);
#25735=LINE('',#143090,#27823);
#25736=LINE('',#143106,#27824);
#25737=LINE('',#143131,#27825);
#25738=LINE('',#143147,#27826);
#25739=LINE('',#143172,#27827);
#25740=LINE('',#143187,#27828);
#25741=LINE('',#143208,#27829);
#25742=LINE('',#143220,#27830);
#25743=LINE('',#143245,#27831);
#25744=LINE('',#143261,#27832);
#25745=LINE('',#143286,#27833);
#25746=LINE('',#143302,#27834);
#25747=LINE('',#143327,#27835);
#25748=LINE('',#143343,#27836);
#25749=LINE('',#143368,#27837);
#25750=LINE('',#143384,#27838);
#25751=LINE('',#143409,#27839);
#25752=LINE('',#143425,#27840);
#25753=LINE('',#143450,#27841);
#25754=LINE('',#143466,#27842);
#25755=LINE('',#143491,#27843);
#25756=LINE('',#144839,#27844);
#25757=LINE('',#144861,#27845);
#25758=LINE('',#144874,#27846);
#25759=LINE('',#144890,#27847);
#25760=LINE('',#144903,#27848);
#25761=LINE('',#144919,#27849);
#25762=LINE('',#144932,#27850);
#25763=LINE('',#144948,#27851);
#25764=LINE('',#144961,#27852);
#25765=LINE('',#144977,#27853);
#25766=LINE('',#144990,#27854);
#25767=LINE('',#145006,#27855);
#25768=LINE('',#145019,#27856);
#25769=LINE('',#145032,#27857);
#25770=LINE('',#145039,#27858);
#25771=LINE('',#145055,#27859);
#25772=LINE('',#145068,#27860);
#25773=LINE('',#145084,#27861);
#25774=LINE('',#145097,#27862);
#25775=LINE('',#145113,#27863);
#25776=LINE('',#145126,#27864);
#25777=LINE('',#145142,#27865);
#25778=LINE('',#145155,#27866);
#25779=LINE('',#145171,#27867);
#25780=LINE('',#145184,#27868);
#25781=LINE('',#145200,#27869);
#25782=LINE('',#145213,#27870);
#25783=LINE('',#145229,#27871);
#25784=LINE('',#145242,#27872);
#25785=LINE('',#145258,#27873);
#25786=LINE('',#145271,#27874);
#25787=LINE('',#145287,#27875);
#25788=LINE('',#145300,#27876);
#25789=LINE('',#145316,#27877);
#25790=LINE('',#145329,#27878);
#25791=LINE('',#145345,#27879);
#25792=LINE('',#145358,#27880);
#25793=LINE('',#145374,#27881);
#25794=LINE('',#145383,#27882);
#25795=LINE('',#145395,#27883);
#25796=LINE('',#145416,#27884);
#25797=LINE('',#145432,#27885);
#25798=LINE('',#145445,#27886);
#25799=LINE('',#145461,#27887);
#25800=LINE('',#145474,#27888);
#25801=LINE('',#145490,#27889);
#25802=LINE('',#145503,#27890);
#25803=LINE('',#145519,#27891);
#25804=LINE('',#145532,#27892);
#25805=LINE('',#145548,#27893);
#25806=LINE('',#145561,#27894);
#25807=LINE('',#145577,#27895);
#25808=LINE('',#145590,#27896);
#25809=LINE('',#145606,#27897);
#25810=LINE('',#145619,#27898);
#25811=LINE('',#145635,#27899);
#25812=LINE('',#145648,#27900);
#25813=LINE('',#145661,#27901);
#25814=LINE('',#145677,#27902);
#25815=LINE('',#145689,#27903);
#25816=LINE('',#145706,#27904);
#25817=LINE('',#145722,#27905);
#25818=LINE('',#145739,#27906);
#25819=LINE('',#145755,#27907);
#25820=LINE('',#145772,#27908);
#25821=LINE('',#145788,#27909);
#25822=LINE('',#145805,#27910);
#25823=LINE('',#145821,#27911);
#25824=LINE('',#145838,#27912);
#25825=LINE('',#145854,#27913);
#25826=LINE('',#145871,#27914);
#25827=LINE('',#145887,#27915);
#25828=LINE('',#145904,#27916);
#25829=LINE('',#145920,#27917);
#25830=LINE('',#145937,#27918);
#25831=LINE('',#145953,#27919);
#25832=LINE('',#145970,#27920);
#25833=LINE('',#145986,#27921);
#25834=LINE('',#146003,#27922);
#25835=LINE('',#146019,#27923);
#25836=LINE('',#146036,#27924);
#25837=LINE('',#146052,#27925);
#25838=LINE('',#146069,#27926);
#25839=LINE('',#146085,#27927);
#25840=LINE('',#146102,#27928);
#25841=LINE('',#146117,#27929);
#25842=LINE('',#146130,#27930);
#25843=LINE('',#146142,#27931);
#25844=LINE('',#146159,#27932);
#25845=LINE('',#146175,#27933);
#25846=LINE('',#146192,#27934);
#25847=LINE('',#146208,#27935);
#25848=LINE('',#146225,#27936);
#25849=LINE('',#146241,#27937);
#25850=LINE('',#146258,#27938);
#25851=LINE('',#146274,#27939);
#25852=LINE('',#146291,#27940);
#25853=LINE('',#146307,#27941);
#25854=LINE('',#146324,#27942);
#25855=LINE('',#146340,#27943);
#25856=LINE('',#146357,#27944);
#25857=LINE('',#146373,#27945);
#25858=LINE('',#146390,#27946);
#25859=LINE('',#146406,#27947);
#25860=LINE('',#146423,#27948);
#25861=LINE('',#146439,#27949);
#25862=LINE('',#146456,#27950);
#25863=LINE('',#146472,#27951);
#25864=LINE('',#146489,#27952);
#25865=LINE('',#146505,#27953);
#25866=LINE('',#146522,#27954);
#25867=LINE('',#146538,#27955);
#25868=LINE('',#146555,#27956);
#25869=LINE('',#146571,#27957);
#25870=LINE('',#146588,#27958);
#25871=LINE('',#146609,#27959);
#25872=LINE('',#148721,#27960);
#25873=LINE('',#148744,#27961);
#25874=LINE('',#148764,#27962);
#25875=LINE('',#148787,#27963);
#25876=LINE('',#148807,#27964);
#25877=LINE('',#148830,#27965);
#25878=LINE('',#148850,#27966);
#25879=LINE('',#148873,#27967);
#25880=LINE('',#148893,#27968);
#25881=LINE('',#148916,#27969);
#25882=LINE('',#148936,#27970);
#25883=LINE('',#148959,#27971);
#25884=LINE('',#148979,#27972);
#25885=LINE('',#149002,#27973);
#25886=LINE('',#149022,#27974);
#25887=LINE('',#149045,#27975);
#25888=LINE('',#149065,#27976);
#25889=LINE('',#149088,#27977);
#25890=LINE('',#149108,#27978);
#25891=LINE('',#149131,#27979);
#25892=LINE('',#149151,#27980);
#25893=LINE('',#149174,#27981);
#25894=LINE('',#149194,#27982);
#25895=LINE('',#149217,#27983);
#25896=LINE('',#149237,#27984);
#25897=LINE('',#149260,#27985);
#25898=LINE('',#149280,#27986);
#25899=LINE('',#149303,#27987);
#25900=LINE('',#149320,#27988);
#25901=LINE('',#149331,#27989);
#25902=LINE('',#149351,#27990);
#25903=LINE('',#149374,#27991);
#25904=LINE('',#149394,#27992);
#25905=LINE('',#149417,#27993);
#25906=LINE('',#149437,#27994);
#25907=LINE('',#149460,#27995);
#25908=LINE('',#149480,#27996);
#25909=LINE('',#149499,#27997);
#25910=LINE('',#149515,#27998);
#25911=LINE('',#149546,#27999);
#25912=LINE('',#149566,#28000);
#25913=LINE('',#149589,#28001);
#25914=LINE('',#149609,#28002);
#25915=LINE('',#149632,#28003);
#25916=LINE('',#149652,#28004);
#25917=LINE('',#149675,#28005);
#25918=LINE('',#149695,#28006);
#25919=LINE('',#149718,#28007);
#25920=LINE('',#149738,#28008);
#25921=LINE('',#149761,#28009);
#25922=LINE('',#149781,#28010);
#25923=LINE('',#149804,#28011);
#25924=LINE('',#149824,#28012);
#25925=LINE('',#149847,#28013);
#25926=LINE('',#149867,#28014);
#25927=LINE('',#149890,#28015);
#25928=LINE('',#149910,#28016);
#25929=LINE('',#149933,#28017);
#25930=LINE('',#149945,#28018);
#25931=LINE('',#149969,#28019);
#25932=LINE('',#149984,#28020);
#25933=LINE('',#150008,#28021);
#25934=LINE('',#150023,#28022);
#25935=LINE('',#150047,#28023);
#25936=LINE('',#150062,#28024);
#25937=LINE('',#150086,#28025);
#25938=LINE('',#150101,#28026);
#25939=LINE('',#150125,#28027);
#25940=LINE('',#150140,#28028);
#25941=LINE('',#150164,#28029);
#25942=LINE('',#150179,#28030);
#25943=LINE('',#150203,#28031);
#25944=LINE('',#150218,#28032);
#25945=LINE('',#150242,#28033);
#25946=LINE('',#150257,#28034);
#25947=LINE('',#150281,#28035);
#25948=LINE('',#150296,#28036);
#25949=LINE('',#150320,#28037);
#25950=LINE('',#150335,#28038);
#25951=LINE('',#150359,#28039);
#25952=LINE('',#150374,#28040);
#25953=LINE('',#150398,#28041);
#25954=LINE('',#150413,#28042);
#25955=LINE('',#150437,#28043);
#25956=LINE('',#150452,#28044);
#25957=LINE('',#150476,#28045);
#25958=LINE('',#150491,#28046);
#25959=LINE('',#150515,#28047);
#25960=LINE('',#150530,#28048);
#25961=LINE('',#150554,#28049);
#25962=LINE('',#150569,#28050);
#25963=LINE('',#150593,#28051);
#25964=LINE('',#150608,#28052);
#25965=LINE('',#150632,#28053);
#25966=LINE('',#150647,#28054);
#25967=LINE('',#150671,#28055);
#25968=LINE('',#150686,#28056);
#25969=LINE('',#150710,#28057);
#25970=LINE('',#150725,#28058);
#25971=LINE('',#150749,#28059);
#25972=LINE('',#150763,#28060);
#25973=LINE('',#150776,#28061);
#25974=LINE('',#150788,#28062);
#25975=LINE('',#150812,#28063);
#25976=LINE('',#150827,#28064);
#25977=LINE('',#150851,#28065);
#25978=LINE('',#150866,#28066);
#25979=LINE('',#150890,#28067);
#25980=LINE('',#150905,#28068);
#25981=LINE('',#150929,#28069);
#25982=LINE('',#150944,#28070);
#25983=LINE('',#150968,#28071);
#25984=LINE('',#150983,#28072);
#25985=LINE('',#151007,#28073);
#25986=LINE('',#151022,#28074);
#25987=LINE('',#151046,#28075);
#25988=LINE('',#152514,#28076);
#25989=LINE('',#152544,#28077);
#25990=LINE('',#152561,#28078);
#25991=LINE('',#152585,#28079);
#25992=LINE('',#152602,#28080);
#25993=LINE('',#152626,#28081);
#25994=LINE('',#152643,#28082);
#25995=LINE('',#152667,#28083);
#25996=LINE('',#152684,#28084);
#25997=LINE('',#152708,#28085);
#25998=LINE('',#152725,#28086);
#25999=LINE('',#152749,#28087);
#26000=LINE('',#152766,#28088);
#26001=LINE('',#152787,#28089);
#26002=LINE('',#152798,#28090);
#26003=LINE('',#152822,#28091);
#26004=LINE('',#152839,#28092);
#26005=LINE('',#152863,#28093);
#26006=LINE('',#152880,#28094);
#26007=LINE('',#152904,#28095);
#26008=LINE('',#152921,#28096);
#26009=LINE('',#152945,#28097);
#26010=LINE('',#152962,#28098);
#26011=LINE('',#152986,#28099);
#26012=LINE('',#153003,#28100);
#26013=LINE('',#153027,#28101);
#26014=LINE('',#153044,#28102);
#26015=LINE('',#153068,#28103);
#26016=LINE('',#153085,#28104);
#26017=LINE('',#153109,#28105);
#26018=LINE('',#153126,#28106);
#26019=LINE('',#153150,#28107);
#26020=LINE('',#153167,#28108);
#26021=LINE('',#153191,#28109);
#26022=LINE('',#153208,#28110);
#26023=LINE('',#153232,#28111);
#26024=LINE('',#153245,#28112);
#26025=LINE('',#153265,#28113);
#26026=LINE('',#153290,#28114);
#26027=LINE('',#153314,#28115);
#26028=LINE('',#153331,#28116);
#26029=LINE('',#153355,#28117);
#26030=LINE('',#153372,#28118);
#26031=LINE('',#153396,#28119);
#26032=LINE('',#153413,#28120);
#26033=LINE('',#153437,#28121);
#26034=LINE('',#153454,#28122);
#26035=LINE('',#153478,#28123);
#26036=LINE('',#153495,#28124);
#26037=LINE('',#153519,#28125);
#26038=LINE('',#153536,#28126);
#26039=LINE('',#153560,#28127);
#26040=LINE('',#153577,#28128);
#26041=LINE('',#153601,#28129);
#26042=LINE('',#153618,#28130);
#26043=LINE('',#153642,#28131);
#26044=LINE('',#153659,#28132);
#26045=LINE('',#153680,#28133);
#26046=LINE('',#153704,#28134);
#26047=LINE('',#153715,#28135);
#26048=LINE('',#153763,#28136);
#26049=LINE('',#153774,#28137);
#26050=LINE('',#153822,#28138);
#26051=LINE('',#153833,#28139);
#26052=LINE('',#153881,#28140);
#26053=LINE('',#153892,#28141);
#26054=LINE('',#153940,#28142);
#26055=LINE('',#153951,#28143);
#26056=LINE('',#153999,#28144);
#26057=LINE('',#154010,#28145);
#26058=LINE('',#154058,#28146);
#26059=LINE('',#154069,#28147);
#26060=LINE('',#154117,#28148);
#26061=LINE('',#154128,#28149);
#26062=LINE('',#154176,#28150);
#26063=LINE('',#154187,#28151);
#26064=LINE('',#154235,#28152);
#26065=LINE('',#154246,#28153);
#26066=LINE('',#154294,#28154);
#26067=LINE('',#154305,#28155);
#26068=LINE('',#154353,#28156);
#26069=LINE('',#154364,#28157);
#26070=LINE('',#154412,#28158);
#26071=LINE('',#154423,#28159);
#26072=LINE('',#154471,#28160);
#26073=LINE('',#154481,#28161);
#26074=LINE('',#154497,#28162);
#26075=LINE('',#154508,#28163);
#26076=LINE('',#154556,#28164);
#26077=LINE('',#154567,#28165);
#26078=LINE('',#154615,#28166);
#26079=LINE('',#154626,#28167);
#26080=LINE('',#154674,#28168);
#26081=LINE('',#154685,#28169);
#26082=LINE('',#154733,#28170);
#26083=LINE('',#154744,#28171);
#26084=LINE('',#154792,#28172);
#26085=LINE('',#154803,#28173);
#26086=LINE('',#154851,#28174);
#26087=LINE('',#154861,#28175);
#26088=LINE('',#154877,#28176);
#26089=LINE('',#154888,#28177);
#26090=LINE('',#154936,#28178);
#26091=LINE('',#154947,#28179);
#26092=LINE('',#154995,#28180);
#26093=LINE('',#155006,#28181);
#26094=LINE('',#155054,#28182);
#26095=LINE('',#155065,#28183);
#26096=LINE('',#155113,#28184);
#26097=LINE('',#155124,#28185);
#26098=LINE('',#155172,#28186);
#26099=LINE('',#155183,#28187);
#26100=LINE('',#155231,#28188);
#26101=LINE('',#155242,#28189);
#26102=LINE('',#155290,#28190);
#26103=LINE('',#155325,#28191);
#26104=LINE('',#157185,#28192);
#26105=LINE('',#157202,#28193);
#26106=LINE('',#157218,#28194);
#26107=LINE('',#157235,#28195);
#26108=LINE('',#157251,#28196);
#26109=LINE('',#157268,#28197);
#26110=LINE('',#157284,#28198);
#26111=LINE('',#157301,#28199);
#26112=LINE('',#157317,#28200);
#26113=LINE('',#157334,#28201);
#26114=LINE('',#157350,#28202);
#26115=LINE('',#157367,#28203);
#26116=LINE('',#157383,#28204);
#26117=LINE('',#157400,#28205);
#26118=LINE('',#157416,#28206);
#26119=LINE('',#157433,#28207);
#26120=LINE('',#157449,#28208);
#26121=LINE('',#157466,#28209);
#26122=LINE('',#157482,#28210);
#26123=LINE('',#157499,#28211);
#26124=LINE('',#157515,#28212);
#26125=LINE('',#157532,#28213);
#26126=LINE('',#157548,#28214);
#26127=LINE('',#157565,#28215);
#26128=LINE('',#157581,#28216);
#26129=LINE('',#157598,#28217);
#26130=LINE('',#157614,#28218);
#26131=LINE('',#157631,#28219);
#26132=LINE('',#157644,#28220);
#26133=LINE('',#157655,#28221);
#26134=LINE('',#157671,#28222);
#26135=LINE('',#157688,#28223);
#26136=LINE('',#157704,#28224);
#26137=LINE('',#157721,#28225);
#26138=LINE('',#157737,#28226);
#26139=LINE('',#157750,#28227);
#26140=LINE('',#157762,#28228);
#26141=LINE('',#157787,#28229);
#26142=LINE('',#157803,#28230);
#26143=LINE('',#157820,#28231);
#26144=LINE('',#157836,#28232);
#26145=LINE('',#157853,#28233);
#26146=LINE('',#157869,#28234);
#26147=LINE('',#157886,#28235);
#26148=LINE('',#157902,#28236);
#26149=LINE('',#157919,#28237);
#26150=LINE('',#157935,#28238);
#26151=LINE('',#157952,#28239);
#26152=LINE('',#157968,#28240);
#26153=LINE('',#157985,#28241);
#26154=LINE('',#158001,#28242);
#26155=LINE('',#158018,#28243);
#26156=LINE('',#158034,#28244);
#26157=LINE('',#158051,#28245);
#26158=LINE('',#158067,#28246);
#26159=LINE('',#158084,#28247);
#26160=LINE('',#158100,#28248);
#26161=LINE('',#158117,#28249);
#26162=LINE('',#158129,#28250);
#26163=LINE('',#158173,#28251);
#26164=LINE('',#158204,#28252);
#26165=LINE('',#158259,#28253);
#26166=LINE('',#158290,#28254);
#26167=LINE('',#158344,#28255);
#26168=LINE('',#158375,#28256);
#26169=LINE('',#158430,#28257);
#26170=LINE('',#158461,#28258);
#26171=LINE('',#158514,#28259);
#26172=LINE('',#158545,#28260);
#26173=LINE('',#158600,#28261);
#26174=LINE('',#158631,#28262);
#26175=LINE('',#158685,#28263);
#26176=LINE('',#158716,#28264);
#26177=LINE('',#158771,#28265);
#26178=LINE('',#158802,#28266);
#26179=LINE('',#158856,#28267);
#26180=LINE('',#158887,#28268);
#26181=LINE('',#158942,#28269);
#26182=LINE('',#158973,#28270);
#26183=LINE('',#159028,#28271);
#26184=LINE('',#159059,#28272);
#26185=LINE('',#159114,#28273);
#26186=LINE('',#159145,#28274);
#26187=LINE('',#159199,#28275);
#26188=LINE('',#159230,#28276);
#26189=LINE('',#159284,#28277);
#26190=LINE('',#159315,#28278);
#26191=LINE('',#159370,#28279);
#26192=LINE('',#159401,#28280);
#26193=LINE('',#159456,#28281);
#26194=LINE('',#159487,#28282);
#26195=LINE('',#159541,#28283);
#26196=LINE('',#159572,#28284);
#26197=LINE('',#159626,#28285);
#26198=LINE('',#159657,#28286);
#26199=LINE('',#159712,#28287);
#26200=LINE('',#159743,#28288);
#26201=LINE('',#159797,#28289);
#26202=LINE('',#159828,#28290);
#26203=LINE('',#159883,#28291);
#26204=LINE('',#159914,#28292);
#26205=LINE('',#159969,#28293);
#26206=LINE('',#160000,#28294);
#26207=LINE('',#160055,#28295);
#26208=LINE('',#160086,#28296);
#26209=LINE('',#160141,#28297);
#26210=LINE('',#160172,#28298);
#26211=LINE('',#160226,#28299);
#26212=LINE('',#160257,#28300);
#26213=LINE('',#160312,#28301);
#26214=LINE('',#160343,#28302);
#26215=LINE('',#160398,#28303);
#26216=LINE('',#160429,#28304);
#26217=LINE('',#160484,#28305);
#26218=LINE('',#160515,#28306);
#26219=LINE('',#160570,#28307);
#26220=LINE('',#161339,#28308);
#26221=LINE('',#161361,#28309);
#26222=LINE('',#161381,#28310);
#26223=LINE('',#161400,#28311);
#26224=LINE('',#161420,#28312);
#26225=LINE('',#161439,#28313);
#26226=LINE('',#161459,#28314);
#26227=LINE('',#161478,#28315);
#26228=LINE('',#161498,#28316);
#26229=LINE('',#161517,#28317);
#26230=LINE('',#161537,#28318);
#26231=LINE('',#161556,#28319);
#26232=LINE('',#161576,#28320);
#26233=LINE('',#161592,#28321);
#26234=LINE('',#161607,#28322);
#26235=LINE('',#161623,#28323);
#26236=LINE('',#161643,#28324);
#26237=LINE('',#161662,#28325);
#26238=LINE('',#161682,#28326);
#26239=LINE('',#161701,#28327);
#26240=LINE('',#161721,#28328);
#26241=LINE('',#161740,#28329);
#26242=LINE('',#161760,#28330);
#26243=LINE('',#161779,#28331);
#26244=LINE('',#161799,#28332);
#26245=LINE('',#161818,#28333);
#26246=LINE('',#161838,#28334);
#26247=LINE('',#161857,#28335);
#26248=LINE('',#161877,#28336);
#26249=LINE('',#161896,#28337);
#26250=LINE('',#161916,#28338);
#26251=LINE('',#161935,#28339);
#26252=LINE('',#161955,#28340);
#26253=LINE('',#161974,#28341);
#26254=LINE('',#161994,#28342);
#26255=LINE('',#162005,#28343);
#26256=LINE('',#162033,#28344);
#26257=LINE('',#162052,#28345);
#26258=LINE('',#162072,#28346);
#26259=LINE('',#162091,#28347);
#26260=LINE('',#162111,#28348);
#26261=LINE('',#162130,#28349);
#26262=LINE('',#162150,#28350);
#26263=LINE('',#162169,#28351);
#26264=LINE('',#162189,#28352);
#26265=LINE('',#162208,#28353);
#26266=LINE('',#162228,#28354);
#26267=LINE('',#162247,#28355);
#26268=LINE('',#162267,#28356);
#26269=LINE('',#162286,#28357);
#26270=LINE('',#162306,#28358);
#26271=LINE('',#162325,#28359);
#26272=LINE('',#162345,#28360);
#26273=LINE('',#162364,#28361);
#26274=LINE('',#162384,#28362);
#26275=LINE('',#162403,#28363);
#26276=LINE('',#162423,#28364);
#26277=LINE('',#162445,#28365);
#26278=LINE('',#163037,#28366);
#26279=LINE('',#163085,#28367);
#26280=LINE('',#163096,#28368);
#26281=LINE('',#163144,#28369);
#26282=LINE('',#163155,#28370);
#26283=LINE('',#163203,#28371);
#26284=LINE('',#163214,#28372);
#26285=LINE('',#163262,#28373);
#26286=LINE('',#163273,#28374);
#26287=LINE('',#163321,#28375);
#26288=LINE('',#163332,#28376);
#26289=LINE('',#163380,#28377);
#26290=LINE('',#163391,#28378);
#26291=LINE('',#163439,#28379);
#26292=LINE('',#163450,#28380);
#26293=LINE('',#163498,#28381);
#26294=LINE('',#163509,#28382);
#26295=LINE('',#163557,#28383);
#26296=LINE('',#163568,#28384);
#26297=LINE('',#163616,#28385);
#26298=LINE('',#163627,#28386);
#26299=LINE('',#163675,#28387);
#26300=LINE('',#163686,#28388);
#26301=LINE('',#163734,#28389);
#26302=LINE('',#163745,#28390);
#26303=LINE('',#163793,#28391);
#26304=LINE('',#163804,#28392);
#26305=LINE('',#163852,#28393);
#26306=LINE('',#163863,#28394);
#26307=LINE('',#163911,#28395);
#26308=LINE('',#163922,#28396);
#26309=LINE('',#163970,#28397);
#26310=LINE('',#163981,#28398);
#26311=LINE('',#164029,#28399);
#26312=LINE('',#164040,#28400);
#26313=LINE('',#164088,#28401);
#26314=LINE('',#164099,#28402);
#26315=LINE('',#164147,#28403);
#26316=LINE('',#164158,#28404);
#26317=LINE('',#164206,#28405);
#26318=LINE('',#164217,#28406);
#26319=LINE('',#164265,#28407);
#26320=LINE('',#164275,#28408);
#26321=LINE('',#164291,#28409);
#26322=LINE('',#164302,#28410);
#26323=LINE('',#164350,#28411);
#26324=LINE('',#164361,#28412);
#26325=LINE('',#164409,#28413);
#26326=LINE('',#164420,#28414);
#26327=LINE('',#164468,#28415);
#26328=LINE('',#164479,#28416);
#26329=LINE('',#164527,#28417);
#26330=LINE('',#164538,#28418);
#26331=LINE('',#164586,#28419);
#26332=LINE('',#164597,#28420);
#26333=LINE('',#164645,#28421);
#26334=LINE('',#164655,#28422);
#26335=LINE('',#164671,#28423);
#26336=LINE('',#165580,#28424);
#26337=LINE('',#165635,#28425);
#26338=LINE('',#165666,#28426);
#26339=LINE('',#165721,#28427);
#26340=LINE('',#165752,#28428);
#26341=LINE('',#165807,#28429);
#26342=LINE('',#165838,#28430);
#26343=LINE('',#165893,#28431);
#26344=LINE('',#165924,#28432);
#26345=LINE('',#165978,#28433);
#26346=LINE('',#166009,#28434);
#26347=LINE('',#166064,#28435);
#26348=LINE('',#166095,#28436);
#26349=LINE('',#166150,#28437);
#26350=LINE('',#166181,#28438);
#26351=LINE('',#166236,#28439);
#26352=LINE('',#166267,#28440);
#26353=LINE('',#166322,#28441);
#26354=LINE('',#166353,#28442);
#26355=LINE('',#166407,#28443);
#26356=LINE('',#166438,#28444);
#26357=LINE('',#166493,#28445);
#26358=LINE('',#166524,#28446);
#26359=LINE('',#166578,#28447);
#26360=LINE('',#166609,#28448);
#26361=LINE('',#166663,#28449);
#26362=LINE('',#166694,#28450);
#26363=LINE('',#166749,#28451);
#26364=LINE('',#166780,#28452);
#26365=LINE('',#166835,#28453);
#26366=LINE('',#166866,#28454);
#26367=LINE('',#166920,#28455);
#26368=LINE('',#166951,#28456);
#26369=LINE('',#167005,#28457);
#26370=LINE('',#167036,#28458);
#26371=LINE('',#167091,#28459);
#26372=LINE('',#167122,#28460);
#26373=LINE('',#167177,#28461);
#26374=LINE('',#167208,#28462);
#26375=LINE('',#167263,#28463);
#26376=LINE('',#167294,#28464);
#26377=LINE('',#167348,#28465);
#26378=LINE('',#167379,#28466);
#26379=LINE('',#167434,#28467);
#26380=LINE('',#167465,#28468);
#26381=LINE('',#167519,#28469);
#26382=LINE('',#167550,#28470);
#26383=LINE('',#167605,#28471);
#26384=LINE('',#167636,#28472);
#26385=LINE('',#167689,#28473);
#26386=LINE('',#167720,#28474);
#26387=LINE('',#167775,#28475);
#26388=LINE('',#167806,#28476);
#26389=LINE('',#167860,#28477);
#26390=LINE('',#167891,#28478);
#26391=LINE('',#167946,#28479);
#26392=LINE('',#167977,#28480);
#26393=LINE('',#168032,#28481);
#26394=LINE('',#168050,#28482);
#26395=LINE('',#168057,#28483);
#26396=LINE('',#168071,#28484);
#26397=LINE('',#168075,#28485);
#26398=LINE('',#168080,#28486);
#26399=LINE('',#168093,#28487);
#26400=LINE('',#168100,#28488);
#26401=LINE('',#168126,#28489);
#26402=LINE('',#168129,#28490);
#26403=LINE('',#168138,#28491);
#26404=LINE('',#168153,#28492);
#26405=LINE('',#168176,#28493);
#26406=LINE('',#168179,#28494);
#26407=LINE('',#168186,#28495);
#26408=LINE('',#168190,#28496);
#26409=LINE('',#168389,#28497);
#26410=LINE('',#168396,#28498);
#26411=LINE('',#168401,#28499);
#26412=LINE('',#168416,#28500);
#26413=LINE('',#168428,#28501);
#26414=LINE('',#168431,#28502);
#26415=LINE('',#168447,#28503);
#26416=LINE('',#168531,#28504);
#26417=LINE('',#168643,#28505);
#26418=LINE('',#168656,#28506);
#26419=LINE('',#168669,#28507);
#26420=LINE('',#168990,#28508);
#26421=LINE('',#168991,#28509);
#26422=LINE('',#169875,#28510);
#26423=LINE('',#169876,#28511);
#26424=LINE('',#169880,#28512);
#26425=LINE('',#169964,#28513);
#26426=LINE('',#169971,#28514);
#26427=LINE('',#169992,#28515);
#26428=LINE('',#170079,#28516);
#26429=LINE('',#170081,#28517);
#26430=LINE('',#170084,#28518);
#26431=LINE('',#170086,#28519);
#26432=LINE('',#170089,#28520);
#26433=LINE('',#170094,#28521);
#26434=LINE('',#170098,#28522);
#26435=LINE('',#170101,#28523);
#26436=LINE('',#170104,#28524);
#26437=LINE('',#170106,#28525);
#26438=LINE('',#170108,#28526);
#26439=LINE('',#170118,#28527);
#26440=LINE('',#170146,#28528);
#26441=LINE('',#170210,#28529);
#26442=LINE('',#170214,#28530);
#26443=LINE('',#170219,#28531);
#26444=LINE('',#170225,#28532);
#26445=VECTOR('',#77769,6.75);
#26446=VECTOR('',#77886,6.75);
#26447=VECTOR('',#77893,3.25);
#26448=VECTOR('',#77902,7.);
#26449=VECTOR('',#77909,6.125);
#26450=VECTOR('',#77916,6.125);
#26451=VECTOR('',#77981,6.75);
#26452=VECTOR('',#78216,1000.);
#26453=VECTOR('',#78223,1000.);
#26454=VECTOR('',#78230,1000.);
#26455=VECTOR('',#78237,1000.);
#26456=VECTOR('',#78244,1000.);
#26457=VECTOR('',#78251,1000.);
#26458=VECTOR('',#78258,1000.);
#26459=VECTOR('',#78265,1000.);
#26460=VECTOR('',#78272,1000.);
#26461=VECTOR('',#78279,1000.);
#26462=VECTOR('',#78286,1000.);
#26463=VECTOR('',#78293,1000.);
#26464=VECTOR('',#78300,1000.);
#26465=VECTOR('',#78305,1000.);
#26466=VECTOR('',#78306,1000.);
#26467=VECTOR('',#78313,1000.);
#26468=VECTOR('',#78320,1000.);
#26469=VECTOR('',#78327,1000.);
#26470=VECTOR('',#78334,1000.);
#26471=VECTOR('',#78341,1000.);
#26472=VECTOR('',#78348,1000.);
#26473=VECTOR('',#78355,1000.);
#26474=VECTOR('',#78362,1000.);
#26475=VECTOR('',#78369,1000.);
#26476=VECTOR('',#78376,1000.);
#26477=VECTOR('',#78383,1000.);
#26478=VECTOR('',#78390,1000.);
#26479=VECTOR('',#78397,1000.);
#26480=VECTOR('',#78404,1000.);
#26481=VECTOR('',#78411,1000.);
#26482=VECTOR('',#78418,1000.);
#26483=VECTOR('',#78425,1000.);
#26484=VECTOR('',#78432,1000.);
#26485=VECTOR('',#78439,1000.);
#26486=VECTOR('',#78446,1000.);
#26487=VECTOR('',#78453,1000.);
#26488=VECTOR('',#78460,1000.);
#26489=VECTOR('',#78467,1000.);
#26490=VECTOR('',#78474,1000.);
#26491=VECTOR('',#78481,1000.);
#26492=VECTOR('',#78488,1000.);
#26493=VECTOR('',#78495,1000.);
#26494=VECTOR('',#78502,1000.);
#26495=VECTOR('',#78509,1000.);
#26496=VECTOR('',#78516,1000.);
#26497=VECTOR('',#78523,1000.);
#26498=VECTOR('',#78530,1000.);
#26499=VECTOR('',#78537,1000.);
#26500=VECTOR('',#78544,1000.);
#26501=VECTOR('',#78551,1000.);
#26502=VECTOR('',#78554,1000.);
#26503=VECTOR('',#78565,1000.);
#26504=VECTOR('',#78574,1000.);
#26505=VECTOR('',#78579,1000.);
#26506=VECTOR('',#78586,1000.);
#26507=VECTOR('',#78593,1000.);
#26508=VECTOR('',#78600,1000.);
#26509=VECTOR('',#78611,1000.);
#26510=VECTOR('',#78614,1000.);
#26511=VECTOR('',#78615,1000.);
#26512=VECTOR('',#78620,1000.);
#26513=VECTOR('',#78627,1000.);
#26514=VECTOR('',#78632,1000.);
#26515=VECTOR('',#78639,1000.);
#26516=VECTOR('',#78644,1000.);
#26517=VECTOR('',#78651,1000.);
#26518=VECTOR('',#78656,1000.);
#26519=VECTOR('',#78663,1000.);
#26520=VECTOR('',#78668,1000.);
#26521=VECTOR('',#78675,1000.);
#26522=VECTOR('',#78680,1000.);
#26523=VECTOR('',#78687,1000.);
#26524=VECTOR('',#78692,1000.);
#26525=VECTOR('',#78699,1000.);
#26526=VECTOR('',#78704,1000.);
#26527=VECTOR('',#78711,1000.);
#26528=VECTOR('',#78716,1000.);
#26529=VECTOR('',#78723,1000.);
#26530=VECTOR('',#78728,1000.);
#26531=VECTOR('',#78735,1000.);
#26532=VECTOR('',#78740,1000.);
#26533=VECTOR('',#78747,1000.);
#26534=VECTOR('',#78752,1000.);
#26535=VECTOR('',#78759,1000.);
#26536=VECTOR('',#78764,1000.);
#26537=VECTOR('',#78771,1000.);
#26538=VECTOR('',#78772,1000.);
#26539=VECTOR('',#78773,1000.);
#26540=VECTOR('',#78778,1000.);
#26541=VECTOR('',#78785,1000.);
#26542=VECTOR('',#78790,1000.);
#26543=VECTOR('',#78797,1000.);
#26544=VECTOR('',#78802,1000.);
#26545=VECTOR('',#78809,1000.);
#26546=VECTOR('',#78814,1000.);
#26547=VECTOR('',#78821,1000.);
#26548=VECTOR('',#78826,1000.);
#26549=VECTOR('',#78833,1000.);
#26550=VECTOR('',#78838,1000.);
#26551=VECTOR('',#78845,1000.);
#26552=VECTOR('',#78850,1000.);
#26553=VECTOR('',#78857,1000.);
#26554=VECTOR('',#78862,1000.);
#26555=VECTOR('',#78869,1000.);
#26556=VECTOR('',#78874,1000.);
#26557=VECTOR('',#78881,1000.);
#26558=VECTOR('',#78886,1000.);
#26559=VECTOR('',#78893,1000.);
#26560=VECTOR('',#78898,1000.);
#26561=VECTOR('',#78905,1000.);
#26562=VECTOR('',#78910,1000.);
#26563=VECTOR('',#78917,1000.);
#26564=VECTOR('',#78922,1000.);
#26565=VECTOR('',#78929,1000.);
#26566=VECTOR('',#78934,1000.);
#26567=VECTOR('',#78949,1000.);
#26568=VECTOR('',#79126,1000.);
#26569=VECTOR('',#79131,1000.);
#26570=VECTOR('',#79134,1000.);
#26571=VECTOR('',#79139,1000.);
#26572=VECTOR('',#79142,1000.);
#26573=VECTOR('',#79147,1000.);
#26574=VECTOR('',#79150,1000.);
#26575=VECTOR('',#79155,1000.);
#26576=VECTOR('',#79158,1000.);
#26577=VECTOR('',#79163,1000.);
#26578=VECTOR('',#79166,1000.);
#26579=VECTOR('',#79171,1000.);
#26580=VECTOR('',#79174,1000.);
#26581=VECTOR('',#79179,1000.);
#26582=VECTOR('',#79182,1000.);
#26583=VECTOR('',#79187,1000.);
#26584=VECTOR('',#79190,1000.);
#26585=VECTOR('',#79195,1000.);
#26586=VECTOR('',#79198,1000.);
#26587=VECTOR('',#79203,1000.);
#26588=VECTOR('',#79206,1000.);
#26589=VECTOR('',#79211,1000.);
#26590=VECTOR('',#79214,1000.);
#26591=VECTOR('',#79219,1000.);
#26592=VECTOR('',#79222,1000.);
#26593=VECTOR('',#79227,1000.);
#26594=VECTOR('',#79230,1000.);
#26595=VECTOR('',#79235,1000.);
#26596=VECTOR('',#79236,1000.);
#26597=VECTOR('',#79237,1000.);
#26598=VECTOR('',#79240,1000.);
#26599=VECTOR('',#79245,1000.);
#26600=VECTOR('',#79248,1000.);
#26601=VECTOR('',#79253,1000.);
#26602=VECTOR('',#79256,1000.);
#26603=VECTOR('',#79261,1000.);
#26604=VECTOR('',#79264,1000.);
#26605=VECTOR('',#79269,1000.);
#26606=VECTOR('',#79272,1000.);
#26607=VECTOR('',#79277,1000.);
#26608=VECTOR('',#79280,1000.);
#26609=VECTOR('',#79285,1000.);
#26610=VECTOR('',#79288,1000.);
#26611=VECTOR('',#79293,1000.);
#26612=VECTOR('',#79296,1000.);
#26613=VECTOR('',#79301,1000.);
#26614=VECTOR('',#79304,1000.);
#26615=VECTOR('',#79309,1000.);
#26616=VECTOR('',#79312,1000.);
#26617=VECTOR('',#79313,1000.);
#26618=VECTOR('',#79318,1000.);
#26619=VECTOR('',#79325,1000.);
#26620=VECTOR('',#79328,1000.);
#26621=VECTOR('',#79333,1000.);
#26622=VECTOR('',#79336,1000.);
#26623=VECTOR('',#79341,1000.);
#26624=VECTOR('',#79344,1000.);
#26625=VECTOR('',#79349,1000.);
#26626=VECTOR('',#79350,1000.);
#26627=VECTOR('',#79355,1000.);
#26628=VECTOR('',#79360,1000.);
#26629=VECTOR('',#79365,1000.);
#26630=VECTOR('',#79370,1000.);
#26631=VECTOR('',#79375,1000.);
#26632=VECTOR('',#79380,1000.);
#26633=VECTOR('',#79385,1000.);
#26634=VECTOR('',#79390,1000.);
#26635=VECTOR('',#79395,1000.);
#26636=VECTOR('',#79400,1000.);
#26637=VECTOR('',#79405,1000.);
#26638=VECTOR('',#79410,1000.);
#26639=VECTOR('',#79415,1000.);
#26640=VECTOR('',#79420,1000.);
#26641=VECTOR('',#79425,1000.);
#26642=VECTOR('',#79430,1000.);
#26643=VECTOR('',#79435,1000.);
#26644=VECTOR('',#79440,1000.);
#26645=VECTOR('',#79445,1000.);
#26646=VECTOR('',#79450,1000.);
#26647=VECTOR('',#79455,1000.);
#26648=VECTOR('',#79460,1000.);
#26649=VECTOR('',#79465,1000.);
#26650=VECTOR('',#79470,1000.);
#26651=VECTOR('',#79475,1000.);
#26652=VECTOR('',#79480,1000.);
#26653=VECTOR('',#79485,1000.);
#26654=VECTOR('',#79490,1000.);
#26655=VECTOR('',#79495,1000.);
#26656=VECTOR('',#79500,1000.);
#26657=VECTOR('',#79505,1000.);
#26658=VECTOR('',#79510,1000.);
#26659=VECTOR('',#79515,1000.);
#26660=VECTOR('',#79520,1000.);
#26661=VECTOR('',#79525,1000.);
#26662=VECTOR('',#79530,1000.);
#26663=VECTOR('',#79535,1000.);
#26664=VECTOR('',#79540,1000.);
#26665=VECTOR('',#79545,1000.);
#26666=VECTOR('',#79550,1000.);
#26667=VECTOR('',#79555,1000.);
#26668=VECTOR('',#79560,1000.);
#26669=VECTOR('',#79561,1000.);
#26670=VECTOR('',#79562,1000.);
#26671=VECTOR('',#79567,1000.);
#26672=VECTOR('',#79572,1000.);
#26673=VECTOR('',#79577,1000.);
#26674=VECTOR('',#79582,1000.);
#26675=VECTOR('',#79587,1000.);
#26676=VECTOR('',#79592,1000.);
#26677=VECTOR('',#79597,1000.);
#26678=VECTOR('',#79602,1000.);
#26679=VECTOR('',#79607,1000.);
#26680=VECTOR('',#79612,1000.);
#26681=VECTOR('',#79617,1000.);
#26682=VECTOR('',#79622,1000.);
#26683=VECTOR('',#79627,1000.);
#26684=VECTOR('',#79750,1000.);
#26685=VECTOR('',#79751,1000.);
#26686=VECTOR('',#79760,1000.);
#26687=VECTOR('',#79761,1000.);
#26688=VECTOR('',#79770,1000.);
#26689=VECTOR('',#79771,1000.);
#26690=VECTOR('',#79780,1000.);
#26691=VECTOR('',#79781,1000.);
#26692=VECTOR('',#79790,1000.);
#26693=VECTOR('',#79791,1000.);
#26694=VECTOR('',#79800,1000.);
#26695=VECTOR('',#79801,1000.);
#26696=VECTOR('',#79810,1000.);
#26697=VECTOR('',#79811,1000.);
#26698=VECTOR('',#79812,1000.);
#26699=VECTOR('',#79813,1000.);
#26700=VECTOR('',#79822,1000.);
#26701=VECTOR('',#79823,1000.);
#26702=VECTOR('',#79832,1000.);
#26703=VECTOR('',#79833,1000.);
#26704=VECTOR('',#79842,1000.);
#26705=VECTOR('',#79843,1000.);
#26706=VECTOR('',#79852,1000.);
#26707=VECTOR('',#79853,1000.);
#26708=VECTOR('',#79862,1000.);
#26709=VECTOR('',#79863,1000.);
#26710=VECTOR('',#79872,1000.);
#26711=VECTOR('',#79873,1000.);
#26712=VECTOR('',#79882,1000.);
#26713=VECTOR('',#79883,1000.);
#26714=VECTOR('',#79892,1000.);
#26715=VECTOR('',#79893,1000.);
#26716=VECTOR('',#79902,1000.);
#26717=VECTOR('',#79903,1000.);
#26718=VECTOR('',#79912,1000.);
#26719=VECTOR('',#79913,1000.);
#26720=VECTOR('',#79922,1000.);
#26721=VECTOR('',#79923,1000.);
#26722=VECTOR('',#79932,1000.);
#26723=VECTOR('',#79933,1000.);
#26724=VECTOR('',#79942,1000.);
#26725=VECTOR('',#79943,1000.);
#26726=VECTOR('',#79952,1000.);
#26727=VECTOR('',#79953,1000.);
#26728=VECTOR('',#79962,1000.);
#26729=VECTOR('',#79963,1000.);
#26730=VECTOR('',#79972,1000.);
#26731=VECTOR('',#79973,1000.);
#26732=VECTOR('',#79976,1000.);
#26733=VECTOR('',#79983,1000.);
#26734=VECTOR('',#79992,1000.);
#26735=VECTOR('',#79993,1000.);
#26736=VECTOR('',#80002,1000.);
#26737=VECTOR('',#80003,1000.);
#26738=VECTOR('',#80012,1000.);
#26739=VECTOR('',#80013,1000.);
#26740=VECTOR('',#80022,1000.);
#26741=VECTOR('',#80029,1000.);
#26742=VECTOR('',#80032,1000.);
#26743=VECTOR('',#80033,1000.);
#26744=VECTOR('',#80036,1000.);
#26745=VECTOR('',#80043,1000.);
#26746=VECTOR('',#80046,1000.);
#26747=VECTOR('',#80053,1000.);
#26748=VECTOR('',#80056,1000.);
#26749=VECTOR('',#80063,1000.);
#26750=VECTOR('',#80066,1000.);
#26751=VECTOR('',#80073,1000.);
#26752=VECTOR('',#80076,1000.);
#26753=VECTOR('',#80083,1000.);
#26754=VECTOR('',#80086,1000.);
#26755=VECTOR('',#80093,1000.);
#26756=VECTOR('',#80096,1000.);
#26757=VECTOR('',#80103,1000.);
#26758=VECTOR('',#80106,1000.);
#26759=VECTOR('',#80113,1000.);
#26760=VECTOR('',#80116,1000.);
#26761=VECTOR('',#80123,1000.);
#26762=VECTOR('',#80126,1000.);
#26763=VECTOR('',#80133,1000.);
#26764=VECTOR('',#80136,1000.);
#26765=VECTOR('',#80143,1000.);
#26766=VECTOR('',#80146,1000.);
#26767=VECTOR('',#80153,1000.);
#26768=VECTOR('',#80156,1000.);
#26769=VECTOR('',#80163,1000.);
#26770=VECTOR('',#80164,1000.);
#26771=VECTOR('',#80165,1000.);
#26772=VECTOR('',#80168,1000.);
#26773=VECTOR('',#80175,1000.);
#26774=VECTOR('',#80178,1000.);
#26775=VECTOR('',#80185,1000.);
#26776=VECTOR('',#80188,1000.);
#26777=VECTOR('',#80195,1000.);
#26778=VECTOR('',#80198,1000.);
#26779=VECTOR('',#80205,1000.);
#26780=VECTOR('',#80208,1000.);
#26781=VECTOR('',#80215,1000.);
#26782=VECTOR('',#80218,1000.);
#26783=VECTOR('',#80225,1000.);
#26784=VECTOR('',#80228,1000.);
#26785=VECTOR('',#80235,1000.);
#26786=VECTOR('',#80238,1000.);
#26787=VECTOR('',#80245,1000.);
#26788=VECTOR('',#80248,1000.);
#26789=VECTOR('',#80255,1000.);
#26790=VECTOR('',#80258,1000.);
#26791=VECTOR('',#80265,1000.);
#26792=VECTOR('',#80268,1000.);
#26793=VECTOR('',#80275,1000.);
#26794=VECTOR('',#80278,1000.);
#26795=VECTOR('',#80285,1000.);
#26796=VECTOR('',#80288,1000.);
#26797=VECTOR('',#80295,1000.);
#26798=VECTOR('',#80298,1000.);
#26799=VECTOR('',#80311,1000.);
#26800=VECTOR('',#80488,1000.);
#26801=VECTOR('',#80497,1000.);
#26802=VECTOR('',#80500,1000.);
#26803=VECTOR('',#80509,1000.);
#26804=VECTOR('',#80512,1000.);
#26805=VECTOR('',#80521,1000.);
#26806=VECTOR('',#80524,1000.);
#26807=VECTOR('',#80533,1000.);
#26808=VECTOR('',#80536,1000.);
#26809=VECTOR('',#80545,1000.);
#26810=VECTOR('',#80548,1000.);
#26811=VECTOR('',#80557,1000.);
#26812=VECTOR('',#80560,1000.);
#26813=VECTOR('',#80569,1000.);
#26814=VECTOR('',#80572,1000.);
#26815=VECTOR('',#80581,1000.);
#26816=VECTOR('',#80584,1000.);
#26817=VECTOR('',#80593,1000.);
#26818=VECTOR('',#80596,1000.);
#26819=VECTOR('',#80605,1000.);
#26820=VECTOR('',#80608,1000.);
#26821=VECTOR('',#80617,1000.);
#26822=VECTOR('',#80620,1000.);
#26823=VECTOR('',#80629,1000.);
#26824=VECTOR('',#80632,1000.);
#26825=VECTOR('',#80641,1000.);
#26826=VECTOR('',#80644,1000.);
#26827=VECTOR('',#80653,1000.);
#26828=VECTOR('',#80654,1000.);
#26829=VECTOR('',#80655,1000.);
#26830=VECTOR('',#80658,1000.);
#26831=VECTOR('',#80667,1000.);
#26832=VECTOR('',#80670,1000.);
#26833=VECTOR('',#80679,1000.);
#26834=VECTOR('',#80682,1000.);
#26835=VECTOR('',#80691,1000.);
#26836=VECTOR('',#80694,1000.);
#26837=VECTOR('',#80703,1000.);
#26838=VECTOR('',#80706,1000.);
#26839=VECTOR('',#80715,1000.);
#26840=VECTOR('',#80718,1000.);
#26841=VECTOR('',#80727,1000.);
#26842=VECTOR('',#80730,1000.);
#26843=VECTOR('',#80739,1000.);
#26844=VECTOR('',#80742,1000.);
#26845=VECTOR('',#80751,1000.);
#26846=VECTOR('',#80754,1000.);
#26847=VECTOR('',#80757,1000.);
#26848=VECTOR('',#80764,1000.);
#26849=VECTOR('',#80775,1000.);
#26850=VECTOR('',#80778,1000.);
#26851=VECTOR('',#80787,1000.);
#26852=VECTOR('',#80790,1000.);
#26853=VECTOR('',#80799,1000.);
#26854=VECTOR('',#80802,1000.);
#26855=VECTOR('',#80811,1000.);
#26856=VECTOR('',#80814,1000.);
#26857=VECTOR('',#80823,1000.);
#26858=VECTOR('',#80824,1000.);
#26859=VECTOR('',#80827,1000.);
#26860=VECTOR('',#80834,1000.);
#26861=VECTOR('',#80837,1000.);
#26862=VECTOR('',#80844,1000.);
#26863=VECTOR('',#80847,1000.);
#26864=VECTOR('',#80854,1000.);
#26865=VECTOR('',#80857,1000.);
#26866=VECTOR('',#80864,1000.);
#26867=VECTOR('',#80867,1000.);
#26868=VECTOR('',#80874,1000.);
#26869=VECTOR('',#80877,1000.);
#26870=VECTOR('',#80884,1000.);
#26871=VECTOR('',#80887,1000.);
#26872=VECTOR('',#80894,1000.);
#26873=VECTOR('',#80897,1000.);
#26874=VECTOR('',#80904,1000.);
#26875=VECTOR('',#80907,1000.);
#26876=VECTOR('',#80914,1000.);
#26877=VECTOR('',#80917,1000.);
#26878=VECTOR('',#80924,1000.);
#26879=VECTOR('',#80927,1000.);
#26880=VECTOR('',#80934,1000.);
#26881=VECTOR('',#80937,1000.);
#26882=VECTOR('',#80944,1000.);
#26883=VECTOR('',#80947,1000.);
#26884=VECTOR('',#80954,1000.);
#26885=VECTOR('',#80957,1000.);
#26886=VECTOR('',#80964,1000.);
#26887=VECTOR('',#80967,1000.);
#26888=VECTOR('',#80974,1000.);
#26889=VECTOR('',#80977,1000.);
#26890=VECTOR('',#80984,1000.);
#26891=VECTOR('',#80987,1000.);
#26892=VECTOR('',#80994,1000.);
#26893=VECTOR('',#80997,1000.);
#26894=VECTOR('',#81004,1000.);
#26895=VECTOR('',#81007,1000.);
#26896=VECTOR('',#81014,1000.);
#26897=VECTOR('',#81017,1000.);
#26898=VECTOR('',#81024,1000.);
#26899=VECTOR('',#81027,1000.);
#26900=VECTOR('',#81034,1000.);
#26901=VECTOR('',#81037,1000.);
#26902=VECTOR('',#81044,1000.);
#26903=VECTOR('',#81047,1000.);
#26904=VECTOR('',#81054,1000.);
#26905=VECTOR('',#81057,1000.);
#26906=VECTOR('',#81064,1000.);
#26907=VECTOR('',#81067,1000.);
#26908=VECTOR('',#81074,1000.);
#26909=VECTOR('',#81077,1000.);
#26910=VECTOR('',#81084,1000.);
#26911=VECTOR('',#81087,1000.);
#26912=VECTOR('',#81094,1000.);
#26913=VECTOR('',#81097,1000.);
#26914=VECTOR('',#81104,1000.);
#26915=VECTOR('',#81107,1000.);
#26916=VECTOR('',#81348,1000.);
#26917=VECTOR('',#81351,1000.);
#26918=VECTOR('',#81358,1000.);
#26919=VECTOR('',#81361,1000.);
#26920=VECTOR('',#81368,1000.);
#26921=VECTOR('',#81371,1000.);
#26922=VECTOR('',#81378,1000.);
#26923=VECTOR('',#81381,1000.);
#26924=VECTOR('',#81388,1000.);
#26925=VECTOR('',#81391,1000.);
#26926=VECTOR('',#81398,1000.);
#26927=VECTOR('',#81401,1000.);
#26928=VECTOR('',#81408,1000.);
#26929=VECTOR('',#81409,1000.);
#26930=VECTOR('',#81410,1000.);
#26931=VECTOR('',#81413,1000.);
#26932=VECTOR('',#81420,1000.);
#26933=VECTOR('',#81423,1000.);
#26934=VECTOR('',#81430,1000.);
#26935=VECTOR('',#81433,1000.);
#26936=VECTOR('',#81440,1000.);
#26937=VECTOR('',#81443,1000.);
#26938=VECTOR('',#81450,1000.);
#26939=VECTOR('',#81453,1000.);
#26940=VECTOR('',#81460,1000.);
#26941=VECTOR('',#81463,1000.);
#26942=VECTOR('',#81470,1000.);
#26943=VECTOR('',#81473,1000.);
#26944=VECTOR('',#81480,1000.);
#26945=VECTOR('',#81483,1000.);
#26946=VECTOR('',#81490,1000.);
#26947=VECTOR('',#81493,1000.);
#26948=VECTOR('',#81500,1000.);
#26949=VECTOR('',#81503,1000.);
#26950=VECTOR('',#81510,1000.);
#26951=VECTOR('',#81513,1000.);
#26952=VECTOR('',#81520,1000.);
#26953=VECTOR('',#81523,1000.);
#26954=VECTOR('',#81530,1000.);
#26955=VECTOR('',#81533,1000.);
#26956=VECTOR('',#81540,1000.);
#26957=VECTOR('',#81543,1000.);
#26958=VECTOR('',#81550,1000.);
#26959=VECTOR('',#81553,1000.);
#26960=VECTOR('',#81560,1000.);
#26961=VECTOR('',#81563,1000.);
#26962=VECTOR('',#81566,1000.);
#26963=VECTOR('',#81571,1000.);
#26964=VECTOR('',#81580,1000.);
#26965=VECTOR('',#81583,1000.);
#26966=VECTOR('',#81590,1000.);
#26967=VECTOR('',#81593,1000.);
#26968=VECTOR('',#81600,1000.);
#26969=VECTOR('',#81603,1000.);
#26970=VECTOR('',#81610,1000.);
#26971=VECTOR('',#81613,1000.);
#26972=VECTOR('',#81620,1000.);
#26973=VECTOR('',#81627,1000.);
#26974=VECTOR('',#81630,1000.);
#26975=VECTOR('',#81631,1000.);
#26976=VECTOR('',#81636,1000.);
#26977=VECTOR('',#81643,1000.);
#26978=VECTOR('',#81648,1000.);
#26979=VECTOR('',#81655,1000.);
#26980=VECTOR('',#81660,1000.);
#26981=VECTOR('',#81667,1000.);
#26982=VECTOR('',#81672,1000.);
#26983=VECTOR('',#81679,1000.);
#26984=VECTOR('',#81684,1000.);
#26985=VECTOR('',#81691,1000.);
#26986=VECTOR('',#81696,1000.);
#26987=VECTOR('',#81703,1000.);
#26988=VECTOR('',#81708,1000.);
#26989=VECTOR('',#81715,1000.);
#26990=VECTOR('',#81720,1000.);
#26991=VECTOR('',#81727,1000.);
#26992=VECTOR('',#81732,1000.);
#26993=VECTOR('',#81739,1000.);
#26994=VECTOR('',#81744,1000.);
#26995=VECTOR('',#81751,1000.);
#26996=VECTOR('',#81756,1000.);
#26997=VECTOR('',#81763,1000.);
#26998=VECTOR('',#81768,1000.);
#26999=VECTOR('',#81775,1000.);
#27000=VECTOR('',#81780,1000.);
#27001=VECTOR('',#81787,1000.);
#27002=VECTOR('',#81788,1000.);
#27003=VECTOR('',#81789,1000.);
#27004=VECTOR('',#81794,1000.);
#27005=VECTOR('',#81801,1000.);
#27006=VECTOR('',#81806,1000.);
#27007=VECTOR('',#81813,1000.);
#27008=VECTOR('',#81818,1000.);
#27009=VECTOR('',#81825,1000.);
#27010=VECTOR('',#81830,1000.);
#27011=VECTOR('',#81837,1000.);
#27012=VECTOR('',#81842,1000.);
#27013=VECTOR('',#81849,1000.);
#27014=VECTOR('',#81854,1000.);
#27015=VECTOR('',#81861,1000.);
#27016=VECTOR('',#81866,1000.);
#27017=VECTOR('',#81873,1000.);
#27018=VECTOR('',#81878,1000.);
#27019=VECTOR('',#81885,1000.);
#27020=VECTOR('',#81890,1000.);
#27021=VECTOR('',#81897,1000.);
#27022=VECTOR('',#81902,1000.);
#27023=VECTOR('',#81909,1000.);
#27024=VECTOR('',#81914,1000.);
#27025=VECTOR('',#81921,1000.);
#27026=VECTOR('',#81926,1000.);
#27027=VECTOR('',#81933,1000.);
#27028=VECTOR('',#81938,1000.);
#27029=VECTOR('',#81945,1000.);
#27030=VECTOR('',#81950,1000.);
#27031=VECTOR('',#81965,1000.);
#27032=VECTOR('',#82142,1000.);
#27033=VECTOR('',#82149,1000.);
#27034=VECTOR('',#82152,1000.);
#27035=VECTOR('',#82159,1000.);
#27036=VECTOR('',#82162,1000.);
#27037=VECTOR('',#82169,1000.);
#27038=VECTOR('',#82172,1000.);
#27039=VECTOR('',#82179,1000.);
#27040=VECTOR('',#82182,1000.);
#27041=VECTOR('',#82189,1000.);
#27042=VECTOR('',#82192,1000.);
#27043=VECTOR('',#82199,1000.);
#27044=VECTOR('',#82202,1000.);
#27045=VECTOR('',#82209,1000.);
#27046=VECTOR('',#82212,1000.);
#27047=VECTOR('',#82219,1000.);
#27048=VECTOR('',#82222,1000.);
#27049=VECTOR('',#82229,1000.);
#27050=VECTOR('',#82232,1000.);
#27051=VECTOR('',#82239,1000.);
#27052=VECTOR('',#82242,1000.);
#27053=VECTOR('',#82249,1000.);
#27054=VECTOR('',#82252,1000.);
#27055=VECTOR('',#82259,1000.);
#27056=VECTOR('',#82262,1000.);
#27057=VECTOR('',#82269,1000.);
#27058=VECTOR('',#82272,1000.);
#27059=VECTOR('',#82279,1000.);
#27060=VECTOR('',#82280,1000.);
#27061=VECTOR('',#82281,1000.);
#27062=VECTOR('',#82284,1000.);
#27063=VECTOR('',#82291,1000.);
#27064=VECTOR('',#82294,1000.);
#27065=VECTOR('',#82301,1000.);
#27066=VECTOR('',#82304,1000.);
#27067=VECTOR('',#82311,1000.);
#27068=VECTOR('',#82314,1000.);
#27069=VECTOR('',#82321,1000.);
#27070=VECTOR('',#82324,1000.);
#27071=VECTOR('',#82331,1000.);
#27072=VECTOR('',#82334,1000.);
#27073=VECTOR('',#82341,1000.);
#27074=VECTOR('',#82344,1000.);
#27075=VECTOR('',#82351,1000.);
#27076=VECTOR('',#82354,1000.);
#27077=VECTOR('',#82355,1000.);
#27078=VECTOR('',#82362,1000.);
#27079=VECTOR('',#82371,1000.);
#27080=VECTOR('',#82374,1000.);
#27081=VECTOR('',#82381,1000.);
#27082=VECTOR('',#82384,1000.);
#27083=VECTOR('',#82391,1000.);
#27084=VECTOR('',#82394,1000.);
#27085=VECTOR('',#82401,1000.);
#27086=VECTOR('',#82404,1000.);
#27087=VECTOR('',#82411,1000.);
#27088=VECTOR('',#82414,1000.);
#27089=VECTOR('',#82421,1000.);
#27090=VECTOR('',#82422,1000.);
#27091=VECTOR('',#82427,1000.);
#27092=VECTOR('',#82434,1000.);
#27093=VECTOR('',#82439,1000.);
#27094=VECTOR('',#82446,1000.);
#27095=VECTOR('',#82451,1000.);
#27096=VECTOR('',#82458,1000.);
#27097=VECTOR('',#82463,1000.);
#27098=VECTOR('',#82470,1000.);
#27099=VECTOR('',#82475,1000.);
#27100=VECTOR('',#82482,1000.);
#27101=VECTOR('',#82487,1000.);
#27102=VECTOR('',#82494,1000.);
#27103=VECTOR('',#82499,1000.);
#27104=VECTOR('',#82506,1000.);
#27105=VECTOR('',#82511,1000.);
#27106=VECTOR('',#82518,1000.);
#27107=VECTOR('',#82523,1000.);
#27108=VECTOR('',#82530,1000.);
#27109=VECTOR('',#82535,1000.);
#27110=VECTOR('',#82542,1000.);
#27111=VECTOR('',#82547,1000.);
#27112=VECTOR('',#82554,1000.);
#27113=VECTOR('',#82559,1000.);
#27114=VECTOR('',#82566,1000.);
#27115=VECTOR('',#82571,1000.);
#27116=VECTOR('',#82578,1000.);
#27117=VECTOR('',#82583,1000.);
#27118=VECTOR('',#82590,1000.);
#27119=VECTOR('',#82595,1000.);
#27120=VECTOR('',#82602,1000.);
#27121=VECTOR('',#82607,1000.);
#27122=VECTOR('',#82614,1000.);
#27123=VECTOR('',#82619,1000.);
#27124=VECTOR('',#82626,1000.);
#27125=VECTOR('',#82631,1000.);
#27126=VECTOR('',#82638,1000.);
#27127=VECTOR('',#82643,1000.);
#27128=VECTOR('',#82650,1000.);
#27129=VECTOR('',#82655,1000.);
#27130=VECTOR('',#82662,1000.);
#27131=VECTOR('',#82667,1000.);
#27132=VECTOR('',#82674,1000.);
#27133=VECTOR('',#82675,1000.);
#27134=VECTOR('',#82676,1000.);
#27135=VECTOR('',#82681,1000.);
#27136=VECTOR('',#82688,1000.);
#27137=VECTOR('',#82693,1000.);
#27138=VECTOR('',#82700,1000.);
#27139=VECTOR('',#82705,1000.);
#27140=VECTOR('',#82712,1000.);
#27141=VECTOR('',#82717,1000.);
#27142=VECTOR('',#82724,1000.);
#27143=VECTOR('',#82729,1000.);
#27144=VECTOR('',#82736,1000.);
#27145=VECTOR('',#82741,1000.);
#27146=VECTOR('',#82748,1000.);
#27147=VECTOR('',#82753,1000.);
#27148=VECTOR('',#82878,1000.);
#27149=VECTOR('',#82879,1000.);
#27150=VECTOR('',#82888,1000.);
#27151=VECTOR('',#82889,1000.);
#27152=VECTOR('',#82898,1000.);
#27153=VECTOR('',#82899,1000.);
#27154=VECTOR('',#82908,1000.);
#27155=VECTOR('',#82909,1000.);
#27156=VECTOR('',#82918,1000.);
#27157=VECTOR('',#82919,1000.);
#27158=VECTOR('',#82928,1000.);
#27159=VECTOR('',#82929,1000.);
#27160=VECTOR('',#82938,1000.);
#27161=VECTOR('',#82939,1000.);
#27162=VECTOR('',#82940,1000.);
#27163=VECTOR('',#82941,1000.);
#27164=VECTOR('',#82950,1000.);
#27165=VECTOR('',#82951,1000.);
#27166=VECTOR('',#82960,1000.);
#27167=VECTOR('',#82961,1000.);
#27168=VECTOR('',#82970,1000.);
#27169=VECTOR('',#82971,1000.);
#27170=VECTOR('',#82980,1000.);
#27171=VECTOR('',#82981,1000.);
#27172=VECTOR('',#82990,1000.);
#27173=VECTOR('',#82991,1000.);
#27174=VECTOR('',#83000,1000.);
#27175=VECTOR('',#83001,1000.);
#27176=VECTOR('',#83010,1000.);
#27177=VECTOR('',#83011,1000.);
#27178=VECTOR('',#83020,1000.);
#27179=VECTOR('',#83021,1000.);
#27180=VECTOR('',#83030,1000.);
#27181=VECTOR('',#83031,1000.);
#27182=VECTOR('',#83040,1000.);
#27183=VECTOR('',#83041,1000.);
#27184=VECTOR('',#83050,1000.);
#27185=VECTOR('',#83051,1000.);
#27186=VECTOR('',#83060,1000.);
#27187=VECTOR('',#83061,1000.);
#27188=VECTOR('',#83070,1000.);
#27189=VECTOR('',#83071,1000.);
#27190=VECTOR('',#83080,1000.);
#27191=VECTOR('',#83081,1000.);
#27192=VECTOR('',#83084,1000.);
#27193=VECTOR('',#83091,1000.);
#27194=VECTOR('',#83100,1000.);
#27195=VECTOR('',#83101,1000.);
#27196=VECTOR('',#83110,1000.);
#27197=VECTOR('',#83111,1000.);
#27198=VECTOR('',#83120,1000.);
#27199=VECTOR('',#83121,1000.);
#27200=VECTOR('',#83130,1000.);
#27201=VECTOR('',#83131,1000.);
#27202=VECTOR('',#83140,1000.);
#27203=VECTOR('',#83141,1000.);
#27204=VECTOR('',#83150,1000.);
#27205=VECTOR('',#83157,1000.);
#27206=VECTOR('',#83160,1000.);
#27207=VECTOR('',#83161,1000.);
#27208=VECTOR('',#83164,1000.);
#27209=VECTOR('',#83171,1000.);
#27210=VECTOR('',#83174,1000.);
#27211=VECTOR('',#83181,1000.);
#27212=VECTOR('',#83184,1000.);
#27213=VECTOR('',#83191,1000.);
#27214=VECTOR('',#83194,1000.);
#27215=VECTOR('',#83201,1000.);
#27216=VECTOR('',#83204,1000.);
#27217=VECTOR('',#83211,1000.);
#27218=VECTOR('',#83214,1000.);
#27219=VECTOR('',#83221,1000.);
#27220=VECTOR('',#83224,1000.);
#27221=VECTOR('',#83231,1000.);
#27222=VECTOR('',#83234,1000.);
#27223=VECTOR('',#83241,1000.);
#27224=VECTOR('',#83244,1000.);
#27225=VECTOR('',#83251,1000.);
#27226=VECTOR('',#83254,1000.);
#27227=VECTOR('',#83261,1000.);
#27228=VECTOR('',#83264,1000.);
#27229=VECTOR('',#83271,1000.);
#27230=VECTOR('',#83274,1000.);
#27231=VECTOR('',#83281,1000.);
#27232=VECTOR('',#83284,1000.);
#27233=VECTOR('',#83291,1000.);
#27234=VECTOR('',#83292,1000.);
#27235=VECTOR('',#83293,1000.);
#27236=VECTOR('',#83296,1000.);
#27237=VECTOR('',#83303,1000.);
#27238=VECTOR('',#83306,1000.);
#27239=VECTOR('',#83313,1000.);
#27240=VECTOR('',#83316,1000.);
#27241=VECTOR('',#83323,1000.);
#27242=VECTOR('',#83326,1000.);
#27243=VECTOR('',#83333,1000.);
#27244=VECTOR('',#83336,1000.);
#27245=VECTOR('',#83343,1000.);
#27246=VECTOR('',#83346,1000.);
#27247=VECTOR('',#83353,1000.);
#27248=VECTOR('',#83356,1000.);
#27249=VECTOR('',#83363,1000.);
#27250=VECTOR('',#83366,1000.);
#27251=VECTOR('',#83373,1000.);
#27252=VECTOR('',#83376,1000.);
#27253=VECTOR('',#83383,1000.);
#27254=VECTOR('',#83386,1000.);
#27255=VECTOR('',#83393,1000.);
#27256=VECTOR('',#83396,1000.);
#27257=VECTOR('',#83403,1000.);
#27258=VECTOR('',#83406,1000.);
#27259=VECTOR('',#83413,1000.);
#27260=VECTOR('',#83416,1000.);
#27261=VECTOR('',#83423,1000.);
#27262=VECTOR('',#83426,1000.);
#27263=VECTOR('',#83439,1000.);
#27264=VECTOR('',#83616,1000.);
#27265=VECTOR('',#83625,1000.);
#27266=VECTOR('',#83628,1000.);
#27267=VECTOR('',#83637,1000.);
#27268=VECTOR('',#83640,1000.);
#27269=VECTOR('',#83649,1000.);
#27270=VECTOR('',#83652,1000.);
#27271=VECTOR('',#83661,1000.);
#27272=VECTOR('',#83664,1000.);
#27273=VECTOR('',#83673,1000.);
#27274=VECTOR('',#83676,1000.);
#27275=VECTOR('',#83685,1000.);
#27276=VECTOR('',#83688,1000.);
#27277=VECTOR('',#83697,1000.);
#27278=VECTOR('',#83700,1000.);
#27279=VECTOR('',#83709,1000.);
#27280=VECTOR('',#83712,1000.);
#27281=VECTOR('',#83721,1000.);
#27282=VECTOR('',#83724,1000.);
#27283=VECTOR('',#83733,1000.);
#27284=VECTOR('',#83736,1000.);
#27285=VECTOR('',#83745,1000.);
#27286=VECTOR('',#83748,1000.);
#27287=VECTOR('',#83757,1000.);
#27288=VECTOR('',#83760,1000.);
#27289=VECTOR('',#83769,1000.);
#27290=VECTOR('',#83772,1000.);
#27291=VECTOR('',#83781,1000.);
#27292=VECTOR('',#83782,1000.);
#27293=VECTOR('',#83783,1000.);
#27294=VECTOR('',#83786,1000.);
#27295=VECTOR('',#83795,1000.);
#27296=VECTOR('',#83798,1000.);
#27297=VECTOR('',#83807,1000.);
#27298=VECTOR('',#83810,1000.);
#27299=VECTOR('',#83819,1000.);
#27300=VECTOR('',#83822,1000.);
#27301=VECTOR('',#83831,1000.);
#27302=VECTOR('',#83834,1000.);
#27303=VECTOR('',#83843,1000.);
#27304=VECTOR('',#83846,1000.);
#27305=VECTOR('',#83855,1000.);
#27306=VECTOR('',#83858,1000.);
#27307=VECTOR('',#83861,1000.);
#27308=VECTOR('',#83868,1000.);
#27309=VECTOR('',#83879,1000.);
#27310=VECTOR('',#83882,1000.);
#27311=VECTOR('',#83891,1000.);
#27312=VECTOR('',#83894,1000.);
#27313=VECTOR('',#83903,1000.);
#27314=VECTOR('',#83906,1000.);
#27315=VECTOR('',#83915,1000.);
#27316=VECTOR('',#83918,1000.);
#27317=VECTOR('',#83927,1000.);
#27318=VECTOR('',#83930,1000.);
#27319=VECTOR('',#83939,1000.);
#27320=VECTOR('',#83942,1000.);
#27321=VECTOR('',#83951,1000.);
#27322=VECTOR('',#83952,1000.);
#27323=VECTOR('',#83955,1000.);
#27324=VECTOR('',#83962,1000.);
#27325=VECTOR('',#83965,1000.);
#27326=VECTOR('',#83972,1000.);
#27327=VECTOR('',#83975,1000.);
#27328=VECTOR('',#83982,1000.);
#27329=VECTOR('',#83985,1000.);
#27330=VECTOR('',#83992,1000.);
#27331=VECTOR('',#83995,1000.);
#27332=VECTOR('',#84002,1000.);
#27333=VECTOR('',#84005,1000.);
#27334=VECTOR('',#84012,1000.);
#27335=VECTOR('',#84015,1000.);
#27336=VECTOR('',#84022,1000.);
#27337=VECTOR('',#84025,1000.);
#27338=VECTOR('',#84032,1000.);
#27339=VECTOR('',#84035,1000.);
#27340=VECTOR('',#84042,1000.);
#27341=VECTOR('',#84045,1000.);
#27342=VECTOR('',#84052,1000.);
#27343=VECTOR('',#84055,1000.);
#27344=VECTOR('',#84062,1000.);
#27345=VECTOR('',#84065,1000.);
#27346=VECTOR('',#84072,1000.);
#27347=VECTOR('',#84075,1000.);
#27348=VECTOR('',#84082,1000.);
#27349=VECTOR('',#84085,1000.);
#27350=VECTOR('',#84092,1000.);
#27351=VECTOR('',#84095,1000.);
#27352=VECTOR('',#84102,1000.);
#27353=VECTOR('',#84105,1000.);
#27354=VECTOR('',#84112,1000.);
#27355=VECTOR('',#84115,1000.);
#27356=VECTOR('',#84122,1000.);
#27357=VECTOR('',#84125,1000.);
#27358=VECTOR('',#84132,1000.);
#27359=VECTOR('',#84135,1000.);
#27360=VECTOR('',#84142,1000.);
#27361=VECTOR('',#84145,1000.);
#27362=VECTOR('',#84152,1000.);
#27363=VECTOR('',#84155,1000.);
#27364=VECTOR('',#84162,1000.);
#27365=VECTOR('',#84163,1000.);
#27366=VECTOR('',#84164,1000.);
#27367=VECTOR('',#84167,1000.);
#27368=VECTOR('',#84174,1000.);
#27369=VECTOR('',#84177,1000.);
#27370=VECTOR('',#84184,1000.);
#27371=VECTOR('',#84187,1000.);
#27372=VECTOR('',#84194,1000.);
#27373=VECTOR('',#84197,1000.);
#27374=VECTOR('',#84204,1000.);
#27375=VECTOR('',#84207,1000.);
#27376=VECTOR('',#84214,1000.);
#27377=VECTOR('',#84217,1000.);
#27378=VECTOR('',#84224,1000.);
#27379=VECTOR('',#84227,1000.);
#27380=VECTOR('',#84468,1000.);
#27381=VECTOR('',#84471,1000.);
#27382=VECTOR('',#84480,1000.);
#27383=VECTOR('',#84483,1000.);
#27384=VECTOR('',#84492,1000.);
#27385=VECTOR('',#84495,1000.);
#27386=VECTOR('',#84504,1000.);
#27387=VECTOR('',#84507,1000.);
#27388=VECTOR('',#84516,1000.);
#27389=VECTOR('',#84519,1000.);
#27390=VECTOR('',#84528,1000.);
#27391=VECTOR('',#84531,1000.);
#27392=VECTOR('',#84540,1000.);
#27393=VECTOR('',#84541,1000.);
#27394=VECTOR('',#84542,1000.);
#27395=VECTOR('',#84545,1000.);
#27396=VECTOR('',#84554,1000.);
#27397=VECTOR('',#84557,1000.);
#27398=VECTOR('',#84566,1000.);
#27399=VECTOR('',#84569,1000.);
#27400=VECTOR('',#84578,1000.);
#27401=VECTOR('',#84581,1000.);
#27402=VECTOR('',#84590,1000.);
#27403=VECTOR('',#84593,1000.);
#27404=VECTOR('',#84602,1000.);
#27405=VECTOR('',#84605,1000.);
#27406=VECTOR('',#84614,1000.);
#27407=VECTOR('',#84617,1000.);
#27408=VECTOR('',#84626,1000.);
#27409=VECTOR('',#84629,1000.);
#27410=VECTOR('',#84638,1000.);
#27411=VECTOR('',#84641,1000.);
#27412=VECTOR('',#84650,1000.);
#27413=VECTOR('',#84653,1000.);
#27414=VECTOR('',#84662,1000.);
#27415=VECTOR('',#84665,1000.);
#27416=VECTOR('',#84674,1000.);
#27417=VECTOR('',#84677,1000.);
#27418=VECTOR('',#84686,1000.);
#27419=VECTOR('',#84689,1000.);
#27420=VECTOR('',#84698,1000.);
#27421=VECTOR('',#84701,1000.);
#27422=VECTOR('',#84704,1000.);
#27423=VECTOR('',#84711,1000.);
#27424=VECTOR('',#84722,1000.);
#27425=VECTOR('',#84725,1000.);
#27426=VECTOR('',#84734,1000.);
#27427=VECTOR('',#84737,1000.);
#27428=VECTOR('',#84746,1000.);
#27429=VECTOR('',#84749,1000.);
#27430=VECTOR('',#84758,1000.);
#27431=VECTOR('',#84761,1000.);
#27432=VECTOR('',#84770,1000.);
#27433=VECTOR('',#84773,1000.);
#27434=VECTOR('',#84782,1000.);
#27435=VECTOR('',#84785,1000.);
#27436=VECTOR('',#84794,1000.);
#27437=VECTOR('',#84803,1000.);
#27438=VECTOR('',#84806,1000.);
#27439=VECTOR('',#84807,1000.);
#27440=VECTOR('',#84812,1000.);
#27441=VECTOR('',#84819,1000.);
#27442=VECTOR('',#84824,1000.);
#27443=VECTOR('',#84831,1000.);
#27444=VECTOR('',#84836,1000.);
#27445=VECTOR('',#84843,1000.);
#27446=VECTOR('',#84848,1000.);
#27447=VECTOR('',#84855,1000.);
#27448=VECTOR('',#84860,1000.);
#27449=VECTOR('',#84867,1000.);
#27450=VECTOR('',#84872,1000.);
#27451=VECTOR('',#84879,1000.);
#27452=VECTOR('',#84884,1000.);
#27453=VECTOR('',#84891,1000.);
#27454=VECTOR('',#84896,1000.);
#27455=VECTOR('',#84903,1000.);
#27456=VECTOR('',#84908,1000.);
#27457=VECTOR('',#84915,1000.);
#27458=VECTOR('',#84920,1000.);
#27459=VECTOR('',#84927,1000.);
#27460=VECTOR('',#84932,1000.);
#27461=VECTOR('',#84939,1000.);
#27462=VECTOR('',#84944,1000.);
#27463=VECTOR('',#84951,1000.);
#27464=VECTOR('',#84956,1000.);
#27465=VECTOR('',#84963,1000.);
#27466=VECTOR('',#84964,1000.);
#27467=VECTOR('',#84965,1000.);
#27468=VECTOR('',#84970,1000.);
#27469=VECTOR('',#84977,1000.);
#27470=VECTOR('',#84982,1000.);
#27471=VECTOR('',#84989,1000.);
#27472=VECTOR('',#84994,1000.);
#27473=VECTOR('',#85001,1000.);
#27474=VECTOR('',#85006,1000.);
#27475=VECTOR('',#85013,1000.);
#27476=VECTOR('',#85018,1000.);
#27477=VECTOR('',#85025,1000.);
#27478=VECTOR('',#85030,1000.);
#27479=VECTOR('',#85037,1000.);
#27480=VECTOR('',#85042,1000.);
#27481=VECTOR('',#85049,1000.);
#27482=VECTOR('',#85054,1000.);
#27483=VECTOR('',#85061,1000.);
#27484=VECTOR('',#85066,1000.);
#27485=VECTOR('',#85073,1000.);
#27486=VECTOR('',#85078,1000.);
#27487=VECTOR('',#85085,1000.);
#27488=VECTOR('',#85090,1000.);
#27489=VECTOR('',#85097,1000.);
#27490=VECTOR('',#85102,1000.);
#27491=VECTOR('',#85109,1000.);
#27492=VECTOR('',#85114,1000.);
#27493=VECTOR('',#85121,1000.);
#27494=VECTOR('',#85126,1000.);
#27495=VECTOR('',#85141,1000.);
#27496=VECTOR('',#85318,1000.);
#27497=VECTOR('',#85325,1000.);
#27498=VECTOR('',#85328,1000.);
#27499=VECTOR('',#85335,1000.);
#27500=VECTOR('',#85338,1000.);
#27501=VECTOR('',#85345,1000.);
#27502=VECTOR('',#85348,1000.);
#27503=VECTOR('',#85355,1000.);
#27504=VECTOR('',#85358,1000.);
#27505=VECTOR('',#85365,1000.);
#27506=VECTOR('',#85368,1000.);
#27507=VECTOR('',#85375,1000.);
#27508=VECTOR('',#85378,1000.);
#27509=VECTOR('',#85385,1000.);
#27510=VECTOR('',#85388,1000.);
#27511=VECTOR('',#85395,1000.);
#27512=VECTOR('',#85398,1000.);
#27513=VECTOR('',#85405,1000.);
#27514=VECTOR('',#85408,1000.);
#27515=VECTOR('',#85415,1000.);
#27516=VECTOR('',#85418,1000.);
#27517=VECTOR('',#85425,1000.);
#27518=VECTOR('',#85428,1000.);
#27519=VECTOR('',#85435,1000.);
#27520=VECTOR('',#85438,1000.);
#27521=VECTOR('',#85445,1000.);
#27522=VECTOR('',#85448,1000.);
#27523=VECTOR('',#85455,1000.);
#27524=VECTOR('',#85456,1000.);
#27525=VECTOR('',#85457,1000.);
#27526=VECTOR('',#85460,1000.);
#27527=VECTOR('',#85467,1000.);
#27528=VECTOR('',#85470,1000.);
#27529=VECTOR('',#85477,1000.);
#27530=VECTOR('',#85480,1000.);
#27531=VECTOR('',#85487,1000.);
#27532=VECTOR('',#85490,1000.);
#27533=VECTOR('',#85497,1000.);
#27534=VECTOR('',#85500,1000.);
#27535=VECTOR('',#85507,1000.);
#27536=VECTOR('',#85510,1000.);
#27537=VECTOR('',#85511,1000.);
#27538=VECTOR('',#85518,1000.);
#27539=VECTOR('',#85527,1000.);
#27540=VECTOR('',#85530,1000.);
#27541=VECTOR('',#85537,1000.);
#27542=VECTOR('',#85540,1000.);
#27543=VECTOR('',#85547,1000.);
#27544=VECTOR('',#85550,1000.);
#27545=VECTOR('',#85557,1000.);
#27546=VECTOR('',#85560,1000.);
#27547=VECTOR('',#85567,1000.);
#27548=VECTOR('',#85570,1000.);
#27549=VECTOR('',#85577,1000.);
#27550=VECTOR('',#85580,1000.);
#27551=VECTOR('',#85587,1000.);
#27552=VECTOR('',#85590,1000.);
#27553=VECTOR('',#85597,1000.);
#27554=VECTOR('',#85598,1000.);
#27555=VECTOR('',#85603,1000.);
#27556=VECTOR('',#85610,1000.);
#27557=VECTOR('',#85615,1000.);
#27558=VECTOR('',#85622,1000.);
#27559=VECTOR('',#85627,1000.);
#27560=VECTOR('',#85634,1000.);
#27561=VECTOR('',#85639,1000.);
#27562=VECTOR('',#85646,1000.);
#27563=VECTOR('',#85651,1000.);
#27564=VECTOR('',#85658,1000.);
#27565=VECTOR('',#85663,1000.);
#27566=VECTOR('',#85670,1000.);
#27567=VECTOR('',#85675,1000.);
#27568=VECTOR('',#85682,1000.);
#27569=VECTOR('',#85687,1000.);
#27570=VECTOR('',#85694,1000.);
#27571=VECTOR('',#85699,1000.);
#27572=VECTOR('',#85706,1000.);
#27573=VECTOR('',#85711,1000.);
#27574=VECTOR('',#85718,1000.);
#27575=VECTOR('',#85723,1000.);
#27576=VECTOR('',#85730,1000.);
#27577=VECTOR('',#85735,1000.);
#27578=VECTOR('',#85742,1000.);
#27579=VECTOR('',#85747,1000.);
#27580=VECTOR('',#85754,1000.);
#27581=VECTOR('',#85759,1000.);
#27582=VECTOR('',#85766,1000.);
#27583=VECTOR('',#85771,1000.);
#27584=VECTOR('',#85778,1000.);
#27585=VECTOR('',#85783,1000.);
#27586=VECTOR('',#85790,1000.);
#27587=VECTOR('',#85795,1000.);
#27588=VECTOR('',#85802,1000.);
#27589=VECTOR('',#85807,1000.);
#27590=VECTOR('',#85814,1000.);
#27591=VECTOR('',#85819,1000.);
#27592=VECTOR('',#85826,1000.);
#27593=VECTOR('',#85831,1000.);
#27594=VECTOR('',#85838,1000.);
#27595=VECTOR('',#85843,1000.);
#27596=VECTOR('',#85850,1000.);
#27597=VECTOR('',#85855,1000.);
#27598=VECTOR('',#85862,1000.);
#27599=VECTOR('',#85867,1000.);
#27600=VECTOR('',#85874,1000.);
#27601=VECTOR('',#85879,1000.);
#27602=VECTOR('',#85886,1000.);
#27603=VECTOR('',#85891,1000.);
#27604=VECTOR('',#85898,1000.);
#27605=VECTOR('',#85903,1000.);
#27606=VECTOR('',#85910,1000.);
#27607=VECTOR('',#85915,1000.);
#27608=VECTOR('',#85922,1000.);
#27609=VECTOR('',#85927,1000.);
#27610=VECTOR('',#85934,1000.);
#27611=VECTOR('',#85939,1000.);
#27612=VECTOR('',#86064,1000.);
#27613=VECTOR('',#86065,1000.);
#27614=VECTOR('',#86074,1000.);
#27615=VECTOR('',#86075,1000.);
#27616=VECTOR('',#86084,1000.);
#27617=VECTOR('',#86085,1000.);
#27618=VECTOR('',#86094,1000.);
#27619=VECTOR('',#86095,1000.);
#27620=VECTOR('',#86104,1000.);
#27621=VECTOR('',#86105,1000.);
#27622=VECTOR('',#86114,1000.);
#27623=VECTOR('',#86115,1000.);
#27624=VECTOR('',#86124,1000.);
#27625=VECTOR('',#86125,1000.);
#27626=VECTOR('',#86126,1000.);
#27627=VECTOR('',#86127,1000.);
#27628=VECTOR('',#86136,1000.);
#27629=VECTOR('',#86137,1000.);
#27630=VECTOR('',#86146,1000.);
#27631=VECTOR('',#86147,1000.);
#27632=VECTOR('',#86156,1000.);
#27633=VECTOR('',#86157,1000.);
#27634=VECTOR('',#86166,1000.);
#27635=VECTOR('',#86167,1000.);
#27636=VECTOR('',#86176,1000.);
#27637=VECTOR('',#86177,1000.);
#27638=VECTOR('',#86186,1000.);
#27639=VECTOR('',#86187,1000.);
#27640=VECTOR('',#86196,1000.);
#27641=VECTOR('',#86197,1000.);
#27642=VECTOR('',#86206,1000.);
#27643=VECTOR('',#86207,1000.);
#27644=VECTOR('',#86216,1000.);
#27645=VECTOR('',#86217,1000.);
#27646=VECTOR('',#86226,1000.);
#27647=VECTOR('',#86227,1000.);
#27648=VECTOR('',#86236,1000.);
#27649=VECTOR('',#86237,1000.);
#27650=VECTOR('',#86246,1000.);
#27651=VECTOR('',#86247,1000.);
#27652=VECTOR('',#86250,1000.);
#27653=VECTOR('',#86257,1000.);
#27654=VECTOR('',#86266,1000.);
#27655=VECTOR('',#86267,1000.);
#27656=VECTOR('',#86276,1000.);
#27657=VECTOR('',#86277,1000.);
#27658=VECTOR('',#86286,1000.);
#27659=VECTOR('',#86287,1000.);
#27660=VECTOR('',#86296,1000.);
#27661=VECTOR('',#86297,1000.);
#27662=VECTOR('',#86306,1000.);
#27663=VECTOR('',#86307,1000.);
#27664=VECTOR('',#86316,1000.);
#27665=VECTOR('',#86317,1000.);
#27666=VECTOR('',#86326,1000.);
#27667=VECTOR('',#86327,1000.);
#27668=VECTOR('',#86336,1000.);
#27669=VECTOR('',#86343,1000.);
#27670=VECTOR('',#86346,1000.);
#27671=VECTOR('',#86347,1000.);
#27672=VECTOR('',#86350,1000.);
#27673=VECTOR('',#86357,1000.);
#27674=VECTOR('',#86360,1000.);
#27675=VECTOR('',#86367,1000.);
#27676=VECTOR('',#86370,1000.);
#27677=VECTOR('',#86377,1000.);
#27678=VECTOR('',#86380,1000.);
#27679=VECTOR('',#86387,1000.);
#27680=VECTOR('',#86390,1000.);
#27681=VECTOR('',#86397,1000.);
#27682=VECTOR('',#86400,1000.);
#27683=VECTOR('',#86407,1000.);
#27684=VECTOR('',#86410,1000.);
#27685=VECTOR('',#86417,1000.);
#27686=VECTOR('',#86420,1000.);
#27687=VECTOR('',#86427,1000.);
#27688=VECTOR('',#86430,1000.);
#27689=VECTOR('',#86437,1000.);
#27690=VECTOR('',#86440,1000.);
#27691=VECTOR('',#86447,1000.);
#27692=VECTOR('',#86450,1000.);
#27693=VECTOR('',#86457,1000.);
#27694=VECTOR('',#86460,1000.);
#27695=VECTOR('',#86467,1000.);
#27696=VECTOR('',#86470,1000.);
#27697=VECTOR('',#86477,1000.);
#27698=VECTOR('',#86478,1000.);
#27699=VECTOR('',#86479,1000.);
#27700=VECTOR('',#86482,1000.);
#27701=VECTOR('',#86489,1000.);
#27702=VECTOR('',#86492,1000.);
#27703=VECTOR('',#86499,1000.);
#27704=VECTOR('',#86502,1000.);
#27705=VECTOR('',#86509,1000.);
#27706=VECTOR('',#86512,1000.);
#27707=VECTOR('',#86519,1000.);
#27708=VECTOR('',#86522,1000.);
#27709=VECTOR('',#86529,1000.);
#27710=VECTOR('',#86532,1000.);
#27711=VECTOR('',#86539,1000.);
#27712=VECTOR('',#86542,1000.);
#27713=VECTOR('',#86549,1000.);
#27714=VECTOR('',#86552,1000.);
#27715=VECTOR('',#86559,1000.);
#27716=VECTOR('',#86562,1000.);
#27717=VECTOR('',#86569,1000.);
#27718=VECTOR('',#86572,1000.);
#27719=VECTOR('',#86579,1000.);
#27720=VECTOR('',#86582,1000.);
#27721=VECTOR('',#86589,1000.);
#27722=VECTOR('',#86592,1000.);
#27723=VECTOR('',#86599,1000.);
#27724=VECTOR('',#86602,1000.);
#27725=VECTOR('',#86609,1000.);
#27726=VECTOR('',#86612,1000.);
#27727=VECTOR('',#86625,1000.);
#27728=VECTOR('',#86860,1000.);
#27729=VECTOR('',#86869,1000.);
#27730=VECTOR('',#86872,1000.);
#27731=VECTOR('',#86881,1000.);
#27732=VECTOR('',#86884,1000.);
#27733=VECTOR('',#86893,1000.);
#27734=VECTOR('',#86896,1000.);
#27735=VECTOR('',#86905,1000.);
#27736=VECTOR('',#86908,1000.);
#27737=VECTOR('',#86917,1000.);
#27738=VECTOR('',#86920,1000.);
#27739=VECTOR('',#86929,1000.);
#27740=VECTOR('',#86932,1000.);
#27741=VECTOR('',#86941,1000.);
#27742=VECTOR('',#86944,1000.);
#27743=VECTOR('',#86953,1000.);
#27744=VECTOR('',#86956,1000.);
#27745=VECTOR('',#86965,1000.);
#27746=VECTOR('',#86968,1000.);
#27747=VECTOR('',#86977,1000.);
#27748=VECTOR('',#86980,1000.);
#27749=VECTOR('',#86989,1000.);
#27750=VECTOR('',#86992,1000.);
#27751=VECTOR('',#87001,1000.);
#27752=VECTOR('',#87004,1000.);
#27753=VECTOR('',#87013,1000.);
#27754=VECTOR('',#87016,1000.);
#27755=VECTOR('',#87025,1000.);
#27756=VECTOR('',#87026,1000.);
#27757=VECTOR('',#87027,1000.);
#27758=VECTOR('',#87030,1000.);
#27759=VECTOR('',#87039,1000.);
#27760=VECTOR('',#87042,1000.);
#27761=VECTOR('',#87051,1000.);
#27762=VECTOR('',#87054,1000.);
#27763=VECTOR('',#87063,1000.);
#27764=VECTOR('',#87066,1000.);
#27765=VECTOR('',#87075,1000.);
#27766=VECTOR('',#87078,1000.);
#27767=VECTOR('',#87081,1000.);
#27768=VECTOR('',#87088,1000.);
#27769=VECTOR('',#87099,1000.);
#27770=VECTOR('',#87102,1000.);
#27771=VECTOR('',#87111,1000.);
#27772=VECTOR('',#87114,1000.);
#27773=VECTOR('',#87123,1000.);
#27774=VECTOR('',#87126,1000.);
#27775=VECTOR('',#87135,1000.);
#27776=VECTOR('',#87138,1000.);
#27777=VECTOR('',#87147,1000.);
#27778=VECTOR('',#87150,1000.);
#27779=VECTOR('',#87159,1000.);
#27780=VECTOR('',#87162,1000.);
#27781=VECTOR('',#87171,1000.);
#27782=VECTOR('',#87174,1000.);
#27783=VECTOR('',#87183,1000.);
#27784=VECTOR('',#87186,1000.);
#27785=VECTOR('',#87195,1000.);
#27786=VECTOR('',#87196,1000.);
#27787=VECTOR('',#87201,1000.);
#27788=VECTOR('',#87208,1000.);
#27789=VECTOR('',#87213,1000.);
#27790=VECTOR('',#87220,1000.);
#27791=VECTOR('',#87225,1000.);
#27792=VECTOR('',#87232,1000.);
#27793=VECTOR('',#87237,1000.);
#27794=VECTOR('',#87244,1000.);
#27795=VECTOR('',#87249,1000.);
#27796=VECTOR('',#87256,1000.);
#27797=VECTOR('',#87261,1000.);
#27798=VECTOR('',#87268,1000.);
#27799=VECTOR('',#87273,1000.);
#27800=VECTOR('',#87280,1000.);
#27801=VECTOR('',#87285,1000.);
#27802=VECTOR('',#87292,1000.);
#27803=VECTOR('',#87297,1000.);
#27804=VECTOR('',#87304,1000.);
#27805=VECTOR('',#87309,1000.);
#27806=VECTOR('',#87316,1000.);
#27807=VECTOR('',#87321,1000.);
#27808=VECTOR('',#87328,1000.);
#27809=VECTOR('',#87333,1000.);
#27810=VECTOR('',#87340,1000.);
#27811=VECTOR('',#87345,1000.);
#27812=VECTOR('',#87352,1000.);
#27813=VECTOR('',#87357,1000.);
#27814=VECTOR('',#87364,1000.);
#27815=VECTOR('',#87369,1000.);
#27816=VECTOR('',#87376,1000.);
#27817=VECTOR('',#87381,1000.);
#27818=VECTOR('',#87388,1000.);
#27819=VECTOR('',#87393,1000.);
#27820=VECTOR('',#87400,1000.);
#27821=VECTOR('',#87405,1000.);
#27822=VECTOR('',#87412,1000.);
#27823=VECTOR('',#87417,1000.);
#27824=VECTOR('',#87424,1000.);
#27825=VECTOR('',#87429,1000.);
#27826=VECTOR('',#87436,1000.);
#27827=VECTOR('',#87441,1000.);
#27828=VECTOR('',#87448,1000.);
#27829=VECTOR('',#87449,1000.);
#27830=VECTOR('',#87450,1000.);
#27831=VECTOR('',#87455,1000.);
#27832=VECTOR('',#87462,1000.);
#27833=VECTOR('',#87467,1000.);
#27834=VECTOR('',#87474,1000.);
#27835=VECTOR('',#87479,1000.);
#27836=VECTOR('',#87486,1000.);
#27837=VECTOR('',#87491,1000.);
#27838=VECTOR('',#87498,1000.);
#27839=VECTOR('',#87503,1000.);
#27840=VECTOR('',#87510,1000.);
#27841=VECTOR('',#87515,1000.);
#27842=VECTOR('',#87522,1000.);
#27843=VECTOR('',#87527,1000.);
#27844=VECTOR('',#87768,1000.);
#27845=VECTOR('',#87771,1000.);
#27846=VECTOR('',#87780,1000.);
#27847=VECTOR('',#87783,1000.);
#27848=VECTOR('',#87792,1000.);
#27849=VECTOR('',#87795,1000.);
#27850=VECTOR('',#87804,1000.);
#27851=VECTOR('',#87807,1000.);
#27852=VECTOR('',#87816,1000.);
#27853=VECTOR('',#87819,1000.);
#27854=VECTOR('',#87828,1000.);
#27855=VECTOR('',#87831,1000.);
#27856=VECTOR('',#87840,1000.);
#27857=VECTOR('',#87841,1000.);
#27858=VECTOR('',#87842,1000.);
#27859=VECTOR('',#87845,1000.);
#27860=VECTOR('',#87854,1000.);
#27861=VECTOR('',#87857,1000.);
#27862=VECTOR('',#87866,1000.);
#27863=VECTOR('',#87869,1000.);
#27864=VECTOR('',#87878,1000.);
#27865=VECTOR('',#87881,1000.);
#27866=VECTOR('',#87890,1000.);
#27867=VECTOR('',#87893,1000.);
#27868=VECTOR('',#87902,1000.);
#27869=VECTOR('',#87905,1000.);
#27870=VECTOR('',#87914,1000.);
#27871=VECTOR('',#87917,1000.);
#27872=VECTOR('',#87926,1000.);
#27873=VECTOR('',#87929,1000.);
#27874=VECTOR('',#87938,1000.);
#27875=VECTOR('',#87941,1000.);
#27876=VECTOR('',#87950,1000.);
#27877=VECTOR('',#87953,1000.);
#27878=VECTOR('',#87962,1000.);
#27879=VECTOR('',#87965,1000.);
#27880=VECTOR('',#87974,1000.);
#27881=VECTOR('',#87977,1000.);
#27882=VECTOR('',#87980,1000.);
#27883=VECTOR('',#87987,1000.);
#27884=VECTOR('',#87998,1000.);
#27885=VECTOR('',#88001,1000.);
#27886=VECTOR('',#88010,1000.);
#27887=VECTOR('',#88013,1000.);
#27888=VECTOR('',#88022,1000.);
#27889=VECTOR('',#88025,1000.);
#27890=VECTOR('',#88034,1000.);
#27891=VECTOR('',#88037,1000.);
#27892=VECTOR('',#88046,1000.);
#27893=VECTOR('',#88049,1000.);
#27894=VECTOR('',#88058,1000.);
#27895=VECTOR('',#88061,1000.);
#27896=VECTOR('',#88070,1000.);
#27897=VECTOR('',#88073,1000.);
#27898=VECTOR('',#88082,1000.);
#27899=VECTOR('',#88085,1000.);
#27900=VECTOR('',#88094,1000.);
#27901=VECTOR('',#88103,1000.);
#27902=VECTOR('',#88106,1000.);
#27903=VECTOR('',#88107,1000.);
#27904=VECTOR('',#88112,1000.);
#27905=VECTOR('',#88119,1000.);
#27906=VECTOR('',#88124,1000.);
#27907=VECTOR('',#88131,1000.);
#27908=VECTOR('',#88136,1000.);
#27909=VECTOR('',#88143,1000.);
#27910=VECTOR('',#88148,1000.);
#27911=VECTOR('',#88155,1000.);
#27912=VECTOR('',#88160,1000.);
#27913=VECTOR('',#88167,1000.);
#27914=VECTOR('',#88172,1000.);
#27915=VECTOR('',#88179,1000.);
#27916=VECTOR('',#88184,1000.);
#27917=VECTOR('',#88191,1000.);
#27918=VECTOR('',#88196,1000.);
#27919=VECTOR('',#88203,1000.);
#27920=VECTOR('',#88208,1000.);
#27921=VECTOR('',#88215,1000.);
#27922=VECTOR('',#88220,1000.);
#27923=VECTOR('',#88227,1000.);
#27924=VECTOR('',#88232,1000.);
#27925=VECTOR('',#88239,1000.);
#27926=VECTOR('',#88244,1000.);
#27927=VECTOR('',#88251,1000.);
#27928=VECTOR('',#88256,1000.);
#27929=VECTOR('',#88263,1000.);
#27930=VECTOR('',#88264,1000.);
#27931=VECTOR('',#88265,1000.);
#27932=VECTOR('',#88270,1000.);
#27933=VECTOR('',#88277,1000.);
#27934=VECTOR('',#88282,1000.);
#27935=VECTOR('',#88289,1000.);
#27936=VECTOR('',#88294,1000.);
#27937=VECTOR('',#88301,1000.);
#27938=VECTOR('',#88306,1000.);
#27939=VECTOR('',#88313,1000.);
#27940=VECTOR('',#88318,1000.);
#27941=VECTOR('',#88325,1000.);
#27942=VECTOR('',#88330,1000.);
#27943=VECTOR('',#88337,1000.);
#27944=VECTOR('',#88342,1000.);
#27945=VECTOR('',#88349,1000.);
#27946=VECTOR('',#88354,1000.);
#27947=VECTOR('',#88361,1000.);
#27948=VECTOR('',#88366,1000.);
#27949=VECTOR('',#88373,1000.);
#27950=VECTOR('',#88378,1000.);
#27951=VECTOR('',#88385,1000.);
#27952=VECTOR('',#88390,1000.);
#27953=VECTOR('',#88397,1000.);
#27954=VECTOR('',#88402,1000.);
#27955=VECTOR('',#88409,1000.);
#27956=VECTOR('',#88414,1000.);
#27957=VECTOR('',#88421,1000.);
#27958=VECTOR('',#88426,1000.);
#27959=VECTOR('',#88441,1000.);
#27960=VECTOR('',#88618,1000.);
#27961=VECTOR('',#88625,1000.);
#27962=VECTOR('',#88628,1000.);
#27963=VECTOR('',#88635,1000.);
#27964=VECTOR('',#88638,1000.);
#27965=VECTOR('',#88645,1000.);
#27966=VECTOR('',#88648,1000.);
#27967=VECTOR('',#88655,1000.);
#27968=VECTOR('',#88658,1000.);
#27969=VECTOR('',#88665,1000.);
#27970=VECTOR('',#88668,1000.);
#27971=VECTOR('',#88675,1000.);
#27972=VECTOR('',#88678,1000.);
#27973=VECTOR('',#88685,1000.);
#27974=VECTOR('',#88688,1000.);
#27975=VECTOR('',#88695,1000.);
#27976=VECTOR('',#88698,1000.);
#27977=VECTOR('',#88705,1000.);
#27978=VECTOR('',#88708,1000.);
#27979=VECTOR('',#88715,1000.);
#27980=VECTOR('',#88718,1000.);
#27981=VECTOR('',#88725,1000.);
#27982=VECTOR('',#88728,1000.);
#27983=VECTOR('',#88735,1000.);
#27984=VECTOR('',#88738,1000.);
#27985=VECTOR('',#88745,1000.);
#27986=VECTOR('',#88748,1000.);
#27987=VECTOR('',#88755,1000.);
#27988=VECTOR('',#88756,1000.);
#27989=VECTOR('',#88757,1000.);
#27990=VECTOR('',#88760,1000.);
#27991=VECTOR('',#88767,1000.);
#27992=VECTOR('',#88770,1000.);
#27993=VECTOR('',#88777,1000.);
#27994=VECTOR('',#88780,1000.);
#27995=VECTOR('',#88787,1000.);
#27996=VECTOR('',#88790,1000.);
#27997=VECTOR('',#88791,1000.);
#27998=VECTOR('',#88798,1000.);
#27999=VECTOR('',#88807,1000.);
#28000=VECTOR('',#88810,1000.);
#28001=VECTOR('',#88817,1000.);
#28002=VECTOR('',#88820,1000.);
#28003=VECTOR('',#88827,1000.);
#28004=VECTOR('',#88830,1000.);
#28005=VECTOR('',#88837,1000.);
#28006=VECTOR('',#88840,1000.);
#28007=VECTOR('',#88847,1000.);
#28008=VECTOR('',#88850,1000.);
#28009=VECTOR('',#88857,1000.);
#28010=VECTOR('',#88860,1000.);
#28011=VECTOR('',#88867,1000.);
#28012=VECTOR('',#88870,1000.);
#28013=VECTOR('',#88877,1000.);
#28014=VECTOR('',#88880,1000.);
#28015=VECTOR('',#88887,1000.);
#28016=VECTOR('',#88890,1000.);
#28017=VECTOR('',#88897,1000.);
#28018=VECTOR('',#88898,1000.);
#28019=VECTOR('',#88911,1000.);
#28020=VECTOR('',#88918,1000.);
#28021=VECTOR('',#88931,1000.);
#28022=VECTOR('',#88938,1000.);
#28023=VECTOR('',#88951,1000.);
#28024=VECTOR('',#88958,1000.);
#28025=VECTOR('',#88971,1000.);
#28026=VECTOR('',#88978,1000.);
#28027=VECTOR('',#88991,1000.);
#28028=VECTOR('',#88998,1000.);
#28029=VECTOR('',#89011,1000.);
#28030=VECTOR('',#89018,1000.);
#28031=VECTOR('',#89031,1000.);
#28032=VECTOR('',#89038,1000.);
#28033=VECTOR('',#89051,1000.);
#28034=VECTOR('',#89058,1000.);
#28035=VECTOR('',#89071,1000.);
#28036=VECTOR('',#89078,1000.);
#28037=VECTOR('',#89091,1000.);
#28038=VECTOR('',#89098,1000.);
#28039=VECTOR('',#89111,1000.);
#28040=VECTOR('',#89118,1000.);
#28041=VECTOR('',#89131,1000.);
#28042=VECTOR('',#89138,1000.);
#28043=VECTOR('',#89151,1000.);
#28044=VECTOR('',#89158,1000.);
#28045=VECTOR('',#89171,1000.);
#28046=VECTOR('',#89178,1000.);
#28047=VECTOR('',#89191,1000.);
#28048=VECTOR('',#89198,1000.);
#28049=VECTOR('',#89211,1000.);
#28050=VECTOR('',#89218,1000.);
#28051=VECTOR('',#89231,1000.);
#28052=VECTOR('',#89238,1000.);
#28053=VECTOR('',#89251,1000.);
#28054=VECTOR('',#89258,1000.);
#28055=VECTOR('',#89271,1000.);
#28056=VECTOR('',#89278,1000.);
#28057=VECTOR('',#89291,1000.);
#28058=VECTOR('',#89298,1000.);
#28059=VECTOR('',#89311,1000.);
#28060=VECTOR('',#89318,1000.);
#28061=VECTOR('',#89319,1000.);
#28062=VECTOR('',#89320,1000.);
#28063=VECTOR('',#89333,1000.);
#28064=VECTOR('',#89340,1000.);
#28065=VECTOR('',#89353,1000.);
#28066=VECTOR('',#89360,1000.);
#28067=VECTOR('',#89373,1000.);
#28068=VECTOR('',#89380,1000.);
#28069=VECTOR('',#89393,1000.);
#28070=VECTOR('',#89400,1000.);
#28071=VECTOR('',#89413,1000.);
#28072=VECTOR('',#89420,1000.);
#28073=VECTOR('',#89433,1000.);
#28074=VECTOR('',#89440,1000.);
#28075=VECTOR('',#89453,1000.);
#28076=VECTOR('',#89752,1000.);
#28077=VECTOR('',#89755,1000.);
#28078=VECTOR('',#89764,1000.);
#28079=VECTOR('',#89767,1000.);
#28080=VECTOR('',#89776,1000.);
#28081=VECTOR('',#89779,1000.);
#28082=VECTOR('',#89788,1000.);
#28083=VECTOR('',#89791,1000.);
#28084=VECTOR('',#89800,1000.);
#28085=VECTOR('',#89803,1000.);
#28086=VECTOR('',#89812,1000.);
#28087=VECTOR('',#89815,1000.);
#28088=VECTOR('',#89824,1000.);
#28089=VECTOR('',#89825,1000.);
#28090=VECTOR('',#89826,1000.);
#28091=VECTOR('',#89829,1000.);
#28092=VECTOR('',#89838,1000.);
#28093=VECTOR('',#89841,1000.);
#28094=VECTOR('',#89850,1000.);
#28095=VECTOR('',#89853,1000.);
#28096=VECTOR('',#89862,1000.);
#28097=VECTOR('',#89865,1000.);
#28098=VECTOR('',#89874,1000.);
#28099=VECTOR('',#89877,1000.);
#28100=VECTOR('',#89886,1000.);
#28101=VECTOR('',#89889,1000.);
#28102=VECTOR('',#89898,1000.);
#28103=VECTOR('',#89901,1000.);
#28104=VECTOR('',#89910,1000.);
#28105=VECTOR('',#89913,1000.);
#28106=VECTOR('',#89922,1000.);
#28107=VECTOR('',#89925,1000.);
#28108=VECTOR('',#89934,1000.);
#28109=VECTOR('',#89937,1000.);
#28110=VECTOR('',#89946,1000.);
#28111=VECTOR('',#89949,1000.);
#28112=VECTOR('',#89952,1000.);
#28113=VECTOR('',#89959,1000.);
#28114=VECTOR('',#89970,1000.);
#28115=VECTOR('',#89973,1000.);
#28116=VECTOR('',#89982,1000.);
#28117=VECTOR('',#89985,1000.);
#28118=VECTOR('',#89994,1000.);
#28119=VECTOR('',#89997,1000.);
#28120=VECTOR('',#90006,1000.);
#28121=VECTOR('',#90009,1000.);
#28122=VECTOR('',#90018,1000.);
#28123=VECTOR('',#90021,1000.);
#28124=VECTOR('',#90030,1000.);
#28125=VECTOR('',#90033,1000.);
#28126=VECTOR('',#90042,1000.);
#28127=VECTOR('',#90045,1000.);
#28128=VECTOR('',#90054,1000.);
#28129=VECTOR('',#90057,1000.);
#28130=VECTOR('',#90066,1000.);
#28131=VECTOR('',#90069,1000.);
#28132=VECTOR('',#90078,1000.);
#28133=VECTOR('',#90087,1000.);
#28134=VECTOR('',#90088,1000.);
#28135=VECTOR('',#90089,1000.);
#28136=VECTOR('',#90092,1000.);
#28137=VECTOR('',#90093,1000.);
#28138=VECTOR('',#90096,1000.);
#28139=VECTOR('',#90097,1000.);
#28140=VECTOR('',#90100,1000.);
#28141=VECTOR('',#90101,1000.);
#28142=VECTOR('',#90104,1000.);
#28143=VECTOR('',#90105,1000.);
#28144=VECTOR('',#90108,1000.);
#28145=VECTOR('',#90109,1000.);
#28146=VECTOR('',#90112,1000.);
#28147=VECTOR('',#90113,1000.);
#28148=VECTOR('',#90116,1000.);
#28149=VECTOR('',#90117,1000.);
#28150=VECTOR('',#90120,1000.);
#28151=VECTOR('',#90121,1000.);
#28152=VECTOR('',#90124,1000.);
#28153=VECTOR('',#90125,1000.);
#28154=VECTOR('',#90128,1000.);
#28155=VECTOR('',#90129,1000.);
#28156=VECTOR('',#90132,1000.);
#28157=VECTOR('',#90133,1000.);
#28158=VECTOR('',#90136,1000.);
#28159=VECTOR('',#90137,1000.);
#28160=VECTOR('',#90140,1000.);
#28161=VECTOR('',#90141,1000.);
#28162=VECTOR('',#90142,1000.);
#28163=VECTOR('',#90143,1000.);
#28164=VECTOR('',#90146,1000.);
#28165=VECTOR('',#90147,1000.);
#28166=VECTOR('',#90150,1000.);
#28167=VECTOR('',#90151,1000.);
#28168=VECTOR('',#90154,1000.);
#28169=VECTOR('',#90155,1000.);
#28170=VECTOR('',#90158,1000.);
#28171=VECTOR('',#90159,1000.);
#28172=VECTOR('',#90162,1000.);
#28173=VECTOR('',#90163,1000.);
#28174=VECTOR('',#90166,1000.);
#28175=VECTOR('',#90167,1000.);
#28176=VECTOR('',#90168,1000.);
#28177=VECTOR('',#90169,1000.);
#28178=VECTOR('',#90172,1000.);
#28179=VECTOR('',#90173,1000.);
#28180=VECTOR('',#90176,1000.);
#28181=VECTOR('',#90177,1000.);
#28182=VECTOR('',#90180,1000.);
#28183=VECTOR('',#90181,1000.);
#28184=VECTOR('',#90184,1000.);
#28185=VECTOR('',#90185,1000.);
#28186=VECTOR('',#90188,1000.);
#28187=VECTOR('',#90189,1000.);
#28188=VECTOR('',#90192,1000.);
#28189=VECTOR('',#90193,1000.);
#28190=VECTOR('',#90196,1000.);
#28191=VECTOR('',#90199,1000.);
#28192=VECTOR('',#90434,1000.);
#28193=VECTOR('',#90443,1000.);
#28194=VECTOR('',#90446,1000.);
#28195=VECTOR('',#90455,1000.);
#28196=VECTOR('',#90458,1000.);
#28197=VECTOR('',#90467,1000.);
#28198=VECTOR('',#90470,1000.);
#28199=VECTOR('',#90479,1000.);
#28200=VECTOR('',#90482,1000.);
#28201=VECTOR('',#90491,1000.);
#28202=VECTOR('',#90494,1000.);
#28203=VECTOR('',#90503,1000.);
#28204=VECTOR('',#90506,1000.);
#28205=VECTOR('',#90515,1000.);
#28206=VECTOR('',#90518,1000.);
#28207=VECTOR('',#90527,1000.);
#28208=VECTOR('',#90530,1000.);
#28209=VECTOR('',#90539,1000.);
#28210=VECTOR('',#90542,1000.);
#28211=VECTOR('',#90551,1000.);
#28212=VECTOR('',#90554,1000.);
#28213=VECTOR('',#90563,1000.);
#28214=VECTOR('',#90566,1000.);
#28215=VECTOR('',#90575,1000.);
#28216=VECTOR('',#90578,1000.);
#28217=VECTOR('',#90587,1000.);
#28218=VECTOR('',#90590,1000.);
#28219=VECTOR('',#90599,1000.);
#28220=VECTOR('',#90600,1000.);
#28221=VECTOR('',#90601,1000.);
#28222=VECTOR('',#90604,1000.);
#28223=VECTOR('',#90613,1000.);
#28224=VECTOR('',#90616,1000.);
#28225=VECTOR('',#90625,1000.);
#28226=VECTOR('',#90628,1000.);
#28227=VECTOR('',#90631,1000.);
#28228=VECTOR('',#90638,1000.);
#28229=VECTOR('',#90649,1000.);
#28230=VECTOR('',#90652,1000.);
#28231=VECTOR('',#90661,1000.);
#28232=VECTOR('',#90664,1000.);
#28233=VECTOR('',#90673,1000.);
#28234=VECTOR('',#90676,1000.);
#28235=VECTOR('',#90685,1000.);
#28236=VECTOR('',#90688,1000.);
#28237=VECTOR('',#90697,1000.);
#28238=VECTOR('',#90700,1000.);
#28239=VECTOR('',#90709,1000.);
#28240=VECTOR('',#90712,1000.);
#28241=VECTOR('',#90721,1000.);
#28242=VECTOR('',#90724,1000.);
#28243=VECTOR('',#90733,1000.);
#28244=VECTOR('',#90736,1000.);
#28245=VECTOR('',#90745,1000.);
#28246=VECTOR('',#90748,1000.);
#28247=VECTOR('',#90757,1000.);
#28248=VECTOR('',#90760,1000.);
#28249=VECTOR('',#90769,1000.);
#28250=VECTOR('',#90772,1000.);
#28251=VECTOR('',#90773,1000.);
#28252=VECTOR('',#90774,1000.);
#28253=VECTOR('',#90777,1000.);
#28254=VECTOR('',#90778,1000.);
#28255=VECTOR('',#90781,1000.);
#28256=VECTOR('',#90782,1000.);
#28257=VECTOR('',#90785,1000.);
#28258=VECTOR('',#90786,1000.);
#28259=VECTOR('',#90789,1000.);
#28260=VECTOR('',#90790,1000.);
#28261=VECTOR('',#90793,1000.);
#28262=VECTOR('',#90794,1000.);
#28263=VECTOR('',#90797,1000.);
#28264=VECTOR('',#90798,1000.);
#28265=VECTOR('',#90801,1000.);
#28266=VECTOR('',#90802,1000.);
#28267=VECTOR('',#90805,1000.);
#28268=VECTOR('',#90806,1000.);
#28269=VECTOR('',#90809,1000.);
#28270=VECTOR('',#90810,1000.);
#28271=VECTOR('',#90813,1000.);
#28272=VECTOR('',#90814,1000.);
#28273=VECTOR('',#90817,1000.);
#28274=VECTOR('',#90818,1000.);
#28275=VECTOR('',#90821,1000.);
#28276=VECTOR('',#90822,1000.);
#28277=VECTOR('',#90825,1000.);
#28278=VECTOR('',#90826,1000.);
#28279=VECTOR('',#90829,1000.);
#28280=VECTOR('',#90830,1000.);
#28281=VECTOR('',#90833,1000.);
#28282=VECTOR('',#90834,1000.);
#28283=VECTOR('',#90837,1000.);
#28284=VECTOR('',#90838,1000.);
#28285=VECTOR('',#90841,1000.);
#28286=VECTOR('',#90842,1000.);
#28287=VECTOR('',#90845,1000.);
#28288=VECTOR('',#90846,1000.);
#28289=VECTOR('',#90849,1000.);
#28290=VECTOR('',#90850,1000.);
#28291=VECTOR('',#90853,1000.);
#28292=VECTOR('',#90854,1000.);
#28293=VECTOR('',#90857,1000.);
#28294=VECTOR('',#90858,1000.);
#28295=VECTOR('',#90861,1000.);
#28296=VECTOR('',#90862,1000.);
#28297=VECTOR('',#90865,1000.);
#28298=VECTOR('',#90866,1000.);
#28299=VECTOR('',#90869,1000.);
#28300=VECTOR('',#90870,1000.);
#28301=VECTOR('',#90873,1000.);
#28302=VECTOR('',#90874,1000.);
#28303=VECTOR('',#90877,1000.);
#28304=VECTOR('',#90878,1000.);
#28305=VECTOR('',#90881,1000.);
#28306=VECTOR('',#90882,1000.);
#28307=VECTOR('',#90885,1000.);
#28308=VECTOR('',#91004,1000.);
#28309=VECTOR('',#91007,1000.);
#28310=VECTOR('',#91018,1000.);
#28311=VECTOR('',#91027,1000.);
#28312=VECTOR('',#91038,1000.);
#28313=VECTOR('',#91047,1000.);
#28314=VECTOR('',#91058,1000.);
#28315=VECTOR('',#91067,1000.);
#28316=VECTOR('',#91078,1000.);
#28317=VECTOR('',#91087,1000.);
#28318=VECTOR('',#91098,1000.);
#28319=VECTOR('',#91107,1000.);
#28320=VECTOR('',#91118,1000.);
#28321=VECTOR('',#91125,1000.);
#28322=VECTOR('',#91132,1000.);
#28323=VECTOR('',#91135,1000.);
#28324=VECTOR('',#91146,1000.);
#28325=VECTOR('',#91155,1000.);
#28326=VECTOR('',#91166,1000.);
#28327=VECTOR('',#91175,1000.);
#28328=VECTOR('',#91186,1000.);
#28329=VECTOR('',#91195,1000.);
#28330=VECTOR('',#91206,1000.);
#28331=VECTOR('',#91215,1000.);
#28332=VECTOR('',#91226,1000.);
#28333=VECTOR('',#91235,1000.);
#28334=VECTOR('',#91246,1000.);
#28335=VECTOR('',#91255,1000.);
#28336=VECTOR('',#91266,1000.);
#28337=VECTOR('',#91275,1000.);
#28338=VECTOR('',#91286,1000.);
#28339=VECTOR('',#91295,1000.);
#28340=VECTOR('',#91306,1000.);
#28341=VECTOR('',#91315,1000.);
#28342=VECTOR('',#91326,1000.);
#28343=VECTOR('',#91333,1000.);
#28344=VECTOR('',#91346,1000.);
#28345=VECTOR('',#91355,1000.);
#28346=VECTOR('',#91366,1000.);
#28347=VECTOR('',#91375,1000.);
#28348=VECTOR('',#91386,1000.);
#28349=VECTOR('',#91395,1000.);
#28350=VECTOR('',#91406,1000.);
#28351=VECTOR('',#91415,1000.);
#28352=VECTOR('',#91426,1000.);
#28353=VECTOR('',#91435,1000.);
#28354=VECTOR('',#91446,1000.);
#28355=VECTOR('',#91455,1000.);
#28356=VECTOR('',#91466,1000.);
#28357=VECTOR('',#91475,1000.);
#28358=VECTOR('',#91486,1000.);
#28359=VECTOR('',#91495,1000.);
#28360=VECTOR('',#91506,1000.);
#28361=VECTOR('',#91515,1000.);
#28362=VECTOR('',#91526,1000.);
#28363=VECTOR('',#91535,1000.);
#28364=VECTOR('',#91546,1000.);
#28365=VECTOR('',#91569,1000.);
#28366=VECTOR('',#91746,1000.);
#28367=VECTOR('',#91749,1000.);
#28368=VECTOR('',#91750,1000.);
#28369=VECTOR('',#91753,1000.);
#28370=VECTOR('',#91754,1000.);
#28371=VECTOR('',#91757,1000.);
#28372=VECTOR('',#91758,1000.);
#28373=VECTOR('',#91761,1000.);
#28374=VECTOR('',#91762,1000.);
#28375=VECTOR('',#91765,1000.);
#28376=VECTOR('',#91766,1000.);
#28377=VECTOR('',#91769,1000.);
#28378=VECTOR('',#91770,1000.);
#28379=VECTOR('',#91773,1000.);
#28380=VECTOR('',#91774,1000.);
#28381=VECTOR('',#91777,1000.);
#28382=VECTOR('',#91778,1000.);
#28383=VECTOR('',#91781,1000.);
#28384=VECTOR('',#91782,1000.);
#28385=VECTOR('',#91785,1000.);
#28386=VECTOR('',#91786,1000.);
#28387=VECTOR('',#91789,1000.);
#28388=VECTOR('',#91790,1000.);
#28389=VECTOR('',#91793,1000.);
#28390=VECTOR('',#91794,1000.);
#28391=VECTOR('',#91797,1000.);
#28392=VECTOR('',#91798,1000.);
#28393=VECTOR('',#91801,1000.);
#28394=VECTOR('',#91802,1000.);
#28395=VECTOR('',#91805,1000.);
#28396=VECTOR('',#91806,1000.);
#28397=VECTOR('',#91809,1000.);
#28398=VECTOR('',#91810,1000.);
#28399=VECTOR('',#91813,1000.);
#28400=VECTOR('',#91814,1000.);
#28401=VECTOR('',#91817,1000.);
#28402=VECTOR('',#91818,1000.);
#28403=VECTOR('',#91821,1000.);
#28404=VECTOR('',#91822,1000.);
#28405=VECTOR('',#91825,1000.);
#28406=VECTOR('',#91826,1000.);
#28407=VECTOR('',#91829,1000.);
#28408=VECTOR('',#91830,1000.);
#28409=VECTOR('',#91831,1000.);
#28410=VECTOR('',#91832,1000.);
#28411=VECTOR('',#91835,1000.);
#28412=VECTOR('',#91836,1000.);
#28413=VECTOR('',#91839,1000.);
#28414=VECTOR('',#91840,1000.);
#28415=VECTOR('',#91843,1000.);
#28416=VECTOR('',#91844,1000.);
#28417=VECTOR('',#91847,1000.);
#28418=VECTOR('',#91848,1000.);
#28419=VECTOR('',#91851,1000.);
#28420=VECTOR('',#91852,1000.);
#28421=VECTOR('',#91855,1000.);
#28422=VECTOR('',#91856,1000.);
#28423=VECTOR('',#91857,1000.);
#28424=VECTOR('',#92020,1000.);
#28425=VECTOR('',#92023,1000.);
#28426=VECTOR('',#92024,1000.);
#28427=VECTOR('',#92027,1000.);
#28428=VECTOR('',#92028,1000.);
#28429=VECTOR('',#92031,1000.);
#28430=VECTOR('',#92032,1000.);
#28431=VECTOR('',#92035,1000.);
#28432=VECTOR('',#92036,1000.);
#28433=VECTOR('',#92039,1000.);
#28434=VECTOR('',#92040,1000.);
#28435=VECTOR('',#92043,1000.);
#28436=VECTOR('',#92044,1000.);
#28437=VECTOR('',#92047,1000.);
#28438=VECTOR('',#92048,1000.);
#28439=VECTOR('',#92051,1000.);
#28440=VECTOR('',#92052,1000.);
#28441=VECTOR('',#92055,1000.);
#28442=VECTOR('',#92056,1000.);
#28443=VECTOR('',#92059,1000.);
#28444=VECTOR('',#92060,1000.);
#28445=VECTOR('',#92063,1000.);
#28446=VECTOR('',#92064,1000.);
#28447=VECTOR('',#92067,1000.);
#28448=VECTOR('',#92068,1000.);
#28449=VECTOR('',#92071,1000.);
#28450=VECTOR('',#92072,1000.);
#28451=VECTOR('',#92075,1000.);
#28452=VECTOR('',#92076,1000.);
#28453=VECTOR('',#92079,1000.);
#28454=VECTOR('',#92080,1000.);
#28455=VECTOR('',#92083,1000.);
#28456=VECTOR('',#92084,1000.);
#28457=VECTOR('',#92087,1000.);
#28458=VECTOR('',#92088,1000.);
#28459=VECTOR('',#92091,1000.);
#28460=VECTOR('',#92092,1000.);
#28461=VECTOR('',#92095,1000.);
#28462=VECTOR('',#92096,1000.);
#28463=VECTOR('',#92099,1000.);
#28464=VECTOR('',#92100,1000.);
#28465=VECTOR('',#92103,1000.);
#28466=VECTOR('',#92104,1000.);
#28467=VECTOR('',#92107,1000.);
#28468=VECTOR('',#92108,1000.);
#28469=VECTOR('',#92111,1000.);
#28470=VECTOR('',#92112,1000.);
#28471=VECTOR('',#92115,1000.);
#28472=VECTOR('',#92116,1000.);
#28473=VECTOR('',#92119,1000.);
#28474=VECTOR('',#92120,1000.);
#28475=VECTOR('',#92123,1000.);
#28476=VECTOR('',#92124,1000.);
#28477=VECTOR('',#92127,1000.);
#28478=VECTOR('',#92128,1000.);
#28479=VECTOR('',#92131,1000.);
#28480=VECTOR('',#92132,1000.);
#28481=VECTOR('',#92135,1000.);
#28482=VECTOR('',#92146,7.);
#28483=VECTOR('',#92153,1000.);
#28484=VECTOR('',#92156,1000.);
#28485=VECTOR('',#92159,4.5);
#28486=VECTOR('',#92164,1000.);
#28487=VECTOR('',#92167,1000.);
#28488=VECTOR('',#92174,6.5);
#28489=VECTOR('',#92179,1000.);
#28490=VECTOR('',#92182,1000.);
#28491=VECTOR('',#92185,5.9);
#28492=VECTOR('',#92196,5.9);
#28493=VECTOR('',#92207,1000.);
#28494=VECTOR('',#92210,1000.);
#28495=VECTOR('',#92211,1000.);
#28496=VECTOR('',#92218,1000.);
#28497=VECTOR('',#92241,2.5);
#28498=VECTOR('',#92250,2.50000000008162);
#28499=VECTOR('',#92257,2.5);
#28500=VECTOR('',#92260,1000.);
#28501=VECTOR('',#92261,1000.);
#28502=VECTOR('',#92264,2.50000000013396);
#28503=VECTOR('',#92273,1000.);
#28504=VECTOR('',#92278,1000.);
#28505=VECTOR('',#92279,1000.);
#28506=VECTOR('',#92282,1000.);
#28507=VECTOR('',#92285,1000.);
#28508=VECTOR('',#92286,1000.);
#28509=VECTOR('',#92287,1000.);
#28510=VECTOR('',#92294,1000.);
#28511=VECTOR('',#92295,1000.);
#28512=VECTOR('',#92300,1000.);
#28513=VECTOR('',#92309,1000.);
#28514=VECTOR('',#92318,2.5);
#28515=VECTOR('',#92319,2.5);
#28516=VECTOR('',#92342,4.);
#28517=VECTOR('',#92343,1000.);
#28518=VECTOR('',#92346,1000.);
#28519=VECTOR('',#92347,1000.);
#28520=VECTOR('',#92350,1000.);
#28521=VECTOR('',#92355,1.65);
#28522=VECTOR('',#92360,3.826794919);
#28523=VECTOR('',#92365,1.65);
#28524=VECTOR('',#92370,1000.);
#28525=VECTOR('',#92373,1000.);
#28526=VECTOR('',#92376,1.65);
#28527=VECTOR('',#92389,2.5);
#28528=VECTOR('',#92390,2.5);
#28529=VECTOR('',#92395,2.);
#28530=VECTOR('',#92400,2.);
#28531=VECTOR('',#92409,1.676167978);
#28532=VECTOR('',#92416,1.65);
#28533=VERTEX_POINT('',#92438);
#28534=VERTEX_POINT('',#92439);
#28535=VERTEX_POINT('',#92441);
#28536=VERTEX_POINT('',#92448);
#28537=VERTEX_POINT('',#92459);
#28538=VERTEX_POINT('',#92461);
#28539=VERTEX_POINT('',#92463);
#28540=VERTEX_POINT('',#92470);
#28541=VERTEX_POINT('',#92481);
#28542=VERTEX_POINT('',#92488);
#28543=VERTEX_POINT('',#92499);
#28544=VERTEX_POINT('',#92501);
#28545=VERTEX_POINT('',#92503);
#28546=VERTEX_POINT('',#92510);
#28547=VERTEX_POINT('',#92521);
#28548=VERTEX_POINT('',#92528);
#28549=VERTEX_POINT('',#92539);
#28550=VERTEX_POINT('',#92541);
#28551=VERTEX_POINT('',#92543);
#28552=VERTEX_POINT('',#92550);
#28553=VERTEX_POINT('',#92561);
#28554=VERTEX_POINT('',#92568);
#28555=VERTEX_POINT('',#92579);
#28556=VERTEX_POINT('',#92581);
#28557=VERTEX_POINT('',#92583);
#28558=VERTEX_POINT('',#92590);
#28559=VERTEX_POINT('',#92601);
#28560=VERTEX_POINT('',#92608);
#28561=VERTEX_POINT('',#92619);
#28562=VERTEX_POINT('',#92621);
#28563=VERTEX_POINT('',#92623);
#28564=VERTEX_POINT('',#92630);
#28565=VERTEX_POINT('',#92641);
#28566=VERTEX_POINT('',#92648);
#28567=VERTEX_POINT('',#92659);
#28568=VERTEX_POINT('',#92661);
#28569=VERTEX_POINT('',#92663);
#28570=VERTEX_POINT('',#92670);
#28571=VERTEX_POINT('',#92681);
#28572=VERTEX_POINT('',#92688);
#28573=VERTEX_POINT('',#92699);
#28574=VERTEX_POINT('',#92701);
#28575=VERTEX_POINT('',#92703);
#28576=VERTEX_POINT('',#92710);
#28577=VERTEX_POINT('',#92721);
#28578=VERTEX_POINT('',#92728);
#28579=VERTEX_POINT('',#92739);
#28580=VERTEX_POINT('',#92741);
#28581=VERTEX_POINT('',#92743);
#28582=VERTEX_POINT('',#92750);
#28583=VERTEX_POINT('',#92761);
#28584=VERTEX_POINT('',#92768);
#28585=VERTEX_POINT('',#92779);
#28586=VERTEX_POINT('',#92781);
#28587=VERTEX_POINT('',#92783);
#28588=VERTEX_POINT('',#92790);
#28589=VERTEX_POINT('',#92801);
#28590=VERTEX_POINT('',#92808);
#28591=VERTEX_POINT('',#92819);
#28592=VERTEX_POINT('',#92821);
#28593=VERTEX_POINT('',#92823);
#28594=VERTEX_POINT('',#92830);
#28595=VERTEX_POINT('',#92841);
#28596=VERTEX_POINT('',#92848);
#28597=VERTEX_POINT('',#92859);
#28598=VERTEX_POINT('',#92861);
#28599=VERTEX_POINT('',#92863);
#28600=VERTEX_POINT('',#92870);
#28601=VERTEX_POINT('',#92881);
#28602=VERTEX_POINT('',#92888);
#28603=VERTEX_POINT('',#92899);
#28604=VERTEX_POINT('',#92901);
#28605=VERTEX_POINT('',#92903);
#28606=VERTEX_POINT('',#92910);
#28607=VERTEX_POINT('',#92921);
#28608=VERTEX_POINT('',#92928);
#28609=VERTEX_POINT('',#92939);
#28610=VERTEX_POINT('',#92941);
#28611=VERTEX_POINT('',#92943);
#28612=VERTEX_POINT('',#92950);
#28613=VERTEX_POINT('',#92961);
#28614=VERTEX_POINT('',#92968);
#28615=VERTEX_POINT('',#92979);
#28616=VERTEX_POINT('',#92981);
#28617=VERTEX_POINT('',#92983);
#28618=VERTEX_POINT('',#92990);
#28619=VERTEX_POINT('',#93001);
#28620=VERTEX_POINT('',#93008);
#28621=VERTEX_POINT('',#93019);
#28622=VERTEX_POINT('',#93021);
#28623=VERTEX_POINT('',#93023);
#28624=VERTEX_POINT('',#93030);
#28625=VERTEX_POINT('',#93041);
#28626=VERTEX_POINT('',#93048);
#28627=VERTEX_POINT('',#93059);
#28628=VERTEX_POINT('',#93061);
#28629=VERTEX_POINT('',#93063);
#28630=VERTEX_POINT('',#93070);
#28631=VERTEX_POINT('',#93081);
#28632=VERTEX_POINT('',#93088);
#28633=VERTEX_POINT('',#93099);
#28634=VERTEX_POINT('',#93101);
#28635=VERTEX_POINT('',#93103);
#28636=VERTEX_POINT('',#93110);
#28637=VERTEX_POINT('',#93121);
#28638=VERTEX_POINT('',#93128);
#28639=VERTEX_POINT('',#93139);
#28640=VERTEX_POINT('',#93141);
#28641=VERTEX_POINT('',#93143);
#28642=VERTEX_POINT('',#93150);
#28643=VERTEX_POINT('',#93161);
#28644=VERTEX_POINT('',#93168);
#28645=VERTEX_POINT('',#93179);
#28646=VERTEX_POINT('',#93181);
#28647=VERTEX_POINT('',#93183);
#28648=VERTEX_POINT('',#93190);
#28649=VERTEX_POINT('',#93201);
#28650=VERTEX_POINT('',#93208);
#28651=VERTEX_POINT('',#93219);
#28652=VERTEX_POINT('',#93221);
#28653=VERTEX_POINT('',#93223);
#28654=VERTEX_POINT('',#93230);
#28655=VERTEX_POINT('',#93241);
#28656=VERTEX_POINT('',#93248);
#28657=VERTEX_POINT('',#93259);
#28658=VERTEX_POINT('',#93261);
#28659=VERTEX_POINT('',#93263);
#28660=VERTEX_POINT('',#93270);
#28661=VERTEX_POINT('',#93281);
#28662=VERTEX_POINT('',#93288);
#28663=VERTEX_POINT('',#93299);
#28664=VERTEX_POINT('',#93301);
#28665=VERTEX_POINT('',#93303);
#28666=VERTEX_POINT('',#93310);
#28667=VERTEX_POINT('',#93321);
#28668=VERTEX_POINT('',#93328);
#28669=VERTEX_POINT('',#93339);
#28670=VERTEX_POINT('',#93341);
#28671=VERTEX_POINT('',#93343);
#28672=VERTEX_POINT('',#93350);
#28673=VERTEX_POINT('',#93361);
#28674=VERTEX_POINT('',#93368);
#28675=VERTEX_POINT('',#93379);
#28676=VERTEX_POINT('',#93381);
#28677=VERTEX_POINT('',#93383);
#28678=VERTEX_POINT('',#93390);
#28679=VERTEX_POINT('',#93401);
#28680=VERTEX_POINT('',#93408);
#28681=VERTEX_POINT('',#93419);
#28682=VERTEX_POINT('',#93421);
#28683=VERTEX_POINT('',#93423);
#28684=VERTEX_POINT('',#93430);
#28685=VERTEX_POINT('',#93441);
#28686=VERTEX_POINT('',#93448);
#28687=VERTEX_POINT('',#93459);
#28688=VERTEX_POINT('',#93461);
#28689=VERTEX_POINT('',#93463);
#28690=VERTEX_POINT('',#93470);
#28691=VERTEX_POINT('',#93481);
#28692=VERTEX_POINT('',#93488);
#28693=VERTEX_POINT('',#93499);
#28694=VERTEX_POINT('',#93501);
#28695=VERTEX_POINT('',#93503);
#28696=VERTEX_POINT('',#93510);
#28697=VERTEX_POINT('',#93521);
#28698=VERTEX_POINT('',#93528);
#28699=VERTEX_POINT('',#93539);
#28700=VERTEX_POINT('',#93541);
#28701=VERTEX_POINT('',#93543);
#28702=VERTEX_POINT('',#93550);
#28703=VERTEX_POINT('',#93561);
#28704=VERTEX_POINT('',#93568);
#28705=VERTEX_POINT('',#93579);
#28706=VERTEX_POINT('',#93581);
#28707=VERTEX_POINT('',#93583);
#28708=VERTEX_POINT('',#93590);
#28709=VERTEX_POINT('',#93593);
#28710=VERTEX_POINT('',#93605);
#28711=VERTEX_POINT('',#93607);
#28712=VERTEX_POINT('',#93611);
#28713=VERTEX_POINT('',#93623);
#28714=VERTEX_POINT('',#93625);
#28715=VERTEX_POINT('',#93629);
#28716=VERTEX_POINT('',#93630);
#28717=VERTEX_POINT('',#93632);
#28718=VERTEX_POINT('',#93637);
#28719=VERTEX_POINT('',#93641);
#28720=VERTEX_POINT('',#93642);
#28721=VERTEX_POINT('',#93649);
#28722=VERTEX_POINT('',#93651);
#28723=VERTEX_POINT('',#93653);
#28724=VERTEX_POINT('',#93664);
#28725=VERTEX_POINT('',#93671);
#28726=VERTEX_POINT('',#93678);
#28727=VERTEX_POINT('',#93685);
#28728=VERTEX_POINT('',#93687);
#28729=VERTEX_POINT('',#93689);
#28730=VERTEX_POINT('',#93700);
#28731=VERTEX_POINT('',#93707);
#28732=VERTEX_POINT('',#93714);
#28733=VERTEX_POINT('',#93721);
#28734=VERTEX_POINT('',#93723);
#28735=VERTEX_POINT('',#93725);
#28736=VERTEX_POINT('',#93736);
#28737=VERTEX_POINT('',#93743);
#28738=VERTEX_POINT('',#93750);
#28739=VERTEX_POINT('',#93757);
#28740=VERTEX_POINT('',#93759);
#28741=VERTEX_POINT('',#93761);
#28742=VERTEX_POINT('',#93772);
#28743=VERTEX_POINT('',#93779);
#28744=VERTEX_POINT('',#93786);
#28745=VERTEX_POINT('',#93793);
#28746=VERTEX_POINT('',#93795);
#28747=VERTEX_POINT('',#93797);
#28748=VERTEX_POINT('',#93808);
#28749=VERTEX_POINT('',#93815);
#28750=VERTEX_POINT('',#93822);
#28751=VERTEX_POINT('',#93829);
#28752=VERTEX_POINT('',#93831);
#28753=VERTEX_POINT('',#93833);
#28754=VERTEX_POINT('',#93844);
#28755=VERTEX_POINT('',#93851);
#28756=VERTEX_POINT('',#93858);
#28757=VERTEX_POINT('',#93865);
#28758=VERTEX_POINT('',#93867);
#28759=VERTEX_POINT('',#93869);
#28760=VERTEX_POINT('',#93880);
#28761=VERTEX_POINT('',#93887);
#28762=VERTEX_POINT('',#93894);
#28763=VERTEX_POINT('',#93901);
#28764=VERTEX_POINT('',#93903);
#28765=VERTEX_POINT('',#93905);
#28766=VERTEX_POINT('',#93916);
#28767=VERTEX_POINT('',#93923);
#28768=VERTEX_POINT('',#93930);
#28769=VERTEX_POINT('',#93937);
#28770=VERTEX_POINT('',#93939);
#28771=VERTEX_POINT('',#93941);
#28772=VERTEX_POINT('',#93952);
#28773=VERTEX_POINT('',#93959);
#28774=VERTEX_POINT('',#93966);
#28775=VERTEX_POINT('',#93973);
#28776=VERTEX_POINT('',#93975);
#28777=VERTEX_POINT('',#93977);
#28778=VERTEX_POINT('',#93988);
#28779=VERTEX_POINT('',#93995);
#28780=VERTEX_POINT('',#94002);
#28781=VERTEX_POINT('',#94009);
#28782=VERTEX_POINT('',#94011);
#28783=VERTEX_POINT('',#94013);
#28784=VERTEX_POINT('',#94024);
#28785=VERTEX_POINT('',#94031);
#28786=VERTEX_POINT('',#94038);
#28787=VERTEX_POINT('',#94045);
#28788=VERTEX_POINT('',#94047);
#28789=VERTEX_POINT('',#94049);
#28790=VERTEX_POINT('',#94060);
#28791=VERTEX_POINT('',#94067);
#28792=VERTEX_POINT('',#94074);
#28793=VERTEX_POINT('',#94081);
#28794=VERTEX_POINT('',#94083);
#28795=VERTEX_POINT('',#94085);
#28796=VERTEX_POINT('',#94096);
#28797=VERTEX_POINT('',#94103);
#28798=VERTEX_POINT('',#94110);
#28799=VERTEX_POINT('',#94117);
#28800=VERTEX_POINT('',#94119);
#28801=VERTEX_POINT('',#94121);
#28802=VERTEX_POINT('',#94132);
#28803=VERTEX_POINT('',#94139);
#28804=VERTEX_POINT('',#94146);
#28805=VERTEX_POINT('',#94153);
#28806=VERTEX_POINT('',#94155);
#28807=VERTEX_POINT('',#94157);
#28808=VERTEX_POINT('',#94168);
#28809=VERTEX_POINT('',#94171);
#28810=VERTEX_POINT('',#94176);
#28811=VERTEX_POINT('',#94183);
#28812=VERTEX_POINT('',#94190);
#28813=VERTEX_POINT('',#94197);
#28814=VERTEX_POINT('',#94199);
#28815=VERTEX_POINT('',#94201);
#28816=VERTEX_POINT('',#94212);
#28817=VERTEX_POINT('',#94219);
#28818=VERTEX_POINT('',#94226);
#28819=VERTEX_POINT('',#94233);
#28820=VERTEX_POINT('',#94235);
#28821=VERTEX_POINT('',#94237);
#28822=VERTEX_POINT('',#94248);
#28823=VERTEX_POINT('',#94255);
#28824=VERTEX_POINT('',#94262);
#28825=VERTEX_POINT('',#94269);
#28826=VERTEX_POINT('',#94271);
#28827=VERTEX_POINT('',#94273);
#28828=VERTEX_POINT('',#94284);
#28829=VERTEX_POINT('',#94291);
#28830=VERTEX_POINT('',#94298);
#28831=VERTEX_POINT('',#94305);
#28832=VERTEX_POINT('',#94307);
#28833=VERTEX_POINT('',#94309);
#28834=VERTEX_POINT('',#94320);
#28835=VERTEX_POINT('',#94327);
#28836=VERTEX_POINT('',#94334);
#28837=VERTEX_POINT('',#94341);
#28838=VERTEX_POINT('',#94343);
#28839=VERTEX_POINT('',#94345);
#28840=VERTEX_POINT('',#94356);
#28841=VERTEX_POINT('',#94363);
#28842=VERTEX_POINT('',#94370);
#28843=VERTEX_POINT('',#94377);
#28844=VERTEX_POINT('',#94379);
#28845=VERTEX_POINT('',#94381);
#28846=VERTEX_POINT('',#94392);
#28847=VERTEX_POINT('',#94399);
#28848=VERTEX_POINT('',#94406);
#28849=VERTEX_POINT('',#94413);
#28850=VERTEX_POINT('',#94415);
#28851=VERTEX_POINT('',#94417);
#28852=VERTEX_POINT('',#94428);
#28853=VERTEX_POINT('',#94435);
#28854=VERTEX_POINT('',#94442);
#28855=VERTEX_POINT('',#94449);
#28856=VERTEX_POINT('',#94451);
#28857=VERTEX_POINT('',#94453);
#28858=VERTEX_POINT('',#94464);
#28859=VERTEX_POINT('',#94471);
#28860=VERTEX_POINT('',#94478);
#28861=VERTEX_POINT('',#94485);
#28862=VERTEX_POINT('',#94487);
#28863=VERTEX_POINT('',#94489);
#28864=VERTEX_POINT('',#94500);
#28865=VERTEX_POINT('',#94507);
#28866=VERTEX_POINT('',#94514);
#28867=VERTEX_POINT('',#94521);
#28868=VERTEX_POINT('',#94523);
#28869=VERTEX_POINT('',#94525);
#28870=VERTEX_POINT('',#94536);
#28871=VERTEX_POINT('',#94543);
#28872=VERTEX_POINT('',#94550);
#28873=VERTEX_POINT('',#94557);
#28874=VERTEX_POINT('',#94559);
#28875=VERTEX_POINT('',#94561);
#28876=VERTEX_POINT('',#94572);
#28877=VERTEX_POINT('',#94579);
#28878=VERTEX_POINT('',#94586);
#28879=VERTEX_POINT('',#94593);
#28880=VERTEX_POINT('',#94595);
#28881=VERTEX_POINT('',#94597);
#28882=VERTEX_POINT('',#94608);
#28883=VERTEX_POINT('',#94615);
#28884=VERTEX_POINT('',#94622);
#28885=VERTEX_POINT('',#94629);
#28886=VERTEX_POINT('',#94631);
#28887=VERTEX_POINT('',#94633);
#28888=VERTEX_POINT('',#94644);
#28889=VERTEX_POINT('',#94651);
#28890=VERTEX_POINT('',#94658);
#28891=VERTEX_POINT('',#94665);
#28892=VERTEX_POINT('',#94667);
#28893=VERTEX_POINT('',#94669);
#28894=VERTEX_POINT('',#94680);
#28895=VERTEX_POINT('',#94694);
#28896=VERTEX_POINT('',#94695);
#28897=VERTEX_POINT('',#94697);
#28898=VERTEX_POINT('',#94699);
#28899=VERTEX_POINT('',#94715);
#28900=VERTEX_POINT('',#94716);
#28901=VERTEX_POINT('',#94725);
#28902=VERTEX_POINT('',#94727);
#28903=VERTEX_POINT('',#94743);
#28904=VERTEX_POINT('',#94744);
#28905=VERTEX_POINT('',#94757);
#28906=VERTEX_POINT('',#94759);
#28907=VERTEX_POINT('',#94761);
#28908=VERTEX_POINT('',#94765);
#28909=VERTEX_POINT('',#94766);
#28910=VERTEX_POINT('',#94773);
#28911=VERTEX_POINT('',#94780);
#28912=VERTEX_POINT('',#94784);
#28913=VERTEX_POINT('',#94785);
#28914=VERTEX_POINT('',#94794);
#28915=VERTEX_POINT('',#94796);
#28916=VERTEX_POINT('',#94812);
#28917=VERTEX_POINT('',#94813);
#28918=VERTEX_POINT('',#94822);
#28919=VERTEX_POINT('',#94824);
#28920=VERTEX_POINT('',#94840);
#28921=VERTEX_POINT('',#94841);
#28922=VERTEX_POINT('',#94848);
#28923=VERTEX_POINT('',#94850);
#28924=VERTEX_POINT('',#94859);
#28925=VERTEX_POINT('',#94860);
#28926=VERTEX_POINT('',#94862);
#28927=VERTEX_POINT('',#94864);
#28928=VERTEX_POINT('',#94866);
#28929=VERTEX_POINT('',#94881);
#28930=VERTEX_POINT('',#94890);
#28931=VERTEX_POINT('',#94891);
#28932=VERTEX_POINT('',#94904);
#28933=VERTEX_POINT('',#94917);
#28934=VERTEX_POINT('',#94927);
#28935=VERTEX_POINT('',#94928);
#28936=VERTEX_POINT('',#94935);
#28937=VERTEX_POINT('',#94942);
#28938=VERTEX_POINT('',#94946);
#28939=VERTEX_POINT('',#94947);
#28940=VERTEX_POINT('',#94954);
#28941=VERTEX_POINT('',#94956);
#28942=VERTEX_POINT('',#94971);
#28943=VERTEX_POINT('',#94972);
#28944=VERTEX_POINT('',#94979);
#28945=VERTEX_POINT('',#94981);
#28946=VERTEX_POINT('',#94990);
#28947=VERTEX_POINT('',#94991);
#28948=VERTEX_POINT('',#94998);
#28949=VERTEX_POINT('',#95005);
#28950=VERTEX_POINT('',#95009);
#28951=VERTEX_POINT('',#95010);
#28952=VERTEX_POINT('',#95017);
#28953=VERTEX_POINT('',#95024);
#28954=VERTEX_POINT('',#95034);
#28955=VERTEX_POINT('',#95035);
#28956=VERTEX_POINT('',#95048);
#28957=VERTEX_POINT('',#95056);
#28958=VERTEX_POINT('',#95071);
#28959=VERTEX_POINT('',#95072);
#28960=VERTEX_POINT('',#95079);
#28961=VERTEX_POINT('',#95086);
#28962=VERTEX_POINT('',#95096);
#28963=VERTEX_POINT('',#95097);
#28964=VERTEX_POINT('',#95104);
#28965=VERTEX_POINT('',#95111);
#28966=VERTEX_POINT('',#95115);
#28967=VERTEX_POINT('',#95116);
#28968=VERTEX_POINT('',#95129);
#28969=VERTEX_POINT('',#95131);
#28970=VERTEX_POINT('',#95140);
#28971=VERTEX_POINT('',#95141);
#28972=VERTEX_POINT('',#95154);
#28973=VERTEX_POINT('',#95156);
#28974=VERTEX_POINT('',#95177);
#28975=VERTEX_POINT('',#95178);
#28976=VERTEX_POINT('',#95191);
#28977=VERTEX_POINT('',#95204);
#28978=VERTEX_POINT('',#95208);
#28979=VERTEX_POINT('',#95209);
#28980=VERTEX_POINT('',#95216);
#28981=VERTEX_POINT('',#95223);
#28982=VERTEX_POINT('',#95233);
#28983=VERTEX_POINT('',#95234);
#28984=VERTEX_POINT('',#95241);
#28985=VERTEX_POINT('',#95249);
#28986=VERTEX_POINT('',#95258);
#28987=VERTEX_POINT('',#95259);
#28988=VERTEX_POINT('',#95266);
#28989=VERTEX_POINT('',#95268);
#28990=VERTEX_POINT('',#95283);
#28991=VERTEX_POINT('',#95284);
#28992=VERTEX_POINT('',#95297);
#28993=VERTEX_POINT('',#95304);
#28994=VERTEX_POINT('',#95314);
#28995=VERTEX_POINT('',#95315);
#28996=VERTEX_POINT('',#95328);
#28997=VERTEX_POINT('',#95341);
#28998=VERTEX_POINT('',#95345);
#28999=VERTEX_POINT('',#95346);
#29000=VERTEX_POINT('',#95359);
#29001=VERTEX_POINT('',#95361);
#29002=VERTEX_POINT('',#95379);
#29003=VERTEX_POINT('',#95380);
#29004=VERTEX_POINT('',#95393);
#29005=VERTEX_POINT('',#95406);
#29006=VERTEX_POINT('',#95410);
#29007=VERTEX_POINT('',#95411);
#29008=VERTEX_POINT('',#95418);
#29009=VERTEX_POINT('',#95431);
#29010=VERTEX_POINT('',#95441);
#29011=VERTEX_POINT('',#95442);
#29012=VERTEX_POINT('',#95449);
#29013=VERTEX_POINT('',#95457);
#29014=VERTEX_POINT('',#95466);
#29015=VERTEX_POINT('',#95467);
#29016=VERTEX_POINT('',#95474);
#29017=VERTEX_POINT('',#95480);
#29018=VERTEX_POINT('',#95495);
#29019=VERTEX_POINT('',#95496);
#29020=VERTEX_POINT('',#95503);
#29021=VERTEX_POINT('',#95510);
#29022=VERTEX_POINT('',#95526);
#29023=VERTEX_POINT('',#95527);
#29024=VERTEX_POINT('',#95540);
#29025=VERTEX_POINT('',#95553);
#29026=VERTEX_POINT('',#95557);
#29027=VERTEX_POINT('',#95558);
#29028=VERTEX_POINT('',#95565);
#29029=VERTEX_POINT('',#95567);
#29030=VERTEX_POINT('',#95587);
#29031=VERTEX_POINT('',#95588);
#29032=VERTEX_POINT('',#95590);
#29033=VERTEX_POINT('',#95592);
#29034=VERTEX_POINT('',#95615);
#29035=VERTEX_POINT('',#95616);
#29036=VERTEX_POINT('',#95618);
#29037=VERTEX_POINT('',#95628);
#29038=VERTEX_POINT('',#95636);
#29039=VERTEX_POINT('',#95645);
#29040=VERTEX_POINT('',#95663);
#29041=VERTEX_POINT('',#95664);
#29042=VERTEX_POINT('',#95666);
#29043=VERTEX_POINT('',#95676);
#29044=VERTEX_POINT('',#95684);
#29045=VERTEX_POINT('',#95693);
#29046=VERTEX_POINT('',#95711);
#29047=VERTEX_POINT('',#95712);
#29048=VERTEX_POINT('',#95714);
#29049=VERTEX_POINT('',#95724);
#29050=VERTEX_POINT('',#95732);
#29051=VERTEX_POINT('',#95741);
#29052=VERTEX_POINT('',#95759);
#29053=VERTEX_POINT('',#95760);
#29054=VERTEX_POINT('',#95762);
#29055=VERTEX_POINT('',#95772);
#29056=VERTEX_POINT('',#95780);
#29057=VERTEX_POINT('',#95789);
#29058=VERTEX_POINT('',#95807);
#29059=VERTEX_POINT('',#95808);
#29060=VERTEX_POINT('',#95810);
#29061=VERTEX_POINT('',#95820);
#29062=VERTEX_POINT('',#95828);
#29063=VERTEX_POINT('',#95837);
#29064=VERTEX_POINT('',#95855);
#29065=VERTEX_POINT('',#95856);
#29066=VERTEX_POINT('',#95858);
#29067=VERTEX_POINT('',#95868);
#29068=VERTEX_POINT('',#95876);
#29069=VERTEX_POINT('',#95885);
#29070=VERTEX_POINT('',#95903);
#29071=VERTEX_POINT('',#95918);
#29072=VERTEX_POINT('',#95936);
#29073=VERTEX_POINT('',#95937);
#29074=VERTEX_POINT('',#95939);
#29075=VERTEX_POINT('',#95949);
#29076=VERTEX_POINT('',#95957);
#29077=VERTEX_POINT('',#95966);
#29078=VERTEX_POINT('',#95984);
#29079=VERTEX_POINT('',#95985);
#29080=VERTEX_POINT('',#95987);
#29081=VERTEX_POINT('',#95997);
#29082=VERTEX_POINT('',#96005);
#29083=VERTEX_POINT('',#96014);
#29084=VERTEX_POINT('',#96032);
#29085=VERTEX_POINT('',#96033);
#29086=VERTEX_POINT('',#96035);
#29087=VERTEX_POINT('',#96045);
#29088=VERTEX_POINT('',#96053);
#29089=VERTEX_POINT('',#96062);
#29090=VERTEX_POINT('',#96080);
#29091=VERTEX_POINT('',#96081);
#29092=VERTEX_POINT('',#96083);
#29093=VERTEX_POINT('',#96093);
#29094=VERTEX_POINT('',#96101);
#29095=VERTEX_POINT('',#96110);
#29096=VERTEX_POINT('',#96128);
#29097=VERTEX_POINT('',#96129);
#29098=VERTEX_POINT('',#96131);
#29099=VERTEX_POINT('',#96141);
#29100=VERTEX_POINT('',#96149);
#29101=VERTEX_POINT('',#96158);
#29102=VERTEX_POINT('',#96176);
#29103=VERTEX_POINT('',#96177);
#29104=VERTEX_POINT('',#96179);
#29105=VERTEX_POINT('',#96189);
#29106=VERTEX_POINT('',#96197);
#29107=VERTEX_POINT('',#96206);
#29108=VERTEX_POINT('',#96224);
#29109=VERTEX_POINT('',#96225);
#29110=VERTEX_POINT('',#96227);
#29111=VERTEX_POINT('',#96237);
#29112=VERTEX_POINT('',#96245);
#29113=VERTEX_POINT('',#96254);
#29114=VERTEX_POINT('',#96272);
#29115=VERTEX_POINT('',#96273);
#29116=VERTEX_POINT('',#96275);
#29117=VERTEX_POINT('',#96285);
#29118=VERTEX_POINT('',#96293);
#29119=VERTEX_POINT('',#96302);
#29120=VERTEX_POINT('',#96320);
#29121=VERTEX_POINT('',#96321);
#29122=VERTEX_POINT('',#96323);
#29123=VERTEX_POINT('',#96333);
#29124=VERTEX_POINT('',#96341);
#29125=VERTEX_POINT('',#96350);
#29126=VERTEX_POINT('',#96368);
#29127=VERTEX_POINT('',#96369);
#29128=VERTEX_POINT('',#96371);
#29129=VERTEX_POINT('',#96381);
#29130=VERTEX_POINT('',#96389);
#29131=VERTEX_POINT('',#96398);
#29132=VERTEX_POINT('',#96416);
#29133=VERTEX_POINT('',#96417);
#29134=VERTEX_POINT('',#96419);
#29135=VERTEX_POINT('',#96429);
#29136=VERTEX_POINT('',#96437);
#29137=VERTEX_POINT('',#96446);
#29138=VERTEX_POINT('',#96464);
#29139=VERTEX_POINT('',#96465);
#29140=VERTEX_POINT('',#96467);
#29141=VERTEX_POINT('',#96477);
#29142=VERTEX_POINT('',#96485);
#29143=VERTEX_POINT('',#96494);
#29144=VERTEX_POINT('',#96512);
#29145=VERTEX_POINT('',#96513);
#29146=VERTEX_POINT('',#96515);
#29147=VERTEX_POINT('',#96525);
#29148=VERTEX_POINT('',#96533);
#29149=VERTEX_POINT('',#96542);
#29150=VERTEX_POINT('',#96560);
#29151=VERTEX_POINT('',#96561);
#29152=VERTEX_POINT('',#96563);
#29153=VERTEX_POINT('',#96573);
#29154=VERTEX_POINT('',#96581);
#29155=VERTEX_POINT('',#96590);
#29156=VERTEX_POINT('',#96608);
#29157=VERTEX_POINT('',#96609);
#29158=VERTEX_POINT('',#96611);
#29159=VERTEX_POINT('',#96621);
#29160=VERTEX_POINT('',#96629);
#29161=VERTEX_POINT('',#96638);
#29162=VERTEX_POINT('',#96656);
#29163=VERTEX_POINT('',#96657);
#29164=VERTEX_POINT('',#96659);
#29165=VERTEX_POINT('',#96669);
#29166=VERTEX_POINT('',#96677);
#29167=VERTEX_POINT('',#96686);
#29168=VERTEX_POINT('',#96704);
#29169=VERTEX_POINT('',#96705);
#29170=VERTEX_POINT('',#96707);
#29171=VERTEX_POINT('',#96717);
#29172=VERTEX_POINT('',#96725);
#29173=VERTEX_POINT('',#96734);
#29174=VERTEX_POINT('',#96752);
#29175=VERTEX_POINT('',#96753);
#29176=VERTEX_POINT('',#96755);
#29177=VERTEX_POINT('',#96770);
#29178=VERTEX_POINT('',#96772);
#29179=VERTEX_POINT('',#96776);
#29180=VERTEX_POINT('',#96800);
#29181=VERTEX_POINT('',#96801);
#29182=VERTEX_POINT('',#96803);
#29183=VERTEX_POINT('',#96813);
#29184=VERTEX_POINT('',#96815);
#29185=VERTEX_POINT('',#96830);
#29186=VERTEX_POINT('',#96848);
#29187=VERTEX_POINT('',#96849);
#29188=VERTEX_POINT('',#96851);
#29189=VERTEX_POINT('',#96861);
#29190=VERTEX_POINT('',#96869);
#29191=VERTEX_POINT('',#96878);
#29192=VERTEX_POINT('',#96896);
#29193=VERTEX_POINT('',#96897);
#29194=VERTEX_POINT('',#96899);
#29195=VERTEX_POINT('',#96909);
#29196=VERTEX_POINT('',#96917);
#29197=VERTEX_POINT('',#96926);
#29198=VERTEX_POINT('',#96930);
#29199=VERTEX_POINT('',#96931);
#29200=VERTEX_POINT('',#96968);
#29201=VERTEX_POINT('',#96975);
#29202=VERTEX_POINT('',#96987);
#29203=VERTEX_POINT('',#96989);
#29204=VERTEX_POINT('',#97007);
#29205=VERTEX_POINT('',#97011);
#29206=VERTEX_POINT('',#97023);
#29207=VERTEX_POINT('',#97025);
#29208=VERTEX_POINT('',#97043);
#29209=VERTEX_POINT('',#97047);
#29210=VERTEX_POINT('',#97059);
#29211=VERTEX_POINT('',#97061);
#29212=VERTEX_POINT('',#97079);
#29213=VERTEX_POINT('',#97083);
#29214=VERTEX_POINT('',#97095);
#29215=VERTEX_POINT('',#97097);
#29216=VERTEX_POINT('',#97115);
#29217=VERTEX_POINT('',#97119);
#29218=VERTEX_POINT('',#97131);
#29219=VERTEX_POINT('',#97133);
#29220=VERTEX_POINT('',#97151);
#29221=VERTEX_POINT('',#97155);
#29222=VERTEX_POINT('',#97167);
#29223=VERTEX_POINT('',#97169);
#29224=VERTEX_POINT('',#97187);
#29225=VERTEX_POINT('',#97191);
#29226=VERTEX_POINT('',#97203);
#29227=VERTEX_POINT('',#97205);
#29228=VERTEX_POINT('',#97223);
#29229=VERTEX_POINT('',#97227);
#29230=VERTEX_POINT('',#97239);
#29231=VERTEX_POINT('',#97241);
#29232=VERTEX_POINT('',#97259);
#29233=VERTEX_POINT('',#97263);
#29234=VERTEX_POINT('',#97275);
#29235=VERTEX_POINT('',#97277);
#29236=VERTEX_POINT('',#97295);
#29237=VERTEX_POINT('',#97299);
#29238=VERTEX_POINT('',#97311);
#29239=VERTEX_POINT('',#97313);
#29240=VERTEX_POINT('',#97331);
#29241=VERTEX_POINT('',#97335);
#29242=VERTEX_POINT('',#97347);
#29243=VERTEX_POINT('',#97349);
#29244=VERTEX_POINT('',#97367);
#29245=VERTEX_POINT('',#97371);
#29246=VERTEX_POINT('',#97383);
#29247=VERTEX_POINT('',#97385);
#29248=VERTEX_POINT('',#97403);
#29249=VERTEX_POINT('',#97407);
#29250=VERTEX_POINT('',#97419);
#29251=VERTEX_POINT('',#97421);
#29252=VERTEX_POINT('',#97439);
#29253=VERTEX_POINT('',#97443);
#29254=VERTEX_POINT('',#97482);
#29255=VERTEX_POINT('',#97484);
#29256=VERTEX_POINT('',#97502);
#29257=VERTEX_POINT('',#97506);
#29258=VERTEX_POINT('',#97518);
#29259=VERTEX_POINT('',#97520);
#29260=VERTEX_POINT('',#97538);
#29261=VERTEX_POINT('',#97542);
#29262=VERTEX_POINT('',#97554);
#29263=VERTEX_POINT('',#97556);
#29264=VERTEX_POINT('',#97574);
#29265=VERTEX_POINT('',#97578);
#29266=VERTEX_POINT('',#97590);
#29267=VERTEX_POINT('',#97592);
#29268=VERTEX_POINT('',#97610);
#29269=VERTEX_POINT('',#97614);
#29270=VERTEX_POINT('',#97626);
#29271=VERTEX_POINT('',#97628);
#29272=VERTEX_POINT('',#97646);
#29273=VERTEX_POINT('',#97650);
#29274=VERTEX_POINT('',#97662);
#29275=VERTEX_POINT('',#97664);
#29276=VERTEX_POINT('',#97682);
#29277=VERTEX_POINT('',#97686);
#29278=VERTEX_POINT('',#97698);
#29279=VERTEX_POINT('',#97700);
#29280=VERTEX_POINT('',#97718);
#29281=VERTEX_POINT('',#97722);
#29282=VERTEX_POINT('',#97734);
#29283=VERTEX_POINT('',#97736);
#29284=VERTEX_POINT('',#97754);
#29285=VERTEX_POINT('',#97758);
#29286=VERTEX_POINT('',#97770);
#29287=VERTEX_POINT('',#97772);
#29288=VERTEX_POINT('',#97790);
#29289=VERTEX_POINT('',#97794);
#29290=VERTEX_POINT('',#97806);
#29291=VERTEX_POINT('',#97808);
#29292=VERTEX_POINT('',#97826);
#29293=VERTEX_POINT('',#97830);
#29294=VERTEX_POINT('',#97842);
#29295=VERTEX_POINT('',#97844);
#29296=VERTEX_POINT('',#97862);
#29297=VERTEX_POINT('',#97866);
#29298=VERTEX_POINT('',#97878);
#29299=VERTEX_POINT('',#97880);
#29300=VERTEX_POINT('',#97898);
#29301=VERTEX_POINT('',#97902);
#29302=VERTEX_POINT('',#97914);
#29303=VERTEX_POINT('',#97916);
#29304=VERTEX_POINT('',#97934);
#29305=VERTEX_POINT('',#97938);
#29306=VERTEX_POINT('',#97950);
#29307=VERTEX_POINT('',#97952);
#29308=VERTEX_POINT('',#97970);
#29309=VERTEX_POINT('',#97974);
#29310=VERTEX_POINT('',#97978);
#29311=VERTEX_POINT('',#97980);
#29312=VERTEX_POINT('',#97999);
#29313=VERTEX_POINT('',#98021);
#29314=VERTEX_POINT('',#98054);
#29315=VERTEX_POINT('',#98087);
#29316=VERTEX_POINT('',#98120);
#29317=VERTEX_POINT('',#98153);
#29318=VERTEX_POINT('',#98186);
#29319=VERTEX_POINT('',#98219);
#29320=VERTEX_POINT('',#98252);
#29321=VERTEX_POINT('',#98287);
#29322=VERTEX_POINT('',#98320);
#29323=VERTEX_POINT('',#98353);
#29324=VERTEX_POINT('',#98386);
#29325=VERTEX_POINT('',#98419);
#29326=VERTEX_POINT('',#98454);
#29327=VERTEX_POINT('',#98489);
#29328=VERTEX_POINT('',#98522);
#29329=VERTEX_POINT('',#98555);
#29330=VERTEX_POINT('',#98590);
#29331=VERTEX_POINT('',#98623);
#29332=VERTEX_POINT('',#98656);
#29333=VERTEX_POINT('',#98689);
#29334=VERTEX_POINT('',#98722);
#29335=VERTEX_POINT('',#98755);
#29336=VERTEX_POINT('',#98790);
#29337=VERTEX_POINT('',#98825);
#29338=VERTEX_POINT('',#98860);
#29339=VERTEX_POINT('',#98893);
#29340=VERTEX_POINT('',#98926);
#29341=VERTEX_POINT('',#98976);
#29342=VERTEX_POINT('',#98990);
#29343=VERTEX_POINT('',#99015);
#29344=VERTEX_POINT('',#99040);
#29345=VERTEX_POINT('',#99065);
#29346=VERTEX_POINT('',#99090);
#29347=VERTEX_POINT('',#99115);
#29348=VERTEX_POINT('',#99140);
#29349=VERTEX_POINT('',#99165);
#29350=VERTEX_POINT('',#99190);
#29351=VERTEX_POINT('',#99215);
#29352=VERTEX_POINT('',#99240);
#29353=VERTEX_POINT('',#99265);
#29354=VERTEX_POINT('',#99290);
#29355=VERTEX_POINT('',#99315);
#29356=VERTEX_POINT('',#99340);
#29357=VERTEX_POINT('',#99365);
#29358=VERTEX_POINT('',#99390);
#29359=VERTEX_POINT('',#99415);
#29360=VERTEX_POINT('',#99440);
#29361=VERTEX_POINT('',#99465);
#29362=VERTEX_POINT('',#99490);
#29363=VERTEX_POINT('',#99515);
#29364=VERTEX_POINT('',#99540);
#29365=VERTEX_POINT('',#99565);
#29366=VERTEX_POINT('',#99590);
#29367=VERTEX_POINT('',#99615);
#29368=VERTEX_POINT('',#99640);
#29369=VERTEX_POINT('',#99665);
#29370=VERTEX_POINT('',#99697);
#29371=VERTEX_POINT('',#99698);
#29372=VERTEX_POINT('',#99708);
#29373=VERTEX_POINT('',#99710);
#29374=VERTEX_POINT('',#99746);
#29375=VERTEX_POINT('',#99747);
#29376=VERTEX_POINT('',#99757);
#29377=VERTEX_POINT('',#99759);
#29378=VERTEX_POINT('',#99795);
#29379=VERTEX_POINT('',#99796);
#29380=VERTEX_POINT('',#99806);
#29381=VERTEX_POINT('',#99808);
#29382=VERTEX_POINT('',#99844);
#29383=VERTEX_POINT('',#99845);
#29384=VERTEX_POINT('',#99855);
#29385=VERTEX_POINT('',#99857);
#29386=VERTEX_POINT('',#99893);
#29387=VERTEX_POINT('',#99894);
#29388=VERTEX_POINT('',#99904);
#29389=VERTEX_POINT('',#99906);
#29390=VERTEX_POINT('',#99942);
#29391=VERTEX_POINT('',#99943);
#29392=VERTEX_POINT('',#99953);
#29393=VERTEX_POINT('',#99955);
#29394=VERTEX_POINT('',#99991);
#29395=VERTEX_POINT('',#99992);
#29396=VERTEX_POINT('',#100002);
#29397=VERTEX_POINT('',#100004);
#29398=VERTEX_POINT('',#100040);
#29399=VERTEX_POINT('',#100041);
#29400=VERTEX_POINT('',#100051);
#29401=VERTEX_POINT('',#100053);
#29402=VERTEX_POINT('',#100089);
#29403=VERTEX_POINT('',#100090);
#29404=VERTEX_POINT('',#100100);
#29405=VERTEX_POINT('',#100102);
#29406=VERTEX_POINT('',#100138);
#29407=VERTEX_POINT('',#100139);
#29408=VERTEX_POINT('',#100149);
#29409=VERTEX_POINT('',#100151);
#29410=VERTEX_POINT('',#100187);
#29411=VERTEX_POINT('',#100188);
#29412=VERTEX_POINT('',#100198);
#29413=VERTEX_POINT('',#100200);
#29414=VERTEX_POINT('',#100236);
#29415=VERTEX_POINT('',#100237);
#29416=VERTEX_POINT('',#100247);
#29417=VERTEX_POINT('',#100249);
#29418=VERTEX_POINT('',#100285);
#29419=VERTEX_POINT('',#100286);
#29420=VERTEX_POINT('',#100296);
#29421=VERTEX_POINT('',#100298);
#29422=VERTEX_POINT('',#100334);
#29423=VERTEX_POINT('',#100335);
#29424=VERTEX_POINT('',#100345);
#29425=VERTEX_POINT('',#100347);
#29426=VERTEX_POINT('',#100411);
#29427=VERTEX_POINT('',#100412);
#29428=VERTEX_POINT('',#100422);
#29429=VERTEX_POINT('',#100424);
#29430=VERTEX_POINT('',#100460);
#29431=VERTEX_POINT('',#100461);
#29432=VERTEX_POINT('',#100471);
#29433=VERTEX_POINT('',#100473);
#29434=VERTEX_POINT('',#100509);
#29435=VERTEX_POINT('',#100510);
#29436=VERTEX_POINT('',#100520);
#29437=VERTEX_POINT('',#100522);
#29438=VERTEX_POINT('',#100558);
#29439=VERTEX_POINT('',#100559);
#29440=VERTEX_POINT('',#100569);
#29441=VERTEX_POINT('',#100571);
#29442=VERTEX_POINT('',#100607);
#29443=VERTEX_POINT('',#100608);
#29444=VERTEX_POINT('',#100618);
#29445=VERTEX_POINT('',#100620);
#29446=VERTEX_POINT('',#100656);
#29447=VERTEX_POINT('',#100657);
#29448=VERTEX_POINT('',#100667);
#29449=VERTEX_POINT('',#100669);
#29450=VERTEX_POINT('',#100705);
#29451=VERTEX_POINT('',#100706);
#29452=VERTEX_POINT('',#100716);
#29453=VERTEX_POINT('',#100718);
#29454=VERTEX_POINT('',#100754);
#29455=VERTEX_POINT('',#100755);
#29456=VERTEX_POINT('',#100765);
#29457=VERTEX_POINT('',#100767);
#29458=VERTEX_POINT('',#100803);
#29459=VERTEX_POINT('',#100804);
#29460=VERTEX_POINT('',#100814);
#29461=VERTEX_POINT('',#100816);
#29462=VERTEX_POINT('',#100852);
#29463=VERTEX_POINT('',#100853);
#29464=VERTEX_POINT('',#100876);
#29465=VERTEX_POINT('',#100886);
#29466=VERTEX_POINT('',#100901);
#29467=VERTEX_POINT('',#100903);
#29468=VERTEX_POINT('',#100912);
#29469=VERTEX_POINT('',#100920);
#29470=VERTEX_POINT('',#100950);
#29471=VERTEX_POINT('',#100951);
#29472=VERTEX_POINT('',#100961);
#29473=VERTEX_POINT('',#100963);
#29474=VERTEX_POINT('',#100999);
#29475=VERTEX_POINT('',#101000);
#29476=VERTEX_POINT('',#101010);
#29477=VERTEX_POINT('',#101012);
#29478=VERTEX_POINT('',#101048);
#29479=VERTEX_POINT('',#101049);
#29480=VERTEX_POINT('',#101059);
#29481=VERTEX_POINT('',#101061);
#29482=VERTEX_POINT('',#101101);
#29483=VERTEX_POINT('',#101103);
#29484=VERTEX_POINT('',#101121);
#29485=VERTEX_POINT('',#101125);
#29486=VERTEX_POINT('',#101142);
#29487=VERTEX_POINT('',#101144);
#29488=VERTEX_POINT('',#101162);
#29489=VERTEX_POINT('',#101166);
#29490=VERTEX_POINT('',#101183);
#29491=VERTEX_POINT('',#101185);
#29492=VERTEX_POINT('',#101203);
#29493=VERTEX_POINT('',#101207);
#29494=VERTEX_POINT('',#101224);
#29495=VERTEX_POINT('',#101226);
#29496=VERTEX_POINT('',#101244);
#29497=VERTEX_POINT('',#101248);
#29498=VERTEX_POINT('',#101265);
#29499=VERTEX_POINT('',#101267);
#29500=VERTEX_POINT('',#101285);
#29501=VERTEX_POINT('',#101289);
#29502=VERTEX_POINT('',#101306);
#29503=VERTEX_POINT('',#101308);
#29504=VERTEX_POINT('',#101326);
#29505=VERTEX_POINT('',#101330);
#29506=VERTEX_POINT('',#101347);
#29507=VERTEX_POINT('',#101349);
#29508=VERTEX_POINT('',#101367);
#29509=VERTEX_POINT('',#101371);
#29510=VERTEX_POINT('',#101388);
#29511=VERTEX_POINT('',#101390);
#29512=VERTEX_POINT('',#101408);
#29513=VERTEX_POINT('',#101412);
#29514=VERTEX_POINT('',#101429);
#29515=VERTEX_POINT('',#101431);
#29516=VERTEX_POINT('',#101449);
#29517=VERTEX_POINT('',#101453);
#29518=VERTEX_POINT('',#101470);
#29519=VERTEX_POINT('',#101472);
#29520=VERTEX_POINT('',#101490);
#29521=VERTEX_POINT('',#101494);
#29522=VERTEX_POINT('',#101511);
#29523=VERTEX_POINT('',#101513);
#29524=VERTEX_POINT('',#101531);
#29525=VERTEX_POINT('',#101535);
#29526=VERTEX_POINT('',#101552);
#29527=VERTEX_POINT('',#101554);
#29528=VERTEX_POINT('',#101572);
#29529=VERTEX_POINT('',#101576);
#29530=VERTEX_POINT('',#101593);
#29531=VERTEX_POINT('',#101595);
#29532=VERTEX_POINT('',#101613);
#29533=VERTEX_POINT('',#101617);
#29534=VERTEX_POINT('',#101634);
#29535=VERTEX_POINT('',#101636);
#29536=VERTEX_POINT('',#101654);
#29537=VERTEX_POINT('',#101658);
#29538=VERTEX_POINT('',#101675);
#29539=VERTEX_POINT('',#101677);
#29540=VERTEX_POINT('',#101695);
#29541=VERTEX_POINT('',#101699);
#29542=VERTEX_POINT('',#101716);
#29543=VERTEX_POINT('',#101718);
#29544=VERTEX_POINT('',#101736);
#29545=VERTEX_POINT('',#101740);
#29546=VERTEX_POINT('',#101757);
#29547=VERTEX_POINT('',#101759);
#29548=VERTEX_POINT('',#101777);
#29549=VERTEX_POINT('',#101781);
#29550=VERTEX_POINT('',#101798);
#29551=VERTEX_POINT('',#101800);
#29552=VERTEX_POINT('',#101818);
#29553=VERTEX_POINT('',#101822);
#29554=VERTEX_POINT('',#101839);
#29555=VERTEX_POINT('',#101841);
#29556=VERTEX_POINT('',#101859);
#29557=VERTEX_POINT('',#101863);
#29558=VERTEX_POINT('',#101880);
#29559=VERTEX_POINT('',#101882);
#29560=VERTEX_POINT('',#101900);
#29561=VERTEX_POINT('',#101904);
#29562=VERTEX_POINT('',#101921);
#29563=VERTEX_POINT('',#101923);
#29564=VERTEX_POINT('',#101941);
#29565=VERTEX_POINT('',#101945);
#29566=VERTEX_POINT('',#101990);
#29567=VERTEX_POINT('',#101992);
#29568=VERTEX_POINT('',#102010);
#29569=VERTEX_POINT('',#102014);
#29570=VERTEX_POINT('',#102031);
#29571=VERTEX_POINT('',#102033);
#29572=VERTEX_POINT('',#102051);
#29573=VERTEX_POINT('',#102055);
#29574=VERTEX_POINT('',#102072);
#29575=VERTEX_POINT('',#102074);
#29576=VERTEX_POINT('',#102092);
#29577=VERTEX_POINT('',#102096);
#29578=VERTEX_POINT('',#102113);
#29579=VERTEX_POINT('',#102115);
#29580=VERTEX_POINT('',#102133);
#29581=VERTEX_POINT('',#102137);
#29582=VERTEX_POINT('',#102154);
#29583=VERTEX_POINT('',#102156);
#29584=VERTEX_POINT('',#102174);
#29585=VERTEX_POINT('',#102178);
#29586=VERTEX_POINT('',#102195);
#29587=VERTEX_POINT('',#102197);
#29588=VERTEX_POINT('',#102215);
#29589=VERTEX_POINT('',#102219);
#29590=VERTEX_POINT('',#102236);
#29591=VERTEX_POINT('',#102238);
#29592=VERTEX_POINT('',#102256);
#29593=VERTEX_POINT('',#102260);
#29594=VERTEX_POINT('',#102273);
#29595=VERTEX_POINT('',#102308);
#29596=VERTEX_POINT('',#102343);
#29597=VERTEX_POINT('',#102378);
#29598=VERTEX_POINT('',#102413);
#29599=VERTEX_POINT('',#102448);
#29600=VERTEX_POINT('',#102483);
#29601=VERTEX_POINT('',#102518);
#29602=VERTEX_POINT('',#102553);
#29603=VERTEX_POINT('',#102588);
#29604=VERTEX_POINT('',#102623);
#29605=VERTEX_POINT('',#102658);
#29606=VERTEX_POINT('',#102693);
#29607=VERTEX_POINT('',#102728);
#29608=VERTEX_POINT('',#102763);
#29609=VERTEX_POINT('',#102798);
#29610=VERTEX_POINT('',#102833);
#29611=VERTEX_POINT('',#102868);
#29612=VERTEX_POINT('',#102903);
#29613=VERTEX_POINT('',#102938);
#29614=VERTEX_POINT('',#102973);
#29615=VERTEX_POINT('',#103008);
#29616=VERTEX_POINT('',#103043);
#29617=VERTEX_POINT('',#103078);
#29618=VERTEX_POINT('',#103113);
#29619=VERTEX_POINT('',#103148);
#29620=VERTEX_POINT('',#103183);
#29621=VERTEX_POINT('',#103218);
#29622=VERTEX_POINT('',#103253);
#29623=VERTEX_POINT('',#103288);
#29624=VERTEX_POINT('',#103319);
#29625=VERTEX_POINT('',#103350);
#29626=VERTEX_POINT('',#103381);
#29627=VERTEX_POINT('',#103412);
#29628=VERTEX_POINT('',#103443);
#29629=VERTEX_POINT('',#103474);
#29630=VERTEX_POINT('',#103505);
#29631=VERTEX_POINT('',#103536);
#29632=VERTEX_POINT('',#103567);
#29633=VERTEX_POINT('',#103598);
#29634=VERTEX_POINT('',#103629);
#29635=VERTEX_POINT('',#103660);
#29636=VERTEX_POINT('',#103691);
#29637=VERTEX_POINT('',#103722);
#29638=VERTEX_POINT('',#103753);
#29639=VERTEX_POINT('',#103784);
#29640=VERTEX_POINT('',#103815);
#29641=VERTEX_POINT('',#103846);
#29642=VERTEX_POINT('',#103877);
#29643=VERTEX_POINT('',#103908);
#29644=VERTEX_POINT('',#103939);
#29645=VERTEX_POINT('',#103970);
#29646=VERTEX_POINT('',#104001);
#29647=VERTEX_POINT('',#104032);
#29648=VERTEX_POINT('',#104063);
#29649=VERTEX_POINT('',#104094);
#29650=VERTEX_POINT('',#104125);
#29651=VERTEX_POINT('',#104156);
#29652=VERTEX_POINT('',#104187);
#29653=VERTEX_POINT('',#104188);
#29654=VERTEX_POINT('',#104211);
#29655=VERTEX_POINT('',#104212);
#29656=VERTEX_POINT('',#104228);
#29657=VERTEX_POINT('',#104230);
#29658=VERTEX_POINT('',#104254);
#29659=VERTEX_POINT('',#104255);
#29660=VERTEX_POINT('',#104271);
#29661=VERTEX_POINT('',#104273);
#29662=VERTEX_POINT('',#104297);
#29663=VERTEX_POINT('',#104298);
#29664=VERTEX_POINT('',#104314);
#29665=VERTEX_POINT('',#104316);
#29666=VERTEX_POINT('',#104340);
#29667=VERTEX_POINT('',#104341);
#29668=VERTEX_POINT('',#104357);
#29669=VERTEX_POINT('',#104359);
#29670=VERTEX_POINT('',#104383);
#29671=VERTEX_POINT('',#104384);
#29672=VERTEX_POINT('',#104400);
#29673=VERTEX_POINT('',#104402);
#29674=VERTEX_POINT('',#104426);
#29675=VERTEX_POINT('',#104427);
#29676=VERTEX_POINT('',#104443);
#29677=VERTEX_POINT('',#104445);
#29678=VERTEX_POINT('',#104497);
#29679=VERTEX_POINT('',#104498);
#29680=VERTEX_POINT('',#104514);
#29681=VERTEX_POINT('',#104516);
#29682=VERTEX_POINT('',#104540);
#29683=VERTEX_POINT('',#104541);
#29684=VERTEX_POINT('',#104557);
#29685=VERTEX_POINT('',#104559);
#29686=VERTEX_POINT('',#104583);
#29687=VERTEX_POINT('',#104584);
#29688=VERTEX_POINT('',#104600);
#29689=VERTEX_POINT('',#104602);
#29690=VERTEX_POINT('',#104626);
#29691=VERTEX_POINT('',#104627);
#29692=VERTEX_POINT('',#104643);
#29693=VERTEX_POINT('',#104645);
#29694=VERTEX_POINT('',#104669);
#29695=VERTEX_POINT('',#104670);
#29696=VERTEX_POINT('',#104686);
#29697=VERTEX_POINT('',#104688);
#29698=VERTEX_POINT('',#104712);
#29699=VERTEX_POINT('',#104713);
#29700=VERTEX_POINT('',#104729);
#29701=VERTEX_POINT('',#104731);
#29702=VERTEX_POINT('',#104755);
#29703=VERTEX_POINT('',#104756);
#29704=VERTEX_POINT('',#104772);
#29705=VERTEX_POINT('',#104774);
#29706=VERTEX_POINT('',#104798);
#29707=VERTEX_POINT('',#104799);
#29708=VERTEX_POINT('',#104815);
#29709=VERTEX_POINT('',#104817);
#29710=VERTEX_POINT('',#104841);
#29711=VERTEX_POINT('',#104842);
#29712=VERTEX_POINT('',#104858);
#29713=VERTEX_POINT('',#104860);
#29714=VERTEX_POINT('',#104884);
#29715=VERTEX_POINT('',#104885);
#29716=VERTEX_POINT('',#104901);
#29717=VERTEX_POINT('',#104903);
#29718=VERTEX_POINT('',#104927);
#29719=VERTEX_POINT('',#104928);
#29720=VERTEX_POINT('',#104944);
#29721=VERTEX_POINT('',#104946);
#29722=VERTEX_POINT('',#104970);
#29723=VERTEX_POINT('',#104971);
#29724=VERTEX_POINT('',#104987);
#29725=VERTEX_POINT('',#104989);
#29726=VERTEX_POINT('',#105013);
#29727=VERTEX_POINT('',#105014);
#29728=VERTEX_POINT('',#105030);
#29729=VERTEX_POINT('',#105032);
#29730=VERTEX_POINT('',#105056);
#29731=VERTEX_POINT('',#105057);
#29732=VERTEX_POINT('',#105073);
#29733=VERTEX_POINT('',#105075);
#29734=VERTEX_POINT('',#105099);
#29735=VERTEX_POINT('',#105100);
#29736=VERTEX_POINT('',#105116);
#29737=VERTEX_POINT('',#105118);
#29738=VERTEX_POINT('',#105142);
#29739=VERTEX_POINT('',#105143);
#29740=VERTEX_POINT('',#105159);
#29741=VERTEX_POINT('',#105161);
#29742=VERTEX_POINT('',#105185);
#29743=VERTEX_POINT('',#105186);
#29744=VERTEX_POINT('',#105207);
#29745=VERTEX_POINT('',#105211);
#29746=VERTEX_POINT('',#105228);
#29747=VERTEX_POINT('',#105230);
#29748=VERTEX_POINT('',#105245);
#29749=VERTEX_POINT('',#105247);
#29750=VERTEX_POINT('',#105271);
#29751=VERTEX_POINT('',#105272);
#29752=VERTEX_POINT('',#105288);
#29753=VERTEX_POINT('',#105290);
#29754=VERTEX_POINT('',#105314);
#29755=VERTEX_POINT('',#105315);
#29756=VERTEX_POINT('',#105331);
#29757=VERTEX_POINT('',#105333);
#29758=VERTEX_POINT('',#105357);
#29759=VERTEX_POINT('',#105358);
#29760=VERTEX_POINT('',#105374);
#29761=VERTEX_POINT('',#105376);
#29762=VERTEX_POINT('',#105387);
#29763=VERTEX_POINT('',#105388);
#29764=VERTEX_POINT('',#105423);
#29765=VERTEX_POINT('',#105430);
#29766=VERTEX_POINT('',#105447);
#29767=VERTEX_POINT('',#105449);
#29768=VERTEX_POINT('',#105473);
#29769=VERTEX_POINT('',#105477);
#29770=VERTEX_POINT('',#105494);
#29771=VERTEX_POINT('',#105496);
#29772=VERTEX_POINT('',#105520);
#29773=VERTEX_POINT('',#105524);
#29774=VERTEX_POINT('',#105541);
#29775=VERTEX_POINT('',#105543);
#29776=VERTEX_POINT('',#105567);
#29777=VERTEX_POINT('',#105571);
#29778=VERTEX_POINT('',#105588);
#29779=VERTEX_POINT('',#105590);
#29780=VERTEX_POINT('',#105614);
#29781=VERTEX_POINT('',#105618);
#29782=VERTEX_POINT('',#105635);
#29783=VERTEX_POINT('',#105637);
#29784=VERTEX_POINT('',#105661);
#29785=VERTEX_POINT('',#105665);
#29786=VERTEX_POINT('',#105682);
#29787=VERTEX_POINT('',#105684);
#29788=VERTEX_POINT('',#105708);
#29789=VERTEX_POINT('',#105712);
#29790=VERTEX_POINT('',#105729);
#29791=VERTEX_POINT('',#105731);
#29792=VERTEX_POINT('',#105755);
#29793=VERTEX_POINT('',#105759);
#29794=VERTEX_POINT('',#105776);
#29795=VERTEX_POINT('',#105778);
#29796=VERTEX_POINT('',#105802);
#29797=VERTEX_POINT('',#105806);
#29798=VERTEX_POINT('',#105823);
#29799=VERTEX_POINT('',#105825);
#29800=VERTEX_POINT('',#105849);
#29801=VERTEX_POINT('',#105853);
#29802=VERTEX_POINT('',#105870);
#29803=VERTEX_POINT('',#105872);
#29804=VERTEX_POINT('',#105896);
#29805=VERTEX_POINT('',#105900);
#29806=VERTEX_POINT('',#105917);
#29807=VERTEX_POINT('',#105919);
#29808=VERTEX_POINT('',#105943);
#29809=VERTEX_POINT('',#105947);
#29810=VERTEX_POINT('',#105964);
#29811=VERTEX_POINT('',#105966);
#29812=VERTEX_POINT('',#105990);
#29813=VERTEX_POINT('',#105994);
#29814=VERTEX_POINT('',#106011);
#29815=VERTEX_POINT('',#106013);
#29816=VERTEX_POINT('',#106037);
#29817=VERTEX_POINT('',#106041);
#29818=VERTEX_POINT('',#106090);
#29819=VERTEX_POINT('',#106092);
#29820=VERTEX_POINT('',#106116);
#29821=VERTEX_POINT('',#106120);
#29822=VERTEX_POINT('',#106137);
#29823=VERTEX_POINT('',#106139);
#29824=VERTEX_POINT('',#106163);
#29825=VERTEX_POINT('',#106167);
#29826=VERTEX_POINT('',#106184);
#29827=VERTEX_POINT('',#106186);
#29828=VERTEX_POINT('',#106210);
#29829=VERTEX_POINT('',#106214);
#29830=VERTEX_POINT('',#106231);
#29831=VERTEX_POINT('',#106233);
#29832=VERTEX_POINT('',#106257);
#29833=VERTEX_POINT('',#106261);
#29834=VERTEX_POINT('',#106278);
#29835=VERTEX_POINT('',#106280);
#29836=VERTEX_POINT('',#106304);
#29837=VERTEX_POINT('',#106308);
#29838=VERTEX_POINT('',#106325);
#29839=VERTEX_POINT('',#106327);
#29840=VERTEX_POINT('',#106351);
#29841=VERTEX_POINT('',#106355);
#29842=VERTEX_POINT('',#106372);
#29843=VERTEX_POINT('',#106374);
#29844=VERTEX_POINT('',#106398);
#29845=VERTEX_POINT('',#106402);
#29846=VERTEX_POINT('',#106419);
#29847=VERTEX_POINT('',#106421);
#29848=VERTEX_POINT('',#106445);
#29849=VERTEX_POINT('',#106449);
#29850=VERTEX_POINT('',#106466);
#29851=VERTEX_POINT('',#106468);
#29852=VERTEX_POINT('',#106492);
#29853=VERTEX_POINT('',#106496);
#29854=VERTEX_POINT('',#106513);
#29855=VERTEX_POINT('',#106515);
#29856=VERTEX_POINT('',#106539);
#29857=VERTEX_POINT('',#106543);
#29858=VERTEX_POINT('',#106560);
#29859=VERTEX_POINT('',#106562);
#29860=VERTEX_POINT('',#106586);
#29861=VERTEX_POINT('',#106590);
#29862=VERTEX_POINT('',#106607);
#29863=VERTEX_POINT('',#106609);
#29864=VERTEX_POINT('',#106633);
#29865=VERTEX_POINT('',#106637);
#29866=VERTEX_POINT('',#106654);
#29867=VERTEX_POINT('',#106656);
#29868=VERTEX_POINT('',#106680);
#29869=VERTEX_POINT('',#106684);
#29870=VERTEX_POINT('',#106701);
#29871=VERTEX_POINT('',#106703);
#29872=VERTEX_POINT('',#106727);
#29873=VERTEX_POINT('',#106731);
#29874=VERTEX_POINT('',#106735);
#29875=VERTEX_POINT('',#106743);
#29876=VERTEX_POINT('',#106767);
#29877=VERTEX_POINT('',#106790);
#29878=VERTEX_POINT('',#106820);
#29879=VERTEX_POINT('',#106850);
#29880=VERTEX_POINT('',#106880);
#29881=VERTEX_POINT('',#106910);
#29882=VERTEX_POINT('',#106940);
#29883=VERTEX_POINT('',#106970);
#29884=VERTEX_POINT('',#107000);
#29885=VERTEX_POINT('',#107030);
#29886=VERTEX_POINT('',#107060);
#29887=VERTEX_POINT('',#107090);
#29888=VERTEX_POINT('',#107120);
#29889=VERTEX_POINT('',#107150);
#29890=VERTEX_POINT('',#107180);
#29891=VERTEX_POINT('',#107210);
#29892=VERTEX_POINT('',#107240);
#29893=VERTEX_POINT('',#107270);
#29894=VERTEX_POINT('',#107300);
#29895=VERTEX_POINT('',#107330);
#29896=VERTEX_POINT('',#107360);
#29897=VERTEX_POINT('',#107390);
#29898=VERTEX_POINT('',#107420);
#29899=VERTEX_POINT('',#107450);
#29900=VERTEX_POINT('',#107480);
#29901=VERTEX_POINT('',#107510);
#29902=VERTEX_POINT('',#107540);
#29903=VERTEX_POINT('',#107570);
#29904=VERTEX_POINT('',#107600);
#29905=VERTEX_POINT('',#107637);
#29906=VERTEX_POINT('',#107655);
#29907=VERTEX_POINT('',#107689);
#29908=VERTEX_POINT('',#107723);
#29909=VERTEX_POINT('',#107757);
#29910=VERTEX_POINT('',#107791);
#29911=VERTEX_POINT('',#107825);
#29912=VERTEX_POINT('',#107859);
#29913=VERTEX_POINT('',#107893);
#29914=VERTEX_POINT('',#107927);
#29915=VERTEX_POINT('',#107961);
#29916=VERTEX_POINT('',#107995);
#29917=VERTEX_POINT('',#108029);
#29918=VERTEX_POINT('',#108063);
#29919=VERTEX_POINT('',#108097);
#29920=VERTEX_POINT('',#108131);
#29921=VERTEX_POINT('',#108165);
#29922=VERTEX_POINT('',#108199);
#29923=VERTEX_POINT('',#108233);
#29924=VERTEX_POINT('',#108267);
#29925=VERTEX_POINT('',#108301);
#29926=VERTEX_POINT('',#108335);
#29927=VERTEX_POINT('',#108369);
#29928=VERTEX_POINT('',#108403);
#29929=VERTEX_POINT('',#108437);
#29930=VERTEX_POINT('',#108471);
#29931=VERTEX_POINT('',#108505);
#29932=VERTEX_POINT('',#108539);
#29933=VERTEX_POINT('',#108573);
#29934=VERTEX_POINT('',#108622);
#29935=VERTEX_POINT('',#108623);
#29936=VERTEX_POINT('',#108633);
#29937=VERTEX_POINT('',#108635);
#29938=VERTEX_POINT('',#108658);
#29939=VERTEX_POINT('',#108659);
#29940=VERTEX_POINT('',#108669);
#29941=VERTEX_POINT('',#108671);
#29942=VERTEX_POINT('',#108694);
#29943=VERTEX_POINT('',#108695);
#29944=VERTEX_POINT('',#108705);
#29945=VERTEX_POINT('',#108707);
#29946=VERTEX_POINT('',#108730);
#29947=VERTEX_POINT('',#108731);
#29948=VERTEX_POINT('',#108741);
#29949=VERTEX_POINT('',#108743);
#29950=VERTEX_POINT('',#108766);
#29951=VERTEX_POINT('',#108767);
#29952=VERTEX_POINT('',#108777);
#29953=VERTEX_POINT('',#108779);
#29954=VERTEX_POINT('',#108802);
#29955=VERTEX_POINT('',#108803);
#29956=VERTEX_POINT('',#108813);
#29957=VERTEX_POINT('',#108815);
#29958=VERTEX_POINT('',#108838);
#29959=VERTEX_POINT('',#108839);
#29960=VERTEX_POINT('',#108849);
#29961=VERTEX_POINT('',#108851);
#29962=VERTEX_POINT('',#108874);
#29963=VERTEX_POINT('',#108875);
#29964=VERTEX_POINT('',#108885);
#29965=VERTEX_POINT('',#108887);
#29966=VERTEX_POINT('',#108910);
#29967=VERTEX_POINT('',#108911);
#29968=VERTEX_POINT('',#108921);
#29969=VERTEX_POINT('',#108923);
#29970=VERTEX_POINT('',#108946);
#29971=VERTEX_POINT('',#108947);
#29972=VERTEX_POINT('',#108957);
#29973=VERTEX_POINT('',#108959);
#29974=VERTEX_POINT('',#108982);
#29975=VERTEX_POINT('',#108983);
#29976=VERTEX_POINT('',#108993);
#29977=VERTEX_POINT('',#108995);
#29978=VERTEX_POINT('',#109018);
#29979=VERTEX_POINT('',#109019);
#29980=VERTEX_POINT('',#109029);
#29981=VERTEX_POINT('',#109031);
#29982=VERTEX_POINT('',#109054);
#29983=VERTEX_POINT('',#109055);
#29984=VERTEX_POINT('',#109065);
#29985=VERTEX_POINT('',#109067);
#29986=VERTEX_POINT('',#109090);
#29987=VERTEX_POINT('',#109091);
#29988=VERTEX_POINT('',#109101);
#29989=VERTEX_POINT('',#109103);
#29990=VERTEX_POINT('',#109153);
#29991=VERTEX_POINT('',#109154);
#29992=VERTEX_POINT('',#109164);
#29993=VERTEX_POINT('',#109166);
#29994=VERTEX_POINT('',#109189);
#29995=VERTEX_POINT('',#109190);
#29996=VERTEX_POINT('',#109200);
#29997=VERTEX_POINT('',#109202);
#29998=VERTEX_POINT('',#109225);
#29999=VERTEX_POINT('',#109226);
#30000=VERTEX_POINT('',#109236);
#30001=VERTEX_POINT('',#109238);
#30002=VERTEX_POINT('',#109261);
#30003=VERTEX_POINT('',#109262);
#30004=VERTEX_POINT('',#109272);
#30005=VERTEX_POINT('',#109274);
#30006=VERTEX_POINT('',#109297);
#30007=VERTEX_POINT('',#109298);
#30008=VERTEX_POINT('',#109308);
#30009=VERTEX_POINT('',#109310);
#30010=VERTEX_POINT('',#109333);
#30011=VERTEX_POINT('',#109334);
#30012=VERTEX_POINT('',#109344);
#30013=VERTEX_POINT('',#109346);
#30014=VERTEX_POINT('',#109369);
#30015=VERTEX_POINT('',#109370);
#30016=VERTEX_POINT('',#109380);
#30017=VERTEX_POINT('',#109382);
#30018=VERTEX_POINT('',#109405);
#30019=VERTEX_POINT('',#109406);
#30020=VERTEX_POINT('',#109416);
#30021=VERTEX_POINT('',#109418);
#30022=VERTEX_POINT('',#109441);
#30023=VERTEX_POINT('',#109442);
#30024=VERTEX_POINT('',#109460);
#30025=VERTEX_POINT('',#109464);
#30026=VERTEX_POINT('',#109477);
#30027=VERTEX_POINT('',#109479);
#30028=VERTEX_POINT('',#109488);
#30029=VERTEX_POINT('',#109490);
#30030=VERTEX_POINT('',#109513);
#30031=VERTEX_POINT('',#109514);
#30032=VERTEX_POINT('',#109524);
#30033=VERTEX_POINT('',#109526);
#30034=VERTEX_POINT('',#109549);
#30035=VERTEX_POINT('',#109550);
#30036=VERTEX_POINT('',#109560);
#30037=VERTEX_POINT('',#109562);
#30038=VERTEX_POINT('',#109585);
#30039=VERTEX_POINT('',#109586);
#30040=VERTEX_POINT('',#109596);
#30041=VERTEX_POINT('',#109598);
#30042=VERTEX_POINT('',#109621);
#30043=VERTEX_POINT('',#109622);
#30044=VERTEX_POINT('',#109632);
#30045=VERTEX_POINT('',#109634);
#30046=VERTEX_POINT('',#109653);
#30047=VERTEX_POINT('',#109655);
#30048=VERTEX_POINT('',#109677);
#30049=VERTEX_POINT('',#109687);
#30050=VERTEX_POINT('',#109696);
#30051=VERTEX_POINT('',#109698);
#30052=VERTEX_POINT('',#109720);
#30053=VERTEX_POINT('',#109730);
#30054=VERTEX_POINT('',#109739);
#30055=VERTEX_POINT('',#109741);
#30056=VERTEX_POINT('',#109763);
#30057=VERTEX_POINT('',#109773);
#30058=VERTEX_POINT('',#109782);
#30059=VERTEX_POINT('',#109784);
#30060=VERTEX_POINT('',#109806);
#30061=VERTEX_POINT('',#109816);
#30062=VERTEX_POINT('',#109825);
#30063=VERTEX_POINT('',#109827);
#30064=VERTEX_POINT('',#109849);
#30065=VERTEX_POINT('',#109859);
#30066=VERTEX_POINT('',#109868);
#30067=VERTEX_POINT('',#109870);
#30068=VERTEX_POINT('',#109892);
#30069=VERTEX_POINT('',#109902);
#30070=VERTEX_POINT('',#109911);
#30071=VERTEX_POINT('',#109913);
#30072=VERTEX_POINT('',#109935);
#30073=VERTEX_POINT('',#109945);
#30074=VERTEX_POINT('',#109954);
#30075=VERTEX_POINT('',#109956);
#30076=VERTEX_POINT('',#109978);
#30077=VERTEX_POINT('',#109988);
#30078=VERTEX_POINT('',#109997);
#30079=VERTEX_POINT('',#109999);
#30080=VERTEX_POINT('',#110021);
#30081=VERTEX_POINT('',#110031);
#30082=VERTEX_POINT('',#110040);
#30083=VERTEX_POINT('',#110042);
#30084=VERTEX_POINT('',#110064);
#30085=VERTEX_POINT('',#110074);
#30086=VERTEX_POINT('',#110083);
#30087=VERTEX_POINT('',#110085);
#30088=VERTEX_POINT('',#110107);
#30089=VERTEX_POINT('',#110117);
#30090=VERTEX_POINT('',#110126);
#30091=VERTEX_POINT('',#110128);
#30092=VERTEX_POINT('',#110150);
#30093=VERTEX_POINT('',#110160);
#30094=VERTEX_POINT('',#110169);
#30095=VERTEX_POINT('',#110171);
#30096=VERTEX_POINT('',#110193);
#30097=VERTEX_POINT('',#110203);
#30098=VERTEX_POINT('',#110212);
#30099=VERTEX_POINT('',#110214);
#30100=VERTEX_POINT('',#110236);
#30101=VERTEX_POINT('',#110246);
#30102=VERTEX_POINT('',#110255);
#30103=VERTEX_POINT('',#110257);
#30104=VERTEX_POINT('',#110279);
#30105=VERTEX_POINT('',#110289);
#30106=VERTEX_POINT('',#110298);
#30107=VERTEX_POINT('',#110300);
#30108=VERTEX_POINT('',#110322);
#30109=VERTEX_POINT('',#110332);
#30110=VERTEX_POINT('',#110341);
#30111=VERTEX_POINT('',#110343);
#30112=VERTEX_POINT('',#110365);
#30113=VERTEX_POINT('',#110375);
#30114=VERTEX_POINT('',#110384);
#30115=VERTEX_POINT('',#110386);
#30116=VERTEX_POINT('',#110408);
#30117=VERTEX_POINT('',#110418);
#30118=VERTEX_POINT('',#110427);
#30119=VERTEX_POINT('',#110429);
#30120=VERTEX_POINT('',#110451);
#30121=VERTEX_POINT('',#110461);
#30122=VERTEX_POINT('',#110470);
#30123=VERTEX_POINT('',#110472);
#30124=VERTEX_POINT('',#110494);
#30125=VERTEX_POINT('',#110504);
#30126=VERTEX_POINT('',#110513);
#30127=VERTEX_POINT('',#110515);
#30128=VERTEX_POINT('',#110537);
#30129=VERTEX_POINT('',#110547);
#30130=VERTEX_POINT('',#110556);
#30131=VERTEX_POINT('',#110558);
#30132=VERTEX_POINT('',#110580);
#30133=VERTEX_POINT('',#110590);
#30134=VERTEX_POINT('',#110599);
#30135=VERTEX_POINT('',#110601);
#30136=VERTEX_POINT('',#110623);
#30137=VERTEX_POINT('',#110633);
#30138=VERTEX_POINT('',#110642);
#30139=VERTEX_POINT('',#110644);
#30140=VERTEX_POINT('',#110666);
#30141=VERTEX_POINT('',#110676);
#30142=VERTEX_POINT('',#110685);
#30143=VERTEX_POINT('',#110687);
#30144=VERTEX_POINT('',#110709);
#30145=VERTEX_POINT('',#110719);
#30146=VERTEX_POINT('',#110728);
#30147=VERTEX_POINT('',#110730);
#30148=VERTEX_POINT('',#110752);
#30149=VERTEX_POINT('',#110762);
#30150=VERTEX_POINT('',#110771);
#30151=VERTEX_POINT('',#110773);
#30152=VERTEX_POINT('',#110795);
#30153=VERTEX_POINT('',#110805);
#30154=VERTEX_POINT('',#110814);
#30155=VERTEX_POINT('',#110816);
#30156=VERTEX_POINT('',#110838);
#30157=VERTEX_POINT('',#110848);
#30158=VERTEX_POINT('',#110857);
#30159=VERTEX_POINT('',#110859);
#30160=VERTEX_POINT('',#110881);
#30161=VERTEX_POINT('',#110891);
#30162=VERTEX_POINT('',#110904);
#30163=VERTEX_POINT('',#110929);
#30164=VERTEX_POINT('',#110954);
#30165=VERTEX_POINT('',#110979);
#30166=VERTEX_POINT('',#111004);
#30167=VERTEX_POINT('',#111029);
#30168=VERTEX_POINT('',#111054);
#30169=VERTEX_POINT('',#111079);
#30170=VERTEX_POINT('',#111104);
#30171=VERTEX_POINT('',#111129);
#30172=VERTEX_POINT('',#111154);
#30173=VERTEX_POINT('',#111179);
#30174=VERTEX_POINT('',#111204);
#30175=VERTEX_POINT('',#111229);
#30176=VERTEX_POINT('',#111254);
#30177=VERTEX_POINT('',#111279);
#30178=VERTEX_POINT('',#111304);
#30179=VERTEX_POINT('',#111329);
#30180=VERTEX_POINT('',#111354);
#30181=VERTEX_POINT('',#111379);
#30182=VERTEX_POINT('',#111404);
#30183=VERTEX_POINT('',#111429);
#30184=VERTEX_POINT('',#111454);
#30185=VERTEX_POINT('',#111479);
#30186=VERTEX_POINT('',#111504);
#30187=VERTEX_POINT('',#111529);
#30188=VERTEX_POINT('',#111554);
#30189=VERTEX_POINT('',#111579);
#30190=VERTEX_POINT('',#111604);
#30191=VERTEX_POINT('',#111625);
#30192=VERTEX_POINT('',#111650);
#30193=VERTEX_POINT('',#111675);
#30194=VERTEX_POINT('',#111700);
#30195=VERTEX_POINT('',#111725);
#30196=VERTEX_POINT('',#111750);
#30197=VERTEX_POINT('',#111775);
#30198=VERTEX_POINT('',#111800);
#30199=VERTEX_POINT('',#111825);
#30200=VERTEX_POINT('',#111850);
#30201=VERTEX_POINT('',#111875);
#30202=VERTEX_POINT('',#111900);
#30203=VERTEX_POINT('',#111925);
#30204=VERTEX_POINT('',#111950);
#30205=VERTEX_POINT('',#111975);
#30206=VERTEX_POINT('',#112000);
#30207=VERTEX_POINT('',#112025);
#30208=VERTEX_POINT('',#112050);
#30209=VERTEX_POINT('',#112075);
#30210=VERTEX_POINT('',#112100);
#30211=VERTEX_POINT('',#112125);
#30212=VERTEX_POINT('',#112150);
#30213=VERTEX_POINT('',#112175);
#30214=VERTEX_POINT('',#112200);
#30215=VERTEX_POINT('',#112225);
#30216=VERTEX_POINT('',#112250);
#30217=VERTEX_POINT('',#112275);
#30218=VERTEX_POINT('',#112300);
#30219=VERTEX_POINT('',#112325);
#30220=VERTEX_POINT('',#112354);
#30221=VERTEX_POINT('',#112355);
#30222=VERTEX_POINT('',#112374);
#30223=VERTEX_POINT('',#112375);
#30224=VERTEX_POINT('',#112385);
#30225=VERTEX_POINT('',#112396);
#30226=VERTEX_POINT('',#112420);
#30227=VERTEX_POINT('',#112421);
#30228=VERTEX_POINT('',#112431);
#30229=VERTEX_POINT('',#112442);
#30230=VERTEX_POINT('',#112466);
#30231=VERTEX_POINT('',#112467);
#30232=VERTEX_POINT('',#112477);
#30233=VERTEX_POINT('',#112488);
#30234=VERTEX_POINT('',#112512);
#30235=VERTEX_POINT('',#112513);
#30236=VERTEX_POINT('',#112523);
#30237=VERTEX_POINT('',#112534);
#30238=VERTEX_POINT('',#112558);
#30239=VERTEX_POINT('',#112559);
#30240=VERTEX_POINT('',#112569);
#30241=VERTEX_POINT('',#112580);
#30242=VERTEX_POINT('',#112604);
#30243=VERTEX_POINT('',#112605);
#30244=VERTEX_POINT('',#112615);
#30245=VERTEX_POINT('',#112626);
#30246=VERTEX_POINT('',#112678);
#30247=VERTEX_POINT('',#112679);
#30248=VERTEX_POINT('',#112689);
#30249=VERTEX_POINT('',#112700);
#30250=VERTEX_POINT('',#112724);
#30251=VERTEX_POINT('',#112725);
#30252=VERTEX_POINT('',#112735);
#30253=VERTEX_POINT('',#112746);
#30254=VERTEX_POINT('',#112770);
#30255=VERTEX_POINT('',#112771);
#30256=VERTEX_POINT('',#112781);
#30257=VERTEX_POINT('',#112792);
#30258=VERTEX_POINT('',#112816);
#30259=VERTEX_POINT('',#112817);
#30260=VERTEX_POINT('',#112827);
#30261=VERTEX_POINT('',#112838);
#30262=VERTEX_POINT('',#112862);
#30263=VERTEX_POINT('',#112863);
#30264=VERTEX_POINT('',#112873);
#30265=VERTEX_POINT('',#112884);
#30266=VERTEX_POINT('',#112908);
#30267=VERTEX_POINT('',#112909);
#30268=VERTEX_POINT('',#112919);
#30269=VERTEX_POINT('',#112930);
#30270=VERTEX_POINT('',#112954);
#30271=VERTEX_POINT('',#112955);
#30272=VERTEX_POINT('',#112965);
#30273=VERTEX_POINT('',#112976);
#30274=VERTEX_POINT('',#113000);
#30275=VERTEX_POINT('',#113001);
#30276=VERTEX_POINT('',#113011);
#30277=VERTEX_POINT('',#113022);
#30278=VERTEX_POINT('',#113046);
#30279=VERTEX_POINT('',#113047);
#30280=VERTEX_POINT('',#113057);
#30281=VERTEX_POINT('',#113068);
#30282=VERTEX_POINT('',#113092);
#30283=VERTEX_POINT('',#113093);
#30284=VERTEX_POINT('',#113103);
#30285=VERTEX_POINT('',#113114);
#30286=VERTEX_POINT('',#113138);
#30287=VERTEX_POINT('',#113139);
#30288=VERTEX_POINT('',#113149);
#30289=VERTEX_POINT('',#113160);
#30290=VERTEX_POINT('',#113184);
#30291=VERTEX_POINT('',#113185);
#30292=VERTEX_POINT('',#113195);
#30293=VERTEX_POINT('',#113206);
#30294=VERTEX_POINT('',#113230);
#30295=VERTEX_POINT('',#113231);
#30296=VERTEX_POINT('',#113241);
#30297=VERTEX_POINT('',#113252);
#30298=VERTEX_POINT('',#113276);
#30299=VERTEX_POINT('',#113277);
#30300=VERTEX_POINT('',#113287);
#30301=VERTEX_POINT('',#113298);
#30302=VERTEX_POINT('',#113322);
#30303=VERTEX_POINT('',#113323);
#30304=VERTEX_POINT('',#113333);
#30305=VERTEX_POINT('',#113344);
#30306=VERTEX_POINT('',#113368);
#30307=VERTEX_POINT('',#113369);
#30308=VERTEX_POINT('',#113388);
#30309=VERTEX_POINT('',#113392);
#30310=VERTEX_POINT('',#113414);
#30311=VERTEX_POINT('',#113416);
#30312=VERTEX_POINT('',#113425);
#30313=VERTEX_POINT('',#113427);
#30314=VERTEX_POINT('',#113460);
#30315=VERTEX_POINT('',#113461);
#30316=VERTEX_POINT('',#113471);
#30317=VERTEX_POINT('',#113482);
#30318=VERTEX_POINT('',#113506);
#30319=VERTEX_POINT('',#113507);
#30320=VERTEX_POINT('',#113517);
#30321=VERTEX_POINT('',#113528);
#30322=VERTEX_POINT('',#113552);
#30323=VERTEX_POINT('',#113553);
#30324=VERTEX_POINT('',#113563);
#30325=VERTEX_POINT('',#113574);
#30326=VERTEX_POINT('',#113598);
#30327=VERTEX_POINT('',#113599);
#30328=VERTEX_POINT('',#113609);
#30329=VERTEX_POINT('',#113620);
#30330=VERTEX_POINT('',#113635);
#30331=VERTEX_POINT('',#113636);
#30332=VERTEX_POINT('',#113670);
#30333=VERTEX_POINT('',#113671);
#30334=VERTEX_POINT('',#113686);
#30335=VERTEX_POINT('',#113688);
#30336=VERTEX_POINT('',#113706);
#30337=VERTEX_POINT('',#113710);
#30338=VERTEX_POINT('',#113719);
#30339=VERTEX_POINT('',#113721);
#30340=VERTEX_POINT('',#113739);
#30341=VERTEX_POINT('',#113743);
#30342=VERTEX_POINT('',#113752);
#30343=VERTEX_POINT('',#113754);
#30344=VERTEX_POINT('',#113772);
#30345=VERTEX_POINT('',#113776);
#30346=VERTEX_POINT('',#113785);
#30347=VERTEX_POINT('',#113787);
#30348=VERTEX_POINT('',#113805);
#30349=VERTEX_POINT('',#113809);
#30350=VERTEX_POINT('',#113818);
#30351=VERTEX_POINT('',#113820);
#30352=VERTEX_POINT('',#113838);
#30353=VERTEX_POINT('',#113842);
#30354=VERTEX_POINT('',#113851);
#30355=VERTEX_POINT('',#113853);
#30356=VERTEX_POINT('',#113871);
#30357=VERTEX_POINT('',#113875);
#30358=VERTEX_POINT('',#113884);
#30359=VERTEX_POINT('',#113886);
#30360=VERTEX_POINT('',#113904);
#30361=VERTEX_POINT('',#113908);
#30362=VERTEX_POINT('',#113917);
#30363=VERTEX_POINT('',#113919);
#30364=VERTEX_POINT('',#113937);
#30365=VERTEX_POINT('',#113941);
#30366=VERTEX_POINT('',#113950);
#30367=VERTEX_POINT('',#113952);
#30368=VERTEX_POINT('',#113970);
#30369=VERTEX_POINT('',#113974);
#30370=VERTEX_POINT('',#113983);
#30371=VERTEX_POINT('',#113985);
#30372=VERTEX_POINT('',#114003);
#30373=VERTEX_POINT('',#114007);
#30374=VERTEX_POINT('',#114016);
#30375=VERTEX_POINT('',#114018);
#30376=VERTEX_POINT('',#114036);
#30377=VERTEX_POINT('',#114040);
#30378=VERTEX_POINT('',#114049);
#30379=VERTEX_POINT('',#114051);
#30380=VERTEX_POINT('',#114069);
#30381=VERTEX_POINT('',#114073);
#30382=VERTEX_POINT('',#114082);
#30383=VERTEX_POINT('',#114084);
#30384=VERTEX_POINT('',#114102);
#30385=VERTEX_POINT('',#114106);
#30386=VERTEX_POINT('',#114139);
#30387=VERTEX_POINT('',#114141);
#30388=VERTEX_POINT('',#114159);
#30389=VERTEX_POINT('',#114163);
#30390=VERTEX_POINT('',#114172);
#30391=VERTEX_POINT('',#114174);
#30392=VERTEX_POINT('',#114192);
#30393=VERTEX_POINT('',#114196);
#30394=VERTEX_POINT('',#114205);
#30395=VERTEX_POINT('',#114207);
#30396=VERTEX_POINT('',#114225);
#30397=VERTEX_POINT('',#114229);
#30398=VERTEX_POINT('',#114238);
#30399=VERTEX_POINT('',#114240);
#30400=VERTEX_POINT('',#114258);
#30401=VERTEX_POINT('',#114262);
#30402=VERTEX_POINT('',#114271);
#30403=VERTEX_POINT('',#114273);
#30404=VERTEX_POINT('',#114291);
#30405=VERTEX_POINT('',#114295);
#30406=VERTEX_POINT('',#114304);
#30407=VERTEX_POINT('',#114306);
#30408=VERTEX_POINT('',#114324);
#30409=VERTEX_POINT('',#114328);
#30410=VERTEX_POINT('',#114337);
#30411=VERTEX_POINT('',#114339);
#30412=VERTEX_POINT('',#114357);
#30413=VERTEX_POINT('',#114361);
#30414=VERTEX_POINT('',#114370);
#30415=VERTEX_POINT('',#114372);
#30416=VERTEX_POINT('',#114390);
#30417=VERTEX_POINT('',#114394);
#30418=VERTEX_POINT('',#114403);
#30419=VERTEX_POINT('',#114405);
#30420=VERTEX_POINT('',#114423);
#30421=VERTEX_POINT('',#114427);
#30422=VERTEX_POINT('',#114436);
#30423=VERTEX_POINT('',#114438);
#30424=VERTEX_POINT('',#114456);
#30425=VERTEX_POINT('',#114460);
#30426=VERTEX_POINT('',#114469);
#30427=VERTEX_POINT('',#114471);
#30428=VERTEX_POINT('',#114489);
#30429=VERTEX_POINT('',#114493);
#30430=VERTEX_POINT('',#114502);
#30431=VERTEX_POINT('',#114504);
#30432=VERTEX_POINT('',#114522);
#30433=VERTEX_POINT('',#114526);
#30434=VERTEX_POINT('',#114535);
#30435=VERTEX_POINT('',#114537);
#30436=VERTEX_POINT('',#114555);
#30437=VERTEX_POINT('',#114559);
#30438=VERTEX_POINT('',#114568);
#30439=VERTEX_POINT('',#114570);
#30440=VERTEX_POINT('',#114588);
#30441=VERTEX_POINT('',#114592);
#30442=VERTEX_POINT('',#114596);
#30443=VERTEX_POINT('',#114597);
#30444=VERTEX_POINT('',#114614);
#30445=VERTEX_POINT('',#114632);
#30446=VERTEX_POINT('',#114663);
#30447=VERTEX_POINT('',#114694);
#30448=VERTEX_POINT('',#114725);
#30449=VERTEX_POINT('',#114756);
#30450=VERTEX_POINT('',#114787);
#30451=VERTEX_POINT('',#114818);
#30452=VERTEX_POINT('',#114849);
#30453=VERTEX_POINT('',#114880);
#30454=VERTEX_POINT('',#114911);
#30455=VERTEX_POINT('',#114942);
#30456=VERTEX_POINT('',#114973);
#30457=VERTEX_POINT('',#115004);
#30458=VERTEX_POINT('',#115035);
#30459=VERTEX_POINT('',#115066);
#30460=VERTEX_POINT('',#115097);
#30461=VERTEX_POINT('',#115128);
#30462=VERTEX_POINT('',#115159);
#30463=VERTEX_POINT('',#115190);
#30464=VERTEX_POINT('',#115221);
#30465=VERTEX_POINT('',#115252);
#30466=VERTEX_POINT('',#115283);
#30467=VERTEX_POINT('',#115314);
#30468=VERTEX_POINT('',#115345);
#30469=VERTEX_POINT('',#115376);
#30470=VERTEX_POINT('',#115407);
#30471=VERTEX_POINT('',#115438);
#30472=VERTEX_POINT('',#115469);
#30473=VERTEX_POINT('',#115517);
#30474=VERTEX_POINT('',#115531);
#30475=VERTEX_POINT('',#115556);
#30476=VERTEX_POINT('',#115581);
#30477=VERTEX_POINT('',#115606);
#30478=VERTEX_POINT('',#115631);
#30479=VERTEX_POINT('',#115656);
#30480=VERTEX_POINT('',#115681);
#30481=VERTEX_POINT('',#115706);
#30482=VERTEX_POINT('',#115731);
#30483=VERTEX_POINT('',#115756);
#30484=VERTEX_POINT('',#115781);
#30485=VERTEX_POINT('',#115806);
#30486=VERTEX_POINT('',#115831);
#30487=VERTEX_POINT('',#115856);
#30488=VERTEX_POINT('',#115881);
#30489=VERTEX_POINT('',#115906);
#30490=VERTEX_POINT('',#115931);
#30491=VERTEX_POINT('',#115956);
#30492=VERTEX_POINT('',#115981);
#30493=VERTEX_POINT('',#116006);
#30494=VERTEX_POINT('',#116031);
#30495=VERTEX_POINT('',#116056);
#30496=VERTEX_POINT('',#116081);
#30497=VERTEX_POINT('',#116106);
#30498=VERTEX_POINT('',#116131);
#30499=VERTEX_POINT('',#116156);
#30500=VERTEX_POINT('',#116181);
#30501=VERTEX_POINT('',#116206);
#30502=VERTEX_POINT('',#116242);
#30503=VERTEX_POINT('',#116243);
#30504=VERTEX_POINT('',#116253);
#30505=VERTEX_POINT('',#116255);
#30506=VERTEX_POINT('',#116289);
#30507=VERTEX_POINT('',#116290);
#30508=VERTEX_POINT('',#116300);
#30509=VERTEX_POINT('',#116302);
#30510=VERTEX_POINT('',#116336);
#30511=VERTEX_POINT('',#116337);
#30512=VERTEX_POINT('',#116347);
#30513=VERTEX_POINT('',#116349);
#30514=VERTEX_POINT('',#116383);
#30515=VERTEX_POINT('',#116384);
#30516=VERTEX_POINT('',#116394);
#30517=VERTEX_POINT('',#116396);
#30518=VERTEX_POINT('',#116430);
#30519=VERTEX_POINT('',#116431);
#30520=VERTEX_POINT('',#116441);
#30521=VERTEX_POINT('',#116443);
#30522=VERTEX_POINT('',#116477);
#30523=VERTEX_POINT('',#116478);
#30524=VERTEX_POINT('',#116488);
#30525=VERTEX_POINT('',#116490);
#30526=VERTEX_POINT('',#116524);
#30527=VERTEX_POINT('',#116525);
#30528=VERTEX_POINT('',#116535);
#30529=VERTEX_POINT('',#116537);
#30530=VERTEX_POINT('',#116571);
#30531=VERTEX_POINT('',#116572);
#30532=VERTEX_POINT('',#116582);
#30533=VERTEX_POINT('',#116584);
#30534=VERTEX_POINT('',#116618);
#30535=VERTEX_POINT('',#116619);
#30536=VERTEX_POINT('',#116629);
#30537=VERTEX_POINT('',#116631);
#30538=VERTEX_POINT('',#116665);
#30539=VERTEX_POINT('',#116666);
#30540=VERTEX_POINT('',#116676);
#30541=VERTEX_POINT('',#116678);
#30542=VERTEX_POINT('',#116712);
#30543=VERTEX_POINT('',#116713);
#30544=VERTEX_POINT('',#116723);
#30545=VERTEX_POINT('',#116725);
#30546=VERTEX_POINT('',#116759);
#30547=VERTEX_POINT('',#116760);
#30548=VERTEX_POINT('',#116770);
#30549=VERTEX_POINT('',#116772);
#30550=VERTEX_POINT('',#116806);
#30551=VERTEX_POINT('',#116807);
#30552=VERTEX_POINT('',#116817);
#30553=VERTEX_POINT('',#116819);
#30554=VERTEX_POINT('',#116853);
#30555=VERTEX_POINT('',#116854);
#30556=VERTEX_POINT('',#116864);
#30557=VERTEX_POINT('',#116866);
#30558=VERTEX_POINT('',#116932);
#30559=VERTEX_POINT('',#116933);
#30560=VERTEX_POINT('',#116943);
#30561=VERTEX_POINT('',#116945);
#30562=VERTEX_POINT('',#116979);
#30563=VERTEX_POINT('',#116980);
#30564=VERTEX_POINT('',#116990);
#30565=VERTEX_POINT('',#116992);
#30566=VERTEX_POINT('',#117026);
#30567=VERTEX_POINT('',#117027);
#30568=VERTEX_POINT('',#117037);
#30569=VERTEX_POINT('',#117039);
#30570=VERTEX_POINT('',#117073);
#30571=VERTEX_POINT('',#117074);
#30572=VERTEX_POINT('',#117084);
#30573=VERTEX_POINT('',#117086);
#30574=VERTEX_POINT('',#117120);
#30575=VERTEX_POINT('',#117121);
#30576=VERTEX_POINT('',#117131);
#30577=VERTEX_POINT('',#117133);
#30578=VERTEX_POINT('',#117167);
#30579=VERTEX_POINT('',#117168);
#30580=VERTEX_POINT('',#117178);
#30581=VERTEX_POINT('',#117180);
#30582=VERTEX_POINT('',#117214);
#30583=VERTEX_POINT('',#117215);
#30584=VERTEX_POINT('',#117225);
#30585=VERTEX_POINT('',#117227);
#30586=VERTEX_POINT('',#117261);
#30587=VERTEX_POINT('',#117262);
#30588=VERTEX_POINT('',#117285);
#30589=VERTEX_POINT('',#117295);
#30590=VERTEX_POINT('',#117308);
#30591=VERTEX_POINT('',#117310);
#30592=VERTEX_POINT('',#117319);
#30593=VERTEX_POINT('',#117327);
#30594=VERTEX_POINT('',#117355);
#30595=VERTEX_POINT('',#117356);
#30596=VERTEX_POINT('',#117366);
#30597=VERTEX_POINT('',#117368);
#30598=VERTEX_POINT('',#117402);
#30599=VERTEX_POINT('',#117403);
#30600=VERTEX_POINT('',#117413);
#30601=VERTEX_POINT('',#117415);
#30602=VERTEX_POINT('',#117449);
#30603=VERTEX_POINT('',#117450);
#30604=VERTEX_POINT('',#117460);
#30605=VERTEX_POINT('',#117462);
#30606=VERTEX_POINT('',#117496);
#30607=VERTEX_POINT('',#117497);
#30608=VERTEX_POINT('',#117507);
#30609=VERTEX_POINT('',#117509);
#30610=VERTEX_POINT('',#117543);
#30611=VERTEX_POINT('',#117544);
#30612=VERTEX_POINT('',#117554);
#30613=VERTEX_POINT('',#117556);
#30614=VERTEX_POINT('',#117590);
#30615=VERTEX_POINT('',#117592);
#30616=VERTEX_POINT('',#117610);
#30617=VERTEX_POINT('',#117614);
#30618=VERTEX_POINT('',#117627);
#30619=VERTEX_POINT('',#117629);
#30620=VERTEX_POINT('',#117647);
#30621=VERTEX_POINT('',#117651);
#30622=VERTEX_POINT('',#117664);
#30623=VERTEX_POINT('',#117666);
#30624=VERTEX_POINT('',#117684);
#30625=VERTEX_POINT('',#117688);
#30626=VERTEX_POINT('',#117701);
#30627=VERTEX_POINT('',#117703);
#30628=VERTEX_POINT('',#117721);
#30629=VERTEX_POINT('',#117725);
#30630=VERTEX_POINT('',#117738);
#30631=VERTEX_POINT('',#117740);
#30632=VERTEX_POINT('',#117758);
#30633=VERTEX_POINT('',#117762);
#30634=VERTEX_POINT('',#117775);
#30635=VERTEX_POINT('',#117777);
#30636=VERTEX_POINT('',#117795);
#30637=VERTEX_POINT('',#117799);
#30638=VERTEX_POINT('',#117812);
#30639=VERTEX_POINT('',#117814);
#30640=VERTEX_POINT('',#117832);
#30641=VERTEX_POINT('',#117836);
#30642=VERTEX_POINT('',#117849);
#30643=VERTEX_POINT('',#117851);
#30644=VERTEX_POINT('',#117869);
#30645=VERTEX_POINT('',#117873);
#30646=VERTEX_POINT('',#117886);
#30647=VERTEX_POINT('',#117888);
#30648=VERTEX_POINT('',#117906);
#30649=VERTEX_POINT('',#117910);
#30650=VERTEX_POINT('',#117923);
#30651=VERTEX_POINT('',#117925);
#30652=VERTEX_POINT('',#117943);
#30653=VERTEX_POINT('',#117947);
#30654=VERTEX_POINT('',#117960);
#30655=VERTEX_POINT('',#117962);
#30656=VERTEX_POINT('',#117980);
#30657=VERTEX_POINT('',#117984);
#30658=VERTEX_POINT('',#117997);
#30659=VERTEX_POINT('',#117999);
#30660=VERTEX_POINT('',#118017);
#30661=VERTEX_POINT('',#118021);
#30662=VERTEX_POINT('',#118034);
#30663=VERTEX_POINT('',#118036);
#30664=VERTEX_POINT('',#118054);
#30665=VERTEX_POINT('',#118058);
#30666=VERTEX_POINT('',#118071);
#30667=VERTEX_POINT('',#118073);
#30668=VERTEX_POINT('',#118091);
#30669=VERTEX_POINT('',#118095);
#30670=VERTEX_POINT('',#118108);
#30671=VERTEX_POINT('',#118110);
#30672=VERTEX_POINT('',#118128);
#30673=VERTEX_POINT('',#118132);
#30674=VERTEX_POINT('',#118145);
#30675=VERTEX_POINT('',#118147);
#30676=VERTEX_POINT('',#118165);
#30677=VERTEX_POINT('',#118169);
#30678=VERTEX_POINT('',#118182);
#30679=VERTEX_POINT('',#118184);
#30680=VERTEX_POINT('',#118202);
#30681=VERTEX_POINT('',#118206);
#30682=VERTEX_POINT('',#118219);
#30683=VERTEX_POINT('',#118221);
#30684=VERTEX_POINT('',#118239);
#30685=VERTEX_POINT('',#118243);
#30686=VERTEX_POINT('',#118256);
#30687=VERTEX_POINT('',#118258);
#30688=VERTEX_POINT('',#118276);
#30689=VERTEX_POINT('',#118280);
#30690=VERTEX_POINT('',#118293);
#30691=VERTEX_POINT('',#118295);
#30692=VERTEX_POINT('',#118313);
#30693=VERTEX_POINT('',#118317);
#30694=VERTEX_POINT('',#118330);
#30695=VERTEX_POINT('',#118332);
#30696=VERTEX_POINT('',#118350);
#30697=VERTEX_POINT('',#118354);
#30698=VERTEX_POINT('',#118395);
#30699=VERTEX_POINT('',#118397);
#30700=VERTEX_POINT('',#118415);
#30701=VERTEX_POINT('',#118419);
#30702=VERTEX_POINT('',#118432);
#30703=VERTEX_POINT('',#118434);
#30704=VERTEX_POINT('',#118452);
#30705=VERTEX_POINT('',#118456);
#30706=VERTEX_POINT('',#118469);
#30707=VERTEX_POINT('',#118471);
#30708=VERTEX_POINT('',#118489);
#30709=VERTEX_POINT('',#118493);
#30710=VERTEX_POINT('',#118506);
#30711=VERTEX_POINT('',#118508);
#30712=VERTEX_POINT('',#118526);
#30713=VERTEX_POINT('',#118530);
#30714=VERTEX_POINT('',#118543);
#30715=VERTEX_POINT('',#118545);
#30716=VERTEX_POINT('',#118563);
#30717=VERTEX_POINT('',#118567);
#30718=VERTEX_POINT('',#118580);
#30719=VERTEX_POINT('',#118582);
#30720=VERTEX_POINT('',#118600);
#30721=VERTEX_POINT('',#118604);
#30722=VERTEX_POINT('',#118617);
#30723=VERTEX_POINT('',#118619);
#30724=VERTEX_POINT('',#118637);
#30725=VERTEX_POINT('',#118641);
#30726=VERTEX_POINT('',#118650);
#30727=VERTEX_POINT('',#118684);
#30728=VERTEX_POINT('',#118718);
#30729=VERTEX_POINT('',#118752);
#30730=VERTEX_POINT('',#118786);
#30731=VERTEX_POINT('',#118820);
#30732=VERTEX_POINT('',#118854);
#30733=VERTEX_POINT('',#118888);
#30734=VERTEX_POINT('',#118922);
#30735=VERTEX_POINT('',#118956);
#30736=VERTEX_POINT('',#118990);
#30737=VERTEX_POINT('',#119024);
#30738=VERTEX_POINT('',#119058);
#30739=VERTEX_POINT('',#119092);
#30740=VERTEX_POINT('',#119126);
#30741=VERTEX_POINT('',#119160);
#30742=VERTEX_POINT('',#119194);
#30743=VERTEX_POINT('',#119228);
#30744=VERTEX_POINT('',#119262);
#30745=VERTEX_POINT('',#119296);
#30746=VERTEX_POINT('',#119330);
#30747=VERTEX_POINT('',#119364);
#30748=VERTEX_POINT('',#119398);
#30749=VERTEX_POINT('',#119432);
#30750=VERTEX_POINT('',#119466);
#30751=VERTEX_POINT('',#119500);
#30752=VERTEX_POINT('',#119534);
#30753=VERTEX_POINT('',#119568);
#30754=VERTEX_POINT('',#119602);
#30755=VERTEX_POINT('',#119636);
#30756=VERTEX_POINT('',#119674);
#30757=VERTEX_POINT('',#119712);
#30758=VERTEX_POINT('',#119750);
#30759=VERTEX_POINT('',#119788);
#30760=VERTEX_POINT('',#119826);
#30761=VERTEX_POINT('',#119864);
#30762=VERTEX_POINT('',#119902);
#30763=VERTEX_POINT('',#119940);
#30764=VERTEX_POINT('',#119978);
#30765=VERTEX_POINT('',#120016);
#30766=VERTEX_POINT('',#120054);
#30767=VERTEX_POINT('',#120092);
#30768=VERTEX_POINT('',#120130);
#30769=VERTEX_POINT('',#120168);
#30770=VERTEX_POINT('',#120206);
#30771=VERTEX_POINT('',#120244);
#30772=VERTEX_POINT('',#120282);
#30773=VERTEX_POINT('',#120320);
#30774=VERTEX_POINT('',#120358);
#30775=VERTEX_POINT('',#120396);
#30776=VERTEX_POINT('',#120434);
#30777=VERTEX_POINT('',#120472);
#30778=VERTEX_POINT('',#120510);
#30779=VERTEX_POINT('',#120548);
#30780=VERTEX_POINT('',#120586);
#30781=VERTEX_POINT('',#120624);
#30782=VERTEX_POINT('',#120662);
#30783=VERTEX_POINT('',#120700);
#30784=VERTEX_POINT('',#120738);
#30785=VERTEX_POINT('',#120739);
#30786=VERTEX_POINT('',#120762);
#30787=VERTEX_POINT('',#120763);
#30788=VERTEX_POINT('',#120779);
#30789=VERTEX_POINT('',#120781);
#30790=VERTEX_POINT('',#120805);
#30791=VERTEX_POINT('',#120806);
#30792=VERTEX_POINT('',#120822);
#30793=VERTEX_POINT('',#120824);
#30794=VERTEX_POINT('',#120848);
#30795=VERTEX_POINT('',#120849);
#30796=VERTEX_POINT('',#120865);
#30797=VERTEX_POINT('',#120867);
#30798=VERTEX_POINT('',#120891);
#30799=VERTEX_POINT('',#120892);
#30800=VERTEX_POINT('',#120908);
#30801=VERTEX_POINT('',#120910);
#30802=VERTEX_POINT('',#120934);
#30803=VERTEX_POINT('',#120935);
#30804=VERTEX_POINT('',#120951);
#30805=VERTEX_POINT('',#120953);
#30806=VERTEX_POINT('',#120977);
#30807=VERTEX_POINT('',#120978);
#30808=VERTEX_POINT('',#120994);
#30809=VERTEX_POINT('',#120996);
#30810=VERTEX_POINT('',#121048);
#30811=VERTEX_POINT('',#121049);
#30812=VERTEX_POINT('',#121065);
#30813=VERTEX_POINT('',#121067);
#30814=VERTEX_POINT('',#121091);
#30815=VERTEX_POINT('',#121092);
#30816=VERTEX_POINT('',#121108);
#30817=VERTEX_POINT('',#121110);
#30818=VERTEX_POINT('',#121134);
#30819=VERTEX_POINT('',#121135);
#30820=VERTEX_POINT('',#121151);
#30821=VERTEX_POINT('',#121153);
#30822=VERTEX_POINT('',#121177);
#30823=VERTEX_POINT('',#121178);
#30824=VERTEX_POINT('',#121194);
#30825=VERTEX_POINT('',#121196);
#30826=VERTEX_POINT('',#121220);
#30827=VERTEX_POINT('',#121221);
#30828=VERTEX_POINT('',#121237);
#30829=VERTEX_POINT('',#121239);
#30830=VERTEX_POINT('',#121263);
#30831=VERTEX_POINT('',#121264);
#30832=VERTEX_POINT('',#121280);
#30833=VERTEX_POINT('',#121282);
#30834=VERTEX_POINT('',#121306);
#30835=VERTEX_POINT('',#121307);
#30836=VERTEX_POINT('',#121323);
#30837=VERTEX_POINT('',#121325);
#30838=VERTEX_POINT('',#121349);
#30839=VERTEX_POINT('',#121350);
#30840=VERTEX_POINT('',#121366);
#30841=VERTEX_POINT('',#121368);
#30842=VERTEX_POINT('',#121392);
#30843=VERTEX_POINT('',#121393);
#30844=VERTEX_POINT('',#121409);
#30845=VERTEX_POINT('',#121411);
#30846=VERTEX_POINT('',#121435);
#30847=VERTEX_POINT('',#121436);
#30848=VERTEX_POINT('',#121452);
#30849=VERTEX_POINT('',#121454);
#30850=VERTEX_POINT('',#121478);
#30851=VERTEX_POINT('',#121479);
#30852=VERTEX_POINT('',#121495);
#30853=VERTEX_POINT('',#121497);
#30854=VERTEX_POINT('',#121521);
#30855=VERTEX_POINT('',#121522);
#30856=VERTEX_POINT('',#121538);
#30857=VERTEX_POINT('',#121540);
#30858=VERTEX_POINT('',#121564);
#30859=VERTEX_POINT('',#121565);
#30860=VERTEX_POINT('',#121581);
#30861=VERTEX_POINT('',#121583);
#30862=VERTEX_POINT('',#121607);
#30863=VERTEX_POINT('',#121608);
#30864=VERTEX_POINT('',#121624);
#30865=VERTEX_POINT('',#121626);
#30866=VERTEX_POINT('',#121650);
#30867=VERTEX_POINT('',#121651);
#30868=VERTEX_POINT('',#121672);
#30869=VERTEX_POINT('',#121676);
#30870=VERTEX_POINT('',#121693);
#30871=VERTEX_POINT('',#121695);
#30872=VERTEX_POINT('',#121710);
#30873=VERTEX_POINT('',#121712);
#30874=VERTEX_POINT('',#121736);
#30875=VERTEX_POINT('',#121737);
#30876=VERTEX_POINT('',#121753);
#30877=VERTEX_POINT('',#121755);
#30878=VERTEX_POINT('',#121779);
#30879=VERTEX_POINT('',#121780);
#30880=VERTEX_POINT('',#121796);
#30881=VERTEX_POINT('',#121798);
#30882=VERTEX_POINT('',#121822);
#30883=VERTEX_POINT('',#121823);
#30884=VERTEX_POINT('',#121839);
#30885=VERTEX_POINT('',#121841);
#30886=VERTEX_POINT('',#121865);
#30887=VERTEX_POINT('',#121866);
#30888=VERTEX_POINT('',#121882);
#30889=VERTEX_POINT('',#121884);
#30890=VERTEX_POINT('',#121908);
#30891=VERTEX_POINT('',#121909);
#30892=VERTEX_POINT('',#121925);
#30893=VERTEX_POINT('',#121927);
#30894=VERTEX_POINT('',#121938);
#30895=VERTEX_POINT('',#121939);
#30896=VERTEX_POINT('',#121970);
#30897=VERTEX_POINT('',#121977);
#30898=VERTEX_POINT('',#121990);
#30899=VERTEX_POINT('',#121992);
#30900=VERTEX_POINT('',#122012);
#30901=VERTEX_POINT('',#122016);
#30902=VERTEX_POINT('',#122029);
#30903=VERTEX_POINT('',#122031);
#30904=VERTEX_POINT('',#122051);
#30905=VERTEX_POINT('',#122055);
#30906=VERTEX_POINT('',#122068);
#30907=VERTEX_POINT('',#122070);
#30908=VERTEX_POINT('',#122090);
#30909=VERTEX_POINT('',#122094);
#30910=VERTEX_POINT('',#122107);
#30911=VERTEX_POINT('',#122109);
#30912=VERTEX_POINT('',#122129);
#30913=VERTEX_POINT('',#122133);
#30914=VERTEX_POINT('',#122146);
#30915=VERTEX_POINT('',#122148);
#30916=VERTEX_POINT('',#122168);
#30917=VERTEX_POINT('',#122172);
#30918=VERTEX_POINT('',#122185);
#30919=VERTEX_POINT('',#122187);
#30920=VERTEX_POINT('',#122207);
#30921=VERTEX_POINT('',#122211);
#30922=VERTEX_POINT('',#122224);
#30923=VERTEX_POINT('',#122226);
#30924=VERTEX_POINT('',#122246);
#30925=VERTEX_POINT('',#122250);
#30926=VERTEX_POINT('',#122263);
#30927=VERTEX_POINT('',#122265);
#30928=VERTEX_POINT('',#122285);
#30929=VERTEX_POINT('',#122289);
#30930=VERTEX_POINT('',#122302);
#30931=VERTEX_POINT('',#122304);
#30932=VERTEX_POINT('',#122324);
#30933=VERTEX_POINT('',#122328);
#30934=VERTEX_POINT('',#122341);
#30935=VERTEX_POINT('',#122343);
#30936=VERTEX_POINT('',#122363);
#30937=VERTEX_POINT('',#122367);
#30938=VERTEX_POINT('',#122380);
#30939=VERTEX_POINT('',#122382);
#30940=VERTEX_POINT('',#122402);
#30941=VERTEX_POINT('',#122406);
#30942=VERTEX_POINT('',#122419);
#30943=VERTEX_POINT('',#122421);
#30944=VERTEX_POINT('',#122441);
#30945=VERTEX_POINT('',#122445);
#30946=VERTEX_POINT('',#122458);
#30947=VERTEX_POINT('',#122460);
#30948=VERTEX_POINT('',#122480);
#30949=VERTEX_POINT('',#122484);
#30950=VERTEX_POINT('',#122521);
#30951=VERTEX_POINT('',#122523);
#30952=VERTEX_POINT('',#122543);
#30953=VERTEX_POINT('',#122547);
#30954=VERTEX_POINT('',#122560);
#30955=VERTEX_POINT('',#122562);
#30956=VERTEX_POINT('',#122582);
#30957=VERTEX_POINT('',#122586);
#30958=VERTEX_POINT('',#122599);
#30959=VERTEX_POINT('',#122601);
#30960=VERTEX_POINT('',#122621);
#30961=VERTEX_POINT('',#122625);
#30962=VERTEX_POINT('',#122638);
#30963=VERTEX_POINT('',#122640);
#30964=VERTEX_POINT('',#122660);
#30965=VERTEX_POINT('',#122664);
#30966=VERTEX_POINT('',#122677);
#30967=VERTEX_POINT('',#122679);
#30968=VERTEX_POINT('',#122699);
#30969=VERTEX_POINT('',#122703);
#30970=VERTEX_POINT('',#122716);
#30971=VERTEX_POINT('',#122718);
#30972=VERTEX_POINT('',#122738);
#30973=VERTEX_POINT('',#122742);
#30974=VERTEX_POINT('',#122755);
#30975=VERTEX_POINT('',#122757);
#30976=VERTEX_POINT('',#122777);
#30977=VERTEX_POINT('',#122781);
#30978=VERTEX_POINT('',#122794);
#30979=VERTEX_POINT('',#122796);
#30980=VERTEX_POINT('',#122816);
#30981=VERTEX_POINT('',#122820);
#30982=VERTEX_POINT('',#122833);
#30983=VERTEX_POINT('',#122835);
#30984=VERTEX_POINT('',#122855);
#30985=VERTEX_POINT('',#122859);
#30986=VERTEX_POINT('',#122872);
#30987=VERTEX_POINT('',#122874);
#30988=VERTEX_POINT('',#122894);
#30989=VERTEX_POINT('',#122898);
#30990=VERTEX_POINT('',#122911);
#30991=VERTEX_POINT('',#122913);
#30992=VERTEX_POINT('',#122933);
#30993=VERTEX_POINT('',#122937);
#30994=VERTEX_POINT('',#122950);
#30995=VERTEX_POINT('',#122952);
#30996=VERTEX_POINT('',#122972);
#30997=VERTEX_POINT('',#122976);
#30998=VERTEX_POINT('',#122989);
#30999=VERTEX_POINT('',#122991);
#31000=VERTEX_POINT('',#123011);
#31001=VERTEX_POINT('',#123015);
#31002=VERTEX_POINT('',#123028);
#31003=VERTEX_POINT('',#123030);
#31004=VERTEX_POINT('',#123050);
#31005=VERTEX_POINT('',#123054);
#31006=VERTEX_POINT('',#123058);
#31007=VERTEX_POINT('',#123066);
#31008=VERTEX_POINT('',#123086);
#31009=VERTEX_POINT('',#123104);
#31010=VERTEX_POINT('',#123129);
#31011=VERTEX_POINT('',#123154);
#31012=VERTEX_POINT('',#123179);
#31013=VERTEX_POINT('',#123204);
#31014=VERTEX_POINT('',#123229);
#31015=VERTEX_POINT('',#123254);
#31016=VERTEX_POINT('',#123279);
#31017=VERTEX_POINT('',#123304);
#31018=VERTEX_POINT('',#123329);
#31019=VERTEX_POINT('',#123354);
#31020=VERTEX_POINT('',#123379);
#31021=VERTEX_POINT('',#123404);
#31022=VERTEX_POINT('',#123429);
#31023=VERTEX_POINT('',#123454);
#31024=VERTEX_POINT('',#123479);
#31025=VERTEX_POINT('',#123504);
#31026=VERTEX_POINT('',#123529);
#31027=VERTEX_POINT('',#123554);
#31028=VERTEX_POINT('',#123579);
#31029=VERTEX_POINT('',#123604);
#31030=VERTEX_POINT('',#123629);
#31031=VERTEX_POINT('',#123654);
#31032=VERTEX_POINT('',#123679);
#31033=VERTEX_POINT('',#123704);
#31034=VERTEX_POINT('',#123729);
#31035=VERTEX_POINT('',#123754);
#31036=VERTEX_POINT('',#123779);
#31037=VERTEX_POINT('',#123815);
#31038=VERTEX_POINT('',#123841);
#31039=VERTEX_POINT('',#123887);
#31040=VERTEX_POINT('',#123928);
#31041=VERTEX_POINT('',#123969);
#31042=VERTEX_POINT('',#124015);
#31043=VERTEX_POINT('',#124061);
#31044=VERTEX_POINT('',#124102);
#31045=VERTEX_POINT('',#124143);
#31046=VERTEX_POINT('',#124184);
#31047=VERTEX_POINT('',#124225);
#31048=VERTEX_POINT('',#124271);
#31049=VERTEX_POINT('',#124312);
#31050=VERTEX_POINT('',#124353);
#31051=VERTEX_POINT('',#124394);
#31052=VERTEX_POINT('',#124444);
#31053=VERTEX_POINT('',#124494);
#31054=VERTEX_POINT('',#124544);
#31055=VERTEX_POINT('',#124585);
#31056=VERTEX_POINT('',#124626);
#31057=VERTEX_POINT('',#124672);
#31058=VERTEX_POINT('',#124713);
#31059=VERTEX_POINT('',#124754);
#31060=VERTEX_POINT('',#124800);
#31061=VERTEX_POINT('',#124850);
#31062=VERTEX_POINT('',#124891);
#31063=VERTEX_POINT('',#124932);
#31064=VERTEX_POINT('',#124973);
#31065=VERTEX_POINT('',#125019);
#31066=VERTEX_POINT('',#125089);
#31067=VERTEX_POINT('',#125090);
#31068=VERTEX_POINT('',#125100);
#31069=VERTEX_POINT('',#125102);
#31070=VERTEX_POINT('',#125122);
#31071=VERTEX_POINT('',#125123);
#31072=VERTEX_POINT('',#125133);
#31073=VERTEX_POINT('',#125135);
#31074=VERTEX_POINT('',#125155);
#31075=VERTEX_POINT('',#125156);
#31076=VERTEX_POINT('',#125166);
#31077=VERTEX_POINT('',#125168);
#31078=VERTEX_POINT('',#125188);
#31079=VERTEX_POINT('',#125189);
#31080=VERTEX_POINT('',#125199);
#31081=VERTEX_POINT('',#125201);
#31082=VERTEX_POINT('',#125221);
#31083=VERTEX_POINT('',#125222);
#31084=VERTEX_POINT('',#125232);
#31085=VERTEX_POINT('',#125234);
#31086=VERTEX_POINT('',#125254);
#31087=VERTEX_POINT('',#125255);
#31088=VERTEX_POINT('',#125265);
#31089=VERTEX_POINT('',#125267);
#31090=VERTEX_POINT('',#125287);
#31091=VERTEX_POINT('',#125288);
#31092=VERTEX_POINT('',#125298);
#31093=VERTEX_POINT('',#125300);
#31094=VERTEX_POINT('',#125320);
#31095=VERTEX_POINT('',#125321);
#31096=VERTEX_POINT('',#125331);
#31097=VERTEX_POINT('',#125333);
#31098=VERTEX_POINT('',#125353);
#31099=VERTEX_POINT('',#125354);
#31100=VERTEX_POINT('',#125364);
#31101=VERTEX_POINT('',#125366);
#31102=VERTEX_POINT('',#125386);
#31103=VERTEX_POINT('',#125387);
#31104=VERTEX_POINT('',#125397);
#31105=VERTEX_POINT('',#125399);
#31106=VERTEX_POINT('',#125419);
#31107=VERTEX_POINT('',#125420);
#31108=VERTEX_POINT('',#125430);
#31109=VERTEX_POINT('',#125432);
#31110=VERTEX_POINT('',#125452);
#31111=VERTEX_POINT('',#125453);
#31112=VERTEX_POINT('',#125463);
#31113=VERTEX_POINT('',#125465);
#31114=VERTEX_POINT('',#125485);
#31115=VERTEX_POINT('',#125486);
#31116=VERTEX_POINT('',#125496);
#31117=VERTEX_POINT('',#125498);
#31118=VERTEX_POINT('',#125518);
#31119=VERTEX_POINT('',#125519);
#31120=VERTEX_POINT('',#125529);
#31121=VERTEX_POINT('',#125531);
#31122=VERTEX_POINT('',#125575);
#31123=VERTEX_POINT('',#125576);
#31124=VERTEX_POINT('',#125586);
#31125=VERTEX_POINT('',#125588);
#31126=VERTEX_POINT('',#125608);
#31127=VERTEX_POINT('',#125609);
#31128=VERTEX_POINT('',#125619);
#31129=VERTEX_POINT('',#125621);
#31130=VERTEX_POINT('',#125641);
#31131=VERTEX_POINT('',#125642);
#31132=VERTEX_POINT('',#125652);
#31133=VERTEX_POINT('',#125654);
#31134=VERTEX_POINT('',#125674);
#31135=VERTEX_POINT('',#125675);
#31136=VERTEX_POINT('',#125685);
#31137=VERTEX_POINT('',#125687);
#31138=VERTEX_POINT('',#125707);
#31139=VERTEX_POINT('',#125708);
#31140=VERTEX_POINT('',#125718);
#31141=VERTEX_POINT('',#125720);
#31142=VERTEX_POINT('',#125740);
#31143=VERTEX_POINT('',#125741);
#31144=VERTEX_POINT('',#125751);
#31145=VERTEX_POINT('',#125753);
#31146=VERTEX_POINT('',#125773);
#31147=VERTEX_POINT('',#125774);
#31148=VERTEX_POINT('',#125789);
#31149=VERTEX_POINT('',#125793);
#31150=VERTEX_POINT('',#125806);
#31151=VERTEX_POINT('',#125808);
#31152=VERTEX_POINT('',#125817);
#31153=VERTEX_POINT('',#125819);
#31154=VERTEX_POINT('',#125839);
#31155=VERTEX_POINT('',#125840);
#31156=VERTEX_POINT('',#125850);
#31157=VERTEX_POINT('',#125852);
#31158=VERTEX_POINT('',#125872);
#31159=VERTEX_POINT('',#125873);
#31160=VERTEX_POINT('',#125883);
#31161=VERTEX_POINT('',#125885);
#31162=VERTEX_POINT('',#125905);
#31163=VERTEX_POINT('',#125906);
#31164=VERTEX_POINT('',#125916);
#31165=VERTEX_POINT('',#125918);
#31166=VERTEX_POINT('',#125938);
#31167=VERTEX_POINT('',#125939);
#31168=VERTEX_POINT('',#125949);
#31169=VERTEX_POINT('',#125951);
#31170=VERTEX_POINT('',#125971);
#31171=VERTEX_POINT('',#125972);
#31172=VERTEX_POINT('',#125982);
#31173=VERTEX_POINT('',#125984);
#31174=VERTEX_POINT('',#126004);
#31175=VERTEX_POINT('',#126005);
#31176=VERTEX_POINT('',#126015);
#31177=VERTEX_POINT('',#126017);
#31178=VERTEX_POINT('',#126037);
#31179=VERTEX_POINT('',#126039);
#31180=VERTEX_POINT('',#126057);
#31181=VERTEX_POINT('',#126067);
#31182=VERTEX_POINT('',#126080);
#31183=VERTEX_POINT('',#126082);
#31184=VERTEX_POINT('',#126100);
#31185=VERTEX_POINT('',#126110);
#31186=VERTEX_POINT('',#126123);
#31187=VERTEX_POINT('',#126125);
#31188=VERTEX_POINT('',#126143);
#31189=VERTEX_POINT('',#126153);
#31190=VERTEX_POINT('',#126166);
#31191=VERTEX_POINT('',#126168);
#31192=VERTEX_POINT('',#126186);
#31193=VERTEX_POINT('',#126196);
#31194=VERTEX_POINT('',#126209);
#31195=VERTEX_POINT('',#126211);
#31196=VERTEX_POINT('',#126229);
#31197=VERTEX_POINT('',#126239);
#31198=VERTEX_POINT('',#126252);
#31199=VERTEX_POINT('',#126254);
#31200=VERTEX_POINT('',#126272);
#31201=VERTEX_POINT('',#126282);
#31202=VERTEX_POINT('',#126295);
#31203=VERTEX_POINT('',#126297);
#31204=VERTEX_POINT('',#126315);
#31205=VERTEX_POINT('',#126325);
#31206=VERTEX_POINT('',#126338);
#31207=VERTEX_POINT('',#126340);
#31208=VERTEX_POINT('',#126358);
#31209=VERTEX_POINT('',#126368);
#31210=VERTEX_POINT('',#126381);
#31211=VERTEX_POINT('',#126383);
#31212=VERTEX_POINT('',#126401);
#31213=VERTEX_POINT('',#126411);
#31214=VERTEX_POINT('',#126424);
#31215=VERTEX_POINT('',#126426);
#31216=VERTEX_POINT('',#126444);
#31217=VERTEX_POINT('',#126454);
#31218=VERTEX_POINT('',#126467);
#31219=VERTEX_POINT('',#126469);
#31220=VERTEX_POINT('',#126487);
#31221=VERTEX_POINT('',#126497);
#31222=VERTEX_POINT('',#126510);
#31223=VERTEX_POINT('',#126512);
#31224=VERTEX_POINT('',#126530);
#31225=VERTEX_POINT('',#126540);
#31226=VERTEX_POINT('',#126553);
#31227=VERTEX_POINT('',#126555);
#31228=VERTEX_POINT('',#126573);
#31229=VERTEX_POINT('',#126583);
#31230=VERTEX_POINT('',#126596);
#31231=VERTEX_POINT('',#126598);
#31232=VERTEX_POINT('',#126616);
#31233=VERTEX_POINT('',#126626);
#31234=VERTEX_POINT('',#126639);
#31235=VERTEX_POINT('',#126641);
#31236=VERTEX_POINT('',#126659);
#31237=VERTEX_POINT('',#126669);
#31238=VERTEX_POINT('',#126682);
#31239=VERTEX_POINT('',#126684);
#31240=VERTEX_POINT('',#126702);
#31241=VERTEX_POINT('',#126712);
#31242=VERTEX_POINT('',#126725);
#31243=VERTEX_POINT('',#126727);
#31244=VERTEX_POINT('',#126745);
#31245=VERTEX_POINT('',#126755);
#31246=VERTEX_POINT('',#126768);
#31247=VERTEX_POINT('',#126770);
#31248=VERTEX_POINT('',#126788);
#31249=VERTEX_POINT('',#126798);
#31250=VERTEX_POINT('',#126811);
#31251=VERTEX_POINT('',#126813);
#31252=VERTEX_POINT('',#126831);
#31253=VERTEX_POINT('',#126841);
#31254=VERTEX_POINT('',#126854);
#31255=VERTEX_POINT('',#126856);
#31256=VERTEX_POINT('',#126874);
#31257=VERTEX_POINT('',#126884);
#31258=VERTEX_POINT('',#126897);
#31259=VERTEX_POINT('',#126899);
#31260=VERTEX_POINT('',#126917);
#31261=VERTEX_POINT('',#126927);
#31262=VERTEX_POINT('',#126968);
#31263=VERTEX_POINT('',#126970);
#31264=VERTEX_POINT('',#126988);
#31265=VERTEX_POINT('',#126998);
#31266=VERTEX_POINT('',#127011);
#31267=VERTEX_POINT('',#127013);
#31268=VERTEX_POINT('',#127031);
#31269=VERTEX_POINT('',#127041);
#31270=VERTEX_POINT('',#127054);
#31271=VERTEX_POINT('',#127056);
#31272=VERTEX_POINT('',#127074);
#31273=VERTEX_POINT('',#127084);
#31274=VERTEX_POINT('',#127097);
#31275=VERTEX_POINT('',#127099);
#31276=VERTEX_POINT('',#127117);
#31277=VERTEX_POINT('',#127127);
#31278=VERTEX_POINT('',#127140);
#31279=VERTEX_POINT('',#127142);
#31280=VERTEX_POINT('',#127160);
#31281=VERTEX_POINT('',#127170);
#31282=VERTEX_POINT('',#127183);
#31283=VERTEX_POINT('',#127185);
#31284=VERTEX_POINT('',#127203);
#31285=VERTEX_POINT('',#127213);
#31286=VERTEX_POINT('',#127226);
#31287=VERTEX_POINT('',#127228);
#31288=VERTEX_POINT('',#127246);
#31289=VERTEX_POINT('',#127256);
#31290=VERTEX_POINT('',#127269);
#31291=VERTEX_POINT('',#127294);
#31292=VERTEX_POINT('',#127319);
#31293=VERTEX_POINT('',#127344);
#31294=VERTEX_POINT('',#127369);
#31295=VERTEX_POINT('',#127394);
#31296=VERTEX_POINT('',#127419);
#31297=VERTEX_POINT('',#127444);
#31298=VERTEX_POINT('',#127469);
#31299=VERTEX_POINT('',#127494);
#31300=VERTEX_POINT('',#127519);
#31301=VERTEX_POINT('',#127544);
#31302=VERTEX_POINT('',#127569);
#31303=VERTEX_POINT('',#127594);
#31304=VERTEX_POINT('',#127619);
#31305=VERTEX_POINT('',#127644);
#31306=VERTEX_POINT('',#127669);
#31307=VERTEX_POINT('',#127694);
#31308=VERTEX_POINT('',#127719);
#31309=VERTEX_POINT('',#127744);
#31310=VERTEX_POINT('',#127769);
#31311=VERTEX_POINT('',#127794);
#31312=VERTEX_POINT('',#127819);
#31313=VERTEX_POINT('',#127844);
#31314=VERTEX_POINT('',#127869);
#31315=VERTEX_POINT('',#127894);
#31316=VERTEX_POINT('',#127919);
#31317=VERTEX_POINT('',#127944);
#31318=VERTEX_POINT('',#127969);
#31319=VERTEX_POINT('',#127994);
#31320=VERTEX_POINT('',#128019);
#31321=VERTEX_POINT('',#128044);
#31322=VERTEX_POINT('',#128069);
#31323=VERTEX_POINT('',#128094);
#31324=VERTEX_POINT('',#128119);
#31325=VERTEX_POINT('',#128144);
#31326=VERTEX_POINT('',#128169);
#31327=VERTEX_POINT('',#128194);
#31328=VERTEX_POINT('',#128219);
#31329=VERTEX_POINT('',#128244);
#31330=VERTEX_POINT('',#128269);
#31331=VERTEX_POINT('',#128294);
#31332=VERTEX_POINT('',#128319);
#31333=VERTEX_POINT('',#128344);
#31334=VERTEX_POINT('',#128369);
#31335=VERTEX_POINT('',#128394);
#31336=VERTEX_POINT('',#128419);
#31337=VERTEX_POINT('',#128444);
#31338=VERTEX_POINT('',#128469);
#31339=VERTEX_POINT('',#128494);
#31340=VERTEX_POINT('',#128519);
#31341=VERTEX_POINT('',#128544);
#31342=VERTEX_POINT('',#128569);
#31343=VERTEX_POINT('',#128594);
#31344=VERTEX_POINT('',#128619);
#31345=VERTEX_POINT('',#128644);
#31346=VERTEX_POINT('',#128669);
#31347=VERTEX_POINT('',#128694);
#31348=VERTEX_POINT('',#128719);
#31349=VERTEX_POINT('',#128720);
#31350=VERTEX_POINT('',#128739);
#31351=VERTEX_POINT('',#128740);
#31352=VERTEX_POINT('',#128750);
#31353=VERTEX_POINT('',#128752);
#31354=VERTEX_POINT('',#128776);
#31355=VERTEX_POINT('',#128777);
#31356=VERTEX_POINT('',#128787);
#31357=VERTEX_POINT('',#128789);
#31358=VERTEX_POINT('',#128813);
#31359=VERTEX_POINT('',#128814);
#31360=VERTEX_POINT('',#128824);
#31361=VERTEX_POINT('',#128826);
#31362=VERTEX_POINT('',#128850);
#31363=VERTEX_POINT('',#128851);
#31364=VERTEX_POINT('',#128861);
#31365=VERTEX_POINT('',#128863);
#31366=VERTEX_POINT('',#128887);
#31367=VERTEX_POINT('',#128888);
#31368=VERTEX_POINT('',#128898);
#31369=VERTEX_POINT('',#128900);
#31370=VERTEX_POINT('',#128924);
#31371=VERTEX_POINT('',#128925);
#31372=VERTEX_POINT('',#128935);
#31373=VERTEX_POINT('',#128937);
#31374=VERTEX_POINT('',#128989);
#31375=VERTEX_POINT('',#128990);
#31376=VERTEX_POINT('',#129000);
#31377=VERTEX_POINT('',#129002);
#31378=VERTEX_POINT('',#129026);
#31379=VERTEX_POINT('',#129027);
#31380=VERTEX_POINT('',#129037);
#31381=VERTEX_POINT('',#129039);
#31382=VERTEX_POINT('',#129063);
#31383=VERTEX_POINT('',#129064);
#31384=VERTEX_POINT('',#129074);
#31385=VERTEX_POINT('',#129076);
#31386=VERTEX_POINT('',#129100);
#31387=VERTEX_POINT('',#129101);
#31388=VERTEX_POINT('',#129111);
#31389=VERTEX_POINT('',#129113);
#31390=VERTEX_POINT('',#129137);
#31391=VERTEX_POINT('',#129138);
#31392=VERTEX_POINT('',#129148);
#31393=VERTEX_POINT('',#129150);
#31394=VERTEX_POINT('',#129174);
#31395=VERTEX_POINT('',#129175);
#31396=VERTEX_POINT('',#129185);
#31397=VERTEX_POINT('',#129187);
#31398=VERTEX_POINT('',#129211);
#31399=VERTEX_POINT('',#129212);
#31400=VERTEX_POINT('',#129222);
#31401=VERTEX_POINT('',#129224);
#31402=VERTEX_POINT('',#129248);
#31403=VERTEX_POINT('',#129249);
#31404=VERTEX_POINT('',#129259);
#31405=VERTEX_POINT('',#129261);
#31406=VERTEX_POINT('',#129285);
#31407=VERTEX_POINT('',#129286);
#31408=VERTEX_POINT('',#129296);
#31409=VERTEX_POINT('',#129298);
#31410=VERTEX_POINT('',#129322);
#31411=VERTEX_POINT('',#129323);
#31412=VERTEX_POINT('',#129333);
#31413=VERTEX_POINT('',#129335);
#31414=VERTEX_POINT('',#129359);
#31415=VERTEX_POINT('',#129360);
#31416=VERTEX_POINT('',#129370);
#31417=VERTEX_POINT('',#129372);
#31418=VERTEX_POINT('',#129396);
#31419=VERTEX_POINT('',#129397);
#31420=VERTEX_POINT('',#129407);
#31421=VERTEX_POINT('',#129409);
#31422=VERTEX_POINT('',#129433);
#31423=VERTEX_POINT('',#129434);
#31424=VERTEX_POINT('',#129444);
#31425=VERTEX_POINT('',#129446);
#31426=VERTEX_POINT('',#129470);
#31427=VERTEX_POINT('',#129471);
#31428=VERTEX_POINT('',#129490);
#31429=VERTEX_POINT('',#129494);
#31430=VERTEX_POINT('',#129507);
#31431=VERTEX_POINT('',#129509);
#31432=VERTEX_POINT('',#129518);
#31433=VERTEX_POINT('',#129520);
#31434=VERTEX_POINT('',#129544);
#31435=VERTEX_POINT('',#129545);
#31436=VERTEX_POINT('',#129555);
#31437=VERTEX_POINT('',#129557);
#31438=VERTEX_POINT('',#129581);
#31439=VERTEX_POINT('',#129582);
#31440=VERTEX_POINT('',#129592);
#31441=VERTEX_POINT('',#129594);
#31442=VERTEX_POINT('',#129618);
#31443=VERTEX_POINT('',#129619);
#31444=VERTEX_POINT('',#129629);
#31445=VERTEX_POINT('',#129631);
#31446=VERTEX_POINT('',#129655);
#31447=VERTEX_POINT('',#129656);
#31448=VERTEX_POINT('',#129666);
#31449=VERTEX_POINT('',#129668);
#31450=VERTEX_POINT('',#129692);
#31451=VERTEX_POINT('',#129693);
#31452=VERTEX_POINT('',#129703);
#31453=VERTEX_POINT('',#129705);
#31454=VERTEX_POINT('',#129729);
#31455=VERTEX_POINT('',#129730);
#31456=VERTEX_POINT('',#129740);
#31457=VERTEX_POINT('',#129742);
#31458=VERTEX_POINT('',#129757);
#31459=VERTEX_POINT('',#129758);
#31460=VERTEX_POINT('',#129779);
#31461=VERTEX_POINT('',#129786);
#31462=VERTEX_POINT('',#129799);
#31463=VERTEX_POINT('',#129801);
#31464=VERTEX_POINT('',#129815);
#31465=VERTEX_POINT('',#129819);
#31466=VERTEX_POINT('',#129832);
#31467=VERTEX_POINT('',#129834);
#31468=VERTEX_POINT('',#129848);
#31469=VERTEX_POINT('',#129852);
#31470=VERTEX_POINT('',#129865);
#31471=VERTEX_POINT('',#129867);
#31472=VERTEX_POINT('',#129881);
#31473=VERTEX_POINT('',#129885);
#31474=VERTEX_POINT('',#129898);
#31475=VERTEX_POINT('',#129900);
#31476=VERTEX_POINT('',#129914);
#31477=VERTEX_POINT('',#129918);
#31478=VERTEX_POINT('',#129931);
#31479=VERTEX_POINT('',#129933);
#31480=VERTEX_POINT('',#129947);
#31481=VERTEX_POINT('',#129951);
#31482=VERTEX_POINT('',#129964);
#31483=VERTEX_POINT('',#129966);
#31484=VERTEX_POINT('',#129980);
#31485=VERTEX_POINT('',#129984);
#31486=VERTEX_POINT('',#129997);
#31487=VERTEX_POINT('',#129999);
#31488=VERTEX_POINT('',#130013);
#31489=VERTEX_POINT('',#130017);
#31490=VERTEX_POINT('',#130030);
#31491=VERTEX_POINT('',#130032);
#31492=VERTEX_POINT('',#130046);
#31493=VERTEX_POINT('',#130050);
#31494=VERTEX_POINT('',#130063);
#31495=VERTEX_POINT('',#130065);
#31496=VERTEX_POINT('',#130079);
#31497=VERTEX_POINT('',#130083);
#31498=VERTEX_POINT('',#130096);
#31499=VERTEX_POINT('',#130098);
#31500=VERTEX_POINT('',#130112);
#31501=VERTEX_POINT('',#130116);
#31502=VERTEX_POINT('',#130129);
#31503=VERTEX_POINT('',#130131);
#31504=VERTEX_POINT('',#130145);
#31505=VERTEX_POINT('',#130149);
#31506=VERTEX_POINT('',#130162);
#31507=VERTEX_POINT('',#130164);
#31508=VERTEX_POINT('',#130178);
#31509=VERTEX_POINT('',#130182);
#31510=VERTEX_POINT('',#130195);
#31511=VERTEX_POINT('',#130197);
#31512=VERTEX_POINT('',#130211);
#31513=VERTEX_POINT('',#130215);
#31514=VERTEX_POINT('',#130252);
#31515=VERTEX_POINT('',#130254);
#31516=VERTEX_POINT('',#130268);
#31517=VERTEX_POINT('',#130272);
#31518=VERTEX_POINT('',#130285);
#31519=VERTEX_POINT('',#130287);
#31520=VERTEX_POINT('',#130301);
#31521=VERTEX_POINT('',#130305);
#31522=VERTEX_POINT('',#130318);
#31523=VERTEX_POINT('',#130320);
#31524=VERTEX_POINT('',#130334);
#31525=VERTEX_POINT('',#130338);
#31526=VERTEX_POINT('',#130351);
#31527=VERTEX_POINT('',#130353);
#31528=VERTEX_POINT('',#130367);
#31529=VERTEX_POINT('',#130371);
#31530=VERTEX_POINT('',#130384);
#31531=VERTEX_POINT('',#130386);
#31532=VERTEX_POINT('',#130400);
#31533=VERTEX_POINT('',#130404);
#31534=VERTEX_POINT('',#130417);
#31535=VERTEX_POINT('',#130419);
#31536=VERTEX_POINT('',#130433);
#31537=VERTEX_POINT('',#130437);
#31538=VERTEX_POINT('',#130450);
#31539=VERTEX_POINT('',#130452);
#31540=VERTEX_POINT('',#130466);
#31541=VERTEX_POINT('',#130470);
#31542=VERTEX_POINT('',#130483);
#31543=VERTEX_POINT('',#130485);
#31544=VERTEX_POINT('',#130499);
#31545=VERTEX_POINT('',#130503);
#31546=VERTEX_POINT('',#130516);
#31547=VERTEX_POINT('',#130518);
#31548=VERTEX_POINT('',#130532);
#31549=VERTEX_POINT('',#130536);
#31550=VERTEX_POINT('',#130549);
#31551=VERTEX_POINT('',#130551);
#31552=VERTEX_POINT('',#130565);
#31553=VERTEX_POINT('',#130569);
#31554=VERTEX_POINT('',#130582);
#31555=VERTEX_POINT('',#130584);
#31556=VERTEX_POINT('',#130598);
#31557=VERTEX_POINT('',#130602);
#31558=VERTEX_POINT('',#130615);
#31559=VERTEX_POINT('',#130617);
#31560=VERTEX_POINT('',#130631);
#31561=VERTEX_POINT('',#130635);
#31562=VERTEX_POINT('',#130648);
#31563=VERTEX_POINT('',#130650);
#31564=VERTEX_POINT('',#130664);
#31565=VERTEX_POINT('',#130668);
#31566=VERTEX_POINT('',#130681);
#31567=VERTEX_POINT('',#130683);
#31568=VERTEX_POINT('',#130697);
#31569=VERTEX_POINT('',#130701);
#31570=VERTEX_POINT('',#130705);
#31571=VERTEX_POINT('',#130707);
#31572=VERTEX_POINT('',#130727);
#31573=VERTEX_POINT('',#130749);
#31574=VERTEX_POINT('',#130787);
#31575=VERTEX_POINT('',#130825);
#31576=VERTEX_POINT('',#130863);
#31577=VERTEX_POINT('',#130901);
#31578=VERTEX_POINT('',#130939);
#31579=VERTEX_POINT('',#130977);
#31580=VERTEX_POINT('',#131015);
#31581=VERTEX_POINT('',#131053);
#31582=VERTEX_POINT('',#131091);
#31583=VERTEX_POINT('',#131129);
#31584=VERTEX_POINT('',#131167);
#31585=VERTEX_POINT('',#131205);
#31586=VERTEX_POINT('',#131243);
#31587=VERTEX_POINT('',#131281);
#31588=VERTEX_POINT('',#131319);
#31589=VERTEX_POINT('',#131357);
#31590=VERTEX_POINT('',#131395);
#31591=VERTEX_POINT('',#131433);
#31592=VERTEX_POINT('',#131471);
#31593=VERTEX_POINT('',#131509);
#31594=VERTEX_POINT('',#131547);
#31595=VERTEX_POINT('',#131585);
#31596=VERTEX_POINT('',#131623);
#31597=VERTEX_POINT('',#131661);
#31598=VERTEX_POINT('',#131699);
#31599=VERTEX_POINT('',#131737);
#31600=VERTEX_POINT('',#131775);
#31601=VERTEX_POINT('',#131829);
#31602=VERTEX_POINT('',#131847);
#31603=VERTEX_POINT('',#131875);
#31604=VERTEX_POINT('',#131903);
#31605=VERTEX_POINT('',#131931);
#31606=VERTEX_POINT('',#131959);
#31607=VERTEX_POINT('',#131987);
#31608=VERTEX_POINT('',#132015);
#31609=VERTEX_POINT('',#132043);
#31610=VERTEX_POINT('',#132071);
#31611=VERTEX_POINT('',#132099);
#31612=VERTEX_POINT('',#132127);
#31613=VERTEX_POINT('',#132155);
#31614=VERTEX_POINT('',#132183);
#31615=VERTEX_POINT('',#132211);
#31616=VERTEX_POINT('',#132239);
#31617=VERTEX_POINT('',#132267);
#31618=VERTEX_POINT('',#132295);
#31619=VERTEX_POINT('',#132323);
#31620=VERTEX_POINT('',#132351);
#31621=VERTEX_POINT('',#132379);
#31622=VERTEX_POINT('',#132407);
#31623=VERTEX_POINT('',#132435);
#31624=VERTEX_POINT('',#132463);
#31625=VERTEX_POINT('',#132491);
#31626=VERTEX_POINT('',#132519);
#31627=VERTEX_POINT('',#132547);
#31628=VERTEX_POINT('',#132575);
#31629=VERTEX_POINT('',#132603);
#31630=VERTEX_POINT('',#132643);
#31631=VERTEX_POINT('',#132644);
#31632=VERTEX_POINT('',#132654);
#31633=VERTEX_POINT('',#132656);
#31634=VERTEX_POINT('',#132682);
#31635=VERTEX_POINT('',#132683);
#31636=VERTEX_POINT('',#132693);
#31637=VERTEX_POINT('',#132695);
#31638=VERTEX_POINT('',#132721);
#31639=VERTEX_POINT('',#132722);
#31640=VERTEX_POINT('',#132732);
#31641=VERTEX_POINT('',#132734);
#31642=VERTEX_POINT('',#132760);
#31643=VERTEX_POINT('',#132761);
#31644=VERTEX_POINT('',#132771);
#31645=VERTEX_POINT('',#132773);
#31646=VERTEX_POINT('',#132799);
#31647=VERTEX_POINT('',#132800);
#31648=VERTEX_POINT('',#132810);
#31649=VERTEX_POINT('',#132812);
#31650=VERTEX_POINT('',#132838);
#31651=VERTEX_POINT('',#132839);
#31652=VERTEX_POINT('',#132849);
#31653=VERTEX_POINT('',#132851);
#31654=VERTEX_POINT('',#132877);
#31655=VERTEX_POINT('',#132878);
#31656=VERTEX_POINT('',#132888);
#31657=VERTEX_POINT('',#132890);
#31658=VERTEX_POINT('',#132916);
#31659=VERTEX_POINT('',#132917);
#31660=VERTEX_POINT('',#132927);
#31661=VERTEX_POINT('',#132929);
#31662=VERTEX_POINT('',#132955);
#31663=VERTEX_POINT('',#132956);
#31664=VERTEX_POINT('',#132966);
#31665=VERTEX_POINT('',#132968);
#31666=VERTEX_POINT('',#132992);
#31667=VERTEX_POINT('',#132993);
#31668=VERTEX_POINT('',#133003);
#31669=VERTEX_POINT('',#133005);
#31670=VERTEX_POINT('',#133031);
#31671=VERTEX_POINT('',#133032);
#31672=VERTEX_POINT('',#133042);
#31673=VERTEX_POINT('',#133044);
#31674=VERTEX_POINT('',#133070);
#31675=VERTEX_POINT('',#133071);
#31676=VERTEX_POINT('',#133081);
#31677=VERTEX_POINT('',#133083);
#31678=VERTEX_POINT('',#133109);
#31679=VERTEX_POINT('',#133110);
#31680=VERTEX_POINT('',#133120);
#31681=VERTEX_POINT('',#133122);
#31682=VERTEX_POINT('',#133148);
#31683=VERTEX_POINT('',#133149);
#31684=VERTEX_POINT('',#133159);
#31685=VERTEX_POINT('',#133161);
#31686=VERTEX_POINT('',#133211);
#31687=VERTEX_POINT('',#133212);
#31688=VERTEX_POINT('',#133222);
#31689=VERTEX_POINT('',#133224);
#31690=VERTEX_POINT('',#133250);
#31691=VERTEX_POINT('',#133251);
#31692=VERTEX_POINT('',#133261);
#31693=VERTEX_POINT('',#133263);
#31694=VERTEX_POINT('',#133289);
#31695=VERTEX_POINT('',#133290);
#31696=VERTEX_POINT('',#133300);
#31697=VERTEX_POINT('',#133302);
#31698=VERTEX_POINT('',#133328);
#31699=VERTEX_POINT('',#133329);
#31700=VERTEX_POINT('',#133339);
#31701=VERTEX_POINT('',#133341);
#31702=VERTEX_POINT('',#133367);
#31703=VERTEX_POINT('',#133368);
#31704=VERTEX_POINT('',#133378);
#31705=VERTEX_POINT('',#133380);
#31706=VERTEX_POINT('',#133406);
#31707=VERTEX_POINT('',#133407);
#31708=VERTEX_POINT('',#133426);
#31709=VERTEX_POINT('',#133436);
#31710=VERTEX_POINT('',#133445);
#31711=VERTEX_POINT('',#133447);
#31712=VERTEX_POINT('',#133456);
#31713=VERTEX_POINT('',#133464);
#31714=VERTEX_POINT('',#133484);
#31715=VERTEX_POINT('',#133485);
#31716=VERTEX_POINT('',#133495);
#31717=VERTEX_POINT('',#133497);
#31718=VERTEX_POINT('',#133523);
#31719=VERTEX_POINT('',#133524);
#31720=VERTEX_POINT('',#133534);
#31721=VERTEX_POINT('',#133536);
#31722=VERTEX_POINT('',#133562);
#31723=VERTEX_POINT('',#133563);
#31724=VERTEX_POINT('',#133573);
#31725=VERTEX_POINT('',#133575);
#31726=VERTEX_POINT('',#133601);
#31727=VERTEX_POINT('',#133602);
#31728=VERTEX_POINT('',#133612);
#31729=VERTEX_POINT('',#133614);
#31730=VERTEX_POINT('',#133640);
#31731=VERTEX_POINT('',#133641);
#31732=VERTEX_POINT('',#133651);
#31733=VERTEX_POINT('',#133653);
#31734=VERTEX_POINT('',#133679);
#31735=VERTEX_POINT('',#133680);
#31736=VERTEX_POINT('',#133690);
#31737=VERTEX_POINT('',#133692);
#31738=VERTEX_POINT('',#133718);
#31739=VERTEX_POINT('',#133719);
#31740=VERTEX_POINT('',#133729);
#31741=VERTEX_POINT('',#133731);
#31742=VERTEX_POINT('',#133757);
#31743=VERTEX_POINT('',#133759);
#31744=VERTEX_POINT('',#133773);
#31745=VERTEX_POINT('',#133777);
#31746=VERTEX_POINT('',#133786);
#31747=VERTEX_POINT('',#133788);
#31748=VERTEX_POINT('',#133802);
#31749=VERTEX_POINT('',#133806);
#31750=VERTEX_POINT('',#133815);
#31751=VERTEX_POINT('',#133817);
#31752=VERTEX_POINT('',#133831);
#31753=VERTEX_POINT('',#133835);
#31754=VERTEX_POINT('',#133844);
#31755=VERTEX_POINT('',#133846);
#31756=VERTEX_POINT('',#133860);
#31757=VERTEX_POINT('',#133864);
#31758=VERTEX_POINT('',#133873);
#31759=VERTEX_POINT('',#133875);
#31760=VERTEX_POINT('',#133889);
#31761=VERTEX_POINT('',#133893);
#31762=VERTEX_POINT('',#133902);
#31763=VERTEX_POINT('',#133904);
#31764=VERTEX_POINT('',#133918);
#31765=VERTEX_POINT('',#133922);
#31766=VERTEX_POINT('',#133931);
#31767=VERTEX_POINT('',#133933);
#31768=VERTEX_POINT('',#133947);
#31769=VERTEX_POINT('',#133951);
#31770=VERTEX_POINT('',#133960);
#31771=VERTEX_POINT('',#133962);
#31772=VERTEX_POINT('',#133976);
#31773=VERTEX_POINT('',#133980);
#31774=VERTEX_POINT('',#133989);
#31775=VERTEX_POINT('',#133991);
#31776=VERTEX_POINT('',#134005);
#31777=VERTEX_POINT('',#134009);
#31778=VERTEX_POINT('',#134018);
#31779=VERTEX_POINT('',#134020);
#31780=VERTEX_POINT('',#134034);
#31781=VERTEX_POINT('',#134038);
#31782=VERTEX_POINT('',#134047);
#31783=VERTEX_POINT('',#134049);
#31784=VERTEX_POINT('',#134063);
#31785=VERTEX_POINT('',#134067);
#31786=VERTEX_POINT('',#134076);
#31787=VERTEX_POINT('',#134078);
#31788=VERTEX_POINT('',#134092);
#31789=VERTEX_POINT('',#134096);
#31790=VERTEX_POINT('',#134105);
#31791=VERTEX_POINT('',#134107);
#31792=VERTEX_POINT('',#134121);
#31793=VERTEX_POINT('',#134125);
#31794=VERTEX_POINT('',#134134);
#31795=VERTEX_POINT('',#134136);
#31796=VERTEX_POINT('',#134150);
#31797=VERTEX_POINT('',#134154);
#31798=VERTEX_POINT('',#134163);
#31799=VERTEX_POINT('',#134165);
#31800=VERTEX_POINT('',#134179);
#31801=VERTEX_POINT('',#134183);
#31802=VERTEX_POINT('',#134192);
#31803=VERTEX_POINT('',#134194);
#31804=VERTEX_POINT('',#134208);
#31805=VERTEX_POINT('',#134212);
#31806=VERTEX_POINT('',#134221);
#31807=VERTEX_POINT('',#134223);
#31808=VERTEX_POINT('',#134237);
#31809=VERTEX_POINT('',#134241);
#31810=VERTEX_POINT('',#134250);
#31811=VERTEX_POINT('',#134252);
#31812=VERTEX_POINT('',#134266);
#31813=VERTEX_POINT('',#134270);
#31814=VERTEX_POINT('',#134279);
#31815=VERTEX_POINT('',#134281);
#31816=VERTEX_POINT('',#134295);
#31817=VERTEX_POINT('',#134299);
#31818=VERTEX_POINT('',#134308);
#31819=VERTEX_POINT('',#134310);
#31820=VERTEX_POINT('',#134324);
#31821=VERTEX_POINT('',#134328);
#31822=VERTEX_POINT('',#134337);
#31823=VERTEX_POINT('',#134339);
#31824=VERTEX_POINT('',#134353);
#31825=VERTEX_POINT('',#134357);
#31826=VERTEX_POINT('',#134366);
#31827=VERTEX_POINT('',#134368);
#31828=VERTEX_POINT('',#134382);
#31829=VERTEX_POINT('',#134386);
#31830=VERTEX_POINT('',#134395);
#31831=VERTEX_POINT('',#134397);
#31832=VERTEX_POINT('',#134411);
#31833=VERTEX_POINT('',#134415);
#31834=VERTEX_POINT('',#134424);
#31835=VERTEX_POINT('',#134426);
#31836=VERTEX_POINT('',#134440);
#31837=VERTEX_POINT('',#134444);
#31838=VERTEX_POINT('',#134453);
#31839=VERTEX_POINT('',#134455);
#31840=VERTEX_POINT('',#134469);
#31841=VERTEX_POINT('',#134473);
#31842=VERTEX_POINT('',#134482);
#31843=VERTEX_POINT('',#134484);
#31844=VERTEX_POINT('',#134498);
#31845=VERTEX_POINT('',#134502);
#31846=VERTEX_POINT('',#134511);
#31847=VERTEX_POINT('',#134513);
#31848=VERTEX_POINT('',#134527);
#31849=VERTEX_POINT('',#134531);
#31850=VERTEX_POINT('',#134540);
#31851=VERTEX_POINT('',#134542);
#31852=VERTEX_POINT('',#134556);
#31853=VERTEX_POINT('',#134560);
#31854=VERTEX_POINT('',#134569);
#31855=VERTEX_POINT('',#134571);
#31856=VERTEX_POINT('',#134585);
#31857=VERTEX_POINT('',#134589);
#31858=VERTEX_POINT('',#134602);
#31859=VERTEX_POINT('',#134648);
#31860=VERTEX_POINT('',#134694);
#31861=VERTEX_POINT('',#134740);
#31862=VERTEX_POINT('',#134786);
#31863=VERTEX_POINT('',#134832);
#31864=VERTEX_POINT('',#134882);
#31865=VERTEX_POINT('',#134928);
#31866=VERTEX_POINT('',#134974);
#31867=VERTEX_POINT('',#135020);
#31868=VERTEX_POINT('',#135066);
#31869=VERTEX_POINT('',#135112);
#31870=VERTEX_POINT('',#135158);
#31871=VERTEX_POINT('',#135208);
#31872=VERTEX_POINT('',#135258);
#31873=VERTEX_POINT('',#135308);
#31874=VERTEX_POINT('',#135354);
#31875=VERTEX_POINT('',#135400);
#31876=VERTEX_POINT('',#135446);
#31877=VERTEX_POINT('',#135492);
#31878=VERTEX_POINT('',#135538);
#31879=VERTEX_POINT('',#135584);
#31880=VERTEX_POINT('',#135630);
#31881=VERTEX_POINT('',#135676);
#31882=VERTEX_POINT('',#135722);
#31883=VERTEX_POINT('',#135768);
#31884=VERTEX_POINT('',#135814);
#31885=VERTEX_POINT('',#135860);
#31886=VERTEX_POINT('',#135906);
#31887=VERTEX_POINT('',#135956);
#31888=VERTEX_POINT('',#136006);
#31889=VERTEX_POINT('',#136052);
#31890=VERTEX_POINT('',#136102);
#31891=VERTEX_POINT('',#136151);
#31892=VERTEX_POINT('',#136201);
#31893=VERTEX_POINT('',#136247);
#31894=VERTEX_POINT('',#136297);
#31895=VERTEX_POINT('',#136343);
#31896=VERTEX_POINT('',#136389);
#31897=VERTEX_POINT('',#136439);
#31898=VERTEX_POINT('',#136480);
#31899=VERTEX_POINT('',#136521);
#31900=VERTEX_POINT('',#136567);
#31901=VERTEX_POINT('',#136617);
#31902=VERTEX_POINT('',#136663);
#31903=VERTEX_POINT('',#136707);
#31904=VERTEX_POINT('',#136757);
#31905=VERTEX_POINT('',#136798);
#31906=VERTEX_POINT('',#136848);
#31907=VERTEX_POINT('',#136897);
#31908=VERTEX_POINT('',#136946);
#31909=VERTEX_POINT('',#136996);
#31910=VERTEX_POINT('',#137046);
#31911=VERTEX_POINT('',#137087);
#31912=VERTEX_POINT('',#137128);
#31913=VERTEX_POINT('',#137178);
#31914=VERTEX_POINT('',#137219);
#31915=VERTEX_POINT('',#137265);
#31916=VERTEX_POINT('',#137318);
#31917=VERTEX_POINT('',#137319);
#31918=VERTEX_POINT('',#137338);
#31919=VERTEX_POINT('',#137339);
#31920=VERTEX_POINT('',#137355);
#31921=VERTEX_POINT('',#137357);
#31922=VERTEX_POINT('',#137381);
#31923=VERTEX_POINT('',#137382);
#31924=VERTEX_POINT('',#137398);
#31925=VERTEX_POINT('',#137400);
#31926=VERTEX_POINT('',#137424);
#31927=VERTEX_POINT('',#137425);
#31928=VERTEX_POINT('',#137441);
#31929=VERTEX_POINT('',#137443);
#31930=VERTEX_POINT('',#137467);
#31931=VERTEX_POINT('',#137468);
#31932=VERTEX_POINT('',#137484);
#31933=VERTEX_POINT('',#137486);
#31934=VERTEX_POINT('',#137510);
#31935=VERTEX_POINT('',#137511);
#31936=VERTEX_POINT('',#137527);
#31937=VERTEX_POINT('',#137529);
#31938=VERTEX_POINT('',#137553);
#31939=VERTEX_POINT('',#137554);
#31940=VERTEX_POINT('',#137570);
#31941=VERTEX_POINT('',#137572);
#31942=VERTEX_POINT('',#137624);
#31943=VERTEX_POINT('',#137625);
#31944=VERTEX_POINT('',#137641);
#31945=VERTEX_POINT('',#137643);
#31946=VERTEX_POINT('',#137667);
#31947=VERTEX_POINT('',#137668);
#31948=VERTEX_POINT('',#137684);
#31949=VERTEX_POINT('',#137686);
#31950=VERTEX_POINT('',#137710);
#31951=VERTEX_POINT('',#137711);
#31952=VERTEX_POINT('',#137727);
#31953=VERTEX_POINT('',#137729);
#31954=VERTEX_POINT('',#137753);
#31955=VERTEX_POINT('',#137754);
#31956=VERTEX_POINT('',#137770);
#31957=VERTEX_POINT('',#137772);
#31958=VERTEX_POINT('',#137796);
#31959=VERTEX_POINT('',#137797);
#31960=VERTEX_POINT('',#137813);
#31961=VERTEX_POINT('',#137815);
#31962=VERTEX_POINT('',#137839);
#31963=VERTEX_POINT('',#137840);
#31964=VERTEX_POINT('',#137856);
#31965=VERTEX_POINT('',#137858);
#31966=VERTEX_POINT('',#137882);
#31967=VERTEX_POINT('',#137883);
#31968=VERTEX_POINT('',#137899);
#31969=VERTEX_POINT('',#137901);
#31970=VERTEX_POINT('',#137925);
#31971=VERTEX_POINT('',#137926);
#31972=VERTEX_POINT('',#137942);
#31973=VERTEX_POINT('',#137944);
#31974=VERTEX_POINT('',#137968);
#31975=VERTEX_POINT('',#137969);
#31976=VERTEX_POINT('',#137985);
#31977=VERTEX_POINT('',#137987);
#31978=VERTEX_POINT('',#138011);
#31979=VERTEX_POINT('',#138012);
#31980=VERTEX_POINT('',#138028);
#31981=VERTEX_POINT('',#138030);
#31982=VERTEX_POINT('',#138054);
#31983=VERTEX_POINT('',#138055);
#31984=VERTEX_POINT('',#138071);
#31985=VERTEX_POINT('',#138073);
#31986=VERTEX_POINT('',#138097);
#31987=VERTEX_POINT('',#138098);
#31988=VERTEX_POINT('',#138114);
#31989=VERTEX_POINT('',#138116);
#31990=VERTEX_POINT('',#138140);
#31991=VERTEX_POINT('',#138141);
#31992=VERTEX_POINT('',#138166);
#31993=VERTEX_POINT('',#138170);
#31994=VERTEX_POINT('',#138183);
#31995=VERTEX_POINT('',#138185);
#31996=VERTEX_POINT('',#138200);
#31997=VERTEX_POINT('',#138202);
#31998=VERTEX_POINT('',#138226);
#31999=VERTEX_POINT('',#138227);
#32000=VERTEX_POINT('',#138243);
#32001=VERTEX_POINT('',#138245);
#32002=VERTEX_POINT('',#138269);
#32003=VERTEX_POINT('',#138270);
#32004=VERTEX_POINT('',#138286);
#32005=VERTEX_POINT('',#138288);
#32006=VERTEX_POINT('',#138312);
#32007=VERTEX_POINT('',#138313);
#32008=VERTEX_POINT('',#138329);
#32009=VERTEX_POINT('',#138331);
#32010=VERTEX_POINT('',#138355);
#32011=VERTEX_POINT('',#138356);
#32012=VERTEX_POINT('',#138372);
#32013=VERTEX_POINT('',#138374);
#32014=VERTEX_POINT('',#138398);
#32015=VERTEX_POINT('',#138399);
#32016=VERTEX_POINT('',#138415);
#32017=VERTEX_POINT('',#138417);
#32018=VERTEX_POINT('',#138441);
#32019=VERTEX_POINT('',#138442);
#32020=VERTEX_POINT('',#138458);
#32021=VERTEX_POINT('',#138460);
#32022=VERTEX_POINT('',#138484);
#32023=VERTEX_POINT('',#138485);
#32024=VERTEX_POINT('',#138501);
#32025=VERTEX_POINT('',#138503);
#32026=VERTEX_POINT('',#138518);
#32027=VERTEX_POINT('',#138519);
#32028=VERTEX_POINT('',#138550);
#32029=VERTEX_POINT('',#138557);
#32030=VERTEX_POINT('',#138570);
#32031=VERTEX_POINT('',#138572);
#32032=VERTEX_POINT('',#138596);
#32033=VERTEX_POINT('',#138600);
#32034=VERTEX_POINT('',#138613);
#32035=VERTEX_POINT('',#138615);
#32036=VERTEX_POINT('',#138639);
#32037=VERTEX_POINT('',#138643);
#32038=VERTEX_POINT('',#138656);
#32039=VERTEX_POINT('',#138658);
#32040=VERTEX_POINT('',#138682);
#32041=VERTEX_POINT('',#138686);
#32042=VERTEX_POINT('',#138699);
#32043=VERTEX_POINT('',#138701);
#32044=VERTEX_POINT('',#138725);
#32045=VERTEX_POINT('',#138729);
#32046=VERTEX_POINT('',#138742);
#32047=VERTEX_POINT('',#138744);
#32048=VERTEX_POINT('',#138768);
#32049=VERTEX_POINT('',#138772);
#32050=VERTEX_POINT('',#138785);
#32051=VERTEX_POINT('',#138787);
#32052=VERTEX_POINT('',#138811);
#32053=VERTEX_POINT('',#138815);
#32054=VERTEX_POINT('',#138828);
#32055=VERTEX_POINT('',#138830);
#32056=VERTEX_POINT('',#138854);
#32057=VERTEX_POINT('',#138858);
#32058=VERTEX_POINT('',#138871);
#32059=VERTEX_POINT('',#138873);
#32060=VERTEX_POINT('',#138897);
#32061=VERTEX_POINT('',#138901);
#32062=VERTEX_POINT('',#138914);
#32063=VERTEX_POINT('',#138916);
#32064=VERTEX_POINT('',#138940);
#32065=VERTEX_POINT('',#138944);
#32066=VERTEX_POINT('',#138957);
#32067=VERTEX_POINT('',#138959);
#32068=VERTEX_POINT('',#138983);
#32069=VERTEX_POINT('',#138987);
#32070=VERTEX_POINT('',#139000);
#32071=VERTEX_POINT('',#139002);
#32072=VERTEX_POINT('',#139026);
#32073=VERTEX_POINT('',#139030);
#32074=VERTEX_POINT('',#139043);
#32075=VERTEX_POINT('',#139045);
#32076=VERTEX_POINT('',#139069);
#32077=VERTEX_POINT('',#139073);
#32078=VERTEX_POINT('',#139086);
#32079=VERTEX_POINT('',#139088);
#32080=VERTEX_POINT('',#139112);
#32081=VERTEX_POINT('',#139116);
#32082=VERTEX_POINT('',#139157);
#32083=VERTEX_POINT('',#139159);
#32084=VERTEX_POINT('',#139183);
#32085=VERTEX_POINT('',#139187);
#32086=VERTEX_POINT('',#139200);
#32087=VERTEX_POINT('',#139202);
#32088=VERTEX_POINT('',#139226);
#32089=VERTEX_POINT('',#139230);
#32090=VERTEX_POINT('',#139243);
#32091=VERTEX_POINT('',#139245);
#32092=VERTEX_POINT('',#139269);
#32093=VERTEX_POINT('',#139273);
#32094=VERTEX_POINT('',#139286);
#32095=VERTEX_POINT('',#139288);
#32096=VERTEX_POINT('',#139312);
#32097=VERTEX_POINT('',#139316);
#32098=VERTEX_POINT('',#139329);
#32099=VERTEX_POINT('',#139331);
#32100=VERTEX_POINT('',#139355);
#32101=VERTEX_POINT('',#139359);
#32102=VERTEX_POINT('',#139372);
#32103=VERTEX_POINT('',#139374);
#32104=VERTEX_POINT('',#139398);
#32105=VERTEX_POINT('',#139402);
#32106=VERTEX_POINT('',#139415);
#32107=VERTEX_POINT('',#139417);
#32108=VERTEX_POINT('',#139441);
#32109=VERTEX_POINT('',#139445);
#32110=VERTEX_POINT('',#139458);
#32111=VERTEX_POINT('',#139460);
#32112=VERTEX_POINT('',#139484);
#32113=VERTEX_POINT('',#139488);
#32114=VERTEX_POINT('',#139501);
#32115=VERTEX_POINT('',#139503);
#32116=VERTEX_POINT('',#139527);
#32117=VERTEX_POINT('',#139531);
#32118=VERTEX_POINT('',#139544);
#32119=VERTEX_POINT('',#139546);
#32120=VERTEX_POINT('',#139570);
#32121=VERTEX_POINT('',#139574);
#32122=VERTEX_POINT('',#139587);
#32123=VERTEX_POINT('',#139589);
#32124=VERTEX_POINT('',#139613);
#32125=VERTEX_POINT('',#139617);
#32126=VERTEX_POINT('',#139630);
#32127=VERTEX_POINT('',#139632);
#32128=VERTEX_POINT('',#139656);
#32129=VERTEX_POINT('',#139660);
#32130=VERTEX_POINT('',#139673);
#32131=VERTEX_POINT('',#139675);
#32132=VERTEX_POINT('',#139699);
#32133=VERTEX_POINT('',#139703);
#32134=VERTEX_POINT('',#139716);
#32135=VERTEX_POINT('',#139718);
#32136=VERTEX_POINT('',#139742);
#32137=VERTEX_POINT('',#139746);
#32138=VERTEX_POINT('',#139750);
#32139=VERTEX_POINT('',#139758);
#32140=VERTEX_POINT('',#139782);
#32141=VERTEX_POINT('',#139796);
#32142=VERTEX_POINT('',#139821);
#32143=VERTEX_POINT('',#139846);
#32144=VERTEX_POINT('',#139871);
#32145=VERTEX_POINT('',#139896);
#32146=VERTEX_POINT('',#139921);
#32147=VERTEX_POINT('',#139946);
#32148=VERTEX_POINT('',#139971);
#32149=VERTEX_POINT('',#139996);
#32150=VERTEX_POINT('',#140021);
#32151=VERTEX_POINT('',#140046);
#32152=VERTEX_POINT('',#140071);
#32153=VERTEX_POINT('',#140096);
#32154=VERTEX_POINT('',#140121);
#32155=VERTEX_POINT('',#140146);
#32156=VERTEX_POINT('',#140171);
#32157=VERTEX_POINT('',#140196);
#32158=VERTEX_POINT('',#140221);
#32159=VERTEX_POINT('',#140246);
#32160=VERTEX_POINT('',#140271);
#32161=VERTEX_POINT('',#140296);
#32162=VERTEX_POINT('',#140321);
#32163=VERTEX_POINT('',#140346);
#32164=VERTEX_POINT('',#140371);
#32165=VERTEX_POINT('',#140396);
#32166=VERTEX_POINT('',#140421);
#32167=VERTEX_POINT('',#140446);
#32168=VERTEX_POINT('',#140471);
#32169=VERTEX_POINT('',#140507);
#32170=VERTEX_POINT('',#140525);
#32171=VERTEX_POINT('',#140554);
#32172=VERTEX_POINT('',#140583);
#32173=VERTEX_POINT('',#140612);
#32174=VERTEX_POINT('',#140646);
#32175=VERTEX_POINT('',#140675);
#32176=VERTEX_POINT('',#140704);
#32177=VERTEX_POINT('',#140733);
#32178=VERTEX_POINT('',#140762);
#32179=VERTEX_POINT('',#140791);
#32180=VERTEX_POINT('',#140820);
#32181=VERTEX_POINT('',#140849);
#32182=VERTEX_POINT('',#140878);
#32183=VERTEX_POINT('',#140912);
#32184=VERTEX_POINT('',#140941);
#32185=VERTEX_POINT('',#140970);
#32186=VERTEX_POINT('',#140999);
#32187=VERTEX_POINT('',#141033);
#32188=VERTEX_POINT('',#141062);
#32189=VERTEX_POINT('',#141091);
#32190=VERTEX_POINT('',#141120);
#32191=VERTEX_POINT('',#141149);
#32192=VERTEX_POINT('',#141178);
#32193=VERTEX_POINT('',#141212);
#32194=VERTEX_POINT('',#141246);
#32195=VERTEX_POINT('',#141275);
#32196=VERTEX_POINT('',#141304);
#32197=VERTEX_POINT('',#141333);
#32198=VERTEX_POINT('',#141374);
#32199=VERTEX_POINT('',#141375);
#32200=VERTEX_POINT('',#141385);
#32201=VERTEX_POINT('',#141387);
#32202=VERTEX_POINT('',#141407);
#32203=VERTEX_POINT('',#141408);
#32204=VERTEX_POINT('',#141418);
#32205=VERTEX_POINT('',#141420);
#32206=VERTEX_POINT('',#141440);
#32207=VERTEX_POINT('',#141441);
#32208=VERTEX_POINT('',#141451);
#32209=VERTEX_POINT('',#141453);
#32210=VERTEX_POINT('',#141473);
#32211=VERTEX_POINT('',#141474);
#32212=VERTEX_POINT('',#141484);
#32213=VERTEX_POINT('',#141486);
#32214=VERTEX_POINT('',#141506);
#32215=VERTEX_POINT('',#141507);
#32216=VERTEX_POINT('',#141517);
#32217=VERTEX_POINT('',#141519);
#32218=VERTEX_POINT('',#141539);
#32219=VERTEX_POINT('',#141540);
#32220=VERTEX_POINT('',#141550);
#32221=VERTEX_POINT('',#141552);
#32222=VERTEX_POINT('',#141572);
#32223=VERTEX_POINT('',#141573);
#32224=VERTEX_POINT('',#141583);
#32225=VERTEX_POINT('',#141585);
#32226=VERTEX_POINT('',#141605);
#32227=VERTEX_POINT('',#141606);
#32228=VERTEX_POINT('',#141616);
#32229=VERTEX_POINT('',#141618);
#32230=VERTEX_POINT('',#141638);
#32231=VERTEX_POINT('',#141639);
#32232=VERTEX_POINT('',#141649);
#32233=VERTEX_POINT('',#141651);
#32234=VERTEX_POINT('',#141671);
#32235=VERTEX_POINT('',#141672);
#32236=VERTEX_POINT('',#141682);
#32237=VERTEX_POINT('',#141684);
#32238=VERTEX_POINT('',#141704);
#32239=VERTEX_POINT('',#141705);
#32240=VERTEX_POINT('',#141715);
#32241=VERTEX_POINT('',#141717);
#32242=VERTEX_POINT('',#141737);
#32243=VERTEX_POINT('',#141738);
#32244=VERTEX_POINT('',#141748);
#32245=VERTEX_POINT('',#141750);
#32246=VERTEX_POINT('',#141770);
#32247=VERTEX_POINT('',#141771);
#32248=VERTEX_POINT('',#141781);
#32249=VERTEX_POINT('',#141783);
#32250=VERTEX_POINT('',#141803);
#32251=VERTEX_POINT('',#141804);
#32252=VERTEX_POINT('',#141814);
#32253=VERTEX_POINT('',#141816);
#32254=VERTEX_POINT('',#141860);
#32255=VERTEX_POINT('',#141861);
#32256=VERTEX_POINT('',#141871);
#32257=VERTEX_POINT('',#141873);
#32258=VERTEX_POINT('',#141893);
#32259=VERTEX_POINT('',#141894);
#32260=VERTEX_POINT('',#141904);
#32261=VERTEX_POINT('',#141906);
#32262=VERTEX_POINT('',#141926);
#32263=VERTEX_POINT('',#141927);
#32264=VERTEX_POINT('',#141937);
#32265=VERTEX_POINT('',#141939);
#32266=VERTEX_POINT('',#141959);
#32267=VERTEX_POINT('',#141960);
#32268=VERTEX_POINT('',#141970);
#32269=VERTEX_POINT('',#141972);
#32270=VERTEX_POINT('',#141992);
#32271=VERTEX_POINT('',#141993);
#32272=VERTEX_POINT('',#142012);
#32273=VERTEX_POINT('',#142016);
#32274=VERTEX_POINT('',#142025);
#32275=VERTEX_POINT('',#142027);
#32276=VERTEX_POINT('',#142036);
#32277=VERTEX_POINT('',#142038);
#32278=VERTEX_POINT('',#142058);
#32279=VERTEX_POINT('',#142059);
#32280=VERTEX_POINT('',#142069);
#32281=VERTEX_POINT('',#142071);
#32282=VERTEX_POINT('',#142091);
#32283=VERTEX_POINT('',#142092);
#32284=VERTEX_POINT('',#142102);
#32285=VERTEX_POINT('',#142104);
#32286=VERTEX_POINT('',#142124);
#32287=VERTEX_POINT('',#142125);
#32288=VERTEX_POINT('',#142135);
#32289=VERTEX_POINT('',#142137);
#32290=VERTEX_POINT('',#142157);
#32291=VERTEX_POINT('',#142158);
#32292=VERTEX_POINT('',#142168);
#32293=VERTEX_POINT('',#142170);
#32294=VERTEX_POINT('',#142190);
#32295=VERTEX_POINT('',#142191);
#32296=VERTEX_POINT('',#142201);
#32297=VERTEX_POINT('',#142203);
#32298=VERTEX_POINT('',#142223);
#32299=VERTEX_POINT('',#142224);
#32300=VERTEX_POINT('',#142234);
#32301=VERTEX_POINT('',#142236);
#32302=VERTEX_POINT('',#142256);
#32303=VERTEX_POINT('',#142257);
#32304=VERTEX_POINT('',#142267);
#32305=VERTEX_POINT('',#142269);
#32306=VERTEX_POINT('',#142289);
#32307=VERTEX_POINT('',#142290);
#32308=VERTEX_POINT('',#142300);
#32309=VERTEX_POINT('',#142302);
#32310=VERTEX_POINT('',#142326);
#32311=VERTEX_POINT('',#142328);
#32312=VERTEX_POINT('',#142350);
#32313=VERTEX_POINT('',#142354);
#32314=VERTEX_POINT('',#142367);
#32315=VERTEX_POINT('',#142369);
#32316=VERTEX_POINT('',#142391);
#32317=VERTEX_POINT('',#142395);
#32318=VERTEX_POINT('',#142408);
#32319=VERTEX_POINT('',#142410);
#32320=VERTEX_POINT('',#142432);
#32321=VERTEX_POINT('',#142436);
#32322=VERTEX_POINT('',#142449);
#32323=VERTEX_POINT('',#142451);
#32324=VERTEX_POINT('',#142473);
#32325=VERTEX_POINT('',#142477);
#32326=VERTEX_POINT('',#142490);
#32327=VERTEX_POINT('',#142492);
#32328=VERTEX_POINT('',#142514);
#32329=VERTEX_POINT('',#142518);
#32330=VERTEX_POINT('',#142531);
#32331=VERTEX_POINT('',#142533);
#32332=VERTEX_POINT('',#142555);
#32333=VERTEX_POINT('',#142559);
#32334=VERTEX_POINT('',#142572);
#32335=VERTEX_POINT('',#142574);
#32336=VERTEX_POINT('',#142596);
#32337=VERTEX_POINT('',#142600);
#32338=VERTEX_POINT('',#142613);
#32339=VERTEX_POINT('',#142615);
#32340=VERTEX_POINT('',#142637);
#32341=VERTEX_POINT('',#142641);
#32342=VERTEX_POINT('',#142654);
#32343=VERTEX_POINT('',#142656);
#32344=VERTEX_POINT('',#142678);
#32345=VERTEX_POINT('',#142682);
#32346=VERTEX_POINT('',#142695);
#32347=VERTEX_POINT('',#142697);
#32348=VERTEX_POINT('',#142719);
#32349=VERTEX_POINT('',#142723);
#32350=VERTEX_POINT('',#142736);
#32351=VERTEX_POINT('',#142738);
#32352=VERTEX_POINT('',#142760);
#32353=VERTEX_POINT('',#142764);
#32354=VERTEX_POINT('',#142777);
#32355=VERTEX_POINT('',#142779);
#32356=VERTEX_POINT('',#142801);
#32357=VERTEX_POINT('',#142805);
#32358=VERTEX_POINT('',#142818);
#32359=VERTEX_POINT('',#142820);
#32360=VERTEX_POINT('',#142842);
#32361=VERTEX_POINT('',#142846);
#32362=VERTEX_POINT('',#142859);
#32363=VERTEX_POINT('',#142861);
#32364=VERTEX_POINT('',#142883);
#32365=VERTEX_POINT('',#142887);
#32366=VERTEX_POINT('',#142900);
#32367=VERTEX_POINT('',#142902);
#32368=VERTEX_POINT('',#142924);
#32369=VERTEX_POINT('',#142928);
#32370=VERTEX_POINT('',#142941);
#32371=VERTEX_POINT('',#142943);
#32372=VERTEX_POINT('',#142965);
#32373=VERTEX_POINT('',#142969);
#32374=VERTEX_POINT('',#142982);
#32375=VERTEX_POINT('',#142984);
#32376=VERTEX_POINT('',#143006);
#32377=VERTEX_POINT('',#143010);
#32378=VERTEX_POINT('',#143023);
#32379=VERTEX_POINT('',#143025);
#32380=VERTEX_POINT('',#143047);
#32381=VERTEX_POINT('',#143051);
#32382=VERTEX_POINT('',#143064);
#32383=VERTEX_POINT('',#143066);
#32384=VERTEX_POINT('',#143088);
#32385=VERTEX_POINT('',#143092);
#32386=VERTEX_POINT('',#143105);
#32387=VERTEX_POINT('',#143107);
#32388=VERTEX_POINT('',#143129);
#32389=VERTEX_POINT('',#143133);
#32390=VERTEX_POINT('',#143146);
#32391=VERTEX_POINT('',#143148);
#32392=VERTEX_POINT('',#143170);
#32393=VERTEX_POINT('',#143174);
#32394=VERTEX_POINT('',#143219);
#32395=VERTEX_POINT('',#143221);
#32396=VERTEX_POINT('',#143243);
#32397=VERTEX_POINT('',#143247);
#32398=VERTEX_POINT('',#143260);
#32399=VERTEX_POINT('',#143262);
#32400=VERTEX_POINT('',#143284);
#32401=VERTEX_POINT('',#143288);
#32402=VERTEX_POINT('',#143301);
#32403=VERTEX_POINT('',#143303);
#32404=VERTEX_POINT('',#143325);
#32405=VERTEX_POINT('',#143329);
#32406=VERTEX_POINT('',#143342);
#32407=VERTEX_POINT('',#143344);
#32408=VERTEX_POINT('',#143366);
#32409=VERTEX_POINT('',#143370);
#32410=VERTEX_POINT('',#143383);
#32411=VERTEX_POINT('',#143385);
#32412=VERTEX_POINT('',#143407);
#32413=VERTEX_POINT('',#143411);
#32414=VERTEX_POINT('',#143424);
#32415=VERTEX_POINT('',#143426);
#32416=VERTEX_POINT('',#143448);
#32417=VERTEX_POINT('',#143452);
#32418=VERTEX_POINT('',#143465);
#32419=VERTEX_POINT('',#143467);
#32420=VERTEX_POINT('',#143489);
#32421=VERTEX_POINT('',#143493);
#32422=VERTEX_POINT('',#143502);
#32423=VERTEX_POINT('',#143527);
#32424=VERTEX_POINT('',#143552);
#32425=VERTEX_POINT('',#143577);
#32426=VERTEX_POINT('',#143602);
#32427=VERTEX_POINT('',#143627);
#32428=VERTEX_POINT('',#143652);
#32429=VERTEX_POINT('',#143677);
#32430=VERTEX_POINT('',#143702);
#32431=VERTEX_POINT('',#143727);
#32432=VERTEX_POINT('',#143752);
#32433=VERTEX_POINT('',#143777);
#32434=VERTEX_POINT('',#143802);
#32435=VERTEX_POINT('',#143827);
#32436=VERTEX_POINT('',#143852);
#32437=VERTEX_POINT('',#143877);
#32438=VERTEX_POINT('',#143902);
#32439=VERTEX_POINT('',#143927);
#32440=VERTEX_POINT('',#143952);
#32441=VERTEX_POINT('',#143977);
#32442=VERTEX_POINT('',#144002);
#32443=VERTEX_POINT('',#144027);
#32444=VERTEX_POINT('',#144052);
#32445=VERTEX_POINT('',#144077);
#32446=VERTEX_POINT('',#144102);
#32447=VERTEX_POINT('',#144127);
#32448=VERTEX_POINT('',#144152);
#32449=VERTEX_POINT('',#144177);
#32450=VERTEX_POINT('',#144202);
#32451=VERTEX_POINT('',#144227);
#32452=VERTEX_POINT('',#144248);
#32453=VERTEX_POINT('',#144269);
#32454=VERTEX_POINT('',#144290);
#32455=VERTEX_POINT('',#144311);
#32456=VERTEX_POINT('',#144332);
#32457=VERTEX_POINT('',#144353);
#32458=VERTEX_POINT('',#144374);
#32459=VERTEX_POINT('',#144395);
#32460=VERTEX_POINT('',#144416);
#32461=VERTEX_POINT('',#144437);
#32462=VERTEX_POINT('',#144458);
#32463=VERTEX_POINT('',#144479);
#32464=VERTEX_POINT('',#144500);
#32465=VERTEX_POINT('',#144521);
#32466=VERTEX_POINT('',#144542);
#32467=VERTEX_POINT('',#144563);
#32468=VERTEX_POINT('',#144584);
#32469=VERTEX_POINT('',#144605);
#32470=VERTEX_POINT('',#144626);
#32471=VERTEX_POINT('',#144647);
#32472=VERTEX_POINT('',#144668);
#32473=VERTEX_POINT('',#144689);
#32474=VERTEX_POINT('',#144710);
#32475=VERTEX_POINT('',#144731);
#32476=VERTEX_POINT('',#144752);
#32477=VERTEX_POINT('',#144773);
#32478=VERTEX_POINT('',#144794);
#32479=VERTEX_POINT('',#144815);
#32480=VERTEX_POINT('',#144836);
#32481=VERTEX_POINT('',#144837);
#32482=VERTEX_POINT('',#144852);
#32483=VERTEX_POINT('',#144853);
#32484=VERTEX_POINT('',#144863);
#32485=VERTEX_POINT('',#144865);
#32486=VERTEX_POINT('',#144881);
#32487=VERTEX_POINT('',#144882);
#32488=VERTEX_POINT('',#144892);
#32489=VERTEX_POINT('',#144894);
#32490=VERTEX_POINT('',#144910);
#32491=VERTEX_POINT('',#144911);
#32492=VERTEX_POINT('',#144921);
#32493=VERTEX_POINT('',#144923);
#32494=VERTEX_POINT('',#144939);
#32495=VERTEX_POINT('',#144940);
#32496=VERTEX_POINT('',#144950);
#32497=VERTEX_POINT('',#144952);
#32498=VERTEX_POINT('',#144968);
#32499=VERTEX_POINT('',#144969);
#32500=VERTEX_POINT('',#144979);
#32501=VERTEX_POINT('',#144981);
#32502=VERTEX_POINT('',#144997);
#32503=VERTEX_POINT('',#144998);
#32504=VERTEX_POINT('',#145008);
#32505=VERTEX_POINT('',#145010);
#32506=VERTEX_POINT('',#145046);
#32507=VERTEX_POINT('',#145047);
#32508=VERTEX_POINT('',#145057);
#32509=VERTEX_POINT('',#145059);
#32510=VERTEX_POINT('',#145075);
#32511=VERTEX_POINT('',#145076);
#32512=VERTEX_POINT('',#145086);
#32513=VERTEX_POINT('',#145088);
#32514=VERTEX_POINT('',#145104);
#32515=VERTEX_POINT('',#145105);
#32516=VERTEX_POINT('',#145115);
#32517=VERTEX_POINT('',#145117);
#32518=VERTEX_POINT('',#145133);
#32519=VERTEX_POINT('',#145134);
#32520=VERTEX_POINT('',#145144);
#32521=VERTEX_POINT('',#145146);
#32522=VERTEX_POINT('',#145162);
#32523=VERTEX_POINT('',#145163);
#32524=VERTEX_POINT('',#145173);
#32525=VERTEX_POINT('',#145175);
#32526=VERTEX_POINT('',#145191);
#32527=VERTEX_POINT('',#145192);
#32528=VERTEX_POINT('',#145202);
#32529=VERTEX_POINT('',#145204);
#32530=VERTEX_POINT('',#145220);
#32531=VERTEX_POINT('',#145221);
#32532=VERTEX_POINT('',#145231);
#32533=VERTEX_POINT('',#145233);
#32534=VERTEX_POINT('',#145249);
#32535=VERTEX_POINT('',#145250);
#32536=VERTEX_POINT('',#145260);
#32537=VERTEX_POINT('',#145262);
#32538=VERTEX_POINT('',#145278);
#32539=VERTEX_POINT('',#145279);
#32540=VERTEX_POINT('',#145289);
#32541=VERTEX_POINT('',#145291);
#32542=VERTEX_POINT('',#145307);
#32543=VERTEX_POINT('',#145308);
#32544=VERTEX_POINT('',#145318);
#32545=VERTEX_POINT('',#145320);
#32546=VERTEX_POINT('',#145336);
#32547=VERTEX_POINT('',#145337);
#32548=VERTEX_POINT('',#145347);
#32549=VERTEX_POINT('',#145349);
#32550=VERTEX_POINT('',#145365);
#32551=VERTEX_POINT('',#145366);
#32552=VERTEX_POINT('',#145381);
#32553=VERTEX_POINT('',#145385);
#32554=VERTEX_POINT('',#145394);
#32555=VERTEX_POINT('',#145396);
#32556=VERTEX_POINT('',#145405);
#32557=VERTEX_POINT('',#145407);
#32558=VERTEX_POINT('',#145423);
#32559=VERTEX_POINT('',#145424);
#32560=VERTEX_POINT('',#145434);
#32561=VERTEX_POINT('',#145436);
#32562=VERTEX_POINT('',#145452);
#32563=VERTEX_POINT('',#145453);
#32564=VERTEX_POINT('',#145463);
#32565=VERTEX_POINT('',#145465);
#32566=VERTEX_POINT('',#145481);
#32567=VERTEX_POINT('',#145482);
#32568=VERTEX_POINT('',#145492);
#32569=VERTEX_POINT('',#145494);
#32570=VERTEX_POINT('',#145510);
#32571=VERTEX_POINT('',#145511);
#32572=VERTEX_POINT('',#145521);
#32573=VERTEX_POINT('',#145523);
#32574=VERTEX_POINT('',#145539);
#32575=VERTEX_POINT('',#145540);
#32576=VERTEX_POINT('',#145550);
#32577=VERTEX_POINT('',#145552);
#32578=VERTEX_POINT('',#145568);
#32579=VERTEX_POINT('',#145569);
#32580=VERTEX_POINT('',#145579);
#32581=VERTEX_POINT('',#145581);
#32582=VERTEX_POINT('',#145597);
#32583=VERTEX_POINT('',#145598);
#32584=VERTEX_POINT('',#145608);
#32585=VERTEX_POINT('',#145610);
#32586=VERTEX_POINT('',#145626);
#32587=VERTEX_POINT('',#145627);
#32588=VERTEX_POINT('',#145637);
#32589=VERTEX_POINT('',#145639);
#32590=VERTEX_POINT('',#145650);
#32591=VERTEX_POINT('',#145651);
#32592=VERTEX_POINT('',#145668);
#32593=VERTEX_POINT('',#145675);
#32594=VERTEX_POINT('',#145688);
#32595=VERTEX_POINT('',#145690);
#32596=VERTEX_POINT('',#145704);
#32597=VERTEX_POINT('',#145708);
#32598=VERTEX_POINT('',#145721);
#32599=VERTEX_POINT('',#145723);
#32600=VERTEX_POINT('',#145737);
#32601=VERTEX_POINT('',#145741);
#32602=VERTEX_POINT('',#145754);
#32603=VERTEX_POINT('',#145756);
#32604=VERTEX_POINT('',#145770);
#32605=VERTEX_POINT('',#145774);
#32606=VERTEX_POINT('',#145787);
#32607=VERTEX_POINT('',#145789);
#32608=VERTEX_POINT('',#145803);
#32609=VERTEX_POINT('',#145807);
#32610=VERTEX_POINT('',#145820);
#32611=VERTEX_POINT('',#145822);
#32612=VERTEX_POINT('',#145836);
#32613=VERTEX_POINT('',#145840);
#32614=VERTEX_POINT('',#145853);
#32615=VERTEX_POINT('',#145855);
#32616=VERTEX_POINT('',#145869);
#32617=VERTEX_POINT('',#145873);
#32618=VERTEX_POINT('',#145886);
#32619=VERTEX_POINT('',#145888);
#32620=VERTEX_POINT('',#145902);
#32621=VERTEX_POINT('',#145906);
#32622=VERTEX_POINT('',#145919);
#32623=VERTEX_POINT('',#145921);
#32624=VERTEX_POINT('',#145935);
#32625=VERTEX_POINT('',#145939);
#32626=VERTEX_POINT('',#145952);
#32627=VERTEX_POINT('',#145954);
#32628=VERTEX_POINT('',#145968);
#32629=VERTEX_POINT('',#145972);
#32630=VERTEX_POINT('',#145985);
#32631=VERTEX_POINT('',#145987);
#32632=VERTEX_POINT('',#146001);
#32633=VERTEX_POINT('',#146005);
#32634=VERTEX_POINT('',#146018);
#32635=VERTEX_POINT('',#146020);
#32636=VERTEX_POINT('',#146034);
#32637=VERTEX_POINT('',#146038);
#32638=VERTEX_POINT('',#146051);
#32639=VERTEX_POINT('',#146053);
#32640=VERTEX_POINT('',#146067);
#32641=VERTEX_POINT('',#146071);
#32642=VERTEX_POINT('',#146084);
#32643=VERTEX_POINT('',#146086);
#32644=VERTEX_POINT('',#146100);
#32645=VERTEX_POINT('',#146104);
#32646=VERTEX_POINT('',#146141);
#32647=VERTEX_POINT('',#146143);
#32648=VERTEX_POINT('',#146157);
#32649=VERTEX_POINT('',#146161);
#32650=VERTEX_POINT('',#146174);
#32651=VERTEX_POINT('',#146176);
#32652=VERTEX_POINT('',#146190);
#32653=VERTEX_POINT('',#146194);
#32654=VERTEX_POINT('',#146207);
#32655=VERTEX_POINT('',#146209);
#32656=VERTEX_POINT('',#146223);
#32657=VERTEX_POINT('',#146227);
#32658=VERTEX_POINT('',#146240);
#32659=VERTEX_POINT('',#146242);
#32660=VERTEX_POINT('',#146256);
#32661=VERTEX_POINT('',#146260);
#32662=VERTEX_POINT('',#146273);
#32663=VERTEX_POINT('',#146275);
#32664=VERTEX_POINT('',#146289);
#32665=VERTEX_POINT('',#146293);
#32666=VERTEX_POINT('',#146306);
#32667=VERTEX_POINT('',#146308);
#32668=VERTEX_POINT('',#146322);
#32669=VERTEX_POINT('',#146326);
#32670=VERTEX_POINT('',#146339);
#32671=VERTEX_POINT('',#146341);
#32672=VERTEX_POINT('',#146355);
#32673=VERTEX_POINT('',#146359);
#32674=VERTEX_POINT('',#146372);
#32675=VERTEX_POINT('',#146374);
#32676=VERTEX_POINT('',#146388);
#32677=VERTEX_POINT('',#146392);
#32678=VERTEX_POINT('',#146405);
#32679=VERTEX_POINT('',#146407);
#32680=VERTEX_POINT('',#146421);
#32681=VERTEX_POINT('',#146425);
#32682=VERTEX_POINT('',#146438);
#32683=VERTEX_POINT('',#146440);
#32684=VERTEX_POINT('',#146454);
#32685=VERTEX_POINT('',#146458);
#32686=VERTEX_POINT('',#146471);
#32687=VERTEX_POINT('',#146473);
#32688=VERTEX_POINT('',#146487);
#32689=VERTEX_POINT('',#146491);
#32690=VERTEX_POINT('',#146504);
#32691=VERTEX_POINT('',#146506);
#32692=VERTEX_POINT('',#146520);
#32693=VERTEX_POINT('',#146524);
#32694=VERTEX_POINT('',#146537);
#32695=VERTEX_POINT('',#146539);
#32696=VERTEX_POINT('',#146553);
#32697=VERTEX_POINT('',#146557);
#32698=VERTEX_POINT('',#146570);
#32699=VERTEX_POINT('',#146572);
#32700=VERTEX_POINT('',#146586);
#32701=VERTEX_POINT('',#146590);
#32702=VERTEX_POINT('',#146594);
#32703=VERTEX_POINT('',#146596);
#32704=VERTEX_POINT('',#146620);
#32705=VERTEX_POINT('',#146649);
#32706=VERTEX_POINT('',#146695);
#32707=VERTEX_POINT('',#146736);
#32708=VERTEX_POINT('',#146786);
#32709=VERTEX_POINT('',#146827);
#32710=VERTEX_POINT('',#146868);
#32711=VERTEX_POINT('',#146918);
#32712=VERTEX_POINT('',#146968);
#32713=VERTEX_POINT('',#147017);
#32714=VERTEX_POINT('',#147066);
#32715=VERTEX_POINT('',#147116);
#32716=VERTEX_POINT('',#147157);
#32717=VERTEX_POINT('',#147207);
#32718=VERTEX_POINT('',#147251);
#32719=VERTEX_POINT('',#147297);
#32720=VERTEX_POINT('',#147347);
#32721=VERTEX_POINT('',#147393);
#32722=VERTEX_POINT('',#147434);
#32723=VERTEX_POINT('',#147480);
#32724=VERTEX_POINT('',#147530);
#32725=VERTEX_POINT('',#147576);
#32726=VERTEX_POINT('',#147622);
#32727=VERTEX_POINT('',#147672);
#32728=VERTEX_POINT('',#147718);
#32729=VERTEX_POINT('',#147768);
#32730=VERTEX_POINT('',#147817);
#32731=VERTEX_POINT('',#147867);
#32732=VERTEX_POINT('',#147913);
#32733=VERTEX_POINT('',#147983);
#32734=VERTEX_POINT('',#148001);
#32735=VERTEX_POINT('',#148026);
#32736=VERTEX_POINT('',#148051);
#32737=VERTEX_POINT('',#148076);
#32738=VERTEX_POINT('',#148101);
#32739=VERTEX_POINT('',#148126);
#32740=VERTEX_POINT('',#148151);
#32741=VERTEX_POINT('',#148176);
#32742=VERTEX_POINT('',#148201);
#32743=VERTEX_POINT('',#148226);
#32744=VERTEX_POINT('',#148251);
#32745=VERTEX_POINT('',#148276);
#32746=VERTEX_POINT('',#148301);
#32747=VERTEX_POINT('',#148326);
#32748=VERTEX_POINT('',#148351);
#32749=VERTEX_POINT('',#148376);
#32750=VERTEX_POINT('',#148401);
#32751=VERTEX_POINT('',#148426);
#32752=VERTEX_POINT('',#148451);
#32753=VERTEX_POINT('',#148476);
#32754=VERTEX_POINT('',#148501);
#32755=VERTEX_POINT('',#148526);
#32756=VERTEX_POINT('',#148551);
#32757=VERTEX_POINT('',#148576);
#32758=VERTEX_POINT('',#148601);
#32759=VERTEX_POINT('',#148626);
#32760=VERTEX_POINT('',#148651);
#32761=VERTEX_POINT('',#148676);
#32762=VERTEX_POINT('',#148712);
#32763=VERTEX_POINT('',#148713);
#32764=VERTEX_POINT('',#148723);
#32765=VERTEX_POINT('',#148725);
#32766=VERTEX_POINT('',#148755);
#32767=VERTEX_POINT('',#148756);
#32768=VERTEX_POINT('',#148766);
#32769=VERTEX_POINT('',#148768);
#32770=VERTEX_POINT('',#148798);
#32771=VERTEX_POINT('',#148799);
#32772=VERTEX_POINT('',#148809);
#32773=VERTEX_POINT('',#148811);
#32774=VERTEX_POINT('',#148841);
#32775=VERTEX_POINT('',#148842);
#32776=VERTEX_POINT('',#148852);
#32777=VERTEX_POINT('',#148854);
#32778=VERTEX_POINT('',#148884);
#32779=VERTEX_POINT('',#148885);
#32780=VERTEX_POINT('',#148895);
#32781=VERTEX_POINT('',#148897);
#32782=VERTEX_POINT('',#148927);
#32783=VERTEX_POINT('',#148928);
#32784=VERTEX_POINT('',#148938);
#32785=VERTEX_POINT('',#148940);
#32786=VERTEX_POINT('',#148970);
#32787=VERTEX_POINT('',#148971);
#32788=VERTEX_POINT('',#148981);
#32789=VERTEX_POINT('',#148983);
#32790=VERTEX_POINT('',#149013);
#32791=VERTEX_POINT('',#149014);
#32792=VERTEX_POINT('',#149024);
#32793=VERTEX_POINT('',#149026);
#32794=VERTEX_POINT('',#149056);
#32795=VERTEX_POINT('',#149057);
#32796=VERTEX_POINT('',#149067);
#32797=VERTEX_POINT('',#149069);
#32798=VERTEX_POINT('',#149099);
#32799=VERTEX_POINT('',#149100);
#32800=VERTEX_POINT('',#149110);
#32801=VERTEX_POINT('',#149112);
#32802=VERTEX_POINT('',#149142);
#32803=VERTEX_POINT('',#149143);
#32804=VERTEX_POINT('',#149153);
#32805=VERTEX_POINT('',#149155);
#32806=VERTEX_POINT('',#149185);
#32807=VERTEX_POINT('',#149186);
#32808=VERTEX_POINT('',#149196);
#32809=VERTEX_POINT('',#149198);
#32810=VERTEX_POINT('',#149228);
#32811=VERTEX_POINT('',#149229);
#32812=VERTEX_POINT('',#149239);
#32813=VERTEX_POINT('',#149241);
#32814=VERTEX_POINT('',#149271);
#32815=VERTEX_POINT('',#149272);
#32816=VERTEX_POINT('',#149282);
#32817=VERTEX_POINT('',#149284);
#32818=VERTEX_POINT('',#149342);
#32819=VERTEX_POINT('',#149343);
#32820=VERTEX_POINT('',#149353);
#32821=VERTEX_POINT('',#149355);
#32822=VERTEX_POINT('',#149385);
#32823=VERTEX_POINT('',#149386);
#32824=VERTEX_POINT('',#149396);
#32825=VERTEX_POINT('',#149398);
#32826=VERTEX_POINT('',#149428);
#32827=VERTEX_POINT('',#149429);
#32828=VERTEX_POINT('',#149439);
#32829=VERTEX_POINT('',#149441);
#32830=VERTEX_POINT('',#149471);
#32831=VERTEX_POINT('',#149472);
#32832=VERTEX_POINT('',#149491);
#32833=VERTEX_POINT('',#149501);
#32834=VERTEX_POINT('',#149514);
#32835=VERTEX_POINT('',#149516);
#32836=VERTEX_POINT('',#149525);
#32837=VERTEX_POINT('',#149533);
#32838=VERTEX_POINT('',#149557);
#32839=VERTEX_POINT('',#149558);
#32840=VERTEX_POINT('',#149568);
#32841=VERTEX_POINT('',#149570);
#32842=VERTEX_POINT('',#149600);
#32843=VERTEX_POINT('',#149601);
#32844=VERTEX_POINT('',#149611);
#32845=VERTEX_POINT('',#149613);
#32846=VERTEX_POINT('',#149643);
#32847=VERTEX_POINT('',#149644);
#32848=VERTEX_POINT('',#149654);
#32849=VERTEX_POINT('',#149656);
#32850=VERTEX_POINT('',#149686);
#32851=VERTEX_POINT('',#149687);
#32852=VERTEX_POINT('',#149697);
#32853=VERTEX_POINT('',#149699);
#32854=VERTEX_POINT('',#149729);
#32855=VERTEX_POINT('',#149730);
#32856=VERTEX_POINT('',#149740);
#32857=VERTEX_POINT('',#149742);
#32858=VERTEX_POINT('',#149772);
#32859=VERTEX_POINT('',#149773);
#32860=VERTEX_POINT('',#149783);
#32861=VERTEX_POINT('',#149785);
#32862=VERTEX_POINT('',#149815);
#32863=VERTEX_POINT('',#149816);
#32864=VERTEX_POINT('',#149826);
#32865=VERTEX_POINT('',#149828);
#32866=VERTEX_POINT('',#149858);
#32867=VERTEX_POINT('',#149859);
#32868=VERTEX_POINT('',#149869);
#32869=VERTEX_POINT('',#149871);
#32870=VERTEX_POINT('',#149901);
#32871=VERTEX_POINT('',#149902);
#32872=VERTEX_POINT('',#149912);
#32873=VERTEX_POINT('',#149914);
#32874=VERTEX_POINT('',#149944);
#32875=VERTEX_POINT('',#149946);
#32876=VERTEX_POINT('',#149955);
#32877=VERTEX_POINT('',#149956);
#32878=VERTEX_POINT('',#149958);
#32879=VERTEX_POINT('',#149967);
#32880=VERTEX_POINT('',#149983);
#32881=VERTEX_POINT('',#149985);
#32882=VERTEX_POINT('',#149994);
#32883=VERTEX_POINT('',#149995);
#32884=VERTEX_POINT('',#149997);
#32885=VERTEX_POINT('',#150006);
#32886=VERTEX_POINT('',#150022);
#32887=VERTEX_POINT('',#150024);
#32888=VERTEX_POINT('',#150033);
#32889=VERTEX_POINT('',#150034);
#32890=VERTEX_POINT('',#150036);
#32891=VERTEX_POINT('',#150045);
#32892=VERTEX_POINT('',#150061);
#32893=VERTEX_POINT('',#150063);
#32894=VERTEX_POINT('',#150072);
#32895=VERTEX_POINT('',#150073);
#32896=VERTEX_POINT('',#150075);
#32897=VERTEX_POINT('',#150084);
#32898=VERTEX_POINT('',#150100);
#32899=VERTEX_POINT('',#150102);
#32900=VERTEX_POINT('',#150111);
#32901=VERTEX_POINT('',#150112);
#32902=VERTEX_POINT('',#150114);
#32903=VERTEX_POINT('',#150123);
#32904=VERTEX_POINT('',#150139);
#32905=VERTEX_POINT('',#150141);
#32906=VERTEX_POINT('',#150150);
#32907=VERTEX_POINT('',#150151);
#32908=VERTEX_POINT('',#150153);
#32909=VERTEX_POINT('',#150162);
#32910=VERTEX_POINT('',#150178);
#32911=VERTEX_POINT('',#150180);
#32912=VERTEX_POINT('',#150189);
#32913=VERTEX_POINT('',#150190);
#32914=VERTEX_POINT('',#150192);
#32915=VERTEX_POINT('',#150201);
#32916=VERTEX_POINT('',#150217);
#32917=VERTEX_POINT('',#150219);
#32918=VERTEX_POINT('',#150228);
#32919=VERTEX_POINT('',#150229);
#32920=VERTEX_POINT('',#150231);
#32921=VERTEX_POINT('',#150240);
#32922=VERTEX_POINT('',#150256);
#32923=VERTEX_POINT('',#150258);
#32924=VERTEX_POINT('',#150267);
#32925=VERTEX_POINT('',#150268);
#32926=VERTEX_POINT('',#150270);
#32927=VERTEX_POINT('',#150279);
#32928=VERTEX_POINT('',#150295);
#32929=VERTEX_POINT('',#150297);
#32930=VERTEX_POINT('',#150306);
#32931=VERTEX_POINT('',#150307);
#32932=VERTEX_POINT('',#150309);
#32933=VERTEX_POINT('',#150318);
#32934=VERTEX_POINT('',#150334);
#32935=VERTEX_POINT('',#150336);
#32936=VERTEX_POINT('',#150345);
#32937=VERTEX_POINT('',#150346);
#32938=VERTEX_POINT('',#150348);
#32939=VERTEX_POINT('',#150357);
#32940=VERTEX_POINT('',#150373);
#32941=VERTEX_POINT('',#150375);
#32942=VERTEX_POINT('',#150384);
#32943=VERTEX_POINT('',#150385);
#32944=VERTEX_POINT('',#150387);
#32945=VERTEX_POINT('',#150396);
#32946=VERTEX_POINT('',#150412);
#32947=VERTEX_POINT('',#150414);
#32948=VERTEX_POINT('',#150423);
#32949=VERTEX_POINT('',#150424);
#32950=VERTEX_POINT('',#150426);
#32951=VERTEX_POINT('',#150435);
#32952=VERTEX_POINT('',#150451);
#32953=VERTEX_POINT('',#150453);
#32954=VERTEX_POINT('',#150462);
#32955=VERTEX_POINT('',#150463);
#32956=VERTEX_POINT('',#150465);
#32957=VERTEX_POINT('',#150474);
#32958=VERTEX_POINT('',#150490);
#32959=VERTEX_POINT('',#150492);
#32960=VERTEX_POINT('',#150501);
#32961=VERTEX_POINT('',#150502);
#32962=VERTEX_POINT('',#150504);
#32963=VERTEX_POINT('',#150513);
#32964=VERTEX_POINT('',#150529);
#32965=VERTEX_POINT('',#150531);
#32966=VERTEX_POINT('',#150540);
#32967=VERTEX_POINT('',#150541);
#32968=VERTEX_POINT('',#150543);
#32969=VERTEX_POINT('',#150552);
#32970=VERTEX_POINT('',#150568);
#32971=VERTEX_POINT('',#150570);
#32972=VERTEX_POINT('',#150579);
#32973=VERTEX_POINT('',#150580);
#32974=VERTEX_POINT('',#150582);
#32975=VERTEX_POINT('',#150591);
#32976=VERTEX_POINT('',#150607);
#32977=VERTEX_POINT('',#150609);
#32978=VERTEX_POINT('',#150618);
#32979=VERTEX_POINT('',#150619);
#32980=VERTEX_POINT('',#150621);
#32981=VERTEX_POINT('',#150630);
#32982=VERTEX_POINT('',#150646);
#32983=VERTEX_POINT('',#150648);
#32984=VERTEX_POINT('',#150657);
#32985=VERTEX_POINT('',#150658);
#32986=VERTEX_POINT('',#150660);
#32987=VERTEX_POINT('',#150669);
#32988=VERTEX_POINT('',#150685);
#32989=VERTEX_POINT('',#150687);
#32990=VERTEX_POINT('',#150696);
#32991=VERTEX_POINT('',#150697);
#32992=VERTEX_POINT('',#150699);
#32993=VERTEX_POINT('',#150708);
#32994=VERTEX_POINT('',#150724);
#32995=VERTEX_POINT('',#150726);
#32996=VERTEX_POINT('',#150735);
#32997=VERTEX_POINT('',#150736);
#32998=VERTEX_POINT('',#150738);
#32999=VERTEX_POINT('',#150747);
#33000=VERTEX_POINT('',#150787);
#33001=VERTEX_POINT('',#150789);
#33002=VERTEX_POINT('',#150798);
#33003=VERTEX_POINT('',#150799);
#33004=VERTEX_POINT('',#150801);
#33005=VERTEX_POINT('',#150810);
#33006=VERTEX_POINT('',#150826);
#33007=VERTEX_POINT('',#150828);
#33008=VERTEX_POINT('',#150837);
#33009=VERTEX_POINT('',#150838);
#33010=VERTEX_POINT('',#150840);
#33011=VERTEX_POINT('',#150849);
#33012=VERTEX_POINT('',#150865);
#33013=VERTEX_POINT('',#150867);
#33014=VERTEX_POINT('',#150876);
#33015=VERTEX_POINT('',#150877);
#33016=VERTEX_POINT('',#150879);
#33017=VERTEX_POINT('',#150888);
#33018=VERTEX_POINT('',#150904);
#33019=VERTEX_POINT('',#150906);
#33020=VERTEX_POINT('',#150915);
#33021=VERTEX_POINT('',#150916);
#33022=VERTEX_POINT('',#150918);
#33023=VERTEX_POINT('',#150927);
#33024=VERTEX_POINT('',#150943);
#33025=VERTEX_POINT('',#150945);
#33026=VERTEX_POINT('',#150954);
#33027=VERTEX_POINT('',#150955);
#33028=VERTEX_POINT('',#150957);
#33029=VERTEX_POINT('',#150966);
#33030=VERTEX_POINT('',#150982);
#33031=VERTEX_POINT('',#150984);
#33032=VERTEX_POINT('',#150993);
#33033=VERTEX_POINT('',#150994);
#33034=VERTEX_POINT('',#150996);
#33035=VERTEX_POINT('',#151005);
#33036=VERTEX_POINT('',#151021);
#33037=VERTEX_POINT('',#151023);
#33038=VERTEX_POINT('',#151032);
#33039=VERTEX_POINT('',#151033);
#33040=VERTEX_POINT('',#151035);
#33041=VERTEX_POINT('',#151044);
#33042=VERTEX_POINT('',#151060);
#33043=VERTEX_POINT('',#151089);
#33044=VERTEX_POINT('',#151118);
#33045=VERTEX_POINT('',#151147);
#33046=VERTEX_POINT('',#151181);
#33047=VERTEX_POINT('',#151215);
#33048=VERTEX_POINT('',#151244);
#33049=VERTEX_POINT('',#151273);
#33050=VERTEX_POINT('',#151302);
#33051=VERTEX_POINT('',#151331);
#33052=VERTEX_POINT('',#151360);
#33053=VERTEX_POINT('',#151394);
#33054=VERTEX_POINT('',#151423);
#33055=VERTEX_POINT('',#151452);
#33056=VERTEX_POINT('',#151481);
#33057=VERTEX_POINT('',#151515);
#33058=VERTEX_POINT('',#151544);
#33059=VERTEX_POINT('',#151573);
#33060=VERTEX_POINT('',#151602);
#33061=VERTEX_POINT('',#151631);
#33062=VERTEX_POINT('',#151660);
#33063=VERTEX_POINT('',#151689);
#33064=VERTEX_POINT('',#151718);
#33065=VERTEX_POINT('',#151747);
#33066=VERTEX_POINT('',#151781);
#33067=VERTEX_POINT('',#151810);
#33068=VERTEX_POINT('',#151839);
#33069=VERTEX_POINT('',#151868);
#33070=VERTEX_POINT('',#151897);
#33071=VERTEX_POINT('',#151931);
#33072=VERTEX_POINT('',#151951);
#33073=VERTEX_POINT('',#151971);
#33074=VERTEX_POINT('',#151991);
#33075=VERTEX_POINT('',#152011);
#33076=VERTEX_POINT('',#152031);
#33077=VERTEX_POINT('',#152051);
#33078=VERTEX_POINT('',#152071);
#33079=VERTEX_POINT('',#152091);
#33080=VERTEX_POINT('',#152111);
#33081=VERTEX_POINT('',#152131);
#33082=VERTEX_POINT('',#152151);
#33083=VERTEX_POINT('',#152171);
#33084=VERTEX_POINT('',#152191);
#33085=VERTEX_POINT('',#152211);
#33086=VERTEX_POINT('',#152231);
#33087=VERTEX_POINT('',#152251);
#33088=VERTEX_POINT('',#152271);
#33089=VERTEX_POINT('',#152291);
#33090=VERTEX_POINT('',#152311);
#33091=VERTEX_POINT('',#152331);
#33092=VERTEX_POINT('',#152351);
#33093=VERTEX_POINT('',#152371);
#33094=VERTEX_POINT('',#152391);
#33095=VERTEX_POINT('',#152411);
#33096=VERTEX_POINT('',#152431);
#33097=VERTEX_POINT('',#152451);
#33098=VERTEX_POINT('',#152471);
#33099=VERTEX_POINT('',#152491);
#33100=VERTEX_POINT('',#152511);
#33101=VERTEX_POINT('',#152512);
#33102=VERTEX_POINT('',#152535);
#33103=VERTEX_POINT('',#152536);
#33104=VERTEX_POINT('',#152546);
#33105=VERTEX_POINT('',#152548);
#33106=VERTEX_POINT('',#152576);
#33107=VERTEX_POINT('',#152577);
#33108=VERTEX_POINT('',#152587);
#33109=VERTEX_POINT('',#152589);
#33110=VERTEX_POINT('',#152617);
#33111=VERTEX_POINT('',#152618);
#33112=VERTEX_POINT('',#152628);
#33113=VERTEX_POINT('',#152630);
#33114=VERTEX_POINT('',#152658);
#33115=VERTEX_POINT('',#152659);
#33116=VERTEX_POINT('',#152669);
#33117=VERTEX_POINT('',#152671);
#33118=VERTEX_POINT('',#152699);
#33119=VERTEX_POINT('',#152700);
#33120=VERTEX_POINT('',#152710);
#33121=VERTEX_POINT('',#152712);
#33122=VERTEX_POINT('',#152740);
#33123=VERTEX_POINT('',#152741);
#33124=VERTEX_POINT('',#152751);
#33125=VERTEX_POINT('',#152753);
#33126=VERTEX_POINT('',#152813);
#33127=VERTEX_POINT('',#152814);
#33128=VERTEX_POINT('',#152824);
#33129=VERTEX_POINT('',#152826);
#33130=VERTEX_POINT('',#152854);
#33131=VERTEX_POINT('',#152855);
#33132=VERTEX_POINT('',#152865);
#33133=VERTEX_POINT('',#152867);
#33134=VERTEX_POINT('',#152895);
#33135=VERTEX_POINT('',#152896);
#33136=VERTEX_POINT('',#152906);
#33137=VERTEX_POINT('',#152908);
#33138=VERTEX_POINT('',#152936);
#33139=VERTEX_POINT('',#152937);
#33140=VERTEX_POINT('',#152947);
#33141=VERTEX_POINT('',#152949);
#33142=VERTEX_POINT('',#152977);
#33143=VERTEX_POINT('',#152978);
#33144=VERTEX_POINT('',#152988);
#33145=VERTEX_POINT('',#152990);
#33146=VERTEX_POINT('',#153018);
#33147=VERTEX_POINT('',#153019);
#33148=VERTEX_POINT('',#153029);
#33149=VERTEX_POINT('',#153031);
#33150=VERTEX_POINT('',#153059);
#33151=VERTEX_POINT('',#153060);
#33152=VERTEX_POINT('',#153070);
#33153=VERTEX_POINT('',#153072);
#33154=VERTEX_POINT('',#153100);
#33155=VERTEX_POINT('',#153101);
#33156=VERTEX_POINT('',#153111);
#33157=VERTEX_POINT('',#153113);
#33158=VERTEX_POINT('',#153141);
#33159=VERTEX_POINT('',#153142);
#33160=VERTEX_POINT('',#153152);
#33161=VERTEX_POINT('',#153154);
#33162=VERTEX_POINT('',#153182);
#33163=VERTEX_POINT('',#153183);
#33164=VERTEX_POINT('',#153193);
#33165=VERTEX_POINT('',#153195);
#33166=VERTEX_POINT('',#153223);
#33167=VERTEX_POINT('',#153224);
#33168=VERTEX_POINT('',#153243);
#33169=VERTEX_POINT('',#153247);
#33170=VERTEX_POINT('',#153264);
#33171=VERTEX_POINT('',#153266);
#33172=VERTEX_POINT('',#153275);
#33173=VERTEX_POINT('',#153277);
#33174=VERTEX_POINT('',#153305);
#33175=VERTEX_POINT('',#153306);
#33176=VERTEX_POINT('',#153316);
#33177=VERTEX_POINT('',#153318);
#33178=VERTEX_POINT('',#153346);
#33179=VERTEX_POINT('',#153347);
#33180=VERTEX_POINT('',#153357);
#33181=VERTEX_POINT('',#153359);
#33182=VERTEX_POINT('',#153387);
#33183=VERTEX_POINT('',#153388);
#33184=VERTEX_POINT('',#153398);
#33185=VERTEX_POINT('',#153400);
#33186=VERTEX_POINT('',#153428);
#33187=VERTEX_POINT('',#153429);
#33188=VERTEX_POINT('',#153439);
#33189=VERTEX_POINT('',#153441);
#33190=VERTEX_POINT('',#153469);
#33191=VERTEX_POINT('',#153470);
#33192=VERTEX_POINT('',#153480);
#33193=VERTEX_POINT('',#153482);
#33194=VERTEX_POINT('',#153510);
#33195=VERTEX_POINT('',#153511);
#33196=VERTEX_POINT('',#153521);
#33197=VERTEX_POINT('',#153523);
#33198=VERTEX_POINT('',#153551);
#33199=VERTEX_POINT('',#153552);
#33200=VERTEX_POINT('',#153562);
#33201=VERTEX_POINT('',#153564);
#33202=VERTEX_POINT('',#153592);
#33203=VERTEX_POINT('',#153593);
#33204=VERTEX_POINT('',#153603);
#33205=VERTEX_POINT('',#153605);
#33206=VERTEX_POINT('',#153633);
#33207=VERTEX_POINT('',#153634);
#33208=VERTEX_POINT('',#153644);
#33209=VERTEX_POINT('',#153646);
#33210=VERTEX_POINT('',#153661);
#33211=VERTEX_POINT('',#153662);
#33212=VERTEX_POINT('',#153690);
#33213=VERTEX_POINT('',#153697);
#33214=VERTEX_POINT('',#153714);
#33215=VERTEX_POINT('',#153716);
#33216=VERTEX_POINT('',#153730);
#33217=VERTEX_POINT('',#153739);
#33218=VERTEX_POINT('',#153773);
#33219=VERTEX_POINT('',#153775);
#33220=VERTEX_POINT('',#153789);
#33221=VERTEX_POINT('',#153798);
#33222=VERTEX_POINT('',#153832);
#33223=VERTEX_POINT('',#153834);
#33224=VERTEX_POINT('',#153848);
#33225=VERTEX_POINT('',#153857);
#33226=VERTEX_POINT('',#153891);
#33227=VERTEX_POINT('',#153893);
#33228=VERTEX_POINT('',#153907);
#33229=VERTEX_POINT('',#153916);
#33230=VERTEX_POINT('',#153950);
#33231=VERTEX_POINT('',#153952);
#33232=VERTEX_POINT('',#153966);
#33233=VERTEX_POINT('',#153975);
#33234=VERTEX_POINT('',#154009);
#33235=VERTEX_POINT('',#154011);
#33236=VERTEX_POINT('',#154025);
#33237=VERTEX_POINT('',#154034);
#33238=VERTEX_POINT('',#154068);
#33239=VERTEX_POINT('',#154070);
#33240=VERTEX_POINT('',#154084);
#33241=VERTEX_POINT('',#154093);
#33242=VERTEX_POINT('',#154127);
#33243=VERTEX_POINT('',#154129);
#33244=VERTEX_POINT('',#154143);
#33245=VERTEX_POINT('',#154152);
#33246=VERTEX_POINT('',#154186);
#33247=VERTEX_POINT('',#154188);
#33248=VERTEX_POINT('',#154202);
#33249=VERTEX_POINT('',#154211);
#33250=VERTEX_POINT('',#154245);
#33251=VERTEX_POINT('',#154247);
#33252=VERTEX_POINT('',#154261);
#33253=VERTEX_POINT('',#154270);
#33254=VERTEX_POINT('',#154304);
#33255=VERTEX_POINT('',#154306);
#33256=VERTEX_POINT('',#154320);
#33257=VERTEX_POINT('',#154329);
#33258=VERTEX_POINT('',#154363);
#33259=VERTEX_POINT('',#154365);
#33260=VERTEX_POINT('',#154379);
#33261=VERTEX_POINT('',#154388);
#33262=VERTEX_POINT('',#154422);
#33263=VERTEX_POINT('',#154424);
#33264=VERTEX_POINT('',#154438);
#33265=VERTEX_POINT('',#154447);
#33266=VERTEX_POINT('',#154507);
#33267=VERTEX_POINT('',#154509);
#33268=VERTEX_POINT('',#154523);
#33269=VERTEX_POINT('',#154532);
#33270=VERTEX_POINT('',#154566);
#33271=VERTEX_POINT('',#154568);
#33272=VERTEX_POINT('',#154582);
#33273=VERTEX_POINT('',#154591);
#33274=VERTEX_POINT('',#154625);
#33275=VERTEX_POINT('',#154627);
#33276=VERTEX_POINT('',#154641);
#33277=VERTEX_POINT('',#154650);
#33278=VERTEX_POINT('',#154684);
#33279=VERTEX_POINT('',#154686);
#33280=VERTEX_POINT('',#154700);
#33281=VERTEX_POINT('',#154709);
#33282=VERTEX_POINT('',#154743);
#33283=VERTEX_POINT('',#154745);
#33284=VERTEX_POINT('',#154759);
#33285=VERTEX_POINT('',#154768);
#33286=VERTEX_POINT('',#154802);
#33287=VERTEX_POINT('',#154804);
#33288=VERTEX_POINT('',#154818);
#33289=VERTEX_POINT('',#154827);
#33290=VERTEX_POINT('',#154887);
#33291=VERTEX_POINT('',#154889);
#33292=VERTEX_POINT('',#154903);
#33293=VERTEX_POINT('',#154912);
#33294=VERTEX_POINT('',#154946);
#33295=VERTEX_POINT('',#154948);
#33296=VERTEX_POINT('',#154962);
#33297=VERTEX_POINT('',#154971);
#33298=VERTEX_POINT('',#155005);
#33299=VERTEX_POINT('',#155007);
#33300=VERTEX_POINT('',#155021);
#33301=VERTEX_POINT('',#155030);
#33302=VERTEX_POINT('',#155064);
#33303=VERTEX_POINT('',#155066);
#33304=VERTEX_POINT('',#155080);
#33305=VERTEX_POINT('',#155089);
#33306=VERTEX_POINT('',#155123);
#33307=VERTEX_POINT('',#155125);
#33308=VERTEX_POINT('',#155139);
#33309=VERTEX_POINT('',#155148);
#33310=VERTEX_POINT('',#155182);
#33311=VERTEX_POINT('',#155184);
#33312=VERTEX_POINT('',#155198);
#33313=VERTEX_POINT('',#155207);
#33314=VERTEX_POINT('',#155241);
#33315=VERTEX_POINT('',#155243);
#33316=VERTEX_POINT('',#155257);
#33317=VERTEX_POINT('',#155266);
#33318=VERTEX_POINT('',#155292);
#33319=VERTEX_POINT('',#155299);
#33320=VERTEX_POINT('',#155332);
#33321=VERTEX_POINT('',#155346);
#33322=VERTEX_POINT('',#155367);
#33323=VERTEX_POINT('',#155388);
#33324=VERTEX_POINT('',#155409);
#33325=VERTEX_POINT('',#155430);
#33326=VERTEX_POINT('',#155451);
#33327=VERTEX_POINT('',#155472);
#33328=VERTEX_POINT('',#155493);
#33329=VERTEX_POINT('',#155514);
#33330=VERTEX_POINT('',#155535);
#33331=VERTEX_POINT('',#155556);
#33332=VERTEX_POINT('',#155577);
#33333=VERTEX_POINT('',#155598);
#33334=VERTEX_POINT('',#155619);
#33335=VERTEX_POINT('',#155640);
#33336=VERTEX_POINT('',#155661);
#33337=VERTEX_POINT('',#155682);
#33338=VERTEX_POINT('',#155703);
#33339=VERTEX_POINT('',#155724);
#33340=VERTEX_POINT('',#155745);
#33341=VERTEX_POINT('',#155766);
#33342=VERTEX_POINT('',#155787);
#33343=VERTEX_POINT('',#155808);
#33344=VERTEX_POINT('',#155829);
#33345=VERTEX_POINT('',#155850);
#33346=VERTEX_POINT('',#155871);
#33347=VERTEX_POINT('',#155892);
#33348=VERTEX_POINT('',#155913);
#33349=VERTEX_POINT('',#155949);
#33350=VERTEX_POINT('',#155970);
#33351=VERTEX_POINT('',#156013);
#33352=VERTEX_POINT('',#156056);
#33353=VERTEX_POINT('',#156099);
#33354=VERTEX_POINT('',#156142);
#33355=VERTEX_POINT('',#156185);
#33356=VERTEX_POINT('',#156228);
#33357=VERTEX_POINT('',#156271);
#33358=VERTEX_POINT('',#156314);
#33359=VERTEX_POINT('',#156357);
#33360=VERTEX_POINT('',#156400);
#33361=VERTEX_POINT('',#156443);
#33362=VERTEX_POINT('',#156486);
#33363=VERTEX_POINT('',#156529);
#33364=VERTEX_POINT('',#156572);
#33365=VERTEX_POINT('',#156615);
#33366=VERTEX_POINT('',#156658);
#33367=VERTEX_POINT('',#156701);
#33368=VERTEX_POINT('',#156744);
#33369=VERTEX_POINT('',#156787);
#33370=VERTEX_POINT('',#156830);
#33371=VERTEX_POINT('',#156873);
#33372=VERTEX_POINT('',#156916);
#33373=VERTEX_POINT('',#156959);
#33374=VERTEX_POINT('',#157002);
#33375=VERTEX_POINT('',#157045);
#33376=VERTEX_POINT('',#157088);
#33377=VERTEX_POINT('',#157131);
#33378=VERTEX_POINT('',#157176);
#33379=VERTEX_POINT('',#157177);
#33380=VERTEX_POINT('',#157187);
#33381=VERTEX_POINT('',#157189);
#33382=VERTEX_POINT('',#157209);
#33383=VERTEX_POINT('',#157210);
#33384=VERTEX_POINT('',#157220);
#33385=VERTEX_POINT('',#157222);
#33386=VERTEX_POINT('',#157242);
#33387=VERTEX_POINT('',#157243);
#33388=VERTEX_POINT('',#157253);
#33389=VERTEX_POINT('',#157255);
#33390=VERTEX_POINT('',#157275);
#33391=VERTEX_POINT('',#157276);
#33392=VERTEX_POINT('',#157286);
#33393=VERTEX_POINT('',#157288);
#33394=VERTEX_POINT('',#157308);
#33395=VERTEX_POINT('',#157309);
#33396=VERTEX_POINT('',#157319);
#33397=VERTEX_POINT('',#157321);
#33398=VERTEX_POINT('',#157341);
#33399=VERTEX_POINT('',#157342);
#33400=VERTEX_POINT('',#157352);
#33401=VERTEX_POINT('',#157354);
#33402=VERTEX_POINT('',#157374);
#33403=VERTEX_POINT('',#157375);
#33404=VERTEX_POINT('',#157385);
#33405=VERTEX_POINT('',#157387);
#33406=VERTEX_POINT('',#157407);
#33407=VERTEX_POINT('',#157408);
#33408=VERTEX_POINT('',#157418);
#33409=VERTEX_POINT('',#157420);
#33410=VERTEX_POINT('',#157440);
#33411=VERTEX_POINT('',#157441);
#33412=VERTEX_POINT('',#157451);
#33413=VERTEX_POINT('',#157453);
#33414=VERTEX_POINT('',#157473);
#33415=VERTEX_POINT('',#157474);
#33416=VERTEX_POINT('',#157484);
#33417=VERTEX_POINT('',#157486);
#33418=VERTEX_POINT('',#157506);
#33419=VERTEX_POINT('',#157507);
#33420=VERTEX_POINT('',#157517);
#33421=VERTEX_POINT('',#157519);
#33422=VERTEX_POINT('',#157539);
#33423=VERTEX_POINT('',#157540);
#33424=VERTEX_POINT('',#157550);
#33425=VERTEX_POINT('',#157552);
#33426=VERTEX_POINT('',#157572);
#33427=VERTEX_POINT('',#157573);
#33428=VERTEX_POINT('',#157583);
#33429=VERTEX_POINT('',#157585);
#33430=VERTEX_POINT('',#157605);
#33431=VERTEX_POINT('',#157606);
#33432=VERTEX_POINT('',#157616);
#33433=VERTEX_POINT('',#157618);
#33434=VERTEX_POINT('',#157662);
#33435=VERTEX_POINT('',#157663);
#33436=VERTEX_POINT('',#157673);
#33437=VERTEX_POINT('',#157675);
#33438=VERTEX_POINT('',#157695);
#33439=VERTEX_POINT('',#157696);
#33440=VERTEX_POINT('',#157706);
#33441=VERTEX_POINT('',#157708);
#33442=VERTEX_POINT('',#157728);
#33443=VERTEX_POINT('',#157729);
#33444=VERTEX_POINT('',#157748);
#33445=VERTEX_POINT('',#157752);
#33446=VERTEX_POINT('',#157761);
#33447=VERTEX_POINT('',#157763);
#33448=VERTEX_POINT('',#157772);
#33449=VERTEX_POINT('',#157774);
#33450=VERTEX_POINT('',#157794);
#33451=VERTEX_POINT('',#157795);
#33452=VERTEX_POINT('',#157805);
#33453=VERTEX_POINT('',#157807);
#33454=VERTEX_POINT('',#157827);
#33455=VERTEX_POINT('',#157828);
#33456=VERTEX_POINT('',#157838);
#33457=VERTEX_POINT('',#157840);
#33458=VERTEX_POINT('',#157860);
#33459=VERTEX_POINT('',#157861);
#33460=VERTEX_POINT('',#157871);
#33461=VERTEX_POINT('',#157873);
#33462=VERTEX_POINT('',#157893);
#33463=VERTEX_POINT('',#157894);
#33464=VERTEX_POINT('',#157904);
#33465=VERTEX_POINT('',#157906);
#33466=VERTEX_POINT('',#157926);
#33467=VERTEX_POINT('',#157927);
#33468=VERTEX_POINT('',#157937);
#33469=VERTEX_POINT('',#157939);
#33470=VERTEX_POINT('',#157959);
#33471=VERTEX_POINT('',#157960);
#33472=VERTEX_POINT('',#157970);
#33473=VERTEX_POINT('',#157972);
#33474=VERTEX_POINT('',#157992);
#33475=VERTEX_POINT('',#157993);
#33476=VERTEX_POINT('',#158003);
#33477=VERTEX_POINT('',#158005);
#33478=VERTEX_POINT('',#158025);
#33479=VERTEX_POINT('',#158026);
#33480=VERTEX_POINT('',#158036);
#33481=VERTEX_POINT('',#158038);
#33482=VERTEX_POINT('',#158058);
#33483=VERTEX_POINT('',#158059);
#33484=VERTEX_POINT('',#158069);
#33485=VERTEX_POINT('',#158071);
#33486=VERTEX_POINT('',#158091);
#33487=VERTEX_POINT('',#158092);
#33488=VERTEX_POINT('',#158102);
#33489=VERTEX_POINT('',#158104);
#33490=VERTEX_POINT('',#160607);
#33491=VERTEX_POINT('',#160632);
#33492=VERTEX_POINT('',#160657);
#33493=VERTEX_POINT('',#160682);
#33494=VERTEX_POINT('',#160707);
#33495=VERTEX_POINT('',#160732);
#33496=VERTEX_POINT('',#160757);
#33497=VERTEX_POINT('',#160782);
#33498=VERTEX_POINT('',#160807);
#33499=VERTEX_POINT('',#160832);
#33500=VERTEX_POINT('',#160857);
#33501=VERTEX_POINT('',#160882);
#33502=VERTEX_POINT('',#160907);
#33503=VERTEX_POINT('',#160932);
#33504=VERTEX_POINT('',#160957);
#33505=VERTEX_POINT('',#160982);
#33506=VERTEX_POINT('',#161007);
#33507=VERTEX_POINT('',#161032);
#33508=VERTEX_POINT('',#161057);
#33509=VERTEX_POINT('',#161082);
#33510=VERTEX_POINT('',#161107);
#33511=VERTEX_POINT('',#161132);
#33512=VERTEX_POINT('',#161157);
#33513=VERTEX_POINT('',#161182);
#33514=VERTEX_POINT('',#161207);
#33515=VERTEX_POINT('',#161232);
#33516=VERTEX_POINT('',#161257);
#33517=VERTEX_POINT('',#161282);
#33518=VERTEX_POINT('',#161307);
#33519=VERTEX_POINT('',#161336);
#33520=VERTEX_POINT('',#161337);
#33521=VERTEX_POINT('',#161352);
#33522=VERTEX_POINT('',#161353);
#33523=VERTEX_POINT('',#161363);
#33524=VERTEX_POINT('',#161364);
#33525=VERTEX_POINT('',#161366);
#33526=VERTEX_POINT('',#161379);
#33527=VERTEX_POINT('',#161391);
#33528=VERTEX_POINT('',#161392);
#33529=VERTEX_POINT('',#161402);
#33530=VERTEX_POINT('',#161403);
#33531=VERTEX_POINT('',#161405);
#33532=VERTEX_POINT('',#161418);
#33533=VERTEX_POINT('',#161430);
#33534=VERTEX_POINT('',#161431);
#33535=VERTEX_POINT('',#161441);
#33536=VERTEX_POINT('',#161442);
#33537=VERTEX_POINT('',#161444);
#33538=VERTEX_POINT('',#161457);
#33539=VERTEX_POINT('',#161469);
#33540=VERTEX_POINT('',#161470);
#33541=VERTEX_POINT('',#161480);
#33542=VERTEX_POINT('',#161481);
#33543=VERTEX_POINT('',#161483);
#33544=VERTEX_POINT('',#161496);
#33545=VERTEX_POINT('',#161508);
#33546=VERTEX_POINT('',#161509);
#33547=VERTEX_POINT('',#161519);
#33548=VERTEX_POINT('',#161520);
#33549=VERTEX_POINT('',#161522);
#33550=VERTEX_POINT('',#161535);
#33551=VERTEX_POINT('',#161547);
#33552=VERTEX_POINT('',#161548);
#33553=VERTEX_POINT('',#161558);
#33554=VERTEX_POINT('',#161559);
#33555=VERTEX_POINT('',#161561);
#33556=VERTEX_POINT('',#161574);
#33557=VERTEX_POINT('',#161594);
#33558=VERTEX_POINT('',#161614);
#33559=VERTEX_POINT('',#161615);
#33560=VERTEX_POINT('',#161625);
#33561=VERTEX_POINT('',#161626);
#33562=VERTEX_POINT('',#161628);
#33563=VERTEX_POINT('',#161641);
#33564=VERTEX_POINT('',#161653);
#33565=VERTEX_POINT('',#161654);
#33566=VERTEX_POINT('',#161664);
#33567=VERTEX_POINT('',#161665);
#33568=VERTEX_POINT('',#161667);
#33569=VERTEX_POINT('',#161680);
#33570=VERTEX_POINT('',#161692);
#33571=VERTEX_POINT('',#161693);
#33572=VERTEX_POINT('',#161703);
#33573=VERTEX_POINT('',#161704);
#33574=VERTEX_POINT('',#161706);
#33575=VERTEX_POINT('',#161719);
#33576=VERTEX_POINT('',#161731);
#33577=VERTEX_POINT('',#161732);
#33578=VERTEX_POINT('',#161742);
#33579=VERTEX_POINT('',#161743);
#33580=VERTEX_POINT('',#161745);
#33581=VERTEX_POINT('',#161758);
#33582=VERTEX_POINT('',#161770);
#33583=VERTEX_POINT('',#161771);
#33584=VERTEX_POINT('',#161781);
#33585=VERTEX_POINT('',#161782);
#33586=VERTEX_POINT('',#161784);
#33587=VERTEX_POINT('',#161797);
#33588=VERTEX_POINT('',#161809);
#33589=VERTEX_POINT('',#161810);
#33590=VERTEX_POINT('',#161820);
#33591=VERTEX_POINT('',#161821);
#33592=VERTEX_POINT('',#161823);
#33593=VERTEX_POINT('',#161836);
#33594=VERTEX_POINT('',#161848);
#33595=VERTEX_POINT('',#161849);
#33596=VERTEX_POINT('',#161859);
#33597=VERTEX_POINT('',#161860);
#33598=VERTEX_POINT('',#161862);
#33599=VERTEX_POINT('',#161875);
#33600=VERTEX_POINT('',#161887);
#33601=VERTEX_POINT('',#161888);
#33602=VERTEX_POINT('',#161898);
#33603=VERTEX_POINT('',#161899);
#33604=VERTEX_POINT('',#161901);
#33605=VERTEX_POINT('',#161914);
#33606=VERTEX_POINT('',#161926);
#33607=VERTEX_POINT('',#161927);
#33608=VERTEX_POINT('',#161937);
#33609=VERTEX_POINT('',#161938);
#33610=VERTEX_POINT('',#161940);
#33611=VERTEX_POINT('',#161953);
#33612=VERTEX_POINT('',#161965);
#33613=VERTEX_POINT('',#161966);
#33614=VERTEX_POINT('',#161976);
#33615=VERTEX_POINT('',#161977);
#33616=VERTEX_POINT('',#161979);
#33617=VERTEX_POINT('',#161992);
#33618=VERTEX_POINT('',#162004);
#33619=VERTEX_POINT('',#162006);
#33620=VERTEX_POINT('',#162015);
#33621=VERTEX_POINT('',#162016);
#33622=VERTEX_POINT('',#162018);
#33623=VERTEX_POINT('',#162031);
#33624=VERTEX_POINT('',#162043);
#33625=VERTEX_POINT('',#162044);
#33626=VERTEX_POINT('',#162054);
#33627=VERTEX_POINT('',#162055);
#33628=VERTEX_POINT('',#162057);
#33629=VERTEX_POINT('',#162070);
#33630=VERTEX_POINT('',#162082);
#33631=VERTEX_POINT('',#162083);
#33632=VERTEX_POINT('',#162093);
#33633=VERTEX_POINT('',#162094);
#33634=VERTEX_POINT('',#162096);
#33635=VERTEX_POINT('',#162109);
#33636=VERTEX_POINT('',#162121);
#33637=VERTEX_POINT('',#162122);
#33638=VERTEX_POINT('',#162132);
#33639=VERTEX_POINT('',#162133);
#33640=VERTEX_POINT('',#162135);
#33641=VERTEX_POINT('',#162148);
#33642=VERTEX_POINT('',#162160);
#33643=VERTEX_POINT('',#162161);
#33644=VERTEX_POINT('',#162171);
#33645=VERTEX_POINT('',#162172);
#33646=VERTEX_POINT('',#162174);
#33647=VERTEX_POINT('',#162187);
#33648=VERTEX_POINT('',#162199);
#33649=VERTEX_POINT('',#162200);
#33650=VERTEX_POINT('',#162210);
#33651=VERTEX_POINT('',#162211);
#33652=VERTEX_POINT('',#162213);
#33653=VERTEX_POINT('',#162226);
#33654=VERTEX_POINT('',#162238);
#33655=VERTEX_POINT('',#162239);
#33656=VERTEX_POINT('',#162249);
#33657=VERTEX_POINT('',#162250);
#33658=VERTEX_POINT('',#162252);
#33659=VERTEX_POINT('',#162265);
#33660=VERTEX_POINT('',#162277);
#33661=VERTEX_POINT('',#162278);
#33662=VERTEX_POINT('',#162288);
#33663=VERTEX_POINT('',#162289);
#33664=VERTEX_POINT('',#162291);
#33665=VERTEX_POINT('',#162304);
#33666=VERTEX_POINT('',#162316);
#33667=VERTEX_POINT('',#162317);
#33668=VERTEX_POINT('',#162327);
#33669=VERTEX_POINT('',#162328);
#33670=VERTEX_POINT('',#162330);
#33671=VERTEX_POINT('',#162343);
#33672=VERTEX_POINT('',#162355);
#33673=VERTEX_POINT('',#162356);
#33674=VERTEX_POINT('',#162366);
#33675=VERTEX_POINT('',#162367);
#33676=VERTEX_POINT('',#162369);
#33677=VERTEX_POINT('',#162382);
#33678=VERTEX_POINT('',#162394);
#33679=VERTEX_POINT('',#162395);
#33680=VERTEX_POINT('',#162405);
#33681=VERTEX_POINT('',#162406);
#33682=VERTEX_POINT('',#162408);
#33683=VERTEX_POINT('',#162421);
#33684=VERTEX_POINT('',#162428);
#33685=VERTEX_POINT('',#162429);
#33686=VERTEX_POINT('',#162431);
#33687=VERTEX_POINT('',#162436);
#33688=VERTEX_POINT('',#162457);
#33689=VERTEX_POINT('',#162466);
#33690=VERTEX_POINT('',#162486);
#33691=VERTEX_POINT('',#162506);
#33692=VERTEX_POINT('',#162526);
#33693=VERTEX_POINT('',#162546);
#33694=VERTEX_POINT('',#162566);
#33695=VERTEX_POINT('',#162586);
#33696=VERTEX_POINT('',#162606);
#33697=VERTEX_POINT('',#162626);
#33698=VERTEX_POINT('',#162646);
#33699=VERTEX_POINT('',#162666);
#33700=VERTEX_POINT('',#162686);
#33701=VERTEX_POINT('',#162706);
#33702=VERTEX_POINT('',#162726);
#33703=VERTEX_POINT('',#162746);
#33704=VERTEX_POINT('',#162766);
#33705=VERTEX_POINT('',#162786);
#33706=VERTEX_POINT('',#162806);
#33707=VERTEX_POINT('',#162826);
#33708=VERTEX_POINT('',#162846);
#33709=VERTEX_POINT('',#162866);
#33710=VERTEX_POINT('',#162886);
#33711=VERTEX_POINT('',#162906);
#33712=VERTEX_POINT('',#162926);
#33713=VERTEX_POINT('',#162946);
#33714=VERTEX_POINT('',#162966);
#33715=VERTEX_POINT('',#162986);
#33716=VERTEX_POINT('',#163006);
#33717=VERTEX_POINT('',#163036);
#33718=VERTEX_POINT('',#163038);
#33719=VERTEX_POINT('',#163052);
#33720=VERTEX_POINT('',#163053);
#33721=VERTEX_POINT('',#163095);
#33722=VERTEX_POINT('',#163097);
#33723=VERTEX_POINT('',#163111);
#33724=VERTEX_POINT('',#163112);
#33725=VERTEX_POINT('',#163154);
#33726=VERTEX_POINT('',#163156);
#33727=VERTEX_POINT('',#163170);
#33728=VERTEX_POINT('',#163171);
#33729=VERTEX_POINT('',#163213);
#33730=VERTEX_POINT('',#163215);
#33731=VERTEX_POINT('',#163229);
#33732=VERTEX_POINT('',#163230);
#33733=VERTEX_POINT('',#163272);
#33734=VERTEX_POINT('',#163274);
#33735=VERTEX_POINT('',#163288);
#33736=VERTEX_POINT('',#163289);
#33737=VERTEX_POINT('',#163331);
#33738=VERTEX_POINT('',#163333);
#33739=VERTEX_POINT('',#163347);
#33740=VERTEX_POINT('',#163348);
#33741=VERTEX_POINT('',#163390);
#33742=VERTEX_POINT('',#163392);
#33743=VERTEX_POINT('',#163406);
#33744=VERTEX_POINT('',#163407);
#33745=VERTEX_POINT('',#163449);
#33746=VERTEX_POINT('',#163451);
#33747=VERTEX_POINT('',#163465);
#33748=VERTEX_POINT('',#163466);
#33749=VERTEX_POINT('',#163508);
#33750=VERTEX_POINT('',#163510);
#33751=VERTEX_POINT('',#163524);
#33752=VERTEX_POINT('',#163525);
#33753=VERTEX_POINT('',#163567);
#33754=VERTEX_POINT('',#163569);
#33755=VERTEX_POINT('',#163583);
#33756=VERTEX_POINT('',#163584);
#33757=VERTEX_POINT('',#163626);
#33758=VERTEX_POINT('',#163628);
#33759=VERTEX_POINT('',#163642);
#33760=VERTEX_POINT('',#163643);
#33761=VERTEX_POINT('',#163685);
#33762=VERTEX_POINT('',#163687);
#33763=VERTEX_POINT('',#163701);
#33764=VERTEX_POINT('',#163702);
#33765=VERTEX_POINT('',#163744);
#33766=VERTEX_POINT('',#163746);
#33767=VERTEX_POINT('',#163760);
#33768=VERTEX_POINT('',#163761);
#33769=VERTEX_POINT('',#163803);
#33770=VERTEX_POINT('',#163805);
#33771=VERTEX_POINT('',#163819);
#33772=VERTEX_POINT('',#163820);
#33773=VERTEX_POINT('',#163862);
#33774=VERTEX_POINT('',#163864);
#33775=VERTEX_POINT('',#163878);
#33776=VERTEX_POINT('',#163879);
#33777=VERTEX_POINT('',#163921);
#33778=VERTEX_POINT('',#163923);
#33779=VERTEX_POINT('',#163937);
#33780=VERTEX_POINT('',#163938);
#33781=VERTEX_POINT('',#163980);
#33782=VERTEX_POINT('',#163982);
#33783=VERTEX_POINT('',#163996);
#33784=VERTEX_POINT('',#163997);
#33785=VERTEX_POINT('',#164039);
#33786=VERTEX_POINT('',#164041);
#33787=VERTEX_POINT('',#164055);
#33788=VERTEX_POINT('',#164064);
#33789=VERTEX_POINT('',#164098);
#33790=VERTEX_POINT('',#164100);
#33791=VERTEX_POINT('',#164114);
#33792=VERTEX_POINT('',#164115);
#33793=VERTEX_POINT('',#164157);
#33794=VERTEX_POINT('',#164159);
#33795=VERTEX_POINT('',#164173);
#33796=VERTEX_POINT('',#164174);
#33797=VERTEX_POINT('',#164216);
#33798=VERTEX_POINT('',#164218);
#33799=VERTEX_POINT('',#164232);
#33800=VERTEX_POINT('',#164233);
#33801=VERTEX_POINT('',#164301);
#33802=VERTEX_POINT('',#164303);
#33803=VERTEX_POINT('',#164317);
#33804=VERTEX_POINT('',#164318);
#33805=VERTEX_POINT('',#164360);
#33806=VERTEX_POINT('',#164362);
#33807=VERTEX_POINT('',#164376);
#33808=VERTEX_POINT('',#164377);
#33809=VERTEX_POINT('',#164419);
#33810=VERTEX_POINT('',#164421);
#33811=VERTEX_POINT('',#164435);
#33812=VERTEX_POINT('',#164436);
#33813=VERTEX_POINT('',#164478);
#33814=VERTEX_POINT('',#164480);
#33815=VERTEX_POINT('',#164494);
#33816=VERTEX_POINT('',#164495);
#33817=VERTEX_POINT('',#164537);
#33818=VERTEX_POINT('',#164539);
#33819=VERTEX_POINT('',#164553);
#33820=VERTEX_POINT('',#164554);
#33821=VERTEX_POINT('',#164596);
#33822=VERTEX_POINT('',#164598);
#33823=VERTEX_POINT('',#164612);
#33824=VERTEX_POINT('',#164613);
#33825=VERTEX_POINT('',#164686);
#33826=VERTEX_POINT('',#164721);
#33827=VERTEX_POINT('',#164752);
#33828=VERTEX_POINT('',#164780);
#33829=VERTEX_POINT('',#164808);
#33830=VERTEX_POINT('',#164836);
#33831=VERTEX_POINT('',#164864);
#33832=VERTEX_POINT('',#164899);
#33833=VERTEX_POINT('',#164930);
#33834=VERTEX_POINT('',#164958);
#33835=VERTEX_POINT('',#164986);
#33836=VERTEX_POINT('',#165014);
#33837=VERTEX_POINT('',#165049);
#33838=VERTEX_POINT('',#165080);
#33839=VERTEX_POINT('',#165108);
#33840=VERTEX_POINT('',#165143);
#33841=VERTEX_POINT('',#165174);
#33842=VERTEX_POINT('',#165209);
#33843=VERTEX_POINT('',#165240);
#33844=VERTEX_POINT('',#165268);
#33845=VERTEX_POINT('',#165303);
#33846=VERTEX_POINT('',#165341);
#33847=VERTEX_POINT('',#165372);
#33848=VERTEX_POINT('',#165400);
#33849=VERTEX_POINT('',#165428);
#33850=VERTEX_POINT('',#165456);
#33851=VERTEX_POINT('',#165484);
#33852=VERTEX_POINT('',#165512);
#33853=VERTEX_POINT('',#165540);
#33854=VERTEX_POINT('',#168047);
#33855=VERTEX_POINT('',#168049);
#33856=VERTEX_POINT('',#168053);
#33857=VERTEX_POINT('',#168054);
#33858=VERTEX_POINT('',#168056);
#33859=VERTEX_POINT('',#168058);
#33860=VERTEX_POINT('',#168063);
#33861=VERTEX_POINT('',#168065);
#33862=VERTEX_POINT('',#168070);
#33863=VERTEX_POINT('',#168072);
#33864=VERTEX_POINT('',#168074);
#33865=VERTEX_POINT('',#168077);
#33866=VERTEX_POINT('',#168079);
#33867=VERTEX_POINT('',#168081);
#33868=VERTEX_POINT('',#168086);
#33869=VERTEX_POINT('',#168088);
#33870=VERTEX_POINT('',#168095);
#33871=VERTEX_POINT('',#168096);
#33872=VERTEX_POINT('',#168099);
#33873=VERTEX_POINT('',#168103);
#33874=VERTEX_POINT('',#168104);
#33875=VERTEX_POINT('',#168119);
#33876=VERTEX_POINT('',#168128);
#33877=VERTEX_POINT('',#168137);
#33878=VERTEX_POINT('',#168141);
#33879=VERTEX_POINT('',#168143);
#33880=VERTEX_POINT('',#168152);
#33881=VERTEX_POINT('',#168154);
#33882=VERTEX_POINT('',#168178);
#33883=VERTEX_POINT('',#168196);
#33884=VERTEX_POINT('',#168197);
#33885=VERTEX_POINT('',#168199);
#33886=VERTEX_POINT('',#168290);
#33887=VERTEX_POINT('',#168291);
#33888=VERTEX_POINT('',#168335);
#33889=VERTEX_POINT('',#168385);
#33890=VERTEX_POINT('',#168386);
#33891=VERTEX_POINT('',#168388);
#33892=VERTEX_POINT('',#168393);
#33893=VERTEX_POINT('',#168395);
#33894=VERTEX_POINT('',#168399);
#33895=VERTEX_POINT('',#168403);
#33896=VERTEX_POINT('',#168404);
#33897=VERTEX_POINT('',#168415);
#33898=VERTEX_POINT('',#168417);
#33899=VERTEX_POINT('',#168430);
#33900=VERTEX_POINT('',#168434);
#33901=VERTEX_POINT('',#168435);
#33902=VERTEX_POINT('',#168437);
#33903=VERTEX_POINT('',#168444);
#33904=VERTEX_POINT('',#168446);
#33905=VERTEX_POINT('',#168448);
#33906=VERTEX_POINT('',#168450);
#33907=VERTEX_POINT('',#168457);
#33908=VERTEX_POINT('',#168519);
#33909=VERTEX_POINT('',#168530);
#33910=VERTEX_POINT('',#168532);
#33911=VERTEX_POINT('',#168642);
#33912=VERTEX_POINT('',#168655);
#33913=VERTEX_POINT('',#168668);
#33914=VERTEX_POINT('',#168830);
#33915=VERTEX_POINT('',#168831);
#33916=VERTEX_POINT('',#168922);
#33917=VERTEX_POINT('',#168923);
#33918=VERTEX_POINT('',#169032);
#33919=VERTEX_POINT('',#169033);
#33920=VERTEX_POINT('',#169038);
#33921=VERTEX_POINT('',#169045);
#33922=VERTEX_POINT('',#169492);
#33923=VERTEX_POINT('',#169505);
#33924=VERTEX_POINT('',#169684);
#33925=VERTEX_POINT('',#169689);
#33926=VERTEX_POINT('',#169872);
#33927=VERTEX_POINT('',#169873);
#33928=VERTEX_POINT('',#169878);
#33929=VERTEX_POINT('',#169951);
#33930=VERTEX_POINT('',#169968);
#33931=VERTEX_POINT('',#169970);
#33932=VERTEX_POINT('',#169972);
#33933=VERTEX_POINT('',#169991);
#33934=VERTEX_POINT('',#169994);
#33935=VERTEX_POINT('',#170020);
#33936=VERTEX_POINT('',#170021);
#33937=VERTEX_POINT('',#170062);
#33938=VERTEX_POINT('',#170063);
#33939=VERTEX_POINT('',#170065);
#33940=VERTEX_POINT('',#170067);
#33941=VERTEX_POINT('',#170069);
#33942=VERTEX_POINT('',#170072);
#33943=VERTEX_POINT('',#170075);
#33944=VERTEX_POINT('',#170076);
#33945=VERTEX_POINT('',#170080);
#33946=VERTEX_POINT('',#170082);
#33947=VERTEX_POINT('',#170085);
#33948=VERTEX_POINT('',#170087);
#33949=VERTEX_POINT('',#170091);
#33950=VERTEX_POINT('',#170093);
#33951=VERTEX_POINT('',#170097);
#33952=VERTEX_POINT('',#170113);
#33953=VERTEX_POINT('',#170114);
#33954=VERTEX_POINT('',#170117);
#33955=VERTEX_POINT('',#170119);
#33956=VERTEX_POINT('',#170124);
#33957=VERTEX_POINT('',#170145);
#33958=VERTEX_POINT('',#170167);
#33959=VERTEX_POINT('',#170168);
#33960=VERTEX_POINT('',#170209);
#33961=VERTEX_POINT('',#170213);
#33962=VERTEX_POINT('',#170222);
#33963=VERTEX_POINT('',#170224);
#33964=EDGE_CURVE('',#28533,#28534,#24357,.T.);
#33965=EDGE_CURVE('',#28535,#28533,#21046,.F.);
#33966=EDGE_CURVE('',#28536,#28535,#21047,.T.);
#33967=EDGE_CURVE('',#28537,#28536,#15929,.T.);
#33968=EDGE_CURVE('',#28538,#28537,#15930,.T.);
#33969=EDGE_CURVE('',#28539,#28538,#21048,.T.);
#33970=EDGE_CURVE('',#28540,#28539,#21049,.T.);
#33971=EDGE_CURVE('',#28541,#28540,#21050,.T.);
#33972=EDGE_CURVE('',#28542,#28541,#21051,.T.);
#33973=EDGE_CURVE('',#28543,#28542,#15931,.T.);
#33974=EDGE_CURVE('',#28544,#28543,#15932,.T.);
#33975=EDGE_CURVE('',#28545,#28544,#21052,.T.);
#33976=EDGE_CURVE('',#28546,#28545,#21053,.T.);
#33977=EDGE_CURVE('',#28547,#28546,#21054,.T.);
#33978=EDGE_CURVE('',#28548,#28547,#21055,.T.);
#33979=EDGE_CURVE('',#28549,#28548,#15933,.T.);
#33980=EDGE_CURVE('',#28550,#28549,#15934,.T.);
#33981=EDGE_CURVE('',#28551,#28550,#21056,.T.);
#33982=EDGE_CURVE('',#28552,#28551,#21057,.T.);
#33983=EDGE_CURVE('',#28553,#28552,#21058,.T.);
#33984=EDGE_CURVE('',#28554,#28553,#21059,.T.);
#33985=EDGE_CURVE('',#28555,#28554,#15935,.T.);
#33986=EDGE_CURVE('',#28556,#28555,#15936,.T.);
#33987=EDGE_CURVE('',#28557,#28556,#21060,.T.);
#33988=EDGE_CURVE('',#28558,#28557,#21061,.T.);
#33989=EDGE_CURVE('',#28559,#28558,#21062,.T.);
#33990=EDGE_CURVE('',#28560,#28559,#21063,.T.);
#33991=EDGE_CURVE('',#28561,#28560,#15937,.T.);
#33992=EDGE_CURVE('',#28562,#28561,#15938,.T.);
#33993=EDGE_CURVE('',#28563,#28562,#21064,.T.);
#33994=EDGE_CURVE('',#28564,#28563,#21065,.T.);
#33995=EDGE_CURVE('',#28565,#28564,#21066,.T.);
#33996=EDGE_CURVE('',#28566,#28565,#21067,.T.);
#33997=EDGE_CURVE('',#28567,#28566,#15939,.T.);
#33998=EDGE_CURVE('',#28568,#28567,#15940,.T.);
#33999=EDGE_CURVE('',#28569,#28568,#21068,.T.);
#34000=EDGE_CURVE('',#28570,#28569,#21069,.T.);
#34001=EDGE_CURVE('',#28571,#28570,#21070,.T.);
#34002=EDGE_CURVE('',#28572,#28571,#21071,.T.);
#34003=EDGE_CURVE('',#28573,#28572,#15941,.T.);
#34004=EDGE_CURVE('',#28574,#28573,#15942,.T.);
#34005=EDGE_CURVE('',#28575,#28574,#21072,.T.);
#34006=EDGE_CURVE('',#28576,#28575,#21073,.T.);
#34007=EDGE_CURVE('',#28577,#28576,#21074,.T.);
#34008=EDGE_CURVE('',#28578,#28577,#21075,.T.);
#34009=EDGE_CURVE('',#28579,#28578,#15943,.T.);
#34010=EDGE_CURVE('',#28580,#28579,#15944,.T.);
#34011=EDGE_CURVE('',#28581,#28580,#21076,.T.);
#34012=EDGE_CURVE('',#28582,#28581,#21077,.T.);
#34013=EDGE_CURVE('',#28583,#28582,#21078,.T.);
#34014=EDGE_CURVE('',#28584,#28583,#21079,.T.);
#34015=EDGE_CURVE('',#28585,#28584,#15945,.T.);
#34016=EDGE_CURVE('',#28586,#28585,#15946,.T.);
#34017=EDGE_CURVE('',#28587,#28586,#21080,.T.);
#34018=EDGE_CURVE('',#28588,#28587,#21081,.T.);
#34019=EDGE_CURVE('',#28589,#28588,#21082,.T.);
#34020=EDGE_CURVE('',#28590,#28589,#21083,.T.);
#34021=EDGE_CURVE('',#28591,#28590,#15947,.T.);
#34022=EDGE_CURVE('',#28592,#28591,#15948,.T.);
#34023=EDGE_CURVE('',#28593,#28592,#21084,.T.);
#34024=EDGE_CURVE('',#28594,#28593,#21085,.T.);
#34025=EDGE_CURVE('',#28595,#28594,#21086,.T.);
#34026=EDGE_CURVE('',#28596,#28595,#21087,.T.);
#34027=EDGE_CURVE('',#28597,#28596,#15949,.T.);
#34028=EDGE_CURVE('',#28598,#28597,#15950,.T.);
#34029=EDGE_CURVE('',#28599,#28598,#21088,.T.);
#34030=EDGE_CURVE('',#28600,#28599,#21089,.T.);
#34031=EDGE_CURVE('',#28601,#28600,#21090,.T.);
#34032=EDGE_CURVE('',#28602,#28601,#21091,.T.);
#34033=EDGE_CURVE('',#28603,#28602,#15951,.T.);
#34034=EDGE_CURVE('',#28604,#28603,#15952,.T.);
#34035=EDGE_CURVE('',#28605,#28604,#21092,.T.);
#34036=EDGE_CURVE('',#28606,#28605,#21093,.T.);
#34037=EDGE_CURVE('',#28607,#28606,#21094,.T.);
#34038=EDGE_CURVE('',#28608,#28607,#21095,.T.);
#34039=EDGE_CURVE('',#28609,#28608,#15953,.T.);
#34040=EDGE_CURVE('',#28610,#28609,#15954,.T.);
#34041=EDGE_CURVE('',#28611,#28610,#21096,.T.);
#34042=EDGE_CURVE('',#28612,#28611,#21097,.T.);
#34043=EDGE_CURVE('',#28613,#28612,#21098,.T.);
#34044=EDGE_CURVE('',#28614,#28613,#21099,.T.);
#34045=EDGE_CURVE('',#28615,#28614,#15955,.T.);
#34046=EDGE_CURVE('',#28616,#28615,#15956,.T.);
#34047=EDGE_CURVE('',#28617,#28616,#21100,.T.);
#34048=EDGE_CURVE('',#28618,#28617,#21101,.T.);
#34049=EDGE_CURVE('',#28619,#28618,#21102,.T.);
#34050=EDGE_CURVE('',#28620,#28619,#21103,.T.);
#34051=EDGE_CURVE('',#28621,#28620,#15957,.T.);
#34052=EDGE_CURVE('',#28622,#28621,#15958,.T.);
#34053=EDGE_CURVE('',#28623,#28622,#21104,.T.);
#34054=EDGE_CURVE('',#28624,#28623,#21105,.T.);
#34055=EDGE_CURVE('',#28625,#28624,#21106,.T.);
#34056=EDGE_CURVE('',#28626,#28625,#21107,.T.);
#34057=EDGE_CURVE('',#28627,#28626,#15959,.T.);
#34058=EDGE_CURVE('',#28628,#28627,#15960,.T.);
#34059=EDGE_CURVE('',#28629,#28628,#21108,.T.);
#34060=EDGE_CURVE('',#28630,#28629,#21109,.T.);
#34061=EDGE_CURVE('',#28631,#28630,#21110,.T.);
#34062=EDGE_CURVE('',#28632,#28631,#21111,.T.);
#34063=EDGE_CURVE('',#28633,#28632,#15961,.T.);
#34064=EDGE_CURVE('',#28634,#28633,#15962,.T.);
#34065=EDGE_CURVE('',#28635,#28634,#21112,.T.);
#34066=EDGE_CURVE('',#28636,#28635,#21113,.T.);
#34067=EDGE_CURVE('',#28637,#28636,#21114,.T.);
#34068=EDGE_CURVE('',#28638,#28637,#21115,.T.);
#34069=EDGE_CURVE('',#28639,#28638,#15963,.T.);
#34070=EDGE_CURVE('',#28640,#28639,#15964,.T.);
#34071=EDGE_CURVE('',#28641,#28640,#21116,.T.);
#34072=EDGE_CURVE('',#28642,#28641,#21117,.T.);
#34073=EDGE_CURVE('',#28643,#28642,#21118,.T.);
#34074=EDGE_CURVE('',#28644,#28643,#21119,.T.);
#34075=EDGE_CURVE('',#28645,#28644,#15965,.T.);
#34076=EDGE_CURVE('',#28646,#28645,#15966,.T.);
#34077=EDGE_CURVE('',#28647,#28646,#21120,.T.);
#34078=EDGE_CURVE('',#28648,#28647,#21121,.T.);
#34079=EDGE_CURVE('',#28649,#28648,#21122,.T.);
#34080=EDGE_CURVE('',#28650,#28649,#21123,.T.);
#34081=EDGE_CURVE('',#28651,#28650,#15967,.T.);
#34082=EDGE_CURVE('',#28652,#28651,#15968,.T.);
#34083=EDGE_CURVE('',#28653,#28652,#21124,.T.);
#34084=EDGE_CURVE('',#28654,#28653,#21125,.T.);
#34085=EDGE_CURVE('',#28655,#28654,#21126,.T.);
#34086=EDGE_CURVE('',#28656,#28655,#21127,.T.);
#34087=EDGE_CURVE('',#28657,#28656,#15969,.T.);
#34088=EDGE_CURVE('',#28658,#28657,#15970,.T.);
#34089=EDGE_CURVE('',#28659,#28658,#21128,.T.);
#34090=EDGE_CURVE('',#28660,#28659,#21129,.T.);
#34091=EDGE_CURVE('',#28661,#28660,#21130,.T.);
#34092=EDGE_CURVE('',#28662,#28661,#21131,.T.);
#34093=EDGE_CURVE('',#28663,#28662,#15971,.T.);
#34094=EDGE_CURVE('',#28664,#28663,#15972,.T.);
#34095=EDGE_CURVE('',#28665,#28664,#21132,.T.);
#34096=EDGE_CURVE('',#28666,#28665,#21133,.T.);
#34097=EDGE_CURVE('',#28667,#28666,#21134,.T.);
#34098=EDGE_CURVE('',#28668,#28667,#21135,.T.);
#34099=EDGE_CURVE('',#28669,#28668,#15973,.T.);
#34100=EDGE_CURVE('',#28670,#28669,#15974,.T.);
#34101=EDGE_CURVE('',#28671,#28670,#21136,.T.);
#34102=EDGE_CURVE('',#28672,#28671,#21137,.T.);
#34103=EDGE_CURVE('',#28673,#28672,#21138,.T.);
#34104=EDGE_CURVE('',#28674,#28673,#21139,.T.);
#34105=EDGE_CURVE('',#28675,#28674,#15975,.T.);
#34106=EDGE_CURVE('',#28676,#28675,#15976,.T.);
#34107=EDGE_CURVE('',#28677,#28676,#21140,.T.);
#34108=EDGE_CURVE('',#28678,#28677,#21141,.T.);
#34109=EDGE_CURVE('',#28679,#28678,#21142,.T.);
#34110=EDGE_CURVE('',#28680,#28679,#21143,.T.);
#34111=EDGE_CURVE('',#28681,#28680,#15977,.T.);
#34112=EDGE_CURVE('',#28682,#28681,#15978,.T.);
#34113=EDGE_CURVE('',#28683,#28682,#21144,.T.);
#34114=EDGE_CURVE('',#28684,#28683,#21145,.T.);
#34115=EDGE_CURVE('',#28685,#28684,#21146,.T.);
#34116=EDGE_CURVE('',#28686,#28685,#21147,.T.);
#34117=EDGE_CURVE('',#28687,#28686,#15979,.T.);
#34118=EDGE_CURVE('',#28688,#28687,#15980,.T.);
#34119=EDGE_CURVE('',#28689,#28688,#21148,.T.);
#34120=EDGE_CURVE('',#28690,#28689,#21149,.T.);
#34121=EDGE_CURVE('',#28691,#28690,#21150,.T.);
#34122=EDGE_CURVE('',#28692,#28691,#21151,.T.);
#34123=EDGE_CURVE('',#28693,#28692,#15981,.T.);
#34124=EDGE_CURVE('',#28694,#28693,#15982,.T.);
#34125=EDGE_CURVE('',#28695,#28694,#21152,.T.);
#34126=EDGE_CURVE('',#28696,#28695,#21153,.T.);
#34127=EDGE_CURVE('',#28697,#28696,#21154,.T.);
#34128=EDGE_CURVE('',#28698,#28697,#21155,.T.);
#34129=EDGE_CURVE('',#28699,#28698,#15983,.T.);
#34130=EDGE_CURVE('',#28700,#28699,#15984,.T.);
#34131=EDGE_CURVE('',#28701,#28700,#21156,.T.);
#34132=EDGE_CURVE('',#28702,#28701,#21157,.T.);
#34133=EDGE_CURVE('',#28703,#28702,#21158,.T.);
#34134=EDGE_CURVE('',#28704,#28703,#21159,.T.);
#34135=EDGE_CURVE('',#28705,#28704,#15985,.T.);
#34136=EDGE_CURVE('',#28706,#28705,#15986,.T.);
#34137=EDGE_CURVE('',#28707,#28706,#21160,.F.);
#34138=EDGE_CURVE('',#28707,#28708,#24358,.T.);
#34139=EDGE_CURVE('',#28708,#28708,#15987,.T.);
#34140=EDGE_CURVE('',#28709,#28707,#21161,.F.);
#34141=EDGE_CURVE('',#28534,#28709,#21162,.F.);
#34142=EDGE_CURVE('',#28710,#28710,#15988,.T.);
#34143=EDGE_CURVE('',#28710,#28711,#24359,.T.);
#34144=EDGE_CURVE('',#28711,#28711,#15989,.T.);
#34145=EDGE_CURVE('',#28712,#28534,#21163,.F.);
#34146=EDGE_CURVE('',#28533,#28712,#21164,.F.);
#34147=EDGE_CURVE('',#28713,#28713,#15990,.T.);
#34148=EDGE_CURVE('',#28713,#28714,#24360,.T.);
#34149=EDGE_CURVE('',#28714,#28714,#15991,.T.);
#34150=EDGE_CURVE('',#28715,#28716,#15992,.T.);
#34151=EDGE_CURVE('',#28716,#28717,#24361,.T.);
#34152=EDGE_CURVE('',#28717,#28717,#15993,.T.);
#34153=EDGE_CURVE('',#28716,#28715,#15994,.T.);
#34154=EDGE_CURVE('',#28715,#28718,#24362,.T.);
#34155=EDGE_CURVE('',#28718,#28718,#15995,.T.);
#34156=EDGE_CURVE('',#28719,#28720,#21165,.T.);
#34157=EDGE_CURVE('',#28721,#28719,#15996,.T.);
#34158=EDGE_CURVE('',#28722,#28721,#15997,.T.);
#34159=EDGE_CURVE('',#28723,#28722,#21166,.T.);
#34160=EDGE_CURVE('',#28724,#28723,#21167,.T.);
#34161=EDGE_CURVE('',#28725,#28724,#21168,.T.);
#34162=EDGE_CURVE('',#28726,#28725,#21169,.T.);
#34163=EDGE_CURVE('',#28727,#28726,#15998,.T.);
#34164=EDGE_CURVE('',#28728,#28727,#15999,.T.);
#34165=EDGE_CURVE('',#28729,#28728,#21170,.T.);
#34166=EDGE_CURVE('',#28730,#28729,#21171,.T.);
#34167=EDGE_CURVE('',#28731,#28730,#21172,.T.);
#34168=EDGE_CURVE('',#28732,#28731,#21173,.T.);
#34169=EDGE_CURVE('',#28733,#28732,#16000,.T.);
#34170=EDGE_CURVE('',#28734,#28733,#16001,.T.);
#34171=EDGE_CURVE('',#28735,#28734,#21174,.T.);
#34172=EDGE_CURVE('',#28736,#28735,#21175,.T.);
#34173=EDGE_CURVE('',#28737,#28736,#21176,.T.);
#34174=EDGE_CURVE('',#28738,#28737,#21177,.T.);
#34175=EDGE_CURVE('',#28739,#28738,#16002,.T.);
#34176=EDGE_CURVE('',#28740,#28739,#16003,.T.);
#34177=EDGE_CURVE('',#28741,#28740,#21178,.T.);
#34178=EDGE_CURVE('',#28742,#28741,#21179,.T.);
#34179=EDGE_CURVE('',#28743,#28742,#21180,.T.);
#34180=EDGE_CURVE('',#28744,#28743,#21181,.T.);
#34181=EDGE_CURVE('',#28745,#28744,#16004,.T.);
#34182=EDGE_CURVE('',#28746,#28745,#16005,.T.);
#34183=EDGE_CURVE('',#28747,#28746,#21182,.T.);
#34184=EDGE_CURVE('',#28748,#28747,#21183,.T.);
#34185=EDGE_CURVE('',#28749,#28748,#21184,.T.);
#34186=EDGE_CURVE('',#28750,#28749,#21185,.T.);
#34187=EDGE_CURVE('',#28751,#28750,#16006,.T.);
#34188=EDGE_CURVE('',#28752,#28751,#16007,.T.);
#34189=EDGE_CURVE('',#28753,#28752,#21186,.T.);
#34190=EDGE_CURVE('',#28754,#28753,#21187,.T.);
#34191=EDGE_CURVE('',#28755,#28754,#21188,.T.);
#34192=EDGE_CURVE('',#28756,#28755,#21189,.T.);
#34193=EDGE_CURVE('',#28757,#28756,#16008,.T.);
#34194=EDGE_CURVE('',#28758,#28757,#16009,.T.);
#34195=EDGE_CURVE('',#28759,#28758,#21190,.T.);
#34196=EDGE_CURVE('',#28760,#28759,#21191,.T.);
#34197=EDGE_CURVE('',#28761,#28760,#21192,.T.);
#34198=EDGE_CURVE('',#28762,#28761,#21193,.T.);
#34199=EDGE_CURVE('',#28763,#28762,#16010,.T.);
#34200=EDGE_CURVE('',#28764,#28763,#16011,.T.);
#34201=EDGE_CURVE('',#28765,#28764,#21194,.T.);
#34202=EDGE_CURVE('',#28766,#28765,#21195,.T.);
#34203=EDGE_CURVE('',#28767,#28766,#21196,.T.);
#34204=EDGE_CURVE('',#28768,#28767,#21197,.T.);
#34205=EDGE_CURVE('',#28769,#28768,#16012,.T.);
#34206=EDGE_CURVE('',#28770,#28769,#16013,.T.);
#34207=EDGE_CURVE('',#28771,#28770,#21198,.T.);
#34208=EDGE_CURVE('',#28772,#28771,#21199,.T.);
#34209=EDGE_CURVE('',#28773,#28772,#21200,.T.);
#34210=EDGE_CURVE('',#28774,#28773,#21201,.T.);
#34211=EDGE_CURVE('',#28775,#28774,#16014,.T.);
#34212=EDGE_CURVE('',#28776,#28775,#16015,.T.);
#34213=EDGE_CURVE('',#28777,#28776,#21202,.T.);
#34214=EDGE_CURVE('',#28778,#28777,#21203,.T.);
#34215=EDGE_CURVE('',#28779,#28778,#21204,.T.);
#34216=EDGE_CURVE('',#28780,#28779,#21205,.T.);
#34217=EDGE_CURVE('',#28781,#28780,#16016,.T.);
#34218=EDGE_CURVE('',#28782,#28781,#16017,.T.);
#34219=EDGE_CURVE('',#28783,#28782,#21206,.T.);
#34220=EDGE_CURVE('',#28784,#28783,#21207,.T.);
#34221=EDGE_CURVE('',#28785,#28784,#21208,.T.);
#34222=EDGE_CURVE('',#28786,#28785,#21209,.T.);
#34223=EDGE_CURVE('',#28787,#28786,#16018,.T.);
#34224=EDGE_CURVE('',#28788,#28787,#16019,.T.);
#34225=EDGE_CURVE('',#28789,#28788,#21210,.T.);
#34226=EDGE_CURVE('',#28790,#28789,#21211,.T.);
#34227=EDGE_CURVE('',#28791,#28790,#21212,.T.);
#34228=EDGE_CURVE('',#28792,#28791,#21213,.T.);
#34229=EDGE_CURVE('',#28793,#28792,#16020,.T.);
#34230=EDGE_CURVE('',#28794,#28793,#16021,.T.);
#34231=EDGE_CURVE('',#28795,#28794,#21214,.T.);
#34232=EDGE_CURVE('',#28796,#28795,#21215,.T.);
#34233=EDGE_CURVE('',#28797,#28796,#21216,.T.);
#34234=EDGE_CURVE('',#28798,#28797,#21217,.T.);
#34235=EDGE_CURVE('',#28799,#28798,#16022,.T.);
#34236=EDGE_CURVE('',#28800,#28799,#16023,.T.);
#34237=EDGE_CURVE('',#28801,#28800,#21218,.T.);
#34238=EDGE_CURVE('',#28802,#28801,#21219,.T.);
#34239=EDGE_CURVE('',#28803,#28802,#21220,.T.);
#34240=EDGE_CURVE('',#28804,#28803,#21221,.T.);
#34241=EDGE_CURVE('',#28805,#28804,#16024,.T.);
#34242=EDGE_CURVE('',#28806,#28805,#16025,.T.);
#34243=EDGE_CURVE('',#28807,#28806,#21222,.F.);
#34244=EDGE_CURVE('',#28807,#28808,#24363,.T.);
#34245=EDGE_CURVE('',#28808,#28808,#16026,.T.);
#34246=EDGE_CURVE('',#28809,#28807,#21223,.F.);
#34247=EDGE_CURVE('',#28810,#28809,#21224,.T.);
#34248=EDGE_CURVE('',#28811,#28810,#21225,.T.);
#34249=EDGE_CURVE('',#28812,#28811,#21226,.T.);
#34250=EDGE_CURVE('',#28813,#28812,#16027,.T.);
#34251=EDGE_CURVE('',#28814,#28813,#16028,.T.);
#34252=EDGE_CURVE('',#28815,#28814,#21227,.T.);
#34253=EDGE_CURVE('',#28816,#28815,#21228,.T.);
#34254=EDGE_CURVE('',#28817,#28816,#21229,.T.);
#34255=EDGE_CURVE('',#28818,#28817,#21230,.T.);
#34256=EDGE_CURVE('',#28819,#28818,#16029,.T.);
#34257=EDGE_CURVE('',#28820,#28819,#16030,.T.);
#34258=EDGE_CURVE('',#28821,#28820,#21231,.T.);
#34259=EDGE_CURVE('',#28822,#28821,#21232,.T.);
#34260=EDGE_CURVE('',#28823,#28822,#21233,.T.);
#34261=EDGE_CURVE('',#28824,#28823,#21234,.T.);
#34262=EDGE_CURVE('',#28825,#28824,#16031,.T.);
#34263=EDGE_CURVE('',#28826,#28825,#16032,.T.);
#34264=EDGE_CURVE('',#28827,#28826,#21235,.T.);
#34265=EDGE_CURVE('',#28828,#28827,#21236,.T.);
#34266=EDGE_CURVE('',#28829,#28828,#21237,.T.);
#34267=EDGE_CURVE('',#28830,#28829,#21238,.T.);
#34268=EDGE_CURVE('',#28831,#28830,#16033,.T.);
#34269=EDGE_CURVE('',#28832,#28831,#16034,.T.);
#34270=EDGE_CURVE('',#28833,#28832,#21239,.T.);
#34271=EDGE_CURVE('',#28834,#28833,#21240,.T.);
#34272=EDGE_CURVE('',#28835,#28834,#21241,.T.);
#34273=EDGE_CURVE('',#28836,#28835,#21242,.T.);
#34274=EDGE_CURVE('',#28837,#28836,#16035,.T.);
#34275=EDGE_CURVE('',#28838,#28837,#16036,.T.);
#34276=EDGE_CURVE('',#28839,#28838,#21243,.T.);
#34277=EDGE_CURVE('',#28840,#28839,#21244,.T.);
#34278=EDGE_CURVE('',#28841,#28840,#21245,.T.);
#34279=EDGE_CURVE('',#28842,#28841,#21246,.T.);
#34280=EDGE_CURVE('',#28843,#28842,#16037,.T.);
#34281=EDGE_CURVE('',#28844,#28843,#16038,.T.);
#34282=EDGE_CURVE('',#28845,#28844,#21247,.T.);
#34283=EDGE_CURVE('',#28846,#28845,#21248,.T.);
#34284=EDGE_CURVE('',#28847,#28846,#21249,.T.);
#34285=EDGE_CURVE('',#28848,#28847,#21250,.T.);
#34286=EDGE_CURVE('',#28849,#28848,#16039,.T.);
#34287=EDGE_CURVE('',#28850,#28849,#16040,.T.);
#34288=EDGE_CURVE('',#28851,#28850,#21251,.T.);
#34289=EDGE_CURVE('',#28852,#28851,#21252,.T.);
#34290=EDGE_CURVE('',#28853,#28852,#21253,.T.);
#34291=EDGE_CURVE('',#28854,#28853,#21254,.T.);
#34292=EDGE_CURVE('',#28855,#28854,#16041,.T.);
#34293=EDGE_CURVE('',#28856,#28855,#16042,.T.);
#34294=EDGE_CURVE('',#28857,#28856,#21255,.T.);
#34295=EDGE_CURVE('',#28858,#28857,#21256,.T.);
#34296=EDGE_CURVE('',#28859,#28858,#21257,.T.);
#34297=EDGE_CURVE('',#28860,#28859,#21258,.T.);
#34298=EDGE_CURVE('',#28861,#28860,#16043,.T.);
#34299=EDGE_CURVE('',#28862,#28861,#16044,.T.);
#34300=EDGE_CURVE('',#28863,#28862,#21259,.T.);
#34301=EDGE_CURVE('',#28864,#28863,#21260,.T.);
#34302=EDGE_CURVE('',#28865,#28864,#21261,.T.);
#34303=EDGE_CURVE('',#28866,#28865,#21262,.T.);
#34304=EDGE_CURVE('',#28867,#28866,#16045,.T.);
#34305=EDGE_CURVE('',#28868,#28867,#16046,.T.);
#34306=EDGE_CURVE('',#28869,#28868,#21263,.T.);
#34307=EDGE_CURVE('',#28870,#28869,#21264,.T.);
#34308=EDGE_CURVE('',#28871,#28870,#21265,.T.);
#34309=EDGE_CURVE('',#28872,#28871,#21266,.T.);
#34310=EDGE_CURVE('',#28873,#28872,#16047,.T.);
#34311=EDGE_CURVE('',#28874,#28873,#16048,.T.);
#34312=EDGE_CURVE('',#28875,#28874,#21267,.T.);
#34313=EDGE_CURVE('',#28876,#28875,#21268,.T.);
#34314=EDGE_CURVE('',#28877,#28876,#21269,.T.);
#34315=EDGE_CURVE('',#28878,#28877,#21270,.T.);
#34316=EDGE_CURVE('',#28879,#28878,#16049,.T.);
#34317=EDGE_CURVE('',#28880,#28879,#16050,.T.);
#34318=EDGE_CURVE('',#28881,#28880,#21271,.T.);
#34319=EDGE_CURVE('',#28882,#28881,#21272,.T.);
#34320=EDGE_CURVE('',#28883,#28882,#21273,.T.);
#34321=EDGE_CURVE('',#28884,#28883,#21274,.T.);
#34322=EDGE_CURVE('',#28885,#28884,#16051,.T.);
#34323=EDGE_CURVE('',#28886,#28885,#16052,.T.);
#34324=EDGE_CURVE('',#28887,#28886,#21275,.T.);
#34325=EDGE_CURVE('',#28888,#28887,#21276,.T.);
#34326=EDGE_CURVE('',#28889,#28888,#21277,.T.);
#34327=EDGE_CURVE('',#28890,#28889,#21278,.T.);
#34328=EDGE_CURVE('',#28891,#28890,#16053,.T.);
#34329=EDGE_CURVE('',#28892,#28891,#16054,.T.);
#34330=EDGE_CURVE('',#28893,#28892,#21279,.T.);
#34331=EDGE_CURVE('',#28894,#28893,#21280,.F.);
#34332=EDGE_CURVE('',#28720,#28894,#21281,.F.);
#34333=EDGE_CURVE('',#28895,#28896,#16055,.F.);
#34334=EDGE_CURVE('',#28897,#28895,#16056,.F.);
#34335=EDGE_CURVE('',#28898,#28897,#21282,.T.);
#34336=EDGE_CURVE('',#28896,#28898,#21283,.T.);
#34337=EDGE_CURVE('',#28899,#28900,#21284,.F.);
#34338=EDGE_CURVE('',#28901,#28899,#16057,.F.);
#34339=EDGE_CURVE('',#28902,#28901,#21285,.T.);
#34340=EDGE_CURVE('',#28900,#28902,#21286,.T.);
#34341=EDGE_CURVE('',#28903,#28904,#21287,.F.);
#34342=EDGE_CURVE('',#28905,#28903,#16058,.T.);
#34343=EDGE_CURVE('',#28906,#28905,#16059,.T.);
#34344=EDGE_CURVE('',#28907,#28906,#16060,.T.);
#34345=EDGE_CURVE('',#28904,#28907,#16061,.T.);
#34346=EDGE_CURVE('',#28908,#28909,#21288,.F.);
#34347=EDGE_CURVE('',#28910,#28908,#21289,.F.);
#34348=EDGE_CURVE('',#28911,#28910,#16062,.T.);
#34349=EDGE_CURVE('',#28909,#28911,#16063,.T.);
#34350=EDGE_CURVE('',#28912,#28913,#21290,.F.);
#34351=EDGE_CURVE('',#28914,#28912,#16064,.F.);
#34352=EDGE_CURVE('',#28915,#28914,#21291,.T.);
#34353=EDGE_CURVE('',#28913,#28915,#21292,.T.);
#34354=EDGE_CURVE('',#28916,#28917,#21293,.F.);
#34355=EDGE_CURVE('',#28918,#28916,#16065,.F.);
#34356=EDGE_CURVE('',#28919,#28918,#21294,.T.);
#34357=EDGE_CURVE('',#28917,#28919,#21295,.T.);
#34358=EDGE_CURVE('',#28920,#28921,#21296,.F.);
#34359=EDGE_CURVE('',#28922,#28920,#16066,.T.);
#34360=EDGE_CURVE('',#28923,#28922,#16067,.T.);
#34361=EDGE_CURVE('',#28921,#28923,#21297,.F.);
#34362=EDGE_CURVE('',#28924,#28925,#16068,.T.);
#34363=EDGE_CURVE('',#28926,#28924,#16069,.T.);
#34364=EDGE_CURVE('',#28927,#28926,#16070,.T.);
#34365=EDGE_CURVE('',#28928,#28927,#21298,.F.);
#34366=EDGE_CURVE('',#28925,#28928,#16071,.T.);
#34367=EDGE_CURVE('',#28929,#28925,#21299,.F.);
#34368=EDGE_CURVE('',#28924,#28929,#16072,.T.);
#34369=EDGE_CURVE('',#28930,#28931,#21300,.F.);
#34370=EDGE_CURVE('',#28932,#28930,#21301,.F.);
#34371=EDGE_CURVE('',#28933,#28932,#16073,.T.);
#34372=EDGE_CURVE('',#28931,#28933,#21302,.T.);
#34373=EDGE_CURVE('',#28934,#28935,#21303,.F.);
#34374=EDGE_CURVE('',#28936,#28934,#21304,.F.);
#34375=EDGE_CURVE('',#28937,#28936,#16074,.T.);
#34376=EDGE_CURVE('',#28935,#28937,#16075,.T.);
#34377=EDGE_CURVE('',#28938,#28939,#21305,.F.);
#34378=EDGE_CURVE('',#28940,#28938,#16076,.T.);
#34379=EDGE_CURVE('',#28941,#28940,#16077,.T.);
#34380=EDGE_CURVE('',#28939,#28941,#21306,.F.);
#34381=EDGE_CURVE('',#28942,#28943,#21307,.F.);
#34382=EDGE_CURVE('',#28944,#28942,#16078,.T.);
#34383=EDGE_CURVE('',#28945,#28944,#16079,.T.);
#34384=EDGE_CURVE('',#28943,#28945,#21308,.F.);
#34385=EDGE_CURVE('',#28946,#28947,#21309,.F.);
#34386=EDGE_CURVE('',#28948,#28946,#21310,.F.);
#34387=EDGE_CURVE('',#28949,#28948,#16080,.T.);
#34388=EDGE_CURVE('',#28947,#28949,#16081,.T.);
#34389=EDGE_CURVE('',#28950,#28951,#21311,.F.);
#34390=EDGE_CURVE('',#28952,#28950,#21312,.F.);
#34391=EDGE_CURVE('',#28953,#28952,#21313,.T.);
#34392=EDGE_CURVE('',#28951,#28953,#16082,.T.);
#34393=EDGE_CURVE('',#28954,#28955,#21314,.F.);
#34394=EDGE_CURVE('',#28956,#28954,#21315,.T.);
#34395=EDGE_CURVE('',#28957,#28956,#16083,.T.);
#34396=EDGE_CURVE('',#28955,#28957,#21316,.F.);
#34397=EDGE_CURVE('',#28958,#28959,#21317,.F.);
#34398=EDGE_CURVE('',#28960,#28958,#21318,.F.);
#34399=EDGE_CURVE('',#28961,#28960,#16084,.T.);
#34400=EDGE_CURVE('',#28959,#28961,#21319,.T.);
#34401=EDGE_CURVE('',#28962,#28963,#21320,.F.);
#34402=EDGE_CURVE('',#28964,#28962,#21321,.F.);
#34403=EDGE_CURVE('',#28965,#28964,#16085,.T.);
#34404=EDGE_CURVE('',#28963,#28965,#16086,.T.);
#34405=EDGE_CURVE('',#28966,#28967,#21322,.F.);
#34406=EDGE_CURVE('',#28968,#28966,#16087,.T.);
#34407=EDGE_CURVE('',#28969,#28968,#16088,.T.);
#34408=EDGE_CURVE('',#28967,#28969,#21323,.F.);
#34409=EDGE_CURVE('',#28970,#28971,#21324,.F.);
#34410=EDGE_CURVE('',#28972,#28970,#16089,.T.);
#34411=EDGE_CURVE('',#28973,#28972,#21325,.T.);
#34412=EDGE_CURVE('',#28971,#28973,#21326,.F.);
#34413=EDGE_CURVE('',#28974,#28975,#21327,.F.);
#34414=EDGE_CURVE('',#28976,#28974,#21328,.F.);
#34415=EDGE_CURVE('',#28977,#28976,#16090,.T.);
#34416=EDGE_CURVE('',#28975,#28977,#16091,.T.);
#34417=EDGE_CURVE('',#28978,#28979,#21329,.F.);
#34418=EDGE_CURVE('',#28980,#28978,#21330,.F.);
#34419=EDGE_CURVE('',#28981,#28980,#21331,.T.);
#34420=EDGE_CURVE('',#28979,#28981,#16092,.T.);
#34421=EDGE_CURVE('',#28982,#28983,#21332,.F.);
#34422=EDGE_CURVE('',#28984,#28982,#21333,.T.);
#34423=EDGE_CURVE('',#28985,#28984,#16093,.T.);
#34424=EDGE_CURVE('',#28983,#28985,#21334,.F.);
#34425=EDGE_CURVE('',#28986,#28987,#21335,.F.);
#34426=EDGE_CURVE('',#28988,#28986,#16094,.T.);
#34427=EDGE_CURVE('',#28989,#28988,#16095,.T.);
#34428=EDGE_CURVE('',#28987,#28989,#21336,.F.);
#34429=EDGE_CURVE('',#28990,#28991,#21337,.F.);
#34430=EDGE_CURVE('',#28992,#28990,#21338,.F.);
#34431=EDGE_CURVE('',#28993,#28992,#16096,.T.);
#34432=EDGE_CURVE('',#28991,#28993,#21339,.T.);
#34433=EDGE_CURVE('',#28994,#28995,#21340,.F.);
#34434=EDGE_CURVE('',#28996,#28994,#21341,.F.);
#34435=EDGE_CURVE('',#28997,#28996,#16097,.T.);
#34436=EDGE_CURVE('',#28995,#28997,#16098,.T.);
#34437=EDGE_CURVE('',#28998,#28999,#21342,.F.);
#34438=EDGE_CURVE('',#29000,#28998,#16099,.T.);
#34439=EDGE_CURVE('',#29001,#29000,#21343,.T.);
#34440=EDGE_CURVE('',#28999,#29001,#21344,.F.);
#34441=EDGE_CURVE('',#29002,#29003,#21345,.F.);
#34442=EDGE_CURVE('',#29004,#29002,#21346,.F.);
#34443=EDGE_CURVE('',#29005,#29004,#16100,.T.);
#34444=EDGE_CURVE('',#29003,#29005,#16101,.T.);
#34445=EDGE_CURVE('',#29006,#29007,#21347,.F.);
#34446=EDGE_CURVE('',#29008,#29006,#21348,.F.);
#34447=EDGE_CURVE('',#29009,#29008,#21349,.T.);
#34448=EDGE_CURVE('',#29007,#29009,#16102,.T.);
#34449=EDGE_CURVE('',#29010,#29011,#21350,.F.);
#34450=EDGE_CURVE('',#29012,#29010,#21351,.T.);
#34451=EDGE_CURVE('',#29013,#29012,#16103,.T.);
#34452=EDGE_CURVE('',#29011,#29013,#21352,.F.);
#34453=EDGE_CURVE('',#29014,#29015,#21353,.F.);
#34454=EDGE_CURVE('',#29016,#29014,#4375,.T.);
#34455=EDGE_CURVE('',#29017,#29016,#16104,.T.);
#34456=EDGE_CURVE('',#29015,#29017,#21354,.F.);
#34457=EDGE_CURVE('',#29018,#29019,#21355,.F.);
#34458=EDGE_CURVE('',#29020,#29018,#21356,.F.);
#34459=EDGE_CURVE('',#29021,#29020,#21357,.T.);
#34460=EDGE_CURVE('',#29019,#29021,#21358,.T.);
#34461=EDGE_CURVE('',#29022,#29023,#21359,.F.);
#34462=EDGE_CURVE('',#29024,#29022,#21360,.F.);
#34463=EDGE_CURVE('',#29025,#29024,#16105,.T.);
#34464=EDGE_CURVE('',#29023,#29025,#16106,.T.);
#34465=EDGE_CURVE('',#29026,#29027,#21361,.F.);
#34466=EDGE_CURVE('',#29028,#29026,#16107,.T.);
#34467=EDGE_CURVE('',#29029,#29028,#21362,.T.);
#34468=EDGE_CURVE('',#29027,#29029,#21363,.F.);
#34469=EDGE_CURVE('',#29030,#29031,#16108,.T.);
#34470=EDGE_CURVE('',#29032,#29031,#24364,.T.);
#34471=EDGE_CURVE('',#29033,#29032,#16109,.T.);
#34472=EDGE_CURVE('',#29030,#29033,#21364,.T.);
#34473=EDGE_CURVE('',#29034,#29035,#16110,.T.);
#34474=EDGE_CURVE('',#29036,#29035,#21365,.T.);
#34475=EDGE_CURVE('',#29032,#29036,#16111,.T.);
#34476=EDGE_CURVE('',#29034,#29032,#24365,.T.);
#34477=EDGE_CURVE('',#29037,#29034,#21366,.T.);
#34478=EDGE_CURVE('',#29038,#29037,#16112,.T.);
#34479=EDGE_CURVE('',#29035,#29038,#16113,.T.);
#34480=EDGE_CURVE('',#29039,#29038,#24366,.T.);
#34481=EDGE_CURVE('',#29036,#29039,#16114,.T.);
#34482=EDGE_CURVE('',#29040,#29041,#16115,.T.);
#34483=EDGE_CURVE('',#29042,#29041,#21367,.T.);
#34484=EDGE_CURVE('',#29039,#29042,#16116,.T.);
#34485=EDGE_CURVE('',#29040,#29039,#24367,.T.);
#34486=EDGE_CURVE('',#29043,#29040,#21368,.T.);
#34487=EDGE_CURVE('',#29044,#29043,#16117,.T.);
#34488=EDGE_CURVE('',#29041,#29044,#16118,.T.);
#34489=EDGE_CURVE('',#29045,#29044,#24368,.T.);
#34490=EDGE_CURVE('',#29042,#29045,#16119,.T.);
#34491=EDGE_CURVE('',#29046,#29047,#16120,.T.);
#34492=EDGE_CURVE('',#29048,#29047,#21369,.T.);
#34493=EDGE_CURVE('',#29045,#29048,#16121,.T.);
#34494=EDGE_CURVE('',#29046,#29045,#24369,.T.);
#34495=EDGE_CURVE('',#29049,#29046,#21370,.T.);
#34496=EDGE_CURVE('',#29050,#29049,#16122,.T.);
#34497=EDGE_CURVE('',#29047,#29050,#16123,.T.);
#34498=EDGE_CURVE('',#29051,#29050,#24370,.T.);
#34499=EDGE_CURVE('',#29048,#29051,#16124,.T.);
#34500=EDGE_CURVE('',#29052,#29053,#16125,.T.);
#34501=EDGE_CURVE('',#29054,#29053,#21371,.T.);
#34502=EDGE_CURVE('',#29051,#29054,#16126,.T.);
#34503=EDGE_CURVE('',#29052,#29051,#24371,.T.);
#34504=EDGE_CURVE('',#29055,#29052,#21372,.T.);
#34505=EDGE_CURVE('',#29056,#29055,#16127,.T.);
#34506=EDGE_CURVE('',#29053,#29056,#16128,.T.);
#34507=EDGE_CURVE('',#29057,#29056,#24372,.T.);
#34508=EDGE_CURVE('',#29054,#29057,#16129,.T.);
#34509=EDGE_CURVE('',#29058,#29059,#16130,.T.);
#34510=EDGE_CURVE('',#29060,#29059,#21373,.T.);
#34511=EDGE_CURVE('',#29057,#29060,#16131,.T.);
#34512=EDGE_CURVE('',#29058,#29057,#24373,.T.);
#34513=EDGE_CURVE('',#29061,#29058,#21374,.T.);
#34514=EDGE_CURVE('',#29062,#29061,#16132,.T.);
#34515=EDGE_CURVE('',#29059,#29062,#16133,.T.);
#34516=EDGE_CURVE('',#29063,#29062,#24374,.T.);
#34517=EDGE_CURVE('',#29060,#29063,#16134,.T.);
#34518=EDGE_CURVE('',#29064,#29065,#16135,.T.);
#34519=EDGE_CURVE('',#29066,#29065,#21375,.T.);
#34520=EDGE_CURVE('',#29063,#29066,#16136,.T.);
#34521=EDGE_CURVE('',#29064,#29063,#24375,.T.);
#34522=EDGE_CURVE('',#29067,#29064,#21376,.T.);
#34523=EDGE_CURVE('',#29068,#29067,#16137,.T.);
#34524=EDGE_CURVE('',#29065,#29068,#16138,.T.);
#34525=EDGE_CURVE('',#29069,#29068,#24376,.T.);
#34526=EDGE_CURVE('',#29066,#29069,#16139,.T.);
#34527=EDGE_CURVE('',#29070,#29026,#21377,.T.);
#34528=EDGE_CURVE('',#29069,#29070,#16140,.T.);
#34529=EDGE_CURVE('',#29028,#29069,#24377,.T.);
#34530=EDGE_CURVE('',#29071,#29027,#24378,.T.);
#34531=EDGE_CURVE('',#29070,#29071,#16141,.T.);
#34532=EDGE_CURVE('',#29072,#29073,#16142,.T.);
#34533=EDGE_CURVE('',#29074,#29073,#21378,.T.);
#34534=EDGE_CURVE('',#29071,#29074,#16143,.T.);
#34535=EDGE_CURVE('',#29072,#29071,#24379,.T.);
#34536=EDGE_CURVE('',#29075,#29072,#21379,.T.);
#34537=EDGE_CURVE('',#29076,#29075,#16144,.T.);
#34538=EDGE_CURVE('',#29073,#29076,#16145,.T.);
#34539=EDGE_CURVE('',#29077,#29076,#24380,.T.);
#34540=EDGE_CURVE('',#29074,#29077,#16146,.T.);
#34541=EDGE_CURVE('',#29078,#29079,#16147,.T.);
#34542=EDGE_CURVE('',#29080,#29079,#21380,.T.);
#34543=EDGE_CURVE('',#29077,#29080,#16148,.T.);
#34544=EDGE_CURVE('',#29078,#29077,#24381,.T.);
#34545=EDGE_CURVE('',#29081,#29078,#21381,.T.);
#34546=EDGE_CURVE('',#29082,#29081,#16149,.T.);
#34547=EDGE_CURVE('',#29079,#29082,#16150,.T.);
#34548=EDGE_CURVE('',#29083,#29082,#24382,.T.);
#34549=EDGE_CURVE('',#29080,#29083,#16151,.T.);
#34550=EDGE_CURVE('',#29084,#29085,#16152,.T.);
#34551=EDGE_CURVE('',#29086,#29085,#21382,.T.);
#34552=EDGE_CURVE('',#29083,#29086,#16153,.T.);
#34553=EDGE_CURVE('',#29084,#29083,#24383,.T.);
#34554=EDGE_CURVE('',#29087,#29084,#21383,.T.);
#34555=EDGE_CURVE('',#29088,#29087,#16154,.T.);
#34556=EDGE_CURVE('',#29085,#29088,#16155,.T.);
#34557=EDGE_CURVE('',#29089,#29088,#24384,.T.);
#34558=EDGE_CURVE('',#29086,#29089,#16156,.T.);
#34559=EDGE_CURVE('',#29090,#29091,#16157,.T.);
#34560=EDGE_CURVE('',#29092,#29091,#21384,.T.);
#34561=EDGE_CURVE('',#29089,#29092,#16158,.T.);
#34562=EDGE_CURVE('',#29090,#29089,#24385,.T.);
#34563=EDGE_CURVE('',#29093,#29090,#21385,.T.);
#34564=EDGE_CURVE('',#29094,#29093,#16159,.T.);
#34565=EDGE_CURVE('',#29091,#29094,#16160,.T.);
#34566=EDGE_CURVE('',#29095,#29094,#24386,.T.);
#34567=EDGE_CURVE('',#29092,#29095,#16161,.T.);
#34568=EDGE_CURVE('',#29096,#29097,#16162,.T.);
#34569=EDGE_CURVE('',#29098,#29097,#21386,.T.);
#34570=EDGE_CURVE('',#29095,#29098,#16163,.T.);
#34571=EDGE_CURVE('',#29096,#29095,#24387,.T.);
#34572=EDGE_CURVE('',#29099,#29096,#21387,.T.);
#34573=EDGE_CURVE('',#29100,#29099,#16164,.T.);
#34574=EDGE_CURVE('',#29097,#29100,#16165,.T.);
#34575=EDGE_CURVE('',#29101,#29100,#24388,.T.);
#34576=EDGE_CURVE('',#29098,#29101,#16166,.T.);
#34577=EDGE_CURVE('',#29102,#29103,#16167,.T.);
#34578=EDGE_CURVE('',#29104,#29103,#21388,.T.);
#34579=EDGE_CURVE('',#29101,#29104,#16168,.T.);
#34580=EDGE_CURVE('',#29102,#29101,#24389,.T.);
#34581=EDGE_CURVE('',#29105,#29102,#21389,.T.);
#34582=EDGE_CURVE('',#29106,#29105,#16169,.T.);
#34583=EDGE_CURVE('',#29103,#29106,#16170,.T.);
#34584=EDGE_CURVE('',#29107,#29106,#24390,.T.);
#34585=EDGE_CURVE('',#29104,#29107,#16171,.T.);
#34586=EDGE_CURVE('',#29108,#29109,#16172,.T.);
#34587=EDGE_CURVE('',#29110,#29109,#21390,.T.);
#34588=EDGE_CURVE('',#29107,#29110,#16173,.T.);
#34589=EDGE_CURVE('',#29108,#29107,#24391,.T.);
#34590=EDGE_CURVE('',#29111,#29108,#21391,.T.);
#34591=EDGE_CURVE('',#29112,#29111,#16174,.T.);
#34592=EDGE_CURVE('',#29109,#29112,#16175,.T.);
#34593=EDGE_CURVE('',#29113,#29112,#24392,.T.);
#34594=EDGE_CURVE('',#29110,#29113,#16176,.T.);
#34595=EDGE_CURVE('',#29114,#29115,#16177,.T.);
#34596=EDGE_CURVE('',#29116,#29115,#21392,.T.);
#34597=EDGE_CURVE('',#29113,#29116,#16178,.T.);
#34598=EDGE_CURVE('',#29114,#29113,#24393,.T.);
#34599=EDGE_CURVE('',#29117,#29114,#21393,.T.);
#34600=EDGE_CURVE('',#29118,#29117,#16179,.T.);
#34601=EDGE_CURVE('',#29115,#29118,#16180,.T.);
#34602=EDGE_CURVE('',#29119,#29118,#24394,.T.);
#34603=EDGE_CURVE('',#29116,#29119,#16181,.T.);
#34604=EDGE_CURVE('',#29120,#29121,#16182,.T.);
#34605=EDGE_CURVE('',#29122,#29121,#21394,.T.);
#34606=EDGE_CURVE('',#29119,#29122,#16183,.T.);
#34607=EDGE_CURVE('',#29120,#29119,#24395,.T.);
#34608=EDGE_CURVE('',#29123,#29120,#21395,.T.);
#34609=EDGE_CURVE('',#29124,#29123,#16184,.T.);
#34610=EDGE_CURVE('',#29121,#29124,#16185,.T.);
#34611=EDGE_CURVE('',#29125,#29124,#24396,.T.);
#34612=EDGE_CURVE('',#29122,#29125,#16186,.T.);
#34613=EDGE_CURVE('',#29126,#29127,#16187,.T.);
#34614=EDGE_CURVE('',#29128,#29127,#21396,.T.);
#34615=EDGE_CURVE('',#29125,#29128,#16188,.T.);
#34616=EDGE_CURVE('',#29126,#29125,#24397,.T.);
#34617=EDGE_CURVE('',#29129,#29126,#21397,.T.);
#34618=EDGE_CURVE('',#29130,#29129,#16189,.T.);
#34619=EDGE_CURVE('',#29127,#29130,#16190,.T.);
#34620=EDGE_CURVE('',#29131,#29130,#24398,.T.);
#34621=EDGE_CURVE('',#29128,#29131,#16191,.T.);
#34622=EDGE_CURVE('',#29132,#29133,#16192,.T.);
#34623=EDGE_CURVE('',#29134,#29133,#21398,.T.);
#34624=EDGE_CURVE('',#29131,#29134,#16193,.T.);
#34625=EDGE_CURVE('',#29132,#29131,#24399,.T.);
#34626=EDGE_CURVE('',#29135,#29132,#21399,.T.);
#34627=EDGE_CURVE('',#29136,#29135,#16194,.T.);
#34628=EDGE_CURVE('',#29133,#29136,#16195,.T.);
#34629=EDGE_CURVE('',#29137,#29136,#24400,.T.);
#34630=EDGE_CURVE('',#29134,#29137,#16196,.T.);
#34631=EDGE_CURVE('',#29138,#29139,#16197,.T.);
#34632=EDGE_CURVE('',#29140,#29139,#21400,.T.);
#34633=EDGE_CURVE('',#29137,#29140,#16198,.T.);
#34634=EDGE_CURVE('',#29138,#29137,#24401,.T.);
#34635=EDGE_CURVE('',#29141,#29138,#21401,.T.);
#34636=EDGE_CURVE('',#29142,#29141,#16199,.T.);
#34637=EDGE_CURVE('',#29139,#29142,#16200,.T.);
#34638=EDGE_CURVE('',#29143,#29142,#24402,.T.);
#34639=EDGE_CURVE('',#29140,#29143,#16201,.T.);
#34640=EDGE_CURVE('',#29144,#29145,#16202,.T.);
#34641=EDGE_CURVE('',#29146,#29145,#21402,.T.);
#34642=EDGE_CURVE('',#29143,#29146,#16203,.T.);
#34643=EDGE_CURVE('',#29144,#29143,#24403,.T.);
#34644=EDGE_CURVE('',#29147,#29144,#21403,.T.);
#34645=EDGE_CURVE('',#29148,#29147,#16204,.T.);
#34646=EDGE_CURVE('',#29145,#29148,#16205,.T.);
#34647=EDGE_CURVE('',#29149,#29148,#24404,.T.);
#34648=EDGE_CURVE('',#29146,#29149,#16206,.T.);
#34649=EDGE_CURVE('',#29150,#29151,#16207,.T.);
#34650=EDGE_CURVE('',#29152,#29151,#21404,.T.);
#34651=EDGE_CURVE('',#29149,#29152,#16208,.T.);
#34652=EDGE_CURVE('',#29150,#29149,#24405,.T.);
#34653=EDGE_CURVE('',#29153,#29150,#21405,.T.);
#34654=EDGE_CURVE('',#29154,#29153,#16209,.T.);
#34655=EDGE_CURVE('',#29151,#29154,#16210,.T.);
#34656=EDGE_CURVE('',#29155,#29154,#24406,.T.);
#34657=EDGE_CURVE('',#29152,#29155,#16211,.T.);
#34658=EDGE_CURVE('',#29156,#29157,#16212,.T.);
#34659=EDGE_CURVE('',#29158,#29157,#21406,.T.);
#34660=EDGE_CURVE('',#29155,#29158,#16213,.T.);
#34661=EDGE_CURVE('',#29156,#29155,#24407,.T.);
#34662=EDGE_CURVE('',#29159,#29156,#21407,.T.);
#34663=EDGE_CURVE('',#29160,#29159,#16214,.T.);
#34664=EDGE_CURVE('',#29157,#29160,#16215,.T.);
#34665=EDGE_CURVE('',#29161,#29160,#24408,.T.);
#34666=EDGE_CURVE('',#29158,#29161,#16216,.T.);
#34667=EDGE_CURVE('',#29162,#29163,#16217,.T.);
#34668=EDGE_CURVE('',#29164,#29163,#21408,.T.);
#34669=EDGE_CURVE('',#29161,#29164,#16218,.T.);
#34670=EDGE_CURVE('',#29162,#29161,#24409,.T.);
#34671=EDGE_CURVE('',#29165,#29162,#21409,.T.);
#34672=EDGE_CURVE('',#29166,#29165,#16219,.T.);
#34673=EDGE_CURVE('',#29163,#29166,#16220,.T.);
#34674=EDGE_CURVE('',#29167,#29166,#24410,.T.);
#34675=EDGE_CURVE('',#29164,#29167,#16221,.T.);
#34676=EDGE_CURVE('',#29168,#29169,#16222,.T.);
#34677=EDGE_CURVE('',#29170,#29169,#21410,.T.);
#34678=EDGE_CURVE('',#29167,#29170,#16223,.T.);
#34679=EDGE_CURVE('',#29168,#29167,#24411,.T.);
#34680=EDGE_CURVE('',#29171,#29168,#21411,.T.);
#34681=EDGE_CURVE('',#29172,#29171,#16224,.T.);
#34682=EDGE_CURVE('',#29169,#29172,#16225,.T.);
#34683=EDGE_CURVE('',#29173,#29172,#24412,.T.);
#34684=EDGE_CURVE('',#29170,#29173,#16226,.T.);
#34685=EDGE_CURVE('',#29174,#29175,#16227,.T.);
#34686=EDGE_CURVE('',#29176,#29175,#21412,.T.);
#34687=EDGE_CURVE('',#29173,#29176,#16228,.T.);
#34688=EDGE_CURVE('',#29174,#29173,#24413,.T.);
#34689=EDGE_CURVE('',#29175,#29177,#16229,.T.);
#34690=EDGE_CURVE('',#29178,#29177,#24414,.T.);
#34691=EDGE_CURVE('',#29176,#29178,#16230,.T.);
#34692=EDGE_CURVE('',#29179,#29174,#21413,.T.);
#34693=EDGE_CURVE('',#29177,#29179,#16231,.T.);
#34694=EDGE_CURVE('',#29180,#29181,#16232,.T.);
#34695=EDGE_CURVE('',#29182,#29181,#21414,.T.);
#34696=EDGE_CURVE('',#29178,#29182,#16233,.T.);
#34697=EDGE_CURVE('',#29180,#29178,#24415,.T.);
#34698=EDGE_CURVE('',#29181,#29183,#16234,.T.);
#34699=EDGE_CURVE('',#29184,#29180,#21415,.T.);
#34700=EDGE_CURVE('',#29183,#29184,#16235,.T.);
#34701=EDGE_CURVE('',#29182,#29185,#16236,.T.);
#34702=EDGE_CURVE('',#29185,#29183,#24416,.T.);
#34703=EDGE_CURVE('',#29186,#29187,#16237,.T.);
#34704=EDGE_CURVE('',#29188,#29187,#21416,.T.);
#34705=EDGE_CURVE('',#29185,#29188,#16238,.T.);
#34706=EDGE_CURVE('',#29186,#29185,#24417,.T.);
#34707=EDGE_CURVE('',#29189,#29186,#21417,.T.);
#34708=EDGE_CURVE('',#29190,#29189,#16239,.T.);
#34709=EDGE_CURVE('',#29187,#29190,#16240,.T.);
#34710=EDGE_CURVE('',#29191,#29190,#24418,.T.);
#34711=EDGE_CURVE('',#29188,#29191,#16241,.T.);
#34712=EDGE_CURVE('',#29192,#29193,#16242,.T.);
#34713=EDGE_CURVE('',#29194,#29193,#21418,.T.);
#34714=EDGE_CURVE('',#29191,#29194,#16243,.T.);
#34715=EDGE_CURVE('',#29192,#29191,#24419,.T.);
#34716=EDGE_CURVE('',#29195,#29192,#21419,.T.);
#34717=EDGE_CURVE('',#29196,#29195,#16244,.T.);
#34718=EDGE_CURVE('',#29193,#29196,#16245,.T.);
#34719=EDGE_CURVE('',#29197,#29196,#24420,.T.);
#34720=EDGE_CURVE('',#29194,#29197,#16246,.T.);
#34721=EDGE_CURVE('',#29198,#29199,#21420,.T.);
#34722=EDGE_CURVE('',#29031,#29198,#16247,.T.);
#34723=EDGE_CURVE('',#29199,#29030,#16248,.T.);
#34724=EDGE_CURVE('',#29197,#29033,#16249,.T.);
#34725=EDGE_CURVE('',#29199,#29197,#24421,.T.);
#34726=EDGE_CURVE('',#29200,#29197,#21421,.T.);
#34727=EDGE_CURVE('',#29200,#29201,#16250,.T.);
#34728=EDGE_CURVE('',#29194,#29201,#24422,.T.);
#34729=EDGE_CURVE('',#29202,#29194,#24423,.T.);
#34730=EDGE_CURVE('',#29202,#29203,#16251,.T.);
#34731=EDGE_CURVE('',#29191,#29203,#21422,.T.);
#34732=EDGE_CURVE('',#29203,#29204,#16252,.T.);
#34733=EDGE_CURVE('',#29188,#29204,#24424,.T.);
#34734=EDGE_CURVE('',#29205,#29202,#16253,.T.);
#34735=EDGE_CURVE('',#29204,#29205,#16254,.T.);
#34736=EDGE_CURVE('',#29206,#29188,#24425,.T.);
#34737=EDGE_CURVE('',#29206,#29207,#16255,.T.);
#34738=EDGE_CURVE('',#29185,#29207,#21423,.T.);
#34739=EDGE_CURVE('',#29207,#29208,#16256,.T.);
#34740=EDGE_CURVE('',#29182,#29208,#24426,.T.);
#34741=EDGE_CURVE('',#29209,#29206,#16257,.T.);
#34742=EDGE_CURVE('',#29208,#29209,#16258,.T.);
#34743=EDGE_CURVE('',#29210,#29182,#24427,.T.);
#34744=EDGE_CURVE('',#29210,#29211,#16259,.T.);
#34745=EDGE_CURVE('',#29178,#29211,#21424,.T.);
#34746=EDGE_CURVE('',#29211,#29212,#16260,.T.);
#34747=EDGE_CURVE('',#29176,#29212,#24428,.T.);
#34748=EDGE_CURVE('',#29213,#29210,#16261,.T.);
#34749=EDGE_CURVE('',#29212,#29213,#16262,.T.);
#34750=EDGE_CURVE('',#29214,#29176,#24429,.T.);
#34751=EDGE_CURVE('',#29214,#29215,#16263,.T.);
#34752=EDGE_CURVE('',#29173,#29215,#21425,.T.);
#34753=EDGE_CURVE('',#29215,#29216,#16264,.T.);
#34754=EDGE_CURVE('',#29170,#29216,#24430,.T.);
#34755=EDGE_CURVE('',#29217,#29214,#16265,.T.);
#34756=EDGE_CURVE('',#29216,#29217,#16266,.T.);
#34757=EDGE_CURVE('',#29218,#29170,#24431,.T.);
#34758=EDGE_CURVE('',#29218,#29219,#16267,.T.);
#34759=EDGE_CURVE('',#29167,#29219,#21426,.T.);
#34760=EDGE_CURVE('',#29219,#29220,#16268,.T.);
#34761=EDGE_CURVE('',#29164,#29220,#24432,.T.);
#34762=EDGE_CURVE('',#29221,#29218,#16269,.T.);
#34763=EDGE_CURVE('',#29220,#29221,#16270,.T.);
#34764=EDGE_CURVE('',#29222,#29164,#24433,.T.);
#34765=EDGE_CURVE('',#29222,#29223,#16271,.T.);
#34766=EDGE_CURVE('',#29161,#29223,#21427,.T.);
#34767=EDGE_CURVE('',#29223,#29224,#16272,.T.);
#34768=EDGE_CURVE('',#29158,#29224,#24434,.T.);
#34769=EDGE_CURVE('',#29225,#29222,#16273,.T.);
#34770=EDGE_CURVE('',#29224,#29225,#16274,.T.);
#34771=EDGE_CURVE('',#29226,#29158,#24435,.T.);
#34772=EDGE_CURVE('',#29226,#29227,#16275,.T.);
#34773=EDGE_CURVE('',#29155,#29227,#21428,.T.);
#34774=EDGE_CURVE('',#29227,#29228,#16276,.T.);
#34775=EDGE_CURVE('',#29152,#29228,#24436,.T.);
#34776=EDGE_CURVE('',#29229,#29226,#16277,.T.);
#34777=EDGE_CURVE('',#29228,#29229,#16278,.T.);
#34778=EDGE_CURVE('',#29230,#29152,#24437,.T.);
#34779=EDGE_CURVE('',#29230,#29231,#16279,.T.);
#34780=EDGE_CURVE('',#29149,#29231,#21429,.T.);
#34781=EDGE_CURVE('',#29231,#29232,#16280,.T.);
#34782=EDGE_CURVE('',#29146,#29232,#24438,.T.);
#34783=EDGE_CURVE('',#29233,#29230,#16281,.T.);
#34784=EDGE_CURVE('',#29232,#29233,#16282,.T.);
#34785=EDGE_CURVE('',#29234,#29146,#24439,.T.);
#34786=EDGE_CURVE('',#29234,#29235,#16283,.T.);
#34787=EDGE_CURVE('',#29143,#29235,#21430,.T.);
#34788=EDGE_CURVE('',#29235,#29236,#16284,.T.);
#34789=EDGE_CURVE('',#29140,#29236,#24440,.T.);
#34790=EDGE_CURVE('',#29237,#29234,#16285,.T.);
#34791=EDGE_CURVE('',#29236,#29237,#16286,.T.);
#34792=EDGE_CURVE('',#29238,#29140,#24441,.T.);
#34793=EDGE_CURVE('',#29238,#29239,#16287,.T.);
#34794=EDGE_CURVE('',#29137,#29239,#21431,.T.);
#34795=EDGE_CURVE('',#29239,#29240,#16288,.T.);
#34796=EDGE_CURVE('',#29134,#29240,#24442,.T.);
#34797=EDGE_CURVE('',#29241,#29238,#16289,.T.);
#34798=EDGE_CURVE('',#29240,#29241,#16290,.T.);
#34799=EDGE_CURVE('',#29242,#29134,#24443,.T.);
#34800=EDGE_CURVE('',#29242,#29243,#16291,.T.);
#34801=EDGE_CURVE('',#29131,#29243,#21432,.T.);
#34802=EDGE_CURVE('',#29243,#29244,#16292,.T.);
#34803=EDGE_CURVE('',#29128,#29244,#24444,.T.);
#34804=EDGE_CURVE('',#29245,#29242,#16293,.T.);
#34805=EDGE_CURVE('',#29244,#29245,#16294,.T.);
#34806=EDGE_CURVE('',#29246,#29128,#24445,.T.);
#34807=EDGE_CURVE('',#29246,#29247,#16295,.T.);
#34808=EDGE_CURVE('',#29125,#29247,#21433,.T.);
#34809=EDGE_CURVE('',#29247,#29248,#16296,.T.);
#34810=EDGE_CURVE('',#29122,#29248,#24446,.T.);
#34811=EDGE_CURVE('',#29249,#29246,#16297,.T.);
#34812=EDGE_CURVE('',#29248,#29249,#16298,.T.);
#34813=EDGE_CURVE('',#29250,#29122,#24447,.T.);
#34814=EDGE_CURVE('',#29250,#29251,#16299,.T.);
#34815=EDGE_CURVE('',#29119,#29251,#21434,.T.);
#34816=EDGE_CURVE('',#29251,#29252,#16300,.T.);
#34817=EDGE_CURVE('',#29116,#29252,#24448,.T.);
#34818=EDGE_CURVE('',#29253,#29250,#16301,.T.);
#34819=EDGE_CURVE('',#29252,#29253,#16302,.T.);
#34820=EDGE_CURVE('',#29025,#29116,#24449,.T.);
#34821=EDGE_CURVE('',#29113,#29024,#21435,.T.);
#34822=EDGE_CURVE('',#29110,#29022,#24450,.T.);
#34823=EDGE_CURVE('',#29254,#29110,#24451,.T.);
#34824=EDGE_CURVE('',#29254,#29255,#16303,.T.);
#34825=EDGE_CURVE('',#29107,#29255,#21436,.T.);
#34826=EDGE_CURVE('',#29255,#29256,#16304,.T.);
#34827=EDGE_CURVE('',#29104,#29256,#24452,.T.);
#34828=EDGE_CURVE('',#29257,#29254,#16305,.T.);
#34829=EDGE_CURVE('',#29256,#29257,#16306,.T.);
#34830=EDGE_CURVE('',#29258,#29104,#24453,.T.);
#34831=EDGE_CURVE('',#29258,#29259,#16307,.T.);
#34832=EDGE_CURVE('',#29101,#29259,#21437,.T.);
#34833=EDGE_CURVE('',#29259,#29260,#16308,.T.);
#34834=EDGE_CURVE('',#29098,#29260,#24454,.T.);
#34835=EDGE_CURVE('',#29261,#29258,#16309,.T.);
#34836=EDGE_CURVE('',#29260,#29261,#16310,.T.);
#34837=EDGE_CURVE('',#29262,#29098,#24455,.T.);
#34838=EDGE_CURVE('',#29262,#29263,#16311,.T.);
#34839=EDGE_CURVE('',#29095,#29263,#21438,.T.);
#34840=EDGE_CURVE('',#29263,#29264,#16312,.T.);
#34841=EDGE_CURVE('',#29092,#29264,#24456,.T.);
#34842=EDGE_CURVE('',#29265,#29262,#16313,.T.);
#34843=EDGE_CURVE('',#29264,#29265,#16314,.T.);
#34844=EDGE_CURVE('',#29266,#29092,#24457,.T.);
#34845=EDGE_CURVE('',#29266,#29267,#16315,.T.);
#34846=EDGE_CURVE('',#29089,#29267,#21439,.T.);
#34847=EDGE_CURVE('',#29267,#29268,#16316,.T.);
#34848=EDGE_CURVE('',#29086,#29268,#24458,.T.);
#34849=EDGE_CURVE('',#29269,#29266,#16317,.T.);
#34850=EDGE_CURVE('',#29268,#29269,#16318,.T.);
#34851=EDGE_CURVE('',#29270,#29086,#24459,.T.);
#34852=EDGE_CURVE('',#29270,#29271,#16319,.T.);
#34853=EDGE_CURVE('',#29083,#29271,#21440,.T.);
#34854=EDGE_CURVE('',#29271,#29272,#16320,.T.);
#34855=EDGE_CURVE('',#29080,#29272,#24460,.T.);
#34856=EDGE_CURVE('',#29273,#29270,#16321,.T.);
#34857=EDGE_CURVE('',#29272,#29273,#16322,.T.);
#34858=EDGE_CURVE('',#29274,#29080,#24461,.T.);
#34859=EDGE_CURVE('',#29274,#29275,#16323,.T.);
#34860=EDGE_CURVE('',#29077,#29275,#21441,.T.);
#34861=EDGE_CURVE('',#29275,#29276,#16324,.T.);
#34862=EDGE_CURVE('',#29074,#29276,#24462,.T.);
#34863=EDGE_CURVE('',#29277,#29274,#16325,.T.);
#34864=EDGE_CURVE('',#29276,#29277,#16326,.T.);
#34865=EDGE_CURVE('',#29278,#29074,#24463,.T.);
#34866=EDGE_CURVE('',#29278,#29279,#16327,.T.);
#34867=EDGE_CURVE('',#29071,#29279,#21442,.T.);
#34868=EDGE_CURVE('',#29279,#29280,#16328,.T.);
#34869=EDGE_CURVE('',#29070,#29280,#24464,.T.);
#34870=EDGE_CURVE('',#29281,#29278,#16329,.T.);
#34871=EDGE_CURVE('',#29280,#29281,#16330,.T.);
#34872=EDGE_CURVE('',#29282,#29070,#24465,.T.);
#34873=EDGE_CURVE('',#29282,#29283,#16331,.T.);
#34874=EDGE_CURVE('',#29069,#29283,#21443,.T.);
#34875=EDGE_CURVE('',#29283,#29284,#16332,.T.);
#34876=EDGE_CURVE('',#29066,#29284,#24466,.T.);
#34877=EDGE_CURVE('',#29285,#29282,#16333,.T.);
#34878=EDGE_CURVE('',#29284,#29285,#16334,.T.);
#34879=EDGE_CURVE('',#29286,#29066,#24467,.T.);
#34880=EDGE_CURVE('',#29286,#29287,#16335,.T.);
#34881=EDGE_CURVE('',#29063,#29287,#21444,.T.);
#34882=EDGE_CURVE('',#29287,#29288,#16336,.T.);
#34883=EDGE_CURVE('',#29060,#29288,#24468,.T.);
#34884=EDGE_CURVE('',#29289,#29286,#16337,.T.);
#34885=EDGE_CURVE('',#29288,#29289,#16338,.T.);
#34886=EDGE_CURVE('',#29290,#29060,#24469,.T.);
#34887=EDGE_CURVE('',#29290,#29291,#16339,.T.);
#34888=EDGE_CURVE('',#29057,#29291,#21445,.T.);
#34889=EDGE_CURVE('',#29291,#29292,#16340,.T.);
#34890=EDGE_CURVE('',#29054,#29292,#24470,.T.);
#34891=EDGE_CURVE('',#29293,#29290,#16341,.T.);
#34892=EDGE_CURVE('',#29292,#29293,#16342,.T.);
#34893=EDGE_CURVE('',#29294,#29054,#24471,.T.);
#34894=EDGE_CURVE('',#29294,#29295,#16343,.T.);
#34895=EDGE_CURVE('',#29051,#29295,#21446,.T.);
#34896=EDGE_CURVE('',#29295,#29296,#16344,.T.);
#34897=EDGE_CURVE('',#29048,#29296,#24472,.T.);
#34898=EDGE_CURVE('',#29297,#29294,#16345,.T.);
#34899=EDGE_CURVE('',#29296,#29297,#16346,.T.);
#34900=EDGE_CURVE('',#29298,#29048,#24473,.T.);
#34901=EDGE_CURVE('',#29298,#29299,#16347,.T.);
#34902=EDGE_CURVE('',#29045,#29299,#21447,.T.);
#34903=EDGE_CURVE('',#29299,#29300,#16348,.T.);
#34904=EDGE_CURVE('',#29042,#29300,#24474,.T.);
#34905=EDGE_CURVE('',#29301,#29298,#16349,.T.);
#34906=EDGE_CURVE('',#29300,#29301,#16350,.T.);
#34907=EDGE_CURVE('',#29302,#29042,#24475,.T.);
#34908=EDGE_CURVE('',#29302,#29303,#16351,.T.);
#34909=EDGE_CURVE('',#29039,#29303,#21448,.T.);
#34910=EDGE_CURVE('',#29303,#29304,#16352,.T.);
#34911=EDGE_CURVE('',#29036,#29304,#24476,.T.);
#34912=EDGE_CURVE('',#29305,#29302,#16353,.T.);
#34913=EDGE_CURVE('',#29304,#29305,#16354,.T.);
#34914=EDGE_CURVE('',#29306,#29036,#24477,.T.);
#34915=EDGE_CURVE('',#29306,#29307,#16355,.T.);
#34916=EDGE_CURVE('',#29032,#29307,#21449,.T.);
#34917=EDGE_CURVE('',#29307,#29308,#16356,.T.);
#34918=EDGE_CURVE('',#29033,#29308,#24478,.T.);
#34919=EDGE_CURVE('',#29309,#29306,#16357,.T.);
#34920=EDGE_CURVE('',#29308,#29309,#16358,.T.);
#34921=EDGE_CURVE('',#29310,#29200,#16359,.T.);
#34922=EDGE_CURVE('',#29311,#29310,#16360,.T.);
#34923=EDGE_CURVE('',#29201,#29311,#16361,.T.);
#34924=EDGE_CURVE('',#29310,#29033,#24479,.T.);
#34925=EDGE_CURVE('',#29032,#29312,#16362,.T.);
#34926=EDGE_CURVE('',#29312,#29198,#21450,.T.);
#34927=EDGE_CURVE('',#29313,#29032,#4376,.T.);
#34928=EDGE_CURVE('',#29037,#29313,#21451,.T.);
#34929=EDGE_CURVE('',#29039,#29313,#16363,.T.);
#34930=EDGE_CURVE('',#29314,#29039,#4377,.T.);
#34931=EDGE_CURVE('',#29043,#29314,#21452,.T.);
#34932=EDGE_CURVE('',#29045,#29314,#16364,.T.);
#34933=EDGE_CURVE('',#29315,#29045,#4378,.T.);
#34934=EDGE_CURVE('',#29049,#29315,#21453,.T.);
#34935=EDGE_CURVE('',#29051,#29315,#16365,.T.);
#34936=EDGE_CURVE('',#29316,#29051,#4379,.T.);
#34937=EDGE_CURVE('',#29055,#29316,#21454,.T.);
#34938=EDGE_CURVE('',#29057,#29316,#16366,.T.);
#34939=EDGE_CURVE('',#29317,#29057,#4380,.T.);
#34940=EDGE_CURVE('',#29061,#29317,#21455,.T.);
#34941=EDGE_CURVE('',#29063,#29317,#16367,.T.);
#34942=EDGE_CURVE('',#29318,#29063,#4381,.T.);
#34943=EDGE_CURVE('',#29067,#29318,#21456,.T.);
#34944=EDGE_CURVE('',#29069,#29318,#16368,.T.);
#34945=EDGE_CURVE('',#29319,#29069,#4382,.T.);
#34946=EDGE_CURVE('',#29029,#29319,#21457,.T.);
#34947=EDGE_CURVE('',#29071,#29319,#16369,.T.);
#34948=EDGE_CURVE('',#29320,#29071,#21458,.T.);
#34949=EDGE_CURVE('',#29075,#29320,#21459,.T.);
#34950=EDGE_CURVE('',#29077,#29320,#16370,.T.);
#34951=EDGE_CURVE('',#29321,#29077,#4383,.T.);
#34952=EDGE_CURVE('',#29081,#29321,#21460,.T.);
#34953=EDGE_CURVE('',#29083,#29321,#16371,.T.);
#34954=EDGE_CURVE('',#29322,#29083,#4384,.T.);
#34955=EDGE_CURVE('',#29087,#29322,#21461,.T.);
#34956=EDGE_CURVE('',#29089,#29322,#16372,.T.);
#34957=EDGE_CURVE('',#29323,#29089,#4385,.T.);
#34958=EDGE_CURVE('',#29093,#29323,#21462,.T.);
#34959=EDGE_CURVE('',#29095,#29323,#16373,.T.);
#34960=EDGE_CURVE('',#29324,#29095,#4386,.T.);
#34961=EDGE_CURVE('',#29099,#29324,#21463,.T.);
#34962=EDGE_CURVE('',#29101,#29324,#16374,.T.);
#34963=EDGE_CURVE('',#29325,#29101,#21464,.T.);
#34964=EDGE_CURVE('',#29105,#29325,#21465,.T.);
#34965=EDGE_CURVE('',#29107,#29325,#16375,.T.);
#34966=EDGE_CURVE('',#29326,#29107,#21466,.T.);
#34967=EDGE_CURVE('',#29111,#29326,#21467,.T.);
#34968=EDGE_CURVE('',#29113,#29326,#16376,.T.);
#34969=EDGE_CURVE('',#29327,#29113,#4387,.T.);
#34970=EDGE_CURVE('',#29117,#29327,#21468,.T.);
#34971=EDGE_CURVE('',#29119,#29327,#16377,.T.);
#34972=EDGE_CURVE('',#29328,#29119,#4388,.T.);
#34973=EDGE_CURVE('',#29123,#29328,#21469,.T.);
#34974=EDGE_CURVE('',#29125,#29328,#16378,.T.);
#34975=EDGE_CURVE('',#29329,#29125,#21470,.T.);
#34976=EDGE_CURVE('',#29129,#29329,#21471,.T.);
#34977=EDGE_CURVE('',#29131,#29329,#16379,.T.);
#34978=EDGE_CURVE('',#29330,#29131,#4389,.T.);
#34979=EDGE_CURVE('',#29135,#29330,#21472,.T.);
#34980=EDGE_CURVE('',#29137,#29330,#16380,.T.);
#34981=EDGE_CURVE('',#29331,#29137,#4390,.T.);
#34982=EDGE_CURVE('',#29141,#29331,#21473,.T.);
#34983=EDGE_CURVE('',#29143,#29331,#16381,.T.);
#34984=EDGE_CURVE('',#29332,#29143,#4391,.T.);
#34985=EDGE_CURVE('',#29147,#29332,#21474,.T.);
#34986=EDGE_CURVE('',#29149,#29332,#16382,.T.);
#34987=EDGE_CURVE('',#29333,#29149,#4392,.T.);
#34988=EDGE_CURVE('',#29153,#29333,#21475,.T.);
#34989=EDGE_CURVE('',#29155,#29333,#16383,.T.);
#34990=EDGE_CURVE('',#29334,#29155,#4393,.T.);
#34991=EDGE_CURVE('',#29159,#29334,#21476,.T.);
#34992=EDGE_CURVE('',#29161,#29334,#16384,.T.);
#34993=EDGE_CURVE('',#29335,#29161,#21477,.T.);
#34994=EDGE_CURVE('',#29165,#29335,#21478,.T.);
#34995=EDGE_CURVE('',#29167,#29335,#16385,.T.);
#34996=EDGE_CURVE('',#29336,#29167,#21479,.T.);
#34997=EDGE_CURVE('',#29171,#29336,#21480,.T.);
#34998=EDGE_CURVE('',#29173,#29336,#16386,.T.);
#34999=EDGE_CURVE('',#29337,#29173,#21481,.T.);
#35000=EDGE_CURVE('',#29179,#29337,#21482,.T.);
#35001=EDGE_CURVE('',#29178,#29337,#16387,.T.);
#35002=EDGE_CURVE('',#29338,#29178,#4394,.T.);
#35003=EDGE_CURVE('',#29184,#29338,#21483,.T.);
#35004=EDGE_CURVE('',#29185,#29338,#16388,.T.);
#35005=EDGE_CURVE('',#29339,#29185,#4395,.T.);
#35006=EDGE_CURVE('',#29189,#29339,#21484,.T.);
#35007=EDGE_CURVE('',#29191,#29339,#16389,.T.);
#35008=EDGE_CURVE('',#29340,#29191,#4396,.T.);
#35009=EDGE_CURVE('',#29195,#29340,#21485,.T.);
#35010=EDGE_CURVE('',#29197,#29340,#16390,.T.);
#35011=EDGE_CURVE('',#29312,#29197,#21486,.T.);
#35012=EDGE_CURVE('',#29341,#29311,#21487,.T.);
#35013=EDGE_CURVE('',#29194,#29341,#16391,.T.);
#35014=EDGE_CURVE('',#29342,#29194,#16392,.T.);
#35015=EDGE_CURVE('',#29205,#29342,#21488,.T.);
#35016=EDGE_CURVE('',#29188,#29342,#16393,.T.);
#35017=EDGE_CURVE('',#29343,#29188,#16394,.T.);
#35018=EDGE_CURVE('',#29209,#29343,#21489,.T.);
#35019=EDGE_CURVE('',#29182,#29343,#16395,.T.);
#35020=EDGE_CURVE('',#29344,#29182,#16396,.T.);
#35021=EDGE_CURVE('',#29213,#29344,#21490,.T.);
#35022=EDGE_CURVE('',#29176,#29344,#16397,.T.);
#35023=EDGE_CURVE('',#29345,#29176,#16398,.T.);
#35024=EDGE_CURVE('',#29217,#29345,#21491,.T.);
#35025=EDGE_CURVE('',#29170,#29345,#16399,.T.);
#35026=EDGE_CURVE('',#29346,#29170,#16400,.T.);
#35027=EDGE_CURVE('',#29221,#29346,#21492,.T.);
#35028=EDGE_CURVE('',#29164,#29346,#16401,.T.);
#35029=EDGE_CURVE('',#29347,#29164,#16402,.T.);
#35030=EDGE_CURVE('',#29225,#29347,#21493,.T.);
#35031=EDGE_CURVE('',#29158,#29347,#16403,.T.);
#35032=EDGE_CURVE('',#29348,#29158,#16404,.T.);
#35033=EDGE_CURVE('',#29229,#29348,#21494,.T.);
#35034=EDGE_CURVE('',#29152,#29348,#16405,.T.);
#35035=EDGE_CURVE('',#29349,#29152,#16406,.T.);
#35036=EDGE_CURVE('',#29233,#29349,#21495,.T.);
#35037=EDGE_CURVE('',#29146,#29349,#16407,.T.);
#35038=EDGE_CURVE('',#29350,#29146,#16408,.T.);
#35039=EDGE_CURVE('',#29237,#29350,#21496,.T.);
#35040=EDGE_CURVE('',#29140,#29350,#16409,.T.);
#35041=EDGE_CURVE('',#29351,#29140,#16410,.T.);
#35042=EDGE_CURVE('',#29241,#29351,#21497,.T.);
#35043=EDGE_CURVE('',#29134,#29351,#16411,.T.);
#35044=EDGE_CURVE('',#29352,#29134,#16412,.T.);
#35045=EDGE_CURVE('',#29245,#29352,#21498,.T.);
#35046=EDGE_CURVE('',#29128,#29352,#16413,.T.);
#35047=EDGE_CURVE('',#29353,#29128,#16414,.T.);
#35048=EDGE_CURVE('',#29249,#29353,#21499,.T.);
#35049=EDGE_CURVE('',#29122,#29353,#16415,.T.);
#35050=EDGE_CURVE('',#29354,#29122,#16416,.T.);
#35051=EDGE_CURVE('',#29253,#29354,#21500,.T.);
#35052=EDGE_CURVE('',#29116,#29354,#16417,.T.);
#35053=EDGE_CURVE('',#29355,#29116,#16418,.T.);
#35054=EDGE_CURVE('',#29023,#29355,#21501,.T.);
#35055=EDGE_CURVE('',#29110,#29355,#16419,.T.);
#35056=EDGE_CURVE('',#29356,#29110,#16420,.T.);
#35057=EDGE_CURVE('',#29257,#29356,#21502,.T.);
#35058=EDGE_CURVE('',#29104,#29356,#16421,.T.);
#35059=EDGE_CURVE('',#29357,#29104,#16422,.T.);
#35060=EDGE_CURVE('',#29261,#29357,#21503,.T.);
#35061=EDGE_CURVE('',#29098,#29357,#16423,.T.);
#35062=EDGE_CURVE('',#29358,#29098,#16424,.T.);
#35063=EDGE_CURVE('',#29265,#29358,#21504,.T.);
#35064=EDGE_CURVE('',#29092,#29358,#16425,.T.);
#35065=EDGE_CURVE('',#29359,#29092,#16426,.T.);
#35066=EDGE_CURVE('',#29269,#29359,#21505,.T.);
#35067=EDGE_CURVE('',#29086,#29359,#16427,.T.);
#35068=EDGE_CURVE('',#29360,#29086,#16428,.T.);
#35069=EDGE_CURVE('',#29273,#29360,#21506,.T.);
#35070=EDGE_CURVE('',#29080,#29360,#16429,.T.);
#35071=EDGE_CURVE('',#29361,#29080,#16430,.T.);
#35072=EDGE_CURVE('',#29277,#29361,#21507,.T.);
#35073=EDGE_CURVE('',#29074,#29361,#16431,.T.);
#35074=EDGE_CURVE('',#29362,#29074,#16432,.T.);
#35075=EDGE_CURVE('',#29281,#29362,#21508,.T.);
#35076=EDGE_CURVE('',#29070,#29362,#16433,.T.);
#35077=EDGE_CURVE('',#29363,#29070,#16434,.T.);
#35078=EDGE_CURVE('',#29285,#29363,#21509,.T.);
#35079=EDGE_CURVE('',#29066,#29363,#16435,.T.);
#35080=EDGE_CURVE('',#29364,#29066,#16436,.T.);
#35081=EDGE_CURVE('',#29289,#29364,#21510,.T.);
#35082=EDGE_CURVE('',#29060,#29364,#16437,.T.);
#35083=EDGE_CURVE('',#29365,#29060,#16438,.T.);
#35084=EDGE_CURVE('',#29293,#29365,#21511,.T.);
#35085=EDGE_CURVE('',#29054,#29365,#16439,.T.);
#35086=EDGE_CURVE('',#29366,#29054,#16440,.T.);
#35087=EDGE_CURVE('',#29297,#29366,#21512,.T.);
#35088=EDGE_CURVE('',#29048,#29366,#16441,.T.);
#35089=EDGE_CURVE('',#29367,#29048,#16442,.T.);
#35090=EDGE_CURVE('',#29301,#29367,#21513,.T.);
#35091=EDGE_CURVE('',#29042,#29367,#16443,.T.);
#35092=EDGE_CURVE('',#29368,#29042,#16444,.T.);
#35093=EDGE_CURVE('',#29305,#29368,#21514,.T.);
#35094=EDGE_CURVE('',#29036,#29368,#16445,.T.);
#35095=EDGE_CURVE('',#29369,#29036,#16446,.T.);
#35096=EDGE_CURVE('',#29309,#29369,#21515,.T.);
#35097=EDGE_CURVE('',#29033,#29369,#16447,.T.);
#35098=EDGE_CURVE('',#29341,#29033,#16448,.T.);
#35099=EDGE_CURVE('',#29370,#29371,#16449,.T.);
#35100=EDGE_CURVE('',#29032,#29371,#21516,.T.);
#35101=EDGE_CURVE('',#29370,#29312,#24480,.T.);
#35102=EDGE_CURVE('',#29372,#29370,#16450,.T.);
#35103=EDGE_CURVE('',#29373,#29372,#21517,.T.);
#35104=EDGE_CURVE('',#29371,#29373,#21518,.T.);
#35105=EDGE_CURVE('',#29313,#29373,#24481,.T.);
#35106=EDGE_CURVE('',#29374,#29375,#16451,.T.);
#35107=EDGE_CURVE('',#29039,#29375,#21519,.T.);
#35108=EDGE_CURVE('',#29374,#29313,#24482,.T.);
#35109=EDGE_CURVE('',#29376,#29374,#16452,.T.);
#35110=EDGE_CURVE('',#29377,#29376,#21520,.T.);
#35111=EDGE_CURVE('',#29375,#29377,#21521,.T.);
#35112=EDGE_CURVE('',#29314,#29377,#24483,.T.);
#35113=EDGE_CURVE('',#29378,#29379,#16453,.T.);
#35114=EDGE_CURVE('',#29045,#29379,#21522,.T.);
#35115=EDGE_CURVE('',#29378,#29314,#24484,.T.);
#35116=EDGE_CURVE('',#29380,#29378,#16454,.T.);
#35117=EDGE_CURVE('',#29381,#29380,#21523,.T.);
#35118=EDGE_CURVE('',#29379,#29381,#21524,.T.);
#35119=EDGE_CURVE('',#29315,#29381,#24485,.T.);
#35120=EDGE_CURVE('',#29382,#29383,#16455,.T.);
#35121=EDGE_CURVE('',#29051,#29383,#21525,.T.);
#35122=EDGE_CURVE('',#29382,#29315,#24486,.T.);
#35123=EDGE_CURVE('',#29384,#29382,#16456,.T.);
#35124=EDGE_CURVE('',#29385,#29384,#21526,.T.);
#35125=EDGE_CURVE('',#29383,#29385,#21527,.T.);
#35126=EDGE_CURVE('',#29316,#29385,#24487,.T.);
#35127=EDGE_CURVE('',#29386,#29387,#16457,.T.);
#35128=EDGE_CURVE('',#29057,#29387,#21528,.T.);
#35129=EDGE_CURVE('',#29386,#29316,#24488,.T.);
#35130=EDGE_CURVE('',#29388,#29386,#16458,.T.);
#35131=EDGE_CURVE('',#29389,#29388,#21529,.T.);
#35132=EDGE_CURVE('',#29387,#29389,#21530,.T.);
#35133=EDGE_CURVE('',#29317,#29389,#24489,.T.);
#35134=EDGE_CURVE('',#29390,#29391,#16459,.T.);
#35135=EDGE_CURVE('',#29063,#29391,#21531,.T.);
#35136=EDGE_CURVE('',#29390,#29317,#24490,.T.);
#35137=EDGE_CURVE('',#29392,#29390,#16460,.T.);
#35138=EDGE_CURVE('',#29393,#29392,#21532,.T.);
#35139=EDGE_CURVE('',#29391,#29393,#21533,.T.);
#35140=EDGE_CURVE('',#29318,#29393,#24491,.T.);
#35141=EDGE_CURVE('',#29394,#29395,#16461,.T.);
#35142=EDGE_CURVE('',#29069,#29395,#21534,.T.);
#35143=EDGE_CURVE('',#29394,#29318,#24492,.T.);
#35144=EDGE_CURVE('',#29396,#29394,#16462,.T.);
#35145=EDGE_CURVE('',#29397,#29396,#21535,.T.);
#35146=EDGE_CURVE('',#29395,#29397,#21536,.T.);
#35147=EDGE_CURVE('',#29319,#29397,#24493,.T.);
#35148=EDGE_CURVE('',#29398,#29399,#16463,.T.);
#35149=EDGE_CURVE('',#29071,#29399,#21537,.T.);
#35150=EDGE_CURVE('',#29398,#29319,#24494,.T.);
#35151=EDGE_CURVE('',#29400,#29398,#16464,.T.);
#35152=EDGE_CURVE('',#29401,#29400,#21538,.T.);
#35153=EDGE_CURVE('',#29399,#29401,#21539,.T.);
#35154=EDGE_CURVE('',#29320,#29401,#24495,.T.);
#35155=EDGE_CURVE('',#29402,#29403,#16465,.T.);
#35156=EDGE_CURVE('',#29077,#29403,#21540,.T.);
#35157=EDGE_CURVE('',#29402,#29320,#24496,.T.);
#35158=EDGE_CURVE('',#29404,#29402,#16466,.T.);
#35159=EDGE_CURVE('',#29405,#29404,#21541,.T.);
#35160=EDGE_CURVE('',#29403,#29405,#21542,.T.);
#35161=EDGE_CURVE('',#29321,#29405,#24497,.T.);
#35162=EDGE_CURVE('',#29406,#29407,#16467,.T.);
#35163=EDGE_CURVE('',#29083,#29407,#21543,.T.);
#35164=EDGE_CURVE('',#29406,#29321,#24498,.T.);
#35165=EDGE_CURVE('',#29408,#29406,#16468,.T.);
#35166=EDGE_CURVE('',#29409,#29408,#21544,.T.);
#35167=EDGE_CURVE('',#29407,#29409,#21545,.T.);
#35168=EDGE_CURVE('',#29322,#29409,#24499,.T.);
#35169=EDGE_CURVE('',#29410,#29411,#16469,.T.);
#35170=EDGE_CURVE('',#29089,#29411,#21546,.T.);
#35171=EDGE_CURVE('',#29410,#29322,#24500,.T.);
#35172=EDGE_CURVE('',#29412,#29410,#16470,.T.);
#35173=EDGE_CURVE('',#29413,#29412,#21547,.T.);
#35174=EDGE_CURVE('',#29411,#29413,#21548,.T.);
#35175=EDGE_CURVE('',#29323,#29413,#24501,.T.);
#35176=EDGE_CURVE('',#29414,#29415,#16471,.T.);
#35177=EDGE_CURVE('',#29095,#29415,#21549,.T.);
#35178=EDGE_CURVE('',#29414,#29323,#24502,.T.);
#35179=EDGE_CURVE('',#29416,#29414,#16472,.T.);
#35180=EDGE_CURVE('',#29417,#29416,#21550,.T.);
#35181=EDGE_CURVE('',#29415,#29417,#21551,.T.);
#35182=EDGE_CURVE('',#29324,#29417,#24503,.T.);
#35183=EDGE_CURVE('',#29418,#29419,#16473,.T.);
#35184=EDGE_CURVE('',#29101,#29419,#21552,.T.);
#35185=EDGE_CURVE('',#29418,#29324,#24504,.T.);
#35186=EDGE_CURVE('',#29420,#29418,#16474,.T.);
#35187=EDGE_CURVE('',#29421,#29420,#21553,.T.);
#35188=EDGE_CURVE('',#29419,#29421,#21554,.T.);
#35189=EDGE_CURVE('',#29325,#29421,#24505,.T.);
#35190=EDGE_CURVE('',#29422,#29423,#16475,.T.);
#35191=EDGE_CURVE('',#29107,#29423,#21555,.T.);
#35192=EDGE_CURVE('',#29422,#29325,#24506,.T.);
#35193=EDGE_CURVE('',#29424,#29422,#16476,.T.);
#35194=EDGE_CURVE('',#29425,#29424,#21556,.T.);
#35195=EDGE_CURVE('',#29423,#29425,#21557,.T.);
#35196=EDGE_CURVE('',#29326,#29425,#24507,.T.);
#35197=EDGE_CURVE('',#29113,#29019,#21558,.T.);
#35198=EDGE_CURVE('',#29018,#29326,#24508,.T.);
#35199=EDGE_CURVE('',#29327,#29021,#24509,.T.);
#35200=EDGE_CURVE('',#29426,#29427,#16477,.T.);
#35201=EDGE_CURVE('',#29119,#29427,#21559,.T.);
#35202=EDGE_CURVE('',#29426,#29327,#24510,.T.);
#35203=EDGE_CURVE('',#29428,#29426,#16478,.T.);
#35204=EDGE_CURVE('',#29429,#29428,#21560,.T.);
#35205=EDGE_CURVE('',#29427,#29429,#21561,.T.);
#35206=EDGE_CURVE('',#29328,#29429,#24511,.T.);
#35207=EDGE_CURVE('',#29430,#29431,#16479,.T.);
#35208=EDGE_CURVE('',#29125,#29431,#21562,.T.);
#35209=EDGE_CURVE('',#29430,#29328,#24512,.T.);
#35210=EDGE_CURVE('',#29432,#29430,#16480,.T.);
#35211=EDGE_CURVE('',#29433,#29432,#21563,.T.);
#35212=EDGE_CURVE('',#29431,#29433,#21564,.T.);
#35213=EDGE_CURVE('',#29329,#29433,#24513,.T.);
#35214=EDGE_CURVE('',#29434,#29435,#16481,.T.);
#35215=EDGE_CURVE('',#29131,#29435,#21565,.T.);
#35216=EDGE_CURVE('',#29434,#29329,#24514,.T.);
#35217=EDGE_CURVE('',#29436,#29434,#16482,.T.);
#35218=EDGE_CURVE('',#29437,#29436,#21566,.T.);
#35219=EDGE_CURVE('',#29435,#29437,#21567,.T.);
#35220=EDGE_CURVE('',#29330,#29437,#24515,.T.);
#35221=EDGE_CURVE('',#29438,#29439,#16483,.T.);
#35222=EDGE_CURVE('',#29137,#29439,#21568,.T.);
#35223=EDGE_CURVE('',#29438,#29330,#24516,.T.);
#35224=EDGE_CURVE('',#29440,#29438,#16484,.T.);
#35225=EDGE_CURVE('',#29441,#29440,#21569,.T.);
#35226=EDGE_CURVE('',#29439,#29441,#21570,.T.);
#35227=EDGE_CURVE('',#29331,#29441,#24517,.T.);
#35228=EDGE_CURVE('',#29442,#29443,#16485,.T.);
#35229=EDGE_CURVE('',#29143,#29443,#21571,.T.);
#35230=EDGE_CURVE('',#29442,#29331,#24518,.T.);
#35231=EDGE_CURVE('',#29444,#29442,#16486,.T.);
#35232=EDGE_CURVE('',#29445,#29444,#21572,.T.);
#35233=EDGE_CURVE('',#29443,#29445,#21573,.T.);
#35234=EDGE_CURVE('',#29332,#29445,#24519,.T.);
#35235=EDGE_CURVE('',#29446,#29447,#16487,.T.);
#35236=EDGE_CURVE('',#29149,#29447,#21574,.T.);
#35237=EDGE_CURVE('',#29446,#29332,#24520,.T.);
#35238=EDGE_CURVE('',#29448,#29446,#16488,.T.);
#35239=EDGE_CURVE('',#29449,#29448,#21575,.T.);
#35240=EDGE_CURVE('',#29447,#29449,#21576,.T.);
#35241=EDGE_CURVE('',#29333,#29449,#24521,.T.);
#35242=EDGE_CURVE('',#29450,#29451,#16489,.T.);
#35243=EDGE_CURVE('',#29155,#29451,#21577,.T.);
#35244=EDGE_CURVE('',#29450,#29333,#24522,.T.);
#35245=EDGE_CURVE('',#29452,#29450,#16490,.T.);
#35246=EDGE_CURVE('',#29453,#29452,#21578,.T.);
#35247=EDGE_CURVE('',#29451,#29453,#21579,.T.);
#35248=EDGE_CURVE('',#29334,#29453,#24523,.T.);
#35249=EDGE_CURVE('',#29454,#29455,#16491,.T.);
#35250=EDGE_CURVE('',#29161,#29455,#21580,.T.);
#35251=EDGE_CURVE('',#29454,#29334,#24524,.T.);
#35252=EDGE_CURVE('',#29456,#29454,#16492,.T.);
#35253=EDGE_CURVE('',#29457,#29456,#21581,.T.);
#35254=EDGE_CURVE('',#29455,#29457,#21582,.T.);
#35255=EDGE_CURVE('',#29335,#29457,#24525,.T.);
#35256=EDGE_CURVE('',#29458,#29459,#16493,.T.);
#35257=EDGE_CURVE('',#29167,#29459,#21583,.T.);
#35258=EDGE_CURVE('',#29458,#29335,#24526,.T.);
#35259=EDGE_CURVE('',#29460,#29458,#16494,.T.);
#35260=EDGE_CURVE('',#29461,#29460,#21584,.T.);
#35261=EDGE_CURVE('',#29459,#29461,#21585,.T.);
#35262=EDGE_CURVE('',#29336,#29461,#24527,.T.);
#35263=EDGE_CURVE('',#29462,#29463,#16495,.T.);
#35264=EDGE_CURVE('',#29173,#29463,#21586,.T.);
#35265=EDGE_CURVE('',#29462,#29336,#24528,.T.);
#35266=EDGE_CURVE('',#29463,#29464,#21587,.T.);
#35267=EDGE_CURVE('',#29337,#29464,#24529,.T.);
#35268=EDGE_CURVE('',#29465,#29462,#16496,.T.);
#35269=EDGE_CURVE('',#29464,#29465,#21588,.T.);
#35270=EDGE_CURVE('',#29466,#29337,#24530,.T.);
#35271=EDGE_CURVE('',#29466,#29467,#16497,.T.);
#35272=EDGE_CURVE('',#29178,#29467,#21589,.T.);
#35273=EDGE_CURVE('',#29467,#29468,#21590,.T.);
#35274=EDGE_CURVE('',#29469,#29466,#16498,.T.);
#35275=EDGE_CURVE('',#29468,#29469,#21591,.T.);
#35276=EDGE_CURVE('',#29338,#29468,#24531,.T.);
#35277=EDGE_CURVE('',#29470,#29471,#16499,.T.);
#35278=EDGE_CURVE('',#29185,#29471,#21592,.T.);
#35279=EDGE_CURVE('',#29470,#29338,#24532,.T.);
#35280=EDGE_CURVE('',#29472,#29470,#16500,.T.);
#35281=EDGE_CURVE('',#29473,#29472,#21593,.T.);
#35282=EDGE_CURVE('',#29471,#29473,#21594,.T.);
#35283=EDGE_CURVE('',#29339,#29473,#24533,.T.);
#35284=EDGE_CURVE('',#29474,#29475,#16501,.T.);
#35285=EDGE_CURVE('',#29191,#29475,#21595,.T.);
#35286=EDGE_CURVE('',#29474,#29339,#24534,.T.);
#35287=EDGE_CURVE('',#29476,#29474,#16502,.T.);
#35288=EDGE_CURVE('',#29477,#29476,#21596,.T.);
#35289=EDGE_CURVE('',#29475,#29477,#21597,.T.);
#35290=EDGE_CURVE('',#29340,#29477,#24535,.T.);
#35291=EDGE_CURVE('',#29478,#29479,#16503,.T.);
#35292=EDGE_CURVE('',#29197,#29479,#21598,.T.);
#35293=EDGE_CURVE('',#29478,#29340,#24536,.T.);
#35294=EDGE_CURVE('',#29480,#29478,#16504,.T.);
#35295=EDGE_CURVE('',#29481,#29480,#21599,.T.);
#35296=EDGE_CURVE('',#29479,#29481,#21600,.T.);
#35297=EDGE_CURVE('',#29312,#29481,#24537,.T.);
#35298=EDGE_CURVE('',#29482,#29341,#24538,.T.);
#35299=EDGE_CURVE('',#29482,#29483,#16505,.T.);
#35300=EDGE_CURVE('',#29194,#29483,#21601,.T.);
#35301=EDGE_CURVE('',#29483,#29484,#16506,.T.);
#35302=EDGE_CURVE('',#29342,#29484,#24539,.T.);
#35303=EDGE_CURVE('',#29485,#29482,#16507,.T.);
#35304=EDGE_CURVE('',#29484,#29485,#4397,.T.);
#35305=EDGE_CURVE('',#29486,#29342,#24540,.T.);
#35306=EDGE_CURVE('',#29486,#29487,#16508,.T.);
#35307=EDGE_CURVE('',#29188,#29487,#21602,.T.);
#35308=EDGE_CURVE('',#29487,#29488,#16509,.T.);
#35309=EDGE_CURVE('',#29343,#29488,#24541,.T.);
#35310=EDGE_CURVE('',#29489,#29486,#16510,.T.);
#35311=EDGE_CURVE('',#29488,#29489,#4398,.T.);
#35312=EDGE_CURVE('',#29490,#29343,#24542,.T.);
#35313=EDGE_CURVE('',#29490,#29491,#16511,.T.);
#35314=EDGE_CURVE('',#29182,#29491,#21603,.T.);
#35315=EDGE_CURVE('',#29491,#29492,#16512,.T.);
#35316=EDGE_CURVE('',#29344,#29492,#24543,.T.);
#35317=EDGE_CURVE('',#29493,#29490,#16513,.T.);
#35318=EDGE_CURVE('',#29492,#29493,#4399,.T.);
#35319=EDGE_CURVE('',#29494,#29344,#24544,.T.);
#35320=EDGE_CURVE('',#29494,#29495,#16514,.T.);
#35321=EDGE_CURVE('',#29176,#29495,#21604,.T.);
#35322=EDGE_CURVE('',#29495,#29496,#16515,.T.);
#35323=EDGE_CURVE('',#29345,#29496,#24545,.T.);
#35324=EDGE_CURVE('',#29497,#29494,#16516,.T.);
#35325=EDGE_CURVE('',#29496,#29497,#4400,.T.);
#35326=EDGE_CURVE('',#29498,#29345,#24546,.T.);
#35327=EDGE_CURVE('',#29498,#29499,#16517,.T.);
#35328=EDGE_CURVE('',#29170,#29499,#21605,.T.);
#35329=EDGE_CURVE('',#29499,#29500,#16518,.T.);
#35330=EDGE_CURVE('',#29346,#29500,#24547,.T.);
#35331=EDGE_CURVE('',#29501,#29498,#16519,.T.);
#35332=EDGE_CURVE('',#29500,#29501,#4401,.T.);
#35333=EDGE_CURVE('',#29502,#29346,#24548,.T.);
#35334=EDGE_CURVE('',#29502,#29503,#16520,.T.);
#35335=EDGE_CURVE('',#29164,#29503,#21606,.T.);
#35336=EDGE_CURVE('',#29503,#29504,#16521,.T.);
#35337=EDGE_CURVE('',#29347,#29504,#24549,.T.);
#35338=EDGE_CURVE('',#29505,#29502,#16522,.T.);
#35339=EDGE_CURVE('',#29504,#29505,#4402,.T.);
#35340=EDGE_CURVE('',#29506,#29347,#24550,.T.);
#35341=EDGE_CURVE('',#29506,#29507,#16523,.T.);
#35342=EDGE_CURVE('',#29158,#29507,#21607,.T.);
#35343=EDGE_CURVE('',#29507,#29508,#16524,.T.);
#35344=EDGE_CURVE('',#29348,#29508,#24551,.T.);
#35345=EDGE_CURVE('',#29509,#29506,#16525,.T.);
#35346=EDGE_CURVE('',#29508,#29509,#4403,.T.);
#35347=EDGE_CURVE('',#29510,#29348,#24552,.T.);
#35348=EDGE_CURVE('',#29510,#29511,#16526,.T.);
#35349=EDGE_CURVE('',#29152,#29511,#21608,.T.);
#35350=EDGE_CURVE('',#29511,#29512,#16527,.T.);
#35351=EDGE_CURVE('',#29349,#29512,#24553,.T.);
#35352=EDGE_CURVE('',#29513,#29510,#16528,.T.);
#35353=EDGE_CURVE('',#29512,#29513,#4404,.T.);
#35354=EDGE_CURVE('',#29514,#29349,#24554,.T.);
#35355=EDGE_CURVE('',#29514,#29515,#16529,.T.);
#35356=EDGE_CURVE('',#29146,#29515,#21609,.T.);
#35357=EDGE_CURVE('',#29515,#29516,#16530,.T.);
#35358=EDGE_CURVE('',#29350,#29516,#24555,.T.);
#35359=EDGE_CURVE('',#29517,#29514,#16531,.T.);
#35360=EDGE_CURVE('',#29516,#29517,#4405,.T.);
#35361=EDGE_CURVE('',#29518,#29350,#24556,.T.);
#35362=EDGE_CURVE('',#29518,#29519,#16532,.T.);
#35363=EDGE_CURVE('',#29140,#29519,#21610,.T.);
#35364=EDGE_CURVE('',#29519,#29520,#16533,.T.);
#35365=EDGE_CURVE('',#29351,#29520,#24557,.T.);
#35366=EDGE_CURVE('',#29521,#29518,#16534,.T.);
#35367=EDGE_CURVE('',#29520,#29521,#4406,.T.);
#35368=EDGE_CURVE('',#29522,#29351,#24558,.T.);
#35369=EDGE_CURVE('',#29522,#29523,#16535,.T.);
#35370=EDGE_CURVE('',#29134,#29523,#21611,.T.);
#35371=EDGE_CURVE('',#29523,#29524,#16536,.T.);
#35372=EDGE_CURVE('',#29352,#29524,#24559,.T.);
#35373=EDGE_CURVE('',#29525,#29522,#16537,.T.);
#35374=EDGE_CURVE('',#29524,#29525,#4407,.T.);
#35375=EDGE_CURVE('',#29526,#29352,#24560,.T.);
#35376=EDGE_CURVE('',#29526,#29527,#16538,.T.);
#35377=EDGE_CURVE('',#29128,#29527,#21612,.T.);
#35378=EDGE_CURVE('',#29527,#29528,#16539,.T.);
#35379=EDGE_CURVE('',#29353,#29528,#24561,.T.);
#35380=EDGE_CURVE('',#29529,#29526,#16540,.T.);
#35381=EDGE_CURVE('',#29528,#29529,#4408,.T.);
#35382=EDGE_CURVE('',#29530,#29353,#24562,.T.);
#35383=EDGE_CURVE('',#29530,#29531,#16541,.T.);
#35384=EDGE_CURVE('',#29122,#29531,#21613,.T.);
#35385=EDGE_CURVE('',#29531,#29532,#16542,.T.);
#35386=EDGE_CURVE('',#29354,#29532,#24563,.T.);
#35387=EDGE_CURVE('',#29533,#29530,#16543,.T.);
#35388=EDGE_CURVE('',#29532,#29533,#4409,.T.);
#35389=EDGE_CURVE('',#29534,#29354,#24564,.T.);
#35390=EDGE_CURVE('',#29534,#29535,#16544,.T.);
#35391=EDGE_CURVE('',#29116,#29535,#21614,.T.);
#35392=EDGE_CURVE('',#29535,#29536,#16545,.T.);
#35393=EDGE_CURVE('',#29355,#29536,#24565,.T.);
#35394=EDGE_CURVE('',#29537,#29534,#16546,.T.);
#35395=EDGE_CURVE('',#29536,#29537,#4410,.T.);
#35396=EDGE_CURVE('',#29538,#29355,#24566,.T.);
#35397=EDGE_CURVE('',#29538,#29539,#16547,.T.);
#35398=EDGE_CURVE('',#29110,#29539,#21615,.T.);
#35399=EDGE_CURVE('',#29539,#29540,#16548,.T.);
#35400=EDGE_CURVE('',#29356,#29540,#24567,.T.);
#35401=EDGE_CURVE('',#29541,#29538,#16549,.T.);
#35402=EDGE_CURVE('',#29540,#29541,#4411,.T.);
#35403=EDGE_CURVE('',#29542,#29356,#24568,.T.);
#35404=EDGE_CURVE('',#29542,#29543,#16550,.T.);
#35405=EDGE_CURVE('',#29104,#29543,#21616,.T.);
#35406=EDGE_CURVE('',#29543,#29544,#16551,.T.);
#35407=EDGE_CURVE('',#29357,#29544,#24569,.T.);
#35408=EDGE_CURVE('',#29545,#29542,#16552,.T.);
#35409=EDGE_CURVE('',#29544,#29545,#4412,.T.);
#35410=EDGE_CURVE('',#29546,#29357,#24570,.T.);
#35411=EDGE_CURVE('',#29546,#29547,#16553,.T.);
#35412=EDGE_CURVE('',#29098,#29547,#21617,.T.);
#35413=EDGE_CURVE('',#29547,#29548,#16554,.T.);
#35414=EDGE_CURVE('',#29358,#29548,#24571,.T.);
#35415=EDGE_CURVE('',#29549,#29546,#16555,.T.);
#35416=EDGE_CURVE('',#29548,#29549,#4413,.T.);
#35417=EDGE_CURVE('',#29550,#29358,#24572,.T.);
#35418=EDGE_CURVE('',#29550,#29551,#16556,.T.);
#35419=EDGE_CURVE('',#29092,#29551,#21618,.T.);
#35420=EDGE_CURVE('',#29551,#29552,#16557,.T.);
#35421=EDGE_CURVE('',#29359,#29552,#24573,.T.);
#35422=EDGE_CURVE('',#29553,#29550,#16558,.T.);
#35423=EDGE_CURVE('',#29552,#29553,#4414,.T.);
#35424=EDGE_CURVE('',#29554,#29359,#24574,.T.);
#35425=EDGE_CURVE('',#29554,#29555,#16559,.T.);
#35426=EDGE_CURVE('',#29086,#29555,#21619,.T.);
#35427=EDGE_CURVE('',#29555,#29556,#16560,.T.);
#35428=EDGE_CURVE('',#29360,#29556,#24575,.T.);
#35429=EDGE_CURVE('',#29557,#29554,#16561,.T.);
#35430=EDGE_CURVE('',#29556,#29557,#4415,.T.);
#35431=EDGE_CURVE('',#29558,#29360,#24576,.T.);
#35432=EDGE_CURVE('',#29558,#29559,#16562,.T.);
#35433=EDGE_CURVE('',#29080,#29559,#21620,.T.);
#35434=EDGE_CURVE('',#29559,#29560,#16563,.T.);
#35435=EDGE_CURVE('',#29361,#29560,#24577,.T.);
#35436=EDGE_CURVE('',#29561,#29558,#16564,.T.);
#35437=EDGE_CURVE('',#29560,#29561,#4416,.T.);
#35438=EDGE_CURVE('',#29562,#29361,#24578,.T.);
#35439=EDGE_CURVE('',#29562,#29563,#16565,.T.);
#35440=EDGE_CURVE('',#29074,#29563,#21621,.T.);
#35441=EDGE_CURVE('',#29563,#29564,#16566,.T.);
#35442=EDGE_CURVE('',#29362,#29564,#24579,.T.);
#35443=EDGE_CURVE('',#29565,#29562,#16567,.T.);
#35444=EDGE_CURVE('',#29564,#29565,#4417,.T.);
#35445=EDGE_CURVE('',#29015,#29362,#24580,.T.);
#35446=EDGE_CURVE('',#29070,#29017,#21622,.T.);
#35447=EDGE_CURVE('',#29363,#29016,#24581,.T.);
#35448=EDGE_CURVE('',#29566,#29363,#24582,.T.);
#35449=EDGE_CURVE('',#29566,#29567,#16568,.T.);
#35450=EDGE_CURVE('',#29066,#29567,#21623,.T.);
#35451=EDGE_CURVE('',#29567,#29568,#16569,.T.);
#35452=EDGE_CURVE('',#29364,#29568,#24583,.T.);
#35453=EDGE_CURVE('',#29569,#29566,#16570,.T.);
#35454=EDGE_CURVE('',#29568,#29569,#4418,.T.);
#35455=EDGE_CURVE('',#29570,#29364,#24584,.T.);
#35456=EDGE_CURVE('',#29570,#29571,#16571,.T.);
#35457=EDGE_CURVE('',#29060,#29571,#21624,.T.);
#35458=EDGE_CURVE('',#29571,#29572,#16572,.T.);
#35459=EDGE_CURVE('',#29365,#29572,#24585,.T.);
#35460=EDGE_CURVE('',#29573,#29570,#16573,.T.);
#35461=EDGE_CURVE('',#29572,#29573,#4419,.T.);
#35462=EDGE_CURVE('',#29574,#29365,#24586,.T.);
#35463=EDGE_CURVE('',#29574,#29575,#16574,.T.);
#35464=EDGE_CURVE('',#29054,#29575,#21625,.T.);
#35465=EDGE_CURVE('',#29575,#29576,#16575,.T.);
#35466=EDGE_CURVE('',#29366,#29576,#24587,.T.);
#35467=EDGE_CURVE('',#29577,#29574,#16576,.T.);
#35468=EDGE_CURVE('',#29576,#29577,#4420,.T.);
#35469=EDGE_CURVE('',#29578,#29366,#24588,.T.);
#35470=EDGE_CURVE('',#29578,#29579,#16577,.T.);
#35471=EDGE_CURVE('',#29048,#29579,#21626,.T.);
#35472=EDGE_CURVE('',#29579,#29580,#16578,.T.);
#35473=EDGE_CURVE('',#29367,#29580,#24589,.T.);
#35474=EDGE_CURVE('',#29581,#29578,#16579,.T.);
#35475=EDGE_CURVE('',#29580,#29581,#4421,.T.);
#35476=EDGE_CURVE('',#29582,#29367,#24590,.T.);
#35477=EDGE_CURVE('',#29582,#29583,#16580,.T.);
#35478=EDGE_CURVE('',#29042,#29583,#21627,.T.);
#35479=EDGE_CURVE('',#29583,#29584,#16581,.T.);
#35480=EDGE_CURVE('',#29368,#29584,#24591,.T.);
#35481=EDGE_CURVE('',#29585,#29582,#16582,.T.);
#35482=EDGE_CURVE('',#29584,#29585,#4422,.T.);
#35483=EDGE_CURVE('',#29586,#29368,#24592,.T.);
#35484=EDGE_CURVE('',#29586,#29587,#16583,.T.);
#35485=EDGE_CURVE('',#29036,#29587,#21628,.T.);
#35486=EDGE_CURVE('',#29587,#29588,#16584,.T.);
#35487=EDGE_CURVE('',#29369,#29588,#24593,.T.);
#35488=EDGE_CURVE('',#29589,#29586,#16585,.T.);
#35489=EDGE_CURVE('',#29588,#29589,#4423,.T.);
#35490=EDGE_CURVE('',#29590,#29369,#24594,.T.);
#35491=EDGE_CURVE('',#29590,#29591,#16586,.T.);
#35492=EDGE_CURVE('',#29033,#29591,#21629,.T.);
#35493=EDGE_CURVE('',#29591,#29592,#16587,.T.);
#35494=EDGE_CURVE('',#29341,#29592,#24595,.T.);
#35495=EDGE_CURVE('',#29593,#29590,#16588,.T.);
#35496=EDGE_CURVE('',#29592,#29593,#4424,.T.);
#35497=EDGE_CURVE('',#29594,#29312,#16589,.T.);
#35498=EDGE_CURVE('',#29372,#29594,#21630,.T.);
#35499=EDGE_CURVE('',#29313,#29594,#21631,.T.);
#35500=EDGE_CURVE('',#29595,#29313,#16590,.T.);
#35501=EDGE_CURVE('',#29376,#29595,#21632,.T.);
#35502=EDGE_CURVE('',#29314,#29595,#21633,.T.);
#35503=EDGE_CURVE('',#29596,#29314,#16591,.T.);
#35504=EDGE_CURVE('',#29380,#29596,#21634,.T.);
#35505=EDGE_CURVE('',#29315,#29596,#21635,.T.);
#35506=EDGE_CURVE('',#29597,#29315,#16592,.T.);
#35507=EDGE_CURVE('',#29384,#29597,#21636,.T.);
#35508=EDGE_CURVE('',#29316,#29597,#21637,.T.);
#35509=EDGE_CURVE('',#29598,#29316,#16593,.T.);
#35510=EDGE_CURVE('',#29388,#29598,#21638,.T.);
#35511=EDGE_CURVE('',#29317,#29598,#21639,.T.);
#35512=EDGE_CURVE('',#29599,#29317,#16594,.T.);
#35513=EDGE_CURVE('',#29392,#29599,#21640,.T.);
#35514=EDGE_CURVE('',#29318,#29599,#21641,.T.);
#35515=EDGE_CURVE('',#29600,#29318,#16595,.T.);
#35516=EDGE_CURVE('',#29396,#29600,#21642,.T.);
#35517=EDGE_CURVE('',#29319,#29600,#21643,.T.);
#35518=EDGE_CURVE('',#29601,#29319,#16596,.T.);
#35519=EDGE_CURVE('',#29400,#29601,#21644,.T.);
#35520=EDGE_CURVE('',#29320,#29601,#21645,.T.);
#35521=EDGE_CURVE('',#29602,#29320,#16597,.T.);
#35522=EDGE_CURVE('',#29404,#29602,#21646,.T.);
#35523=EDGE_CURVE('',#29321,#29602,#21647,.T.);
#35524=EDGE_CURVE('',#29603,#29321,#16598,.T.);
#35525=EDGE_CURVE('',#29408,#29603,#21648,.T.);
#35526=EDGE_CURVE('',#29322,#29603,#21649,.T.);
#35527=EDGE_CURVE('',#29604,#29322,#16599,.T.);
#35528=EDGE_CURVE('',#29412,#29604,#21650,.T.);
#35529=EDGE_CURVE('',#29323,#29604,#21651,.T.);
#35530=EDGE_CURVE('',#29605,#29323,#16600,.T.);
#35531=EDGE_CURVE('',#29416,#29605,#21652,.T.);
#35532=EDGE_CURVE('',#29324,#29605,#21653,.T.);
#35533=EDGE_CURVE('',#29606,#29324,#16601,.T.);
#35534=EDGE_CURVE('',#29420,#29606,#21654,.T.);
#35535=EDGE_CURVE('',#29325,#29606,#21655,.T.);
#35536=EDGE_CURVE('',#29607,#29325,#16602,.T.);
#35537=EDGE_CURVE('',#29424,#29607,#21656,.T.);
#35538=EDGE_CURVE('',#29326,#29607,#21657,.T.);
#35539=EDGE_CURVE('',#29608,#29326,#16603,.T.);
#35540=EDGE_CURVE('',#29020,#29608,#21658,.T.);
#35541=EDGE_CURVE('',#29327,#29608,#21659,.T.);
#35542=EDGE_CURVE('',#29609,#29327,#16604,.T.);
#35543=EDGE_CURVE('',#29428,#29609,#21660,.T.);
#35544=EDGE_CURVE('',#29328,#29609,#21661,.T.);
#35545=EDGE_CURVE('',#29610,#29328,#16605,.T.);
#35546=EDGE_CURVE('',#29432,#29610,#21662,.T.);
#35547=EDGE_CURVE('',#29329,#29610,#21663,.T.);
#35548=EDGE_CURVE('',#29611,#29329,#16606,.T.);
#35549=EDGE_CURVE('',#29436,#29611,#21664,.T.);
#35550=EDGE_CURVE('',#29330,#29611,#21665,.T.);
#35551=EDGE_CURVE('',#29612,#29330,#16607,.T.);
#35552=EDGE_CURVE('',#29440,#29612,#21666,.T.);
#35553=EDGE_CURVE('',#29331,#29612,#21667,.T.);
#35554=EDGE_CURVE('',#29613,#29331,#16608,.T.);
#35555=EDGE_CURVE('',#29444,#29613,#21668,.T.);
#35556=EDGE_CURVE('',#29332,#29613,#21669,.T.);
#35557=EDGE_CURVE('',#29614,#29332,#16609,.T.);
#35558=EDGE_CURVE('',#29448,#29614,#21670,.T.);
#35559=EDGE_CURVE('',#29333,#29614,#21671,.T.);
#35560=EDGE_CURVE('',#29615,#29333,#16610,.T.);
#35561=EDGE_CURVE('',#29452,#29615,#21672,.T.);
#35562=EDGE_CURVE('',#29334,#29615,#21673,.T.);
#35563=EDGE_CURVE('',#29616,#29334,#16611,.T.);
#35564=EDGE_CURVE('',#29456,#29616,#21674,.T.);
#35565=EDGE_CURVE('',#29335,#29616,#21675,.T.);
#35566=EDGE_CURVE('',#29617,#29335,#16612,.T.);
#35567=EDGE_CURVE('',#29460,#29617,#21676,.T.);
#35568=EDGE_CURVE('',#29336,#29617,#21677,.T.);
#35569=EDGE_CURVE('',#29618,#29336,#16613,.T.);
#35570=EDGE_CURVE('',#29465,#29618,#21678,.T.);
#35571=EDGE_CURVE('',#29337,#29618,#21679,.T.);
#35572=EDGE_CURVE('',#29619,#29337,#16614,.T.);
#35573=EDGE_CURVE('',#29469,#29619,#21680,.T.);
#35574=EDGE_CURVE('',#29338,#29619,#21681,.T.);
#35575=EDGE_CURVE('',#29620,#29338,#16615,.T.);
#35576=EDGE_CURVE('',#29472,#29620,#21682,.T.);
#35577=EDGE_CURVE('',#29339,#29620,#21683,.T.);
#35578=EDGE_CURVE('',#29621,#29339,#16616,.T.);
#35579=EDGE_CURVE('',#29476,#29621,#21684,.T.);
#35580=EDGE_CURVE('',#29340,#29621,#21685,.T.);
#35581=EDGE_CURVE('',#29622,#29340,#16617,.T.);
#35582=EDGE_CURVE('',#29480,#29622,#21686,.T.);
#35583=EDGE_CURVE('',#29312,#29622,#21687,.T.);
#35584=EDGE_CURVE('',#29623,#29341,#16618,.T.);
#35585=EDGE_CURVE('',#29485,#29623,#21688,.T.);
#35586=EDGE_CURVE('',#29342,#29623,#21689,.T.);
#35587=EDGE_CURVE('',#29624,#29342,#16619,.T.);
#35588=EDGE_CURVE('',#29489,#29624,#21690,.T.);
#35589=EDGE_CURVE('',#29343,#29624,#21691,.T.);
#35590=EDGE_CURVE('',#29625,#29343,#16620,.T.);
#35591=EDGE_CURVE('',#29493,#29625,#21692,.T.);
#35592=EDGE_CURVE('',#29344,#29625,#21693,.T.);
#35593=EDGE_CURVE('',#29626,#29344,#16621,.T.);
#35594=EDGE_CURVE('',#29497,#29626,#21694,.T.);
#35595=EDGE_CURVE('',#29345,#29626,#21695,.T.);
#35596=EDGE_CURVE('',#29627,#29345,#16622,.T.);
#35597=EDGE_CURVE('',#29501,#29627,#21696,.T.);
#35598=EDGE_CURVE('',#29346,#29627,#21697,.T.);
#35599=EDGE_CURVE('',#29628,#29346,#16623,.T.);
#35600=EDGE_CURVE('',#29505,#29628,#21698,.T.);
#35601=EDGE_CURVE('',#29347,#29628,#21699,.T.);
#35602=EDGE_CURVE('',#29629,#29347,#16624,.T.);
#35603=EDGE_CURVE('',#29509,#29629,#21700,.T.);
#35604=EDGE_CURVE('',#29348,#29629,#21701,.T.);
#35605=EDGE_CURVE('',#29630,#29348,#16625,.T.);
#35606=EDGE_CURVE('',#29513,#29630,#21702,.T.);
#35607=EDGE_CURVE('',#29349,#29630,#21703,.T.);
#35608=EDGE_CURVE('',#29631,#29349,#16626,.T.);
#35609=EDGE_CURVE('',#29517,#29631,#21704,.T.);
#35610=EDGE_CURVE('',#29350,#29631,#21705,.T.);
#35611=EDGE_CURVE('',#29632,#29350,#16627,.T.);
#35612=EDGE_CURVE('',#29521,#29632,#21706,.T.);
#35613=EDGE_CURVE('',#29351,#29632,#21707,.T.);
#35614=EDGE_CURVE('',#29633,#29351,#16628,.T.);
#35615=EDGE_CURVE('',#29525,#29633,#21708,.T.);
#35616=EDGE_CURVE('',#29352,#29633,#21709,.T.);
#35617=EDGE_CURVE('',#29634,#29352,#16629,.T.);
#35618=EDGE_CURVE('',#29529,#29634,#21710,.T.);
#35619=EDGE_CURVE('',#29353,#29634,#21711,.T.);
#35620=EDGE_CURVE('',#29635,#29353,#16630,.T.);
#35621=EDGE_CURVE('',#29533,#29635,#21712,.T.);
#35622=EDGE_CURVE('',#29354,#29635,#21713,.T.);
#35623=EDGE_CURVE('',#29636,#29354,#16631,.T.);
#35624=EDGE_CURVE('',#29537,#29636,#21714,.T.);
#35625=EDGE_CURVE('',#29355,#29636,#21715,.T.);
#35626=EDGE_CURVE('',#29637,#29355,#16632,.T.);
#35627=EDGE_CURVE('',#29541,#29637,#21716,.T.);
#35628=EDGE_CURVE('',#29356,#29637,#21717,.T.);
#35629=EDGE_CURVE('',#29638,#29356,#16633,.T.);
#35630=EDGE_CURVE('',#29545,#29638,#21718,.T.);
#35631=EDGE_CURVE('',#29357,#29638,#21719,.T.);
#35632=EDGE_CURVE('',#29639,#29357,#16634,.T.);
#35633=EDGE_CURVE('',#29549,#29639,#21720,.T.);
#35634=EDGE_CURVE('',#29358,#29639,#21721,.T.);
#35635=EDGE_CURVE('',#29640,#29358,#16635,.T.);
#35636=EDGE_CURVE('',#29553,#29640,#21722,.T.);
#35637=EDGE_CURVE('',#29359,#29640,#21723,.T.);
#35638=EDGE_CURVE('',#29641,#29359,#16636,.T.);
#35639=EDGE_CURVE('',#29557,#29641,#21724,.T.);
#35640=EDGE_CURVE('',#29360,#29641,#21725,.T.);
#35641=EDGE_CURVE('',#29642,#29360,#16637,.T.);
#35642=EDGE_CURVE('',#29561,#29642,#21726,.T.);
#35643=EDGE_CURVE('',#29361,#29642,#21727,.T.);
#35644=EDGE_CURVE('',#29643,#29361,#16638,.T.);
#35645=EDGE_CURVE('',#29565,#29643,#21728,.T.);
#35646=EDGE_CURVE('',#29362,#29643,#21729,.T.);
#35647=EDGE_CURVE('',#29644,#29362,#16639,.T.);
#35648=EDGE_CURVE('',#29014,#29644,#21730,.T.);
#35649=EDGE_CURVE('',#29363,#29644,#21731,.T.);
#35650=EDGE_CURVE('',#29645,#29363,#16640,.T.);
#35651=EDGE_CURVE('',#29569,#29645,#21732,.T.);
#35652=EDGE_CURVE('',#29364,#29645,#21733,.T.);
#35653=EDGE_CURVE('',#29646,#29364,#16641,.T.);
#35654=EDGE_CURVE('',#29573,#29646,#21734,.T.);
#35655=EDGE_CURVE('',#29365,#29646,#21735,.T.);
#35656=EDGE_CURVE('',#29647,#29365,#16642,.T.);
#35657=EDGE_CURVE('',#29577,#29647,#21736,.T.);
#35658=EDGE_CURVE('',#29366,#29647,#21737,.T.);
#35659=EDGE_CURVE('',#29648,#29366,#16643,.T.);
#35660=EDGE_CURVE('',#29581,#29648,#21738,.T.);
#35661=EDGE_CURVE('',#29367,#29648,#21739,.T.);
#35662=EDGE_CURVE('',#29649,#29367,#16644,.T.);
#35663=EDGE_CURVE('',#29585,#29649,#21740,.T.);
#35664=EDGE_CURVE('',#29368,#29649,#21741,.T.);
#35665=EDGE_CURVE('',#29650,#29368,#16645,.T.);
#35666=EDGE_CURVE('',#29589,#29650,#21742,.T.);
#35667=EDGE_CURVE('',#29369,#29650,#21743,.T.);
#35668=EDGE_CURVE('',#29651,#29369,#16646,.T.);
#35669=EDGE_CURVE('',#29593,#29651,#21744,.T.);
#35670=EDGE_CURVE('',#29341,#29651,#21745,.T.);
#35671=EDGE_CURVE('',#29652,#29653,#16647,.T.);
#35672=EDGE_CURVE('',#29594,#29653,#24596,.T.);
#35673=EDGE_CURVE('',#29652,#29312,#21746,.T.);
#35674=EDGE_CURVE('',#29654,#29655,#21747,.T.);
#35675=EDGE_CURVE('',#29313,#29655,#21748,.T.);
#35676=EDGE_CURVE('',#29654,#29594,#24597,.T.);
#35677=EDGE_CURVE('',#29656,#29654,#16648,.T.);
#35678=EDGE_CURVE('',#29657,#29656,#16649,.T.);
#35679=EDGE_CURVE('',#29655,#29657,#16650,.T.);
#35680=EDGE_CURVE('',#29595,#29657,#24598,.T.);
#35681=EDGE_CURVE('',#29658,#29659,#21749,.T.);
#35682=EDGE_CURVE('',#29314,#29659,#21750,.T.);
#35683=EDGE_CURVE('',#29658,#29595,#24599,.T.);
#35684=EDGE_CURVE('',#29660,#29658,#16651,.T.);
#35685=EDGE_CURVE('',#29661,#29660,#16652,.T.);
#35686=EDGE_CURVE('',#29659,#29661,#16653,.T.);
#35687=EDGE_CURVE('',#29596,#29661,#24600,.T.);
#35688=EDGE_CURVE('',#29662,#29663,#21751,.T.);
#35689=EDGE_CURVE('',#29315,#29663,#21752,.T.);
#35690=EDGE_CURVE('',#29662,#29596,#24601,.T.);
#35691=EDGE_CURVE('',#29664,#29662,#16654,.T.);
#35692=EDGE_CURVE('',#29665,#29664,#16655,.T.);
#35693=EDGE_CURVE('',#29663,#29665,#16656,.T.);
#35694=EDGE_CURVE('',#29597,#29665,#24602,.T.);
#35695=EDGE_CURVE('',#29666,#29667,#21753,.T.);
#35696=EDGE_CURVE('',#29316,#29667,#21754,.T.);
#35697=EDGE_CURVE('',#29666,#29597,#24603,.T.);
#35698=EDGE_CURVE('',#29668,#29666,#16657,.T.);
#35699=EDGE_CURVE('',#29669,#29668,#16658,.T.);
#35700=EDGE_CURVE('',#29667,#29669,#16659,.T.);
#35701=EDGE_CURVE('',#29598,#29669,#24604,.T.);
#35702=EDGE_CURVE('',#29670,#29671,#21755,.T.);
#35703=EDGE_CURVE('',#29317,#29671,#21756,.T.);
#35704=EDGE_CURVE('',#29670,#29598,#24605,.T.);
#35705=EDGE_CURVE('',#29672,#29670,#16660,.T.);
#35706=EDGE_CURVE('',#29673,#29672,#16661,.T.);
#35707=EDGE_CURVE('',#29671,#29673,#16662,.T.);
#35708=EDGE_CURVE('',#29599,#29673,#24606,.T.);
#35709=EDGE_CURVE('',#29674,#29675,#21757,.T.);
#35710=EDGE_CURVE('',#29318,#29675,#21758,.T.);
#35711=EDGE_CURVE('',#29674,#29599,#24607,.T.);
#35712=EDGE_CURVE('',#29676,#29674,#16663,.T.);
#35713=EDGE_CURVE('',#29677,#29676,#16664,.T.);
#35714=EDGE_CURVE('',#29675,#29677,#16665,.T.);
#35715=EDGE_CURVE('',#29600,#29677,#24608,.T.);
#35716=EDGE_CURVE('',#29319,#29010,#21759,.T.);
#35717=EDGE_CURVE('',#29012,#29600,#24609,.T.);
#35718=EDGE_CURVE('',#29601,#29011,#24610,.T.);
#35719=EDGE_CURVE('',#29678,#29679,#21760,.T.);
#35720=EDGE_CURVE('',#29320,#29679,#21761,.T.);
#35721=EDGE_CURVE('',#29678,#29601,#24611,.T.);
#35722=EDGE_CURVE('',#29680,#29678,#16666,.T.);
#35723=EDGE_CURVE('',#29681,#29680,#16667,.T.);
#35724=EDGE_CURVE('',#29679,#29681,#16668,.T.);
#35725=EDGE_CURVE('',#29602,#29681,#24612,.T.);
#35726=EDGE_CURVE('',#29682,#29683,#21762,.T.);
#35727=EDGE_CURVE('',#29321,#29683,#21763,.T.);
#35728=EDGE_CURVE('',#29682,#29602,#24613,.T.);
#35729=EDGE_CURVE('',#29684,#29682,#16669,.T.);
#35730=EDGE_CURVE('',#29685,#29684,#16670,.T.);
#35731=EDGE_CURVE('',#29683,#29685,#16671,.T.);
#35732=EDGE_CURVE('',#29603,#29685,#24614,.T.);
#35733=EDGE_CURVE('',#29686,#29687,#21764,.T.);
#35734=EDGE_CURVE('',#29322,#29687,#21765,.T.);
#35735=EDGE_CURVE('',#29686,#29603,#24615,.T.);
#35736=EDGE_CURVE('',#29688,#29686,#16672,.T.);
#35737=EDGE_CURVE('',#29689,#29688,#16673,.T.);
#35738=EDGE_CURVE('',#29687,#29689,#16674,.T.);
#35739=EDGE_CURVE('',#29604,#29689,#24616,.T.);
#35740=EDGE_CURVE('',#29690,#29691,#21766,.T.);
#35741=EDGE_CURVE('',#29323,#29691,#21767,.T.);
#35742=EDGE_CURVE('',#29690,#29604,#24617,.T.);
#35743=EDGE_CURVE('',#29692,#29690,#16675,.T.);
#35744=EDGE_CURVE('',#29693,#29692,#16676,.T.);
#35745=EDGE_CURVE('',#29691,#29693,#16677,.T.);
#35746=EDGE_CURVE('',#29605,#29693,#24618,.T.);
#35747=EDGE_CURVE('',#29694,#29695,#21768,.T.);
#35748=EDGE_CURVE('',#29324,#29695,#21769,.T.);
#35749=EDGE_CURVE('',#29694,#29605,#24619,.T.);
#35750=EDGE_CURVE('',#29696,#29694,#16678,.T.);
#35751=EDGE_CURVE('',#29697,#29696,#16679,.T.);
#35752=EDGE_CURVE('',#29695,#29697,#16680,.T.);
#35753=EDGE_CURVE('',#29606,#29697,#24620,.T.);
#35754=EDGE_CURVE('',#29698,#29699,#21770,.T.);
#35755=EDGE_CURVE('',#29325,#29699,#21771,.T.);
#35756=EDGE_CURVE('',#29698,#29606,#24621,.T.);
#35757=EDGE_CURVE('',#29700,#29698,#16681,.T.);
#35758=EDGE_CURVE('',#29701,#29700,#16682,.T.);
#35759=EDGE_CURVE('',#29699,#29701,#16683,.T.);
#35760=EDGE_CURVE('',#29607,#29701,#24622,.T.);
#35761=EDGE_CURVE('',#29702,#29703,#21772,.T.);
#35762=EDGE_CURVE('',#29326,#29703,#21773,.T.);
#35763=EDGE_CURVE('',#29702,#29607,#24623,.T.);
#35764=EDGE_CURVE('',#29704,#29702,#16684,.T.);
#35765=EDGE_CURVE('',#29705,#29704,#16685,.T.);
#35766=EDGE_CURVE('',#29703,#29705,#16686,.T.);
#35767=EDGE_CURVE('',#29608,#29705,#24624,.T.);
#35768=EDGE_CURVE('',#29706,#29707,#21774,.T.);
#35769=EDGE_CURVE('',#29327,#29707,#21775,.T.);
#35770=EDGE_CURVE('',#29706,#29608,#24625,.T.);
#35771=EDGE_CURVE('',#29708,#29706,#16687,.T.);
#35772=EDGE_CURVE('',#29709,#29708,#16688,.T.);
#35773=EDGE_CURVE('',#29707,#29709,#16689,.T.);
#35774=EDGE_CURVE('',#29609,#29709,#24626,.T.);
#35775=EDGE_CURVE('',#29710,#29711,#21776,.T.);
#35776=EDGE_CURVE('',#29328,#29711,#21777,.T.);
#35777=EDGE_CURVE('',#29710,#29609,#24627,.T.);
#35778=EDGE_CURVE('',#29712,#29710,#16690,.T.);
#35779=EDGE_CURVE('',#29713,#29712,#16691,.T.);
#35780=EDGE_CURVE('',#29711,#29713,#16692,.T.);
#35781=EDGE_CURVE('',#29610,#29713,#24628,.T.);
#35782=EDGE_CURVE('',#29714,#29715,#21778,.T.);
#35783=EDGE_CURVE('',#29329,#29715,#21779,.T.);
#35784=EDGE_CURVE('',#29714,#29610,#24629,.T.);
#35785=EDGE_CURVE('',#29716,#29714,#16693,.T.);
#35786=EDGE_CURVE('',#29717,#29716,#16694,.T.);
#35787=EDGE_CURVE('',#29715,#29717,#16695,.T.);
#35788=EDGE_CURVE('',#29611,#29717,#24630,.T.);
#35789=EDGE_CURVE('',#29718,#29719,#21780,.T.);
#35790=EDGE_CURVE('',#29330,#29719,#21781,.T.);
#35791=EDGE_CURVE('',#29718,#29611,#24631,.T.);
#35792=EDGE_CURVE('',#29720,#29718,#16696,.T.);
#35793=EDGE_CURVE('',#29721,#29720,#16697,.T.);
#35794=EDGE_CURVE('',#29719,#29721,#16698,.T.);
#35795=EDGE_CURVE('',#29612,#29721,#24632,.T.);
#35796=EDGE_CURVE('',#29722,#29723,#21782,.T.);
#35797=EDGE_CURVE('',#29331,#29723,#21783,.T.);
#35798=EDGE_CURVE('',#29722,#29612,#24633,.T.);
#35799=EDGE_CURVE('',#29724,#29722,#16699,.T.);
#35800=EDGE_CURVE('',#29725,#29724,#16700,.T.);
#35801=EDGE_CURVE('',#29723,#29725,#16701,.T.);
#35802=EDGE_CURVE('',#29613,#29725,#24634,.T.);
#35803=EDGE_CURVE('',#29726,#29727,#21784,.T.);
#35804=EDGE_CURVE('',#29332,#29727,#21785,.T.);
#35805=EDGE_CURVE('',#29726,#29613,#24635,.T.);
#35806=EDGE_CURVE('',#29728,#29726,#16702,.T.);
#35807=EDGE_CURVE('',#29729,#29728,#16703,.T.);
#35808=EDGE_CURVE('',#29727,#29729,#16704,.T.);
#35809=EDGE_CURVE('',#29614,#29729,#24636,.T.);
#35810=EDGE_CURVE('',#29730,#29731,#21786,.T.);
#35811=EDGE_CURVE('',#29333,#29731,#21787,.T.);
#35812=EDGE_CURVE('',#29730,#29614,#24637,.T.);
#35813=EDGE_CURVE('',#29732,#29730,#16705,.T.);
#35814=EDGE_CURVE('',#29733,#29732,#16706,.T.);
#35815=EDGE_CURVE('',#29731,#29733,#16707,.T.);
#35816=EDGE_CURVE('',#29615,#29733,#24638,.T.);
#35817=EDGE_CURVE('',#29734,#29735,#21788,.T.);
#35818=EDGE_CURVE('',#29334,#29735,#21789,.T.);
#35819=EDGE_CURVE('',#29734,#29615,#24639,.T.);
#35820=EDGE_CURVE('',#29736,#29734,#16708,.T.);
#35821=EDGE_CURVE('',#29737,#29736,#16709,.T.);
#35822=EDGE_CURVE('',#29735,#29737,#16710,.T.);
#35823=EDGE_CURVE('',#29616,#29737,#24640,.T.);
#35824=EDGE_CURVE('',#29738,#29739,#21790,.T.);
#35825=EDGE_CURVE('',#29335,#29739,#21791,.T.);
#35826=EDGE_CURVE('',#29738,#29616,#24641,.T.);
#35827=EDGE_CURVE('',#29740,#29738,#16711,.T.);
#35828=EDGE_CURVE('',#29741,#29740,#16712,.T.);
#35829=EDGE_CURVE('',#29739,#29741,#16713,.T.);
#35830=EDGE_CURVE('',#29617,#29741,#24642,.T.);
#35831=EDGE_CURVE('',#29742,#29743,#21792,.T.);
#35832=EDGE_CURVE('',#29336,#29743,#21793,.T.);
#35833=EDGE_CURVE('',#29742,#29617,#24643,.T.);
#35834=EDGE_CURVE('',#29743,#29744,#16714,.T.);
#35835=EDGE_CURVE('',#29618,#29744,#24644,.T.);
#35836=EDGE_CURVE('',#29745,#29742,#16715,.T.);
#35837=EDGE_CURVE('',#29744,#29745,#16716,.T.);
#35838=EDGE_CURVE('',#29746,#29618,#24645,.T.);
#35839=EDGE_CURVE('',#29746,#29747,#21794,.T.);
#35840=EDGE_CURVE('',#29337,#29747,#21795,.T.);
#35841=EDGE_CURVE('',#29747,#29748,#16717,.T.);
#35842=EDGE_CURVE('',#29749,#29746,#16718,.T.);
#35843=EDGE_CURVE('',#29748,#29749,#16719,.T.);
#35844=EDGE_CURVE('',#29619,#29748,#24646,.T.);
#35845=EDGE_CURVE('',#29750,#29751,#21796,.T.);
#35846=EDGE_CURVE('',#29338,#29751,#21797,.T.);
#35847=EDGE_CURVE('',#29750,#29619,#24647,.T.);
#35848=EDGE_CURVE('',#29752,#29750,#16720,.T.);
#35849=EDGE_CURVE('',#29753,#29752,#16721,.T.);
#35850=EDGE_CURVE('',#29751,#29753,#16722,.T.);
#35851=EDGE_CURVE('',#29620,#29753,#24648,.T.);
#35852=EDGE_CURVE('',#29754,#29755,#21798,.T.);
#35853=EDGE_CURVE('',#29339,#29755,#21799,.T.);
#35854=EDGE_CURVE('',#29754,#29620,#24649,.T.);
#35855=EDGE_CURVE('',#29756,#29754,#16723,.T.);
#35856=EDGE_CURVE('',#29757,#29756,#16724,.T.);
#35857=EDGE_CURVE('',#29755,#29757,#16725,.T.);
#35858=EDGE_CURVE('',#29621,#29757,#24650,.T.);
#35859=EDGE_CURVE('',#29758,#29759,#21800,.T.);
#35860=EDGE_CURVE('',#29340,#29759,#21801,.T.);
#35861=EDGE_CURVE('',#29758,#29621,#24651,.T.);
#35862=EDGE_CURVE('',#29760,#29758,#16726,.T.);
#35863=EDGE_CURVE('',#29761,#29760,#16727,.T.);
#35864=EDGE_CURVE('',#29759,#29761,#16728,.T.);
#35865=EDGE_CURVE('',#29622,#29761,#24652,.T.);
#35866=EDGE_CURVE('',#29762,#29763,#16729,.T.);
#35867=EDGE_CURVE('',#29653,#29762,#16730,.T.);
#35868=EDGE_CURVE('',#29763,#29652,#21802,.T.);
#35869=EDGE_CURVE('',#29763,#29622,#24653,.T.);
#35870=EDGE_CURVE('',#29764,#29341,#21803,.T.);
#35871=EDGE_CURVE('',#29764,#29765,#16731,.T.);
#35872=EDGE_CURVE('',#29623,#29765,#24654,.T.);
#35873=EDGE_CURVE('',#29766,#29623,#24655,.T.);
#35874=EDGE_CURVE('',#29766,#29767,#21804,.T.);
#35875=EDGE_CURVE('',#29342,#29767,#21805,.T.);
#35876=EDGE_CURVE('',#29767,#29768,#16732,.T.);
#35877=EDGE_CURVE('',#29624,#29768,#24656,.T.);
#35878=EDGE_CURVE('',#29769,#29766,#16733,.T.);
#35879=EDGE_CURVE('',#29768,#29769,#16734,.T.);
#35880=EDGE_CURVE('',#29770,#29624,#24657,.T.);
#35881=EDGE_CURVE('',#29770,#29771,#21806,.T.);
#35882=EDGE_CURVE('',#29343,#29771,#21807,.T.);
#35883=EDGE_CURVE('',#29771,#29772,#16735,.T.);
#35884=EDGE_CURVE('',#29625,#29772,#24658,.T.);
#35885=EDGE_CURVE('',#29773,#29770,#16736,.T.);
#35886=EDGE_CURVE('',#29772,#29773,#16737,.T.);
#35887=EDGE_CURVE('',#29774,#29625,#24659,.T.);
#35888=EDGE_CURVE('',#29774,#29775,#21808,.T.);
#35889=EDGE_CURVE('',#29344,#29775,#21809,.T.);
#35890=EDGE_CURVE('',#29775,#29776,#16738,.T.);
#35891=EDGE_CURVE('',#29626,#29776,#24660,.T.);
#35892=EDGE_CURVE('',#29777,#29774,#16739,.T.);
#35893=EDGE_CURVE('',#29776,#29777,#16740,.T.);
#35894=EDGE_CURVE('',#29778,#29626,#24661,.T.);
#35895=EDGE_CURVE('',#29778,#29779,#21810,.T.);
#35896=EDGE_CURVE('',#29345,#29779,#21811,.T.);
#35897=EDGE_CURVE('',#29779,#29780,#16741,.T.);
#35898=EDGE_CURVE('',#29627,#29780,#24662,.T.);
#35899=EDGE_CURVE('',#29781,#29778,#16742,.T.);
#35900=EDGE_CURVE('',#29780,#29781,#16743,.T.);
#35901=EDGE_CURVE('',#29782,#29627,#24663,.T.);
#35902=EDGE_CURVE('',#29782,#29783,#21812,.T.);
#35903=EDGE_CURVE('',#29346,#29783,#21813,.T.);
#35904=EDGE_CURVE('',#29783,#29784,#16744,.T.);
#35905=EDGE_CURVE('',#29628,#29784,#24664,.T.);
#35906=EDGE_CURVE('',#29785,#29782,#16745,.T.);
#35907=EDGE_CURVE('',#29784,#29785,#16746,.T.);
#35908=EDGE_CURVE('',#29786,#29628,#24665,.T.);
#35909=EDGE_CURVE('',#29786,#29787,#21814,.T.);
#35910=EDGE_CURVE('',#29347,#29787,#21815,.T.);
#35911=EDGE_CURVE('',#29787,#29788,#16747,.T.);
#35912=EDGE_CURVE('',#29629,#29788,#24666,.T.);
#35913=EDGE_CURVE('',#29789,#29786,#16748,.T.);
#35914=EDGE_CURVE('',#29788,#29789,#16749,.T.);
#35915=EDGE_CURVE('',#29790,#29629,#24667,.T.);
#35916=EDGE_CURVE('',#29790,#29791,#21816,.T.);
#35917=EDGE_CURVE('',#29348,#29791,#21817,.T.);
#35918=EDGE_CURVE('',#29791,#29792,#16750,.T.);
#35919=EDGE_CURVE('',#29630,#29792,#24668,.T.);
#35920=EDGE_CURVE('',#29793,#29790,#16751,.T.);
#35921=EDGE_CURVE('',#29792,#29793,#16752,.T.);
#35922=EDGE_CURVE('',#29794,#29630,#24669,.T.);
#35923=EDGE_CURVE('',#29794,#29795,#21818,.T.);
#35924=EDGE_CURVE('',#29349,#29795,#21819,.T.);
#35925=EDGE_CURVE('',#29795,#29796,#16753,.T.);
#35926=EDGE_CURVE('',#29631,#29796,#24670,.T.);
#35927=EDGE_CURVE('',#29797,#29794,#16754,.T.);
#35928=EDGE_CURVE('',#29796,#29797,#16755,.T.);
#35929=EDGE_CURVE('',#29798,#29631,#24671,.T.);
#35930=EDGE_CURVE('',#29798,#29799,#21820,.T.);
#35931=EDGE_CURVE('',#29350,#29799,#21821,.T.);
#35932=EDGE_CURVE('',#29799,#29800,#16756,.T.);
#35933=EDGE_CURVE('',#29632,#29800,#24672,.T.);
#35934=EDGE_CURVE('',#29801,#29798,#16757,.T.);
#35935=EDGE_CURVE('',#29800,#29801,#16758,.T.);
#35936=EDGE_CURVE('',#29802,#29632,#24673,.T.);
#35937=EDGE_CURVE('',#29802,#29803,#21822,.T.);
#35938=EDGE_CURVE('',#29351,#29803,#21823,.T.);
#35939=EDGE_CURVE('',#29803,#29804,#16759,.T.);
#35940=EDGE_CURVE('',#29633,#29804,#24674,.T.);
#35941=EDGE_CURVE('',#29805,#29802,#16760,.T.);
#35942=EDGE_CURVE('',#29804,#29805,#16761,.T.);
#35943=EDGE_CURVE('',#29806,#29633,#24675,.T.);
#35944=EDGE_CURVE('',#29806,#29807,#21824,.T.);
#35945=EDGE_CURVE('',#29352,#29807,#21825,.T.);
#35946=EDGE_CURVE('',#29807,#29808,#16762,.T.);
#35947=EDGE_CURVE('',#29634,#29808,#24676,.T.);
#35948=EDGE_CURVE('',#29809,#29806,#16763,.T.);
#35949=EDGE_CURVE('',#29808,#29809,#16764,.T.);
#35950=EDGE_CURVE('',#29810,#29634,#24677,.T.);
#35951=EDGE_CURVE('',#29810,#29811,#21826,.T.);
#35952=EDGE_CURVE('',#29353,#29811,#21827,.T.);
#35953=EDGE_CURVE('',#29811,#29812,#16765,.T.);
#35954=EDGE_CURVE('',#29635,#29812,#24678,.T.);
#35955=EDGE_CURVE('',#29813,#29810,#16766,.T.);
#35956=EDGE_CURVE('',#29812,#29813,#16767,.T.);
#35957=EDGE_CURVE('',#29814,#29635,#24679,.T.);
#35958=EDGE_CURVE('',#29814,#29815,#21828,.T.);
#35959=EDGE_CURVE('',#29354,#29815,#21829,.T.);
#35960=EDGE_CURVE('',#29815,#29816,#16768,.T.);
#35961=EDGE_CURVE('',#29636,#29816,#24680,.T.);
#35962=EDGE_CURVE('',#29817,#29814,#16769,.T.);
#35963=EDGE_CURVE('',#29816,#29817,#16770,.T.);
#35964=EDGE_CURVE('',#29009,#29636,#24681,.T.);
#35965=EDGE_CURVE('',#29355,#29008,#21830,.T.);
#35966=EDGE_CURVE('',#29637,#29006,#24682,.T.);
#35967=EDGE_CURVE('',#29818,#29637,#24683,.T.);
#35968=EDGE_CURVE('',#29818,#29819,#21831,.T.);
#35969=EDGE_CURVE('',#29356,#29819,#21832,.T.);
#35970=EDGE_CURVE('',#29819,#29820,#16771,.T.);
#35971=EDGE_CURVE('',#29638,#29820,#24684,.T.);
#35972=EDGE_CURVE('',#29821,#29818,#16772,.T.);
#35973=EDGE_CURVE('',#29820,#29821,#16773,.T.);
#35974=EDGE_CURVE('',#29822,#29638,#24685,.T.);
#35975=EDGE_CURVE('',#29822,#29823,#21833,.T.);
#35976=EDGE_CURVE('',#29357,#29823,#21834,.T.);
#35977=EDGE_CURVE('',#29823,#29824,#16774,.T.);
#35978=EDGE_CURVE('',#29639,#29824,#24686,.T.);
#35979=EDGE_CURVE('',#29825,#29822,#16775,.T.);
#35980=EDGE_CURVE('',#29824,#29825,#16776,.T.);
#35981=EDGE_CURVE('',#29826,#29639,#24687,.T.);
#35982=EDGE_CURVE('',#29826,#29827,#21835,.T.);
#35983=EDGE_CURVE('',#29358,#29827,#21836,.T.);
#35984=EDGE_CURVE('',#29827,#29828,#16777,.T.);
#35985=EDGE_CURVE('',#29640,#29828,#24688,.T.);
#35986=EDGE_CURVE('',#29829,#29826,#16778,.T.);
#35987=EDGE_CURVE('',#29828,#29829,#16779,.T.);
#35988=EDGE_CURVE('',#29830,#29640,#24689,.T.);
#35989=EDGE_CURVE('',#29830,#29831,#21837,.T.);
#35990=EDGE_CURVE('',#29359,#29831,#21838,.T.);
#35991=EDGE_CURVE('',#29831,#29832,#16780,.T.);
#35992=EDGE_CURVE('',#29641,#29832,#24690,.T.);
#35993=EDGE_CURVE('',#29833,#29830,#16781,.T.);
#35994=EDGE_CURVE('',#29832,#29833,#16782,.T.);
#35995=EDGE_CURVE('',#29834,#29641,#24691,.T.);
#35996=EDGE_CURVE('',#29834,#29835,#21839,.T.);
#35997=EDGE_CURVE('',#29360,#29835,#21840,.T.);
#35998=EDGE_CURVE('',#29835,#29836,#16783,.T.);
#35999=EDGE_CURVE('',#29642,#29836,#24692,.T.);
#36000=EDGE_CURVE('',#29837,#29834,#16784,.T.);
#36001=EDGE_CURVE('',#29836,#29837,#16785,.T.);
#36002=EDGE_CURVE('',#29838,#29642,#24693,.T.);
#36003=EDGE_CURVE('',#29838,#29839,#21841,.T.);
#36004=EDGE_CURVE('',#29361,#29839,#21842,.T.);
#36005=EDGE_CURVE('',#29839,#29840,#16786,.T.);
#36006=EDGE_CURVE('',#29643,#29840,#24694,.T.);
#36007=EDGE_CURVE('',#29841,#29838,#16787,.T.);
#36008=EDGE_CURVE('',#29840,#29841,#16788,.T.);
#36009=EDGE_CURVE('',#29842,#29643,#24695,.T.);
#36010=EDGE_CURVE('',#29842,#29843,#21843,.T.);
#36011=EDGE_CURVE('',#29362,#29843,#21844,.T.);
#36012=EDGE_CURVE('',#29843,#29844,#16789,.T.);
#36013=EDGE_CURVE('',#29644,#29844,#24696,.T.);
#36014=EDGE_CURVE('',#29845,#29842,#16790,.T.);
#36015=EDGE_CURVE('',#29844,#29845,#16791,.T.);
#36016=EDGE_CURVE('',#29846,#29644,#24697,.T.);
#36017=EDGE_CURVE('',#29846,#29847,#21845,.T.);
#36018=EDGE_CURVE('',#29363,#29847,#21846,.T.);
#36019=EDGE_CURVE('',#29847,#29848,#16792,.T.);
#36020=EDGE_CURVE('',#29645,#29848,#24698,.T.);
#36021=EDGE_CURVE('',#29849,#29846,#16793,.T.);
#36022=EDGE_CURVE('',#29848,#29849,#16794,.T.);
#36023=EDGE_CURVE('',#29850,#29645,#24699,.T.);
#36024=EDGE_CURVE('',#29850,#29851,#21847,.T.);
#36025=EDGE_CURVE('',#29364,#29851,#21848,.T.);
#36026=EDGE_CURVE('',#29851,#29852,#16795,.T.);
#36027=EDGE_CURVE('',#29646,#29852,#24700,.T.);
#36028=EDGE_CURVE('',#29853,#29850,#16796,.T.);
#36029=EDGE_CURVE('',#29852,#29853,#16797,.T.);
#36030=EDGE_CURVE('',#29854,#29646,#24701,.T.);
#36031=EDGE_CURVE('',#29854,#29855,#21849,.T.);
#36032=EDGE_CURVE('',#29365,#29855,#21850,.T.);
#36033=EDGE_CURVE('',#29855,#29856,#16798,.T.);
#36034=EDGE_CURVE('',#29647,#29856,#24702,.T.);
#36035=EDGE_CURVE('',#29857,#29854,#16799,.T.);
#36036=EDGE_CURVE('',#29856,#29857,#16800,.T.);
#36037=EDGE_CURVE('',#29858,#29647,#24703,.T.);
#36038=EDGE_CURVE('',#29858,#29859,#21851,.T.);
#36039=EDGE_CURVE('',#29366,#29859,#21852,.T.);
#36040=EDGE_CURVE('',#29859,#29860,#16801,.T.);
#36041=EDGE_CURVE('',#29648,#29860,#24704,.T.);
#36042=EDGE_CURVE('',#29861,#29858,#16802,.T.);
#36043=EDGE_CURVE('',#29860,#29861,#16803,.T.);
#36044=EDGE_CURVE('',#29862,#29648,#24705,.T.);
#36045=EDGE_CURVE('',#29862,#29863,#21853,.T.);
#36046=EDGE_CURVE('',#29367,#29863,#21854,.T.);
#36047=EDGE_CURVE('',#29863,#29864,#16804,.T.);
#36048=EDGE_CURVE('',#29649,#29864,#24706,.T.);
#36049=EDGE_CURVE('',#29865,#29862,#16805,.T.);
#36050=EDGE_CURVE('',#29864,#29865,#16806,.T.);
#36051=EDGE_CURVE('',#29866,#29649,#24707,.T.);
#36052=EDGE_CURVE('',#29866,#29867,#21855,.T.);
#36053=EDGE_CURVE('',#29368,#29867,#21856,.T.);
#36054=EDGE_CURVE('',#29867,#29868,#16807,.T.);
#36055=EDGE_CURVE('',#29650,#29868,#24708,.T.);
#36056=EDGE_CURVE('',#29869,#29866,#16808,.T.);
#36057=EDGE_CURVE('',#29868,#29869,#16809,.T.);
#36058=EDGE_CURVE('',#29870,#29650,#24709,.T.);
#36059=EDGE_CURVE('',#29870,#29871,#21857,.T.);
#36060=EDGE_CURVE('',#29369,#29871,#21858,.T.);
#36061=EDGE_CURVE('',#29871,#29872,#16810,.T.);
#36062=EDGE_CURVE('',#29651,#29872,#24710,.T.);
#36063=EDGE_CURVE('',#29873,#29870,#16811,.T.);
#36064=EDGE_CURVE('',#29872,#29873,#16812,.T.);
#36065=EDGE_CURVE('',#29874,#29764,#21859,.T.);
#36066=EDGE_CURVE('',#29875,#29874,#16813,.T.);
#36067=EDGE_CURVE('',#29765,#29875,#16814,.T.);
#36068=EDGE_CURVE('',#29874,#29651,#24711,.T.);
#36069=EDGE_CURVE('',#29594,#29876,#16815,.T.);
#36070=EDGE_CURVE('',#29876,#29762,#21860,.T.);
#36071=EDGE_CURVE('',#29877,#29594,#16816,.T.);
#36072=EDGE_CURVE('',#29656,#29877,#21861,.T.);
#36073=EDGE_CURVE('',#29595,#29877,#16817,.T.);
#36074=EDGE_CURVE('',#29878,#29595,#16818,.T.);
#36075=EDGE_CURVE('',#29660,#29878,#21862,.T.);
#36076=EDGE_CURVE('',#29596,#29878,#16819,.T.);
#36077=EDGE_CURVE('',#29879,#29596,#16820,.T.);
#36078=EDGE_CURVE('',#29664,#29879,#21863,.T.);
#36079=EDGE_CURVE('',#29597,#29879,#16821,.T.);
#36080=EDGE_CURVE('',#29880,#29597,#16822,.T.);
#36081=EDGE_CURVE('',#29668,#29880,#21864,.T.);
#36082=EDGE_CURVE('',#29598,#29880,#16823,.T.);
#36083=EDGE_CURVE('',#29881,#29598,#16824,.T.);
#36084=EDGE_CURVE('',#29672,#29881,#21865,.T.);
#36085=EDGE_CURVE('',#29599,#29881,#16825,.T.);
#36086=EDGE_CURVE('',#29882,#29599,#16826,.T.);
#36087=EDGE_CURVE('',#29676,#29882,#21866,.T.);
#36088=EDGE_CURVE('',#29600,#29882,#16827,.T.);
#36089=EDGE_CURVE('',#29883,#29600,#16828,.T.);
#36090=EDGE_CURVE('',#29013,#29883,#21867,.T.);
#36091=EDGE_CURVE('',#29601,#29883,#16829,.T.);
#36092=EDGE_CURVE('',#29884,#29601,#16830,.T.);
#36093=EDGE_CURVE('',#29680,#29884,#21868,.T.);
#36094=EDGE_CURVE('',#29602,#29884,#16831,.T.);
#36095=EDGE_CURVE('',#29885,#29602,#16832,.T.);
#36096=EDGE_CURVE('',#29684,#29885,#21869,.T.);
#36097=EDGE_CURVE('',#29603,#29885,#16833,.T.);
#36098=EDGE_CURVE('',#29886,#29603,#16834,.T.);
#36099=EDGE_CURVE('',#29688,#29886,#21870,.T.);
#36100=EDGE_CURVE('',#29604,#29886,#16835,.T.);
#36101=EDGE_CURVE('',#29887,#29604,#16836,.T.);
#36102=EDGE_CURVE('',#29692,#29887,#21871,.T.);
#36103=EDGE_CURVE('',#29605,#29887,#16837,.T.);
#36104=EDGE_CURVE('',#29888,#29605,#16838,.T.);
#36105=EDGE_CURVE('',#29696,#29888,#21872,.T.);
#36106=EDGE_CURVE('',#29606,#29888,#16839,.T.);
#36107=EDGE_CURVE('',#29889,#29606,#16840,.T.);
#36108=EDGE_CURVE('',#29700,#29889,#21873,.T.);
#36109=EDGE_CURVE('',#29607,#29889,#16841,.T.);
#36110=EDGE_CURVE('',#29890,#29607,#16842,.T.);
#36111=EDGE_CURVE('',#29704,#29890,#21874,.T.);
#36112=EDGE_CURVE('',#29608,#29890,#16843,.T.);
#36113=EDGE_CURVE('',#29891,#29608,#16844,.T.);
#36114=EDGE_CURVE('',#29708,#29891,#21875,.T.);
#36115=EDGE_CURVE('',#29609,#29891,#16845,.T.);
#36116=EDGE_CURVE('',#29892,#29609,#16846,.T.);
#36117=EDGE_CURVE('',#29712,#29892,#21876,.T.);
#36118=EDGE_CURVE('',#29610,#29892,#16847,.T.);
#36119=EDGE_CURVE('',#29893,#29610,#16848,.T.);
#36120=EDGE_CURVE('',#29716,#29893,#21877,.T.);
#36121=EDGE_CURVE('',#29611,#29893,#16849,.T.);
#36122=EDGE_CURVE('',#29894,#29611,#16850,.T.);
#36123=EDGE_CURVE('',#29720,#29894,#21878,.T.);
#36124=EDGE_CURVE('',#29612,#29894,#16851,.T.);
#36125=EDGE_CURVE('',#29895,#29612,#16852,.T.);
#36126=EDGE_CURVE('',#29724,#29895,#21879,.T.);
#36127=EDGE_CURVE('',#29613,#29895,#16853,.T.);
#36128=EDGE_CURVE('',#29896,#29613,#16854,.T.);
#36129=EDGE_CURVE('',#29728,#29896,#21880,.T.);
#36130=EDGE_CURVE('',#29614,#29896,#16855,.T.);
#36131=EDGE_CURVE('',#29897,#29614,#16856,.T.);
#36132=EDGE_CURVE('',#29732,#29897,#21881,.T.);
#36133=EDGE_CURVE('',#29615,#29897,#16857,.T.);
#36134=EDGE_CURVE('',#29898,#29615,#16858,.T.);
#36135=EDGE_CURVE('',#29736,#29898,#21882,.T.);
#36136=EDGE_CURVE('',#29616,#29898,#16859,.T.);
#36137=EDGE_CURVE('',#29899,#29616,#16860,.T.);
#36138=EDGE_CURVE('',#29740,#29899,#21883,.T.);
#36139=EDGE_CURVE('',#29617,#29899,#16861,.T.);
#36140=EDGE_CURVE('',#29900,#29617,#16862,.T.);
#36141=EDGE_CURVE('',#29745,#29900,#21884,.T.);
#36142=EDGE_CURVE('',#29618,#29900,#16863,.T.);
#36143=EDGE_CURVE('',#29901,#29618,#16864,.T.);
#36144=EDGE_CURVE('',#29749,#29901,#21885,.T.);
#36145=EDGE_CURVE('',#29619,#29901,#16865,.T.);
#36146=EDGE_CURVE('',#29902,#29619,#16866,.T.);
#36147=EDGE_CURVE('',#29752,#29902,#21886,.T.);
#36148=EDGE_CURVE('',#29620,#29902,#16867,.T.);
#36149=EDGE_CURVE('',#29903,#29620,#16868,.T.);
#36150=EDGE_CURVE('',#29756,#29903,#21887,.T.);
#36151=EDGE_CURVE('',#29621,#29903,#16869,.T.);
#36152=EDGE_CURVE('',#29904,#29621,#16870,.T.);
#36153=EDGE_CURVE('',#29760,#29904,#21888,.T.);
#36154=EDGE_CURVE('',#29622,#29904,#16871,.T.);
#36155=EDGE_CURVE('',#29876,#29622,#16872,.T.);
#36156=EDGE_CURVE('',#29905,#29875,#21889,.T.);
#36157=EDGE_CURVE('',#29623,#29905,#16873,.T.);
#36158=EDGE_CURVE('',#29906,#29623,#21890,.T.);
#36159=EDGE_CURVE('',#29769,#29906,#21891,.T.);
#36160=EDGE_CURVE('',#29624,#29906,#16874,.T.);
#36161=EDGE_CURVE('',#29907,#29624,#21892,.T.);
#36162=EDGE_CURVE('',#29773,#29907,#21893,.T.);
#36163=EDGE_CURVE('',#29625,#29907,#16875,.T.);
#36164=EDGE_CURVE('',#29908,#29625,#21894,.T.);
#36165=EDGE_CURVE('',#29777,#29908,#21895,.T.);
#36166=EDGE_CURVE('',#29626,#29908,#16876,.T.);
#36167=EDGE_CURVE('',#29909,#29626,#21896,.T.);
#36168=EDGE_CURVE('',#29781,#29909,#21897,.T.);
#36169=EDGE_CURVE('',#29627,#29909,#16877,.T.);
#36170=EDGE_CURVE('',#29910,#29627,#21898,.T.);
#36171=EDGE_CURVE('',#29785,#29910,#21899,.T.);
#36172=EDGE_CURVE('',#29628,#29910,#16878,.T.);
#36173=EDGE_CURVE('',#29911,#29628,#21900,.T.);
#36174=EDGE_CURVE('',#29789,#29911,#21901,.T.);
#36175=EDGE_CURVE('',#29629,#29911,#16879,.T.);
#36176=EDGE_CURVE('',#29912,#29629,#21902,.T.);
#36177=EDGE_CURVE('',#29793,#29912,#21903,.T.);
#36178=EDGE_CURVE('',#29630,#29912,#16880,.T.);
#36179=EDGE_CURVE('',#29913,#29630,#21904,.T.);
#36180=EDGE_CURVE('',#29797,#29913,#21905,.T.);
#36181=EDGE_CURVE('',#29631,#29913,#16881,.T.);
#36182=EDGE_CURVE('',#29914,#29631,#21906,.T.);
#36183=EDGE_CURVE('',#29801,#29914,#21907,.T.);
#36184=EDGE_CURVE('',#29632,#29914,#16882,.T.);
#36185=EDGE_CURVE('',#29915,#29632,#21908,.T.);
#36186=EDGE_CURVE('',#29805,#29915,#21909,.T.);
#36187=EDGE_CURVE('',#29633,#29915,#16883,.T.);
#36188=EDGE_CURVE('',#29916,#29633,#21910,.T.);
#36189=EDGE_CURVE('',#29809,#29916,#21911,.T.);
#36190=EDGE_CURVE('',#29634,#29916,#16884,.T.);
#36191=EDGE_CURVE('',#29917,#29634,#21912,.T.);
#36192=EDGE_CURVE('',#29813,#29917,#21913,.T.);
#36193=EDGE_CURVE('',#29635,#29917,#16885,.T.);
#36194=EDGE_CURVE('',#29918,#29635,#21914,.T.);
#36195=EDGE_CURVE('',#29817,#29918,#21915,.T.);
#36196=EDGE_CURVE('',#29636,#29918,#16886,.T.);
#36197=EDGE_CURVE('',#29919,#29636,#21916,.T.);
#36198=EDGE_CURVE('',#29007,#29919,#21917,.T.);
#36199=EDGE_CURVE('',#29637,#29919,#16887,.T.);
#36200=EDGE_CURVE('',#29920,#29637,#21918,.T.);
#36201=EDGE_CURVE('',#29821,#29920,#21919,.T.);
#36202=EDGE_CURVE('',#29638,#29920,#16888,.T.);
#36203=EDGE_CURVE('',#29921,#29638,#21920,.T.);
#36204=EDGE_CURVE('',#29825,#29921,#21921,.T.);
#36205=EDGE_CURVE('',#29639,#29921,#16889,.T.);
#36206=EDGE_CURVE('',#29922,#29639,#21922,.T.);
#36207=EDGE_CURVE('',#29829,#29922,#21923,.T.);
#36208=EDGE_CURVE('',#29640,#29922,#16890,.T.);
#36209=EDGE_CURVE('',#29923,#29640,#21924,.T.);
#36210=EDGE_CURVE('',#29833,#29923,#21925,.T.);
#36211=EDGE_CURVE('',#29641,#29923,#16891,.T.);
#36212=EDGE_CURVE('',#29924,#29641,#21926,.T.);
#36213=EDGE_CURVE('',#29837,#29924,#21927,.T.);
#36214=EDGE_CURVE('',#29642,#29924,#16892,.T.);
#36215=EDGE_CURVE('',#29925,#29642,#21928,.T.);
#36216=EDGE_CURVE('',#29841,#29925,#21929,.T.);
#36217=EDGE_CURVE('',#29643,#29925,#16893,.T.);
#36218=EDGE_CURVE('',#29926,#29643,#21930,.T.);
#36219=EDGE_CURVE('',#29845,#29926,#21931,.T.);
#36220=EDGE_CURVE('',#29644,#29926,#16894,.T.);
#36221=EDGE_CURVE('',#29927,#29644,#21932,.T.);
#36222=EDGE_CURVE('',#29849,#29927,#21933,.T.);
#36223=EDGE_CURVE('',#29645,#29927,#16895,.T.);
#36224=EDGE_CURVE('',#29928,#29645,#21934,.T.);
#36225=EDGE_CURVE('',#29853,#29928,#21935,.T.);
#36226=EDGE_CURVE('',#29646,#29928,#16896,.T.);
#36227=EDGE_CURVE('',#29929,#29646,#21936,.T.);
#36228=EDGE_CURVE('',#29857,#29929,#21937,.T.);
#36229=EDGE_CURVE('',#29647,#29929,#16897,.T.);
#36230=EDGE_CURVE('',#29930,#29647,#21938,.T.);
#36231=EDGE_CURVE('',#29861,#29930,#21939,.T.);
#36232=EDGE_CURVE('',#29648,#29930,#16898,.T.);
#36233=EDGE_CURVE('',#29931,#29648,#21940,.T.);
#36234=EDGE_CURVE('',#29865,#29931,#21941,.T.);
#36235=EDGE_CURVE('',#29649,#29931,#16899,.T.);
#36236=EDGE_CURVE('',#29932,#29649,#21942,.T.);
#36237=EDGE_CURVE('',#29869,#29932,#21943,.T.);
#36238=EDGE_CURVE('',#29650,#29932,#16900,.T.);
#36239=EDGE_CURVE('',#29933,#29650,#21944,.T.);
#36240=EDGE_CURVE('',#29873,#29933,#21945,.T.);
#36241=EDGE_CURVE('',#29651,#29933,#16901,.T.);
#36242=EDGE_CURVE('',#29905,#29651,#4425,.T.);
#36243=EDGE_CURVE('',#29934,#29935,#16902,.T.);
#36244=EDGE_CURVE('',#29594,#29935,#21946,.T.);
#36245=EDGE_CURVE('',#29934,#29876,#24712,.T.);
#36246=EDGE_CURVE('',#29936,#29934,#16903,.T.);
#36247=EDGE_CURVE('',#29937,#29936,#16904,.T.);
#36248=EDGE_CURVE('',#29935,#29937,#16905,.T.);
#36249=EDGE_CURVE('',#29877,#29937,#24713,.T.);
#36250=EDGE_CURVE('',#29938,#29939,#16906,.T.);
#36251=EDGE_CURVE('',#29595,#29939,#21947,.T.);
#36252=EDGE_CURVE('',#29938,#29877,#24714,.T.);
#36253=EDGE_CURVE('',#29940,#29938,#16907,.T.);
#36254=EDGE_CURVE('',#29941,#29940,#16908,.T.);
#36255=EDGE_CURVE('',#29939,#29941,#16909,.T.);
#36256=EDGE_CURVE('',#29878,#29941,#24715,.T.);
#36257=EDGE_CURVE('',#29942,#29943,#16910,.T.);
#36258=EDGE_CURVE('',#29596,#29943,#21948,.T.);
#36259=EDGE_CURVE('',#29942,#29878,#24716,.T.);
#36260=EDGE_CURVE('',#29944,#29942,#16911,.T.);
#36261=EDGE_CURVE('',#29945,#29944,#16912,.T.);
#36262=EDGE_CURVE('',#29943,#29945,#16913,.T.);
#36263=EDGE_CURVE('',#29879,#29945,#24717,.T.);
#36264=EDGE_CURVE('',#29946,#29947,#16914,.T.);
#36265=EDGE_CURVE('',#29597,#29947,#21949,.T.);
#36266=EDGE_CURVE('',#29946,#29879,#24718,.T.);
#36267=EDGE_CURVE('',#29948,#29946,#16915,.T.);
#36268=EDGE_CURVE('',#29949,#29948,#16916,.T.);
#36269=EDGE_CURVE('',#29947,#29949,#16917,.T.);
#36270=EDGE_CURVE('',#29880,#29949,#24719,.T.);
#36271=EDGE_CURVE('',#29950,#29951,#16918,.T.);
#36272=EDGE_CURVE('',#29598,#29951,#21950,.T.);
#36273=EDGE_CURVE('',#29950,#29880,#24720,.T.);
#36274=EDGE_CURVE('',#29952,#29950,#16919,.T.);
#36275=EDGE_CURVE('',#29953,#29952,#16920,.T.);
#36276=EDGE_CURVE('',#29951,#29953,#16921,.T.);
#36277=EDGE_CURVE('',#29881,#29953,#24721,.T.);
#36278=EDGE_CURVE('',#29954,#29955,#16922,.T.);
#36279=EDGE_CURVE('',#29599,#29955,#21951,.T.);
#36280=EDGE_CURVE('',#29954,#29881,#24722,.T.);
#36281=EDGE_CURVE('',#29956,#29954,#16923,.T.);
#36282=EDGE_CURVE('',#29957,#29956,#16924,.T.);
#36283=EDGE_CURVE('',#29955,#29957,#16925,.T.);
#36284=EDGE_CURVE('',#29882,#29957,#24723,.T.);
#36285=EDGE_CURVE('',#29958,#29959,#16926,.T.);
#36286=EDGE_CURVE('',#29600,#29959,#21952,.T.);
#36287=EDGE_CURVE('',#29958,#29882,#24724,.T.);
#36288=EDGE_CURVE('',#29960,#29958,#16927,.T.);
#36289=EDGE_CURVE('',#29961,#29960,#16928,.T.);
#36290=EDGE_CURVE('',#29959,#29961,#16929,.T.);
#36291=EDGE_CURVE('',#29883,#29961,#24725,.T.);
#36292=EDGE_CURVE('',#29962,#29963,#16930,.T.);
#36293=EDGE_CURVE('',#29601,#29963,#21953,.T.);
#36294=EDGE_CURVE('',#29962,#29883,#24726,.T.);
#36295=EDGE_CURVE('',#29964,#29962,#16931,.T.);
#36296=EDGE_CURVE('',#29965,#29964,#16932,.T.);
#36297=EDGE_CURVE('',#29963,#29965,#16933,.T.);
#36298=EDGE_CURVE('',#29884,#29965,#24727,.T.);
#36299=EDGE_CURVE('',#29966,#29967,#16934,.T.);
#36300=EDGE_CURVE('',#29602,#29967,#21954,.T.);
#36301=EDGE_CURVE('',#29966,#29884,#24728,.T.);
#36302=EDGE_CURVE('',#29968,#29966,#16935,.T.);
#36303=EDGE_CURVE('',#29969,#29968,#16936,.T.);
#36304=EDGE_CURVE('',#29967,#29969,#16937,.T.);
#36305=EDGE_CURVE('',#29885,#29969,#24729,.T.);
#36306=EDGE_CURVE('',#29970,#29971,#16938,.T.);
#36307=EDGE_CURVE('',#29603,#29971,#21955,.T.);
#36308=EDGE_CURVE('',#29970,#29885,#24730,.T.);
#36309=EDGE_CURVE('',#29972,#29970,#16939,.T.);
#36310=EDGE_CURVE('',#29973,#29972,#16940,.T.);
#36311=EDGE_CURVE('',#29971,#29973,#16941,.T.);
#36312=EDGE_CURVE('',#29886,#29973,#24731,.T.);
#36313=EDGE_CURVE('',#29974,#29975,#16942,.T.);
#36314=EDGE_CURVE('',#29604,#29975,#21956,.T.);
#36315=EDGE_CURVE('',#29974,#29886,#24732,.T.);
#36316=EDGE_CURVE('',#29976,#29974,#16943,.T.);
#36317=EDGE_CURVE('',#29977,#29976,#16944,.T.);
#36318=EDGE_CURVE('',#29975,#29977,#16945,.T.);
#36319=EDGE_CURVE('',#29887,#29977,#24733,.T.);
#36320=EDGE_CURVE('',#29978,#29979,#16946,.T.);
#36321=EDGE_CURVE('',#29605,#29979,#21957,.T.);
#36322=EDGE_CURVE('',#29978,#29887,#24734,.T.);
#36323=EDGE_CURVE('',#29980,#29978,#16947,.T.);
#36324=EDGE_CURVE('',#29981,#29980,#16948,.T.);
#36325=EDGE_CURVE('',#29979,#29981,#16949,.T.);
#36326=EDGE_CURVE('',#29888,#29981,#24735,.T.);
#36327=EDGE_CURVE('',#29982,#29983,#16950,.T.);
#36328=EDGE_CURVE('',#29606,#29983,#21958,.T.);
#36329=EDGE_CURVE('',#29982,#29888,#24736,.T.);
#36330=EDGE_CURVE('',#29984,#29982,#16951,.T.);
#36331=EDGE_CURVE('',#29985,#29984,#16952,.T.);
#36332=EDGE_CURVE('',#29983,#29985,#16953,.T.);
#36333=EDGE_CURVE('',#29889,#29985,#24737,.T.);
#36334=EDGE_CURVE('',#29986,#29987,#16954,.T.);
#36335=EDGE_CURVE('',#29607,#29987,#21959,.T.);
#36336=EDGE_CURVE('',#29986,#29889,#24738,.T.);
#36337=EDGE_CURVE('',#29988,#29986,#16955,.T.);
#36338=EDGE_CURVE('',#29989,#29988,#16956,.T.);
#36339=EDGE_CURVE('',#29987,#29989,#16957,.T.);
#36340=EDGE_CURVE('',#29890,#29989,#24739,.T.);
#36341=EDGE_CURVE('',#29608,#29003,#21960,.T.);
#36342=EDGE_CURVE('',#29002,#29890,#24740,.T.);
#36343=EDGE_CURVE('',#29891,#29005,#24741,.T.);
#36344=EDGE_CURVE('',#29990,#29991,#16958,.T.);
#36345=EDGE_CURVE('',#29609,#29991,#21961,.T.);
#36346=EDGE_CURVE('',#29990,#29891,#24742,.T.);
#36347=EDGE_CURVE('',#29992,#29990,#16959,.T.);
#36348=EDGE_CURVE('',#29993,#29992,#16960,.T.);
#36349=EDGE_CURVE('',#29991,#29993,#16961,.T.);
#36350=EDGE_CURVE('',#29892,#29993,#24743,.T.);
#36351=EDGE_CURVE('',#29994,#29995,#16962,.T.);
#36352=EDGE_CURVE('',#29610,#29995,#21962,.T.);
#36353=EDGE_CURVE('',#29994,#29892,#24744,.T.);
#36354=EDGE_CURVE('',#29996,#29994,#16963,.T.);
#36355=EDGE_CURVE('',#29997,#29996,#16964,.T.);
#36356=EDGE_CURVE('',#29995,#29997,#16965,.T.);
#36357=EDGE_CURVE('',#29893,#29997,#24745,.T.);
#36358=EDGE_CURVE('',#29998,#29999,#16966,.T.);
#36359=EDGE_CURVE('',#29611,#29999,#21963,.T.);
#36360=EDGE_CURVE('',#29998,#29893,#24746,.T.);
#36361=EDGE_CURVE('',#30000,#29998,#16967,.T.);
#36362=EDGE_CURVE('',#30001,#30000,#16968,.T.);
#36363=EDGE_CURVE('',#29999,#30001,#16969,.T.);
#36364=EDGE_CURVE('',#29894,#30001,#24747,.T.);
#36365=EDGE_CURVE('',#30002,#30003,#16970,.T.);
#36366=EDGE_CURVE('',#29612,#30003,#21964,.T.);
#36367=EDGE_CURVE('',#30002,#29894,#24748,.T.);
#36368=EDGE_CURVE('',#30004,#30002,#16971,.T.);
#36369=EDGE_CURVE('',#30005,#30004,#16972,.T.);
#36370=EDGE_CURVE('',#30003,#30005,#16973,.T.);
#36371=EDGE_CURVE('',#29895,#30005,#24749,.T.);
#36372=EDGE_CURVE('',#30006,#30007,#16974,.T.);
#36373=EDGE_CURVE('',#29613,#30007,#21965,.T.);
#36374=EDGE_CURVE('',#30006,#29895,#24750,.T.);
#36375=EDGE_CURVE('',#30008,#30006,#16975,.T.);
#36376=EDGE_CURVE('',#30009,#30008,#16976,.T.);
#36377=EDGE_CURVE('',#30007,#30009,#16977,.T.);
#36378=EDGE_CURVE('',#29896,#30009,#24751,.T.);
#36379=EDGE_CURVE('',#30010,#30011,#16978,.T.);
#36380=EDGE_CURVE('',#29614,#30011,#21966,.T.);
#36381=EDGE_CURVE('',#30010,#29896,#24752,.T.);
#36382=EDGE_CURVE('',#30012,#30010,#16979,.T.);
#36383=EDGE_CURVE('',#30013,#30012,#16980,.T.);
#36384=EDGE_CURVE('',#30011,#30013,#16981,.T.);
#36385=EDGE_CURVE('',#29897,#30013,#24753,.T.);
#36386=EDGE_CURVE('',#30014,#30015,#16982,.T.);
#36387=EDGE_CURVE('',#29615,#30015,#21967,.T.);
#36388=EDGE_CURVE('',#30014,#29897,#24754,.T.);
#36389=EDGE_CURVE('',#30016,#30014,#16983,.T.);
#36390=EDGE_CURVE('',#30017,#30016,#16984,.T.);
#36391=EDGE_CURVE('',#30015,#30017,#16985,.T.);
#36392=EDGE_CURVE('',#29898,#30017,#24755,.T.);
#36393=EDGE_CURVE('',#30018,#30019,#16986,.T.);
#36394=EDGE_CURVE('',#29616,#30019,#21968,.T.);
#36395=EDGE_CURVE('',#30018,#29898,#24756,.T.);
#36396=EDGE_CURVE('',#30020,#30018,#16987,.T.);
#36397=EDGE_CURVE('',#30021,#30020,#16988,.T.);
#36398=EDGE_CURVE('',#30019,#30021,#16989,.T.);
#36399=EDGE_CURVE('',#29899,#30021,#24757,.T.);
#36400=EDGE_CURVE('',#30022,#30023,#16990,.T.);
#36401=EDGE_CURVE('',#29617,#30023,#21969,.T.);
#36402=EDGE_CURVE('',#30022,#29899,#24758,.T.);
#36403=EDGE_CURVE('',#30023,#30024,#16991,.T.);
#36404=EDGE_CURVE('',#29900,#30024,#24759,.T.);
#36405=EDGE_CURVE('',#30025,#30022,#16992,.T.);
#36406=EDGE_CURVE('',#30024,#30025,#16993,.T.);
#36407=EDGE_CURVE('',#30026,#29900,#24760,.T.);
#36408=EDGE_CURVE('',#30026,#30027,#16994,.T.);
#36409=EDGE_CURVE('',#29618,#30027,#21970,.T.);
#36410=EDGE_CURVE('',#30027,#30028,#16995,.T.);
#36411=EDGE_CURVE('',#30029,#30026,#16996,.T.);
#36412=EDGE_CURVE('',#30028,#30029,#16997,.T.);
#36413=EDGE_CURVE('',#29901,#30028,#24761,.T.);
#36414=EDGE_CURVE('',#30030,#30031,#16998,.T.);
#36415=EDGE_CURVE('',#29619,#30031,#21971,.T.);
#36416=EDGE_CURVE('',#30030,#29901,#24762,.T.);
#36417=EDGE_CURVE('',#30032,#30030,#16999,.T.);
#36418=EDGE_CURVE('',#30033,#30032,#17000,.T.);
#36419=EDGE_CURVE('',#30031,#30033,#17001,.T.);
#36420=EDGE_CURVE('',#29902,#30033,#24763,.T.);
#36421=EDGE_CURVE('',#30034,#30035,#17002,.T.);
#36422=EDGE_CURVE('',#29620,#30035,#21972,.T.);
#36423=EDGE_CURVE('',#30034,#29902,#24764,.T.);
#36424=EDGE_CURVE('',#30036,#30034,#17003,.T.);
#36425=EDGE_CURVE('',#30037,#30036,#17004,.T.);
#36426=EDGE_CURVE('',#30035,#30037,#17005,.T.);
#36427=EDGE_CURVE('',#29903,#30037,#24765,.T.);
#36428=EDGE_CURVE('',#30038,#30039,#17006,.T.);
#36429=EDGE_CURVE('',#29621,#30039,#21973,.T.);
#36430=EDGE_CURVE('',#30038,#29903,#24766,.T.);
#36431=EDGE_CURVE('',#30040,#30038,#17007,.T.);
#36432=EDGE_CURVE('',#30041,#30040,#17008,.T.);
#36433=EDGE_CURVE('',#30039,#30041,#17009,.T.);
#36434=EDGE_CURVE('',#29904,#30041,#24767,.T.);
#36435=EDGE_CURVE('',#30042,#30043,#17010,.T.);
#36436=EDGE_CURVE('',#29622,#30043,#21974,.T.);
#36437=EDGE_CURVE('',#30042,#29904,#24768,.T.);
#36438=EDGE_CURVE('',#30044,#30042,#17011,.T.);
#36439=EDGE_CURVE('',#30045,#30044,#17012,.T.);
#36440=EDGE_CURVE('',#30043,#30045,#17013,.T.);
#36441=EDGE_CURVE('',#29876,#30045,#24769,.T.);
#36442=EDGE_CURVE('',#30046,#29905,#24770,.T.);
#36443=EDGE_CURVE('',#30046,#30047,#17014,.T.);
#36444=EDGE_CURVE('',#29623,#30047,#21975,.T.);
#36445=EDGE_CURVE('',#30047,#30048,#21976,.T.);
#36446=EDGE_CURVE('',#29906,#30048,#24771,.T.);
#36447=EDGE_CURVE('',#30049,#30046,#17015,.T.);
#36448=EDGE_CURVE('',#30048,#30049,#17016,.T.);
#36449=EDGE_CURVE('',#30050,#29906,#24772,.T.);
#36450=EDGE_CURVE('',#30050,#30051,#17017,.T.);
#36451=EDGE_CURVE('',#29624,#30051,#21977,.T.);
#36452=EDGE_CURVE('',#30051,#30052,#21978,.T.);
#36453=EDGE_CURVE('',#29907,#30052,#24773,.T.);
#36454=EDGE_CURVE('',#30053,#30050,#17018,.T.);
#36455=EDGE_CURVE('',#30052,#30053,#17019,.T.);
#36456=EDGE_CURVE('',#30054,#29907,#24774,.T.);
#36457=EDGE_CURVE('',#30054,#30055,#17020,.T.);
#36458=EDGE_CURVE('',#29625,#30055,#21979,.T.);
#36459=EDGE_CURVE('',#30055,#30056,#21980,.T.);
#36460=EDGE_CURVE('',#29908,#30056,#24775,.T.);
#36461=EDGE_CURVE('',#30057,#30054,#17021,.T.);
#36462=EDGE_CURVE('',#30056,#30057,#17022,.T.);
#36463=EDGE_CURVE('',#30058,#29908,#24776,.T.);
#36464=EDGE_CURVE('',#30058,#30059,#17023,.T.);
#36465=EDGE_CURVE('',#29626,#30059,#21981,.T.);
#36466=EDGE_CURVE('',#30059,#30060,#21982,.T.);
#36467=EDGE_CURVE('',#29909,#30060,#24777,.T.);
#36468=EDGE_CURVE('',#30061,#30058,#17024,.T.);
#36469=EDGE_CURVE('',#30060,#30061,#17025,.T.);
#36470=EDGE_CURVE('',#30062,#29909,#24778,.T.);
#36471=EDGE_CURVE('',#30062,#30063,#17026,.T.);
#36472=EDGE_CURVE('',#29627,#30063,#21983,.T.);
#36473=EDGE_CURVE('',#30063,#30064,#21984,.T.);
#36474=EDGE_CURVE('',#29910,#30064,#24779,.T.);
#36475=EDGE_CURVE('',#30065,#30062,#17027,.T.);
#36476=EDGE_CURVE('',#30064,#30065,#17028,.T.);
#36477=EDGE_CURVE('',#30066,#29910,#24780,.T.);
#36478=EDGE_CURVE('',#30066,#30067,#17029,.T.);
#36479=EDGE_CURVE('',#29628,#30067,#21985,.T.);
#36480=EDGE_CURVE('',#30067,#30068,#21986,.T.);
#36481=EDGE_CURVE('',#29911,#30068,#24781,.T.);
#36482=EDGE_CURVE('',#30069,#30066,#17030,.T.);
#36483=EDGE_CURVE('',#30068,#30069,#17031,.T.);
#36484=EDGE_CURVE('',#30070,#29911,#24782,.T.);
#36485=EDGE_CURVE('',#30070,#30071,#17032,.T.);
#36486=EDGE_CURVE('',#29629,#30071,#21987,.T.);
#36487=EDGE_CURVE('',#30071,#30072,#21988,.T.);
#36488=EDGE_CURVE('',#29912,#30072,#24783,.T.);
#36489=EDGE_CURVE('',#30073,#30070,#17033,.T.);
#36490=EDGE_CURVE('',#30072,#30073,#17034,.T.);
#36491=EDGE_CURVE('',#30074,#29912,#24784,.T.);
#36492=EDGE_CURVE('',#30074,#30075,#17035,.T.);
#36493=EDGE_CURVE('',#29630,#30075,#21989,.T.);
#36494=EDGE_CURVE('',#30075,#30076,#21990,.T.);
#36495=EDGE_CURVE('',#29913,#30076,#24785,.T.);
#36496=EDGE_CURVE('',#30077,#30074,#17036,.T.);
#36497=EDGE_CURVE('',#30076,#30077,#17037,.T.);
#36498=EDGE_CURVE('',#30078,#29913,#24786,.T.);
#36499=EDGE_CURVE('',#30078,#30079,#17038,.T.);
#36500=EDGE_CURVE('',#29631,#30079,#21991,.T.);
#36501=EDGE_CURVE('',#30079,#30080,#21992,.T.);
#36502=EDGE_CURVE('',#29914,#30080,#24787,.T.);
#36503=EDGE_CURVE('',#30081,#30078,#17039,.T.);
#36504=EDGE_CURVE('',#30080,#30081,#17040,.T.);
#36505=EDGE_CURVE('',#30082,#29914,#24788,.T.);
#36506=EDGE_CURVE('',#30082,#30083,#17041,.T.);
#36507=EDGE_CURVE('',#29632,#30083,#21993,.T.);
#36508=EDGE_CURVE('',#30083,#30084,#21994,.T.);
#36509=EDGE_CURVE('',#29915,#30084,#24789,.T.);
#36510=EDGE_CURVE('',#30085,#30082,#17042,.T.);
#36511=EDGE_CURVE('',#30084,#30085,#17043,.T.);
#36512=EDGE_CURVE('',#30086,#29915,#24790,.T.);
#36513=EDGE_CURVE('',#30086,#30087,#17044,.T.);
#36514=EDGE_CURVE('',#29633,#30087,#21995,.T.);
#36515=EDGE_CURVE('',#30087,#30088,#21996,.T.);
#36516=EDGE_CURVE('',#29916,#30088,#24791,.T.);
#36517=EDGE_CURVE('',#30089,#30086,#17045,.T.);
#36518=EDGE_CURVE('',#30088,#30089,#17046,.T.);
#36519=EDGE_CURVE('',#30090,#29916,#24792,.T.);
#36520=EDGE_CURVE('',#30090,#30091,#17047,.T.);
#36521=EDGE_CURVE('',#29634,#30091,#21997,.T.);
#36522=EDGE_CURVE('',#30091,#30092,#21998,.T.);
#36523=EDGE_CURVE('',#29917,#30092,#24793,.T.);
#36524=EDGE_CURVE('',#30093,#30090,#17048,.T.);
#36525=EDGE_CURVE('',#30092,#30093,#17049,.T.);
#36526=EDGE_CURVE('',#30094,#29917,#24794,.T.);
#36527=EDGE_CURVE('',#30094,#30095,#17050,.T.);
#36528=EDGE_CURVE('',#29635,#30095,#21999,.T.);
#36529=EDGE_CURVE('',#30095,#30096,#22000,.T.);
#36530=EDGE_CURVE('',#29918,#30096,#24795,.T.);
#36531=EDGE_CURVE('',#30097,#30094,#17051,.T.);
#36532=EDGE_CURVE('',#30096,#30097,#17052,.T.);
#36533=EDGE_CURVE('',#30098,#29918,#24796,.T.);
#36534=EDGE_CURVE('',#30098,#30099,#17053,.T.);
#36535=EDGE_CURVE('',#29636,#30099,#22001,.T.);
#36536=EDGE_CURVE('',#30099,#30100,#22002,.T.);
#36537=EDGE_CURVE('',#29919,#30100,#24797,.T.);
#36538=EDGE_CURVE('',#30101,#30098,#17054,.T.);
#36539=EDGE_CURVE('',#30100,#30101,#17055,.T.);
#36540=EDGE_CURVE('',#30102,#29919,#24798,.T.);
#36541=EDGE_CURVE('',#30102,#30103,#17056,.T.);
#36542=EDGE_CURVE('',#29637,#30103,#22003,.T.);
#36543=EDGE_CURVE('',#30103,#30104,#22004,.T.);
#36544=EDGE_CURVE('',#29920,#30104,#24799,.T.);
#36545=EDGE_CURVE('',#30105,#30102,#17057,.T.);
#36546=EDGE_CURVE('',#30104,#30105,#17058,.T.);
#36547=EDGE_CURVE('',#30106,#29920,#24800,.T.);
#36548=EDGE_CURVE('',#30106,#30107,#17059,.T.);
#36549=EDGE_CURVE('',#29638,#30107,#22005,.T.);
#36550=EDGE_CURVE('',#30107,#30108,#22006,.T.);
#36551=EDGE_CURVE('',#29921,#30108,#24801,.T.);
#36552=EDGE_CURVE('',#30109,#30106,#17060,.T.);
#36553=EDGE_CURVE('',#30108,#30109,#17061,.T.);
#36554=EDGE_CURVE('',#30110,#29921,#24802,.T.);
#36555=EDGE_CURVE('',#30110,#30111,#17062,.T.);
#36556=EDGE_CURVE('',#29639,#30111,#22007,.T.);
#36557=EDGE_CURVE('',#30111,#30112,#22008,.T.);
#36558=EDGE_CURVE('',#29922,#30112,#24803,.T.);
#36559=EDGE_CURVE('',#30113,#30110,#17063,.T.);
#36560=EDGE_CURVE('',#30112,#30113,#17064,.T.);
#36561=EDGE_CURVE('',#30114,#29922,#24804,.T.);
#36562=EDGE_CURVE('',#30114,#30115,#17065,.T.);
#36563=EDGE_CURVE('',#29640,#30115,#22009,.T.);
#36564=EDGE_CURVE('',#30115,#30116,#22010,.T.);
#36565=EDGE_CURVE('',#29923,#30116,#24805,.T.);
#36566=EDGE_CURVE('',#30117,#30114,#17066,.T.);
#36567=EDGE_CURVE('',#30116,#30117,#17067,.T.);
#36568=EDGE_CURVE('',#30118,#29923,#24806,.T.);
#36569=EDGE_CURVE('',#30118,#30119,#17068,.T.);
#36570=EDGE_CURVE('',#29641,#30119,#22011,.T.);
#36571=EDGE_CURVE('',#30119,#30120,#22012,.T.);
#36572=EDGE_CURVE('',#29924,#30120,#24807,.T.);
#36573=EDGE_CURVE('',#30121,#30118,#17069,.T.);
#36574=EDGE_CURVE('',#30120,#30121,#17070,.T.);
#36575=EDGE_CURVE('',#30122,#29924,#24808,.T.);
#36576=EDGE_CURVE('',#30122,#30123,#17071,.T.);
#36577=EDGE_CURVE('',#29642,#30123,#22013,.T.);
#36578=EDGE_CURVE('',#30123,#30124,#22014,.T.);
#36579=EDGE_CURVE('',#29925,#30124,#24809,.T.);
#36580=EDGE_CURVE('',#30125,#30122,#17072,.T.);
#36581=EDGE_CURVE('',#30124,#30125,#17073,.T.);
#36582=EDGE_CURVE('',#30126,#29925,#24810,.T.);
#36583=EDGE_CURVE('',#30126,#30127,#17074,.T.);
#36584=EDGE_CURVE('',#29643,#30127,#22015,.T.);
#36585=EDGE_CURVE('',#30127,#30128,#22016,.T.);
#36586=EDGE_CURVE('',#29926,#30128,#24811,.T.);
#36587=EDGE_CURVE('',#30129,#30126,#17075,.T.);
#36588=EDGE_CURVE('',#30128,#30129,#17076,.T.);
#36589=EDGE_CURVE('',#30130,#29926,#24812,.T.);
#36590=EDGE_CURVE('',#30130,#30131,#17077,.T.);
#36591=EDGE_CURVE('',#29644,#30131,#22017,.T.);
#36592=EDGE_CURVE('',#30131,#30132,#22018,.T.);
#36593=EDGE_CURVE('',#29927,#30132,#24813,.T.);
#36594=EDGE_CURVE('',#30133,#30130,#17078,.T.);
#36595=EDGE_CURVE('',#30132,#30133,#17079,.T.);
#36596=EDGE_CURVE('',#30134,#29927,#24814,.T.);
#36597=EDGE_CURVE('',#30134,#30135,#17080,.T.);
#36598=EDGE_CURVE('',#29645,#30135,#22019,.T.);
#36599=EDGE_CURVE('',#30135,#30136,#22020,.T.);
#36600=EDGE_CURVE('',#29928,#30136,#24815,.T.);
#36601=EDGE_CURVE('',#30137,#30134,#17081,.T.);
#36602=EDGE_CURVE('',#30136,#30137,#17082,.T.);
#36603=EDGE_CURVE('',#30138,#29928,#24816,.T.);
#36604=EDGE_CURVE('',#30138,#30139,#17083,.T.);
#36605=EDGE_CURVE('',#29646,#30139,#22021,.T.);
#36606=EDGE_CURVE('',#30139,#30140,#22022,.T.);
#36607=EDGE_CURVE('',#29929,#30140,#24817,.T.);
#36608=EDGE_CURVE('',#30141,#30138,#17084,.T.);
#36609=EDGE_CURVE('',#30140,#30141,#17085,.T.);
#36610=EDGE_CURVE('',#30142,#29929,#24818,.T.);
#36611=EDGE_CURVE('',#30142,#30143,#17086,.T.);
#36612=EDGE_CURVE('',#29647,#30143,#22023,.T.);
#36613=EDGE_CURVE('',#30143,#30144,#22024,.T.);
#36614=EDGE_CURVE('',#29930,#30144,#24819,.T.);
#36615=EDGE_CURVE('',#30145,#30142,#17087,.T.);
#36616=EDGE_CURVE('',#30144,#30145,#17088,.T.);
#36617=EDGE_CURVE('',#30146,#29930,#24820,.T.);
#36618=EDGE_CURVE('',#30146,#30147,#17089,.T.);
#36619=EDGE_CURVE('',#29648,#30147,#22025,.T.);
#36620=EDGE_CURVE('',#30147,#30148,#22026,.T.);
#36621=EDGE_CURVE('',#29931,#30148,#24821,.T.);
#36622=EDGE_CURVE('',#30149,#30146,#17090,.T.);
#36623=EDGE_CURVE('',#30148,#30149,#17091,.T.);
#36624=EDGE_CURVE('',#30150,#29931,#24822,.T.);
#36625=EDGE_CURVE('',#30150,#30151,#17092,.T.);
#36626=EDGE_CURVE('',#29649,#30151,#22027,.T.);
#36627=EDGE_CURVE('',#30151,#30152,#22028,.T.);
#36628=EDGE_CURVE('',#29932,#30152,#24823,.T.);
#36629=EDGE_CURVE('',#30153,#30150,#17093,.T.);
#36630=EDGE_CURVE('',#30152,#30153,#17094,.T.);
#36631=EDGE_CURVE('',#30154,#29932,#24824,.T.);
#36632=EDGE_CURVE('',#30154,#30155,#17095,.T.);
#36633=EDGE_CURVE('',#29650,#30155,#22029,.T.);
#36634=EDGE_CURVE('',#30155,#30156,#22030,.T.);
#36635=EDGE_CURVE('',#29933,#30156,#24825,.T.);
#36636=EDGE_CURVE('',#30157,#30154,#17096,.T.);
#36637=EDGE_CURVE('',#30156,#30157,#17097,.T.);
#36638=EDGE_CURVE('',#30158,#29933,#24826,.T.);
#36639=EDGE_CURVE('',#30158,#30159,#17098,.T.);
#36640=EDGE_CURVE('',#29651,#30159,#22031,.T.);
#36641=EDGE_CURVE('',#30159,#30160,#22032,.T.);
#36642=EDGE_CURVE('',#29905,#30160,#24827,.T.);
#36643=EDGE_CURVE('',#30161,#30158,#17099,.T.);
#36644=EDGE_CURVE('',#30160,#30161,#17100,.T.);
#36645=EDGE_CURVE('',#30162,#29876,#17101,.T.);
#36646=EDGE_CURVE('',#29936,#30162,#22033,.T.);
#36647=EDGE_CURVE('',#29877,#30162,#17102,.T.);
#36648=EDGE_CURVE('',#30163,#29877,#17103,.T.);
#36649=EDGE_CURVE('',#29940,#30163,#22034,.T.);
#36650=EDGE_CURVE('',#29878,#30163,#17104,.T.);
#36651=EDGE_CURVE('',#30164,#29878,#17105,.T.);
#36652=EDGE_CURVE('',#29944,#30164,#22035,.T.);
#36653=EDGE_CURVE('',#29879,#30164,#17106,.T.);
#36654=EDGE_CURVE('',#30165,#29879,#17107,.T.);
#36655=EDGE_CURVE('',#29948,#30165,#22036,.T.);
#36656=EDGE_CURVE('',#29880,#30165,#17108,.T.);
#36657=EDGE_CURVE('',#30166,#29880,#17109,.T.);
#36658=EDGE_CURVE('',#29952,#30166,#22037,.T.);
#36659=EDGE_CURVE('',#29881,#30166,#17110,.T.);
#36660=EDGE_CURVE('',#30167,#29881,#17111,.T.);
#36661=EDGE_CURVE('',#29956,#30167,#22038,.T.);
#36662=EDGE_CURVE('',#29882,#30167,#17112,.T.);
#36663=EDGE_CURVE('',#30168,#29882,#17113,.T.);
#36664=EDGE_CURVE('',#29960,#30168,#22039,.T.);
#36665=EDGE_CURVE('',#29883,#30168,#17114,.T.);
#36666=EDGE_CURVE('',#30169,#29883,#17115,.T.);
#36667=EDGE_CURVE('',#29964,#30169,#22040,.T.);
#36668=EDGE_CURVE('',#29884,#30169,#17116,.T.);
#36669=EDGE_CURVE('',#30170,#29884,#17117,.T.);
#36670=EDGE_CURVE('',#29968,#30170,#22041,.T.);
#36671=EDGE_CURVE('',#29885,#30170,#17118,.T.);
#36672=EDGE_CURVE('',#30171,#29885,#17119,.T.);
#36673=EDGE_CURVE('',#29972,#30171,#22042,.T.);
#36674=EDGE_CURVE('',#29886,#30171,#17120,.T.);
#36675=EDGE_CURVE('',#30172,#29886,#17121,.T.);
#36676=EDGE_CURVE('',#29976,#30172,#22043,.T.);
#36677=EDGE_CURVE('',#29887,#30172,#17122,.T.);
#36678=EDGE_CURVE('',#30173,#29887,#17123,.T.);
#36679=EDGE_CURVE('',#29980,#30173,#22044,.T.);
#36680=EDGE_CURVE('',#29888,#30173,#17124,.T.);
#36681=EDGE_CURVE('',#30174,#29888,#17125,.T.);
#36682=EDGE_CURVE('',#29984,#30174,#22045,.T.);
#36683=EDGE_CURVE('',#29889,#30174,#17126,.T.);
#36684=EDGE_CURVE('',#30175,#29889,#17127,.T.);
#36685=EDGE_CURVE('',#29988,#30175,#22046,.T.);
#36686=EDGE_CURVE('',#29890,#30175,#17128,.T.);
#36687=EDGE_CURVE('',#30176,#29890,#17129,.T.);
#36688=EDGE_CURVE('',#29004,#30176,#22047,.T.);
#36689=EDGE_CURVE('',#29891,#30176,#17130,.T.);
#36690=EDGE_CURVE('',#30177,#29891,#17131,.T.);
#36691=EDGE_CURVE('',#29992,#30177,#22048,.T.);
#36692=EDGE_CURVE('',#29892,#30177,#17132,.T.);
#36693=EDGE_CURVE('',#30178,#29892,#17133,.T.);
#36694=EDGE_CURVE('',#29996,#30178,#22049,.T.);
#36695=EDGE_CURVE('',#29893,#30178,#17134,.T.);
#36696=EDGE_CURVE('',#30179,#29893,#17135,.T.);
#36697=EDGE_CURVE('',#30000,#30179,#22050,.T.);
#36698=EDGE_CURVE('',#29894,#30179,#17136,.T.);
#36699=EDGE_CURVE('',#30180,#29894,#17137,.T.);
#36700=EDGE_CURVE('',#30004,#30180,#22051,.T.);
#36701=EDGE_CURVE('',#29895,#30180,#17138,.T.);
#36702=EDGE_CURVE('',#30181,#29895,#17139,.T.);
#36703=EDGE_CURVE('',#30008,#30181,#22052,.T.);
#36704=EDGE_CURVE('',#29896,#30181,#17140,.T.);
#36705=EDGE_CURVE('',#30182,#29896,#17141,.T.);
#36706=EDGE_CURVE('',#30012,#30182,#22053,.T.);
#36707=EDGE_CURVE('',#29897,#30182,#17142,.T.);
#36708=EDGE_CURVE('',#30183,#29897,#17143,.T.);
#36709=EDGE_CURVE('',#30016,#30183,#22054,.T.);
#36710=EDGE_CURVE('',#29898,#30183,#17144,.T.);
#36711=EDGE_CURVE('',#30184,#29898,#17145,.T.);
#36712=EDGE_CURVE('',#30020,#30184,#22055,.T.);
#36713=EDGE_CURVE('',#29899,#30184,#17146,.T.);
#36714=EDGE_CURVE('',#30185,#29899,#17147,.T.);
#36715=EDGE_CURVE('',#30025,#30185,#22056,.T.);
#36716=EDGE_CURVE('',#29900,#30185,#17148,.T.);
#36717=EDGE_CURVE('',#30186,#29900,#17149,.T.);
#36718=EDGE_CURVE('',#30029,#30186,#22057,.T.);
#36719=EDGE_CURVE('',#29901,#30186,#17150,.T.);
#36720=EDGE_CURVE('',#30187,#29901,#17151,.T.);
#36721=EDGE_CURVE('',#30032,#30187,#22058,.T.);
#36722=EDGE_CURVE('',#29902,#30187,#17152,.T.);
#36723=EDGE_CURVE('',#30188,#29902,#17153,.T.);
#36724=EDGE_CURVE('',#30036,#30188,#22059,.T.);
#36725=EDGE_CURVE('',#29903,#30188,#17154,.T.);
#36726=EDGE_CURVE('',#30189,#29903,#17155,.T.);
#36727=EDGE_CURVE('',#30040,#30189,#22060,.T.);
#36728=EDGE_CURVE('',#29904,#30189,#17156,.T.);
#36729=EDGE_CURVE('',#30190,#29904,#17157,.T.);
#36730=EDGE_CURVE('',#30044,#30190,#22061,.T.);
#36731=EDGE_CURVE('',#29876,#30190,#17158,.T.);
#36732=EDGE_CURVE('',#30191,#29905,#17159,.T.);
#36733=EDGE_CURVE('',#30049,#30191,#22062,.T.);
#36734=EDGE_CURVE('',#29906,#30191,#17160,.T.);
#36735=EDGE_CURVE('',#30192,#29906,#17161,.T.);
#36736=EDGE_CURVE('',#30053,#30192,#22063,.T.);
#36737=EDGE_CURVE('',#29907,#30192,#17162,.T.);
#36738=EDGE_CURVE('',#30193,#29907,#17163,.T.);
#36739=EDGE_CURVE('',#30057,#30193,#22064,.T.);
#36740=EDGE_CURVE('',#29908,#30193,#17164,.T.);
#36741=EDGE_CURVE('',#30194,#29908,#17165,.T.);
#36742=EDGE_CURVE('',#30061,#30194,#22065,.T.);
#36743=EDGE_CURVE('',#29909,#30194,#17166,.T.);
#36744=EDGE_CURVE('',#30195,#29909,#17167,.T.);
#36745=EDGE_CURVE('',#30065,#30195,#22066,.T.);
#36746=EDGE_CURVE('',#29910,#30195,#17168,.T.);
#36747=EDGE_CURVE('',#30196,#29910,#17169,.T.);
#36748=EDGE_CURVE('',#30069,#30196,#22067,.T.);
#36749=EDGE_CURVE('',#29911,#30196,#17170,.T.);
#36750=EDGE_CURVE('',#30197,#29911,#17171,.T.);
#36751=EDGE_CURVE('',#30073,#30197,#22068,.T.);
#36752=EDGE_CURVE('',#29912,#30197,#17172,.T.);
#36753=EDGE_CURVE('',#30198,#29912,#17173,.T.);
#36754=EDGE_CURVE('',#30077,#30198,#22069,.T.);
#36755=EDGE_CURVE('',#29913,#30198,#17174,.T.);
#36756=EDGE_CURVE('',#30199,#29913,#17175,.T.);
#36757=EDGE_CURVE('',#30081,#30199,#22070,.T.);
#36758=EDGE_CURVE('',#29914,#30199,#17176,.T.);
#36759=EDGE_CURVE('',#30200,#29914,#17177,.T.);
#36760=EDGE_CURVE('',#30085,#30200,#22071,.T.);
#36761=EDGE_CURVE('',#29915,#30200,#17178,.T.);
#36762=EDGE_CURVE('',#30201,#29915,#17179,.T.);
#36763=EDGE_CURVE('',#30089,#30201,#22072,.T.);
#36764=EDGE_CURVE('',#29916,#30201,#17180,.T.);
#36765=EDGE_CURVE('',#30202,#29916,#17181,.T.);
#36766=EDGE_CURVE('',#30093,#30202,#22073,.T.);
#36767=EDGE_CURVE('',#29917,#30202,#17182,.T.);
#36768=EDGE_CURVE('',#30203,#29917,#17183,.T.);
#36769=EDGE_CURVE('',#30097,#30203,#22074,.T.);
#36770=EDGE_CURVE('',#29918,#30203,#17184,.T.);
#36771=EDGE_CURVE('',#30204,#29918,#17185,.T.);
#36772=EDGE_CURVE('',#30101,#30204,#22075,.T.);
#36773=EDGE_CURVE('',#29919,#30204,#17186,.T.);
#36774=EDGE_CURVE('',#30205,#29919,#17187,.T.);
#36775=EDGE_CURVE('',#30105,#30205,#22076,.T.);
#36776=EDGE_CURVE('',#29920,#30205,#17188,.T.);
#36777=EDGE_CURVE('',#30206,#29920,#17189,.T.);
#36778=EDGE_CURVE('',#30109,#30206,#22077,.T.);
#36779=EDGE_CURVE('',#29921,#30206,#17190,.T.);
#36780=EDGE_CURVE('',#30207,#29921,#17191,.T.);
#36781=EDGE_CURVE('',#30113,#30207,#22078,.T.);
#36782=EDGE_CURVE('',#29922,#30207,#17192,.T.);
#36783=EDGE_CURVE('',#30208,#29922,#17193,.T.);
#36784=EDGE_CURVE('',#30117,#30208,#22079,.T.);
#36785=EDGE_CURVE('',#29923,#30208,#17194,.T.);
#36786=EDGE_CURVE('',#30209,#29923,#17195,.T.);
#36787=EDGE_CURVE('',#30121,#30209,#22080,.T.);
#36788=EDGE_CURVE('',#29924,#30209,#17196,.T.);
#36789=EDGE_CURVE('',#30210,#29924,#17197,.T.);
#36790=EDGE_CURVE('',#30125,#30210,#22081,.T.);
#36791=EDGE_CURVE('',#29925,#30210,#17198,.T.);
#36792=EDGE_CURVE('',#30211,#29925,#17199,.T.);
#36793=EDGE_CURVE('',#30129,#30211,#22082,.T.);
#36794=EDGE_CURVE('',#29926,#30211,#17200,.T.);
#36795=EDGE_CURVE('',#30212,#29926,#17201,.T.);
#36796=EDGE_CURVE('',#30133,#30212,#22083,.T.);
#36797=EDGE_CURVE('',#29927,#30212,#17202,.T.);
#36798=EDGE_CURVE('',#30213,#29927,#17203,.T.);
#36799=EDGE_CURVE('',#30137,#30213,#22084,.T.);
#36800=EDGE_CURVE('',#29928,#30213,#17204,.T.);
#36801=EDGE_CURVE('',#30214,#29928,#17205,.T.);
#36802=EDGE_CURVE('',#30141,#30214,#22085,.T.);
#36803=EDGE_CURVE('',#29929,#30214,#17206,.T.);
#36804=EDGE_CURVE('',#30215,#29929,#17207,.T.);
#36805=EDGE_CURVE('',#30145,#30215,#22086,.T.);
#36806=EDGE_CURVE('',#29930,#30215,#17208,.T.);
#36807=EDGE_CURVE('',#30216,#29930,#17209,.T.);
#36808=EDGE_CURVE('',#30149,#30216,#22087,.T.);
#36809=EDGE_CURVE('',#29931,#30216,#17210,.T.);
#36810=EDGE_CURVE('',#30217,#29931,#17211,.T.);
#36811=EDGE_CURVE('',#30153,#30217,#22088,.T.);
#36812=EDGE_CURVE('',#29932,#30217,#17212,.T.);
#36813=EDGE_CURVE('',#30218,#29932,#17213,.T.);
#36814=EDGE_CURVE('',#30157,#30218,#22089,.T.);
#36815=EDGE_CURVE('',#29933,#30218,#17214,.T.);
#36816=EDGE_CURVE('',#30219,#29933,#17215,.T.);
#36817=EDGE_CURVE('',#30161,#30219,#22090,.T.);
#36818=EDGE_CURVE('',#29905,#30219,#17216,.T.);
#36819=EDGE_CURVE('',#30220,#30221,#17217,.T.);
#36820=EDGE_CURVE('',#30162,#30221,#24828,.T.);
#36821=EDGE_CURVE('',#30220,#29876,#22091,.T.);
#36822=EDGE_CURVE('',#30222,#30223,#17218,.T.);
#36823=EDGE_CURVE('',#29877,#30223,#22092,.T.);
#36824=EDGE_CURVE('',#30222,#30162,#24829,.T.);
#36825=EDGE_CURVE('',#30224,#30222,#22093,.T.);
#36826=EDGE_CURVE('',#30225,#30224,#17219,.T.);
#36827=EDGE_CURVE('',#30223,#30225,#17220,.T.);
#36828=EDGE_CURVE('',#30163,#30225,#24830,.T.);
#36829=EDGE_CURVE('',#30226,#30227,#17221,.T.);
#36830=EDGE_CURVE('',#29878,#30227,#22094,.T.);
#36831=EDGE_CURVE('',#30226,#30163,#24831,.T.);
#36832=EDGE_CURVE('',#30228,#30226,#22095,.T.);
#36833=EDGE_CURVE('',#30229,#30228,#17222,.T.);
#36834=EDGE_CURVE('',#30227,#30229,#17223,.T.);
#36835=EDGE_CURVE('',#30164,#30229,#24832,.T.);
#36836=EDGE_CURVE('',#30230,#30231,#17224,.T.);
#36837=EDGE_CURVE('',#29879,#30231,#22096,.T.);
#36838=EDGE_CURVE('',#30230,#30164,#24833,.T.);
#36839=EDGE_CURVE('',#30232,#30230,#22097,.T.);
#36840=EDGE_CURVE('',#30233,#30232,#17225,.T.);
#36841=EDGE_CURVE('',#30231,#30233,#17226,.T.);
#36842=EDGE_CURVE('',#30165,#30233,#24834,.T.);
#36843=EDGE_CURVE('',#30234,#30235,#17227,.T.);
#36844=EDGE_CURVE('',#29880,#30235,#22098,.T.);
#36845=EDGE_CURVE('',#30234,#30165,#24835,.T.);
#36846=EDGE_CURVE('',#30236,#30234,#22099,.T.);
#36847=EDGE_CURVE('',#30237,#30236,#17228,.T.);
#36848=EDGE_CURVE('',#30235,#30237,#17229,.T.);
#36849=EDGE_CURVE('',#30166,#30237,#24836,.T.);
#36850=EDGE_CURVE('',#30238,#30239,#17230,.T.);
#36851=EDGE_CURVE('',#29881,#30239,#22100,.T.);
#36852=EDGE_CURVE('',#30238,#30166,#24837,.T.);
#36853=EDGE_CURVE('',#30240,#30238,#22101,.T.);
#36854=EDGE_CURVE('',#30241,#30240,#17231,.T.);
#36855=EDGE_CURVE('',#30239,#30241,#17232,.T.);
#36856=EDGE_CURVE('',#30167,#30241,#24838,.T.);
#36857=EDGE_CURVE('',#30242,#30243,#17233,.T.);
#36858=EDGE_CURVE('',#29882,#30243,#22102,.T.);
#36859=EDGE_CURVE('',#30242,#30167,#24839,.T.);
#36860=EDGE_CURVE('',#30244,#30242,#22103,.T.);
#36861=EDGE_CURVE('',#30245,#30244,#17234,.T.);
#36862=EDGE_CURVE('',#30243,#30245,#17235,.T.);
#36863=EDGE_CURVE('',#30168,#30245,#24840,.T.);
#36864=EDGE_CURVE('',#29883,#28998,#22104,.T.);
#36865=EDGE_CURVE('',#29000,#30168,#24841,.T.);
#36866=EDGE_CURVE('',#30169,#28999,#24842,.T.);
#36867=EDGE_CURVE('',#30246,#30247,#17236,.T.);
#36868=EDGE_CURVE('',#29884,#30247,#22105,.T.);
#36869=EDGE_CURVE('',#30246,#30169,#24843,.T.);
#36870=EDGE_CURVE('',#30248,#30246,#22106,.T.);
#36871=EDGE_CURVE('',#30249,#30248,#17237,.T.);
#36872=EDGE_CURVE('',#30247,#30249,#17238,.T.);
#36873=EDGE_CURVE('',#30170,#30249,#24844,.T.);
#36874=EDGE_CURVE('',#30250,#30251,#17239,.T.);
#36875=EDGE_CURVE('',#29885,#30251,#22107,.T.);
#36876=EDGE_CURVE('',#30250,#30170,#24845,.T.);
#36877=EDGE_CURVE('',#30252,#30250,#22108,.T.);
#36878=EDGE_CURVE('',#30253,#30252,#17240,.T.);
#36879=EDGE_CURVE('',#30251,#30253,#17241,.T.);
#36880=EDGE_CURVE('',#30171,#30253,#24846,.T.);
#36881=EDGE_CURVE('',#30254,#30255,#17242,.T.);
#36882=EDGE_CURVE('',#29886,#30255,#22109,.T.);
#36883=EDGE_CURVE('',#30254,#30171,#24847,.T.);
#36884=EDGE_CURVE('',#30256,#30254,#22110,.T.);
#36885=EDGE_CURVE('',#30257,#30256,#17243,.T.);
#36886=EDGE_CURVE('',#30255,#30257,#17244,.T.);
#36887=EDGE_CURVE('',#30172,#30257,#24848,.T.);
#36888=EDGE_CURVE('',#30258,#30259,#17245,.T.);
#36889=EDGE_CURVE('',#29887,#30259,#22111,.T.);
#36890=EDGE_CURVE('',#30258,#30172,#24849,.T.);
#36891=EDGE_CURVE('',#30260,#30258,#22112,.T.);
#36892=EDGE_CURVE('',#30261,#30260,#17246,.T.);
#36893=EDGE_CURVE('',#30259,#30261,#17247,.T.);
#36894=EDGE_CURVE('',#30173,#30261,#24850,.T.);
#36895=EDGE_CURVE('',#30262,#30263,#17248,.T.);
#36896=EDGE_CURVE('',#29888,#30263,#22113,.T.);
#36897=EDGE_CURVE('',#30262,#30173,#24851,.T.);
#36898=EDGE_CURVE('',#30264,#30262,#22114,.T.);
#36899=EDGE_CURVE('',#30265,#30264,#17249,.T.);
#36900=EDGE_CURVE('',#30263,#30265,#17250,.T.);
#36901=EDGE_CURVE('',#30174,#30265,#24852,.T.);
#36902=EDGE_CURVE('',#30266,#30267,#17251,.T.);
#36903=EDGE_CURVE('',#29889,#30267,#22115,.T.);
#36904=EDGE_CURVE('',#30266,#30174,#24853,.T.);
#36905=EDGE_CURVE('',#30268,#30266,#22116,.T.);
#36906=EDGE_CURVE('',#30269,#30268,#17252,.T.);
#36907=EDGE_CURVE('',#30267,#30269,#17253,.T.);
#36908=EDGE_CURVE('',#30175,#30269,#24854,.T.);
#36909=EDGE_CURVE('',#30270,#30271,#17254,.T.);
#36910=EDGE_CURVE('',#29890,#30271,#22117,.T.);
#36911=EDGE_CURVE('',#30270,#30175,#24855,.T.);
#36912=EDGE_CURVE('',#30272,#30270,#22118,.T.);
#36913=EDGE_CURVE('',#30273,#30272,#17255,.T.);
#36914=EDGE_CURVE('',#30271,#30273,#17256,.T.);
#36915=EDGE_CURVE('',#30176,#30273,#24856,.T.);
#36916=EDGE_CURVE('',#30274,#30275,#17257,.T.);
#36917=EDGE_CURVE('',#29891,#30275,#22119,.T.);
#36918=EDGE_CURVE('',#30274,#30176,#24857,.T.);
#36919=EDGE_CURVE('',#30276,#30274,#22120,.T.);
#36920=EDGE_CURVE('',#30277,#30276,#17258,.T.);
#36921=EDGE_CURVE('',#30275,#30277,#17259,.T.);
#36922=EDGE_CURVE('',#30177,#30277,#24858,.T.);
#36923=EDGE_CURVE('',#30278,#30279,#17260,.T.);
#36924=EDGE_CURVE('',#29892,#30279,#22121,.T.);
#36925=EDGE_CURVE('',#30278,#30177,#24859,.T.);
#36926=EDGE_CURVE('',#30280,#30278,#22122,.T.);
#36927=EDGE_CURVE('',#30281,#30280,#17261,.T.);
#36928=EDGE_CURVE('',#30279,#30281,#17262,.T.);
#36929=EDGE_CURVE('',#30178,#30281,#24860,.T.);
#36930=EDGE_CURVE('',#30282,#30283,#17263,.T.);
#36931=EDGE_CURVE('',#29893,#30283,#22123,.T.);
#36932=EDGE_CURVE('',#30282,#30178,#24861,.T.);
#36933=EDGE_CURVE('',#30284,#30282,#22124,.T.);
#36934=EDGE_CURVE('',#30285,#30284,#17264,.T.);
#36935=EDGE_CURVE('',#30283,#30285,#17265,.T.);
#36936=EDGE_CURVE('',#30179,#30285,#24862,.T.);
#36937=EDGE_CURVE('',#30286,#30287,#17266,.T.);
#36938=EDGE_CURVE('',#29894,#30287,#22125,.T.);
#36939=EDGE_CURVE('',#30286,#30179,#24863,.T.);
#36940=EDGE_CURVE('',#30288,#30286,#22126,.T.);
#36941=EDGE_CURVE('',#30289,#30288,#17267,.T.);
#36942=EDGE_CURVE('',#30287,#30289,#17268,.T.);
#36943=EDGE_CURVE('',#30180,#30289,#24864,.T.);
#36944=EDGE_CURVE('',#30290,#30291,#17269,.T.);
#36945=EDGE_CURVE('',#29895,#30291,#22127,.T.);
#36946=EDGE_CURVE('',#30290,#30180,#24865,.T.);
#36947=EDGE_CURVE('',#30292,#30290,#22128,.T.);
#36948=EDGE_CURVE('',#30293,#30292,#17270,.T.);
#36949=EDGE_CURVE('',#30291,#30293,#17271,.T.);
#36950=EDGE_CURVE('',#30181,#30293,#24866,.T.);
#36951=EDGE_CURVE('',#30294,#30295,#17272,.T.);
#36952=EDGE_CURVE('',#29896,#30295,#22129,.T.);
#36953=EDGE_CURVE('',#30294,#30181,#24867,.T.);
#36954=EDGE_CURVE('',#30296,#30294,#22130,.T.);
#36955=EDGE_CURVE('',#30297,#30296,#17273,.T.);
#36956=EDGE_CURVE('',#30295,#30297,#17274,.T.);
#36957=EDGE_CURVE('',#30182,#30297,#24868,.T.);
#36958=EDGE_CURVE('',#30298,#30299,#17275,.T.);
#36959=EDGE_CURVE('',#29897,#30299,#22131,.T.);
#36960=EDGE_CURVE('',#30298,#30182,#24869,.T.);
#36961=EDGE_CURVE('',#30300,#30298,#22132,.T.);
#36962=EDGE_CURVE('',#30301,#30300,#17276,.T.);
#36963=EDGE_CURVE('',#30299,#30301,#17277,.T.);
#36964=EDGE_CURVE('',#30183,#30301,#24870,.T.);
#36965=EDGE_CURVE('',#30302,#30303,#17278,.T.);
#36966=EDGE_CURVE('',#29898,#30303,#22133,.T.);
#36967=EDGE_CURVE('',#30302,#30183,#24871,.T.);
#36968=EDGE_CURVE('',#30304,#30302,#22134,.T.);
#36969=EDGE_CURVE('',#30305,#30304,#17279,.T.);
#36970=EDGE_CURVE('',#30303,#30305,#17280,.T.);
#36971=EDGE_CURVE('',#30184,#30305,#24872,.T.);
#36972=EDGE_CURVE('',#30306,#30307,#17281,.T.);
#36973=EDGE_CURVE('',#29899,#30307,#22135,.T.);
#36974=EDGE_CURVE('',#30306,#30184,#24873,.T.);
#36975=EDGE_CURVE('',#30307,#30308,#17282,.T.);
#36976=EDGE_CURVE('',#30185,#30308,#24874,.T.);
#36977=EDGE_CURVE('',#30309,#30306,#22136,.T.);
#36978=EDGE_CURVE('',#30308,#30309,#17283,.T.);
#36979=EDGE_CURVE('',#30310,#30185,#24875,.T.);
#36980=EDGE_CURVE('',#30310,#30311,#17284,.T.);
#36981=EDGE_CURVE('',#29900,#30311,#22137,.T.);
#36982=EDGE_CURVE('',#30311,#30312,#17285,.T.);
#36983=EDGE_CURVE('',#30313,#30310,#22138,.T.);
#36984=EDGE_CURVE('',#30312,#30313,#17286,.T.);
#36985=EDGE_CURVE('',#30186,#30312,#24876,.T.);
#36986=EDGE_CURVE('',#30314,#30315,#17287,.T.);
#36987=EDGE_CURVE('',#29901,#30315,#22139,.T.);
#36988=EDGE_CURVE('',#30314,#30186,#24877,.T.);
#36989=EDGE_CURVE('',#30316,#30314,#22140,.T.);
#36990=EDGE_CURVE('',#30317,#30316,#17288,.T.);
#36991=EDGE_CURVE('',#30315,#30317,#17289,.T.);
#36992=EDGE_CURVE('',#30187,#30317,#24878,.T.);
#36993=EDGE_CURVE('',#30318,#30319,#17290,.T.);
#36994=EDGE_CURVE('',#29902,#30319,#22141,.T.);
#36995=EDGE_CURVE('',#30318,#30187,#24879,.T.);
#36996=EDGE_CURVE('',#30320,#30318,#22142,.T.);
#36997=EDGE_CURVE('',#30321,#30320,#17291,.T.);
#36998=EDGE_CURVE('',#30319,#30321,#17292,.T.);
#36999=EDGE_CURVE('',#30188,#30321,#24880,.T.);
#37000=EDGE_CURVE('',#30322,#30323,#17293,.T.);
#37001=EDGE_CURVE('',#29903,#30323,#22143,.T.);
#37002=EDGE_CURVE('',#30322,#30188,#24881,.T.);
#37003=EDGE_CURVE('',#30324,#30322,#22144,.T.);
#37004=EDGE_CURVE('',#30325,#30324,#17294,.T.);
#37005=EDGE_CURVE('',#30323,#30325,#17295,.T.);
#37006=EDGE_CURVE('',#30189,#30325,#24882,.T.);
#37007=EDGE_CURVE('',#30326,#30327,#17296,.T.);
#37008=EDGE_CURVE('',#29904,#30327,#22145,.T.);
#37009=EDGE_CURVE('',#30326,#30189,#24883,.T.);
#37010=EDGE_CURVE('',#30328,#30326,#22146,.T.);
#37011=EDGE_CURVE('',#30329,#30328,#17297,.T.);
#37012=EDGE_CURVE('',#30327,#30329,#17298,.T.);
#37013=EDGE_CURVE('',#30190,#30329,#24884,.T.);
#37014=EDGE_CURVE('',#30330,#30331,#22147,.T.);
#37015=EDGE_CURVE('',#30221,#30330,#17299,.T.);
#37016=EDGE_CURVE('',#30331,#30220,#17300,.T.);
#37017=EDGE_CURVE('',#30331,#30190,#24885,.T.);
#37018=EDGE_CURVE('',#30332,#30333,#17301,.T.);
#37019=EDGE_CURVE('',#30191,#30333,#24886,.T.);
#37020=EDGE_CURVE('',#30332,#29905,#22148,.T.);
#37021=EDGE_CURVE('',#30334,#30191,#24887,.T.);
#37022=EDGE_CURVE('',#30334,#30335,#17302,.T.);
#37023=EDGE_CURVE('',#29906,#30335,#22149,.T.);
#37024=EDGE_CURVE('',#30335,#30336,#17303,.T.);
#37025=EDGE_CURVE('',#30192,#30336,#24888,.T.);
#37026=EDGE_CURVE('',#30337,#30334,#17304,.T.);
#37027=EDGE_CURVE('',#30336,#30337,#17305,.T.);
#37028=EDGE_CURVE('',#30338,#30192,#24889,.T.);
#37029=EDGE_CURVE('',#30338,#30339,#17306,.T.);
#37030=EDGE_CURVE('',#29907,#30339,#22150,.T.);
#37031=EDGE_CURVE('',#30339,#30340,#17307,.T.);
#37032=EDGE_CURVE('',#30193,#30340,#24890,.T.);
#37033=EDGE_CURVE('',#30341,#30338,#17308,.T.);
#37034=EDGE_CURVE('',#30340,#30341,#17309,.T.);
#37035=EDGE_CURVE('',#30342,#30193,#24891,.T.);
#37036=EDGE_CURVE('',#30342,#30343,#17310,.T.);
#37037=EDGE_CURVE('',#29908,#30343,#22151,.T.);
#37038=EDGE_CURVE('',#30343,#30344,#17311,.T.);
#37039=EDGE_CURVE('',#30194,#30344,#24892,.T.);
#37040=EDGE_CURVE('',#30345,#30342,#17312,.T.);
#37041=EDGE_CURVE('',#30344,#30345,#17313,.T.);
#37042=EDGE_CURVE('',#30346,#30194,#24893,.T.);
#37043=EDGE_CURVE('',#30346,#30347,#17314,.T.);
#37044=EDGE_CURVE('',#29909,#30347,#22152,.T.);
#37045=EDGE_CURVE('',#30347,#30348,#17315,.T.);
#37046=EDGE_CURVE('',#30195,#30348,#24894,.T.);
#37047=EDGE_CURVE('',#30349,#30346,#17316,.T.);
#37048=EDGE_CURVE('',#30348,#30349,#17317,.T.);
#37049=EDGE_CURVE('',#30350,#30195,#24895,.T.);
#37050=EDGE_CURVE('',#30350,#30351,#17318,.T.);
#37051=EDGE_CURVE('',#29910,#30351,#22153,.T.);
#37052=EDGE_CURVE('',#30351,#30352,#17319,.T.);
#37053=EDGE_CURVE('',#30196,#30352,#24896,.T.);
#37054=EDGE_CURVE('',#30353,#30350,#17320,.T.);
#37055=EDGE_CURVE('',#30352,#30353,#17321,.T.);
#37056=EDGE_CURVE('',#30354,#30196,#24897,.T.);
#37057=EDGE_CURVE('',#30354,#30355,#17322,.T.);
#37058=EDGE_CURVE('',#29911,#30355,#22154,.T.);
#37059=EDGE_CURVE('',#30355,#30356,#17323,.T.);
#37060=EDGE_CURVE('',#30197,#30356,#24898,.T.);
#37061=EDGE_CURVE('',#30357,#30354,#17324,.T.);
#37062=EDGE_CURVE('',#30356,#30357,#17325,.T.);
#37063=EDGE_CURVE('',#30358,#30197,#24899,.T.);
#37064=EDGE_CURVE('',#30358,#30359,#17326,.T.);
#37065=EDGE_CURVE('',#29912,#30359,#22155,.T.);
#37066=EDGE_CURVE('',#30359,#30360,#17327,.T.);
#37067=EDGE_CURVE('',#30198,#30360,#24900,.T.);
#37068=EDGE_CURVE('',#30361,#30358,#17328,.T.);
#37069=EDGE_CURVE('',#30360,#30361,#17329,.T.);
#37070=EDGE_CURVE('',#30362,#30198,#24901,.T.);
#37071=EDGE_CURVE('',#30362,#30363,#17330,.T.);
#37072=EDGE_CURVE('',#29913,#30363,#22156,.T.);
#37073=EDGE_CURVE('',#30363,#30364,#17331,.T.);
#37074=EDGE_CURVE('',#30199,#30364,#24902,.T.);
#37075=EDGE_CURVE('',#30365,#30362,#17332,.T.);
#37076=EDGE_CURVE('',#30364,#30365,#17333,.T.);
#37077=EDGE_CURVE('',#30366,#30199,#24903,.T.);
#37078=EDGE_CURVE('',#30366,#30367,#17334,.T.);
#37079=EDGE_CURVE('',#29914,#30367,#22157,.T.);
#37080=EDGE_CURVE('',#30367,#30368,#17335,.T.);
#37081=EDGE_CURVE('',#30200,#30368,#24904,.T.);
#37082=EDGE_CURVE('',#30369,#30366,#17336,.T.);
#37083=EDGE_CURVE('',#30368,#30369,#17337,.T.);
#37084=EDGE_CURVE('',#30370,#30200,#24905,.T.);
#37085=EDGE_CURVE('',#30370,#30371,#17338,.T.);
#37086=EDGE_CURVE('',#29915,#30371,#22158,.T.);
#37087=EDGE_CURVE('',#30371,#30372,#17339,.T.);
#37088=EDGE_CURVE('',#30201,#30372,#24906,.T.);
#37089=EDGE_CURVE('',#30373,#30370,#17340,.T.);
#37090=EDGE_CURVE('',#30372,#30373,#17341,.T.);
#37091=EDGE_CURVE('',#30374,#30201,#24907,.T.);
#37092=EDGE_CURVE('',#30374,#30375,#17342,.T.);
#37093=EDGE_CURVE('',#29916,#30375,#22159,.T.);
#37094=EDGE_CURVE('',#30375,#30376,#17343,.T.);
#37095=EDGE_CURVE('',#30202,#30376,#24908,.T.);
#37096=EDGE_CURVE('',#30377,#30374,#17344,.T.);
#37097=EDGE_CURVE('',#30376,#30377,#17345,.T.);
#37098=EDGE_CURVE('',#30378,#30202,#24909,.T.);
#37099=EDGE_CURVE('',#30378,#30379,#17346,.T.);
#37100=EDGE_CURVE('',#29917,#30379,#22160,.T.);
#37101=EDGE_CURVE('',#30379,#30380,#17347,.T.);
#37102=EDGE_CURVE('',#30203,#30380,#24910,.T.);
#37103=EDGE_CURVE('',#30381,#30378,#17348,.T.);
#37104=EDGE_CURVE('',#30380,#30381,#17349,.T.);
#37105=EDGE_CURVE('',#30382,#30203,#24911,.T.);
#37106=EDGE_CURVE('',#30382,#30383,#17350,.T.);
#37107=EDGE_CURVE('',#29918,#30383,#22161,.T.);
#37108=EDGE_CURVE('',#30383,#30384,#17351,.T.);
#37109=EDGE_CURVE('',#30204,#30384,#24912,.T.);
#37110=EDGE_CURVE('',#30385,#30382,#17352,.T.);
#37111=EDGE_CURVE('',#30384,#30385,#17353,.T.);
#37112=EDGE_CURVE('',#28997,#30204,#24913,.T.);
#37113=EDGE_CURVE('',#29919,#28996,#22162,.T.);
#37114=EDGE_CURVE('',#30205,#28994,#24914,.T.);
#37115=EDGE_CURVE('',#30386,#30205,#24915,.T.);
#37116=EDGE_CURVE('',#30386,#30387,#17354,.T.);
#37117=EDGE_CURVE('',#29920,#30387,#22163,.T.);
#37118=EDGE_CURVE('',#30387,#30388,#17355,.T.);
#37119=EDGE_CURVE('',#30206,#30388,#24916,.T.);
#37120=EDGE_CURVE('',#30389,#30386,#17356,.T.);
#37121=EDGE_CURVE('',#30388,#30389,#17357,.T.);
#37122=EDGE_CURVE('',#30390,#30206,#24917,.T.);
#37123=EDGE_CURVE('',#30390,#30391,#17358,.T.);
#37124=EDGE_CURVE('',#29921,#30391,#22164,.T.);
#37125=EDGE_CURVE('',#30391,#30392,#17359,.T.);
#37126=EDGE_CURVE('',#30207,#30392,#24918,.T.);
#37127=EDGE_CURVE('',#30393,#30390,#17360,.T.);
#37128=EDGE_CURVE('',#30392,#30393,#17361,.T.);
#37129=EDGE_CURVE('',#30394,#30207,#24919,.T.);
#37130=EDGE_CURVE('',#30394,#30395,#17362,.T.);
#37131=EDGE_CURVE('',#29922,#30395,#22165,.T.);
#37132=EDGE_CURVE('',#30395,#30396,#17363,.T.);
#37133=EDGE_CURVE('',#30208,#30396,#24920,.T.);
#37134=EDGE_CURVE('',#30397,#30394,#17364,.T.);
#37135=EDGE_CURVE('',#30396,#30397,#17365,.T.);
#37136=EDGE_CURVE('',#30398,#30208,#24921,.T.);
#37137=EDGE_CURVE('',#30398,#30399,#17366,.T.);
#37138=EDGE_CURVE('',#29923,#30399,#22166,.T.);
#37139=EDGE_CURVE('',#30399,#30400,#17367,.T.);
#37140=EDGE_CURVE('',#30209,#30400,#24922,.T.);
#37141=EDGE_CURVE('',#30401,#30398,#17368,.T.);
#37142=EDGE_CURVE('',#30400,#30401,#17369,.T.);
#37143=EDGE_CURVE('',#30402,#30209,#24923,.T.);
#37144=EDGE_CURVE('',#30402,#30403,#17370,.T.);
#37145=EDGE_CURVE('',#29924,#30403,#22167,.T.);
#37146=EDGE_CURVE('',#30403,#30404,#17371,.T.);
#37147=EDGE_CURVE('',#30210,#30404,#24924,.T.);
#37148=EDGE_CURVE('',#30405,#30402,#17372,.T.);
#37149=EDGE_CURVE('',#30404,#30405,#17373,.T.);
#37150=EDGE_CURVE('',#30406,#30210,#24925,.T.);
#37151=EDGE_CURVE('',#30406,#30407,#17374,.T.);
#37152=EDGE_CURVE('',#29925,#30407,#22168,.T.);
#37153=EDGE_CURVE('',#30407,#30408,#17375,.T.);
#37154=EDGE_CURVE('',#30211,#30408,#24926,.T.);
#37155=EDGE_CURVE('',#30409,#30406,#17376,.T.);
#37156=EDGE_CURVE('',#30408,#30409,#17377,.T.);
#37157=EDGE_CURVE('',#30410,#30211,#24927,.T.);
#37158=EDGE_CURVE('',#30410,#30411,#17378,.T.);
#37159=EDGE_CURVE('',#29926,#30411,#22169,.T.);
#37160=EDGE_CURVE('',#30411,#30412,#17379,.T.);
#37161=EDGE_CURVE('',#30212,#30412,#24928,.T.);
#37162=EDGE_CURVE('',#30413,#30410,#17380,.T.);
#37163=EDGE_CURVE('',#30412,#30413,#17381,.T.);
#37164=EDGE_CURVE('',#30414,#30212,#24929,.T.);
#37165=EDGE_CURVE('',#30414,#30415,#17382,.T.);
#37166=EDGE_CURVE('',#29927,#30415,#22170,.T.);
#37167=EDGE_CURVE('',#30415,#30416,#17383,.T.);
#37168=EDGE_CURVE('',#30213,#30416,#24930,.T.);
#37169=EDGE_CURVE('',#30417,#30414,#17384,.T.);
#37170=EDGE_CURVE('',#30416,#30417,#17385,.T.);
#37171=EDGE_CURVE('',#30418,#30213,#24931,.T.);
#37172=EDGE_CURVE('',#30418,#30419,#17386,.T.);
#37173=EDGE_CURVE('',#29928,#30419,#22171,.T.);
#37174=EDGE_CURVE('',#30419,#30420,#17387,.T.);
#37175=EDGE_CURVE('',#30214,#30420,#24932,.T.);
#37176=EDGE_CURVE('',#30421,#30418,#17388,.T.);
#37177=EDGE_CURVE('',#30420,#30421,#17389,.T.);
#37178=EDGE_CURVE('',#30422,#30214,#24933,.T.);
#37179=EDGE_CURVE('',#30422,#30423,#17390,.T.);
#37180=EDGE_CURVE('',#29929,#30423,#22172,.T.);
#37181=EDGE_CURVE('',#30423,#30424,#17391,.T.);
#37182=EDGE_CURVE('',#30215,#30424,#24934,.T.);
#37183=EDGE_CURVE('',#30425,#30422,#17392,.T.);
#37184=EDGE_CURVE('',#30424,#30425,#17393,.T.);
#37185=EDGE_CURVE('',#30426,#30215,#24935,.T.);
#37186=EDGE_CURVE('',#30426,#30427,#17394,.T.);
#37187=EDGE_CURVE('',#29930,#30427,#22173,.T.);
#37188=EDGE_CURVE('',#30427,#30428,#17395,.T.);
#37189=EDGE_CURVE('',#30216,#30428,#24936,.T.);
#37190=EDGE_CURVE('',#30429,#30426,#17396,.T.);
#37191=EDGE_CURVE('',#30428,#30429,#17397,.T.);
#37192=EDGE_CURVE('',#30430,#30216,#24937,.T.);
#37193=EDGE_CURVE('',#30430,#30431,#17398,.T.);
#37194=EDGE_CURVE('',#29931,#30431,#22174,.T.);
#37195=EDGE_CURVE('',#30431,#30432,#17399,.T.);
#37196=EDGE_CURVE('',#30217,#30432,#24938,.T.);
#37197=EDGE_CURVE('',#30433,#30430,#17400,.T.);
#37198=EDGE_CURVE('',#30432,#30433,#17401,.T.);
#37199=EDGE_CURVE('',#30434,#30217,#24939,.T.);
#37200=EDGE_CURVE('',#30434,#30435,#17402,.T.);
#37201=EDGE_CURVE('',#29932,#30435,#22175,.T.);
#37202=EDGE_CURVE('',#30435,#30436,#17403,.T.);
#37203=EDGE_CURVE('',#30218,#30436,#24940,.T.);
#37204=EDGE_CURVE('',#30437,#30434,#17404,.T.);
#37205=EDGE_CURVE('',#30436,#30437,#17405,.T.);
#37206=EDGE_CURVE('',#30438,#30218,#24941,.T.);
#37207=EDGE_CURVE('',#30438,#30439,#17406,.T.);
#37208=EDGE_CURVE('',#29933,#30439,#22176,.T.);
#37209=EDGE_CURVE('',#30439,#30440,#17407,.T.);
#37210=EDGE_CURVE('',#30219,#30440,#24942,.T.);
#37211=EDGE_CURVE('',#30441,#30438,#17408,.T.);
#37212=EDGE_CURVE('',#30440,#30441,#17409,.T.);
#37213=EDGE_CURVE('',#30442,#30443,#17410,.T.);
#37214=EDGE_CURVE('',#30333,#30442,#17411,.T.);
#37215=EDGE_CURVE('',#30443,#30332,#17412,.T.);
#37216=EDGE_CURVE('',#30443,#30219,#24943,.T.);
#37217=EDGE_CURVE('',#30162,#30444,#17413,.T.);
#37218=EDGE_CURVE('',#30444,#30330,#22177,.T.);
#37219=EDGE_CURVE('',#30445,#30162,#22178,.T.);
#37220=EDGE_CURVE('',#30224,#30445,#22179,.T.);
#37221=EDGE_CURVE('',#30163,#30445,#17414,.T.);
#37222=EDGE_CURVE('',#30446,#30163,#22180,.T.);
#37223=EDGE_CURVE('',#30228,#30446,#22181,.T.);
#37224=EDGE_CURVE('',#30164,#30446,#17415,.T.);
#37225=EDGE_CURVE('',#30447,#30164,#22182,.T.);
#37226=EDGE_CURVE('',#30232,#30447,#22183,.T.);
#37227=EDGE_CURVE('',#30165,#30447,#17416,.T.);
#37228=EDGE_CURVE('',#30448,#30165,#22184,.T.);
#37229=EDGE_CURVE('',#30236,#30448,#22185,.T.);
#37230=EDGE_CURVE('',#30166,#30448,#17417,.T.);
#37231=EDGE_CURVE('',#30449,#30166,#22186,.T.);
#37232=EDGE_CURVE('',#30240,#30449,#22187,.T.);
#37233=EDGE_CURVE('',#30167,#30449,#17418,.T.);
#37234=EDGE_CURVE('',#30450,#30167,#22188,.T.);
#37235=EDGE_CURVE('',#30244,#30450,#22189,.T.);
#37236=EDGE_CURVE('',#30168,#30450,#17419,.T.);
#37237=EDGE_CURVE('',#30451,#30168,#22190,.T.);
#37238=EDGE_CURVE('',#29001,#30451,#22191,.T.);
#37239=EDGE_CURVE('',#30169,#30451,#17420,.T.);
#37240=EDGE_CURVE('',#30452,#30169,#22192,.T.);
#37241=EDGE_CURVE('',#30248,#30452,#22193,.T.);
#37242=EDGE_CURVE('',#30170,#30452,#17421,.T.);
#37243=EDGE_CURVE('',#30453,#30170,#22194,.T.);
#37244=EDGE_CURVE('',#30252,#30453,#22195,.T.);
#37245=EDGE_CURVE('',#30171,#30453,#17422,.T.);
#37246=EDGE_CURVE('',#30454,#30171,#22196,.T.);
#37247=EDGE_CURVE('',#30256,#30454,#22197,.T.);
#37248=EDGE_CURVE('',#30172,#30454,#17423,.T.);
#37249=EDGE_CURVE('',#30455,#30172,#22198,.T.);
#37250=EDGE_CURVE('',#30260,#30455,#22199,.T.);
#37251=EDGE_CURVE('',#30173,#30455,#17424,.T.);
#37252=EDGE_CURVE('',#30456,#30173,#22200,.T.);
#37253=EDGE_CURVE('',#30264,#30456,#22201,.T.);
#37254=EDGE_CURVE('',#30174,#30456,#17425,.T.);
#37255=EDGE_CURVE('',#30457,#30174,#22202,.T.);
#37256=EDGE_CURVE('',#30268,#30457,#22203,.T.);
#37257=EDGE_CURVE('',#30175,#30457,#17426,.T.);
#37258=EDGE_CURVE('',#30458,#30175,#22204,.T.);
#37259=EDGE_CURVE('',#30272,#30458,#22205,.T.);
#37260=EDGE_CURVE('',#30176,#30458,#17427,.T.);
#37261=EDGE_CURVE('',#30459,#30176,#22206,.T.);
#37262=EDGE_CURVE('',#30276,#30459,#22207,.T.);
#37263=EDGE_CURVE('',#30177,#30459,#17428,.T.);
#37264=EDGE_CURVE('',#30460,#30177,#22208,.T.);
#37265=EDGE_CURVE('',#30280,#30460,#22209,.T.);
#37266=EDGE_CURVE('',#30178,#30460,#17429,.T.);
#37267=EDGE_CURVE('',#30461,#30178,#22210,.T.);
#37268=EDGE_CURVE('',#30284,#30461,#22211,.T.);
#37269=EDGE_CURVE('',#30179,#30461,#17430,.T.);
#37270=EDGE_CURVE('',#30462,#30179,#22212,.T.);
#37271=EDGE_CURVE('',#30288,#30462,#22213,.T.);
#37272=EDGE_CURVE('',#30180,#30462,#17431,.T.);
#37273=EDGE_CURVE('',#30463,#30180,#22214,.T.);
#37274=EDGE_CURVE('',#30292,#30463,#22215,.T.);
#37275=EDGE_CURVE('',#30181,#30463,#17432,.T.);
#37276=EDGE_CURVE('',#30464,#30181,#22216,.T.);
#37277=EDGE_CURVE('',#30296,#30464,#22217,.T.);
#37278=EDGE_CURVE('',#30182,#30464,#17433,.T.);
#37279=EDGE_CURVE('',#30465,#30182,#22218,.T.);
#37280=EDGE_CURVE('',#30300,#30465,#22219,.T.);
#37281=EDGE_CURVE('',#30183,#30465,#17434,.T.);
#37282=EDGE_CURVE('',#30466,#30183,#22220,.T.);
#37283=EDGE_CURVE('',#30304,#30466,#22221,.T.);
#37284=EDGE_CURVE('',#30184,#30466,#17435,.T.);
#37285=EDGE_CURVE('',#30467,#30184,#22222,.T.);
#37286=EDGE_CURVE('',#30309,#30467,#22223,.T.);
#37287=EDGE_CURVE('',#30185,#30467,#17436,.T.);
#37288=EDGE_CURVE('',#30468,#30185,#22224,.T.);
#37289=EDGE_CURVE('',#30313,#30468,#22225,.T.);
#37290=EDGE_CURVE('',#30186,#30468,#17437,.T.);
#37291=EDGE_CURVE('',#30469,#30186,#22226,.T.);
#37292=EDGE_CURVE('',#30316,#30469,#22227,.T.);
#37293=EDGE_CURVE('',#30187,#30469,#17438,.T.);
#37294=EDGE_CURVE('',#30470,#30187,#22228,.T.);
#37295=EDGE_CURVE('',#30320,#30470,#22229,.T.);
#37296=EDGE_CURVE('',#30188,#30470,#17439,.T.);
#37297=EDGE_CURVE('',#30471,#30188,#22230,.T.);
#37298=EDGE_CURVE('',#30324,#30471,#22231,.T.);
#37299=EDGE_CURVE('',#30189,#30471,#17440,.T.);
#37300=EDGE_CURVE('',#30472,#30189,#22232,.T.);
#37301=EDGE_CURVE('',#30328,#30472,#22233,.T.);
#37302=EDGE_CURVE('',#30190,#30472,#17441,.T.);
#37303=EDGE_CURVE('',#30444,#30190,#22234,.T.);
#37304=EDGE_CURVE('',#30473,#30442,#22235,.T.);
#37305=EDGE_CURVE('',#30191,#30473,#17442,.T.);
#37306=EDGE_CURVE('',#30474,#30191,#17443,.T.);
#37307=EDGE_CURVE('',#30337,#30474,#22236,.T.);
#37308=EDGE_CURVE('',#30192,#30474,#17444,.T.);
#37309=EDGE_CURVE('',#30475,#30192,#17445,.T.);
#37310=EDGE_CURVE('',#30341,#30475,#22237,.T.);
#37311=EDGE_CURVE('',#30193,#30475,#17446,.T.);
#37312=EDGE_CURVE('',#30476,#30193,#17447,.T.);
#37313=EDGE_CURVE('',#30345,#30476,#22238,.T.);
#37314=EDGE_CURVE('',#30194,#30476,#17448,.T.);
#37315=EDGE_CURVE('',#30477,#30194,#17449,.T.);
#37316=EDGE_CURVE('',#30349,#30477,#22239,.T.);
#37317=EDGE_CURVE('',#30195,#30477,#17450,.T.);
#37318=EDGE_CURVE('',#30478,#30195,#17451,.T.);
#37319=EDGE_CURVE('',#30353,#30478,#22240,.T.);
#37320=EDGE_CURVE('',#30196,#30478,#17452,.T.);
#37321=EDGE_CURVE('',#30479,#30196,#17453,.T.);
#37322=EDGE_CURVE('',#30357,#30479,#22241,.T.);
#37323=EDGE_CURVE('',#30197,#30479,#17454,.T.);
#37324=EDGE_CURVE('',#30480,#30197,#17455,.T.);
#37325=EDGE_CURVE('',#30361,#30480,#22242,.T.);
#37326=EDGE_CURVE('',#30198,#30480,#17456,.T.);
#37327=EDGE_CURVE('',#30481,#30198,#17457,.T.);
#37328=EDGE_CURVE('',#30365,#30481,#22243,.T.);
#37329=EDGE_CURVE('',#30199,#30481,#17458,.T.);
#37330=EDGE_CURVE('',#30482,#30199,#17459,.T.);
#37331=EDGE_CURVE('',#30369,#30482,#22244,.T.);
#37332=EDGE_CURVE('',#30200,#30482,#17460,.T.);
#37333=EDGE_CURVE('',#30483,#30200,#17461,.T.);
#37334=EDGE_CURVE('',#30373,#30483,#22245,.T.);
#37335=EDGE_CURVE('',#30201,#30483,#17462,.T.);
#37336=EDGE_CURVE('',#30484,#30201,#17463,.T.);
#37337=EDGE_CURVE('',#30377,#30484,#22246,.T.);
#37338=EDGE_CURVE('',#30202,#30484,#17464,.T.);
#37339=EDGE_CURVE('',#30485,#30202,#17465,.T.);
#37340=EDGE_CURVE('',#30381,#30485,#22247,.T.);
#37341=EDGE_CURVE('',#30203,#30485,#17466,.T.);
#37342=EDGE_CURVE('',#30486,#30203,#17467,.T.);
#37343=EDGE_CURVE('',#30385,#30486,#22248,.T.);
#37344=EDGE_CURVE('',#30204,#30486,#17468,.T.);
#37345=EDGE_CURVE('',#30487,#30204,#17469,.T.);
#37346=EDGE_CURVE('',#28995,#30487,#22249,.T.);
#37347=EDGE_CURVE('',#30205,#30487,#17470,.T.);
#37348=EDGE_CURVE('',#30488,#30205,#17471,.T.);
#37349=EDGE_CURVE('',#30389,#30488,#22250,.T.);
#37350=EDGE_CURVE('',#30206,#30488,#17472,.T.);
#37351=EDGE_CURVE('',#30489,#30206,#17473,.T.);
#37352=EDGE_CURVE('',#30393,#30489,#22251,.T.);
#37353=EDGE_CURVE('',#30207,#30489,#17474,.T.);
#37354=EDGE_CURVE('',#30490,#30207,#17475,.T.);
#37355=EDGE_CURVE('',#30397,#30490,#22252,.T.);
#37356=EDGE_CURVE('',#30208,#30490,#17476,.T.);
#37357=EDGE_CURVE('',#30491,#30208,#17477,.T.);
#37358=EDGE_CURVE('',#30401,#30491,#22253,.T.);
#37359=EDGE_CURVE('',#30209,#30491,#17478,.T.);
#37360=EDGE_CURVE('',#30492,#30209,#17479,.T.);
#37361=EDGE_CURVE('',#30405,#30492,#22254,.T.);
#37362=EDGE_CURVE('',#30210,#30492,#17480,.T.);
#37363=EDGE_CURVE('',#30493,#30210,#17481,.T.);
#37364=EDGE_CURVE('',#30409,#30493,#22255,.T.);
#37365=EDGE_CURVE('',#30211,#30493,#17482,.T.);
#37366=EDGE_CURVE('',#30494,#30211,#17483,.T.);
#37367=EDGE_CURVE('',#30413,#30494,#22256,.T.);
#37368=EDGE_CURVE('',#30212,#30494,#17484,.T.);
#37369=EDGE_CURVE('',#30495,#30212,#17485,.T.);
#37370=EDGE_CURVE('',#30417,#30495,#22257,.T.);
#37371=EDGE_CURVE('',#30213,#30495,#17486,.T.);
#37372=EDGE_CURVE('',#30496,#30213,#17487,.T.);
#37373=EDGE_CURVE('',#30421,#30496,#22258,.T.);
#37374=EDGE_CURVE('',#30214,#30496,#17488,.T.);
#37375=EDGE_CURVE('',#30497,#30214,#17489,.T.);
#37376=EDGE_CURVE('',#30425,#30497,#22259,.T.);
#37377=EDGE_CURVE('',#30215,#30497,#17490,.T.);
#37378=EDGE_CURVE('',#30498,#30215,#17491,.T.);
#37379=EDGE_CURVE('',#30429,#30498,#22260,.T.);
#37380=EDGE_CURVE('',#30216,#30498,#17492,.T.);
#37381=EDGE_CURVE('',#30499,#30216,#17493,.T.);
#37382=EDGE_CURVE('',#30433,#30499,#22261,.T.);
#37383=EDGE_CURVE('',#30217,#30499,#17494,.T.);
#37384=EDGE_CURVE('',#30500,#30217,#17495,.T.);
#37385=EDGE_CURVE('',#30437,#30500,#22262,.T.);
#37386=EDGE_CURVE('',#30218,#30500,#17496,.T.);
#37387=EDGE_CURVE('',#30501,#30218,#17497,.T.);
#37388=EDGE_CURVE('',#30441,#30501,#22263,.T.);
#37389=EDGE_CURVE('',#30219,#30501,#17498,.T.);
#37390=EDGE_CURVE('',#30473,#30219,#17499,.T.);
#37391=EDGE_CURVE('',#30502,#30503,#17500,.T.);
#37392=EDGE_CURVE('',#30162,#30503,#22264,.T.);
#37393=EDGE_CURVE('',#30502,#30444,#24944,.T.);
#37394=EDGE_CURVE('',#30504,#30502,#17501,.T.);
#37395=EDGE_CURVE('',#30505,#30504,#17502,.T.);
#37396=EDGE_CURVE('',#30503,#30505,#22265,.T.);
#37397=EDGE_CURVE('',#30445,#30505,#24945,.T.);
#37398=EDGE_CURVE('',#30506,#30507,#17503,.T.);
#37399=EDGE_CURVE('',#30163,#30507,#22266,.T.);
#37400=EDGE_CURVE('',#30506,#30445,#24946,.T.);
#37401=EDGE_CURVE('',#30508,#30506,#17504,.T.);
#37402=EDGE_CURVE('',#30509,#30508,#17505,.T.);
#37403=EDGE_CURVE('',#30507,#30509,#22267,.T.);
#37404=EDGE_CURVE('',#30446,#30509,#24947,.T.);
#37405=EDGE_CURVE('',#30510,#30511,#17506,.T.);
#37406=EDGE_CURVE('',#30164,#30511,#22268,.T.);
#37407=EDGE_CURVE('',#30510,#30446,#24948,.T.);
#37408=EDGE_CURVE('',#30512,#30510,#17507,.T.);
#37409=EDGE_CURVE('',#30513,#30512,#17508,.T.);
#37410=EDGE_CURVE('',#30511,#30513,#22269,.T.);
#37411=EDGE_CURVE('',#30447,#30513,#24949,.T.);
#37412=EDGE_CURVE('',#30514,#30515,#17509,.T.);
#37413=EDGE_CURVE('',#30165,#30515,#22270,.T.);
#37414=EDGE_CURVE('',#30514,#30447,#24950,.T.);
#37415=EDGE_CURVE('',#30516,#30514,#17510,.T.);
#37416=EDGE_CURVE('',#30517,#30516,#17511,.T.);
#37417=EDGE_CURVE('',#30515,#30517,#22271,.T.);
#37418=EDGE_CURVE('',#30448,#30517,#24951,.T.);
#37419=EDGE_CURVE('',#30518,#30519,#17512,.T.);
#37420=EDGE_CURVE('',#30166,#30519,#22272,.T.);
#37421=EDGE_CURVE('',#30518,#30448,#24952,.T.);
#37422=EDGE_CURVE('',#30520,#30518,#17513,.T.);
#37423=EDGE_CURVE('',#30521,#30520,#17514,.T.);
#37424=EDGE_CURVE('',#30519,#30521,#22273,.T.);
#37425=EDGE_CURVE('',#30449,#30521,#24953,.T.);
#37426=EDGE_CURVE('',#30522,#30523,#17515,.T.);
#37427=EDGE_CURVE('',#30167,#30523,#22274,.T.);
#37428=EDGE_CURVE('',#30522,#30449,#24954,.T.);
#37429=EDGE_CURVE('',#30524,#30522,#17516,.T.);
#37430=EDGE_CURVE('',#30525,#30524,#17517,.T.);
#37431=EDGE_CURVE('',#30523,#30525,#22275,.T.);
#37432=EDGE_CURVE('',#30450,#30525,#24955,.T.);
#37433=EDGE_CURVE('',#30526,#30527,#17518,.T.);
#37434=EDGE_CURVE('',#30168,#30527,#22276,.T.);
#37435=EDGE_CURVE('',#30526,#30450,#24956,.T.);
#37436=EDGE_CURVE('',#30528,#30526,#17519,.T.);
#37437=EDGE_CURVE('',#30529,#30528,#17520,.T.);
#37438=EDGE_CURVE('',#30527,#30529,#22277,.T.);
#37439=EDGE_CURVE('',#30451,#30529,#24957,.T.);
#37440=EDGE_CURVE('',#30530,#30531,#17521,.T.);
#37441=EDGE_CURVE('',#30169,#30531,#22278,.T.);
#37442=EDGE_CURVE('',#30530,#30451,#24958,.T.);
#37443=EDGE_CURVE('',#30532,#30530,#17522,.T.);
#37444=EDGE_CURVE('',#30533,#30532,#17523,.T.);
#37445=EDGE_CURVE('',#30531,#30533,#22279,.T.);
#37446=EDGE_CURVE('',#30452,#30533,#24959,.T.);
#37447=EDGE_CURVE('',#30534,#30535,#17524,.T.);
#37448=EDGE_CURVE('',#30170,#30535,#22280,.T.);
#37449=EDGE_CURVE('',#30534,#30452,#24960,.T.);
#37450=EDGE_CURVE('',#30536,#30534,#17525,.T.);
#37451=EDGE_CURVE('',#30537,#30536,#17526,.T.);
#37452=EDGE_CURVE('',#30535,#30537,#22281,.T.);
#37453=EDGE_CURVE('',#30453,#30537,#24961,.T.);
#37454=EDGE_CURVE('',#30538,#30539,#17527,.T.);
#37455=EDGE_CURVE('',#30171,#30539,#22282,.T.);
#37456=EDGE_CURVE('',#30538,#30453,#24962,.T.);
#37457=EDGE_CURVE('',#30540,#30538,#17528,.T.);
#37458=EDGE_CURVE('',#30541,#30540,#17529,.T.);
#37459=EDGE_CURVE('',#30539,#30541,#22283,.T.);
#37460=EDGE_CURVE('',#30454,#30541,#24963,.T.);
#37461=EDGE_CURVE('',#30542,#30543,#17530,.T.);
#37462=EDGE_CURVE('',#30172,#30543,#22284,.T.);
#37463=EDGE_CURVE('',#30542,#30454,#24964,.T.);
#37464=EDGE_CURVE('',#30544,#30542,#17531,.T.);
#37465=EDGE_CURVE('',#30545,#30544,#17532,.T.);
#37466=EDGE_CURVE('',#30543,#30545,#22285,.T.);
#37467=EDGE_CURVE('',#30455,#30545,#24965,.T.);
#37468=EDGE_CURVE('',#30546,#30547,#17533,.T.);
#37469=EDGE_CURVE('',#30173,#30547,#22286,.T.);
#37470=EDGE_CURVE('',#30546,#30455,#24966,.T.);
#37471=EDGE_CURVE('',#30548,#30546,#17534,.T.);
#37472=EDGE_CURVE('',#30549,#30548,#17535,.T.);
#37473=EDGE_CURVE('',#30547,#30549,#22287,.T.);
#37474=EDGE_CURVE('',#30456,#30549,#24967,.T.);
#37475=EDGE_CURVE('',#30550,#30551,#17536,.T.);
#37476=EDGE_CURVE('',#30174,#30551,#22288,.T.);
#37477=EDGE_CURVE('',#30550,#30456,#24968,.T.);
#37478=EDGE_CURVE('',#30552,#30550,#17537,.T.);
#37479=EDGE_CURVE('',#30553,#30552,#17538,.T.);
#37480=EDGE_CURVE('',#30551,#30553,#22289,.T.);
#37481=EDGE_CURVE('',#30457,#30553,#24969,.T.);
#37482=EDGE_CURVE('',#30554,#30555,#17539,.T.);
#37483=EDGE_CURVE('',#30175,#30555,#22290,.T.);
#37484=EDGE_CURVE('',#30554,#30457,#24970,.T.);
#37485=EDGE_CURVE('',#30556,#30554,#17540,.T.);
#37486=EDGE_CURVE('',#30557,#30556,#17541,.T.);
#37487=EDGE_CURVE('',#30555,#30557,#22291,.T.);
#37488=EDGE_CURVE('',#30458,#30557,#24971,.T.);
#37489=EDGE_CURVE('',#30176,#28991,#22292,.T.);
#37490=EDGE_CURVE('',#28990,#30458,#24972,.T.);
#37491=EDGE_CURVE('',#30459,#28993,#24973,.T.);
#37492=EDGE_CURVE('',#30558,#30559,#17542,.T.);
#37493=EDGE_CURVE('',#30177,#30559,#22293,.T.);
#37494=EDGE_CURVE('',#30558,#30459,#24974,.T.);
#37495=EDGE_CURVE('',#30560,#30558,#17543,.T.);
#37496=EDGE_CURVE('',#30561,#30560,#17544,.T.);
#37497=EDGE_CURVE('',#30559,#30561,#22294,.T.);
#37498=EDGE_CURVE('',#30460,#30561,#24975,.T.);
#37499=EDGE_CURVE('',#30562,#30563,#17545,.T.);
#37500=EDGE_CURVE('',#30178,#30563,#22295,.T.);
#37501=EDGE_CURVE('',#30562,#30460,#24976,.T.);
#37502=EDGE_CURVE('',#30564,#30562,#17546,.T.);
#37503=EDGE_CURVE('',#30565,#30564,#17547,.T.);
#37504=EDGE_CURVE('',#30563,#30565,#22296,.T.);
#37505=EDGE_CURVE('',#30461,#30565,#24977,.T.);
#37506=EDGE_CURVE('',#30566,#30567,#17548,.T.);
#37507=EDGE_CURVE('',#30179,#30567,#22297,.T.);
#37508=EDGE_CURVE('',#30566,#30461,#24978,.T.);
#37509=EDGE_CURVE('',#30568,#30566,#17549,.T.);
#37510=EDGE_CURVE('',#30569,#30568,#17550,.T.);
#37511=EDGE_CURVE('',#30567,#30569,#22298,.T.);
#37512=EDGE_CURVE('',#30462,#30569,#24979,.T.);
#37513=EDGE_CURVE('',#30570,#30571,#17551,.T.);
#37514=EDGE_CURVE('',#30180,#30571,#22299,.T.);
#37515=EDGE_CURVE('',#30570,#30462,#24980,.T.);
#37516=EDGE_CURVE('',#30572,#30570,#17552,.T.);
#37517=EDGE_CURVE('',#30573,#30572,#17553,.T.);
#37518=EDGE_CURVE('',#30571,#30573,#22300,.T.);
#37519=EDGE_CURVE('',#30463,#30573,#24981,.T.);
#37520=EDGE_CURVE('',#30574,#30575,#17554,.T.);
#37521=EDGE_CURVE('',#30181,#30575,#22301,.T.);
#37522=EDGE_CURVE('',#30574,#30463,#24982,.T.);
#37523=EDGE_CURVE('',#30576,#30574,#17555,.T.);
#37524=EDGE_CURVE('',#30577,#30576,#17556,.T.);
#37525=EDGE_CURVE('',#30575,#30577,#22302,.T.);
#37526=EDGE_CURVE('',#30464,#30577,#24983,.T.);
#37527=EDGE_CURVE('',#30578,#30579,#17557,.T.);
#37528=EDGE_CURVE('',#30182,#30579,#22303,.T.);
#37529=EDGE_CURVE('',#30578,#30464,#24984,.T.);
#37530=EDGE_CURVE('',#30580,#30578,#17558,.T.);
#37531=EDGE_CURVE('',#30581,#30580,#17559,.T.);
#37532=EDGE_CURVE('',#30579,#30581,#22304,.T.);
#37533=EDGE_CURVE('',#30465,#30581,#24985,.T.);
#37534=EDGE_CURVE('',#30582,#30583,#17560,.T.);
#37535=EDGE_CURVE('',#30183,#30583,#22305,.T.);
#37536=EDGE_CURVE('',#30582,#30465,#24986,.T.);
#37537=EDGE_CURVE('',#30584,#30582,#17561,.T.);
#37538=EDGE_CURVE('',#30585,#30584,#17562,.T.);
#37539=EDGE_CURVE('',#30583,#30585,#22306,.T.);
#37540=EDGE_CURVE('',#30466,#30585,#24987,.T.);
#37541=EDGE_CURVE('',#30586,#30587,#17563,.T.);
#37542=EDGE_CURVE('',#30184,#30587,#22307,.T.);
#37543=EDGE_CURVE('',#30586,#30466,#24988,.T.);
#37544=EDGE_CURVE('',#30587,#30588,#22308,.T.);
#37545=EDGE_CURVE('',#30467,#30588,#24989,.T.);
#37546=EDGE_CURVE('',#30589,#30586,#17564,.T.);
#37547=EDGE_CURVE('',#30588,#30589,#17565,.T.);
#37548=EDGE_CURVE('',#30590,#30467,#24990,.T.);
#37549=EDGE_CURVE('',#30590,#30591,#17566,.T.);
#37550=EDGE_CURVE('',#30185,#30591,#22309,.T.);
#37551=EDGE_CURVE('',#30591,#30592,#22310,.T.);
#37552=EDGE_CURVE('',#30593,#30590,#17567,.T.);
#37553=EDGE_CURVE('',#30592,#30593,#17568,.T.);
#37554=EDGE_CURVE('',#30468,#30592,#24991,.T.);
#37555=EDGE_CURVE('',#30594,#30595,#17569,.T.);
#37556=EDGE_CURVE('',#30186,#30595,#22311,.T.);
#37557=EDGE_CURVE('',#30594,#30468,#24992,.T.);
#37558=EDGE_CURVE('',#30596,#30594,#17570,.T.);
#37559=EDGE_CURVE('',#30597,#30596,#17571,.T.);
#37560=EDGE_CURVE('',#30595,#30597,#22312,.T.);
#37561=EDGE_CURVE('',#30469,#30597,#24993,.T.);
#37562=EDGE_CURVE('',#30598,#30599,#17572,.T.);
#37563=EDGE_CURVE('',#30187,#30599,#22313,.T.);
#37564=EDGE_CURVE('',#30598,#30469,#24994,.T.);
#37565=EDGE_CURVE('',#30600,#30598,#17573,.T.);
#37566=EDGE_CURVE('',#30601,#30600,#17574,.T.);
#37567=EDGE_CURVE('',#30599,#30601,#22314,.T.);
#37568=EDGE_CURVE('',#30470,#30601,#24995,.T.);
#37569=EDGE_CURVE('',#30602,#30603,#17575,.T.);
#37570=EDGE_CURVE('',#30188,#30603,#22315,.T.);
#37571=EDGE_CURVE('',#30602,#30470,#24996,.T.);
#37572=EDGE_CURVE('',#30604,#30602,#17576,.T.);
#37573=EDGE_CURVE('',#30605,#30604,#17577,.T.);
#37574=EDGE_CURVE('',#30603,#30605,#22316,.T.);
#37575=EDGE_CURVE('',#30471,#30605,#24997,.T.);
#37576=EDGE_CURVE('',#30606,#30607,#17578,.T.);
#37577=EDGE_CURVE('',#30189,#30607,#22317,.T.);
#37578=EDGE_CURVE('',#30606,#30471,#24998,.T.);
#37579=EDGE_CURVE('',#30608,#30606,#17579,.T.);
#37580=EDGE_CURVE('',#30609,#30608,#17580,.T.);
#37581=EDGE_CURVE('',#30607,#30609,#22318,.T.);
#37582=EDGE_CURVE('',#30472,#30609,#24999,.T.);
#37583=EDGE_CURVE('',#30610,#30611,#17581,.T.);
#37584=EDGE_CURVE('',#30190,#30611,#22319,.T.);
#37585=EDGE_CURVE('',#30610,#30472,#25000,.T.);
#37586=EDGE_CURVE('',#30612,#30610,#17582,.T.);
#37587=EDGE_CURVE('',#30613,#30612,#17583,.T.);
#37588=EDGE_CURVE('',#30611,#30613,#22320,.T.);
#37589=EDGE_CURVE('',#30444,#30613,#25001,.T.);
#37590=EDGE_CURVE('',#30614,#30473,#25002,.T.);
#37591=EDGE_CURVE('',#30614,#30615,#17584,.T.);
#37592=EDGE_CURVE('',#30191,#30615,#22321,.T.);
#37593=EDGE_CURVE('',#30615,#30616,#17585,.T.);
#37594=EDGE_CURVE('',#30474,#30616,#25003,.T.);
#37595=EDGE_CURVE('',#30617,#30614,#17586,.T.);
#37596=EDGE_CURVE('',#30616,#30617,#17587,.T.);
#37597=EDGE_CURVE('',#30618,#30474,#25004,.T.);
#37598=EDGE_CURVE('',#30618,#30619,#17588,.T.);
#37599=EDGE_CURVE('',#30192,#30619,#22322,.T.);
#37600=EDGE_CURVE('',#30619,#30620,#17589,.T.);
#37601=EDGE_CURVE('',#30475,#30620,#25005,.T.);
#37602=EDGE_CURVE('',#30621,#30618,#17590,.T.);
#37603=EDGE_CURVE('',#30620,#30621,#17591,.T.);
#37604=EDGE_CURVE('',#30622,#30475,#25006,.T.);
#37605=EDGE_CURVE('',#30622,#30623,#17592,.T.);
#37606=EDGE_CURVE('',#30193,#30623,#22323,.T.);
#37607=EDGE_CURVE('',#30623,#30624,#17593,.T.);
#37608=EDGE_CURVE('',#30476,#30624,#25007,.T.);
#37609=EDGE_CURVE('',#30625,#30622,#17594,.T.);
#37610=EDGE_CURVE('',#30624,#30625,#17595,.T.);
#37611=EDGE_CURVE('',#30626,#30476,#25008,.T.);
#37612=EDGE_CURVE('',#30626,#30627,#17596,.T.);
#37613=EDGE_CURVE('',#30194,#30627,#22324,.T.);
#37614=EDGE_CURVE('',#30627,#30628,#17597,.T.);
#37615=EDGE_CURVE('',#30477,#30628,#25009,.T.);
#37616=EDGE_CURVE('',#30629,#30626,#17598,.T.);
#37617=EDGE_CURVE('',#30628,#30629,#17599,.T.);
#37618=EDGE_CURVE('',#30630,#30477,#25010,.T.);
#37619=EDGE_CURVE('',#30630,#30631,#17600,.T.);
#37620=EDGE_CURVE('',#30195,#30631,#22325,.T.);
#37621=EDGE_CURVE('',#30631,#30632,#17601,.T.);
#37622=EDGE_CURVE('',#30478,#30632,#25011,.T.);
#37623=EDGE_CURVE('',#30633,#30630,#17602,.T.);
#37624=EDGE_CURVE('',#30632,#30633,#17603,.T.);
#37625=EDGE_CURVE('',#30634,#30478,#25012,.T.);
#37626=EDGE_CURVE('',#30634,#30635,#17604,.T.);
#37627=EDGE_CURVE('',#30196,#30635,#22326,.T.);
#37628=EDGE_CURVE('',#30635,#30636,#17605,.T.);
#37629=EDGE_CURVE('',#30479,#30636,#25013,.T.);
#37630=EDGE_CURVE('',#30637,#30634,#17606,.T.);
#37631=EDGE_CURVE('',#30636,#30637,#17607,.T.);
#37632=EDGE_CURVE('',#30638,#30479,#25014,.T.);
#37633=EDGE_CURVE('',#30638,#30639,#17608,.T.);
#37634=EDGE_CURVE('',#30197,#30639,#22327,.T.);
#37635=EDGE_CURVE('',#30639,#30640,#17609,.T.);
#37636=EDGE_CURVE('',#30480,#30640,#25015,.T.);
#37637=EDGE_CURVE('',#30641,#30638,#17610,.T.);
#37638=EDGE_CURVE('',#30640,#30641,#17611,.T.);
#37639=EDGE_CURVE('',#30642,#30480,#25016,.T.);
#37640=EDGE_CURVE('',#30642,#30643,#17612,.T.);
#37641=EDGE_CURVE('',#30198,#30643,#22328,.T.);
#37642=EDGE_CURVE('',#30643,#30644,#17613,.T.);
#37643=EDGE_CURVE('',#30481,#30644,#25017,.T.);
#37644=EDGE_CURVE('',#30645,#30642,#17614,.T.);
#37645=EDGE_CURVE('',#30644,#30645,#17615,.T.);
#37646=EDGE_CURVE('',#30646,#30481,#25018,.T.);
#37647=EDGE_CURVE('',#30646,#30647,#17616,.T.);
#37648=EDGE_CURVE('',#30199,#30647,#22329,.T.);
#37649=EDGE_CURVE('',#30647,#30648,#17617,.T.);
#37650=EDGE_CURVE('',#30482,#30648,#25019,.T.);
#37651=EDGE_CURVE('',#30649,#30646,#17618,.T.);
#37652=EDGE_CURVE('',#30648,#30649,#17619,.T.);
#37653=EDGE_CURVE('',#30650,#30482,#25020,.T.);
#37654=EDGE_CURVE('',#30650,#30651,#17620,.T.);
#37655=EDGE_CURVE('',#30200,#30651,#22330,.T.);
#37656=EDGE_CURVE('',#30651,#30652,#17621,.T.);
#37657=EDGE_CURVE('',#30483,#30652,#25021,.T.);
#37658=EDGE_CURVE('',#30653,#30650,#17622,.T.);
#37659=EDGE_CURVE('',#30652,#30653,#17623,.T.);
#37660=EDGE_CURVE('',#30654,#30483,#25022,.T.);
#37661=EDGE_CURVE('',#30654,#30655,#17624,.T.);
#37662=EDGE_CURVE('',#30201,#30655,#22331,.T.);
#37663=EDGE_CURVE('',#30655,#30656,#17625,.T.);
#37664=EDGE_CURVE('',#30484,#30656,#25023,.T.);
#37665=EDGE_CURVE('',#30657,#30654,#17626,.T.);
#37666=EDGE_CURVE('',#30656,#30657,#17627,.T.);
#37667=EDGE_CURVE('',#30658,#30484,#25024,.T.);
#37668=EDGE_CURVE('',#30658,#30659,#17628,.T.);
#37669=EDGE_CURVE('',#30202,#30659,#22332,.T.);
#37670=EDGE_CURVE('',#30659,#30660,#17629,.T.);
#37671=EDGE_CURVE('',#30485,#30660,#25025,.T.);
#37672=EDGE_CURVE('',#30661,#30658,#17630,.T.);
#37673=EDGE_CURVE('',#30660,#30661,#17631,.T.);
#37674=EDGE_CURVE('',#30662,#30485,#25026,.T.);
#37675=EDGE_CURVE('',#30662,#30663,#17632,.T.);
#37676=EDGE_CURVE('',#30203,#30663,#22333,.T.);
#37677=EDGE_CURVE('',#30663,#30664,#17633,.T.);
#37678=EDGE_CURVE('',#30486,#30664,#25027,.T.);
#37679=EDGE_CURVE('',#30665,#30662,#17634,.T.);
#37680=EDGE_CURVE('',#30664,#30665,#17635,.T.);
#37681=EDGE_CURVE('',#30666,#30486,#25028,.T.);
#37682=EDGE_CURVE('',#30666,#30667,#17636,.T.);
#37683=EDGE_CURVE('',#30204,#30667,#22334,.T.);
#37684=EDGE_CURVE('',#30667,#30668,#17637,.T.);
#37685=EDGE_CURVE('',#30487,#30668,#25029,.T.);
#37686=EDGE_CURVE('',#30669,#30666,#17638,.T.);
#37687=EDGE_CURVE('',#30668,#30669,#17639,.T.);
#37688=EDGE_CURVE('',#30670,#30487,#25030,.T.);
#37689=EDGE_CURVE('',#30670,#30671,#17640,.T.);
#37690=EDGE_CURVE('',#30205,#30671,#22335,.T.);
#37691=EDGE_CURVE('',#30671,#30672,#17641,.T.);
#37692=EDGE_CURVE('',#30488,#30672,#25031,.T.);
#37693=EDGE_CURVE('',#30673,#30670,#17642,.T.);
#37694=EDGE_CURVE('',#30672,#30673,#17643,.T.);
#37695=EDGE_CURVE('',#30674,#30488,#25032,.T.);
#37696=EDGE_CURVE('',#30674,#30675,#17644,.T.);
#37697=EDGE_CURVE('',#30206,#30675,#22336,.T.);
#37698=EDGE_CURVE('',#30675,#30676,#17645,.T.);
#37699=EDGE_CURVE('',#30489,#30676,#25033,.T.);
#37700=EDGE_CURVE('',#30677,#30674,#17646,.T.);
#37701=EDGE_CURVE('',#30676,#30677,#17647,.T.);
#37702=EDGE_CURVE('',#30678,#30489,#25034,.T.);
#37703=EDGE_CURVE('',#30678,#30679,#17648,.T.);
#37704=EDGE_CURVE('',#30207,#30679,#22337,.T.);
#37705=EDGE_CURVE('',#30679,#30680,#17649,.T.);
#37706=EDGE_CURVE('',#30490,#30680,#25035,.T.);
#37707=EDGE_CURVE('',#30681,#30678,#17650,.T.);
#37708=EDGE_CURVE('',#30680,#30681,#17651,.T.);
#37709=EDGE_CURVE('',#30682,#30490,#25036,.T.);
#37710=EDGE_CURVE('',#30682,#30683,#17652,.T.);
#37711=EDGE_CURVE('',#30208,#30683,#22338,.T.);
#37712=EDGE_CURVE('',#30683,#30684,#17653,.T.);
#37713=EDGE_CURVE('',#30491,#30684,#25037,.T.);
#37714=EDGE_CURVE('',#30685,#30682,#17654,.T.);
#37715=EDGE_CURVE('',#30684,#30685,#17655,.T.);
#37716=EDGE_CURVE('',#30686,#30491,#25038,.T.);
#37717=EDGE_CURVE('',#30686,#30687,#17656,.T.);
#37718=EDGE_CURVE('',#30209,#30687,#22339,.T.);
#37719=EDGE_CURVE('',#30687,#30688,#17657,.T.);
#37720=EDGE_CURVE('',#30492,#30688,#25039,.T.);
#37721=EDGE_CURVE('',#30689,#30686,#17658,.T.);
#37722=EDGE_CURVE('',#30688,#30689,#17659,.T.);
#37723=EDGE_CURVE('',#30690,#30492,#25040,.T.);
#37724=EDGE_CURVE('',#30690,#30691,#17660,.T.);
#37725=EDGE_CURVE('',#30210,#30691,#22340,.T.);
#37726=EDGE_CURVE('',#30691,#30692,#17661,.T.);
#37727=EDGE_CURVE('',#30493,#30692,#25041,.T.);
#37728=EDGE_CURVE('',#30693,#30690,#17662,.T.);
#37729=EDGE_CURVE('',#30692,#30693,#17663,.T.);
#37730=EDGE_CURVE('',#30694,#30493,#25042,.T.);
#37731=EDGE_CURVE('',#30694,#30695,#17664,.T.);
#37732=EDGE_CURVE('',#30211,#30695,#22341,.T.);
#37733=EDGE_CURVE('',#30695,#30696,#17665,.T.);
#37734=EDGE_CURVE('',#30494,#30696,#25043,.T.);
#37735=EDGE_CURVE('',#30697,#30694,#17666,.T.);
#37736=EDGE_CURVE('',#30696,#30697,#17667,.T.);
#37737=EDGE_CURVE('',#28987,#30494,#25044,.T.);
#37738=EDGE_CURVE('',#30212,#28989,#22342,.T.);
#37739=EDGE_CURVE('',#30495,#28988,#25045,.T.);
#37740=EDGE_CURVE('',#30698,#30495,#25046,.T.);
#37741=EDGE_CURVE('',#30698,#30699,#17668,.T.);
#37742=EDGE_CURVE('',#30213,#30699,#22343,.T.);
#37743=EDGE_CURVE('',#30699,#30700,#17669,.T.);
#37744=EDGE_CURVE('',#30496,#30700,#25047,.T.);
#37745=EDGE_CURVE('',#30701,#30698,#17670,.T.);
#37746=EDGE_CURVE('',#30700,#30701,#17671,.T.);
#37747=EDGE_CURVE('',#30702,#30496,#25048,.T.);
#37748=EDGE_CURVE('',#30702,#30703,#17672,.T.);
#37749=EDGE_CURVE('',#30214,#30703,#22344,.T.);
#37750=EDGE_CURVE('',#30703,#30704,#17673,.T.);
#37751=EDGE_CURVE('',#30497,#30704,#25049,.T.);
#37752=EDGE_CURVE('',#30705,#30702,#17674,.T.);
#37753=EDGE_CURVE('',#30704,#30705,#17675,.T.);
#37754=EDGE_CURVE('',#30706,#30497,#25050,.T.);
#37755=EDGE_CURVE('',#30706,#30707,#17676,.T.);
#37756=EDGE_CURVE('',#30215,#30707,#22345,.T.);
#37757=EDGE_CURVE('',#30707,#30708,#17677,.T.);
#37758=EDGE_CURVE('',#30498,#30708,#25051,.T.);
#37759=EDGE_CURVE('',#30709,#30706,#17678,.T.);
#37760=EDGE_CURVE('',#30708,#30709,#17679,.T.);
#37761=EDGE_CURVE('',#30710,#30498,#25052,.T.);
#37762=EDGE_CURVE('',#30710,#30711,#17680,.T.);
#37763=EDGE_CURVE('',#30216,#30711,#22346,.T.);
#37764=EDGE_CURVE('',#30711,#30712,#17681,.T.);
#37765=EDGE_CURVE('',#30499,#30712,#25053,.T.);
#37766=EDGE_CURVE('',#30713,#30710,#17682,.T.);
#37767=EDGE_CURVE('',#30712,#30713,#17683,.T.);
#37768=EDGE_CURVE('',#30714,#30499,#25054,.T.);
#37769=EDGE_CURVE('',#30714,#30715,#17684,.T.);
#37770=EDGE_CURVE('',#30217,#30715,#22347,.T.);
#37771=EDGE_CURVE('',#30715,#30716,#17685,.T.);
#37772=EDGE_CURVE('',#30500,#30716,#25055,.T.);
#37773=EDGE_CURVE('',#30717,#30714,#17686,.T.);
#37774=EDGE_CURVE('',#30716,#30717,#17687,.T.);
#37775=EDGE_CURVE('',#30718,#30500,#25056,.T.);
#37776=EDGE_CURVE('',#30718,#30719,#17688,.T.);
#37777=EDGE_CURVE('',#30218,#30719,#22348,.T.);
#37778=EDGE_CURVE('',#30719,#30720,#17689,.T.);
#37779=EDGE_CURVE('',#30501,#30720,#25057,.T.);
#37780=EDGE_CURVE('',#30721,#30718,#17690,.T.);
#37781=EDGE_CURVE('',#30720,#30721,#17691,.T.);
#37782=EDGE_CURVE('',#30722,#30501,#25058,.T.);
#37783=EDGE_CURVE('',#30722,#30723,#17692,.T.);
#37784=EDGE_CURVE('',#30219,#30723,#22349,.T.);
#37785=EDGE_CURVE('',#30723,#30724,#17693,.T.);
#37786=EDGE_CURVE('',#30473,#30724,#25059,.T.);
#37787=EDGE_CURVE('',#30725,#30722,#17694,.T.);
#37788=EDGE_CURVE('',#30724,#30725,#17695,.T.);
#37789=EDGE_CURVE('',#30726,#30444,#17696,.T.);
#37790=EDGE_CURVE('',#30504,#30726,#22350,.T.);
#37791=EDGE_CURVE('',#30445,#30726,#22351,.T.);
#37792=EDGE_CURVE('',#30727,#30445,#17697,.T.);
#37793=EDGE_CURVE('',#30508,#30727,#22352,.T.);
#37794=EDGE_CURVE('',#30446,#30727,#22353,.T.);
#37795=EDGE_CURVE('',#30728,#30446,#17698,.T.);
#37796=EDGE_CURVE('',#30512,#30728,#22354,.T.);
#37797=EDGE_CURVE('',#30447,#30728,#22355,.T.);
#37798=EDGE_CURVE('',#30729,#30447,#17699,.T.);
#37799=EDGE_CURVE('',#30516,#30729,#22356,.T.);
#37800=EDGE_CURVE('',#30448,#30729,#22357,.T.);
#37801=EDGE_CURVE('',#30730,#30448,#17700,.T.);
#37802=EDGE_CURVE('',#30520,#30730,#22358,.T.);
#37803=EDGE_CURVE('',#30449,#30730,#22359,.T.);
#37804=EDGE_CURVE('',#30731,#30449,#17701,.T.);
#37805=EDGE_CURVE('',#30524,#30731,#22360,.T.);
#37806=EDGE_CURVE('',#30450,#30731,#22361,.T.);
#37807=EDGE_CURVE('',#30732,#30450,#17702,.T.);
#37808=EDGE_CURVE('',#30528,#30732,#22362,.T.);
#37809=EDGE_CURVE('',#30451,#30732,#22363,.T.);
#37810=EDGE_CURVE('',#30733,#30451,#17703,.T.);
#37811=EDGE_CURVE('',#30532,#30733,#22364,.T.);
#37812=EDGE_CURVE('',#30452,#30733,#22365,.T.);
#37813=EDGE_CURVE('',#30734,#30452,#17704,.T.);
#37814=EDGE_CURVE('',#30536,#30734,#22366,.T.);
#37815=EDGE_CURVE('',#30453,#30734,#22367,.T.);
#37816=EDGE_CURVE('',#30735,#30453,#17705,.T.);
#37817=EDGE_CURVE('',#30540,#30735,#22368,.T.);
#37818=EDGE_CURVE('',#30454,#30735,#22369,.T.);
#37819=EDGE_CURVE('',#30736,#30454,#17706,.T.);
#37820=EDGE_CURVE('',#30544,#30736,#22370,.T.);
#37821=EDGE_CURVE('',#30455,#30736,#22371,.T.);
#37822=EDGE_CURVE('',#30737,#30455,#17707,.T.);
#37823=EDGE_CURVE('',#30548,#30737,#22372,.T.);
#37824=EDGE_CURVE('',#30456,#30737,#22373,.T.);
#37825=EDGE_CURVE('',#30738,#30456,#17708,.T.);
#37826=EDGE_CURVE('',#30552,#30738,#22374,.T.);
#37827=EDGE_CURVE('',#30457,#30738,#22375,.T.);
#37828=EDGE_CURVE('',#30739,#30457,#17709,.T.);
#37829=EDGE_CURVE('',#30556,#30739,#22376,.T.);
#37830=EDGE_CURVE('',#30458,#30739,#22377,.T.);
#37831=EDGE_CURVE('',#30740,#30458,#17710,.T.);
#37832=EDGE_CURVE('',#28992,#30740,#22378,.T.);
#37833=EDGE_CURVE('',#30459,#30740,#22379,.T.);
#37834=EDGE_CURVE('',#30741,#30459,#17711,.T.);
#37835=EDGE_CURVE('',#30560,#30741,#22380,.T.);
#37836=EDGE_CURVE('',#30460,#30741,#22381,.T.);
#37837=EDGE_CURVE('',#30742,#30460,#17712,.T.);
#37838=EDGE_CURVE('',#30564,#30742,#22382,.T.);
#37839=EDGE_CURVE('',#30461,#30742,#22383,.T.);
#37840=EDGE_CURVE('',#30743,#30461,#17713,.T.);
#37841=EDGE_CURVE('',#30568,#30743,#22384,.T.);
#37842=EDGE_CURVE('',#30462,#30743,#22385,.T.);
#37843=EDGE_CURVE('',#30744,#30462,#17714,.T.);
#37844=EDGE_CURVE('',#30572,#30744,#22386,.T.);
#37845=EDGE_CURVE('',#30463,#30744,#22387,.T.);
#37846=EDGE_CURVE('',#30745,#30463,#17715,.T.);
#37847=EDGE_CURVE('',#30576,#30745,#22388,.T.);
#37848=EDGE_CURVE('',#30464,#30745,#22389,.T.);
#37849=EDGE_CURVE('',#30746,#30464,#17716,.T.);
#37850=EDGE_CURVE('',#30580,#30746,#22390,.T.);
#37851=EDGE_CURVE('',#30465,#30746,#22391,.T.);
#37852=EDGE_CURVE('',#30747,#30465,#17717,.T.);
#37853=EDGE_CURVE('',#30584,#30747,#22392,.T.);
#37854=EDGE_CURVE('',#30466,#30747,#22393,.T.);
#37855=EDGE_CURVE('',#30748,#30466,#17718,.T.);
#37856=EDGE_CURVE('',#30589,#30748,#22394,.T.);
#37857=EDGE_CURVE('',#30467,#30748,#22395,.T.);
#37858=EDGE_CURVE('',#30749,#30467,#17719,.T.);
#37859=EDGE_CURVE('',#30593,#30749,#22396,.T.);
#37860=EDGE_CURVE('',#30468,#30749,#22397,.T.);
#37861=EDGE_CURVE('',#30750,#30468,#17720,.T.);
#37862=EDGE_CURVE('',#30596,#30750,#22398,.T.);
#37863=EDGE_CURVE('',#30469,#30750,#22399,.T.);
#37864=EDGE_CURVE('',#30751,#30469,#17721,.T.);
#37865=EDGE_CURVE('',#30600,#30751,#22400,.T.);
#37866=EDGE_CURVE('',#30470,#30751,#22401,.T.);
#37867=EDGE_CURVE('',#30752,#30470,#17722,.T.);
#37868=EDGE_CURVE('',#30604,#30752,#22402,.T.);
#37869=EDGE_CURVE('',#30471,#30752,#22403,.T.);
#37870=EDGE_CURVE('',#30753,#30471,#17723,.T.);
#37871=EDGE_CURVE('',#30608,#30753,#22404,.T.);
#37872=EDGE_CURVE('',#30472,#30753,#22405,.T.);
#37873=EDGE_CURVE('',#30754,#30472,#17724,.T.);
#37874=EDGE_CURVE('',#30612,#30754,#22406,.T.);
#37875=EDGE_CURVE('',#30444,#30754,#22407,.T.);
#37876=EDGE_CURVE('',#30755,#30473,#17725,.T.);
#37877=EDGE_CURVE('',#30617,#30755,#22408,.T.);
#37878=EDGE_CURVE('',#30474,#30755,#22409,.T.);
#37879=EDGE_CURVE('',#30756,#30474,#17726,.T.);
#37880=EDGE_CURVE('',#30621,#30756,#22410,.T.);
#37881=EDGE_CURVE('',#30475,#30756,#22411,.T.);
#37882=EDGE_CURVE('',#30757,#30475,#17727,.T.);
#37883=EDGE_CURVE('',#30625,#30757,#22412,.T.);
#37884=EDGE_CURVE('',#30476,#30757,#22413,.T.);
#37885=EDGE_CURVE('',#30758,#30476,#17728,.T.);
#37886=EDGE_CURVE('',#30629,#30758,#22414,.T.);
#37887=EDGE_CURVE('',#30477,#30758,#22415,.T.);
#37888=EDGE_CURVE('',#30759,#30477,#17729,.T.);
#37889=EDGE_CURVE('',#30633,#30759,#22416,.T.);
#37890=EDGE_CURVE('',#30478,#30759,#22417,.T.);
#37891=EDGE_CURVE('',#30760,#30478,#17730,.T.);
#37892=EDGE_CURVE('',#30637,#30760,#22418,.T.);
#37893=EDGE_CURVE('',#30479,#30760,#22419,.T.);
#37894=EDGE_CURVE('',#30761,#30479,#17731,.T.);
#37895=EDGE_CURVE('',#30641,#30761,#22420,.T.);
#37896=EDGE_CURVE('',#30480,#30761,#22421,.T.);
#37897=EDGE_CURVE('',#30762,#30480,#17732,.T.);
#37898=EDGE_CURVE('',#30645,#30762,#22422,.T.);
#37899=EDGE_CURVE('',#30481,#30762,#22423,.T.);
#37900=EDGE_CURVE('',#30763,#30481,#17733,.T.);
#37901=EDGE_CURVE('',#30649,#30763,#22424,.T.);
#37902=EDGE_CURVE('',#30482,#30763,#22425,.T.);
#37903=EDGE_CURVE('',#30764,#30482,#17734,.T.);
#37904=EDGE_CURVE('',#30653,#30764,#22426,.T.);
#37905=EDGE_CURVE('',#30483,#30764,#22427,.T.);
#37906=EDGE_CURVE('',#30765,#30483,#17735,.T.);
#37907=EDGE_CURVE('',#30657,#30765,#22428,.T.);
#37908=EDGE_CURVE('',#30484,#30765,#22429,.T.);
#37909=EDGE_CURVE('',#30766,#30484,#17736,.T.);
#37910=EDGE_CURVE('',#30661,#30766,#22430,.T.);
#37911=EDGE_CURVE('',#30485,#30766,#22431,.T.);
#37912=EDGE_CURVE('',#30767,#30485,#17737,.T.);
#37913=EDGE_CURVE('',#30665,#30767,#22432,.T.);
#37914=EDGE_CURVE('',#30486,#30767,#22433,.T.);
#37915=EDGE_CURVE('',#30768,#30486,#17738,.T.);
#37916=EDGE_CURVE('',#30669,#30768,#22434,.T.);
#37917=EDGE_CURVE('',#30487,#30768,#22435,.T.);
#37918=EDGE_CURVE('',#30769,#30487,#17739,.T.);
#37919=EDGE_CURVE('',#30673,#30769,#22436,.T.);
#37920=EDGE_CURVE('',#30488,#30769,#22437,.T.);
#37921=EDGE_CURVE('',#30770,#30488,#17740,.T.);
#37922=EDGE_CURVE('',#30677,#30770,#22438,.T.);
#37923=EDGE_CURVE('',#30489,#30770,#22439,.T.);
#37924=EDGE_CURVE('',#30771,#30489,#17741,.T.);
#37925=EDGE_CURVE('',#30681,#30771,#22440,.T.);
#37926=EDGE_CURVE('',#30490,#30771,#22441,.T.);
#37927=EDGE_CURVE('',#30772,#30490,#17742,.T.);
#37928=EDGE_CURVE('',#30685,#30772,#22442,.T.);
#37929=EDGE_CURVE('',#30491,#30772,#22443,.T.);
#37930=EDGE_CURVE('',#30773,#30491,#17743,.T.);
#37931=EDGE_CURVE('',#30689,#30773,#22444,.T.);
#37932=EDGE_CURVE('',#30492,#30773,#22445,.T.);
#37933=EDGE_CURVE('',#30774,#30492,#17744,.T.);
#37934=EDGE_CURVE('',#30693,#30774,#22446,.T.);
#37935=EDGE_CURVE('',#30493,#30774,#22447,.T.);
#37936=EDGE_CURVE('',#30775,#30493,#17745,.T.);
#37937=EDGE_CURVE('',#30697,#30775,#22448,.T.);
#37938=EDGE_CURVE('',#30494,#30775,#22449,.T.);
#37939=EDGE_CURVE('',#30776,#30494,#17746,.T.);
#37940=EDGE_CURVE('',#28986,#30776,#22450,.T.);
#37941=EDGE_CURVE('',#30495,#30776,#22451,.T.);
#37942=EDGE_CURVE('',#30777,#30495,#17747,.T.);
#37943=EDGE_CURVE('',#30701,#30777,#22452,.T.);
#37944=EDGE_CURVE('',#30496,#30777,#22453,.T.);
#37945=EDGE_CURVE('',#30778,#30496,#17748,.T.);
#37946=EDGE_CURVE('',#30705,#30778,#22454,.T.);
#37947=EDGE_CURVE('',#30497,#30778,#22455,.T.);
#37948=EDGE_CURVE('',#30779,#30497,#17749,.T.);
#37949=EDGE_CURVE('',#30709,#30779,#22456,.T.);
#37950=EDGE_CURVE('',#30498,#30779,#22457,.T.);
#37951=EDGE_CURVE('',#30780,#30498,#17750,.T.);
#37952=EDGE_CURVE('',#30713,#30780,#22458,.T.);
#37953=EDGE_CURVE('',#30499,#30780,#22459,.T.);
#37954=EDGE_CURVE('',#30781,#30499,#17751,.T.);
#37955=EDGE_CURVE('',#30717,#30781,#22460,.T.);
#37956=EDGE_CURVE('',#30500,#30781,#22461,.T.);
#37957=EDGE_CURVE('',#30782,#30500,#17752,.T.);
#37958=EDGE_CURVE('',#30721,#30782,#22462,.T.);
#37959=EDGE_CURVE('',#30501,#30782,#22463,.T.);
#37960=EDGE_CURVE('',#30783,#30501,#17753,.T.);
#37961=EDGE_CURVE('',#30725,#30783,#22464,.T.);
#37962=EDGE_CURVE('',#30473,#30783,#22465,.T.);
#37963=EDGE_CURVE('',#30784,#30785,#17754,.T.);
#37964=EDGE_CURVE('',#30726,#30785,#25060,.T.);
#37965=EDGE_CURVE('',#30784,#30444,#22466,.T.);
#37966=EDGE_CURVE('',#30786,#30787,#22467,.T.);
#37967=EDGE_CURVE('',#30445,#30787,#22468,.T.);
#37968=EDGE_CURVE('',#30786,#30726,#25061,.T.);
#37969=EDGE_CURVE('',#30788,#30786,#17755,.T.);
#37970=EDGE_CURVE('',#30789,#30788,#17756,.T.);
#37971=EDGE_CURVE('',#30787,#30789,#17757,.T.);
#37972=EDGE_CURVE('',#30727,#30789,#25062,.T.);
#37973=EDGE_CURVE('',#30790,#30791,#22469,.T.);
#37974=EDGE_CURVE('',#30446,#30791,#22470,.T.);
#37975=EDGE_CURVE('',#30790,#30727,#25063,.T.);
#37976=EDGE_CURVE('',#30792,#30790,#17758,.T.);
#37977=EDGE_CURVE('',#30793,#30792,#17759,.T.);
#37978=EDGE_CURVE('',#30791,#30793,#17760,.T.);
#37979=EDGE_CURVE('',#30728,#30793,#25064,.T.);
#37980=EDGE_CURVE('',#30794,#30795,#22471,.T.);
#37981=EDGE_CURVE('',#30447,#30795,#22472,.T.);
#37982=EDGE_CURVE('',#30794,#30728,#25065,.T.);
#37983=EDGE_CURVE('',#30796,#30794,#17761,.T.);
#37984=EDGE_CURVE('',#30797,#30796,#17762,.T.);
#37985=EDGE_CURVE('',#30795,#30797,#17763,.T.);
#37986=EDGE_CURVE('',#30729,#30797,#25066,.T.);
#37987=EDGE_CURVE('',#30798,#30799,#22473,.T.);
#37988=EDGE_CURVE('',#30448,#30799,#22474,.T.);
#37989=EDGE_CURVE('',#30798,#30729,#25067,.T.);
#37990=EDGE_CURVE('',#30800,#30798,#17764,.T.);
#37991=EDGE_CURVE('',#30801,#30800,#17765,.T.);
#37992=EDGE_CURVE('',#30799,#30801,#17766,.T.);
#37993=EDGE_CURVE('',#30730,#30801,#25068,.T.);
#37994=EDGE_CURVE('',#30802,#30803,#22475,.T.);
#37995=EDGE_CURVE('',#30449,#30803,#22476,.T.);
#37996=EDGE_CURVE('',#30802,#30730,#25069,.T.);
#37997=EDGE_CURVE('',#30804,#30802,#17767,.T.);
#37998=EDGE_CURVE('',#30805,#30804,#17768,.T.);
#37999=EDGE_CURVE('',#30803,#30805,#17769,.T.);
#38000=EDGE_CURVE('',#30731,#30805,#25070,.T.);
#38001=EDGE_CURVE('',#30806,#30807,#22477,.T.);
#38002=EDGE_CURVE('',#30450,#30807,#22478,.T.);
#38003=EDGE_CURVE('',#30806,#30731,#25071,.T.);
#38004=EDGE_CURVE('',#30808,#30806,#17770,.T.);
#38005=EDGE_CURVE('',#30809,#30808,#17771,.T.);
#38006=EDGE_CURVE('',#30807,#30809,#17772,.T.);
#38007=EDGE_CURVE('',#30732,#30809,#25072,.T.);
#38008=EDGE_CURVE('',#30451,#28982,#22479,.T.);
#38009=EDGE_CURVE('',#28984,#30732,#25073,.T.);
#38010=EDGE_CURVE('',#30733,#28983,#25074,.T.);
#38011=EDGE_CURVE('',#30810,#30811,#22480,.T.);
#38012=EDGE_CURVE('',#30452,#30811,#22481,.T.);
#38013=EDGE_CURVE('',#30810,#30733,#25075,.T.);
#38014=EDGE_CURVE('',#30812,#30810,#17773,.T.);
#38015=EDGE_CURVE('',#30813,#30812,#17774,.T.);
#38016=EDGE_CURVE('',#30811,#30813,#17775,.T.);
#38017=EDGE_CURVE('',#30734,#30813,#25076,.T.);
#38018=EDGE_CURVE('',#30814,#30815,#22482,.T.);
#38019=EDGE_CURVE('',#30453,#30815,#22483,.T.);
#38020=EDGE_CURVE('',#30814,#30734,#25077,.T.);
#38021=EDGE_CURVE('',#30816,#30814,#17776,.T.);
#38022=EDGE_CURVE('',#30817,#30816,#17777,.T.);
#38023=EDGE_CURVE('',#30815,#30817,#17778,.T.);
#38024=EDGE_CURVE('',#30735,#30817,#25078,.T.);
#38025=EDGE_CURVE('',#30818,#30819,#22484,.T.);
#38026=EDGE_CURVE('',#30454,#30819,#22485,.T.);
#38027=EDGE_CURVE('',#30818,#30735,#25079,.T.);
#38028=EDGE_CURVE('',#30820,#30818,#17779,.T.);
#38029=EDGE_CURVE('',#30821,#30820,#17780,.T.);
#38030=EDGE_CURVE('',#30819,#30821,#17781,.T.);
#38031=EDGE_CURVE('',#30736,#30821,#25080,.T.);
#38032=EDGE_CURVE('',#30822,#30823,#22486,.T.);
#38033=EDGE_CURVE('',#30455,#30823,#22487,.T.);
#38034=EDGE_CURVE('',#30822,#30736,#25081,.T.);
#38035=EDGE_CURVE('',#30824,#30822,#17782,.T.);
#38036=EDGE_CURVE('',#30825,#30824,#17783,.T.);
#38037=EDGE_CURVE('',#30823,#30825,#17784,.T.);
#38038=EDGE_CURVE('',#30737,#30825,#25082,.T.);
#38039=EDGE_CURVE('',#30826,#30827,#22488,.T.);
#38040=EDGE_CURVE('',#30456,#30827,#22489,.T.);
#38041=EDGE_CURVE('',#30826,#30737,#25083,.T.);
#38042=EDGE_CURVE('',#30828,#30826,#17785,.T.);
#38043=EDGE_CURVE('',#30829,#30828,#17786,.T.);
#38044=EDGE_CURVE('',#30827,#30829,#17787,.T.);
#38045=EDGE_CURVE('',#30738,#30829,#25084,.T.);
#38046=EDGE_CURVE('',#30830,#30831,#22490,.T.);
#38047=EDGE_CURVE('',#30457,#30831,#22491,.T.);
#38048=EDGE_CURVE('',#30830,#30738,#25085,.T.);
#38049=EDGE_CURVE('',#30832,#30830,#17788,.T.);
#38050=EDGE_CURVE('',#30833,#30832,#17789,.T.);
#38051=EDGE_CURVE('',#30831,#30833,#17790,.T.);
#38052=EDGE_CURVE('',#30739,#30833,#25086,.T.);
#38053=EDGE_CURVE('',#30834,#30835,#22492,.T.);
#38054=EDGE_CURVE('',#30458,#30835,#22493,.T.);
#38055=EDGE_CURVE('',#30834,#30739,#25087,.T.);
#38056=EDGE_CURVE('',#30836,#30834,#17791,.T.);
#38057=EDGE_CURVE('',#30837,#30836,#17792,.T.);
#38058=EDGE_CURVE('',#30835,#30837,#17793,.T.);
#38059=EDGE_CURVE('',#30740,#30837,#25088,.T.);
#38060=EDGE_CURVE('',#30838,#30839,#22494,.T.);
#38061=EDGE_CURVE('',#30459,#30839,#22495,.T.);
#38062=EDGE_CURVE('',#30838,#30740,#25089,.T.);
#38063=EDGE_CURVE('',#30840,#30838,#17794,.T.);
#38064=EDGE_CURVE('',#30841,#30840,#17795,.T.);
#38065=EDGE_CURVE('',#30839,#30841,#17796,.T.);
#38066=EDGE_CURVE('',#30741,#30841,#25090,.T.);
#38067=EDGE_CURVE('',#30842,#30843,#22496,.T.);
#38068=EDGE_CURVE('',#30460,#30843,#22497,.T.);
#38069=EDGE_CURVE('',#30842,#30741,#25091,.T.);
#38070=EDGE_CURVE('',#30844,#30842,#17797,.T.);
#38071=EDGE_CURVE('',#30845,#30844,#17798,.T.);
#38072=EDGE_CURVE('',#30843,#30845,#17799,.T.);
#38073=EDGE_CURVE('',#30742,#30845,#25092,.T.);
#38074=EDGE_CURVE('',#30846,#30847,#22498,.T.);
#38075=EDGE_CURVE('',#30461,#30847,#22499,.T.);
#38076=EDGE_CURVE('',#30846,#30742,#25093,.T.);
#38077=EDGE_CURVE('',#30848,#30846,#17800,.T.);
#38078=EDGE_CURVE('',#30849,#30848,#17801,.T.);
#38079=EDGE_CURVE('',#30847,#30849,#17802,.T.);
#38080=EDGE_CURVE('',#30743,#30849,#25094,.T.);
#38081=EDGE_CURVE('',#30850,#30851,#22500,.T.);
#38082=EDGE_CURVE('',#30462,#30851,#22501,.T.);
#38083=EDGE_CURVE('',#30850,#30743,#25095,.T.);
#38084=EDGE_CURVE('',#30852,#30850,#17803,.T.);
#38085=EDGE_CURVE('',#30853,#30852,#17804,.T.);
#38086=EDGE_CURVE('',#30851,#30853,#17805,.T.);
#38087=EDGE_CURVE('',#30744,#30853,#25096,.T.);
#38088=EDGE_CURVE('',#30854,#30855,#22502,.T.);
#38089=EDGE_CURVE('',#30463,#30855,#22503,.T.);
#38090=EDGE_CURVE('',#30854,#30744,#25097,.T.);
#38091=EDGE_CURVE('',#30856,#30854,#17806,.T.);
#38092=EDGE_CURVE('',#30857,#30856,#17807,.T.);
#38093=EDGE_CURVE('',#30855,#30857,#17808,.T.);
#38094=EDGE_CURVE('',#30745,#30857,#25098,.T.);
#38095=EDGE_CURVE('',#30858,#30859,#22504,.T.);
#38096=EDGE_CURVE('',#30464,#30859,#22505,.T.);
#38097=EDGE_CURVE('',#30858,#30745,#25099,.T.);
#38098=EDGE_CURVE('',#30860,#30858,#17809,.T.);
#38099=EDGE_CURVE('',#30861,#30860,#17810,.T.);
#38100=EDGE_CURVE('',#30859,#30861,#17811,.T.);
#38101=EDGE_CURVE('',#30746,#30861,#25100,.T.);
#38102=EDGE_CURVE('',#30862,#30863,#22506,.T.);
#38103=EDGE_CURVE('',#30465,#30863,#22507,.T.);
#38104=EDGE_CURVE('',#30862,#30746,#25101,.T.);
#38105=EDGE_CURVE('',#30864,#30862,#17812,.T.);
#38106=EDGE_CURVE('',#30865,#30864,#17813,.T.);
#38107=EDGE_CURVE('',#30863,#30865,#17814,.T.);
#38108=EDGE_CURVE('',#30747,#30865,#25102,.T.);
#38109=EDGE_CURVE('',#30866,#30867,#22508,.T.);
#38110=EDGE_CURVE('',#30466,#30867,#22509,.T.);
#38111=EDGE_CURVE('',#30866,#30747,#25103,.T.);
#38112=EDGE_CURVE('',#30867,#30868,#17815,.T.);
#38113=EDGE_CURVE('',#30748,#30868,#25104,.T.);
#38114=EDGE_CURVE('',#30869,#30866,#17816,.T.);
#38115=EDGE_CURVE('',#30868,#30869,#17817,.T.);
#38116=EDGE_CURVE('',#30870,#30748,#25105,.T.);
#38117=EDGE_CURVE('',#30870,#30871,#22510,.T.);
#38118=EDGE_CURVE('',#30467,#30871,#22511,.T.);
#38119=EDGE_CURVE('',#30871,#30872,#17818,.T.);
#38120=EDGE_CURVE('',#30873,#30870,#17819,.T.);
#38121=EDGE_CURVE('',#30872,#30873,#17820,.T.);
#38122=EDGE_CURVE('',#30749,#30872,#25106,.T.);
#38123=EDGE_CURVE('',#30874,#30875,#22512,.T.);
#38124=EDGE_CURVE('',#30468,#30875,#22513,.T.);
#38125=EDGE_CURVE('',#30874,#30749,#25107,.T.);
#38126=EDGE_CURVE('',#30876,#30874,#17821,.T.);
#38127=EDGE_CURVE('',#30877,#30876,#17822,.T.);
#38128=EDGE_CURVE('',#30875,#30877,#17823,.T.);
#38129=EDGE_CURVE('',#30750,#30877,#25108,.T.);
#38130=EDGE_CURVE('',#30878,#30879,#22514,.T.);
#38131=EDGE_CURVE('',#30469,#30879,#22515,.T.);
#38132=EDGE_CURVE('',#30878,#30750,#25109,.T.);
#38133=EDGE_CURVE('',#30880,#30878,#17824,.T.);
#38134=EDGE_CURVE('',#30881,#30880,#17825,.T.);
#38135=EDGE_CURVE('',#30879,#30881,#17826,.T.);
#38136=EDGE_CURVE('',#30751,#30881,#25110,.T.);
#38137=EDGE_CURVE('',#30882,#30883,#22516,.T.);
#38138=EDGE_CURVE('',#30470,#30883,#22517,.T.);
#38139=EDGE_CURVE('',#30882,#30751,#25111,.T.);
#38140=EDGE_CURVE('',#30884,#30882,#17827,.T.);
#38141=EDGE_CURVE('',#30885,#30884,#17828,.T.);
#38142=EDGE_CURVE('',#30883,#30885,#17829,.T.);
#38143=EDGE_CURVE('',#30752,#30885,#25112,.T.);
#38144=EDGE_CURVE('',#30886,#30887,#22518,.T.);
#38145=EDGE_CURVE('',#30471,#30887,#22519,.T.);
#38146=EDGE_CURVE('',#30886,#30752,#25113,.T.);
#38147=EDGE_CURVE('',#30888,#30886,#17830,.T.);
#38148=EDGE_CURVE('',#30889,#30888,#17831,.T.);
#38149=EDGE_CURVE('',#30887,#30889,#17832,.T.);
#38150=EDGE_CURVE('',#30753,#30889,#25114,.T.);
#38151=EDGE_CURVE('',#30890,#30891,#22520,.T.);
#38152=EDGE_CURVE('',#30472,#30891,#22521,.T.);
#38153=EDGE_CURVE('',#30890,#30753,#25115,.T.);
#38154=EDGE_CURVE('',#30892,#30890,#17833,.T.);
#38155=EDGE_CURVE('',#30893,#30892,#17834,.T.);
#38156=EDGE_CURVE('',#30891,#30893,#17835,.T.);
#38157=EDGE_CURVE('',#30754,#30893,#25116,.T.);
#38158=EDGE_CURVE('',#30894,#30895,#17836,.T.);
#38159=EDGE_CURVE('',#30785,#30894,#17837,.T.);
#38160=EDGE_CURVE('',#30895,#30784,#22522,.T.);
#38161=EDGE_CURVE('',#30895,#30754,#25117,.T.);
#38162=EDGE_CURVE('',#30896,#30473,#22523,.T.);
#38163=EDGE_CURVE('',#30896,#30897,#17838,.T.);
#38164=EDGE_CURVE('',#30755,#30897,#25118,.T.);
#38165=EDGE_CURVE('',#30898,#30755,#25119,.T.);
#38166=EDGE_CURVE('',#30898,#30899,#22524,.T.);
#38167=EDGE_CURVE('',#30474,#30899,#22525,.T.);
#38168=EDGE_CURVE('',#30899,#30900,#17839,.T.);
#38169=EDGE_CURVE('',#30756,#30900,#25120,.T.);
#38170=EDGE_CURVE('',#30901,#30898,#17840,.T.);
#38171=EDGE_CURVE('',#30900,#30901,#17841,.T.);
#38172=EDGE_CURVE('',#30902,#30756,#25121,.T.);
#38173=EDGE_CURVE('',#30902,#30903,#22526,.T.);
#38174=EDGE_CURVE('',#30475,#30903,#22527,.T.);
#38175=EDGE_CURVE('',#30903,#30904,#17842,.T.);
#38176=EDGE_CURVE('',#30757,#30904,#25122,.T.);
#38177=EDGE_CURVE('',#30905,#30902,#17843,.T.);
#38178=EDGE_CURVE('',#30904,#30905,#17844,.T.);
#38179=EDGE_CURVE('',#30906,#30757,#25123,.T.);
#38180=EDGE_CURVE('',#30906,#30907,#22528,.T.);
#38181=EDGE_CURVE('',#30476,#30907,#22529,.T.);
#38182=EDGE_CURVE('',#30907,#30908,#17845,.T.);
#38183=EDGE_CURVE('',#30758,#30908,#25124,.T.);
#38184=EDGE_CURVE('',#30909,#30906,#17846,.T.);
#38185=EDGE_CURVE('',#30908,#30909,#17847,.T.);
#38186=EDGE_CURVE('',#30910,#30758,#25125,.T.);
#38187=EDGE_CURVE('',#30910,#30911,#22530,.T.);
#38188=EDGE_CURVE('',#30477,#30911,#22531,.T.);
#38189=EDGE_CURVE('',#30911,#30912,#17848,.T.);
#38190=EDGE_CURVE('',#30759,#30912,#25126,.T.);
#38191=EDGE_CURVE('',#30913,#30910,#17849,.T.);
#38192=EDGE_CURVE('',#30912,#30913,#17850,.T.);
#38193=EDGE_CURVE('',#30914,#30759,#25127,.T.);
#38194=EDGE_CURVE('',#30914,#30915,#22532,.T.);
#38195=EDGE_CURVE('',#30478,#30915,#22533,.T.);
#38196=EDGE_CURVE('',#30915,#30916,#17851,.T.);
#38197=EDGE_CURVE('',#30760,#30916,#25128,.T.);
#38198=EDGE_CURVE('',#30917,#30914,#17852,.T.);
#38199=EDGE_CURVE('',#30916,#30917,#17853,.T.);
#38200=EDGE_CURVE('',#30918,#30760,#25129,.T.);
#38201=EDGE_CURVE('',#30918,#30919,#22534,.T.);
#38202=EDGE_CURVE('',#30479,#30919,#22535,.T.);
#38203=EDGE_CURVE('',#30919,#30920,#17854,.T.);
#38204=EDGE_CURVE('',#30761,#30920,#25130,.T.);
#38205=EDGE_CURVE('',#30921,#30918,#17855,.T.);
#38206=EDGE_CURVE('',#30920,#30921,#17856,.T.);
#38207=EDGE_CURVE('',#30922,#30761,#25131,.T.);
#38208=EDGE_CURVE('',#30922,#30923,#22536,.T.);
#38209=EDGE_CURVE('',#30480,#30923,#22537,.T.);
#38210=EDGE_CURVE('',#30923,#30924,#17857,.T.);
#38211=EDGE_CURVE('',#30762,#30924,#25132,.T.);
#38212=EDGE_CURVE('',#30925,#30922,#17858,.T.);
#38213=EDGE_CURVE('',#30924,#30925,#17859,.T.);
#38214=EDGE_CURVE('',#30926,#30762,#25133,.T.);
#38215=EDGE_CURVE('',#30926,#30927,#22538,.T.);
#38216=EDGE_CURVE('',#30481,#30927,#22539,.T.);
#38217=EDGE_CURVE('',#30927,#30928,#17860,.T.);
#38218=EDGE_CURVE('',#30763,#30928,#25134,.T.);
#38219=EDGE_CURVE('',#30929,#30926,#17861,.T.);
#38220=EDGE_CURVE('',#30928,#30929,#17862,.T.);
#38221=EDGE_CURVE('',#30930,#30763,#25135,.T.);
#38222=EDGE_CURVE('',#30930,#30931,#22540,.T.);
#38223=EDGE_CURVE('',#30482,#30931,#22541,.T.);
#38224=EDGE_CURVE('',#30931,#30932,#17863,.T.);
#38225=EDGE_CURVE('',#30764,#30932,#25136,.T.);
#38226=EDGE_CURVE('',#30933,#30930,#17864,.T.);
#38227=EDGE_CURVE('',#30932,#30933,#17865,.T.);
#38228=EDGE_CURVE('',#30934,#30764,#25137,.T.);
#38229=EDGE_CURVE('',#30934,#30935,#22542,.T.);
#38230=EDGE_CURVE('',#30483,#30935,#22543,.T.);
#38231=EDGE_CURVE('',#30935,#30936,#17866,.T.);
#38232=EDGE_CURVE('',#30765,#30936,#25138,.T.);
#38233=EDGE_CURVE('',#30937,#30934,#17867,.T.);
#38234=EDGE_CURVE('',#30936,#30937,#17868,.T.);
#38235=EDGE_CURVE('',#30938,#30765,#25139,.T.);
#38236=EDGE_CURVE('',#30938,#30939,#22544,.T.);
#38237=EDGE_CURVE('',#30484,#30939,#22545,.T.);
#38238=EDGE_CURVE('',#30939,#30940,#17869,.T.);
#38239=EDGE_CURVE('',#30766,#30940,#25140,.T.);
#38240=EDGE_CURVE('',#30941,#30938,#17870,.T.);
#38241=EDGE_CURVE('',#30940,#30941,#17871,.T.);
#38242=EDGE_CURVE('',#30942,#30766,#25141,.T.);
#38243=EDGE_CURVE('',#30942,#30943,#22546,.T.);
#38244=EDGE_CURVE('',#30485,#30943,#22547,.T.);
#38245=EDGE_CURVE('',#30943,#30944,#17872,.T.);
#38246=EDGE_CURVE('',#30767,#30944,#25142,.T.);
#38247=EDGE_CURVE('',#30945,#30942,#17873,.T.);
#38248=EDGE_CURVE('',#30944,#30945,#17874,.T.);
#38249=EDGE_CURVE('',#30946,#30767,#25143,.T.);
#38250=EDGE_CURVE('',#30946,#30947,#22548,.T.);
#38251=EDGE_CURVE('',#30486,#30947,#22549,.T.);
#38252=EDGE_CURVE('',#30947,#30948,#17875,.T.);
#38253=EDGE_CURVE('',#30768,#30948,#25144,.T.);
#38254=EDGE_CURVE('',#30949,#30946,#17876,.T.);
#38255=EDGE_CURVE('',#30948,#30949,#17877,.T.);
#38256=EDGE_CURVE('',#28981,#30768,#25145,.T.);
#38257=EDGE_CURVE('',#30487,#28980,#22550,.T.);
#38258=EDGE_CURVE('',#30769,#28978,#25146,.T.);
#38259=EDGE_CURVE('',#30950,#30769,#25147,.T.);
#38260=EDGE_CURVE('',#30950,#30951,#22551,.T.);
#38261=EDGE_CURVE('',#30488,#30951,#22552,.T.);
#38262=EDGE_CURVE('',#30951,#30952,#17878,.T.);
#38263=EDGE_CURVE('',#30770,#30952,#25148,.T.);
#38264=EDGE_CURVE('',#30953,#30950,#17879,.T.);
#38265=EDGE_CURVE('',#30952,#30953,#17880,.T.);
#38266=EDGE_CURVE('',#30954,#30770,#25149,.T.);
#38267=EDGE_CURVE('',#30954,#30955,#22553,.T.);
#38268=EDGE_CURVE('',#30489,#30955,#22554,.T.);
#38269=EDGE_CURVE('',#30955,#30956,#17881,.T.);
#38270=EDGE_CURVE('',#30771,#30956,#25150,.T.);
#38271=EDGE_CURVE('',#30957,#30954,#17882,.T.);
#38272=EDGE_CURVE('',#30956,#30957,#17883,.T.);
#38273=EDGE_CURVE('',#30958,#30771,#25151,.T.);
#38274=EDGE_CURVE('',#30958,#30959,#22555,.T.);
#38275=EDGE_CURVE('',#30490,#30959,#22556,.T.);
#38276=EDGE_CURVE('',#30959,#30960,#17884,.T.);
#38277=EDGE_CURVE('',#30772,#30960,#25152,.T.);
#38278=EDGE_CURVE('',#30961,#30958,#17885,.T.);
#38279=EDGE_CURVE('',#30960,#30961,#17886,.T.);
#38280=EDGE_CURVE('',#30962,#30772,#25153,.T.);
#38281=EDGE_CURVE('',#30962,#30963,#22557,.T.);
#38282=EDGE_CURVE('',#30491,#30963,#22558,.T.);
#38283=EDGE_CURVE('',#30963,#30964,#17887,.T.);
#38284=EDGE_CURVE('',#30773,#30964,#25154,.T.);
#38285=EDGE_CURVE('',#30965,#30962,#17888,.T.);
#38286=EDGE_CURVE('',#30964,#30965,#17889,.T.);
#38287=EDGE_CURVE('',#30966,#30773,#25155,.T.);
#38288=EDGE_CURVE('',#30966,#30967,#22559,.T.);
#38289=EDGE_CURVE('',#30492,#30967,#22560,.T.);
#38290=EDGE_CURVE('',#30967,#30968,#17890,.T.);
#38291=EDGE_CURVE('',#30774,#30968,#25156,.T.);
#38292=EDGE_CURVE('',#30969,#30966,#17891,.T.);
#38293=EDGE_CURVE('',#30968,#30969,#17892,.T.);
#38294=EDGE_CURVE('',#30970,#30774,#25157,.T.);
#38295=EDGE_CURVE('',#30970,#30971,#22561,.T.);
#38296=EDGE_CURVE('',#30493,#30971,#22562,.T.);
#38297=EDGE_CURVE('',#30971,#30972,#17893,.T.);
#38298=EDGE_CURVE('',#30775,#30972,#25158,.T.);
#38299=EDGE_CURVE('',#30973,#30970,#17894,.T.);
#38300=EDGE_CURVE('',#30972,#30973,#17895,.T.);
#38301=EDGE_CURVE('',#30974,#30775,#25159,.T.);
#38302=EDGE_CURVE('',#30974,#30975,#22563,.T.);
#38303=EDGE_CURVE('',#30494,#30975,#22564,.T.);
#38304=EDGE_CURVE('',#30975,#30976,#17896,.T.);
#38305=EDGE_CURVE('',#30776,#30976,#25160,.T.);
#38306=EDGE_CURVE('',#30977,#30974,#17897,.T.);
#38307=EDGE_CURVE('',#30976,#30977,#17898,.T.);
#38308=EDGE_CURVE('',#30978,#30776,#25161,.T.);
#38309=EDGE_CURVE('',#30978,#30979,#22565,.T.);
#38310=EDGE_CURVE('',#30495,#30979,#22566,.T.);
#38311=EDGE_CURVE('',#30979,#30980,#17899,.T.);
#38312=EDGE_CURVE('',#30777,#30980,#25162,.T.);
#38313=EDGE_CURVE('',#30981,#30978,#17900,.T.);
#38314=EDGE_CURVE('',#30980,#30981,#17901,.T.);
#38315=EDGE_CURVE('',#30982,#30777,#25163,.T.);
#38316=EDGE_CURVE('',#30982,#30983,#22567,.T.);
#38317=EDGE_CURVE('',#30496,#30983,#22568,.T.);
#38318=EDGE_CURVE('',#30983,#30984,#17902,.T.);
#38319=EDGE_CURVE('',#30778,#30984,#25164,.T.);
#38320=EDGE_CURVE('',#30985,#30982,#17903,.T.);
#38321=EDGE_CURVE('',#30984,#30985,#17904,.T.);
#38322=EDGE_CURVE('',#30986,#30778,#25165,.T.);
#38323=EDGE_CURVE('',#30986,#30987,#22569,.T.);
#38324=EDGE_CURVE('',#30497,#30987,#22570,.T.);
#38325=EDGE_CURVE('',#30987,#30988,#17905,.T.);
#38326=EDGE_CURVE('',#30779,#30988,#25166,.T.);
#38327=EDGE_CURVE('',#30989,#30986,#17906,.T.);
#38328=EDGE_CURVE('',#30988,#30989,#17907,.T.);
#38329=EDGE_CURVE('',#30990,#30779,#25167,.T.);
#38330=EDGE_CURVE('',#30990,#30991,#22571,.T.);
#38331=EDGE_CURVE('',#30498,#30991,#22572,.T.);
#38332=EDGE_CURVE('',#30991,#30992,#17908,.T.);
#38333=EDGE_CURVE('',#30780,#30992,#25168,.T.);
#38334=EDGE_CURVE('',#30993,#30990,#17909,.T.);
#38335=EDGE_CURVE('',#30992,#30993,#17910,.T.);
#38336=EDGE_CURVE('',#30994,#30780,#25169,.T.);
#38337=EDGE_CURVE('',#30994,#30995,#22573,.T.);
#38338=EDGE_CURVE('',#30499,#30995,#22574,.T.);
#38339=EDGE_CURVE('',#30995,#30996,#17911,.T.);
#38340=EDGE_CURVE('',#30781,#30996,#25170,.T.);
#38341=EDGE_CURVE('',#30997,#30994,#17912,.T.);
#38342=EDGE_CURVE('',#30996,#30997,#17913,.T.);
#38343=EDGE_CURVE('',#30998,#30781,#25171,.T.);
#38344=EDGE_CURVE('',#30998,#30999,#22575,.T.);
#38345=EDGE_CURVE('',#30500,#30999,#22576,.T.);
#38346=EDGE_CURVE('',#30999,#31000,#17914,.T.);
#38347=EDGE_CURVE('',#30782,#31000,#25172,.T.);
#38348=EDGE_CURVE('',#31001,#30998,#17915,.T.);
#38349=EDGE_CURVE('',#31000,#31001,#17916,.T.);
#38350=EDGE_CURVE('',#31002,#30782,#25173,.T.);
#38351=EDGE_CURVE('',#31002,#31003,#22577,.T.);
#38352=EDGE_CURVE('',#30501,#31003,#22578,.T.);
#38353=EDGE_CURVE('',#31003,#31004,#17917,.T.);
#38354=EDGE_CURVE('',#30783,#31004,#25174,.T.);
#38355=EDGE_CURVE('',#31005,#31002,#17918,.T.);
#38356=EDGE_CURVE('',#31004,#31005,#17919,.T.);
#38357=EDGE_CURVE('',#31006,#30896,#22579,.T.);
#38358=EDGE_CURVE('',#31007,#31006,#17920,.T.);
#38359=EDGE_CURVE('',#30897,#31007,#17921,.T.);
#38360=EDGE_CURVE('',#31006,#30783,#25175,.T.);
#38361=EDGE_CURVE('',#30726,#31008,#17922,.T.);
#38362=EDGE_CURVE('',#31008,#30894,#22580,.T.);
#38363=EDGE_CURVE('',#31009,#30726,#17923,.T.);
#38364=EDGE_CURVE('',#30788,#31009,#22581,.T.);
#38365=EDGE_CURVE('',#30727,#31009,#17924,.T.);
#38366=EDGE_CURVE('',#31010,#30727,#17925,.T.);
#38367=EDGE_CURVE('',#30792,#31010,#22582,.T.);
#38368=EDGE_CURVE('',#30728,#31010,#17926,.T.);
#38369=EDGE_CURVE('',#31011,#30728,#17927,.T.);
#38370=EDGE_CURVE('',#30796,#31011,#22583,.T.);
#38371=EDGE_CURVE('',#30729,#31011,#17928,.T.);
#38372=EDGE_CURVE('',#31012,#30729,#17929,.T.);
#38373=EDGE_CURVE('',#30800,#31012,#22584,.T.);
#38374=EDGE_CURVE('',#30730,#31012,#17930,.T.);
#38375=EDGE_CURVE('',#31013,#30730,#17931,.T.);
#38376=EDGE_CURVE('',#30804,#31013,#22585,.T.);
#38377=EDGE_CURVE('',#30731,#31013,#17932,.T.);
#38378=EDGE_CURVE('',#31014,#30731,#17933,.T.);
#38379=EDGE_CURVE('',#30808,#31014,#22586,.T.);
#38380=EDGE_CURVE('',#30732,#31014,#17934,.T.);
#38381=EDGE_CURVE('',#31015,#30732,#17935,.T.);
#38382=EDGE_CURVE('',#28985,#31015,#22587,.T.);
#38383=EDGE_CURVE('',#30733,#31015,#17936,.T.);
#38384=EDGE_CURVE('',#31016,#30733,#17937,.T.);
#38385=EDGE_CURVE('',#30812,#31016,#22588,.T.);
#38386=EDGE_CURVE('',#30734,#31016,#17938,.T.);
#38387=EDGE_CURVE('',#31017,#30734,#17939,.T.);
#38388=EDGE_CURVE('',#30816,#31017,#22589,.T.);
#38389=EDGE_CURVE('',#30735,#31017,#17940,.T.);
#38390=EDGE_CURVE('',#31018,#30735,#17941,.T.);
#38391=EDGE_CURVE('',#30820,#31018,#22590,.T.);
#38392=EDGE_CURVE('',#30736,#31018,#17942,.T.);
#38393=EDGE_CURVE('',#31019,#30736,#17943,.T.);
#38394=EDGE_CURVE('',#30824,#31019,#22591,.T.);
#38395=EDGE_CURVE('',#30737,#31019,#17944,.T.);
#38396=EDGE_CURVE('',#31020,#30737,#17945,.T.);
#38397=EDGE_CURVE('',#30828,#31020,#22592,.T.);
#38398=EDGE_CURVE('',#30738,#31020,#17946,.T.);
#38399=EDGE_CURVE('',#31021,#30738,#17947,.T.);
#38400=EDGE_CURVE('',#30832,#31021,#22593,.T.);
#38401=EDGE_CURVE('',#30739,#31021,#17948,.T.);
#38402=EDGE_CURVE('',#31022,#30739,#17949,.T.);
#38403=EDGE_CURVE('',#30836,#31022,#22594,.T.);
#38404=EDGE_CURVE('',#30740,#31022,#17950,.T.);
#38405=EDGE_CURVE('',#31023,#30740,#17951,.T.);
#38406=EDGE_CURVE('',#30840,#31023,#22595,.T.);
#38407=EDGE_CURVE('',#30741,#31023,#17952,.T.);
#38408=EDGE_CURVE('',#31024,#30741,#17953,.T.);
#38409=EDGE_CURVE('',#30844,#31024,#22596,.T.);
#38410=EDGE_CURVE('',#30742,#31024,#17954,.T.);
#38411=EDGE_CURVE('',#31025,#30742,#17955,.T.);
#38412=EDGE_CURVE('',#30848,#31025,#22597,.T.);
#38413=EDGE_CURVE('',#30743,#31025,#17956,.T.);
#38414=EDGE_CURVE('',#31026,#30743,#17957,.T.);
#38415=EDGE_CURVE('',#30852,#31026,#22598,.T.);
#38416=EDGE_CURVE('',#30744,#31026,#17958,.T.);
#38417=EDGE_CURVE('',#31027,#30744,#17959,.T.);
#38418=EDGE_CURVE('',#30856,#31027,#22599,.T.);
#38419=EDGE_CURVE('',#30745,#31027,#17960,.T.);
#38420=EDGE_CURVE('',#31028,#30745,#17961,.T.);
#38421=EDGE_CURVE('',#30860,#31028,#22600,.T.);
#38422=EDGE_CURVE('',#30746,#31028,#17962,.T.);
#38423=EDGE_CURVE('',#31029,#30746,#17963,.T.);
#38424=EDGE_CURVE('',#30864,#31029,#22601,.T.);
#38425=EDGE_CURVE('',#30747,#31029,#17964,.T.);
#38426=EDGE_CURVE('',#31030,#30747,#17965,.T.);
#38427=EDGE_CURVE('',#30869,#31030,#22602,.T.);
#38428=EDGE_CURVE('',#30748,#31030,#17966,.T.);
#38429=EDGE_CURVE('',#31031,#30748,#17967,.T.);
#38430=EDGE_CURVE('',#30873,#31031,#22603,.T.);
#38431=EDGE_CURVE('',#30749,#31031,#17968,.T.);
#38432=EDGE_CURVE('',#31032,#30749,#17969,.T.);
#38433=EDGE_CURVE('',#30876,#31032,#22604,.T.);
#38434=EDGE_CURVE('',#30750,#31032,#17970,.T.);
#38435=EDGE_CURVE('',#31033,#30750,#17971,.T.);
#38436=EDGE_CURVE('',#30880,#31033,#22605,.T.);
#38437=EDGE_CURVE('',#30751,#31033,#17972,.T.);
#38438=EDGE_CURVE('',#31034,#30751,#17973,.T.);
#38439=EDGE_CURVE('',#30884,#31034,#22606,.T.);
#38440=EDGE_CURVE('',#30752,#31034,#17974,.T.);
#38441=EDGE_CURVE('',#31035,#30752,#17975,.T.);
#38442=EDGE_CURVE('',#30888,#31035,#22607,.T.);
#38443=EDGE_CURVE('',#30753,#31035,#17976,.T.);
#38444=EDGE_CURVE('',#31036,#30753,#17977,.T.);
#38445=EDGE_CURVE('',#30892,#31036,#22608,.T.);
#38446=EDGE_CURVE('',#30754,#31036,#17978,.T.);
#38447=EDGE_CURVE('',#31008,#30754,#17979,.T.);
#38448=EDGE_CURVE('',#31037,#31007,#22609,.T.);
#38449=EDGE_CURVE('',#30755,#31037,#17980,.T.);
#38450=EDGE_CURVE('',#31038,#30755,#22610,.T.);
#38451=EDGE_CURVE('',#30901,#31038,#22611,.T.);
#38452=EDGE_CURVE('',#30756,#31038,#17981,.T.);
#38453=EDGE_CURVE('',#31039,#30756,#4426,.T.);
#38454=EDGE_CURVE('',#30905,#31039,#22612,.T.);
#38455=EDGE_CURVE('',#30757,#31039,#17982,.T.);
#38456=EDGE_CURVE('',#31040,#30757,#4427,.T.);
#38457=EDGE_CURVE('',#30909,#31040,#22613,.T.);
#38458=EDGE_CURVE('',#30758,#31040,#17983,.T.);
#38459=EDGE_CURVE('',#31041,#30758,#22614,.T.);
#38460=EDGE_CURVE('',#30913,#31041,#22615,.T.);
#38461=EDGE_CURVE('',#30759,#31041,#17984,.T.);
#38462=EDGE_CURVE('',#31042,#30759,#22616,.T.);
#38463=EDGE_CURVE('',#30917,#31042,#22617,.T.);
#38464=EDGE_CURVE('',#30760,#31042,#17985,.T.);
#38465=EDGE_CURVE('',#31043,#30760,#4428,.T.);
#38466=EDGE_CURVE('',#30921,#31043,#22618,.T.);
#38467=EDGE_CURVE('',#30761,#31043,#17986,.T.);
#38468=EDGE_CURVE('',#31044,#30761,#4429,.T.);
#38469=EDGE_CURVE('',#30925,#31044,#22619,.T.);
#38470=EDGE_CURVE('',#30762,#31044,#17987,.T.);
#38471=EDGE_CURVE('',#31045,#30762,#4430,.T.);
#38472=EDGE_CURVE('',#30929,#31045,#22620,.T.);
#38473=EDGE_CURVE('',#30763,#31045,#17988,.T.);
#38474=EDGE_CURVE('',#31046,#30763,#4431,.T.);
#38475=EDGE_CURVE('',#30933,#31046,#22621,.T.);
#38476=EDGE_CURVE('',#30764,#31046,#17989,.T.);
#38477=EDGE_CURVE('',#31047,#30764,#22622,.T.);
#38478=EDGE_CURVE('',#30937,#31047,#22623,.T.);
#38479=EDGE_CURVE('',#30765,#31047,#17990,.T.);
#38480=EDGE_CURVE('',#31048,#30765,#4432,.T.);
#38481=EDGE_CURVE('',#30941,#31048,#22624,.T.);
#38482=EDGE_CURVE('',#30766,#31048,#17991,.T.);
#38483=EDGE_CURVE('',#31049,#30766,#4433,.T.);
#38484=EDGE_CURVE('',#30945,#31049,#22625,.T.);
#38485=EDGE_CURVE('',#30767,#31049,#17992,.T.);
#38486=EDGE_CURVE('',#31050,#30767,#4434,.T.);
#38487=EDGE_CURVE('',#30949,#31050,#22626,.T.);
#38488=EDGE_CURVE('',#30768,#31050,#17993,.T.);
#38489=EDGE_CURVE('',#31051,#30768,#22627,.T.);
#38490=EDGE_CURVE('',#28979,#31051,#22628,.T.);
#38491=EDGE_CURVE('',#30769,#31051,#17994,.T.);
#38492=EDGE_CURVE('',#31052,#30769,#22629,.T.);
#38493=EDGE_CURVE('',#30953,#31052,#22630,.T.);
#38494=EDGE_CURVE('',#30770,#31052,#17995,.T.);
#38495=EDGE_CURVE('',#31053,#30770,#22631,.T.);
#38496=EDGE_CURVE('',#30957,#31053,#22632,.T.);
#38497=EDGE_CURVE('',#30771,#31053,#17996,.T.);
#38498=EDGE_CURVE('',#31054,#30771,#4435,.T.);
#38499=EDGE_CURVE('',#30961,#31054,#22633,.T.);
#38500=EDGE_CURVE('',#30772,#31054,#17997,.T.);
#38501=EDGE_CURVE('',#31055,#30772,#4436,.T.);
#38502=EDGE_CURVE('',#30965,#31055,#22634,.T.);
#38503=EDGE_CURVE('',#30773,#31055,#17998,.T.);
#38504=EDGE_CURVE('',#31056,#30773,#22635,.T.);
#38505=EDGE_CURVE('',#30969,#31056,#22636,.T.);
#38506=EDGE_CURVE('',#30774,#31056,#17999,.T.);
#38507=EDGE_CURVE('',#31057,#30774,#4437,.T.);
#38508=EDGE_CURVE('',#30973,#31057,#22637,.T.);
#38509=EDGE_CURVE('',#30775,#31057,#18000,.T.);
#38510=EDGE_CURVE('',#31058,#30775,#4438,.T.);
#38511=EDGE_CURVE('',#30977,#31058,#22638,.T.);
#38512=EDGE_CURVE('',#30776,#31058,#18001,.T.);
#38513=EDGE_CURVE('',#31059,#30776,#22639,.T.);
#38514=EDGE_CURVE('',#30981,#31059,#22640,.T.);
#38515=EDGE_CURVE('',#30777,#31059,#18002,.T.);
#38516=EDGE_CURVE('',#31060,#30777,#22641,.T.);
#38517=EDGE_CURVE('',#30985,#31060,#22642,.T.);
#38518=EDGE_CURVE('',#30778,#31060,#18003,.T.);
#38519=EDGE_CURVE('',#31061,#30778,#4439,.T.);
#38520=EDGE_CURVE('',#30989,#31061,#22643,.T.);
#38521=EDGE_CURVE('',#30779,#31061,#18004,.T.);
#38522=EDGE_CURVE('',#31062,#30779,#4440,.T.);
#38523=EDGE_CURVE('',#30993,#31062,#22644,.T.);
#38524=EDGE_CURVE('',#30780,#31062,#18005,.T.);
#38525=EDGE_CURVE('',#31063,#30780,#4441,.T.);
#38526=EDGE_CURVE('',#30997,#31063,#22645,.T.);
#38527=EDGE_CURVE('',#30781,#31063,#18006,.T.);
#38528=EDGE_CURVE('',#31064,#30781,#22646,.T.);
#38529=EDGE_CURVE('',#31001,#31064,#22647,.T.);
#38530=EDGE_CURVE('',#30782,#31064,#18007,.T.);
#38531=EDGE_CURVE('',#31065,#30782,#22648,.T.);
#38532=EDGE_CURVE('',#31005,#31065,#22649,.T.);
#38533=EDGE_CURVE('',#30783,#31065,#18008,.T.);
#38534=EDGE_CURVE('',#31037,#30783,#22650,.T.);
#38535=EDGE_CURVE('',#31066,#31067,#18009,.T.);
#38536=EDGE_CURVE('',#30726,#31067,#22651,.T.);
#38537=EDGE_CURVE('',#31066,#31008,#25176,.T.);
#38538=EDGE_CURVE('',#31068,#31066,#18010,.T.);
#38539=EDGE_CURVE('',#31069,#31068,#18011,.T.);
#38540=EDGE_CURVE('',#31067,#31069,#18012,.T.);
#38541=EDGE_CURVE('',#31009,#31069,#25177,.T.);
#38542=EDGE_CURVE('',#31070,#31071,#18013,.T.);
#38543=EDGE_CURVE('',#30727,#31071,#22652,.T.);
#38544=EDGE_CURVE('',#31070,#31009,#25178,.T.);
#38545=EDGE_CURVE('',#31072,#31070,#18014,.T.);
#38546=EDGE_CURVE('',#31073,#31072,#18015,.T.);
#38547=EDGE_CURVE('',#31071,#31073,#18016,.T.);
#38548=EDGE_CURVE('',#31010,#31073,#25179,.T.);
#38549=EDGE_CURVE('',#31074,#31075,#18017,.T.);
#38550=EDGE_CURVE('',#30728,#31075,#22653,.T.);
#38551=EDGE_CURVE('',#31074,#31010,#25180,.T.);
#38552=EDGE_CURVE('',#31076,#31074,#18018,.T.);
#38553=EDGE_CURVE('',#31077,#31076,#18019,.T.);
#38554=EDGE_CURVE('',#31075,#31077,#18020,.T.);
#38555=EDGE_CURVE('',#31011,#31077,#25181,.T.);
#38556=EDGE_CURVE('',#31078,#31079,#18021,.T.);
#38557=EDGE_CURVE('',#30729,#31079,#22654,.T.);
#38558=EDGE_CURVE('',#31078,#31011,#25182,.T.);
#38559=EDGE_CURVE('',#31080,#31078,#18022,.T.);
#38560=EDGE_CURVE('',#31081,#31080,#18023,.T.);
#38561=EDGE_CURVE('',#31079,#31081,#18024,.T.);
#38562=EDGE_CURVE('',#31012,#31081,#25183,.T.);
#38563=EDGE_CURVE('',#31082,#31083,#18025,.T.);
#38564=EDGE_CURVE('',#30730,#31083,#22655,.T.);
#38565=EDGE_CURVE('',#31082,#31012,#25184,.T.);
#38566=EDGE_CURVE('',#31084,#31082,#18026,.T.);
#38567=EDGE_CURVE('',#31085,#31084,#18027,.T.);
#38568=EDGE_CURVE('',#31083,#31085,#18028,.T.);
#38569=EDGE_CURVE('',#31013,#31085,#25185,.T.);
#38570=EDGE_CURVE('',#31086,#31087,#18029,.T.);
#38571=EDGE_CURVE('',#30731,#31087,#22656,.T.);
#38572=EDGE_CURVE('',#31086,#31013,#25186,.T.);
#38573=EDGE_CURVE('',#31088,#31086,#18030,.T.);
#38574=EDGE_CURVE('',#31089,#31088,#18031,.T.);
#38575=EDGE_CURVE('',#31087,#31089,#18032,.T.);
#38576=EDGE_CURVE('',#31014,#31089,#25187,.T.);
#38577=EDGE_CURVE('',#31090,#31091,#18033,.T.);
#38578=EDGE_CURVE('',#30732,#31091,#22657,.T.);
#38579=EDGE_CURVE('',#31090,#31014,#25188,.T.);
#38580=EDGE_CURVE('',#31092,#31090,#18034,.T.);
#38581=EDGE_CURVE('',#31093,#31092,#18035,.T.);
#38582=EDGE_CURVE('',#31091,#31093,#18036,.T.);
#38583=EDGE_CURVE('',#31015,#31093,#25189,.T.);
#38584=EDGE_CURVE('',#31094,#31095,#18037,.T.);
#38585=EDGE_CURVE('',#30733,#31095,#22658,.T.);
#38586=EDGE_CURVE('',#31094,#31015,#25190,.T.);
#38587=EDGE_CURVE('',#31096,#31094,#18038,.T.);
#38588=EDGE_CURVE('',#31097,#31096,#18039,.T.);
#38589=EDGE_CURVE('',#31095,#31097,#18040,.T.);
#38590=EDGE_CURVE('',#31016,#31097,#25191,.T.);
#38591=EDGE_CURVE('',#31098,#31099,#18041,.T.);
#38592=EDGE_CURVE('',#30734,#31099,#22659,.T.);
#38593=EDGE_CURVE('',#31098,#31016,#25192,.T.);
#38594=EDGE_CURVE('',#31100,#31098,#18042,.T.);
#38595=EDGE_CURVE('',#31101,#31100,#18043,.T.);
#38596=EDGE_CURVE('',#31099,#31101,#18044,.T.);
#38597=EDGE_CURVE('',#31017,#31101,#25193,.T.);
#38598=EDGE_CURVE('',#31102,#31103,#18045,.T.);
#38599=EDGE_CURVE('',#30735,#31103,#22660,.T.);
#38600=EDGE_CURVE('',#31102,#31017,#25194,.T.);
#38601=EDGE_CURVE('',#31104,#31102,#18046,.T.);
#38602=EDGE_CURVE('',#31105,#31104,#18047,.T.);
#38603=EDGE_CURVE('',#31103,#31105,#18048,.T.);
#38604=EDGE_CURVE('',#31018,#31105,#25195,.T.);
#38605=EDGE_CURVE('',#31106,#31107,#18049,.T.);
#38606=EDGE_CURVE('',#30736,#31107,#22661,.T.);
#38607=EDGE_CURVE('',#31106,#31018,#25196,.T.);
#38608=EDGE_CURVE('',#31108,#31106,#18050,.T.);
#38609=EDGE_CURVE('',#31109,#31108,#18051,.T.);
#38610=EDGE_CURVE('',#31107,#31109,#18052,.T.);
#38611=EDGE_CURVE('',#31019,#31109,#25197,.T.);
#38612=EDGE_CURVE('',#31110,#31111,#18053,.T.);
#38613=EDGE_CURVE('',#30737,#31111,#22662,.T.);
#38614=EDGE_CURVE('',#31110,#31019,#25198,.T.);
#38615=EDGE_CURVE('',#31112,#31110,#18054,.T.);
#38616=EDGE_CURVE('',#31113,#31112,#18055,.T.);
#38617=EDGE_CURVE('',#31111,#31113,#18056,.T.);
#38618=EDGE_CURVE('',#31020,#31113,#25199,.T.);
#38619=EDGE_CURVE('',#31114,#31115,#18057,.T.);
#38620=EDGE_CURVE('',#30738,#31115,#22663,.T.);
#38621=EDGE_CURVE('',#31114,#31020,#25200,.T.);
#38622=EDGE_CURVE('',#31116,#31114,#18058,.T.);
#38623=EDGE_CURVE('',#31117,#31116,#18059,.T.);
#38624=EDGE_CURVE('',#31115,#31117,#18060,.T.);
#38625=EDGE_CURVE('',#31021,#31117,#25201,.T.);
#38626=EDGE_CURVE('',#31118,#31119,#18061,.T.);
#38627=EDGE_CURVE('',#30739,#31119,#22664,.T.);
#38628=EDGE_CURVE('',#31118,#31021,#25202,.T.);
#38629=EDGE_CURVE('',#31120,#31118,#18062,.T.);
#38630=EDGE_CURVE('',#31121,#31120,#18063,.T.);
#38631=EDGE_CURVE('',#31119,#31121,#18064,.T.);
#38632=EDGE_CURVE('',#31022,#31121,#25203,.T.);
#38633=EDGE_CURVE('',#30740,#28975,#22665,.T.);
#38634=EDGE_CURVE('',#28974,#31022,#25204,.T.);
#38635=EDGE_CURVE('',#31023,#28977,#25205,.T.);
#38636=EDGE_CURVE('',#31122,#31123,#18065,.T.);
#38637=EDGE_CURVE('',#30741,#31123,#22666,.T.);
#38638=EDGE_CURVE('',#31122,#31023,#25206,.T.);
#38639=EDGE_CURVE('',#31124,#31122,#18066,.T.);
#38640=EDGE_CURVE('',#31125,#31124,#18067,.T.);
#38641=EDGE_CURVE('',#31123,#31125,#18068,.T.);
#38642=EDGE_CURVE('',#31024,#31125,#25207,.T.);
#38643=EDGE_CURVE('',#31126,#31127,#18069,.T.);
#38644=EDGE_CURVE('',#30742,#31127,#22667,.T.);
#38645=EDGE_CURVE('',#31126,#31024,#25208,.T.);
#38646=EDGE_CURVE('',#31128,#31126,#18070,.T.);
#38647=EDGE_CURVE('',#31129,#31128,#18071,.T.);
#38648=EDGE_CURVE('',#31127,#31129,#18072,.T.);
#38649=EDGE_CURVE('',#31025,#31129,#25209,.T.);
#38650=EDGE_CURVE('',#31130,#31131,#18073,.T.);
#38651=EDGE_CURVE('',#30743,#31131,#22668,.T.);
#38652=EDGE_CURVE('',#31130,#31025,#25210,.T.);
#38653=EDGE_CURVE('',#31132,#31130,#18074,.T.);
#38654=EDGE_CURVE('',#31133,#31132,#18075,.T.);
#38655=EDGE_CURVE('',#31131,#31133,#18076,.T.);
#38656=EDGE_CURVE('',#31026,#31133,#25211,.T.);
#38657=EDGE_CURVE('',#31134,#31135,#18077,.T.);
#38658=EDGE_CURVE('',#30744,#31135,#22669,.T.);
#38659=EDGE_CURVE('',#31134,#31026,#25212,.T.);
#38660=EDGE_CURVE('',#31136,#31134,#18078,.T.);
#38661=EDGE_CURVE('',#31137,#31136,#18079,.T.);
#38662=EDGE_CURVE('',#31135,#31137,#18080,.T.);
#38663=EDGE_CURVE('',#31027,#31137,#25213,.T.);
#38664=EDGE_CURVE('',#31138,#31139,#18081,.T.);
#38665=EDGE_CURVE('',#30745,#31139,#22670,.T.);
#38666=EDGE_CURVE('',#31138,#31027,#25214,.T.);
#38667=EDGE_CURVE('',#31140,#31138,#18082,.T.);
#38668=EDGE_CURVE('',#31141,#31140,#18083,.T.);
#38669=EDGE_CURVE('',#31139,#31141,#18084,.T.);
#38670=EDGE_CURVE('',#31028,#31141,#25215,.T.);
#38671=EDGE_CURVE('',#31142,#31143,#18085,.T.);
#38672=EDGE_CURVE('',#30746,#31143,#22671,.T.);
#38673=EDGE_CURVE('',#31142,#31028,#25216,.T.);
#38674=EDGE_CURVE('',#31144,#31142,#18086,.T.);
#38675=EDGE_CURVE('',#31145,#31144,#18087,.T.);
#38676=EDGE_CURVE('',#31143,#31145,#18088,.T.);
#38677=EDGE_CURVE('',#31029,#31145,#25217,.T.);
#38678=EDGE_CURVE('',#31146,#31147,#18089,.T.);
#38679=EDGE_CURVE('',#30747,#31147,#22672,.T.);
#38680=EDGE_CURVE('',#31146,#31029,#25218,.T.);
#38681=EDGE_CURVE('',#31147,#31148,#18090,.T.);
#38682=EDGE_CURVE('',#31030,#31148,#25219,.T.);
#38683=EDGE_CURVE('',#31149,#31146,#18091,.T.);
#38684=EDGE_CURVE('',#31148,#31149,#18092,.T.);
#38685=EDGE_CURVE('',#31150,#31030,#25220,.T.);
#38686=EDGE_CURVE('',#31150,#31151,#18093,.T.);
#38687=EDGE_CURVE('',#30748,#31151,#22673,.T.);
#38688=EDGE_CURVE('',#31151,#31152,#18094,.T.);
#38689=EDGE_CURVE('',#31153,#31150,#18095,.T.);
#38690=EDGE_CURVE('',#31152,#31153,#18096,.T.);
#38691=EDGE_CURVE('',#31031,#31152,#25221,.T.);
#38692=EDGE_CURVE('',#31154,#31155,#18097,.T.);
#38693=EDGE_CURVE('',#30749,#31155,#22674,.T.);
#38694=EDGE_CURVE('',#31154,#31031,#25222,.T.);
#38695=EDGE_CURVE('',#31156,#31154,#18098,.T.);
#38696=EDGE_CURVE('',#31157,#31156,#18099,.T.);
#38697=EDGE_CURVE('',#31155,#31157,#18100,.T.);
#38698=EDGE_CURVE('',#31032,#31157,#25223,.T.);
#38699=EDGE_CURVE('',#31158,#31159,#18101,.T.);
#38700=EDGE_CURVE('',#30750,#31159,#22675,.T.);
#38701=EDGE_CURVE('',#31158,#31032,#25224,.T.);
#38702=EDGE_CURVE('',#31160,#31158,#18102,.T.);
#38703=EDGE_CURVE('',#31161,#31160,#18103,.T.);
#38704=EDGE_CURVE('',#31159,#31161,#18104,.T.);
#38705=EDGE_CURVE('',#31033,#31161,#25225,.T.);
#38706=EDGE_CURVE('',#31162,#31163,#18105,.T.);
#38707=EDGE_CURVE('',#30751,#31163,#22676,.T.);
#38708=EDGE_CURVE('',#31162,#31033,#25226,.T.);
#38709=EDGE_CURVE('',#31164,#31162,#18106,.T.);
#38710=EDGE_CURVE('',#31165,#31164,#18107,.T.);
#38711=EDGE_CURVE('',#31163,#31165,#18108,.T.);
#38712=EDGE_CURVE('',#31034,#31165,#25227,.T.);
#38713=EDGE_CURVE('',#31166,#31167,#18109,.T.);
#38714=EDGE_CURVE('',#30752,#31167,#22677,.T.);
#38715=EDGE_CURVE('',#31166,#31034,#25228,.T.);
#38716=EDGE_CURVE('',#31168,#31166,#18110,.T.);
#38717=EDGE_CURVE('',#31169,#31168,#18111,.T.);
#38718=EDGE_CURVE('',#31167,#31169,#18112,.T.);
#38719=EDGE_CURVE('',#31035,#31169,#25229,.T.);
#38720=EDGE_CURVE('',#31170,#31171,#18113,.T.);
#38721=EDGE_CURVE('',#30753,#31171,#22678,.T.);
#38722=EDGE_CURVE('',#31170,#31035,#25230,.T.);
#38723=EDGE_CURVE('',#31172,#31170,#18114,.T.);
#38724=EDGE_CURVE('',#31173,#31172,#18115,.T.);
#38725=EDGE_CURVE('',#31171,#31173,#18116,.T.);
#38726=EDGE_CURVE('',#31036,#31173,#25231,.T.);
#38727=EDGE_CURVE('',#31174,#31175,#18117,.T.);
#38728=EDGE_CURVE('',#30754,#31175,#22679,.T.);
#38729=EDGE_CURVE('',#31174,#31036,#25232,.T.);
#38730=EDGE_CURVE('',#31176,#31174,#18118,.T.);
#38731=EDGE_CURVE('',#31177,#31176,#18119,.T.);
#38732=EDGE_CURVE('',#31175,#31177,#18120,.T.);
#38733=EDGE_CURVE('',#31008,#31177,#25233,.T.);
#38734=EDGE_CURVE('',#31178,#31037,#25234,.T.);
#38735=EDGE_CURVE('',#31178,#31179,#18121,.T.);
#38736=EDGE_CURVE('',#30755,#31179,#22680,.T.);
#38737=EDGE_CURVE('',#31179,#31180,#22681,.T.);
#38738=EDGE_CURVE('',#31038,#31180,#25235,.T.);
#38739=EDGE_CURVE('',#31181,#31178,#18122,.T.);
#38740=EDGE_CURVE('',#31180,#31181,#18123,.T.);
#38741=EDGE_CURVE('',#31182,#31038,#25236,.T.);
#38742=EDGE_CURVE('',#31182,#31183,#18124,.T.);
#38743=EDGE_CURVE('',#30756,#31183,#22682,.T.);
#38744=EDGE_CURVE('',#31183,#31184,#22683,.T.);
#38745=EDGE_CURVE('',#31039,#31184,#25237,.T.);
#38746=EDGE_CURVE('',#31185,#31182,#18125,.T.);
#38747=EDGE_CURVE('',#31184,#31185,#18126,.T.);
#38748=EDGE_CURVE('',#31186,#31039,#25238,.T.);
#38749=EDGE_CURVE('',#31186,#31187,#18127,.T.);
#38750=EDGE_CURVE('',#30757,#31187,#22684,.T.);
#38751=EDGE_CURVE('',#31187,#31188,#22685,.T.);
#38752=EDGE_CURVE('',#31040,#31188,#25239,.T.);
#38753=EDGE_CURVE('',#31189,#31186,#18128,.T.);
#38754=EDGE_CURVE('',#31188,#31189,#18129,.T.);
#38755=EDGE_CURVE('',#31190,#31040,#25240,.T.);
#38756=EDGE_CURVE('',#31190,#31191,#18130,.T.);
#38757=EDGE_CURVE('',#30758,#31191,#22686,.T.);
#38758=EDGE_CURVE('',#31191,#31192,#22687,.T.);
#38759=EDGE_CURVE('',#31041,#31192,#25241,.T.);
#38760=EDGE_CURVE('',#31193,#31190,#18131,.T.);
#38761=EDGE_CURVE('',#31192,#31193,#18132,.T.);
#38762=EDGE_CURVE('',#31194,#31041,#25242,.T.);
#38763=EDGE_CURVE('',#31194,#31195,#18133,.T.);
#38764=EDGE_CURVE('',#30759,#31195,#22688,.T.);
#38765=EDGE_CURVE('',#31195,#31196,#22689,.T.);
#38766=EDGE_CURVE('',#31042,#31196,#25243,.T.);
#38767=EDGE_CURVE('',#31197,#31194,#18134,.T.);
#38768=EDGE_CURVE('',#31196,#31197,#18135,.T.);
#38769=EDGE_CURVE('',#31198,#31042,#25244,.T.);
#38770=EDGE_CURVE('',#31198,#31199,#18136,.T.);
#38771=EDGE_CURVE('',#30760,#31199,#22690,.T.);
#38772=EDGE_CURVE('',#31199,#31200,#22691,.T.);
#38773=EDGE_CURVE('',#31043,#31200,#25245,.T.);
#38774=EDGE_CURVE('',#31201,#31198,#18137,.T.);
#38775=EDGE_CURVE('',#31200,#31201,#18138,.T.);
#38776=EDGE_CURVE('',#31202,#31043,#25246,.T.);
#38777=EDGE_CURVE('',#31202,#31203,#18139,.T.);
#38778=EDGE_CURVE('',#30761,#31203,#22692,.T.);
#38779=EDGE_CURVE('',#31203,#31204,#22693,.T.);
#38780=EDGE_CURVE('',#31044,#31204,#25247,.T.);
#38781=EDGE_CURVE('',#31205,#31202,#18140,.T.);
#38782=EDGE_CURVE('',#31204,#31205,#18141,.T.);
#38783=EDGE_CURVE('',#31206,#31044,#25248,.T.);
#38784=EDGE_CURVE('',#31206,#31207,#18142,.T.);
#38785=EDGE_CURVE('',#30762,#31207,#22694,.T.);
#38786=EDGE_CURVE('',#31207,#31208,#22695,.T.);
#38787=EDGE_CURVE('',#31045,#31208,#25249,.T.);
#38788=EDGE_CURVE('',#31209,#31206,#18143,.T.);
#38789=EDGE_CURVE('',#31208,#31209,#18144,.T.);
#38790=EDGE_CURVE('',#31210,#31045,#25250,.T.);
#38791=EDGE_CURVE('',#31210,#31211,#18145,.T.);
#38792=EDGE_CURVE('',#30763,#31211,#22696,.T.);
#38793=EDGE_CURVE('',#31211,#31212,#22697,.T.);
#38794=EDGE_CURVE('',#31046,#31212,#25251,.T.);
#38795=EDGE_CURVE('',#31213,#31210,#18146,.T.);
#38796=EDGE_CURVE('',#31212,#31213,#18147,.T.);
#38797=EDGE_CURVE('',#31214,#31046,#25252,.T.);
#38798=EDGE_CURVE('',#31214,#31215,#18148,.T.);
#38799=EDGE_CURVE('',#30764,#31215,#22698,.T.);
#38800=EDGE_CURVE('',#31215,#31216,#22699,.T.);
#38801=EDGE_CURVE('',#31047,#31216,#25253,.T.);
#38802=EDGE_CURVE('',#31217,#31214,#18149,.T.);
#38803=EDGE_CURVE('',#31216,#31217,#18150,.T.);
#38804=EDGE_CURVE('',#31218,#31047,#25254,.T.);
#38805=EDGE_CURVE('',#31218,#31219,#18151,.T.);
#38806=EDGE_CURVE('',#30765,#31219,#22700,.T.);
#38807=EDGE_CURVE('',#31219,#31220,#22701,.T.);
#38808=EDGE_CURVE('',#31048,#31220,#25255,.T.);
#38809=EDGE_CURVE('',#31221,#31218,#18152,.T.);
#38810=EDGE_CURVE('',#31220,#31221,#18153,.T.);
#38811=EDGE_CURVE('',#31222,#31048,#25256,.T.);
#38812=EDGE_CURVE('',#31222,#31223,#18154,.T.);
#38813=EDGE_CURVE('',#30766,#31223,#22702,.T.);
#38814=EDGE_CURVE('',#31223,#31224,#22703,.T.);
#38815=EDGE_CURVE('',#31049,#31224,#25257,.T.);
#38816=EDGE_CURVE('',#31225,#31222,#18155,.T.);
#38817=EDGE_CURVE('',#31224,#31225,#18156,.T.);
#38818=EDGE_CURVE('',#31226,#31049,#25258,.T.);
#38819=EDGE_CURVE('',#31226,#31227,#18157,.T.);
#38820=EDGE_CURVE('',#30767,#31227,#22704,.T.);
#38821=EDGE_CURVE('',#31227,#31228,#22705,.T.);
#38822=EDGE_CURVE('',#31050,#31228,#25259,.T.);
#38823=EDGE_CURVE('',#31229,#31226,#18158,.T.);
#38824=EDGE_CURVE('',#31228,#31229,#18159,.T.);
#38825=EDGE_CURVE('',#31230,#31050,#25260,.T.);
#38826=EDGE_CURVE('',#31230,#31231,#18160,.T.);
#38827=EDGE_CURVE('',#30768,#31231,#22706,.T.);
#38828=EDGE_CURVE('',#31231,#31232,#22707,.T.);
#38829=EDGE_CURVE('',#31051,#31232,#25261,.T.);
#38830=EDGE_CURVE('',#31233,#31230,#18161,.T.);
#38831=EDGE_CURVE('',#31232,#31233,#18162,.T.);
#38832=EDGE_CURVE('',#31234,#31051,#25262,.T.);
#38833=EDGE_CURVE('',#31234,#31235,#18163,.T.);
#38834=EDGE_CURVE('',#30769,#31235,#22708,.T.);
#38835=EDGE_CURVE('',#31235,#31236,#22709,.T.);
#38836=EDGE_CURVE('',#31052,#31236,#25263,.T.);
#38837=EDGE_CURVE('',#31237,#31234,#18164,.T.);
#38838=EDGE_CURVE('',#31236,#31237,#18165,.T.);
#38839=EDGE_CURVE('',#31238,#31052,#25264,.T.);
#38840=EDGE_CURVE('',#31238,#31239,#18166,.T.);
#38841=EDGE_CURVE('',#30770,#31239,#22710,.T.);
#38842=EDGE_CURVE('',#31239,#31240,#22711,.T.);
#38843=EDGE_CURVE('',#31053,#31240,#25265,.T.);
#38844=EDGE_CURVE('',#31241,#31238,#18167,.T.);
#38845=EDGE_CURVE('',#31240,#31241,#18168,.T.);
#38846=EDGE_CURVE('',#31242,#31053,#25266,.T.);
#38847=EDGE_CURVE('',#31242,#31243,#18169,.T.);
#38848=EDGE_CURVE('',#30771,#31243,#22712,.T.);
#38849=EDGE_CURVE('',#31243,#31244,#22713,.T.);
#38850=EDGE_CURVE('',#31054,#31244,#25267,.T.);
#38851=EDGE_CURVE('',#31245,#31242,#18170,.T.);
#38852=EDGE_CURVE('',#31244,#31245,#18171,.T.);
#38853=EDGE_CURVE('',#31246,#31054,#25268,.T.);
#38854=EDGE_CURVE('',#31246,#31247,#18172,.T.);
#38855=EDGE_CURVE('',#30772,#31247,#22714,.T.);
#38856=EDGE_CURVE('',#31247,#31248,#22715,.T.);
#38857=EDGE_CURVE('',#31055,#31248,#25269,.T.);
#38858=EDGE_CURVE('',#31249,#31246,#18173,.T.);
#38859=EDGE_CURVE('',#31248,#31249,#18174,.T.);
#38860=EDGE_CURVE('',#31250,#31055,#25270,.T.);
#38861=EDGE_CURVE('',#31250,#31251,#18175,.T.);
#38862=EDGE_CURVE('',#30773,#31251,#22716,.T.);
#38863=EDGE_CURVE('',#31251,#31252,#22717,.T.);
#38864=EDGE_CURVE('',#31056,#31252,#25271,.T.);
#38865=EDGE_CURVE('',#31253,#31250,#18176,.T.);
#38866=EDGE_CURVE('',#31252,#31253,#18177,.T.);
#38867=EDGE_CURVE('',#31254,#31056,#25272,.T.);
#38868=EDGE_CURVE('',#31254,#31255,#18178,.T.);
#38869=EDGE_CURVE('',#30774,#31255,#22718,.T.);
#38870=EDGE_CURVE('',#31255,#31256,#22719,.T.);
#38871=EDGE_CURVE('',#31057,#31256,#25273,.T.);
#38872=EDGE_CURVE('',#31257,#31254,#18179,.T.);
#38873=EDGE_CURVE('',#31256,#31257,#18180,.T.);
#38874=EDGE_CURVE('',#31258,#31057,#25274,.T.);
#38875=EDGE_CURVE('',#31258,#31259,#18181,.T.);
#38876=EDGE_CURVE('',#30775,#31259,#22720,.T.);
#38877=EDGE_CURVE('',#31259,#31260,#22721,.T.);
#38878=EDGE_CURVE('',#31058,#31260,#25275,.T.);
#38879=EDGE_CURVE('',#31261,#31258,#18182,.T.);
#38880=EDGE_CURVE('',#31260,#31261,#18183,.T.);
#38881=EDGE_CURVE('',#28971,#31058,#25276,.T.);
#38882=EDGE_CURVE('',#30776,#28973,#22722,.T.);
#38883=EDGE_CURVE('',#31059,#28972,#25277,.T.);
#38884=EDGE_CURVE('',#31262,#31059,#25278,.T.);
#38885=EDGE_CURVE('',#31262,#31263,#18184,.T.);
#38886=EDGE_CURVE('',#30777,#31263,#22723,.T.);
#38887=EDGE_CURVE('',#31263,#31264,#22724,.T.);
#38888=EDGE_CURVE('',#31060,#31264,#25279,.T.);
#38889=EDGE_CURVE('',#31265,#31262,#18185,.T.);
#38890=EDGE_CURVE('',#31264,#31265,#18186,.T.);
#38891=EDGE_CURVE('',#31266,#31060,#25280,.T.);
#38892=EDGE_CURVE('',#31266,#31267,#18187,.T.);
#38893=EDGE_CURVE('',#30778,#31267,#22725,.T.);
#38894=EDGE_CURVE('',#31267,#31268,#22726,.T.);
#38895=EDGE_CURVE('',#31061,#31268,#25281,.T.);
#38896=EDGE_CURVE('',#31269,#31266,#18188,.T.);
#38897=EDGE_CURVE('',#31268,#31269,#18189,.T.);
#38898=EDGE_CURVE('',#31270,#31061,#25282,.T.);
#38899=EDGE_CURVE('',#31270,#31271,#18190,.T.);
#38900=EDGE_CURVE('',#30779,#31271,#22727,.T.);
#38901=EDGE_CURVE('',#31271,#31272,#22728,.T.);
#38902=EDGE_CURVE('',#31062,#31272,#25283,.T.);
#38903=EDGE_CURVE('',#31273,#31270,#18191,.T.);
#38904=EDGE_CURVE('',#31272,#31273,#18192,.T.);
#38905=EDGE_CURVE('',#31274,#31062,#25284,.T.);
#38906=EDGE_CURVE('',#31274,#31275,#18193,.T.);
#38907=EDGE_CURVE('',#30780,#31275,#22729,.T.);
#38908=EDGE_CURVE('',#31275,#31276,#22730,.T.);
#38909=EDGE_CURVE('',#31063,#31276,#25285,.T.);
#38910=EDGE_CURVE('',#31277,#31274,#18194,.T.);
#38911=EDGE_CURVE('',#31276,#31277,#18195,.T.);
#38912=EDGE_CURVE('',#31278,#31063,#25286,.T.);
#38913=EDGE_CURVE('',#31278,#31279,#18196,.T.);
#38914=EDGE_CURVE('',#30781,#31279,#22731,.T.);
#38915=EDGE_CURVE('',#31279,#31280,#22732,.T.);
#38916=EDGE_CURVE('',#31064,#31280,#25287,.T.);
#38917=EDGE_CURVE('',#31281,#31278,#18197,.T.);
#38918=EDGE_CURVE('',#31280,#31281,#18198,.T.);
#38919=EDGE_CURVE('',#31282,#31064,#25288,.T.);
#38920=EDGE_CURVE('',#31282,#31283,#18199,.T.);
#38921=EDGE_CURVE('',#30782,#31283,#22733,.T.);
#38922=EDGE_CURVE('',#31283,#31284,#22734,.T.);
#38923=EDGE_CURVE('',#31065,#31284,#25289,.T.);
#38924=EDGE_CURVE('',#31285,#31282,#18200,.T.);
#38925=EDGE_CURVE('',#31284,#31285,#18201,.T.);
#38926=EDGE_CURVE('',#31286,#31065,#25290,.T.);
#38927=EDGE_CURVE('',#31286,#31287,#18202,.T.);
#38928=EDGE_CURVE('',#30783,#31287,#22735,.T.);
#38929=EDGE_CURVE('',#31287,#31288,#22736,.T.);
#38930=EDGE_CURVE('',#31037,#31288,#25291,.T.);
#38931=EDGE_CURVE('',#31289,#31286,#18203,.T.);
#38932=EDGE_CURVE('',#31288,#31289,#18204,.T.);
#38933=EDGE_CURVE('',#31290,#31008,#18205,.T.);
#38934=EDGE_CURVE('',#31068,#31290,#22737,.T.);
#38935=EDGE_CURVE('',#31009,#31290,#18206,.T.);
#38936=EDGE_CURVE('',#31291,#31009,#18207,.T.);
#38937=EDGE_CURVE('',#31072,#31291,#22738,.T.);
#38938=EDGE_CURVE('',#31010,#31291,#18208,.T.);
#38939=EDGE_CURVE('',#31292,#31010,#18209,.T.);
#38940=EDGE_CURVE('',#31076,#31292,#22739,.T.);
#38941=EDGE_CURVE('',#31011,#31292,#18210,.T.);
#38942=EDGE_CURVE('',#31293,#31011,#18211,.T.);
#38943=EDGE_CURVE('',#31080,#31293,#22740,.T.);
#38944=EDGE_CURVE('',#31012,#31293,#18212,.T.);
#38945=EDGE_CURVE('',#31294,#31012,#18213,.T.);
#38946=EDGE_CURVE('',#31084,#31294,#22741,.T.);
#38947=EDGE_CURVE('',#31013,#31294,#18214,.T.);
#38948=EDGE_CURVE('',#31295,#31013,#18215,.T.);
#38949=EDGE_CURVE('',#31088,#31295,#22742,.T.);
#38950=EDGE_CURVE('',#31014,#31295,#18216,.T.);
#38951=EDGE_CURVE('',#31296,#31014,#18217,.T.);
#38952=EDGE_CURVE('',#31092,#31296,#22743,.T.);
#38953=EDGE_CURVE('',#31015,#31296,#18218,.T.);
#38954=EDGE_CURVE('',#31297,#31015,#18219,.T.);
#38955=EDGE_CURVE('',#31096,#31297,#22744,.T.);
#38956=EDGE_CURVE('',#31016,#31297,#18220,.T.);
#38957=EDGE_CURVE('',#31298,#31016,#18221,.T.);
#38958=EDGE_CURVE('',#31100,#31298,#22745,.T.);
#38959=EDGE_CURVE('',#31017,#31298,#18222,.T.);
#38960=EDGE_CURVE('',#31299,#31017,#18223,.T.);
#38961=EDGE_CURVE('',#31104,#31299,#22746,.T.);
#38962=EDGE_CURVE('',#31018,#31299,#18224,.T.);
#38963=EDGE_CURVE('',#31300,#31018,#18225,.T.);
#38964=EDGE_CURVE('',#31108,#31300,#22747,.T.);
#38965=EDGE_CURVE('',#31019,#31300,#18226,.T.);
#38966=EDGE_CURVE('',#31301,#31019,#18227,.T.);
#38967=EDGE_CURVE('',#31112,#31301,#22748,.T.);
#38968=EDGE_CURVE('',#31020,#31301,#18228,.T.);
#38969=EDGE_CURVE('',#31302,#31020,#18229,.T.);
#38970=EDGE_CURVE('',#31116,#31302,#22749,.T.);
#38971=EDGE_CURVE('',#31021,#31302,#18230,.T.);
#38972=EDGE_CURVE('',#31303,#31021,#18231,.T.);
#38973=EDGE_CURVE('',#31120,#31303,#22750,.T.);
#38974=EDGE_CURVE('',#31022,#31303,#18232,.T.);
#38975=EDGE_CURVE('',#31304,#31022,#18233,.T.);
#38976=EDGE_CURVE('',#28976,#31304,#22751,.T.);
#38977=EDGE_CURVE('',#31023,#31304,#18234,.T.);
#38978=EDGE_CURVE('',#31305,#31023,#18235,.T.);
#38979=EDGE_CURVE('',#31124,#31305,#22752,.T.);
#38980=EDGE_CURVE('',#31024,#31305,#18236,.T.);
#38981=EDGE_CURVE('',#31306,#31024,#18237,.T.);
#38982=EDGE_CURVE('',#31128,#31306,#22753,.T.);
#38983=EDGE_CURVE('',#31025,#31306,#18238,.T.);
#38984=EDGE_CURVE('',#31307,#31025,#18239,.T.);
#38985=EDGE_CURVE('',#31132,#31307,#22754,.T.);
#38986=EDGE_CURVE('',#31026,#31307,#18240,.T.);
#38987=EDGE_CURVE('',#31308,#31026,#18241,.T.);
#38988=EDGE_CURVE('',#31136,#31308,#22755,.T.);
#38989=EDGE_CURVE('',#31027,#31308,#18242,.T.);
#38990=EDGE_CURVE('',#31309,#31027,#18243,.T.);
#38991=EDGE_CURVE('',#31140,#31309,#22756,.T.);
#38992=EDGE_CURVE('',#31028,#31309,#18244,.T.);
#38993=EDGE_CURVE('',#31310,#31028,#18245,.T.);
#38994=EDGE_CURVE('',#31144,#31310,#22757,.T.);
#38995=EDGE_CURVE('',#31029,#31310,#18246,.T.);
#38996=EDGE_CURVE('',#31311,#31029,#18247,.T.);
#38997=EDGE_CURVE('',#31149,#31311,#22758,.T.);
#38998=EDGE_CURVE('',#31030,#31311,#18248,.T.);
#38999=EDGE_CURVE('',#31312,#31030,#18249,.T.);
#39000=EDGE_CURVE('',#31153,#31312,#22759,.T.);
#39001=EDGE_CURVE('',#31031,#31312,#18250,.T.);
#39002=EDGE_CURVE('',#31313,#31031,#18251,.T.);
#39003=EDGE_CURVE('',#31156,#31313,#22760,.T.);
#39004=EDGE_CURVE('',#31032,#31313,#18252,.T.);
#39005=EDGE_CURVE('',#31314,#31032,#18253,.T.);
#39006=EDGE_CURVE('',#31160,#31314,#22761,.T.);
#39007=EDGE_CURVE('',#31033,#31314,#18254,.T.);
#39008=EDGE_CURVE('',#31315,#31033,#18255,.T.);
#39009=EDGE_CURVE('',#31164,#31315,#22762,.T.);
#39010=EDGE_CURVE('',#31034,#31315,#18256,.T.);
#39011=EDGE_CURVE('',#31316,#31034,#18257,.T.);
#39012=EDGE_CURVE('',#31168,#31316,#22763,.T.);
#39013=EDGE_CURVE('',#31035,#31316,#18258,.T.);
#39014=EDGE_CURVE('',#31317,#31035,#18259,.T.);
#39015=EDGE_CURVE('',#31172,#31317,#22764,.T.);
#39016=EDGE_CURVE('',#31036,#31317,#18260,.T.);
#39017=EDGE_CURVE('',#31318,#31036,#18261,.T.);
#39018=EDGE_CURVE('',#31176,#31318,#22765,.T.);
#39019=EDGE_CURVE('',#31008,#31318,#18262,.T.);
#39020=EDGE_CURVE('',#31319,#31037,#18263,.T.);
#39021=EDGE_CURVE('',#31181,#31319,#22766,.T.);
#39022=EDGE_CURVE('',#31038,#31319,#18264,.T.);
#39023=EDGE_CURVE('',#31320,#31038,#18265,.T.);
#39024=EDGE_CURVE('',#31185,#31320,#22767,.T.);
#39025=EDGE_CURVE('',#31039,#31320,#18266,.T.);
#39026=EDGE_CURVE('',#31321,#31039,#18267,.T.);
#39027=EDGE_CURVE('',#31189,#31321,#22768,.T.);
#39028=EDGE_CURVE('',#31040,#31321,#18268,.T.);
#39029=EDGE_CURVE('',#31322,#31040,#18269,.T.);
#39030=EDGE_CURVE('',#31193,#31322,#22769,.T.);
#39031=EDGE_CURVE('',#31041,#31322,#18270,.T.);
#39032=EDGE_CURVE('',#31323,#31041,#18271,.T.);
#39033=EDGE_CURVE('',#31197,#31323,#22770,.T.);
#39034=EDGE_CURVE('',#31042,#31323,#18272,.T.);
#39035=EDGE_CURVE('',#31324,#31042,#18273,.T.);
#39036=EDGE_CURVE('',#31201,#31324,#22771,.T.);
#39037=EDGE_CURVE('',#31043,#31324,#18274,.T.);
#39038=EDGE_CURVE('',#31325,#31043,#18275,.T.);
#39039=EDGE_CURVE('',#31205,#31325,#22772,.T.);
#39040=EDGE_CURVE('',#31044,#31325,#18276,.T.);
#39041=EDGE_CURVE('',#31326,#31044,#18277,.T.);
#39042=EDGE_CURVE('',#31209,#31326,#22773,.T.);
#39043=EDGE_CURVE('',#31045,#31326,#18278,.T.);
#39044=EDGE_CURVE('',#31327,#31045,#18279,.T.);
#39045=EDGE_CURVE('',#31213,#31327,#22774,.T.);
#39046=EDGE_CURVE('',#31046,#31327,#18280,.T.);
#39047=EDGE_CURVE('',#31328,#31046,#18281,.T.);
#39048=EDGE_CURVE('',#31217,#31328,#22775,.T.);
#39049=EDGE_CURVE('',#31047,#31328,#18282,.T.);
#39050=EDGE_CURVE('',#31329,#31047,#18283,.T.);
#39051=EDGE_CURVE('',#31221,#31329,#22776,.T.);
#39052=EDGE_CURVE('',#31048,#31329,#18284,.T.);
#39053=EDGE_CURVE('',#31330,#31048,#18285,.T.);
#39054=EDGE_CURVE('',#31225,#31330,#22777,.T.);
#39055=EDGE_CURVE('',#31049,#31330,#18286,.T.);
#39056=EDGE_CURVE('',#31331,#31049,#18287,.T.);
#39057=EDGE_CURVE('',#31229,#31331,#22778,.T.);
#39058=EDGE_CURVE('',#31050,#31331,#18288,.T.);
#39059=EDGE_CURVE('',#31332,#31050,#18289,.T.);
#39060=EDGE_CURVE('',#31233,#31332,#22779,.T.);
#39061=EDGE_CURVE('',#31051,#31332,#18290,.T.);
#39062=EDGE_CURVE('',#31333,#31051,#18291,.T.);
#39063=EDGE_CURVE('',#31237,#31333,#22780,.T.);
#39064=EDGE_CURVE('',#31052,#31333,#18292,.T.);
#39065=EDGE_CURVE('',#31334,#31052,#18293,.T.);
#39066=EDGE_CURVE('',#31241,#31334,#22781,.T.);
#39067=EDGE_CURVE('',#31053,#31334,#18294,.T.);
#39068=EDGE_CURVE('',#31335,#31053,#18295,.T.);
#39069=EDGE_CURVE('',#31245,#31335,#22782,.T.);
#39070=EDGE_CURVE('',#31054,#31335,#18296,.T.);
#39071=EDGE_CURVE('',#31336,#31054,#18297,.T.);
#39072=EDGE_CURVE('',#31249,#31336,#22783,.T.);
#39073=EDGE_CURVE('',#31055,#31336,#18298,.T.);
#39074=EDGE_CURVE('',#31337,#31055,#18299,.T.);
#39075=EDGE_CURVE('',#31253,#31337,#22784,.T.);
#39076=EDGE_CURVE('',#31056,#31337,#18300,.T.);
#39077=EDGE_CURVE('',#31338,#31056,#18301,.T.);
#39078=EDGE_CURVE('',#31257,#31338,#22785,.T.);
#39079=EDGE_CURVE('',#31057,#31338,#18302,.T.);
#39080=EDGE_CURVE('',#31339,#31057,#18303,.T.);
#39081=EDGE_CURVE('',#31261,#31339,#22786,.T.);
#39082=EDGE_CURVE('',#31058,#31339,#18304,.T.);
#39083=EDGE_CURVE('',#31340,#31058,#18305,.T.);
#39084=EDGE_CURVE('',#28970,#31340,#22787,.T.);
#39085=EDGE_CURVE('',#31059,#31340,#18306,.T.);
#39086=EDGE_CURVE('',#31341,#31059,#18307,.T.);
#39087=EDGE_CURVE('',#31265,#31341,#22788,.T.);
#39088=EDGE_CURVE('',#31060,#31341,#18308,.T.);
#39089=EDGE_CURVE('',#31342,#31060,#18309,.T.);
#39090=EDGE_CURVE('',#31269,#31342,#22789,.T.);
#39091=EDGE_CURVE('',#31061,#31342,#18310,.T.);
#39092=EDGE_CURVE('',#31343,#31061,#18311,.T.);
#39093=EDGE_CURVE('',#31273,#31343,#22790,.T.);
#39094=EDGE_CURVE('',#31062,#31343,#18312,.T.);
#39095=EDGE_CURVE('',#31344,#31062,#18313,.T.);
#39096=EDGE_CURVE('',#31277,#31344,#22791,.T.);
#39097=EDGE_CURVE('',#31063,#31344,#18314,.T.);
#39098=EDGE_CURVE('',#31345,#31063,#18315,.T.);
#39099=EDGE_CURVE('',#31281,#31345,#22792,.T.);
#39100=EDGE_CURVE('',#31064,#31345,#18316,.T.);
#39101=EDGE_CURVE('',#31346,#31064,#18317,.T.);
#39102=EDGE_CURVE('',#31285,#31346,#22793,.T.);
#39103=EDGE_CURVE('',#31065,#31346,#18318,.T.);
#39104=EDGE_CURVE('',#31347,#31065,#18319,.T.);
#39105=EDGE_CURVE('',#31289,#31347,#22794,.T.);
#39106=EDGE_CURVE('',#31037,#31347,#18320,.T.);
#39107=EDGE_CURVE('',#31348,#31349,#18321,.T.);
#39108=EDGE_CURVE('',#31290,#31349,#25292,.T.);
#39109=EDGE_CURVE('',#31348,#31008,#22795,.T.);
#39110=EDGE_CURVE('',#31350,#31351,#18322,.T.);
#39111=EDGE_CURVE('',#31009,#31351,#22796,.T.);
#39112=EDGE_CURVE('',#31350,#31290,#25293,.T.);
#39113=EDGE_CURVE('',#31352,#31350,#18323,.T.);
#39114=EDGE_CURVE('',#31353,#31352,#18324,.T.);
#39115=EDGE_CURVE('',#31351,#31353,#18325,.T.);
#39116=EDGE_CURVE('',#31291,#31353,#25294,.T.);
#39117=EDGE_CURVE('',#31354,#31355,#18326,.T.);
#39118=EDGE_CURVE('',#31010,#31355,#22797,.T.);
#39119=EDGE_CURVE('',#31354,#31291,#25295,.T.);
#39120=EDGE_CURVE('',#31356,#31354,#18327,.T.);
#39121=EDGE_CURVE('',#31357,#31356,#18328,.T.);
#39122=EDGE_CURVE('',#31355,#31357,#18329,.T.);
#39123=EDGE_CURVE('',#31292,#31357,#25296,.T.);
#39124=EDGE_CURVE('',#31358,#31359,#18330,.T.);
#39125=EDGE_CURVE('',#31011,#31359,#22798,.T.);
#39126=EDGE_CURVE('',#31358,#31292,#25297,.T.);
#39127=EDGE_CURVE('',#31360,#31358,#18331,.T.);
#39128=EDGE_CURVE('',#31361,#31360,#18332,.T.);
#39129=EDGE_CURVE('',#31359,#31361,#18333,.T.);
#39130=EDGE_CURVE('',#31293,#31361,#25298,.T.);
#39131=EDGE_CURVE('',#31362,#31363,#18334,.T.);
#39132=EDGE_CURVE('',#31012,#31363,#22799,.T.);
#39133=EDGE_CURVE('',#31362,#31293,#25299,.T.);
#39134=EDGE_CURVE('',#31364,#31362,#18335,.T.);
#39135=EDGE_CURVE('',#31365,#31364,#18336,.T.);
#39136=EDGE_CURVE('',#31363,#31365,#18337,.T.);
#39137=EDGE_CURVE('',#31294,#31365,#25300,.T.);
#39138=EDGE_CURVE('',#31366,#31367,#18338,.T.);
#39139=EDGE_CURVE('',#31013,#31367,#22800,.T.);
#39140=EDGE_CURVE('',#31366,#31294,#25301,.T.);
#39141=EDGE_CURVE('',#31368,#31366,#18339,.T.);
#39142=EDGE_CURVE('',#31369,#31368,#18340,.T.);
#39143=EDGE_CURVE('',#31367,#31369,#18341,.T.);
#39144=EDGE_CURVE('',#31295,#31369,#25302,.T.);
#39145=EDGE_CURVE('',#31370,#31371,#18342,.T.);
#39146=EDGE_CURVE('',#31014,#31371,#22801,.T.);
#39147=EDGE_CURVE('',#31370,#31295,#25303,.T.);
#39148=EDGE_CURVE('',#31372,#31370,#18343,.T.);
#39149=EDGE_CURVE('',#31373,#31372,#18344,.T.);
#39150=EDGE_CURVE('',#31371,#31373,#18345,.T.);
#39151=EDGE_CURVE('',#31296,#31373,#25304,.T.);
#39152=EDGE_CURVE('',#31015,#28966,#22802,.T.);
#39153=EDGE_CURVE('',#28968,#31296,#25305,.T.);
#39154=EDGE_CURVE('',#31297,#28967,#25306,.T.);
#39155=EDGE_CURVE('',#31374,#31375,#18346,.T.);
#39156=EDGE_CURVE('',#31016,#31375,#22803,.T.);
#39157=EDGE_CURVE('',#31374,#31297,#25307,.T.);
#39158=EDGE_CURVE('',#31376,#31374,#18347,.T.);
#39159=EDGE_CURVE('',#31377,#31376,#18348,.T.);
#39160=EDGE_CURVE('',#31375,#31377,#18349,.T.);
#39161=EDGE_CURVE('',#31298,#31377,#25308,.T.);
#39162=EDGE_CURVE('',#31378,#31379,#18350,.T.);
#39163=EDGE_CURVE('',#31017,#31379,#22804,.T.);
#39164=EDGE_CURVE('',#31378,#31298,#25309,.T.);
#39165=EDGE_CURVE('',#31380,#31378,#18351,.T.);
#39166=EDGE_CURVE('',#31381,#31380,#18352,.T.);
#39167=EDGE_CURVE('',#31379,#31381,#18353,.T.);
#39168=EDGE_CURVE('',#31299,#31381,#25310,.T.);
#39169=EDGE_CURVE('',#31382,#31383,#18354,.T.);
#39170=EDGE_CURVE('',#31018,#31383,#22805,.T.);
#39171=EDGE_CURVE('',#31382,#31299,#25311,.T.);
#39172=EDGE_CURVE('',#31384,#31382,#18355,.T.);
#39173=EDGE_CURVE('',#31385,#31384,#18356,.T.);
#39174=EDGE_CURVE('',#31383,#31385,#18357,.T.);
#39175=EDGE_CURVE('',#31300,#31385,#25312,.T.);
#39176=EDGE_CURVE('',#31386,#31387,#18358,.T.);
#39177=EDGE_CURVE('',#31019,#31387,#22806,.T.);
#39178=EDGE_CURVE('',#31386,#31300,#25313,.T.);
#39179=EDGE_CURVE('',#31388,#31386,#18359,.T.);
#39180=EDGE_CURVE('',#31389,#31388,#18360,.T.);
#39181=EDGE_CURVE('',#31387,#31389,#18361,.T.);
#39182=EDGE_CURVE('',#31301,#31389,#25314,.T.);
#39183=EDGE_CURVE('',#31390,#31391,#18362,.T.);
#39184=EDGE_CURVE('',#31020,#31391,#22807,.T.);
#39185=EDGE_CURVE('',#31390,#31301,#25315,.T.);
#39186=EDGE_CURVE('',#31392,#31390,#18363,.T.);
#39187=EDGE_CURVE('',#31393,#31392,#18364,.T.);
#39188=EDGE_CURVE('',#31391,#31393,#18365,.T.);
#39189=EDGE_CURVE('',#31302,#31393,#25316,.T.);
#39190=EDGE_CURVE('',#31394,#31395,#18366,.T.);
#39191=EDGE_CURVE('',#31021,#31395,#22808,.T.);
#39192=EDGE_CURVE('',#31394,#31302,#25317,.T.);
#39193=EDGE_CURVE('',#31396,#31394,#18367,.T.);
#39194=EDGE_CURVE('',#31397,#31396,#18368,.T.);
#39195=EDGE_CURVE('',#31395,#31397,#18369,.T.);
#39196=EDGE_CURVE('',#31303,#31397,#25318,.T.);
#39197=EDGE_CURVE('',#31398,#31399,#18370,.T.);
#39198=EDGE_CURVE('',#31022,#31399,#22809,.T.);
#39199=EDGE_CURVE('',#31398,#31303,#25319,.T.);
#39200=EDGE_CURVE('',#31400,#31398,#18371,.T.);
#39201=EDGE_CURVE('',#31401,#31400,#18372,.T.);
#39202=EDGE_CURVE('',#31399,#31401,#18373,.T.);
#39203=EDGE_CURVE('',#31304,#31401,#25320,.T.);
#39204=EDGE_CURVE('',#31402,#31403,#18374,.T.);
#39205=EDGE_CURVE('',#31023,#31403,#22810,.T.);
#39206=EDGE_CURVE('',#31402,#31304,#25321,.T.);
#39207=EDGE_CURVE('',#31404,#31402,#18375,.T.);
#39208=EDGE_CURVE('',#31405,#31404,#18376,.T.);
#39209=EDGE_CURVE('',#31403,#31405,#18377,.T.);
#39210=EDGE_CURVE('',#31305,#31405,#25322,.T.);
#39211=EDGE_CURVE('',#31406,#31407,#18378,.T.);
#39212=EDGE_CURVE('',#31024,#31407,#22811,.T.);
#39213=EDGE_CURVE('',#31406,#31305,#25323,.T.);
#39214=EDGE_CURVE('',#31408,#31406,#18379,.T.);
#39215=EDGE_CURVE('',#31409,#31408,#18380,.T.);
#39216=EDGE_CURVE('',#31407,#31409,#18381,.T.);
#39217=EDGE_CURVE('',#31306,#31409,#25324,.T.);
#39218=EDGE_CURVE('',#31410,#31411,#18382,.T.);
#39219=EDGE_CURVE('',#31025,#31411,#22812,.T.);
#39220=EDGE_CURVE('',#31410,#31306,#25325,.T.);
#39221=EDGE_CURVE('',#31412,#31410,#18383,.T.);
#39222=EDGE_CURVE('',#31413,#31412,#18384,.T.);
#39223=EDGE_CURVE('',#31411,#31413,#18385,.T.);
#39224=EDGE_CURVE('',#31307,#31413,#25326,.T.);
#39225=EDGE_CURVE('',#31414,#31415,#18386,.T.);
#39226=EDGE_CURVE('',#31026,#31415,#22813,.T.);
#39227=EDGE_CURVE('',#31414,#31307,#25327,.T.);
#39228=EDGE_CURVE('',#31416,#31414,#18387,.T.);
#39229=EDGE_CURVE('',#31417,#31416,#18388,.T.);
#39230=EDGE_CURVE('',#31415,#31417,#18389,.T.);
#39231=EDGE_CURVE('',#31308,#31417,#25328,.T.);
#39232=EDGE_CURVE('',#31418,#31419,#18390,.T.);
#39233=EDGE_CURVE('',#31027,#31419,#22814,.T.);
#39234=EDGE_CURVE('',#31418,#31308,#25329,.T.);
#39235=EDGE_CURVE('',#31420,#31418,#18391,.T.);
#39236=EDGE_CURVE('',#31421,#31420,#18392,.T.);
#39237=EDGE_CURVE('',#31419,#31421,#18393,.T.);
#39238=EDGE_CURVE('',#31309,#31421,#25330,.T.);
#39239=EDGE_CURVE('',#31422,#31423,#18394,.T.);
#39240=EDGE_CURVE('',#31028,#31423,#22815,.T.);
#39241=EDGE_CURVE('',#31422,#31309,#25331,.T.);
#39242=EDGE_CURVE('',#31424,#31422,#18395,.T.);
#39243=EDGE_CURVE('',#31425,#31424,#18396,.T.);
#39244=EDGE_CURVE('',#31423,#31425,#18397,.T.);
#39245=EDGE_CURVE('',#31310,#31425,#25332,.T.);
#39246=EDGE_CURVE('',#31426,#31427,#18398,.T.);
#39247=EDGE_CURVE('',#31029,#31427,#22816,.T.);
#39248=EDGE_CURVE('',#31426,#31310,#25333,.T.);
#39249=EDGE_CURVE('',#31427,#31428,#18399,.T.);
#39250=EDGE_CURVE('',#31311,#31428,#25334,.T.);
#39251=EDGE_CURVE('',#31429,#31426,#18400,.T.);
#39252=EDGE_CURVE('',#31428,#31429,#18401,.T.);
#39253=EDGE_CURVE('',#31430,#31311,#25335,.T.);
#39254=EDGE_CURVE('',#31430,#31431,#18402,.T.);
#39255=EDGE_CURVE('',#31030,#31431,#22817,.T.);
#39256=EDGE_CURVE('',#31431,#31432,#18403,.T.);
#39257=EDGE_CURVE('',#31433,#31430,#18404,.T.);
#39258=EDGE_CURVE('',#31432,#31433,#18405,.T.);
#39259=EDGE_CURVE('',#31312,#31432,#25336,.T.);
#39260=EDGE_CURVE('',#31434,#31435,#18406,.T.);
#39261=EDGE_CURVE('',#31031,#31435,#22818,.T.);
#39262=EDGE_CURVE('',#31434,#31312,#25337,.T.);
#39263=EDGE_CURVE('',#31436,#31434,#18407,.T.);
#39264=EDGE_CURVE('',#31437,#31436,#18408,.T.);
#39265=EDGE_CURVE('',#31435,#31437,#18409,.T.);
#39266=EDGE_CURVE('',#31313,#31437,#25338,.T.);
#39267=EDGE_CURVE('',#31438,#31439,#18410,.T.);
#39268=EDGE_CURVE('',#31032,#31439,#22819,.T.);
#39269=EDGE_CURVE('',#31438,#31313,#25339,.T.);
#39270=EDGE_CURVE('',#31440,#31438,#18411,.T.);
#39271=EDGE_CURVE('',#31441,#31440,#18412,.T.);
#39272=EDGE_CURVE('',#31439,#31441,#18413,.T.);
#39273=EDGE_CURVE('',#31314,#31441,#25340,.T.);
#39274=EDGE_CURVE('',#31442,#31443,#18414,.T.);
#39275=EDGE_CURVE('',#31033,#31443,#22820,.T.);
#39276=EDGE_CURVE('',#31442,#31314,#25341,.T.);
#39277=EDGE_CURVE('',#31444,#31442,#18415,.T.);
#39278=EDGE_CURVE('',#31445,#31444,#18416,.T.);
#39279=EDGE_CURVE('',#31443,#31445,#18417,.T.);
#39280=EDGE_CURVE('',#31315,#31445,#25342,.T.);
#39281=EDGE_CURVE('',#31446,#31447,#18418,.T.);
#39282=EDGE_CURVE('',#31034,#31447,#22821,.T.);
#39283=EDGE_CURVE('',#31446,#31315,#25343,.T.);
#39284=EDGE_CURVE('',#31448,#31446,#18419,.T.);
#39285=EDGE_CURVE('',#31449,#31448,#18420,.T.);
#39286=EDGE_CURVE('',#31447,#31449,#18421,.T.);
#39287=EDGE_CURVE('',#31316,#31449,#25344,.T.);
#39288=EDGE_CURVE('',#31450,#31451,#18422,.T.);
#39289=EDGE_CURVE('',#31035,#31451,#22822,.T.);
#39290=EDGE_CURVE('',#31450,#31316,#25345,.T.);
#39291=EDGE_CURVE('',#31452,#31450,#18423,.T.);
#39292=EDGE_CURVE('',#31453,#31452,#18424,.T.);
#39293=EDGE_CURVE('',#31451,#31453,#18425,.T.);
#39294=EDGE_CURVE('',#31317,#31453,#25346,.T.);
#39295=EDGE_CURVE('',#31454,#31455,#18426,.T.);
#39296=EDGE_CURVE('',#31036,#31455,#22823,.T.);
#39297=EDGE_CURVE('',#31454,#31317,#25347,.T.);
#39298=EDGE_CURVE('',#31456,#31454,#18427,.T.);
#39299=EDGE_CURVE('',#31457,#31456,#18428,.T.);
#39300=EDGE_CURVE('',#31455,#31457,#18429,.T.);
#39301=EDGE_CURVE('',#31318,#31457,#25348,.T.);
#39302=EDGE_CURVE('',#31458,#31459,#18430,.T.);
#39303=EDGE_CURVE('',#31349,#31458,#18431,.T.);
#39304=EDGE_CURVE('',#31459,#31348,#18432,.T.);
#39305=EDGE_CURVE('',#31459,#31318,#25349,.T.);
#39306=EDGE_CURVE('',#31460,#31037,#22824,.T.);
#39307=EDGE_CURVE('',#31460,#31461,#18433,.T.);
#39308=EDGE_CURVE('',#31319,#31461,#25350,.T.);
#39309=EDGE_CURVE('',#31462,#31319,#25351,.T.);
#39310=EDGE_CURVE('',#31462,#31463,#18434,.T.);
#39311=EDGE_CURVE('',#31038,#31463,#22825,.T.);
#39312=EDGE_CURVE('',#31463,#31464,#18435,.T.);
#39313=EDGE_CURVE('',#31320,#31464,#25352,.T.);
#39314=EDGE_CURVE('',#31465,#31462,#18436,.T.);
#39315=EDGE_CURVE('',#31464,#31465,#18437,.T.);
#39316=EDGE_CURVE('',#31466,#31320,#25353,.T.);
#39317=EDGE_CURVE('',#31466,#31467,#18438,.T.);
#39318=EDGE_CURVE('',#31039,#31467,#22826,.T.);
#39319=EDGE_CURVE('',#31467,#31468,#18439,.T.);
#39320=EDGE_CURVE('',#31321,#31468,#25354,.T.);
#39321=EDGE_CURVE('',#31469,#31466,#18440,.T.);
#39322=EDGE_CURVE('',#31468,#31469,#18441,.T.);
#39323=EDGE_CURVE('',#31470,#31321,#25355,.T.);
#39324=EDGE_CURVE('',#31470,#31471,#18442,.T.);
#39325=EDGE_CURVE('',#31040,#31471,#22827,.T.);
#39326=EDGE_CURVE('',#31471,#31472,#18443,.T.);
#39327=EDGE_CURVE('',#31322,#31472,#25356,.T.);
#39328=EDGE_CURVE('',#31473,#31470,#18444,.T.);
#39329=EDGE_CURVE('',#31472,#31473,#18445,.T.);
#39330=EDGE_CURVE('',#31474,#31322,#25357,.T.);
#39331=EDGE_CURVE('',#31474,#31475,#18446,.T.);
#39332=EDGE_CURVE('',#31041,#31475,#22828,.T.);
#39333=EDGE_CURVE('',#31475,#31476,#18447,.T.);
#39334=EDGE_CURVE('',#31323,#31476,#25358,.T.);
#39335=EDGE_CURVE('',#31477,#31474,#18448,.T.);
#39336=EDGE_CURVE('',#31476,#31477,#18449,.T.);
#39337=EDGE_CURVE('',#31478,#31323,#25359,.T.);
#39338=EDGE_CURVE('',#31478,#31479,#18450,.T.);
#39339=EDGE_CURVE('',#31042,#31479,#22829,.T.);
#39340=EDGE_CURVE('',#31479,#31480,#18451,.T.);
#39341=EDGE_CURVE('',#31324,#31480,#25360,.T.);
#39342=EDGE_CURVE('',#31481,#31478,#18452,.T.);
#39343=EDGE_CURVE('',#31480,#31481,#18453,.T.);
#39344=EDGE_CURVE('',#31482,#31324,#25361,.T.);
#39345=EDGE_CURVE('',#31482,#31483,#18454,.T.);
#39346=EDGE_CURVE('',#31043,#31483,#22830,.T.);
#39347=EDGE_CURVE('',#31483,#31484,#18455,.T.);
#39348=EDGE_CURVE('',#31325,#31484,#25362,.T.);
#39349=EDGE_CURVE('',#31485,#31482,#18456,.T.);
#39350=EDGE_CURVE('',#31484,#31485,#18457,.T.);
#39351=EDGE_CURVE('',#31486,#31325,#25363,.T.);
#39352=EDGE_CURVE('',#31486,#31487,#18458,.T.);
#39353=EDGE_CURVE('',#31044,#31487,#22831,.T.);
#39354=EDGE_CURVE('',#31487,#31488,#18459,.T.);
#39355=EDGE_CURVE('',#31326,#31488,#25364,.T.);
#39356=EDGE_CURVE('',#31489,#31486,#18460,.T.);
#39357=EDGE_CURVE('',#31488,#31489,#18461,.T.);
#39358=EDGE_CURVE('',#31490,#31326,#25365,.T.);
#39359=EDGE_CURVE('',#31490,#31491,#18462,.T.);
#39360=EDGE_CURVE('',#31045,#31491,#22832,.T.);
#39361=EDGE_CURVE('',#31491,#31492,#18463,.T.);
#39362=EDGE_CURVE('',#31327,#31492,#25366,.T.);
#39363=EDGE_CURVE('',#31493,#31490,#18464,.T.);
#39364=EDGE_CURVE('',#31492,#31493,#18465,.T.);
#39365=EDGE_CURVE('',#31494,#31327,#25367,.T.);
#39366=EDGE_CURVE('',#31494,#31495,#18466,.T.);
#39367=EDGE_CURVE('',#31046,#31495,#22833,.T.);
#39368=EDGE_CURVE('',#31495,#31496,#18467,.T.);
#39369=EDGE_CURVE('',#31328,#31496,#25368,.T.);
#39370=EDGE_CURVE('',#31497,#31494,#18468,.T.);
#39371=EDGE_CURVE('',#31496,#31497,#18469,.T.);
#39372=EDGE_CURVE('',#31498,#31328,#25369,.T.);
#39373=EDGE_CURVE('',#31498,#31499,#18470,.T.);
#39374=EDGE_CURVE('',#31047,#31499,#22834,.T.);
#39375=EDGE_CURVE('',#31499,#31500,#18471,.T.);
#39376=EDGE_CURVE('',#31329,#31500,#25370,.T.);
#39377=EDGE_CURVE('',#31501,#31498,#18472,.T.);
#39378=EDGE_CURVE('',#31500,#31501,#18473,.T.);
#39379=EDGE_CURVE('',#31502,#31329,#25371,.T.);
#39380=EDGE_CURVE('',#31502,#31503,#18474,.T.);
#39381=EDGE_CURVE('',#31048,#31503,#22835,.T.);
#39382=EDGE_CURVE('',#31503,#31504,#18475,.T.);
#39383=EDGE_CURVE('',#31330,#31504,#25372,.T.);
#39384=EDGE_CURVE('',#31505,#31502,#18476,.T.);
#39385=EDGE_CURVE('',#31504,#31505,#18477,.T.);
#39386=EDGE_CURVE('',#31506,#31330,#25373,.T.);
#39387=EDGE_CURVE('',#31506,#31507,#18478,.T.);
#39388=EDGE_CURVE('',#31049,#31507,#22836,.T.);
#39389=EDGE_CURVE('',#31507,#31508,#18479,.T.);
#39390=EDGE_CURVE('',#31331,#31508,#25374,.T.);
#39391=EDGE_CURVE('',#31509,#31506,#18480,.T.);
#39392=EDGE_CURVE('',#31508,#31509,#18481,.T.);
#39393=EDGE_CURVE('',#31510,#31331,#25375,.T.);
#39394=EDGE_CURVE('',#31510,#31511,#18482,.T.);
#39395=EDGE_CURVE('',#31050,#31511,#22837,.T.);
#39396=EDGE_CURVE('',#31511,#31512,#18483,.T.);
#39397=EDGE_CURVE('',#31332,#31512,#25376,.T.);
#39398=EDGE_CURVE('',#31513,#31510,#18484,.T.);
#39399=EDGE_CURVE('',#31512,#31513,#18485,.T.);
#39400=EDGE_CURVE('',#28965,#31332,#25377,.T.);
#39401=EDGE_CURVE('',#31051,#28964,#22838,.T.);
#39402=EDGE_CURVE('',#31333,#28962,#25378,.T.);
#39403=EDGE_CURVE('',#31514,#31333,#25379,.T.);
#39404=EDGE_CURVE('',#31514,#31515,#18486,.T.);
#39405=EDGE_CURVE('',#31052,#31515,#22839,.T.);
#39406=EDGE_CURVE('',#31515,#31516,#18487,.T.);
#39407=EDGE_CURVE('',#31334,#31516,#25380,.T.);
#39408=EDGE_CURVE('',#31517,#31514,#18488,.T.);
#39409=EDGE_CURVE('',#31516,#31517,#18489,.T.);
#39410=EDGE_CURVE('',#31518,#31334,#25381,.T.);
#39411=EDGE_CURVE('',#31518,#31519,#18490,.T.);
#39412=EDGE_CURVE('',#31053,#31519,#22840,.T.);
#39413=EDGE_CURVE('',#31519,#31520,#18491,.T.);
#39414=EDGE_CURVE('',#31335,#31520,#25382,.T.);
#39415=EDGE_CURVE('',#31521,#31518,#18492,.T.);
#39416=EDGE_CURVE('',#31520,#31521,#18493,.T.);
#39417=EDGE_CURVE('',#31522,#31335,#25383,.T.);
#39418=EDGE_CURVE('',#31522,#31523,#18494,.T.);
#39419=EDGE_CURVE('',#31054,#31523,#22841,.T.);
#39420=EDGE_CURVE('',#31523,#31524,#18495,.T.);
#39421=EDGE_CURVE('',#31336,#31524,#25384,.T.);
#39422=EDGE_CURVE('',#31525,#31522,#18496,.T.);
#39423=EDGE_CURVE('',#31524,#31525,#18497,.T.);
#39424=EDGE_CURVE('',#31526,#31336,#25385,.T.);
#39425=EDGE_CURVE('',#31526,#31527,#18498,.T.);
#39426=EDGE_CURVE('',#31055,#31527,#22842,.T.);
#39427=EDGE_CURVE('',#31527,#31528,#18499,.T.);
#39428=EDGE_CURVE('',#31337,#31528,#25386,.T.);
#39429=EDGE_CURVE('',#31529,#31526,#18500,.T.);
#39430=EDGE_CURVE('',#31528,#31529,#18501,.T.);
#39431=EDGE_CURVE('',#31530,#31337,#25387,.T.);
#39432=EDGE_CURVE('',#31530,#31531,#18502,.T.);
#39433=EDGE_CURVE('',#31056,#31531,#22843,.T.);
#39434=EDGE_CURVE('',#31531,#31532,#18503,.T.);
#39435=EDGE_CURVE('',#31338,#31532,#25388,.T.);
#39436=EDGE_CURVE('',#31533,#31530,#18504,.T.);
#39437=EDGE_CURVE('',#31532,#31533,#18505,.T.);
#39438=EDGE_CURVE('',#31534,#31338,#25389,.T.);
#39439=EDGE_CURVE('',#31534,#31535,#18506,.T.);
#39440=EDGE_CURVE('',#31057,#31535,#22844,.T.);
#39441=EDGE_CURVE('',#31535,#31536,#18507,.T.);
#39442=EDGE_CURVE('',#31339,#31536,#25390,.T.);
#39443=EDGE_CURVE('',#31537,#31534,#18508,.T.);
#39444=EDGE_CURVE('',#31536,#31537,#18509,.T.);
#39445=EDGE_CURVE('',#31538,#31339,#25391,.T.);
#39446=EDGE_CURVE('',#31538,#31539,#18510,.T.);
#39447=EDGE_CURVE('',#31058,#31539,#22845,.T.);
#39448=EDGE_CURVE('',#31539,#31540,#18511,.T.);
#39449=EDGE_CURVE('',#31340,#31540,#25392,.T.);
#39450=EDGE_CURVE('',#31541,#31538,#18512,.T.);
#39451=EDGE_CURVE('',#31540,#31541,#18513,.T.);
#39452=EDGE_CURVE('',#31542,#31340,#25393,.T.);
#39453=EDGE_CURVE('',#31542,#31543,#18514,.T.);
#39454=EDGE_CURVE('',#31059,#31543,#22846,.T.);
#39455=EDGE_CURVE('',#31543,#31544,#18515,.T.);
#39456=EDGE_CURVE('',#31341,#31544,#25394,.T.);
#39457=EDGE_CURVE('',#31545,#31542,#18516,.T.);
#39458=EDGE_CURVE('',#31544,#31545,#18517,.T.);
#39459=EDGE_CURVE('',#31546,#31341,#25395,.T.);
#39460=EDGE_CURVE('',#31546,#31547,#18518,.T.);
#39461=EDGE_CURVE('',#31060,#31547,#22847,.T.);
#39462=EDGE_CURVE('',#31547,#31548,#18519,.T.);
#39463=EDGE_CURVE('',#31342,#31548,#25396,.T.);
#39464=EDGE_CURVE('',#31549,#31546,#18520,.T.);
#39465=EDGE_CURVE('',#31548,#31549,#18521,.T.);
#39466=EDGE_CURVE('',#31550,#31342,#25397,.T.);
#39467=EDGE_CURVE('',#31550,#31551,#18522,.T.);
#39468=EDGE_CURVE('',#31061,#31551,#22848,.T.);
#39469=EDGE_CURVE('',#31551,#31552,#18523,.T.);
#39470=EDGE_CURVE('',#31343,#31552,#25398,.T.);
#39471=EDGE_CURVE('',#31553,#31550,#18524,.T.);
#39472=EDGE_CURVE('',#31552,#31553,#18525,.T.);
#39473=EDGE_CURVE('',#31554,#31343,#25399,.T.);
#39474=EDGE_CURVE('',#31554,#31555,#18526,.T.);
#39475=EDGE_CURVE('',#31062,#31555,#22849,.T.);
#39476=EDGE_CURVE('',#31555,#31556,#18527,.T.);
#39477=EDGE_CURVE('',#31344,#31556,#25400,.T.);
#39478=EDGE_CURVE('',#31557,#31554,#18528,.T.);
#39479=EDGE_CURVE('',#31556,#31557,#18529,.T.);
#39480=EDGE_CURVE('',#31558,#31344,#25401,.T.);
#39481=EDGE_CURVE('',#31558,#31559,#18530,.T.);
#39482=EDGE_CURVE('',#31063,#31559,#22850,.T.);
#39483=EDGE_CURVE('',#31559,#31560,#18531,.T.);
#39484=EDGE_CURVE('',#31345,#31560,#25402,.T.);
#39485=EDGE_CURVE('',#31561,#31558,#18532,.T.);
#39486=EDGE_CURVE('',#31560,#31561,#18533,.T.);
#39487=EDGE_CURVE('',#31562,#31345,#25403,.T.);
#39488=EDGE_CURVE('',#31562,#31563,#18534,.T.);
#39489=EDGE_CURVE('',#31064,#31563,#22851,.T.);
#39490=EDGE_CURVE('',#31563,#31564,#18535,.T.);
#39491=EDGE_CURVE('',#31346,#31564,#25404,.T.);
#39492=EDGE_CURVE('',#31565,#31562,#18536,.T.);
#39493=EDGE_CURVE('',#31564,#31565,#18537,.T.);
#39494=EDGE_CURVE('',#31566,#31346,#25405,.T.);
#39495=EDGE_CURVE('',#31566,#31567,#18538,.T.);
#39496=EDGE_CURVE('',#31065,#31567,#22852,.T.);
#39497=EDGE_CURVE('',#31567,#31568,#18539,.T.);
#39498=EDGE_CURVE('',#31347,#31568,#25406,.T.);
#39499=EDGE_CURVE('',#31569,#31566,#18540,.T.);
#39500=EDGE_CURVE('',#31568,#31569,#18541,.T.);
#39501=EDGE_CURVE('',#31570,#31460,#18542,.T.);
#39502=EDGE_CURVE('',#31571,#31570,#18543,.T.);
#39503=EDGE_CURVE('',#31461,#31571,#18544,.T.);
#39504=EDGE_CURVE('',#31570,#31347,#25407,.T.);
#39505=EDGE_CURVE('',#31290,#31572,#18545,.T.);
#39506=EDGE_CURVE('',#31572,#31458,#22853,.T.);
#39507=EDGE_CURVE('',#31573,#31290,#22854,.T.);
#39508=EDGE_CURVE('',#31352,#31573,#22855,.T.);
#39509=EDGE_CURVE('',#31291,#31573,#18546,.T.);
#39510=EDGE_CURVE('',#31574,#31291,#22856,.T.);
#39511=EDGE_CURVE('',#31356,#31574,#22857,.T.);
#39512=EDGE_CURVE('',#31292,#31574,#18547,.T.);
#39513=EDGE_CURVE('',#31575,#31292,#22858,.T.);
#39514=EDGE_CURVE('',#31360,#31575,#22859,.T.);
#39515=EDGE_CURVE('',#31293,#31575,#18548,.T.);
#39516=EDGE_CURVE('',#31576,#31293,#22860,.T.);
#39517=EDGE_CURVE('',#31364,#31576,#22861,.T.);
#39518=EDGE_CURVE('',#31294,#31576,#18549,.T.);
#39519=EDGE_CURVE('',#31577,#31294,#22862,.T.);
#39520=EDGE_CURVE('',#31368,#31577,#22863,.T.);
#39521=EDGE_CURVE('',#31295,#31577,#18550,.T.);
#39522=EDGE_CURVE('',#31578,#31295,#22864,.T.);
#39523=EDGE_CURVE('',#31372,#31578,#22865,.T.);
#39524=EDGE_CURVE('',#31296,#31578,#18551,.T.);
#39525=EDGE_CURVE('',#31579,#31296,#22866,.T.);
#39526=EDGE_CURVE('',#28969,#31579,#22867,.T.);
#39527=EDGE_CURVE('',#31297,#31579,#18552,.T.);
#39528=EDGE_CURVE('',#31580,#31297,#22868,.T.);
#39529=EDGE_CURVE('',#31376,#31580,#22869,.T.);
#39530=EDGE_CURVE('',#31298,#31580,#18553,.T.);
#39531=EDGE_CURVE('',#31581,#31298,#22870,.T.);
#39532=EDGE_CURVE('',#31380,#31581,#22871,.T.);
#39533=EDGE_CURVE('',#31299,#31581,#18554,.T.);
#39534=EDGE_CURVE('',#31582,#31299,#22872,.T.);
#39535=EDGE_CURVE('',#31384,#31582,#22873,.T.);
#39536=EDGE_CURVE('',#31300,#31582,#18555,.T.);
#39537=EDGE_CURVE('',#31583,#31300,#22874,.T.);
#39538=EDGE_CURVE('',#31388,#31583,#22875,.T.);
#39539=EDGE_CURVE('',#31301,#31583,#18556,.T.);
#39540=EDGE_CURVE('',#31584,#31301,#22876,.T.);
#39541=EDGE_CURVE('',#31392,#31584,#22877,.T.);
#39542=EDGE_CURVE('',#31302,#31584,#18557,.T.);
#39543=EDGE_CURVE('',#31585,#31302,#22878,.T.);
#39544=EDGE_CURVE('',#31396,#31585,#22879,.T.);
#39545=EDGE_CURVE('',#31303,#31585,#18558,.T.);
#39546=EDGE_CURVE('',#31586,#31303,#22880,.T.);
#39547=EDGE_CURVE('',#31400,#31586,#22881,.T.);
#39548=EDGE_CURVE('',#31304,#31586,#18559,.T.);
#39549=EDGE_CURVE('',#31587,#31304,#22882,.T.);
#39550=EDGE_CURVE('',#31404,#31587,#22883,.T.);
#39551=EDGE_CURVE('',#31305,#31587,#18560,.T.);
#39552=EDGE_CURVE('',#31588,#31305,#22884,.T.);
#39553=EDGE_CURVE('',#31408,#31588,#22885,.T.);
#39554=EDGE_CURVE('',#31306,#31588,#18561,.T.);
#39555=EDGE_CURVE('',#31589,#31306,#22886,.T.);
#39556=EDGE_CURVE('',#31412,#31589,#22887,.T.);
#39557=EDGE_CURVE('',#31307,#31589,#18562,.T.);
#39558=EDGE_CURVE('',#31590,#31307,#22888,.T.);
#39559=EDGE_CURVE('',#31416,#31590,#22889,.T.);
#39560=EDGE_CURVE('',#31308,#31590,#18563,.T.);
#39561=EDGE_CURVE('',#31591,#31308,#22890,.T.);
#39562=EDGE_CURVE('',#31420,#31591,#22891,.T.);
#39563=EDGE_CURVE('',#31309,#31591,#18564,.T.);
#39564=EDGE_CURVE('',#31592,#31309,#22892,.T.);
#39565=EDGE_CURVE('',#31424,#31592,#22893,.T.);
#39566=EDGE_CURVE('',#31310,#31592,#18565,.T.);
#39567=EDGE_CURVE('',#31593,#31310,#22894,.T.);
#39568=EDGE_CURVE('',#31429,#31593,#22895,.T.);
#39569=EDGE_CURVE('',#31311,#31593,#18566,.T.);
#39570=EDGE_CURVE('',#31594,#31311,#22896,.T.);
#39571=EDGE_CURVE('',#31433,#31594,#22897,.T.);
#39572=EDGE_CURVE('',#31312,#31594,#18567,.T.);
#39573=EDGE_CURVE('',#31595,#31312,#22898,.T.);
#39574=EDGE_CURVE('',#31436,#31595,#22899,.T.);
#39575=EDGE_CURVE('',#31313,#31595,#18568,.T.);
#39576=EDGE_CURVE('',#31596,#31313,#22900,.T.);
#39577=EDGE_CURVE('',#31440,#31596,#22901,.T.);
#39578=EDGE_CURVE('',#31314,#31596,#18569,.T.);
#39579=EDGE_CURVE('',#31597,#31314,#22902,.T.);
#39580=EDGE_CURVE('',#31444,#31597,#22903,.T.);
#39581=EDGE_CURVE('',#31315,#31597,#18570,.T.);
#39582=EDGE_CURVE('',#31598,#31315,#22904,.T.);
#39583=EDGE_CURVE('',#31448,#31598,#22905,.T.);
#39584=EDGE_CURVE('',#31316,#31598,#18571,.T.);
#39585=EDGE_CURVE('',#31599,#31316,#22906,.T.);
#39586=EDGE_CURVE('',#31452,#31599,#22907,.T.);
#39587=EDGE_CURVE('',#31317,#31599,#18572,.T.);
#39588=EDGE_CURVE('',#31600,#31317,#22908,.T.);
#39589=EDGE_CURVE('',#31456,#31600,#22909,.T.);
#39590=EDGE_CURVE('',#31318,#31600,#18573,.T.);
#39591=EDGE_CURVE('',#31572,#31318,#22910,.T.);
#39592=EDGE_CURVE('',#31601,#31571,#22911,.T.);
#39593=EDGE_CURVE('',#31319,#31601,#18574,.T.);
#39594=EDGE_CURVE('',#31602,#31319,#18575,.T.);
#39595=EDGE_CURVE('',#31465,#31602,#22912,.T.);
#39596=EDGE_CURVE('',#31320,#31602,#18576,.T.);
#39597=EDGE_CURVE('',#31603,#31320,#18577,.T.);
#39598=EDGE_CURVE('',#31469,#31603,#22913,.T.);
#39599=EDGE_CURVE('',#31321,#31603,#18578,.T.);
#39600=EDGE_CURVE('',#31604,#31321,#18579,.T.);
#39601=EDGE_CURVE('',#31473,#31604,#22914,.T.);
#39602=EDGE_CURVE('',#31322,#31604,#18580,.T.);
#39603=EDGE_CURVE('',#31605,#31322,#18581,.T.);
#39604=EDGE_CURVE('',#31477,#31605,#22915,.T.);
#39605=EDGE_CURVE('',#31323,#31605,#18582,.T.);
#39606=EDGE_CURVE('',#31606,#31323,#18583,.T.);
#39607=EDGE_CURVE('',#31481,#31606,#22916,.T.);
#39608=EDGE_CURVE('',#31324,#31606,#18584,.T.);
#39609=EDGE_CURVE('',#31607,#31324,#18585,.T.);
#39610=EDGE_CURVE('',#31485,#31607,#22917,.T.);
#39611=EDGE_CURVE('',#31325,#31607,#18586,.T.);
#39612=EDGE_CURVE('',#31608,#31325,#18587,.T.);
#39613=EDGE_CURVE('',#31489,#31608,#22918,.T.);
#39614=EDGE_CURVE('',#31326,#31608,#18588,.T.);
#39615=EDGE_CURVE('',#31609,#31326,#18589,.T.);
#39616=EDGE_CURVE('',#31493,#31609,#22919,.T.);
#39617=EDGE_CURVE('',#31327,#31609,#18590,.T.);
#39618=EDGE_CURVE('',#31610,#31327,#18591,.T.);
#39619=EDGE_CURVE('',#31497,#31610,#22920,.T.);
#39620=EDGE_CURVE('',#31328,#31610,#18592,.T.);
#39621=EDGE_CURVE('',#31611,#31328,#18593,.T.);
#39622=EDGE_CURVE('',#31501,#31611,#22921,.T.);
#39623=EDGE_CURVE('',#31329,#31611,#18594,.T.);
#39624=EDGE_CURVE('',#31612,#31329,#18595,.T.);
#39625=EDGE_CURVE('',#31505,#31612,#22922,.T.);
#39626=EDGE_CURVE('',#31330,#31612,#18596,.T.);
#39627=EDGE_CURVE('',#31613,#31330,#18597,.T.);
#39628=EDGE_CURVE('',#31509,#31613,#22923,.T.);
#39629=EDGE_CURVE('',#31331,#31613,#18598,.T.);
#39630=EDGE_CURVE('',#31614,#31331,#18599,.T.);
#39631=EDGE_CURVE('',#31513,#31614,#22924,.T.);
#39632=EDGE_CURVE('',#31332,#31614,#18600,.T.);
#39633=EDGE_CURVE('',#31615,#31332,#18601,.T.);
#39634=EDGE_CURVE('',#28963,#31615,#22925,.T.);
#39635=EDGE_CURVE('',#31333,#31615,#18602,.T.);
#39636=EDGE_CURVE('',#31616,#31333,#18603,.T.);
#39637=EDGE_CURVE('',#31517,#31616,#22926,.T.);
#39638=EDGE_CURVE('',#31334,#31616,#18604,.T.);
#39639=EDGE_CURVE('',#31617,#31334,#18605,.T.);
#39640=EDGE_CURVE('',#31521,#31617,#22927,.T.);
#39641=EDGE_CURVE('',#31335,#31617,#18606,.T.);
#39642=EDGE_CURVE('',#31618,#31335,#18607,.T.);
#39643=EDGE_CURVE('',#31525,#31618,#22928,.T.);
#39644=EDGE_CURVE('',#31336,#31618,#18608,.T.);
#39645=EDGE_CURVE('',#31619,#31336,#18609,.T.);
#39646=EDGE_CURVE('',#31529,#31619,#22929,.T.);
#39647=EDGE_CURVE('',#31337,#31619,#18610,.T.);
#39648=EDGE_CURVE('',#31620,#31337,#18611,.T.);
#39649=EDGE_CURVE('',#31533,#31620,#22930,.T.);
#39650=EDGE_CURVE('',#31338,#31620,#18612,.T.);
#39651=EDGE_CURVE('',#31621,#31338,#18613,.T.);
#39652=EDGE_CURVE('',#31537,#31621,#22931,.T.);
#39653=EDGE_CURVE('',#31339,#31621,#18614,.T.);
#39654=EDGE_CURVE('',#31622,#31339,#18615,.T.);
#39655=EDGE_CURVE('',#31541,#31622,#22932,.T.);
#39656=EDGE_CURVE('',#31340,#31622,#18616,.T.);
#39657=EDGE_CURVE('',#31623,#31340,#18617,.T.);
#39658=EDGE_CURVE('',#31545,#31623,#22933,.T.);
#39659=EDGE_CURVE('',#31341,#31623,#18618,.T.);
#39660=EDGE_CURVE('',#31624,#31341,#18619,.T.);
#39661=EDGE_CURVE('',#31549,#31624,#22934,.T.);
#39662=EDGE_CURVE('',#31342,#31624,#18620,.T.);
#39663=EDGE_CURVE('',#31625,#31342,#18621,.T.);
#39664=EDGE_CURVE('',#31553,#31625,#22935,.T.);
#39665=EDGE_CURVE('',#31343,#31625,#18622,.T.);
#39666=EDGE_CURVE('',#31626,#31343,#18623,.T.);
#39667=EDGE_CURVE('',#31557,#31626,#22936,.T.);
#39668=EDGE_CURVE('',#31344,#31626,#18624,.T.);
#39669=EDGE_CURVE('',#31627,#31344,#18625,.T.);
#39670=EDGE_CURVE('',#31561,#31627,#22937,.T.);
#39671=EDGE_CURVE('',#31345,#31627,#18626,.T.);
#39672=EDGE_CURVE('',#31628,#31345,#18627,.T.);
#39673=EDGE_CURVE('',#31565,#31628,#22938,.T.);
#39674=EDGE_CURVE('',#31346,#31628,#18628,.T.);
#39675=EDGE_CURVE('',#31629,#31346,#18629,.T.);
#39676=EDGE_CURVE('',#31569,#31629,#22939,.T.);
#39677=EDGE_CURVE('',#31347,#31629,#18630,.T.);
#39678=EDGE_CURVE('',#31601,#31347,#18631,.T.);
#39679=EDGE_CURVE('',#31630,#31631,#18632,.T.);
#39680=EDGE_CURVE('',#31290,#31631,#22940,.T.);
#39681=EDGE_CURVE('',#31630,#31572,#25408,.T.);
#39682=EDGE_CURVE('',#31632,#31630,#18633,.T.);
#39683=EDGE_CURVE('',#31633,#31632,#18634,.T.);
#39684=EDGE_CURVE('',#31631,#31633,#22941,.T.);
#39685=EDGE_CURVE('',#31573,#31633,#25409,.T.);
#39686=EDGE_CURVE('',#31634,#31635,#18635,.T.);
#39687=EDGE_CURVE('',#31291,#31635,#22942,.T.);
#39688=EDGE_CURVE('',#31634,#31573,#25410,.T.);
#39689=EDGE_CURVE('',#31636,#31634,#18636,.T.);
#39690=EDGE_CURVE('',#31637,#31636,#18637,.T.);
#39691=EDGE_CURVE('',#31635,#31637,#22943,.T.);
#39692=EDGE_CURVE('',#31574,#31637,#25411,.T.);
#39693=EDGE_CURVE('',#31638,#31639,#18638,.T.);
#39694=EDGE_CURVE('',#31292,#31639,#22944,.T.);
#39695=EDGE_CURVE('',#31638,#31574,#25412,.T.);
#39696=EDGE_CURVE('',#31640,#31638,#18639,.T.);
#39697=EDGE_CURVE('',#31641,#31640,#18640,.T.);
#39698=EDGE_CURVE('',#31639,#31641,#22945,.T.);
#39699=EDGE_CURVE('',#31575,#31641,#25413,.T.);
#39700=EDGE_CURVE('',#31642,#31643,#18641,.T.);
#39701=EDGE_CURVE('',#31293,#31643,#22946,.T.);
#39702=EDGE_CURVE('',#31642,#31575,#25414,.T.);
#39703=EDGE_CURVE('',#31644,#31642,#18642,.T.);
#39704=EDGE_CURVE('',#31645,#31644,#18643,.T.);
#39705=EDGE_CURVE('',#31643,#31645,#22947,.T.);
#39706=EDGE_CURVE('',#31576,#31645,#25415,.T.);
#39707=EDGE_CURVE('',#31646,#31647,#18644,.T.);
#39708=EDGE_CURVE('',#31294,#31647,#22948,.T.);
#39709=EDGE_CURVE('',#31646,#31576,#25416,.T.);
#39710=EDGE_CURVE('',#31648,#31646,#18645,.T.);
#39711=EDGE_CURVE('',#31649,#31648,#18646,.T.);
#39712=EDGE_CURVE('',#31647,#31649,#22949,.T.);
#39713=EDGE_CURVE('',#31577,#31649,#25417,.T.);
#39714=EDGE_CURVE('',#31650,#31651,#18647,.T.);
#39715=EDGE_CURVE('',#31295,#31651,#22950,.T.);
#39716=EDGE_CURVE('',#31650,#31577,#25418,.T.);
#39717=EDGE_CURVE('',#31652,#31650,#18648,.T.);
#39718=EDGE_CURVE('',#31653,#31652,#18649,.T.);
#39719=EDGE_CURVE('',#31651,#31653,#22951,.T.);
#39720=EDGE_CURVE('',#31578,#31653,#25419,.T.);
#39721=EDGE_CURVE('',#31654,#31655,#18650,.T.);
#39722=EDGE_CURVE('',#31296,#31655,#22952,.T.);
#39723=EDGE_CURVE('',#31654,#31578,#25420,.T.);
#39724=EDGE_CURVE('',#31656,#31654,#18651,.T.);
#39725=EDGE_CURVE('',#31657,#31656,#18652,.T.);
#39726=EDGE_CURVE('',#31655,#31657,#22953,.T.);
#39727=EDGE_CURVE('',#31579,#31657,#25421,.T.);
#39728=EDGE_CURVE('',#31658,#31659,#18653,.T.);
#39729=EDGE_CURVE('',#31297,#31659,#22954,.T.);
#39730=EDGE_CURVE('',#31658,#31579,#25422,.T.);
#39731=EDGE_CURVE('',#31660,#31658,#18654,.T.);
#39732=EDGE_CURVE('',#31661,#31660,#18655,.T.);
#39733=EDGE_CURVE('',#31659,#31661,#22955,.T.);
#39734=EDGE_CURVE('',#31580,#31661,#25423,.T.);
#39735=EDGE_CURVE('',#31662,#31663,#18656,.T.);
#39736=EDGE_CURVE('',#31298,#31663,#22956,.T.);
#39737=EDGE_CURVE('',#31662,#31580,#25424,.T.);
#39738=EDGE_CURVE('',#31664,#31662,#18657,.T.);
#39739=EDGE_CURVE('',#31665,#31664,#18658,.T.);
#39740=EDGE_CURVE('',#31663,#31665,#4442,.T.);
#39741=EDGE_CURVE('',#31581,#31665,#25425,.T.);
#39742=EDGE_CURVE('',#31666,#31667,#18659,.T.);
#39743=EDGE_CURVE('',#31299,#31667,#22957,.T.);
#39744=EDGE_CURVE('',#31666,#31581,#25426,.T.);
#39745=EDGE_CURVE('',#31668,#31666,#18660,.T.);
#39746=EDGE_CURVE('',#31669,#31668,#18661,.T.);
#39747=EDGE_CURVE('',#31667,#31669,#22958,.T.);
#39748=EDGE_CURVE('',#31582,#31669,#25427,.T.);
#39749=EDGE_CURVE('',#31670,#31671,#18662,.T.);
#39750=EDGE_CURVE('',#31300,#31671,#22959,.T.);
#39751=EDGE_CURVE('',#31670,#31582,#25428,.T.);
#39752=EDGE_CURVE('',#31672,#31670,#18663,.T.);
#39753=EDGE_CURVE('',#31673,#31672,#18664,.T.);
#39754=EDGE_CURVE('',#31671,#31673,#22960,.T.);
#39755=EDGE_CURVE('',#31583,#31673,#25429,.T.);
#39756=EDGE_CURVE('',#31674,#31675,#18665,.T.);
#39757=EDGE_CURVE('',#31301,#31675,#22961,.T.);
#39758=EDGE_CURVE('',#31674,#31583,#25430,.T.);
#39759=EDGE_CURVE('',#31676,#31674,#18666,.T.);
#39760=EDGE_CURVE('',#31677,#31676,#18667,.T.);
#39761=EDGE_CURVE('',#31675,#31677,#22962,.T.);
#39762=EDGE_CURVE('',#31584,#31677,#25431,.T.);
#39763=EDGE_CURVE('',#31678,#31679,#18668,.T.);
#39764=EDGE_CURVE('',#31302,#31679,#22963,.T.);
#39765=EDGE_CURVE('',#31678,#31584,#25432,.T.);
#39766=EDGE_CURVE('',#31680,#31678,#18669,.T.);
#39767=EDGE_CURVE('',#31681,#31680,#18670,.T.);
#39768=EDGE_CURVE('',#31679,#31681,#22964,.T.);
#39769=EDGE_CURVE('',#31585,#31681,#25433,.T.);
#39770=EDGE_CURVE('',#31682,#31683,#18671,.T.);
#39771=EDGE_CURVE('',#31303,#31683,#22965,.T.);
#39772=EDGE_CURVE('',#31682,#31585,#25434,.T.);
#39773=EDGE_CURVE('',#31684,#31682,#18672,.T.);
#39774=EDGE_CURVE('',#31685,#31684,#18673,.T.);
#39775=EDGE_CURVE('',#31683,#31685,#22966,.T.);
#39776=EDGE_CURVE('',#31586,#31685,#25435,.T.);
#39777=EDGE_CURVE('',#31304,#28959,#22967,.T.);
#39778=EDGE_CURVE('',#28958,#31586,#25436,.T.);
#39779=EDGE_CURVE('',#31587,#28961,#25437,.T.);
#39780=EDGE_CURVE('',#31686,#31687,#18674,.T.);
#39781=EDGE_CURVE('',#31305,#31687,#22968,.T.);
#39782=EDGE_CURVE('',#31686,#31587,#25438,.T.);
#39783=EDGE_CURVE('',#31688,#31686,#18675,.T.);
#39784=EDGE_CURVE('',#31689,#31688,#18676,.T.);
#39785=EDGE_CURVE('',#31687,#31689,#22969,.T.);
#39786=EDGE_CURVE('',#31588,#31689,#25439,.T.);
#39787=EDGE_CURVE('',#31690,#31691,#18677,.T.);
#39788=EDGE_CURVE('',#31306,#31691,#22970,.T.);
#39789=EDGE_CURVE('',#31690,#31588,#25440,.T.);
#39790=EDGE_CURVE('',#31692,#31690,#18678,.T.);
#39791=EDGE_CURVE('',#31693,#31692,#18679,.T.);
#39792=EDGE_CURVE('',#31691,#31693,#22971,.T.);
#39793=EDGE_CURVE('',#31589,#31693,#25441,.T.);
#39794=EDGE_CURVE('',#31694,#31695,#18680,.T.);
#39795=EDGE_CURVE('',#31307,#31695,#22972,.T.);
#39796=EDGE_CURVE('',#31694,#31589,#25442,.T.);
#39797=EDGE_CURVE('',#31696,#31694,#18681,.T.);
#39798=EDGE_CURVE('',#31697,#31696,#18682,.T.);
#39799=EDGE_CURVE('',#31695,#31697,#22973,.T.);
#39800=EDGE_CURVE('',#31590,#31697,#25443,.T.);
#39801=EDGE_CURVE('',#31698,#31699,#18683,.T.);
#39802=EDGE_CURVE('',#31308,#31699,#22974,.T.);
#39803=EDGE_CURVE('',#31698,#31590,#25444,.T.);
#39804=EDGE_CURVE('',#31700,#31698,#18684,.T.);
#39805=EDGE_CURVE('',#31701,#31700,#18685,.T.);
#39806=EDGE_CURVE('',#31699,#31701,#22975,.T.);
#39807=EDGE_CURVE('',#31591,#31701,#25445,.T.);
#39808=EDGE_CURVE('',#31702,#31703,#18686,.T.);
#39809=EDGE_CURVE('',#31309,#31703,#22976,.T.);
#39810=EDGE_CURVE('',#31702,#31591,#25446,.T.);
#39811=EDGE_CURVE('',#31704,#31702,#18687,.T.);
#39812=EDGE_CURVE('',#31705,#31704,#18688,.T.);
#39813=EDGE_CURVE('',#31703,#31705,#22977,.T.);
#39814=EDGE_CURVE('',#31592,#31705,#25447,.T.);
#39815=EDGE_CURVE('',#31706,#31707,#18689,.T.);
#39816=EDGE_CURVE('',#31310,#31707,#22978,.T.);
#39817=EDGE_CURVE('',#31706,#31592,#25448,.T.);
#39818=EDGE_CURVE('',#31707,#31708,#22979,.T.);
#39819=EDGE_CURVE('',#31593,#31708,#25449,.T.);
#39820=EDGE_CURVE('',#31709,#31706,#18690,.T.);
#39821=EDGE_CURVE('',#31708,#31709,#18691,.T.);
#39822=EDGE_CURVE('',#31710,#31593,#25450,.T.);
#39823=EDGE_CURVE('',#31710,#31711,#18692,.T.);
#39824=EDGE_CURVE('',#31311,#31711,#22980,.T.);
#39825=EDGE_CURVE('',#31711,#31712,#22981,.T.);
#39826=EDGE_CURVE('',#31713,#31710,#18693,.T.);
#39827=EDGE_CURVE('',#31712,#31713,#18694,.T.);
#39828=EDGE_CURVE('',#31594,#31712,#25451,.T.);
#39829=EDGE_CURVE('',#31714,#31715,#18695,.T.);
#39830=EDGE_CURVE('',#31312,#31715,#22982,.T.);
#39831=EDGE_CURVE('',#31714,#31594,#25452,.T.);
#39832=EDGE_CURVE('',#31716,#31714,#18696,.T.);
#39833=EDGE_CURVE('',#31717,#31716,#18697,.T.);
#39834=EDGE_CURVE('',#31715,#31717,#22983,.T.);
#39835=EDGE_CURVE('',#31595,#31717,#25453,.T.);
#39836=EDGE_CURVE('',#31718,#31719,#18698,.T.);
#39837=EDGE_CURVE('',#31313,#31719,#22984,.T.);
#39838=EDGE_CURVE('',#31718,#31595,#25454,.T.);
#39839=EDGE_CURVE('',#31720,#31718,#18699,.T.);
#39840=EDGE_CURVE('',#31721,#31720,#18700,.T.);
#39841=EDGE_CURVE('',#31719,#31721,#22985,.T.);
#39842=EDGE_CURVE('',#31596,#31721,#25455,.T.);
#39843=EDGE_CURVE('',#31722,#31723,#18701,.T.);
#39844=EDGE_CURVE('',#31314,#31723,#22986,.T.);
#39845=EDGE_CURVE('',#31722,#31596,#25456,.T.);
#39846=EDGE_CURVE('',#31724,#31722,#18702,.T.);
#39847=EDGE_CURVE('',#31725,#31724,#18703,.T.);
#39848=EDGE_CURVE('',#31723,#31725,#22987,.T.);
#39849=EDGE_CURVE('',#31597,#31725,#25457,.T.);
#39850=EDGE_CURVE('',#31726,#31727,#18704,.T.);
#39851=EDGE_CURVE('',#31315,#31727,#22988,.T.);
#39852=EDGE_CURVE('',#31726,#31597,#25458,.T.);
#39853=EDGE_CURVE('',#31728,#31726,#18705,.T.);
#39854=EDGE_CURVE('',#31729,#31728,#18706,.T.);
#39855=EDGE_CURVE('',#31727,#31729,#22989,.T.);
#39856=EDGE_CURVE('',#31598,#31729,#25459,.T.);
#39857=EDGE_CURVE('',#31730,#31731,#18707,.T.);
#39858=EDGE_CURVE('',#31316,#31731,#22990,.T.);
#39859=EDGE_CURVE('',#31730,#31598,#25460,.T.);
#39860=EDGE_CURVE('',#31732,#31730,#18708,.T.);
#39861=EDGE_CURVE('',#31733,#31732,#18709,.T.);
#39862=EDGE_CURVE('',#31731,#31733,#22991,.T.);
#39863=EDGE_CURVE('',#31599,#31733,#25461,.T.);
#39864=EDGE_CURVE('',#31734,#31735,#18710,.T.);
#39865=EDGE_CURVE('',#31317,#31735,#22992,.T.);
#39866=EDGE_CURVE('',#31734,#31599,#25462,.T.);
#39867=EDGE_CURVE('',#31736,#31734,#18711,.T.);
#39868=EDGE_CURVE('',#31737,#31736,#18712,.T.);
#39869=EDGE_CURVE('',#31735,#31737,#22993,.T.);
#39870=EDGE_CURVE('',#31600,#31737,#25463,.T.);
#39871=EDGE_CURVE('',#31738,#31739,#18713,.T.);
#39872=EDGE_CURVE('',#31318,#31739,#22994,.T.);
#39873=EDGE_CURVE('',#31738,#31600,#25464,.T.);
#39874=EDGE_CURVE('',#31740,#31738,#18714,.T.);
#39875=EDGE_CURVE('',#31741,#31740,#18715,.T.);
#39876=EDGE_CURVE('',#31739,#31741,#22995,.T.);
#39877=EDGE_CURVE('',#31572,#31741,#25465,.T.);
#39878=EDGE_CURVE('',#31742,#31601,#25466,.T.);
#39879=EDGE_CURVE('',#31742,#31743,#18716,.T.);
#39880=EDGE_CURVE('',#31319,#31743,#22996,.T.);
#39881=EDGE_CURVE('',#31743,#31744,#18717,.T.);
#39882=EDGE_CURVE('',#31602,#31744,#25467,.T.);
#39883=EDGE_CURVE('',#31745,#31742,#18718,.T.);
#39884=EDGE_CURVE('',#31744,#31745,#18719,.T.);
#39885=EDGE_CURVE('',#31746,#31602,#25468,.T.);
#39886=EDGE_CURVE('',#31746,#31747,#18720,.T.);
#39887=EDGE_CURVE('',#31320,#31747,#22997,.T.);
#39888=EDGE_CURVE('',#31747,#31748,#18721,.T.);
#39889=EDGE_CURVE('',#31603,#31748,#25469,.T.);
#39890=EDGE_CURVE('',#31749,#31746,#18722,.T.);
#39891=EDGE_CURVE('',#31748,#31749,#18723,.T.);
#39892=EDGE_CURVE('',#31750,#31603,#25470,.T.);
#39893=EDGE_CURVE('',#31750,#31751,#18724,.T.);
#39894=EDGE_CURVE('',#31321,#31751,#22998,.T.);
#39895=EDGE_CURVE('',#31751,#31752,#18725,.T.);
#39896=EDGE_CURVE('',#31604,#31752,#25471,.T.);
#39897=EDGE_CURVE('',#31753,#31750,#18726,.T.);
#39898=EDGE_CURVE('',#31752,#31753,#18727,.T.);
#39899=EDGE_CURVE('',#31754,#31604,#25472,.T.);
#39900=EDGE_CURVE('',#31754,#31755,#18728,.T.);
#39901=EDGE_CURVE('',#31322,#31755,#22999,.T.);
#39902=EDGE_CURVE('',#31755,#31756,#18729,.T.);
#39903=EDGE_CURVE('',#31605,#31756,#25473,.T.);
#39904=EDGE_CURVE('',#31757,#31754,#18730,.T.);
#39905=EDGE_CURVE('',#31756,#31757,#18731,.T.);
#39906=EDGE_CURVE('',#31758,#31605,#25474,.T.);
#39907=EDGE_CURVE('',#31758,#31759,#18732,.T.);
#39908=EDGE_CURVE('',#31323,#31759,#23000,.T.);
#39909=EDGE_CURVE('',#31759,#31760,#18733,.T.);
#39910=EDGE_CURVE('',#31606,#31760,#25475,.T.);
#39911=EDGE_CURVE('',#31761,#31758,#18734,.T.);
#39912=EDGE_CURVE('',#31760,#31761,#18735,.T.);
#39913=EDGE_CURVE('',#31762,#31606,#25476,.T.);
#39914=EDGE_CURVE('',#31762,#31763,#18736,.T.);
#39915=EDGE_CURVE('',#31324,#31763,#23001,.T.);
#39916=EDGE_CURVE('',#31763,#31764,#18737,.T.);
#39917=EDGE_CURVE('',#31607,#31764,#25477,.T.);
#39918=EDGE_CURVE('',#31765,#31762,#18738,.T.);
#39919=EDGE_CURVE('',#31764,#31765,#18739,.T.);
#39920=EDGE_CURVE('',#31766,#31607,#25478,.T.);
#39921=EDGE_CURVE('',#31766,#31767,#18740,.T.);
#39922=EDGE_CURVE('',#31325,#31767,#23002,.T.);
#39923=EDGE_CURVE('',#31767,#31768,#18741,.T.);
#39924=EDGE_CURVE('',#31608,#31768,#25479,.T.);
#39925=EDGE_CURVE('',#31769,#31766,#18742,.T.);
#39926=EDGE_CURVE('',#31768,#31769,#18743,.T.);
#39927=EDGE_CURVE('',#31770,#31608,#25480,.T.);
#39928=EDGE_CURVE('',#31770,#31771,#18744,.T.);
#39929=EDGE_CURVE('',#31326,#31771,#23003,.T.);
#39930=EDGE_CURVE('',#31771,#31772,#18745,.T.);
#39931=EDGE_CURVE('',#31609,#31772,#25481,.T.);
#39932=EDGE_CURVE('',#31773,#31770,#18746,.T.);
#39933=EDGE_CURVE('',#31772,#31773,#18747,.T.);
#39934=EDGE_CURVE('',#31774,#31609,#25482,.T.);
#39935=EDGE_CURVE('',#31774,#31775,#18748,.T.);
#39936=EDGE_CURVE('',#31327,#31775,#23004,.T.);
#39937=EDGE_CURVE('',#31775,#31776,#18749,.T.);
#39938=EDGE_CURVE('',#31610,#31776,#25483,.T.);
#39939=EDGE_CURVE('',#31777,#31774,#18750,.T.);
#39940=EDGE_CURVE('',#31776,#31777,#18751,.T.);
#39941=EDGE_CURVE('',#31778,#31610,#25484,.T.);
#39942=EDGE_CURVE('',#31778,#31779,#18752,.T.);
#39943=EDGE_CURVE('',#31328,#31779,#23005,.T.);
#39944=EDGE_CURVE('',#31779,#31780,#18753,.T.);
#39945=EDGE_CURVE('',#31611,#31780,#25485,.T.);
#39946=EDGE_CURVE('',#31781,#31778,#18754,.T.);
#39947=EDGE_CURVE('',#31780,#31781,#18755,.T.);
#39948=EDGE_CURVE('',#31782,#31611,#25486,.T.);
#39949=EDGE_CURVE('',#31782,#31783,#18756,.T.);
#39950=EDGE_CURVE('',#31329,#31783,#23006,.T.);
#39951=EDGE_CURVE('',#31783,#31784,#18757,.T.);
#39952=EDGE_CURVE('',#31612,#31784,#25487,.T.);
#39953=EDGE_CURVE('',#31785,#31782,#18758,.T.);
#39954=EDGE_CURVE('',#31784,#31785,#18759,.T.);
#39955=EDGE_CURVE('',#31786,#31612,#25488,.T.);
#39956=EDGE_CURVE('',#31786,#31787,#18760,.T.);
#39957=EDGE_CURVE('',#31330,#31787,#23007,.T.);
#39958=EDGE_CURVE('',#31787,#31788,#18761,.T.);
#39959=EDGE_CURVE('',#31613,#31788,#25489,.T.);
#39960=EDGE_CURVE('',#31789,#31786,#18762,.T.);
#39961=EDGE_CURVE('',#31788,#31789,#18763,.T.);
#39962=EDGE_CURVE('',#31790,#31613,#25490,.T.);
#39963=EDGE_CURVE('',#31790,#31791,#18764,.T.);
#39964=EDGE_CURVE('',#31331,#31791,#23008,.T.);
#39965=EDGE_CURVE('',#31791,#31792,#18765,.T.);
#39966=EDGE_CURVE('',#31614,#31792,#25491,.T.);
#39967=EDGE_CURVE('',#31793,#31790,#18766,.T.);
#39968=EDGE_CURVE('',#31792,#31793,#18767,.T.);
#39969=EDGE_CURVE('',#31794,#31614,#25492,.T.);
#39970=EDGE_CURVE('',#31794,#31795,#18768,.T.);
#39971=EDGE_CURVE('',#31332,#31795,#23009,.T.);
#39972=EDGE_CURVE('',#31795,#31796,#18769,.T.);
#39973=EDGE_CURVE('',#31615,#31796,#25493,.T.);
#39974=EDGE_CURVE('',#31797,#31794,#18770,.T.);
#39975=EDGE_CURVE('',#31796,#31797,#18771,.T.);
#39976=EDGE_CURVE('',#31798,#31615,#25494,.T.);
#39977=EDGE_CURVE('',#31798,#31799,#18772,.T.);
#39978=EDGE_CURVE('',#31333,#31799,#23010,.T.);
#39979=EDGE_CURVE('',#31799,#31800,#18773,.T.);
#39980=EDGE_CURVE('',#31616,#31800,#25495,.T.);
#39981=EDGE_CURVE('',#31801,#31798,#18774,.T.);
#39982=EDGE_CURVE('',#31800,#31801,#18775,.T.);
#39983=EDGE_CURVE('',#31802,#31616,#25496,.T.);
#39984=EDGE_CURVE('',#31802,#31803,#18776,.T.);
#39985=EDGE_CURVE('',#31334,#31803,#23011,.T.);
#39986=EDGE_CURVE('',#31803,#31804,#18777,.T.);
#39987=EDGE_CURVE('',#31617,#31804,#25497,.T.);
#39988=EDGE_CURVE('',#31805,#31802,#18778,.T.);
#39989=EDGE_CURVE('',#31804,#31805,#18779,.T.);
#39990=EDGE_CURVE('',#31806,#31617,#25498,.T.);
#39991=EDGE_CURVE('',#31806,#31807,#18780,.T.);
#39992=EDGE_CURVE('',#31335,#31807,#23012,.T.);
#39993=EDGE_CURVE('',#31807,#31808,#18781,.T.);
#39994=EDGE_CURVE('',#31618,#31808,#25499,.T.);
#39995=EDGE_CURVE('',#31809,#31806,#18782,.T.);
#39996=EDGE_CURVE('',#31808,#31809,#18783,.T.);
#39997=EDGE_CURVE('',#31810,#31618,#25500,.T.);
#39998=EDGE_CURVE('',#31810,#31811,#18784,.T.);
#39999=EDGE_CURVE('',#31336,#31811,#23013,.T.);
#40000=EDGE_CURVE('',#31811,#31812,#18785,.T.);
#40001=EDGE_CURVE('',#31619,#31812,#25501,.T.);
#40002=EDGE_CURVE('',#31813,#31810,#18786,.T.);
#40003=EDGE_CURVE('',#31812,#31813,#18787,.T.);
#40004=EDGE_CURVE('',#31814,#31619,#25502,.T.);
#40005=EDGE_CURVE('',#31814,#31815,#18788,.T.);
#40006=EDGE_CURVE('',#31337,#31815,#23014,.T.);
#40007=EDGE_CURVE('',#31815,#31816,#18789,.T.);
#40008=EDGE_CURVE('',#31620,#31816,#25503,.T.);
#40009=EDGE_CURVE('',#31817,#31814,#18790,.T.);
#40010=EDGE_CURVE('',#31816,#31817,#18791,.T.);
#40011=EDGE_CURVE('',#31818,#31620,#25504,.T.);
#40012=EDGE_CURVE('',#31818,#31819,#18792,.T.);
#40013=EDGE_CURVE('',#31338,#31819,#23015,.T.);
#40014=EDGE_CURVE('',#31819,#31820,#18793,.T.);
#40015=EDGE_CURVE('',#31621,#31820,#25505,.T.);
#40016=EDGE_CURVE('',#31821,#31818,#18794,.T.);
#40017=EDGE_CURVE('',#31820,#31821,#18795,.T.);
#40018=EDGE_CURVE('',#31822,#31621,#25506,.T.);
#40019=EDGE_CURVE('',#31822,#31823,#18796,.T.);
#40020=EDGE_CURVE('',#31339,#31823,#23016,.T.);
#40021=EDGE_CURVE('',#31823,#31824,#18797,.T.);
#40022=EDGE_CURVE('',#31622,#31824,#25507,.T.);
#40023=EDGE_CURVE('',#31825,#31822,#18798,.T.);
#40024=EDGE_CURVE('',#31824,#31825,#18799,.T.);
#40025=EDGE_CURVE('',#31826,#31622,#25508,.T.);
#40026=EDGE_CURVE('',#31826,#31827,#18800,.T.);
#40027=EDGE_CURVE('',#31340,#31827,#23017,.T.);
#40028=EDGE_CURVE('',#31827,#31828,#18801,.T.);
#40029=EDGE_CURVE('',#31623,#31828,#25509,.T.);
#40030=EDGE_CURVE('',#31829,#31826,#18802,.T.);
#40031=EDGE_CURVE('',#31828,#31829,#18803,.T.);
#40032=EDGE_CURVE('',#31830,#31623,#25510,.T.);
#40033=EDGE_CURVE('',#31830,#31831,#18804,.T.);
#40034=EDGE_CURVE('',#31341,#31831,#23018,.T.);
#40035=EDGE_CURVE('',#31831,#31832,#18805,.T.);
#40036=EDGE_CURVE('',#31624,#31832,#25511,.T.);
#40037=EDGE_CURVE('',#31833,#31830,#18806,.T.);
#40038=EDGE_CURVE('',#31832,#31833,#18807,.T.);
#40039=EDGE_CURVE('',#31834,#31624,#25512,.T.);
#40040=EDGE_CURVE('',#31834,#31835,#18808,.T.);
#40041=EDGE_CURVE('',#31342,#31835,#23019,.T.);
#40042=EDGE_CURVE('',#31835,#31836,#18809,.T.);
#40043=EDGE_CURVE('',#31625,#31836,#25513,.T.);
#40044=EDGE_CURVE('',#31837,#31834,#18810,.T.);
#40045=EDGE_CURVE('',#31836,#31837,#18811,.T.);
#40046=EDGE_CURVE('',#31838,#31625,#25514,.T.);
#40047=EDGE_CURVE('',#31838,#31839,#18812,.T.);
#40048=EDGE_CURVE('',#31343,#31839,#23020,.T.);
#40049=EDGE_CURVE('',#31839,#31840,#18813,.T.);
#40050=EDGE_CURVE('',#31626,#31840,#25515,.T.);
#40051=EDGE_CURVE('',#31841,#31838,#18814,.T.);
#40052=EDGE_CURVE('',#31840,#31841,#18815,.T.);
#40053=EDGE_CURVE('',#31842,#31626,#25516,.T.);
#40054=EDGE_CURVE('',#31842,#31843,#18816,.T.);
#40055=EDGE_CURVE('',#31344,#31843,#23021,.T.);
#40056=EDGE_CURVE('',#31843,#31844,#18817,.T.);
#40057=EDGE_CURVE('',#31627,#31844,#25517,.T.);
#40058=EDGE_CURVE('',#31845,#31842,#18818,.T.);
#40059=EDGE_CURVE('',#31844,#31845,#18819,.T.);
#40060=EDGE_CURVE('',#31846,#31627,#25518,.T.);
#40061=EDGE_CURVE('',#31846,#31847,#18820,.T.);
#40062=EDGE_CURVE('',#31345,#31847,#23022,.T.);
#40063=EDGE_CURVE('',#31847,#31848,#18821,.T.);
#40064=EDGE_CURVE('',#31628,#31848,#25519,.T.);
#40065=EDGE_CURVE('',#31849,#31846,#18822,.T.);
#40066=EDGE_CURVE('',#31848,#31849,#18823,.T.);
#40067=EDGE_CURVE('',#31850,#31628,#25520,.T.);
#40068=EDGE_CURVE('',#31850,#31851,#18824,.T.);
#40069=EDGE_CURVE('',#31346,#31851,#23023,.T.);
#40070=EDGE_CURVE('',#31851,#31852,#18825,.T.);
#40071=EDGE_CURVE('',#31629,#31852,#25521,.T.);
#40072=EDGE_CURVE('',#31853,#31850,#18826,.T.);
#40073=EDGE_CURVE('',#31852,#31853,#18827,.T.);
#40074=EDGE_CURVE('',#31854,#31629,#25522,.T.);
#40075=EDGE_CURVE('',#31854,#31855,#18828,.T.);
#40076=EDGE_CURVE('',#31347,#31855,#23024,.T.);
#40077=EDGE_CURVE('',#31855,#31856,#18829,.T.);
#40078=EDGE_CURVE('',#31601,#31856,#25523,.T.);
#40079=EDGE_CURVE('',#31857,#31854,#18830,.T.);
#40080=EDGE_CURVE('',#31856,#31857,#18831,.T.);
#40081=EDGE_CURVE('',#31858,#31572,#18832,.T.);
#40082=EDGE_CURVE('',#31632,#31858,#23025,.T.);
#40083=EDGE_CURVE('',#31573,#31858,#23026,.T.);
#40084=EDGE_CURVE('',#31859,#31573,#18833,.T.);
#40085=EDGE_CURVE('',#31636,#31859,#23027,.T.);
#40086=EDGE_CURVE('',#31574,#31859,#23028,.T.);
#40087=EDGE_CURVE('',#31860,#31574,#18834,.T.);
#40088=EDGE_CURVE('',#31640,#31860,#23029,.T.);
#40089=EDGE_CURVE('',#31575,#31860,#23030,.T.);
#40090=EDGE_CURVE('',#31861,#31575,#18835,.T.);
#40091=EDGE_CURVE('',#31644,#31861,#23031,.T.);
#40092=EDGE_CURVE('',#31576,#31861,#23032,.T.);
#40093=EDGE_CURVE('',#31862,#31576,#18836,.T.);
#40094=EDGE_CURVE('',#31648,#31862,#23033,.T.);
#40095=EDGE_CURVE('',#31577,#31862,#23034,.T.);
#40096=EDGE_CURVE('',#31863,#31577,#18837,.T.);
#40097=EDGE_CURVE('',#31652,#31863,#23035,.T.);
#40098=EDGE_CURVE('',#31578,#31863,#23036,.T.);
#40099=EDGE_CURVE('',#31864,#31578,#18838,.T.);
#40100=EDGE_CURVE('',#31656,#31864,#23037,.T.);
#40101=EDGE_CURVE('',#31579,#31864,#23038,.T.);
#40102=EDGE_CURVE('',#31865,#31579,#18839,.T.);
#40103=EDGE_CURVE('',#31660,#31865,#23039,.T.);
#40104=EDGE_CURVE('',#31580,#31865,#23040,.T.);
#40105=EDGE_CURVE('',#31866,#31580,#18840,.T.);
#40106=EDGE_CURVE('',#31664,#31866,#23041,.T.);
#40107=EDGE_CURVE('',#31581,#31866,#23042,.T.);
#40108=EDGE_CURVE('',#31867,#31581,#18841,.T.);
#40109=EDGE_CURVE('',#31668,#31867,#23043,.T.);
#40110=EDGE_CURVE('',#31582,#31867,#23044,.T.);
#40111=EDGE_CURVE('',#31868,#31582,#18842,.T.);
#40112=EDGE_CURVE('',#31672,#31868,#23045,.T.);
#40113=EDGE_CURVE('',#31583,#31868,#23046,.T.);
#40114=EDGE_CURVE('',#31869,#31583,#18843,.T.);
#40115=EDGE_CURVE('',#31676,#31869,#23047,.T.);
#40116=EDGE_CURVE('',#31584,#31869,#23048,.T.);
#40117=EDGE_CURVE('',#31870,#31584,#18844,.T.);
#40118=EDGE_CURVE('',#31680,#31870,#23049,.T.);
#40119=EDGE_CURVE('',#31585,#31870,#23050,.T.);
#40120=EDGE_CURVE('',#31871,#31585,#18845,.T.);
#40121=EDGE_CURVE('',#31684,#31871,#23051,.T.);
#40122=EDGE_CURVE('',#31586,#31871,#23052,.T.);
#40123=EDGE_CURVE('',#31872,#31586,#18846,.T.);
#40124=EDGE_CURVE('',#28960,#31872,#23053,.T.);
#40125=EDGE_CURVE('',#31587,#31872,#23054,.T.);
#40126=EDGE_CURVE('',#31873,#31587,#18847,.T.);
#40127=EDGE_CURVE('',#31688,#31873,#23055,.T.);
#40128=EDGE_CURVE('',#31588,#31873,#23056,.T.);
#40129=EDGE_CURVE('',#31874,#31588,#18848,.T.);
#40130=EDGE_CURVE('',#31692,#31874,#23057,.T.);
#40131=EDGE_CURVE('',#31589,#31874,#23058,.T.);
#40132=EDGE_CURVE('',#31875,#31589,#18849,.T.);
#40133=EDGE_CURVE('',#31696,#31875,#23059,.T.);
#40134=EDGE_CURVE('',#31590,#31875,#23060,.T.);
#40135=EDGE_CURVE('',#31876,#31590,#18850,.T.);
#40136=EDGE_CURVE('',#31700,#31876,#23061,.T.);
#40137=EDGE_CURVE('',#31591,#31876,#23062,.T.);
#40138=EDGE_CURVE('',#31877,#31591,#18851,.T.);
#40139=EDGE_CURVE('',#31704,#31877,#23063,.T.);
#40140=EDGE_CURVE('',#31592,#31877,#23064,.T.);
#40141=EDGE_CURVE('',#31878,#31592,#18852,.T.);
#40142=EDGE_CURVE('',#31709,#31878,#23065,.T.);
#40143=EDGE_CURVE('',#31593,#31878,#23066,.T.);
#40144=EDGE_CURVE('',#31879,#31593,#18853,.T.);
#40145=EDGE_CURVE('',#31713,#31879,#23067,.T.);
#40146=EDGE_CURVE('',#31594,#31879,#23068,.T.);
#40147=EDGE_CURVE('',#31880,#31594,#18854,.T.);
#40148=EDGE_CURVE('',#31716,#31880,#23069,.T.);
#40149=EDGE_CURVE('',#31595,#31880,#23070,.T.);
#40150=EDGE_CURVE('',#31881,#31595,#18855,.T.);
#40151=EDGE_CURVE('',#31720,#31881,#23071,.T.);
#40152=EDGE_CURVE('',#31596,#31881,#23072,.T.);
#40153=EDGE_CURVE('',#31882,#31596,#18856,.T.);
#40154=EDGE_CURVE('',#31724,#31882,#23073,.T.);
#40155=EDGE_CURVE('',#31597,#31882,#23074,.T.);
#40156=EDGE_CURVE('',#31883,#31597,#18857,.T.);
#40157=EDGE_CURVE('',#31728,#31883,#23075,.T.);
#40158=EDGE_CURVE('',#31598,#31883,#23076,.T.);
#40159=EDGE_CURVE('',#31884,#31598,#18858,.T.);
#40160=EDGE_CURVE('',#31732,#31884,#23077,.T.);
#40161=EDGE_CURVE('',#31599,#31884,#23078,.T.);
#40162=EDGE_CURVE('',#31885,#31599,#18859,.T.);
#40163=EDGE_CURVE('',#31736,#31885,#23079,.T.);
#40164=EDGE_CURVE('',#31600,#31885,#23080,.T.);
#40165=EDGE_CURVE('',#31886,#31600,#18860,.T.);
#40166=EDGE_CURVE('',#31740,#31886,#23081,.T.);
#40167=EDGE_CURVE('',#31572,#31886,#23082,.T.);
#40168=EDGE_CURVE('',#31887,#31601,#18861,.T.);
#40169=EDGE_CURVE('',#31745,#31887,#23083,.T.);
#40170=EDGE_CURVE('',#31602,#31887,#23084,.T.);
#40171=EDGE_CURVE('',#31888,#31602,#18862,.T.);
#40172=EDGE_CURVE('',#31749,#31888,#23085,.T.);
#40173=EDGE_CURVE('',#31603,#31888,#23086,.T.);
#40174=EDGE_CURVE('',#31889,#31603,#18863,.T.);
#40175=EDGE_CURVE('',#31753,#31889,#23087,.T.);
#40176=EDGE_CURVE('',#31604,#31889,#23088,.T.);
#40177=EDGE_CURVE('',#31890,#31604,#18864,.T.);
#40178=EDGE_CURVE('',#31757,#31890,#23089,.T.);
#40179=EDGE_CURVE('',#31605,#31890,#23090,.T.);
#40180=EDGE_CURVE('',#31891,#31605,#18865,.T.);
#40181=EDGE_CURVE('',#31761,#31891,#23091,.T.);
#40182=EDGE_CURVE('',#31606,#31891,#23092,.T.);
#40183=EDGE_CURVE('',#31892,#31606,#18866,.T.);
#40184=EDGE_CURVE('',#31765,#31892,#23093,.T.);
#40185=EDGE_CURVE('',#31607,#31892,#23094,.T.);
#40186=EDGE_CURVE('',#31893,#31607,#18867,.T.);
#40187=EDGE_CURVE('',#31769,#31893,#23095,.T.);
#40188=EDGE_CURVE('',#31608,#31893,#23096,.T.);
#40189=EDGE_CURVE('',#31894,#31608,#18868,.T.);
#40190=EDGE_CURVE('',#31773,#31894,#23097,.T.);
#40191=EDGE_CURVE('',#31609,#31894,#23098,.T.);
#40192=EDGE_CURVE('',#31895,#31609,#18869,.T.);
#40193=EDGE_CURVE('',#31777,#31895,#23099,.T.);
#40194=EDGE_CURVE('',#31610,#31895,#23100,.T.);
#40195=EDGE_CURVE('',#31896,#31610,#18870,.T.);
#40196=EDGE_CURVE('',#31781,#31896,#23101,.T.);
#40197=EDGE_CURVE('',#31611,#31896,#23102,.T.);
#40198=EDGE_CURVE('',#31897,#31611,#18871,.T.);
#40199=EDGE_CURVE('',#31785,#31897,#23103,.T.);
#40200=EDGE_CURVE('',#31612,#31897,#4443,.T.);
#40201=EDGE_CURVE('',#31898,#31612,#18872,.T.);
#40202=EDGE_CURVE('',#31789,#31898,#23104,.T.);
#40203=EDGE_CURVE('',#31613,#31898,#4444,.T.);
#40204=EDGE_CURVE('',#31899,#31613,#18873,.T.);
#40205=EDGE_CURVE('',#31793,#31899,#23105,.T.);
#40206=EDGE_CURVE('',#31614,#31899,#23106,.T.);
#40207=EDGE_CURVE('',#31900,#31614,#18874,.T.);
#40208=EDGE_CURVE('',#31797,#31900,#23107,.T.);
#40209=EDGE_CURVE('',#31615,#31900,#23108,.T.);
#40210=EDGE_CURVE('',#31901,#31615,#18875,.T.);
#40211=EDGE_CURVE('',#31801,#31901,#23109,.T.);
#40212=EDGE_CURVE('',#31616,#31901,#23110,.T.);
#40213=EDGE_CURVE('',#31902,#31616,#18876,.T.);
#40214=EDGE_CURVE('',#31805,#31902,#23111,.T.);
#40215=EDGE_CURVE('',#31617,#31902,#4445,.T.);
#40216=EDGE_CURVE('',#31903,#31617,#18877,.T.);
#40217=EDGE_CURVE('',#31809,#31903,#23112,.T.);
#40218=EDGE_CURVE('',#31618,#31903,#23113,.T.);
#40219=EDGE_CURVE('',#31904,#31618,#18878,.T.);
#40220=EDGE_CURVE('',#31813,#31904,#23114,.T.);
#40221=EDGE_CURVE('',#31619,#31904,#4446,.T.);
#40222=EDGE_CURVE('',#31905,#31619,#18879,.T.);
#40223=EDGE_CURVE('',#31817,#31905,#23115,.T.);
#40224=EDGE_CURVE('',#31620,#31905,#23116,.T.);
#40225=EDGE_CURVE('',#31906,#31620,#18880,.T.);
#40226=EDGE_CURVE('',#31821,#31906,#23117,.T.);
#40227=EDGE_CURVE('',#31621,#31906,#23118,.T.);
#40228=EDGE_CURVE('',#31907,#31621,#18881,.T.);
#40229=EDGE_CURVE('',#31825,#31907,#23119,.T.);
#40230=EDGE_CURVE('',#31622,#31907,#23120,.T.);
#40231=EDGE_CURVE('',#31908,#31622,#18882,.T.);
#40232=EDGE_CURVE('',#31829,#31908,#23121,.T.);
#40233=EDGE_CURVE('',#31623,#31908,#23122,.T.);
#40234=EDGE_CURVE('',#31909,#31623,#18883,.T.);
#40235=EDGE_CURVE('',#31833,#31909,#23123,.T.);
#40236=EDGE_CURVE('',#31624,#31909,#23124,.T.);
#40237=EDGE_CURVE('',#31910,#31624,#18884,.T.);
#40238=EDGE_CURVE('',#31837,#31910,#23125,.T.);
#40239=EDGE_CURVE('',#31625,#31910,#4447,.T.);
#40240=EDGE_CURVE('',#31911,#31625,#18885,.T.);
#40241=EDGE_CURVE('',#31841,#31911,#23126,.T.);
#40242=EDGE_CURVE('',#31626,#31911,#4448,.T.);
#40243=EDGE_CURVE('',#31912,#31626,#18886,.T.);
#40244=EDGE_CURVE('',#31845,#31912,#23127,.T.);
#40245=EDGE_CURVE('',#31627,#31912,#23128,.T.);
#40246=EDGE_CURVE('',#31913,#31627,#18887,.T.);
#40247=EDGE_CURVE('',#31849,#31913,#23129,.T.);
#40248=EDGE_CURVE('',#31628,#31913,#4449,.T.);
#40249=EDGE_CURVE('',#31914,#31628,#18888,.T.);
#40250=EDGE_CURVE('',#31853,#31914,#23130,.T.);
#40251=EDGE_CURVE('',#31629,#31914,#23131,.T.);
#40252=EDGE_CURVE('',#31915,#31629,#18889,.T.);
#40253=EDGE_CURVE('',#31857,#31915,#23132,.T.);
#40254=EDGE_CURVE('',#31601,#31915,#23133,.T.);
#40255=EDGE_CURVE('',#31916,#31917,#18890,.T.);
#40256=EDGE_CURVE('',#31858,#31917,#25524,.T.);
#40257=EDGE_CURVE('',#31916,#31572,#23134,.T.);
#40258=EDGE_CURVE('',#31918,#31919,#23135,.T.);
#40259=EDGE_CURVE('',#31573,#31919,#23136,.T.);
#40260=EDGE_CURVE('',#31918,#31858,#25525,.T.);
#40261=EDGE_CURVE('',#31920,#31918,#18891,.T.);
#40262=EDGE_CURVE('',#31921,#31920,#18892,.T.);
#40263=EDGE_CURVE('',#31919,#31921,#18893,.T.);
#40264=EDGE_CURVE('',#31859,#31921,#25526,.T.);
#40265=EDGE_CURVE('',#31922,#31923,#23137,.T.);
#40266=EDGE_CURVE('',#31574,#31923,#23138,.T.);
#40267=EDGE_CURVE('',#31922,#31859,#25527,.T.);
#40268=EDGE_CURVE('',#31924,#31922,#18894,.T.);
#40269=EDGE_CURVE('',#31925,#31924,#18895,.T.);
#40270=EDGE_CURVE('',#31923,#31925,#18896,.T.);
#40271=EDGE_CURVE('',#31860,#31925,#25528,.T.);
#40272=EDGE_CURVE('',#31926,#31927,#23139,.T.);
#40273=EDGE_CURVE('',#31575,#31927,#23140,.T.);
#40274=EDGE_CURVE('',#31926,#31860,#25529,.T.);
#40275=EDGE_CURVE('',#31928,#31926,#18897,.T.);
#40276=EDGE_CURVE('',#31929,#31928,#18898,.T.);
#40277=EDGE_CURVE('',#31927,#31929,#18899,.T.);
#40278=EDGE_CURVE('',#31861,#31929,#25530,.T.);
#40279=EDGE_CURVE('',#31930,#31931,#23141,.T.);
#40280=EDGE_CURVE('',#31576,#31931,#23142,.T.);
#40281=EDGE_CURVE('',#31930,#31861,#25531,.T.);
#40282=EDGE_CURVE('',#31932,#31930,#18900,.T.);
#40283=EDGE_CURVE('',#31933,#31932,#18901,.T.);
#40284=EDGE_CURVE('',#31931,#31933,#18902,.T.);
#40285=EDGE_CURVE('',#31862,#31933,#25532,.T.);
#40286=EDGE_CURVE('',#31934,#31935,#23143,.T.);
#40287=EDGE_CURVE('',#31577,#31935,#23144,.T.);
#40288=EDGE_CURVE('',#31934,#31862,#25533,.T.);
#40289=EDGE_CURVE('',#31936,#31934,#18903,.T.);
#40290=EDGE_CURVE('',#31937,#31936,#18904,.T.);
#40291=EDGE_CURVE('',#31935,#31937,#18905,.T.);
#40292=EDGE_CURVE('',#31863,#31937,#25534,.T.);
#40293=EDGE_CURVE('',#31938,#31939,#23145,.T.);
#40294=EDGE_CURVE('',#31578,#31939,#23146,.T.);
#40295=EDGE_CURVE('',#31938,#31863,#25535,.T.);
#40296=EDGE_CURVE('',#31940,#31938,#18906,.T.);
#40297=EDGE_CURVE('',#31941,#31940,#18907,.T.);
#40298=EDGE_CURVE('',#31939,#31941,#18908,.T.);
#40299=EDGE_CURVE('',#31864,#31941,#25536,.T.);
#40300=EDGE_CURVE('',#31579,#28954,#23147,.T.);
#40301=EDGE_CURVE('',#28956,#31864,#25537,.T.);
#40302=EDGE_CURVE('',#31865,#28955,#25538,.T.);
#40303=EDGE_CURVE('',#31942,#31943,#23148,.T.);
#40304=EDGE_CURVE('',#31580,#31943,#23149,.T.);
#40305=EDGE_CURVE('',#31942,#31865,#25539,.T.);
#40306=EDGE_CURVE('',#31944,#31942,#18909,.T.);
#40307=EDGE_CURVE('',#31945,#31944,#18910,.T.);
#40308=EDGE_CURVE('',#31943,#31945,#18911,.T.);
#40309=EDGE_CURVE('',#31866,#31945,#25540,.T.);
#40310=EDGE_CURVE('',#31946,#31947,#23150,.T.);
#40311=EDGE_CURVE('',#31581,#31947,#23151,.T.);
#40312=EDGE_CURVE('',#31946,#31866,#25541,.T.);
#40313=EDGE_CURVE('',#31948,#31946,#18912,.T.);
#40314=EDGE_CURVE('',#31949,#31948,#18913,.T.);
#40315=EDGE_CURVE('',#31947,#31949,#18914,.T.);
#40316=EDGE_CURVE('',#31867,#31949,#25542,.T.);
#40317=EDGE_CURVE('',#31950,#31951,#23152,.T.);
#40318=EDGE_CURVE('',#31582,#31951,#23153,.T.);
#40319=EDGE_CURVE('',#31950,#31867,#25543,.T.);
#40320=EDGE_CURVE('',#31952,#31950,#18915,.T.);
#40321=EDGE_CURVE('',#31953,#31952,#18916,.T.);
#40322=EDGE_CURVE('',#31951,#31953,#18917,.T.);
#40323=EDGE_CURVE('',#31868,#31953,#25544,.T.);
#40324=EDGE_CURVE('',#31954,#31955,#23154,.T.);
#40325=EDGE_CURVE('',#31583,#31955,#23155,.T.);
#40326=EDGE_CURVE('',#31954,#31868,#25545,.T.);
#40327=EDGE_CURVE('',#31956,#31954,#18918,.T.);
#40328=EDGE_CURVE('',#31957,#31956,#18919,.T.);
#40329=EDGE_CURVE('',#31955,#31957,#18920,.T.);
#40330=EDGE_CURVE('',#31869,#31957,#25546,.T.);
#40331=EDGE_CURVE('',#31958,#31959,#23156,.T.);
#40332=EDGE_CURVE('',#31584,#31959,#23157,.T.);
#40333=EDGE_CURVE('',#31958,#31869,#25547,.T.);
#40334=EDGE_CURVE('',#31960,#31958,#18921,.T.);
#40335=EDGE_CURVE('',#31961,#31960,#18922,.T.);
#40336=EDGE_CURVE('',#31959,#31961,#18923,.T.);
#40337=EDGE_CURVE('',#31870,#31961,#25548,.T.);
#40338=EDGE_CURVE('',#31962,#31963,#23158,.T.);
#40339=EDGE_CURVE('',#31585,#31963,#23159,.T.);
#40340=EDGE_CURVE('',#31962,#31870,#25549,.T.);
#40341=EDGE_CURVE('',#31964,#31962,#18924,.T.);
#40342=EDGE_CURVE('',#31965,#31964,#18925,.T.);
#40343=EDGE_CURVE('',#31963,#31965,#18926,.T.);
#40344=EDGE_CURVE('',#31871,#31965,#25550,.T.);
#40345=EDGE_CURVE('',#31966,#31967,#23160,.T.);
#40346=EDGE_CURVE('',#31586,#31967,#23161,.T.);
#40347=EDGE_CURVE('',#31966,#31871,#25551,.T.);
#40348=EDGE_CURVE('',#31968,#31966,#18927,.T.);
#40349=EDGE_CURVE('',#31969,#31968,#18928,.T.);
#40350=EDGE_CURVE('',#31967,#31969,#18929,.T.);
#40351=EDGE_CURVE('',#31872,#31969,#25552,.T.);
#40352=EDGE_CURVE('',#31970,#31971,#23162,.T.);
#40353=EDGE_CURVE('',#31587,#31971,#23163,.T.);
#40354=EDGE_CURVE('',#31970,#31872,#25553,.T.);
#40355=EDGE_CURVE('',#31972,#31970,#18930,.T.);
#40356=EDGE_CURVE('',#31973,#31972,#18931,.T.);
#40357=EDGE_CURVE('',#31971,#31973,#18932,.T.);
#40358=EDGE_CURVE('',#31873,#31973,#25554,.T.);
#40359=EDGE_CURVE('',#31974,#31975,#23164,.T.);
#40360=EDGE_CURVE('',#31588,#31975,#23165,.T.);
#40361=EDGE_CURVE('',#31974,#31873,#25555,.T.);
#40362=EDGE_CURVE('',#31976,#31974,#18933,.T.);
#40363=EDGE_CURVE('',#31977,#31976,#18934,.T.);
#40364=EDGE_CURVE('',#31975,#31977,#18935,.T.);
#40365=EDGE_CURVE('',#31874,#31977,#25556,.T.);
#40366=EDGE_CURVE('',#31978,#31979,#23166,.T.);
#40367=EDGE_CURVE('',#31589,#31979,#23167,.T.);
#40368=EDGE_CURVE('',#31978,#31874,#25557,.T.);
#40369=EDGE_CURVE('',#31980,#31978,#18936,.T.);
#40370=EDGE_CURVE('',#31981,#31980,#18937,.T.);
#40371=EDGE_CURVE('',#31979,#31981,#18938,.T.);
#40372=EDGE_CURVE('',#31875,#31981,#25558,.T.);
#40373=EDGE_CURVE('',#31982,#31983,#23168,.T.);
#40374=EDGE_CURVE('',#31590,#31983,#23169,.T.);
#40375=EDGE_CURVE('',#31982,#31875,#25559,.T.);
#40376=EDGE_CURVE('',#31984,#31982,#18939,.T.);
#40377=EDGE_CURVE('',#31985,#31984,#18940,.T.);
#40378=EDGE_CURVE('',#31983,#31985,#18941,.T.);
#40379=EDGE_CURVE('',#31876,#31985,#25560,.T.);
#40380=EDGE_CURVE('',#31986,#31987,#23170,.T.);
#40381=EDGE_CURVE('',#31591,#31987,#23171,.T.);
#40382=EDGE_CURVE('',#31986,#31876,#25561,.T.);
#40383=EDGE_CURVE('',#31988,#31986,#18942,.T.);
#40384=EDGE_CURVE('',#31989,#31988,#18943,.T.);
#40385=EDGE_CURVE('',#31987,#31989,#18944,.T.);
#40386=EDGE_CURVE('',#31877,#31989,#25562,.T.);
#40387=EDGE_CURVE('',#31990,#31991,#23172,.T.);
#40388=EDGE_CURVE('',#31592,#31991,#23173,.T.);
#40389=EDGE_CURVE('',#31990,#31877,#25563,.T.);
#40390=EDGE_CURVE('',#31991,#31992,#18945,.T.);
#40391=EDGE_CURVE('',#31878,#31992,#25564,.T.);
#40392=EDGE_CURVE('',#31993,#31990,#18946,.T.);
#40393=EDGE_CURVE('',#31992,#31993,#18947,.T.);
#40394=EDGE_CURVE('',#31994,#31878,#25565,.T.);
#40395=EDGE_CURVE('',#31994,#31995,#23174,.T.);
#40396=EDGE_CURVE('',#31593,#31995,#23175,.T.);
#40397=EDGE_CURVE('',#31995,#31996,#18948,.T.);
#40398=EDGE_CURVE('',#31997,#31994,#18949,.T.);
#40399=EDGE_CURVE('',#31996,#31997,#18950,.T.);
#40400=EDGE_CURVE('',#31879,#31996,#25566,.T.);
#40401=EDGE_CURVE('',#31998,#31999,#23176,.T.);
#40402=EDGE_CURVE('',#31594,#31999,#23177,.T.);
#40403=EDGE_CURVE('',#31998,#31879,#25567,.T.);
#40404=EDGE_CURVE('',#32000,#31998,#18951,.T.);
#40405=EDGE_CURVE('',#32001,#32000,#18952,.T.);
#40406=EDGE_CURVE('',#31999,#32001,#18953,.T.);
#40407=EDGE_CURVE('',#31880,#32001,#25568,.T.);
#40408=EDGE_CURVE('',#32002,#32003,#23178,.T.);
#40409=EDGE_CURVE('',#31595,#32003,#23179,.T.);
#40410=EDGE_CURVE('',#32002,#31880,#25569,.T.);
#40411=EDGE_CURVE('',#32004,#32002,#18954,.T.);
#40412=EDGE_CURVE('',#32005,#32004,#18955,.T.);
#40413=EDGE_CURVE('',#32003,#32005,#18956,.T.);
#40414=EDGE_CURVE('',#31881,#32005,#25570,.T.);
#40415=EDGE_CURVE('',#32006,#32007,#23180,.T.);
#40416=EDGE_CURVE('',#31596,#32007,#23181,.T.);
#40417=EDGE_CURVE('',#32006,#31881,#25571,.T.);
#40418=EDGE_CURVE('',#32008,#32006,#18957,.T.);
#40419=EDGE_CURVE('',#32009,#32008,#18958,.T.);
#40420=EDGE_CURVE('',#32007,#32009,#18959,.T.);
#40421=EDGE_CURVE('',#31882,#32009,#25572,.T.);
#40422=EDGE_CURVE('',#32010,#32011,#23182,.T.);
#40423=EDGE_CURVE('',#31597,#32011,#23183,.T.);
#40424=EDGE_CURVE('',#32010,#31882,#25573,.T.);
#40425=EDGE_CURVE('',#32012,#32010,#18960,.T.);
#40426=EDGE_CURVE('',#32013,#32012,#18961,.T.);
#40427=EDGE_CURVE('',#32011,#32013,#18962,.T.);
#40428=EDGE_CURVE('',#31883,#32013,#25574,.T.);
#40429=EDGE_CURVE('',#32014,#32015,#23184,.T.);
#40430=EDGE_CURVE('',#31598,#32015,#23185,.T.);
#40431=EDGE_CURVE('',#32014,#31883,#25575,.T.);
#40432=EDGE_CURVE('',#32016,#32014,#18963,.T.);
#40433=EDGE_CURVE('',#32017,#32016,#18964,.T.);
#40434=EDGE_CURVE('',#32015,#32017,#18965,.T.);
#40435=EDGE_CURVE('',#31884,#32017,#25576,.T.);
#40436=EDGE_CURVE('',#32018,#32019,#23186,.T.);
#40437=EDGE_CURVE('',#31599,#32019,#23187,.T.);
#40438=EDGE_CURVE('',#32018,#31884,#25577,.T.);
#40439=EDGE_CURVE('',#32020,#32018,#18966,.T.);
#40440=EDGE_CURVE('',#32021,#32020,#18967,.T.);
#40441=EDGE_CURVE('',#32019,#32021,#18968,.T.);
#40442=EDGE_CURVE('',#31885,#32021,#25578,.T.);
#40443=EDGE_CURVE('',#32022,#32023,#23188,.T.);
#40444=EDGE_CURVE('',#31600,#32023,#23189,.T.);
#40445=EDGE_CURVE('',#32022,#31885,#25579,.T.);
#40446=EDGE_CURVE('',#32024,#32022,#18969,.T.);
#40447=EDGE_CURVE('',#32025,#32024,#18970,.T.);
#40448=EDGE_CURVE('',#32023,#32025,#18971,.T.);
#40449=EDGE_CURVE('',#31886,#32025,#25580,.T.);
#40450=EDGE_CURVE('',#32026,#32027,#18972,.T.);
#40451=EDGE_CURVE('',#31917,#32026,#18973,.T.);
#40452=EDGE_CURVE('',#32027,#31916,#23190,.T.);
#40453=EDGE_CURVE('',#32027,#31886,#25581,.T.);
#40454=EDGE_CURVE('',#32028,#31601,#23191,.T.);
#40455=EDGE_CURVE('',#32028,#32029,#18974,.T.);
#40456=EDGE_CURVE('',#31887,#32029,#25582,.T.);
#40457=EDGE_CURVE('',#32030,#31887,#25583,.T.);
#40458=EDGE_CURVE('',#32030,#32031,#23192,.T.);
#40459=EDGE_CURVE('',#31602,#32031,#23193,.T.);
#40460=EDGE_CURVE('',#32031,#32032,#18975,.T.);
#40461=EDGE_CURVE('',#31888,#32032,#25584,.T.);
#40462=EDGE_CURVE('',#32033,#32030,#18976,.T.);
#40463=EDGE_CURVE('',#32032,#32033,#18977,.T.);
#40464=EDGE_CURVE('',#32034,#31888,#25585,.T.);
#40465=EDGE_CURVE('',#32034,#32035,#23194,.T.);
#40466=EDGE_CURVE('',#31603,#32035,#23195,.T.);
#40467=EDGE_CURVE('',#32035,#32036,#18978,.T.);
#40468=EDGE_CURVE('',#31889,#32036,#25586,.T.);
#40469=EDGE_CURVE('',#32037,#32034,#18979,.T.);
#40470=EDGE_CURVE('',#32036,#32037,#18980,.T.);
#40471=EDGE_CURVE('',#32038,#31889,#25587,.T.);
#40472=EDGE_CURVE('',#32038,#32039,#23196,.T.);
#40473=EDGE_CURVE('',#31604,#32039,#23197,.T.);
#40474=EDGE_CURVE('',#32039,#32040,#18981,.T.);
#40475=EDGE_CURVE('',#31890,#32040,#25588,.T.);
#40476=EDGE_CURVE('',#32041,#32038,#18982,.T.);
#40477=EDGE_CURVE('',#32040,#32041,#18983,.T.);
#40478=EDGE_CURVE('',#32042,#31890,#25589,.T.);
#40479=EDGE_CURVE('',#32042,#32043,#23198,.T.);
#40480=EDGE_CURVE('',#31605,#32043,#23199,.T.);
#40481=EDGE_CURVE('',#32043,#32044,#18984,.T.);
#40482=EDGE_CURVE('',#31891,#32044,#25590,.T.);
#40483=EDGE_CURVE('',#32045,#32042,#18985,.T.);
#40484=EDGE_CURVE('',#32044,#32045,#18986,.T.);
#40485=EDGE_CURVE('',#32046,#31891,#25591,.T.);
#40486=EDGE_CURVE('',#32046,#32047,#23200,.T.);
#40487=EDGE_CURVE('',#31606,#32047,#23201,.T.);
#40488=EDGE_CURVE('',#32047,#32048,#18987,.T.);
#40489=EDGE_CURVE('',#31892,#32048,#25592,.T.);
#40490=EDGE_CURVE('',#32049,#32046,#18988,.T.);
#40491=EDGE_CURVE('',#32048,#32049,#18989,.T.);
#40492=EDGE_CURVE('',#32050,#31892,#25593,.T.);
#40493=EDGE_CURVE('',#32050,#32051,#23202,.T.);
#40494=EDGE_CURVE('',#31607,#32051,#23203,.T.);
#40495=EDGE_CURVE('',#32051,#32052,#18990,.T.);
#40496=EDGE_CURVE('',#31893,#32052,#25594,.T.);
#40497=EDGE_CURVE('',#32053,#32050,#18991,.T.);
#40498=EDGE_CURVE('',#32052,#32053,#18992,.T.);
#40499=EDGE_CURVE('',#32054,#31893,#25595,.T.);
#40500=EDGE_CURVE('',#32054,#32055,#23204,.T.);
#40501=EDGE_CURVE('',#31608,#32055,#23205,.T.);
#40502=EDGE_CURVE('',#32055,#32056,#18993,.T.);
#40503=EDGE_CURVE('',#31894,#32056,#25596,.T.);
#40504=EDGE_CURVE('',#32057,#32054,#18994,.T.);
#40505=EDGE_CURVE('',#32056,#32057,#18995,.T.);
#40506=EDGE_CURVE('',#32058,#31894,#25597,.T.);
#40507=EDGE_CURVE('',#32058,#32059,#23206,.T.);
#40508=EDGE_CURVE('',#31609,#32059,#23207,.T.);
#40509=EDGE_CURVE('',#32059,#32060,#18996,.T.);
#40510=EDGE_CURVE('',#31895,#32060,#25598,.T.);
#40511=EDGE_CURVE('',#32061,#32058,#18997,.T.);
#40512=EDGE_CURVE('',#32060,#32061,#18998,.T.);
#40513=EDGE_CURVE('',#32062,#31895,#25599,.T.);
#40514=EDGE_CURVE('',#32062,#32063,#23208,.T.);
#40515=EDGE_CURVE('',#31610,#32063,#23209,.T.);
#40516=EDGE_CURVE('',#32063,#32064,#18999,.T.);
#40517=EDGE_CURVE('',#31896,#32064,#25600,.T.);
#40518=EDGE_CURVE('',#32065,#32062,#19000,.T.);
#40519=EDGE_CURVE('',#32064,#32065,#19001,.T.);
#40520=EDGE_CURVE('',#32066,#31896,#25601,.T.);
#40521=EDGE_CURVE('',#32066,#32067,#23210,.T.);
#40522=EDGE_CURVE('',#31611,#32067,#23211,.T.);
#40523=EDGE_CURVE('',#32067,#32068,#19002,.T.);
#40524=EDGE_CURVE('',#31897,#32068,#25602,.T.);
#40525=EDGE_CURVE('',#32069,#32066,#19003,.T.);
#40526=EDGE_CURVE('',#32068,#32069,#19004,.T.);
#40527=EDGE_CURVE('',#32070,#31897,#25603,.T.);
#40528=EDGE_CURVE('',#32070,#32071,#23212,.T.);
#40529=EDGE_CURVE('',#31612,#32071,#23213,.T.);
#40530=EDGE_CURVE('',#32071,#32072,#19005,.T.);
#40531=EDGE_CURVE('',#31898,#32072,#25604,.T.);
#40532=EDGE_CURVE('',#32073,#32070,#19006,.T.);
#40533=EDGE_CURVE('',#32072,#32073,#19007,.T.);
#40534=EDGE_CURVE('',#32074,#31898,#25605,.T.);
#40535=EDGE_CURVE('',#32074,#32075,#23214,.T.);
#40536=EDGE_CURVE('',#31613,#32075,#23215,.T.);
#40537=EDGE_CURVE('',#32075,#32076,#19008,.T.);
#40538=EDGE_CURVE('',#31899,#32076,#25606,.T.);
#40539=EDGE_CURVE('',#32077,#32074,#19009,.T.);
#40540=EDGE_CURVE('',#32076,#32077,#19010,.T.);
#40541=EDGE_CURVE('',#32078,#31899,#25607,.T.);
#40542=EDGE_CURVE('',#32078,#32079,#23216,.T.);
#40543=EDGE_CURVE('',#31614,#32079,#23217,.T.);
#40544=EDGE_CURVE('',#32079,#32080,#19011,.T.);
#40545=EDGE_CURVE('',#31900,#32080,#25608,.T.);
#40546=EDGE_CURVE('',#32081,#32078,#19012,.T.);
#40547=EDGE_CURVE('',#32080,#32081,#19013,.T.);
#40548=EDGE_CURVE('',#28953,#31900,#25609,.T.);
#40549=EDGE_CURVE('',#31615,#28952,#23218,.T.);
#40550=EDGE_CURVE('',#31901,#28950,#25610,.T.);
#40551=EDGE_CURVE('',#32082,#31901,#25611,.T.);
#40552=EDGE_CURVE('',#32082,#32083,#23219,.T.);
#40553=EDGE_CURVE('',#31616,#32083,#23220,.T.);
#40554=EDGE_CURVE('',#32083,#32084,#19014,.T.);
#40555=EDGE_CURVE('',#31902,#32084,#25612,.T.);
#40556=EDGE_CURVE('',#32085,#32082,#19015,.T.);
#40557=EDGE_CURVE('',#32084,#32085,#19016,.T.);
#40558=EDGE_CURVE('',#32086,#31902,#25613,.T.);
#40559=EDGE_CURVE('',#32086,#32087,#23221,.T.);
#40560=EDGE_CURVE('',#31617,#32087,#23222,.T.);
#40561=EDGE_CURVE('',#32087,#32088,#19017,.T.);
#40562=EDGE_CURVE('',#31903,#32088,#25614,.T.);
#40563=EDGE_CURVE('',#32089,#32086,#19018,.T.);
#40564=EDGE_CURVE('',#32088,#32089,#19019,.T.);
#40565=EDGE_CURVE('',#32090,#31903,#25615,.T.);
#40566=EDGE_CURVE('',#32090,#32091,#23223,.T.);
#40567=EDGE_CURVE('',#31618,#32091,#23224,.T.);
#40568=EDGE_CURVE('',#32091,#32092,#19020,.T.);
#40569=EDGE_CURVE('',#31904,#32092,#25616,.T.);
#40570=EDGE_CURVE('',#32093,#32090,#19021,.T.);
#40571=EDGE_CURVE('',#32092,#32093,#19022,.T.);
#40572=EDGE_CURVE('',#32094,#31904,#25617,.T.);
#40573=EDGE_CURVE('',#32094,#32095,#23225,.T.);
#40574=EDGE_CURVE('',#31619,#32095,#23226,.T.);
#40575=EDGE_CURVE('',#32095,#32096,#19023,.T.);
#40576=EDGE_CURVE('',#31905,#32096,#25618,.T.);
#40577=EDGE_CURVE('',#32097,#32094,#19024,.T.);
#40578=EDGE_CURVE('',#32096,#32097,#19025,.T.);
#40579=EDGE_CURVE('',#32098,#31905,#25619,.T.);
#40580=EDGE_CURVE('',#32098,#32099,#23227,.T.);
#40581=EDGE_CURVE('',#31620,#32099,#23228,.T.);
#40582=EDGE_CURVE('',#32099,#32100,#19026,.T.);
#40583=EDGE_CURVE('',#31906,#32100,#25620,.T.);
#40584=EDGE_CURVE('',#32101,#32098,#19027,.T.);
#40585=EDGE_CURVE('',#32100,#32101,#19028,.T.);
#40586=EDGE_CURVE('',#32102,#31906,#25621,.T.);
#40587=EDGE_CURVE('',#32102,#32103,#23229,.T.);
#40588=EDGE_CURVE('',#31621,#32103,#23230,.T.);
#40589=EDGE_CURVE('',#32103,#32104,#19029,.T.);
#40590=EDGE_CURVE('',#31907,#32104,#25622,.T.);
#40591=EDGE_CURVE('',#32105,#32102,#19030,.T.);
#40592=EDGE_CURVE('',#32104,#32105,#19031,.T.);
#40593=EDGE_CURVE('',#32106,#31907,#25623,.T.);
#40594=EDGE_CURVE('',#32106,#32107,#23231,.T.);
#40595=EDGE_CURVE('',#31622,#32107,#23232,.T.);
#40596=EDGE_CURVE('',#32107,#32108,#19032,.T.);
#40597=EDGE_CURVE('',#31908,#32108,#25624,.T.);
#40598=EDGE_CURVE('',#32109,#32106,#19033,.T.);
#40599=EDGE_CURVE('',#32108,#32109,#19034,.T.);
#40600=EDGE_CURVE('',#32110,#31908,#25625,.T.);
#40601=EDGE_CURVE('',#32110,#32111,#23233,.T.);
#40602=EDGE_CURVE('',#31623,#32111,#23234,.T.);
#40603=EDGE_CURVE('',#32111,#32112,#19035,.T.);
#40604=EDGE_CURVE('',#31909,#32112,#25626,.T.);
#40605=EDGE_CURVE('',#32113,#32110,#19036,.T.);
#40606=EDGE_CURVE('',#32112,#32113,#19037,.T.);
#40607=EDGE_CURVE('',#32114,#31909,#25627,.T.);
#40608=EDGE_CURVE('',#32114,#32115,#23235,.T.);
#40609=EDGE_CURVE('',#31624,#32115,#23236,.T.);
#40610=EDGE_CURVE('',#32115,#32116,#19038,.T.);
#40611=EDGE_CURVE('',#31910,#32116,#25628,.T.);
#40612=EDGE_CURVE('',#32117,#32114,#19039,.T.);
#40613=EDGE_CURVE('',#32116,#32117,#19040,.T.);
#40614=EDGE_CURVE('',#32118,#31910,#25629,.T.);
#40615=EDGE_CURVE('',#32118,#32119,#23237,.T.);
#40616=EDGE_CURVE('',#31625,#32119,#23238,.T.);
#40617=EDGE_CURVE('',#32119,#32120,#19041,.T.);
#40618=EDGE_CURVE('',#31911,#32120,#25630,.T.);
#40619=EDGE_CURVE('',#32121,#32118,#19042,.T.);
#40620=EDGE_CURVE('',#32120,#32121,#19043,.T.);
#40621=EDGE_CURVE('',#32122,#31911,#25631,.T.);
#40622=EDGE_CURVE('',#32122,#32123,#23239,.T.);
#40623=EDGE_CURVE('',#31626,#32123,#23240,.T.);
#40624=EDGE_CURVE('',#32123,#32124,#19044,.T.);
#40625=EDGE_CURVE('',#31912,#32124,#25632,.T.);
#40626=EDGE_CURVE('',#32125,#32122,#19045,.T.);
#40627=EDGE_CURVE('',#32124,#32125,#19046,.T.);
#40628=EDGE_CURVE('',#32126,#31912,#25633,.T.);
#40629=EDGE_CURVE('',#32126,#32127,#23241,.T.);
#40630=EDGE_CURVE('',#31627,#32127,#23242,.T.);
#40631=EDGE_CURVE('',#32127,#32128,#19047,.T.);
#40632=EDGE_CURVE('',#31913,#32128,#25634,.T.);
#40633=EDGE_CURVE('',#32129,#32126,#19048,.T.);
#40634=EDGE_CURVE('',#32128,#32129,#19049,.T.);
#40635=EDGE_CURVE('',#32130,#31913,#25635,.T.);
#40636=EDGE_CURVE('',#32130,#32131,#23243,.T.);
#40637=EDGE_CURVE('',#31628,#32131,#23244,.T.);
#40638=EDGE_CURVE('',#32131,#32132,#19050,.T.);
#40639=EDGE_CURVE('',#31914,#32132,#25636,.T.);
#40640=EDGE_CURVE('',#32133,#32130,#19051,.T.);
#40641=EDGE_CURVE('',#32132,#32133,#19052,.T.);
#40642=EDGE_CURVE('',#32134,#31914,#25637,.T.);
#40643=EDGE_CURVE('',#32134,#32135,#23245,.T.);
#40644=EDGE_CURVE('',#31629,#32135,#23246,.T.);
#40645=EDGE_CURVE('',#32135,#32136,#19053,.T.);
#40646=EDGE_CURVE('',#31915,#32136,#25638,.T.);
#40647=EDGE_CURVE('',#32137,#32134,#19054,.T.);
#40648=EDGE_CURVE('',#32136,#32137,#19055,.T.);
#40649=EDGE_CURVE('',#32138,#32028,#23247,.T.);
#40650=EDGE_CURVE('',#32139,#32138,#19056,.T.);
#40651=EDGE_CURVE('',#32029,#32139,#19057,.T.);
#40652=EDGE_CURVE('',#32138,#31915,#25639,.T.);
#40653=EDGE_CURVE('',#31858,#32140,#19058,.T.);
#40654=EDGE_CURVE('',#32140,#32026,#23248,.T.);
#40655=EDGE_CURVE('',#32141,#31858,#19059,.T.);
#40656=EDGE_CURVE('',#31920,#32141,#23249,.T.);
#40657=EDGE_CURVE('',#31859,#32141,#19060,.T.);
#40658=EDGE_CURVE('',#32142,#31859,#19061,.T.);
#40659=EDGE_CURVE('',#31924,#32142,#23250,.T.);
#40660=EDGE_CURVE('',#31860,#32142,#19062,.T.);
#40661=EDGE_CURVE('',#32143,#31860,#19063,.T.);
#40662=EDGE_CURVE('',#31928,#32143,#23251,.T.);
#40663=EDGE_CURVE('',#31861,#32143,#19064,.T.);
#40664=EDGE_CURVE('',#32144,#31861,#19065,.T.);
#40665=EDGE_CURVE('',#31932,#32144,#23252,.T.);
#40666=EDGE_CURVE('',#31862,#32144,#19066,.T.);
#40667=EDGE_CURVE('',#32145,#31862,#19067,.T.);
#40668=EDGE_CURVE('',#31936,#32145,#23253,.T.);
#40669=EDGE_CURVE('',#31863,#32145,#19068,.T.);
#40670=EDGE_CURVE('',#32146,#31863,#19069,.T.);
#40671=EDGE_CURVE('',#31940,#32146,#23254,.T.);
#40672=EDGE_CURVE('',#31864,#32146,#19070,.T.);
#40673=EDGE_CURVE('',#32147,#31864,#19071,.T.);
#40674=EDGE_CURVE('',#28957,#32147,#23255,.T.);
#40675=EDGE_CURVE('',#31865,#32147,#19072,.T.);
#40676=EDGE_CURVE('',#32148,#31865,#19073,.T.);
#40677=EDGE_CURVE('',#31944,#32148,#23256,.T.);
#40678=EDGE_CURVE('',#31866,#32148,#19074,.T.);
#40679=EDGE_CURVE('',#32149,#31866,#19075,.T.);
#40680=EDGE_CURVE('',#31948,#32149,#23257,.T.);
#40681=EDGE_CURVE('',#31867,#32149,#19076,.T.);
#40682=EDGE_CURVE('',#32150,#31867,#19077,.T.);
#40683=EDGE_CURVE('',#31952,#32150,#23258,.T.);
#40684=EDGE_CURVE('',#31868,#32150,#19078,.T.);
#40685=EDGE_CURVE('',#32151,#31868,#19079,.T.);
#40686=EDGE_CURVE('',#31956,#32151,#23259,.T.);
#40687=EDGE_CURVE('',#31869,#32151,#19080,.T.);
#40688=EDGE_CURVE('',#32152,#31869,#19081,.T.);
#40689=EDGE_CURVE('',#31960,#32152,#23260,.T.);
#40690=EDGE_CURVE('',#31870,#32152,#19082,.T.);
#40691=EDGE_CURVE('',#32153,#31870,#19083,.T.);
#40692=EDGE_CURVE('',#31964,#32153,#23261,.T.);
#40693=EDGE_CURVE('',#31871,#32153,#19084,.T.);
#40694=EDGE_CURVE('',#32154,#31871,#19085,.T.);
#40695=EDGE_CURVE('',#31968,#32154,#23262,.T.);
#40696=EDGE_CURVE('',#31872,#32154,#19086,.T.);
#40697=EDGE_CURVE('',#32155,#31872,#19087,.T.);
#40698=EDGE_CURVE('',#31972,#32155,#23263,.T.);
#40699=EDGE_CURVE('',#31873,#32155,#19088,.T.);
#40700=EDGE_CURVE('',#32156,#31873,#19089,.T.);
#40701=EDGE_CURVE('',#31976,#32156,#23264,.T.);
#40702=EDGE_CURVE('',#31874,#32156,#19090,.T.);
#40703=EDGE_CURVE('',#32157,#31874,#19091,.T.);
#40704=EDGE_CURVE('',#31980,#32157,#23265,.T.);
#40705=EDGE_CURVE('',#31875,#32157,#19092,.T.);
#40706=EDGE_CURVE('',#32158,#31875,#19093,.T.);
#40707=EDGE_CURVE('',#31984,#32158,#23266,.T.);
#40708=EDGE_CURVE('',#31876,#32158,#19094,.T.);
#40709=EDGE_CURVE('',#32159,#31876,#19095,.T.);
#40710=EDGE_CURVE('',#31988,#32159,#23267,.T.);
#40711=EDGE_CURVE('',#31877,#32159,#19096,.T.);
#40712=EDGE_CURVE('',#32160,#31877,#19097,.T.);
#40713=EDGE_CURVE('',#31993,#32160,#23268,.T.);
#40714=EDGE_CURVE('',#31878,#32160,#19098,.T.);
#40715=EDGE_CURVE('',#32161,#31878,#19099,.T.);
#40716=EDGE_CURVE('',#31997,#32161,#23269,.T.);
#40717=EDGE_CURVE('',#31879,#32161,#19100,.T.);
#40718=EDGE_CURVE('',#32162,#31879,#19101,.T.);
#40719=EDGE_CURVE('',#32000,#32162,#23270,.T.);
#40720=EDGE_CURVE('',#31880,#32162,#19102,.T.);
#40721=EDGE_CURVE('',#32163,#31880,#19103,.T.);
#40722=EDGE_CURVE('',#32004,#32163,#23271,.T.);
#40723=EDGE_CURVE('',#31881,#32163,#19104,.T.);
#40724=EDGE_CURVE('',#32164,#31881,#19105,.T.);
#40725=EDGE_CURVE('',#32008,#32164,#23272,.T.);
#40726=EDGE_CURVE('',#31882,#32164,#19106,.T.);
#40727=EDGE_CURVE('',#32165,#31882,#19107,.T.);
#40728=EDGE_CURVE('',#32012,#32165,#23273,.T.);
#40729=EDGE_CURVE('',#31883,#32165,#19108,.T.);
#40730=EDGE_CURVE('',#32166,#31883,#19109,.T.);
#40731=EDGE_CURVE('',#32016,#32166,#23274,.T.);
#40732=EDGE_CURVE('',#31884,#32166,#19110,.T.);
#40733=EDGE_CURVE('',#32167,#31884,#19111,.T.);
#40734=EDGE_CURVE('',#32020,#32167,#23275,.T.);
#40735=EDGE_CURVE('',#31885,#32167,#19112,.T.);
#40736=EDGE_CURVE('',#32168,#31885,#19113,.T.);
#40737=EDGE_CURVE('',#32024,#32168,#23276,.T.);
#40738=EDGE_CURVE('',#31886,#32168,#19114,.T.);
#40739=EDGE_CURVE('',#32140,#31886,#19115,.T.);
#40740=EDGE_CURVE('',#32169,#32139,#23277,.T.);
#40741=EDGE_CURVE('',#31887,#32169,#19116,.T.);
#40742=EDGE_CURVE('',#32170,#31887,#19117,.T.);
#40743=EDGE_CURVE('',#32033,#32170,#23278,.T.);
#40744=EDGE_CURVE('',#31888,#32170,#19118,.T.);
#40745=EDGE_CURVE('',#32171,#31888,#19119,.T.);
#40746=EDGE_CURVE('',#32037,#32171,#23279,.T.);
#40747=EDGE_CURVE('',#31889,#32171,#19120,.T.);
#40748=EDGE_CURVE('',#32172,#31889,#19121,.T.);
#40749=EDGE_CURVE('',#32041,#32172,#23280,.T.);
#40750=EDGE_CURVE('',#31890,#32172,#19122,.T.);
#40751=EDGE_CURVE('',#32173,#31890,#19123,.T.);
#40752=EDGE_CURVE('',#32045,#32173,#23281,.T.);
#40753=EDGE_CURVE('',#31891,#32173,#19124,.T.);
#40754=EDGE_CURVE('',#32174,#31891,#19125,.T.);
#40755=EDGE_CURVE('',#32049,#32174,#23282,.T.);
#40756=EDGE_CURVE('',#31892,#32174,#19126,.T.);
#40757=EDGE_CURVE('',#32175,#31892,#19127,.T.);
#40758=EDGE_CURVE('',#32053,#32175,#23283,.T.);
#40759=EDGE_CURVE('',#31893,#32175,#19128,.T.);
#40760=EDGE_CURVE('',#32176,#31893,#19129,.T.);
#40761=EDGE_CURVE('',#32057,#32176,#23284,.T.);
#40762=EDGE_CURVE('',#31894,#32176,#19130,.T.);
#40763=EDGE_CURVE('',#32177,#31894,#19131,.T.);
#40764=EDGE_CURVE('',#32061,#32177,#23285,.T.);
#40765=EDGE_CURVE('',#31895,#32177,#19132,.T.);
#40766=EDGE_CURVE('',#32178,#31895,#19133,.T.);
#40767=EDGE_CURVE('',#32065,#32178,#23286,.T.);
#40768=EDGE_CURVE('',#31896,#32178,#19134,.T.);
#40769=EDGE_CURVE('',#32179,#31896,#19135,.T.);
#40770=EDGE_CURVE('',#32069,#32179,#23287,.T.);
#40771=EDGE_CURVE('',#31897,#32179,#19136,.T.);
#40772=EDGE_CURVE('',#32180,#31897,#19137,.T.);
#40773=EDGE_CURVE('',#32073,#32180,#23288,.T.);
#40774=EDGE_CURVE('',#31898,#32180,#19138,.T.);
#40775=EDGE_CURVE('',#32181,#31898,#19139,.T.);
#40776=EDGE_CURVE('',#32077,#32181,#23289,.T.);
#40777=EDGE_CURVE('',#31899,#32181,#19140,.T.);
#40778=EDGE_CURVE('',#32182,#31899,#19141,.T.);
#40779=EDGE_CURVE('',#32081,#32182,#23290,.T.);
#40780=EDGE_CURVE('',#31900,#32182,#19142,.T.);
#40781=EDGE_CURVE('',#32183,#31900,#19143,.T.);
#40782=EDGE_CURVE('',#28951,#32183,#23291,.T.);
#40783=EDGE_CURVE('',#31901,#32183,#19144,.T.);
#40784=EDGE_CURVE('',#32184,#31901,#19145,.T.);
#40785=EDGE_CURVE('',#32085,#32184,#23292,.T.);
#40786=EDGE_CURVE('',#31902,#32184,#19146,.T.);
#40787=EDGE_CURVE('',#32185,#31902,#19147,.T.);
#40788=EDGE_CURVE('',#32089,#32185,#23293,.T.);
#40789=EDGE_CURVE('',#31903,#32185,#19148,.T.);
#40790=EDGE_CURVE('',#32186,#31903,#19149,.T.);
#40791=EDGE_CURVE('',#32093,#32186,#23294,.T.);
#40792=EDGE_CURVE('',#31904,#32186,#19150,.T.);
#40793=EDGE_CURVE('',#32187,#31904,#19151,.T.);
#40794=EDGE_CURVE('',#32097,#32187,#23295,.T.);
#40795=EDGE_CURVE('',#31905,#32187,#19152,.T.);
#40796=EDGE_CURVE('',#32188,#31905,#19153,.T.);
#40797=EDGE_CURVE('',#32101,#32188,#23296,.T.);
#40798=EDGE_CURVE('',#31906,#32188,#19154,.T.);
#40799=EDGE_CURVE('',#32189,#31906,#19155,.T.);
#40800=EDGE_CURVE('',#32105,#32189,#23297,.T.);
#40801=EDGE_CURVE('',#31907,#32189,#19156,.T.);
#40802=EDGE_CURVE('',#32190,#31907,#19157,.T.);
#40803=EDGE_CURVE('',#32109,#32190,#23298,.T.);
#40804=EDGE_CURVE('',#31908,#32190,#19158,.T.);
#40805=EDGE_CURVE('',#32191,#31908,#19159,.T.);
#40806=EDGE_CURVE('',#32113,#32191,#23299,.T.);
#40807=EDGE_CURVE('',#31909,#32191,#19160,.T.);
#40808=EDGE_CURVE('',#32192,#31909,#19161,.T.);
#40809=EDGE_CURVE('',#32117,#32192,#23300,.T.);
#40810=EDGE_CURVE('',#31910,#32192,#19162,.T.);
#40811=EDGE_CURVE('',#32193,#31910,#19163,.T.);
#40812=EDGE_CURVE('',#32121,#32193,#23301,.T.);
#40813=EDGE_CURVE('',#31911,#32193,#19164,.T.);
#40814=EDGE_CURVE('',#32194,#31911,#19165,.T.);
#40815=EDGE_CURVE('',#32125,#32194,#23302,.T.);
#40816=EDGE_CURVE('',#31912,#32194,#19166,.T.);
#40817=EDGE_CURVE('',#32195,#31912,#19167,.T.);
#40818=EDGE_CURVE('',#32129,#32195,#23303,.T.);
#40819=EDGE_CURVE('',#31913,#32195,#19168,.T.);
#40820=EDGE_CURVE('',#32196,#31913,#19169,.T.);
#40821=EDGE_CURVE('',#32133,#32196,#23304,.T.);
#40822=EDGE_CURVE('',#31914,#32196,#19170,.T.);
#40823=EDGE_CURVE('',#32197,#31914,#19171,.T.);
#40824=EDGE_CURVE('',#32137,#32197,#23305,.T.);
#40825=EDGE_CURVE('',#31915,#32197,#19172,.T.);
#40826=EDGE_CURVE('',#32169,#31915,#19173,.T.);
#40827=EDGE_CURVE('',#32198,#32199,#19174,.T.);
#40828=EDGE_CURVE('',#31858,#32199,#23306,.T.);
#40829=EDGE_CURVE('',#32198,#32140,#25640,.T.);
#40830=EDGE_CURVE('',#32200,#32198,#19175,.T.);
#40831=EDGE_CURVE('',#32201,#32200,#19176,.T.);
#40832=EDGE_CURVE('',#32199,#32201,#19177,.T.);
#40833=EDGE_CURVE('',#32141,#32201,#25641,.T.);
#40834=EDGE_CURVE('',#32202,#32203,#19178,.T.);
#40835=EDGE_CURVE('',#31859,#32203,#23307,.T.);
#40836=EDGE_CURVE('',#32202,#32141,#25642,.T.);
#40837=EDGE_CURVE('',#32204,#32202,#19179,.T.);
#40838=EDGE_CURVE('',#32205,#32204,#19180,.T.);
#40839=EDGE_CURVE('',#32203,#32205,#19181,.T.);
#40840=EDGE_CURVE('',#32142,#32205,#25643,.T.);
#40841=EDGE_CURVE('',#32206,#32207,#19182,.T.);
#40842=EDGE_CURVE('',#31860,#32207,#23308,.T.);
#40843=EDGE_CURVE('',#32206,#32142,#25644,.T.);
#40844=EDGE_CURVE('',#32208,#32206,#19183,.T.);
#40845=EDGE_CURVE('',#32209,#32208,#19184,.T.);
#40846=EDGE_CURVE('',#32207,#32209,#19185,.T.);
#40847=EDGE_CURVE('',#32143,#32209,#25645,.T.);
#40848=EDGE_CURVE('',#32210,#32211,#19186,.T.);
#40849=EDGE_CURVE('',#31861,#32211,#23309,.T.);
#40850=EDGE_CURVE('',#32210,#32143,#25646,.T.);
#40851=EDGE_CURVE('',#32212,#32210,#19187,.T.);
#40852=EDGE_CURVE('',#32213,#32212,#19188,.T.);
#40853=EDGE_CURVE('',#32211,#32213,#19189,.T.);
#40854=EDGE_CURVE('',#32144,#32213,#25647,.T.);
#40855=EDGE_CURVE('',#32214,#32215,#19190,.T.);
#40856=EDGE_CURVE('',#31862,#32215,#23310,.T.);
#40857=EDGE_CURVE('',#32214,#32144,#25648,.T.);
#40858=EDGE_CURVE('',#32216,#32214,#19191,.T.);
#40859=EDGE_CURVE('',#32217,#32216,#19192,.T.);
#40860=EDGE_CURVE('',#32215,#32217,#19193,.T.);
#40861=EDGE_CURVE('',#32145,#32217,#25649,.T.);
#40862=EDGE_CURVE('',#32218,#32219,#19194,.T.);
#40863=EDGE_CURVE('',#31863,#32219,#23311,.T.);
#40864=EDGE_CURVE('',#32218,#32145,#25650,.T.);
#40865=EDGE_CURVE('',#32220,#32218,#19195,.T.);
#40866=EDGE_CURVE('',#32221,#32220,#19196,.T.);
#40867=EDGE_CURVE('',#32219,#32221,#19197,.T.);
#40868=EDGE_CURVE('',#32146,#32221,#25651,.T.);
#40869=EDGE_CURVE('',#32222,#32223,#19198,.T.);
#40870=EDGE_CURVE('',#31864,#32223,#23312,.T.);
#40871=EDGE_CURVE('',#32222,#32146,#25652,.T.);
#40872=EDGE_CURVE('',#32224,#32222,#19199,.T.);
#40873=EDGE_CURVE('',#32225,#32224,#19200,.T.);
#40874=EDGE_CURVE('',#32223,#32225,#19201,.T.);
#40875=EDGE_CURVE('',#32147,#32225,#25653,.T.);
#40876=EDGE_CURVE('',#32226,#32227,#19202,.T.);
#40877=EDGE_CURVE('',#31865,#32227,#23313,.T.);
#40878=EDGE_CURVE('',#32226,#32147,#25654,.T.);
#40879=EDGE_CURVE('',#32228,#32226,#19203,.T.);
#40880=EDGE_CURVE('',#32229,#32228,#19204,.T.);
#40881=EDGE_CURVE('',#32227,#32229,#19205,.T.);
#40882=EDGE_CURVE('',#32148,#32229,#25655,.T.);
#40883=EDGE_CURVE('',#32230,#32231,#19206,.T.);
#40884=EDGE_CURVE('',#31866,#32231,#23314,.T.);
#40885=EDGE_CURVE('',#32230,#32148,#25656,.T.);
#40886=EDGE_CURVE('',#32232,#32230,#19207,.T.);
#40887=EDGE_CURVE('',#32233,#32232,#19208,.T.);
#40888=EDGE_CURVE('',#32231,#32233,#19209,.T.);
#40889=EDGE_CURVE('',#32149,#32233,#25657,.T.);
#40890=EDGE_CURVE('',#32234,#32235,#19210,.T.);
#40891=EDGE_CURVE('',#31867,#32235,#23315,.T.);
#40892=EDGE_CURVE('',#32234,#32149,#25658,.T.);
#40893=EDGE_CURVE('',#32236,#32234,#19211,.T.);
#40894=EDGE_CURVE('',#32237,#32236,#19212,.T.);
#40895=EDGE_CURVE('',#32235,#32237,#19213,.T.);
#40896=EDGE_CURVE('',#32150,#32237,#25659,.T.);
#40897=EDGE_CURVE('',#32238,#32239,#19214,.T.);
#40898=EDGE_CURVE('',#31868,#32239,#23316,.T.);
#40899=EDGE_CURVE('',#32238,#32150,#25660,.T.);
#40900=EDGE_CURVE('',#32240,#32238,#19215,.T.);
#40901=EDGE_CURVE('',#32241,#32240,#19216,.T.);
#40902=EDGE_CURVE('',#32239,#32241,#19217,.T.);
#40903=EDGE_CURVE('',#32151,#32241,#25661,.T.);
#40904=EDGE_CURVE('',#32242,#32243,#19218,.T.);
#40905=EDGE_CURVE('',#31869,#32243,#23317,.T.);
#40906=EDGE_CURVE('',#32242,#32151,#25662,.T.);
#40907=EDGE_CURVE('',#32244,#32242,#19219,.T.);
#40908=EDGE_CURVE('',#32245,#32244,#19220,.T.);
#40909=EDGE_CURVE('',#32243,#32245,#19221,.T.);
#40910=EDGE_CURVE('',#32152,#32245,#25663,.T.);
#40911=EDGE_CURVE('',#32246,#32247,#19222,.T.);
#40912=EDGE_CURVE('',#31870,#32247,#23318,.T.);
#40913=EDGE_CURVE('',#32246,#32152,#25664,.T.);
#40914=EDGE_CURVE('',#32248,#32246,#19223,.T.);
#40915=EDGE_CURVE('',#32249,#32248,#19224,.T.);
#40916=EDGE_CURVE('',#32247,#32249,#19225,.T.);
#40917=EDGE_CURVE('',#32153,#32249,#25665,.T.);
#40918=EDGE_CURVE('',#32250,#32251,#19226,.T.);
#40919=EDGE_CURVE('',#31871,#32251,#23319,.T.);
#40920=EDGE_CURVE('',#32250,#32153,#25666,.T.);
#40921=EDGE_CURVE('',#32252,#32250,#19227,.T.);
#40922=EDGE_CURVE('',#32253,#32252,#19228,.T.);
#40923=EDGE_CURVE('',#32251,#32253,#19229,.T.);
#40924=EDGE_CURVE('',#32154,#32253,#25667,.T.);
#40925=EDGE_CURVE('',#31872,#28947,#23320,.T.);
#40926=EDGE_CURVE('',#28946,#32154,#25668,.T.);
#40927=EDGE_CURVE('',#32155,#28949,#25669,.T.);
#40928=EDGE_CURVE('',#32254,#32255,#19230,.T.);
#40929=EDGE_CURVE('',#31873,#32255,#23321,.T.);
#40930=EDGE_CURVE('',#32254,#32155,#25670,.T.);
#40931=EDGE_CURVE('',#32256,#32254,#19231,.T.);
#40932=EDGE_CURVE('',#32257,#32256,#19232,.T.);
#40933=EDGE_CURVE('',#32255,#32257,#19233,.T.);
#40934=EDGE_CURVE('',#32156,#32257,#25671,.T.);
#40935=EDGE_CURVE('',#32258,#32259,#19234,.T.);
#40936=EDGE_CURVE('',#31874,#32259,#23322,.T.);
#40937=EDGE_CURVE('',#32258,#32156,#25672,.T.);
#40938=EDGE_CURVE('',#32260,#32258,#19235,.T.);
#40939=EDGE_CURVE('',#32261,#32260,#19236,.T.);
#40940=EDGE_CURVE('',#32259,#32261,#19237,.T.);
#40941=EDGE_CURVE('',#32157,#32261,#25673,.T.);
#40942=EDGE_CURVE('',#32262,#32263,#19238,.T.);
#40943=EDGE_CURVE('',#31875,#32263,#23323,.T.);
#40944=EDGE_CURVE('',#32262,#32157,#25674,.T.);
#40945=EDGE_CURVE('',#32264,#32262,#19239,.T.);
#40946=EDGE_CURVE('',#32265,#32264,#19240,.T.);
#40947=EDGE_CURVE('',#32263,#32265,#19241,.T.);
#40948=EDGE_CURVE('',#32158,#32265,#25675,.T.);
#40949=EDGE_CURVE('',#32266,#32267,#19242,.T.);
#40950=EDGE_CURVE('',#31876,#32267,#23324,.T.);
#40951=EDGE_CURVE('',#32266,#32158,#25676,.T.);
#40952=EDGE_CURVE('',#32268,#32266,#19243,.T.);
#40953=EDGE_CURVE('',#32269,#32268,#19244,.T.);
#40954=EDGE_CURVE('',#32267,#32269,#19245,.T.);
#40955=EDGE_CURVE('',#32159,#32269,#25677,.T.);
#40956=EDGE_CURVE('',#32270,#32271,#19246,.T.);
#40957=EDGE_CURVE('',#31877,#32271,#23325,.T.);
#40958=EDGE_CURVE('',#32270,#32159,#25678,.T.);
#40959=EDGE_CURVE('',#32271,#32272,#19247,.T.);
#40960=EDGE_CURVE('',#32160,#32272,#25679,.T.);
#40961=EDGE_CURVE('',#32273,#32270,#19248,.T.);
#40962=EDGE_CURVE('',#32272,#32273,#19249,.T.);
#40963=EDGE_CURVE('',#32274,#32160,#25680,.T.);
#40964=EDGE_CURVE('',#32274,#32275,#19250,.T.);
#40965=EDGE_CURVE('',#31878,#32275,#23326,.T.);
#40966=EDGE_CURVE('',#32275,#32276,#19251,.T.);
#40967=EDGE_CURVE('',#32277,#32274,#19252,.T.);
#40968=EDGE_CURVE('',#32276,#32277,#19253,.T.);
#40969=EDGE_CURVE('',#32161,#32276,#25681,.T.);
#40970=EDGE_CURVE('',#32278,#32279,#19254,.T.);
#40971=EDGE_CURVE('',#31879,#32279,#23327,.T.);
#40972=EDGE_CURVE('',#32278,#32161,#25682,.T.);
#40973=EDGE_CURVE('',#32280,#32278,#19255,.T.);
#40974=EDGE_CURVE('',#32281,#32280,#19256,.T.);
#40975=EDGE_CURVE('',#32279,#32281,#19257,.T.);
#40976=EDGE_CURVE('',#32162,#32281,#25683,.T.);
#40977=EDGE_CURVE('',#32282,#32283,#19258,.T.);
#40978=EDGE_CURVE('',#31880,#32283,#23328,.T.);
#40979=EDGE_CURVE('',#32282,#32162,#25684,.T.);
#40980=EDGE_CURVE('',#32284,#32282,#19259,.T.);
#40981=EDGE_CURVE('',#32285,#32284,#19260,.T.);
#40982=EDGE_CURVE('',#32283,#32285,#19261,.T.);
#40983=EDGE_CURVE('',#32163,#32285,#25685,.T.);
#40984=EDGE_CURVE('',#32286,#32287,#19262,.T.);
#40985=EDGE_CURVE('',#31881,#32287,#23329,.T.);
#40986=EDGE_CURVE('',#32286,#32163,#25686,.T.);
#40987=EDGE_CURVE('',#32288,#32286,#19263,.T.);
#40988=EDGE_CURVE('',#32289,#32288,#19264,.T.);
#40989=EDGE_CURVE('',#32287,#32289,#19265,.T.);
#40990=EDGE_CURVE('',#32164,#32289,#25687,.T.);
#40991=EDGE_CURVE('',#32290,#32291,#19266,.T.);
#40992=EDGE_CURVE('',#31882,#32291,#23330,.T.);
#40993=EDGE_CURVE('',#32290,#32164,#25688,.T.);
#40994=EDGE_CURVE('',#32292,#32290,#19267,.T.);
#40995=EDGE_CURVE('',#32293,#32292,#19268,.T.);
#40996=EDGE_CURVE('',#32291,#32293,#19269,.T.);
#40997=EDGE_CURVE('',#32165,#32293,#25689,.T.);
#40998=EDGE_CURVE('',#32294,#32295,#19270,.T.);
#40999=EDGE_CURVE('',#31883,#32295,#23331,.T.);
#41000=EDGE_CURVE('',#32294,#32165,#25690,.T.);
#41001=EDGE_CURVE('',#32296,#32294,#19271,.T.);
#41002=EDGE_CURVE('',#32297,#32296,#19272,.T.);
#41003=EDGE_CURVE('',#32295,#32297,#19273,.T.);
#41004=EDGE_CURVE('',#32166,#32297,#25691,.T.);
#41005=EDGE_CURVE('',#32298,#32299,#19274,.T.);
#41006=EDGE_CURVE('',#31884,#32299,#23332,.T.);
#41007=EDGE_CURVE('',#32298,#32166,#25692,.T.);
#41008=EDGE_CURVE('',#32300,#32298,#19275,.T.);
#41009=EDGE_CURVE('',#32301,#32300,#19276,.T.);
#41010=EDGE_CURVE('',#32299,#32301,#19277,.T.);
#41011=EDGE_CURVE('',#32167,#32301,#25693,.T.);
#41012=EDGE_CURVE('',#32302,#32303,#19278,.T.);
#41013=EDGE_CURVE('',#31885,#32303,#23333,.T.);
#41014=EDGE_CURVE('',#32302,#32167,#25694,.T.);
#41015=EDGE_CURVE('',#32304,#32302,#19279,.T.);
#41016=EDGE_CURVE('',#32305,#32304,#19280,.T.);
#41017=EDGE_CURVE('',#32303,#32305,#19281,.T.);
#41018=EDGE_CURVE('',#32168,#32305,#25695,.T.);
#41019=EDGE_CURVE('',#32306,#32307,#19282,.T.);
#41020=EDGE_CURVE('',#31886,#32307,#23334,.T.);
#41021=EDGE_CURVE('',#32306,#32168,#25696,.T.);
#41022=EDGE_CURVE('',#32308,#32306,#19283,.T.);
#41023=EDGE_CURVE('',#32309,#32308,#19284,.T.);
#41024=EDGE_CURVE('',#32307,#32309,#19285,.T.);
#41025=EDGE_CURVE('',#32140,#32309,#25697,.T.);
#41026=EDGE_CURVE('',#32310,#32169,#25698,.T.);
#41027=EDGE_CURVE('',#32310,#32311,#19286,.T.);
#41028=EDGE_CURVE('',#31887,#32311,#23335,.T.);
#41029=EDGE_CURVE('',#32311,#32312,#19287,.T.);
#41030=EDGE_CURVE('',#32170,#32312,#25699,.T.);
#41031=EDGE_CURVE('',#32313,#32310,#19288,.T.);
#41032=EDGE_CURVE('',#32312,#32313,#19289,.T.);
#41033=EDGE_CURVE('',#32314,#32170,#25700,.T.);
#41034=EDGE_CURVE('',#32314,#32315,#19290,.T.);
#41035=EDGE_CURVE('',#31888,#32315,#23336,.T.);
#41036=EDGE_CURVE('',#32315,#32316,#19291,.T.);
#41037=EDGE_CURVE('',#32171,#32316,#25701,.T.);
#41038=EDGE_CURVE('',#32317,#32314,#19292,.T.);
#41039=EDGE_CURVE('',#32316,#32317,#19293,.T.);
#41040=EDGE_CURVE('',#32318,#32171,#25702,.T.);
#41041=EDGE_CURVE('',#32318,#32319,#19294,.T.);
#41042=EDGE_CURVE('',#31889,#32319,#23337,.T.);
#41043=EDGE_CURVE('',#32319,#32320,#19295,.T.);
#41044=EDGE_CURVE('',#32172,#32320,#25703,.T.);
#41045=EDGE_CURVE('',#32321,#32318,#19296,.T.);
#41046=EDGE_CURVE('',#32320,#32321,#19297,.T.);
#41047=EDGE_CURVE('',#32322,#32172,#25704,.T.);
#41048=EDGE_CURVE('',#32322,#32323,#19298,.T.);
#41049=EDGE_CURVE('',#31890,#32323,#23338,.T.);
#41050=EDGE_CURVE('',#32323,#32324,#19299,.T.);
#41051=EDGE_CURVE('',#32173,#32324,#25705,.T.);
#41052=EDGE_CURVE('',#32325,#32322,#19300,.T.);
#41053=EDGE_CURVE('',#32324,#32325,#19301,.T.);
#41054=EDGE_CURVE('',#32326,#32173,#25706,.T.);
#41055=EDGE_CURVE('',#32326,#32327,#19302,.T.);
#41056=EDGE_CURVE('',#31891,#32327,#23339,.T.);
#41057=EDGE_CURVE('',#32327,#32328,#19303,.T.);
#41058=EDGE_CURVE('',#32174,#32328,#25707,.T.);
#41059=EDGE_CURVE('',#32329,#32326,#19304,.T.);
#41060=EDGE_CURVE('',#32328,#32329,#19305,.T.);
#41061=EDGE_CURVE('',#32330,#32174,#25708,.T.);
#41062=EDGE_CURVE('',#32330,#32331,#19306,.T.);
#41063=EDGE_CURVE('',#31892,#32331,#23340,.T.);
#41064=EDGE_CURVE('',#32331,#32332,#19307,.T.);
#41065=EDGE_CURVE('',#32175,#32332,#25709,.T.);
#41066=EDGE_CURVE('',#32333,#32330,#19308,.T.);
#41067=EDGE_CURVE('',#32332,#32333,#19309,.T.);
#41068=EDGE_CURVE('',#32334,#32175,#25710,.T.);
#41069=EDGE_CURVE('',#32334,#32335,#19310,.T.);
#41070=EDGE_CURVE('',#31893,#32335,#23341,.T.);
#41071=EDGE_CURVE('',#32335,#32336,#19311,.T.);
#41072=EDGE_CURVE('',#32176,#32336,#25711,.T.);
#41073=EDGE_CURVE('',#32337,#32334,#19312,.T.);
#41074=EDGE_CURVE('',#32336,#32337,#19313,.T.);
#41075=EDGE_CURVE('',#32338,#32176,#25712,.T.);
#41076=EDGE_CURVE('',#32338,#32339,#19314,.T.);
#41077=EDGE_CURVE('',#31894,#32339,#23342,.T.);
#41078=EDGE_CURVE('',#32339,#32340,#19315,.T.);
#41079=EDGE_CURVE('',#32177,#32340,#25713,.T.);
#41080=EDGE_CURVE('',#32341,#32338,#19316,.T.);
#41081=EDGE_CURVE('',#32340,#32341,#19317,.T.);
#41082=EDGE_CURVE('',#32342,#32177,#25714,.T.);
#41083=EDGE_CURVE('',#32342,#32343,#19318,.T.);
#41084=EDGE_CURVE('',#31895,#32343,#23343,.T.);
#41085=EDGE_CURVE('',#32343,#32344,#19319,.T.);
#41086=EDGE_CURVE('',#32178,#32344,#25715,.T.);
#41087=EDGE_CURVE('',#32345,#32342,#19320,.T.);
#41088=EDGE_CURVE('',#32344,#32345,#19321,.T.);
#41089=EDGE_CURVE('',#32346,#32178,#25716,.T.);
#41090=EDGE_CURVE('',#32346,#32347,#19322,.T.);
#41091=EDGE_CURVE('',#31896,#32347,#23344,.T.);
#41092=EDGE_CURVE('',#32347,#32348,#19323,.T.);
#41093=EDGE_CURVE('',#32179,#32348,#25717,.T.);
#41094=EDGE_CURVE('',#32349,#32346,#19324,.T.);
#41095=EDGE_CURVE('',#32348,#32349,#19325,.T.);
#41096=EDGE_CURVE('',#32350,#32179,#25718,.T.);
#41097=EDGE_CURVE('',#32350,#32351,#19326,.T.);
#41098=EDGE_CURVE('',#31897,#32351,#23345,.T.);
#41099=EDGE_CURVE('',#32351,#32352,#19327,.T.);
#41100=EDGE_CURVE('',#32180,#32352,#25719,.T.);
#41101=EDGE_CURVE('',#32353,#32350,#19328,.T.);
#41102=EDGE_CURVE('',#32352,#32353,#19329,.T.);
#41103=EDGE_CURVE('',#32354,#32180,#25720,.T.);
#41104=EDGE_CURVE('',#32354,#32355,#19330,.T.);
#41105=EDGE_CURVE('',#31898,#32355,#23346,.T.);
#41106=EDGE_CURVE('',#32355,#32356,#19331,.T.);
#41107=EDGE_CURVE('',#32181,#32356,#25721,.T.);
#41108=EDGE_CURVE('',#32357,#32354,#19332,.T.);
#41109=EDGE_CURVE('',#32356,#32357,#19333,.T.);
#41110=EDGE_CURVE('',#32358,#32181,#25722,.T.);
#41111=EDGE_CURVE('',#32358,#32359,#19334,.T.);
#41112=EDGE_CURVE('',#31899,#32359,#23347,.T.);
#41113=EDGE_CURVE('',#32359,#32360,#19335,.T.);
#41114=EDGE_CURVE('',#32182,#32360,#25723,.T.);
#41115=EDGE_CURVE('',#32361,#32358,#19336,.T.);
#41116=EDGE_CURVE('',#32360,#32361,#19337,.T.);
#41117=EDGE_CURVE('',#32362,#32182,#25724,.T.);
#41118=EDGE_CURVE('',#32362,#32363,#19338,.T.);
#41119=EDGE_CURVE('',#31900,#32363,#23348,.T.);
#41120=EDGE_CURVE('',#32363,#32364,#19339,.T.);
#41121=EDGE_CURVE('',#32183,#32364,#25725,.T.);
#41122=EDGE_CURVE('',#32365,#32362,#19340,.T.);
#41123=EDGE_CURVE('',#32364,#32365,#19341,.T.);
#41124=EDGE_CURVE('',#32366,#32183,#25726,.T.);
#41125=EDGE_CURVE('',#32366,#32367,#19342,.T.);
#41126=EDGE_CURVE('',#31901,#32367,#23349,.T.);
#41127=EDGE_CURVE('',#32367,#32368,#19343,.T.);
#41128=EDGE_CURVE('',#32184,#32368,#25727,.T.);
#41129=EDGE_CURVE('',#32369,#32366,#19344,.T.);
#41130=EDGE_CURVE('',#32368,#32369,#19345,.T.);
#41131=EDGE_CURVE('',#32370,#32184,#25728,.T.);
#41132=EDGE_CURVE('',#32370,#32371,#19346,.T.);
#41133=EDGE_CURVE('',#31902,#32371,#23350,.T.);
#41134=EDGE_CURVE('',#32371,#32372,#19347,.T.);
#41135=EDGE_CURVE('',#32185,#32372,#25729,.T.);
#41136=EDGE_CURVE('',#32373,#32370,#19348,.T.);
#41137=EDGE_CURVE('',#32372,#32373,#19349,.T.);
#41138=EDGE_CURVE('',#32374,#32185,#25730,.T.);
#41139=EDGE_CURVE('',#32374,#32375,#19350,.T.);
#41140=EDGE_CURVE('',#31903,#32375,#23351,.T.);
#41141=EDGE_CURVE('',#32375,#32376,#19351,.T.);
#41142=EDGE_CURVE('',#32186,#32376,#25731,.T.);
#41143=EDGE_CURVE('',#32377,#32374,#19352,.T.);
#41144=EDGE_CURVE('',#32376,#32377,#19353,.T.);
#41145=EDGE_CURVE('',#32378,#32186,#25732,.T.);
#41146=EDGE_CURVE('',#32378,#32379,#19354,.T.);
#41147=EDGE_CURVE('',#31904,#32379,#23352,.T.);
#41148=EDGE_CURVE('',#32379,#32380,#19355,.T.);
#41149=EDGE_CURVE('',#32187,#32380,#25733,.T.);
#41150=EDGE_CURVE('',#32381,#32378,#19356,.T.);
#41151=EDGE_CURVE('',#32380,#32381,#19357,.T.);
#41152=EDGE_CURVE('',#32382,#32187,#25734,.T.);
#41153=EDGE_CURVE('',#32382,#32383,#19358,.T.);
#41154=EDGE_CURVE('',#31905,#32383,#23353,.T.);
#41155=EDGE_CURVE('',#32383,#32384,#19359,.T.);
#41156=EDGE_CURVE('',#32188,#32384,#25735,.T.);
#41157=EDGE_CURVE('',#32385,#32382,#19360,.T.);
#41158=EDGE_CURVE('',#32384,#32385,#19361,.T.);
#41159=EDGE_CURVE('',#32386,#32188,#25736,.T.);
#41160=EDGE_CURVE('',#32386,#32387,#19362,.T.);
#41161=EDGE_CURVE('',#31906,#32387,#23354,.T.);
#41162=EDGE_CURVE('',#32387,#32388,#19363,.T.);
#41163=EDGE_CURVE('',#32189,#32388,#25737,.T.);
#41164=EDGE_CURVE('',#32389,#32386,#19364,.T.);
#41165=EDGE_CURVE('',#32388,#32389,#19365,.T.);
#41166=EDGE_CURVE('',#32390,#32189,#25738,.T.);
#41167=EDGE_CURVE('',#32390,#32391,#19366,.T.);
#41168=EDGE_CURVE('',#31907,#32391,#23355,.T.);
#41169=EDGE_CURVE('',#32391,#32392,#19367,.T.);
#41170=EDGE_CURVE('',#32190,#32392,#25739,.T.);
#41171=EDGE_CURVE('',#32393,#32390,#19368,.T.);
#41172=EDGE_CURVE('',#32392,#32393,#19369,.T.);
#41173=EDGE_CURVE('',#28943,#32190,#25740,.T.);
#41174=EDGE_CURVE('',#31908,#28945,#23356,.T.);
#41175=EDGE_CURVE('',#32191,#28944,#25741,.T.);
#41176=EDGE_CURVE('',#32394,#32191,#25742,.T.);
#41177=EDGE_CURVE('',#32394,#32395,#19370,.T.);
#41178=EDGE_CURVE('',#31909,#32395,#23357,.T.);
#41179=EDGE_CURVE('',#32395,#32396,#19371,.T.);
#41180=EDGE_CURVE('',#32192,#32396,#25743,.T.);
#41181=EDGE_CURVE('',#32397,#32394,#19372,.T.);
#41182=EDGE_CURVE('',#32396,#32397,#19373,.T.);
#41183=EDGE_CURVE('',#32398,#32192,#25744,.T.);
#41184=EDGE_CURVE('',#32398,#32399,#19374,.T.);
#41185=EDGE_CURVE('',#31910,#32399,#23358,.T.);
#41186=EDGE_CURVE('',#32399,#32400,#19375,.T.);
#41187=EDGE_CURVE('',#32193,#32400,#25745,.T.);
#41188=EDGE_CURVE('',#32401,#32398,#19376,.T.);
#41189=EDGE_CURVE('',#32400,#32401,#19377,.T.);
#41190=EDGE_CURVE('',#32402,#32193,#25746,.T.);
#41191=EDGE_CURVE('',#32402,#32403,#19378,.T.);
#41192=EDGE_CURVE('',#31911,#32403,#23359,.T.);
#41193=EDGE_CURVE('',#32403,#32404,#19379,.T.);
#41194=EDGE_CURVE('',#32194,#32404,#25747,.T.);
#41195=EDGE_CURVE('',#32405,#32402,#19380,.T.);
#41196=EDGE_CURVE('',#32404,#32405,#19381,.T.);
#41197=EDGE_CURVE('',#32406,#32194,#25748,.T.);
#41198=EDGE_CURVE('',#32406,#32407,#19382,.T.);
#41199=EDGE_CURVE('',#31912,#32407,#23360,.T.);
#41200=EDGE_CURVE('',#32407,#32408,#19383,.T.);
#41201=EDGE_CURVE('',#32195,#32408,#25749,.T.);
#41202=EDGE_CURVE('',#32409,#32406,#19384,.T.);
#41203=EDGE_CURVE('',#32408,#32409,#19385,.T.);
#41204=EDGE_CURVE('',#32410,#32195,#25750,.T.);
#41205=EDGE_CURVE('',#32410,#32411,#19386,.T.);
#41206=EDGE_CURVE('',#31913,#32411,#23361,.T.);
#41207=EDGE_CURVE('',#32411,#32412,#19387,.T.);
#41208=EDGE_CURVE('',#32196,#32412,#25751,.T.);
#41209=EDGE_CURVE('',#32413,#32410,#19388,.T.);
#41210=EDGE_CURVE('',#32412,#32413,#19389,.T.);
#41211=EDGE_CURVE('',#32414,#32196,#25752,.T.);
#41212=EDGE_CURVE('',#32414,#32415,#19390,.T.);
#41213=EDGE_CURVE('',#31914,#32415,#23362,.T.);
#41214=EDGE_CURVE('',#32415,#32416,#19391,.T.);
#41215=EDGE_CURVE('',#32197,#32416,#25753,.T.);
#41216=EDGE_CURVE('',#32417,#32414,#19392,.T.);
#41217=EDGE_CURVE('',#32416,#32417,#19393,.T.);
#41218=EDGE_CURVE('',#32418,#32197,#25754,.T.);
#41219=EDGE_CURVE('',#32418,#32419,#19394,.T.);
#41220=EDGE_CURVE('',#31915,#32419,#23363,.T.);
#41221=EDGE_CURVE('',#32419,#32420,#19395,.T.);
#41222=EDGE_CURVE('',#32169,#32420,#25755,.T.);
#41223=EDGE_CURVE('',#32421,#32418,#19396,.T.);
#41224=EDGE_CURVE('',#32420,#32421,#19397,.T.);
#41225=EDGE_CURVE('',#32422,#32140,#19398,.T.);
#41226=EDGE_CURVE('',#32200,#32422,#23364,.T.);
#41227=EDGE_CURVE('',#32141,#32422,#19399,.T.);
#41228=EDGE_CURVE('',#32423,#32141,#19400,.T.);
#41229=EDGE_CURVE('',#32204,#32423,#23365,.T.);
#41230=EDGE_CURVE('',#32142,#32423,#19401,.T.);
#41231=EDGE_CURVE('',#32424,#32142,#19402,.T.);
#41232=EDGE_CURVE('',#32208,#32424,#23366,.T.);
#41233=EDGE_CURVE('',#32143,#32424,#19403,.T.);
#41234=EDGE_CURVE('',#32425,#32143,#19404,.T.);
#41235=EDGE_CURVE('',#32212,#32425,#23367,.T.);
#41236=EDGE_CURVE('',#32144,#32425,#19405,.T.);
#41237=EDGE_CURVE('',#32426,#32144,#19406,.T.);
#41238=EDGE_CURVE('',#32216,#32426,#23368,.T.);
#41239=EDGE_CURVE('',#32145,#32426,#19407,.T.);
#41240=EDGE_CURVE('',#32427,#32145,#19408,.T.);
#41241=EDGE_CURVE('',#32220,#32427,#23369,.T.);
#41242=EDGE_CURVE('',#32146,#32427,#19409,.T.);
#41243=EDGE_CURVE('',#32428,#32146,#19410,.T.);
#41244=EDGE_CURVE('',#32224,#32428,#23370,.T.);
#41245=EDGE_CURVE('',#32147,#32428,#19411,.T.);
#41246=EDGE_CURVE('',#32429,#32147,#19412,.T.);
#41247=EDGE_CURVE('',#32228,#32429,#23371,.T.);
#41248=EDGE_CURVE('',#32148,#32429,#19413,.T.);
#41249=EDGE_CURVE('',#32430,#32148,#19414,.T.);
#41250=EDGE_CURVE('',#32232,#32430,#23372,.T.);
#41251=EDGE_CURVE('',#32149,#32430,#19415,.T.);
#41252=EDGE_CURVE('',#32431,#32149,#19416,.T.);
#41253=EDGE_CURVE('',#32236,#32431,#23373,.T.);
#41254=EDGE_CURVE('',#32150,#32431,#19417,.T.);
#41255=EDGE_CURVE('',#32432,#32150,#19418,.T.);
#41256=EDGE_CURVE('',#32240,#32432,#23374,.T.);
#41257=EDGE_CURVE('',#32151,#32432,#19419,.T.);
#41258=EDGE_CURVE('',#32433,#32151,#19420,.T.);
#41259=EDGE_CURVE('',#32244,#32433,#23375,.T.);
#41260=EDGE_CURVE('',#32152,#32433,#19421,.T.);
#41261=EDGE_CURVE('',#32434,#32152,#19422,.T.);
#41262=EDGE_CURVE('',#32248,#32434,#23376,.T.);
#41263=EDGE_CURVE('',#32153,#32434,#19423,.T.);
#41264=EDGE_CURVE('',#32435,#32153,#19424,.T.);
#41265=EDGE_CURVE('',#32252,#32435,#23377,.T.);
#41266=EDGE_CURVE('',#32154,#32435,#19425,.T.);
#41267=EDGE_CURVE('',#32436,#32154,#19426,.T.);
#41268=EDGE_CURVE('',#28948,#32436,#23378,.T.);
#41269=EDGE_CURVE('',#32155,#32436,#19427,.T.);
#41270=EDGE_CURVE('',#32437,#32155,#19428,.T.);
#41271=EDGE_CURVE('',#32256,#32437,#23379,.T.);
#41272=EDGE_CURVE('',#32156,#32437,#19429,.T.);
#41273=EDGE_CURVE('',#32438,#32156,#19430,.T.);
#41274=EDGE_CURVE('',#32260,#32438,#23380,.T.);
#41275=EDGE_CURVE('',#32157,#32438,#19431,.T.);
#41276=EDGE_CURVE('',#32439,#32157,#19432,.T.);
#41277=EDGE_CURVE('',#32264,#32439,#23381,.T.);
#41278=EDGE_CURVE('',#32158,#32439,#19433,.T.);
#41279=EDGE_CURVE('',#32440,#32158,#19434,.T.);
#41280=EDGE_CURVE('',#32268,#32440,#23382,.T.);
#41281=EDGE_CURVE('',#32159,#32440,#19435,.T.);
#41282=EDGE_CURVE('',#32441,#32159,#19436,.T.);
#41283=EDGE_CURVE('',#32273,#32441,#23383,.T.);
#41284=EDGE_CURVE('',#32160,#32441,#19437,.T.);
#41285=EDGE_CURVE('',#32442,#32160,#19438,.T.);
#41286=EDGE_CURVE('',#32277,#32442,#23384,.T.);
#41287=EDGE_CURVE('',#32161,#32442,#19439,.T.);
#41288=EDGE_CURVE('',#32443,#32161,#19440,.T.);
#41289=EDGE_CURVE('',#32280,#32443,#23385,.T.);
#41290=EDGE_CURVE('',#32162,#32443,#19441,.T.);
#41291=EDGE_CURVE('',#32444,#32162,#19442,.T.);
#41292=EDGE_CURVE('',#32284,#32444,#23386,.T.);
#41293=EDGE_CURVE('',#32163,#32444,#19443,.T.);
#41294=EDGE_CURVE('',#32445,#32163,#19444,.T.);
#41295=EDGE_CURVE('',#32288,#32445,#23387,.T.);
#41296=EDGE_CURVE('',#32164,#32445,#19445,.T.);
#41297=EDGE_CURVE('',#32446,#32164,#19446,.T.);
#41298=EDGE_CURVE('',#32292,#32446,#23388,.T.);
#41299=EDGE_CURVE('',#32165,#32446,#19447,.T.);
#41300=EDGE_CURVE('',#32447,#32165,#19448,.T.);
#41301=EDGE_CURVE('',#32296,#32447,#23389,.T.);
#41302=EDGE_CURVE('',#32166,#32447,#19449,.T.);
#41303=EDGE_CURVE('',#32448,#32166,#19450,.T.);
#41304=EDGE_CURVE('',#32300,#32448,#23390,.T.);
#41305=EDGE_CURVE('',#32167,#32448,#19451,.T.);
#41306=EDGE_CURVE('',#32449,#32167,#19452,.T.);
#41307=EDGE_CURVE('',#32304,#32449,#23391,.T.);
#41308=EDGE_CURVE('',#32168,#32449,#19453,.T.);
#41309=EDGE_CURVE('',#32450,#32168,#19454,.T.);
#41310=EDGE_CURVE('',#32308,#32450,#23392,.T.);
#41311=EDGE_CURVE('',#32140,#32450,#19455,.T.);
#41312=EDGE_CURVE('',#32451,#32169,#19456,.T.);
#41313=EDGE_CURVE('',#32313,#32451,#23393,.T.);
#41314=EDGE_CURVE('',#32170,#32451,#19457,.T.);
#41315=EDGE_CURVE('',#32452,#32170,#19458,.T.);
#41316=EDGE_CURVE('',#32317,#32452,#23394,.T.);
#41317=EDGE_CURVE('',#32171,#32452,#19459,.T.);
#41318=EDGE_CURVE('',#32453,#32171,#19460,.T.);
#41319=EDGE_CURVE('',#32321,#32453,#23395,.T.);
#41320=EDGE_CURVE('',#32172,#32453,#19461,.T.);
#41321=EDGE_CURVE('',#32454,#32172,#19462,.T.);
#41322=EDGE_CURVE('',#32325,#32454,#23396,.T.);
#41323=EDGE_CURVE('',#32173,#32454,#19463,.T.);
#41324=EDGE_CURVE('',#32455,#32173,#19464,.T.);
#41325=EDGE_CURVE('',#32329,#32455,#23397,.T.);
#41326=EDGE_CURVE('',#32174,#32455,#19465,.T.);
#41327=EDGE_CURVE('',#32456,#32174,#19466,.T.);
#41328=EDGE_CURVE('',#32333,#32456,#23398,.T.);
#41329=EDGE_CURVE('',#32175,#32456,#19467,.T.);
#41330=EDGE_CURVE('',#32457,#32175,#19468,.T.);
#41331=EDGE_CURVE('',#32337,#32457,#23399,.T.);
#41332=EDGE_CURVE('',#32176,#32457,#19469,.T.);
#41333=EDGE_CURVE('',#32458,#32176,#19470,.T.);
#41334=EDGE_CURVE('',#32341,#32458,#23400,.T.);
#41335=EDGE_CURVE('',#32177,#32458,#19471,.T.);
#41336=EDGE_CURVE('',#32459,#32177,#19472,.T.);
#41337=EDGE_CURVE('',#32345,#32459,#23401,.T.);
#41338=EDGE_CURVE('',#32178,#32459,#19473,.T.);
#41339=EDGE_CURVE('',#32460,#32178,#19474,.T.);
#41340=EDGE_CURVE('',#32349,#32460,#23402,.T.);
#41341=EDGE_CURVE('',#32179,#32460,#19475,.T.);
#41342=EDGE_CURVE('',#32461,#32179,#19476,.T.);
#41343=EDGE_CURVE('',#32353,#32461,#23403,.T.);
#41344=EDGE_CURVE('',#32180,#32461,#19477,.T.);
#41345=EDGE_CURVE('',#32462,#32180,#19478,.T.);
#41346=EDGE_CURVE('',#32357,#32462,#23404,.T.);
#41347=EDGE_CURVE('',#32181,#32462,#19479,.T.);
#41348=EDGE_CURVE('',#32463,#32181,#19480,.T.);
#41349=EDGE_CURVE('',#32361,#32463,#23405,.T.);
#41350=EDGE_CURVE('',#32182,#32463,#19481,.T.);
#41351=EDGE_CURVE('',#32464,#32182,#19482,.T.);
#41352=EDGE_CURVE('',#32365,#32464,#23406,.T.);
#41353=EDGE_CURVE('',#32183,#32464,#19483,.T.);
#41354=EDGE_CURVE('',#32465,#32183,#19484,.T.);
#41355=EDGE_CURVE('',#32369,#32465,#23407,.T.);
#41356=EDGE_CURVE('',#32184,#32465,#19485,.T.);
#41357=EDGE_CURVE('',#32466,#32184,#19486,.T.);
#41358=EDGE_CURVE('',#32373,#32466,#23408,.T.);
#41359=EDGE_CURVE('',#32185,#32466,#19487,.T.);
#41360=EDGE_CURVE('',#32467,#32185,#19488,.T.);
#41361=EDGE_CURVE('',#32377,#32467,#23409,.T.);
#41362=EDGE_CURVE('',#32186,#32467,#19489,.T.);
#41363=EDGE_CURVE('',#32468,#32186,#19490,.T.);
#41364=EDGE_CURVE('',#32381,#32468,#23410,.T.);
#41365=EDGE_CURVE('',#32187,#32468,#19491,.T.);
#41366=EDGE_CURVE('',#32469,#32187,#19492,.T.);
#41367=EDGE_CURVE('',#32385,#32469,#23411,.T.);
#41368=EDGE_CURVE('',#32188,#32469,#19493,.T.);
#41369=EDGE_CURVE('',#32470,#32188,#19494,.T.);
#41370=EDGE_CURVE('',#32389,#32470,#23412,.T.);
#41371=EDGE_CURVE('',#32189,#32470,#19495,.T.);
#41372=EDGE_CURVE('',#32471,#32189,#19496,.T.);
#41373=EDGE_CURVE('',#32393,#32471,#23413,.T.);
#41374=EDGE_CURVE('',#32190,#32471,#19497,.T.);
#41375=EDGE_CURVE('',#32472,#32190,#19498,.T.);
#41376=EDGE_CURVE('',#28942,#32472,#23414,.T.);
#41377=EDGE_CURVE('',#32191,#32472,#19499,.T.);
#41378=EDGE_CURVE('',#32473,#32191,#19500,.T.);
#41379=EDGE_CURVE('',#32397,#32473,#23415,.T.);
#41380=EDGE_CURVE('',#32192,#32473,#19501,.T.);
#41381=EDGE_CURVE('',#32474,#32192,#19502,.T.);
#41382=EDGE_CURVE('',#32401,#32474,#23416,.T.);
#41383=EDGE_CURVE('',#32193,#32474,#19503,.T.);
#41384=EDGE_CURVE('',#32475,#32193,#19504,.T.);
#41385=EDGE_CURVE('',#32405,#32475,#23417,.T.);
#41386=EDGE_CURVE('',#32194,#32475,#19505,.T.);
#41387=EDGE_CURVE('',#32476,#32194,#19506,.T.);
#41388=EDGE_CURVE('',#32409,#32476,#23418,.T.);
#41389=EDGE_CURVE('',#32195,#32476,#19507,.T.);
#41390=EDGE_CURVE('',#32477,#32195,#19508,.T.);
#41391=EDGE_CURVE('',#32413,#32477,#23419,.T.);
#41392=EDGE_CURVE('',#32196,#32477,#19509,.T.);
#41393=EDGE_CURVE('',#32478,#32196,#19510,.T.);
#41394=EDGE_CURVE('',#32417,#32478,#23420,.T.);
#41395=EDGE_CURVE('',#32197,#32478,#19511,.T.);
#41396=EDGE_CURVE('',#32479,#32197,#19512,.T.);
#41397=EDGE_CURVE('',#32421,#32479,#23421,.T.);
#41398=EDGE_CURVE('',#32169,#32479,#19513,.T.);
#41399=EDGE_CURVE('',#32480,#32481,#19514,.T.);
#41400=EDGE_CURVE('',#32422,#32481,#25756,.T.);
#41401=EDGE_CURVE('',#32480,#32140,#23422,.T.);
#41402=EDGE_CURVE('',#32482,#32483,#19515,.T.);
#41403=EDGE_CURVE('',#32141,#32483,#23423,.T.);
#41404=EDGE_CURVE('',#32482,#32422,#25757,.T.);
#41405=EDGE_CURVE('',#32484,#32482,#19516,.T.);
#41406=EDGE_CURVE('',#32485,#32484,#19517,.T.);
#41407=EDGE_CURVE('',#32483,#32485,#19518,.T.);
#41408=EDGE_CURVE('',#32423,#32485,#25758,.T.);
#41409=EDGE_CURVE('',#32486,#32487,#19519,.T.);
#41410=EDGE_CURVE('',#32142,#32487,#23424,.T.);
#41411=EDGE_CURVE('',#32486,#32423,#25759,.T.);
#41412=EDGE_CURVE('',#32488,#32486,#19520,.T.);
#41413=EDGE_CURVE('',#32489,#32488,#19521,.T.);
#41414=EDGE_CURVE('',#32487,#32489,#19522,.T.);
#41415=EDGE_CURVE('',#32424,#32489,#25760,.T.);
#41416=EDGE_CURVE('',#32490,#32491,#19523,.T.);
#41417=EDGE_CURVE('',#32143,#32491,#23425,.T.);
#41418=EDGE_CURVE('',#32490,#32424,#25761,.T.);
#41419=EDGE_CURVE('',#32492,#32490,#19524,.T.);
#41420=EDGE_CURVE('',#32493,#32492,#19525,.T.);
#41421=EDGE_CURVE('',#32491,#32493,#19526,.T.);
#41422=EDGE_CURVE('',#32425,#32493,#25762,.T.);
#41423=EDGE_CURVE('',#32494,#32495,#19527,.T.);
#41424=EDGE_CURVE('',#32144,#32495,#23426,.T.);
#41425=EDGE_CURVE('',#32494,#32425,#25763,.T.);
#41426=EDGE_CURVE('',#32496,#32494,#19528,.T.);
#41427=EDGE_CURVE('',#32497,#32496,#19529,.T.);
#41428=EDGE_CURVE('',#32495,#32497,#19530,.T.);
#41429=EDGE_CURVE('',#32426,#32497,#25764,.T.);
#41430=EDGE_CURVE('',#32498,#32499,#19531,.T.);
#41431=EDGE_CURVE('',#32145,#32499,#23427,.T.);
#41432=EDGE_CURVE('',#32498,#32426,#25765,.T.);
#41433=EDGE_CURVE('',#32500,#32498,#19532,.T.);
#41434=EDGE_CURVE('',#32501,#32500,#19533,.T.);
#41435=EDGE_CURVE('',#32499,#32501,#19534,.T.);
#41436=EDGE_CURVE('',#32427,#32501,#25766,.T.);
#41437=EDGE_CURVE('',#32502,#32503,#19535,.T.);
#41438=EDGE_CURVE('',#32146,#32503,#23428,.T.);
#41439=EDGE_CURVE('',#32502,#32427,#25767,.T.);
#41440=EDGE_CURVE('',#32504,#32502,#19536,.T.);
#41441=EDGE_CURVE('',#32505,#32504,#19537,.T.);
#41442=EDGE_CURVE('',#32503,#32505,#19538,.T.);
#41443=EDGE_CURVE('',#32428,#32505,#25768,.T.);
#41444=EDGE_CURVE('',#32147,#28938,#23429,.T.);
#41445=EDGE_CURVE('',#28940,#32428,#25769,.T.);
#41446=EDGE_CURVE('',#32429,#28939,#25770,.T.);
#41447=EDGE_CURVE('',#32506,#32507,#19539,.T.);
#41448=EDGE_CURVE('',#32148,#32507,#23430,.T.);
#41449=EDGE_CURVE('',#32506,#32429,#25771,.T.);
#41450=EDGE_CURVE('',#32508,#32506,#19540,.T.);
#41451=EDGE_CURVE('',#32509,#32508,#19541,.T.);
#41452=EDGE_CURVE('',#32507,#32509,#19542,.T.);
#41453=EDGE_CURVE('',#32430,#32509,#25772,.T.);
#41454=EDGE_CURVE('',#32510,#32511,#19543,.T.);
#41455=EDGE_CURVE('',#32149,#32511,#23431,.T.);
#41456=EDGE_CURVE('',#32510,#32430,#25773,.T.);
#41457=EDGE_CURVE('',#32512,#32510,#19544,.T.);
#41458=EDGE_CURVE('',#32513,#32512,#19545,.T.);
#41459=EDGE_CURVE('',#32511,#32513,#19546,.T.);
#41460=EDGE_CURVE('',#32431,#32513,#25774,.T.);
#41461=EDGE_CURVE('',#32514,#32515,#19547,.T.);
#41462=EDGE_CURVE('',#32150,#32515,#23432,.T.);
#41463=EDGE_CURVE('',#32514,#32431,#25775,.T.);
#41464=EDGE_CURVE('',#32516,#32514,#19548,.T.);
#41465=EDGE_CURVE('',#32517,#32516,#19549,.T.);
#41466=EDGE_CURVE('',#32515,#32517,#19550,.T.);
#41467=EDGE_CURVE('',#32432,#32517,#25776,.T.);
#41468=EDGE_CURVE('',#32518,#32519,#19551,.T.);
#41469=EDGE_CURVE('',#32151,#32519,#23433,.T.);
#41470=EDGE_CURVE('',#32518,#32432,#25777,.T.);
#41471=EDGE_CURVE('',#32520,#32518,#19552,.T.);
#41472=EDGE_CURVE('',#32521,#32520,#19553,.T.);
#41473=EDGE_CURVE('',#32519,#32521,#19554,.T.);
#41474=EDGE_CURVE('',#32433,#32521,#25778,.T.);
#41475=EDGE_CURVE('',#32522,#32523,#19555,.T.);
#41476=EDGE_CURVE('',#32152,#32523,#23434,.T.);
#41477=EDGE_CURVE('',#32522,#32433,#25779,.T.);
#41478=EDGE_CURVE('',#32524,#32522,#19556,.T.);
#41479=EDGE_CURVE('',#32525,#32524,#19557,.T.);
#41480=EDGE_CURVE('',#32523,#32525,#19558,.T.);
#41481=EDGE_CURVE('',#32434,#32525,#25780,.T.);
#41482=EDGE_CURVE('',#32526,#32527,#19559,.T.);
#41483=EDGE_CURVE('',#32153,#32527,#23435,.T.);
#41484=EDGE_CURVE('',#32526,#32434,#25781,.T.);
#41485=EDGE_CURVE('',#32528,#32526,#19560,.T.);
#41486=EDGE_CURVE('',#32529,#32528,#19561,.T.);
#41487=EDGE_CURVE('',#32527,#32529,#19562,.T.);
#41488=EDGE_CURVE('',#32435,#32529,#25782,.T.);
#41489=EDGE_CURVE('',#32530,#32531,#19563,.T.);
#41490=EDGE_CURVE('',#32154,#32531,#23436,.T.);
#41491=EDGE_CURVE('',#32530,#32435,#25783,.T.);
#41492=EDGE_CURVE('',#32532,#32530,#19564,.T.);
#41493=EDGE_CURVE('',#32533,#32532,#19565,.T.);
#41494=EDGE_CURVE('',#32531,#32533,#19566,.T.);
#41495=EDGE_CURVE('',#32436,#32533,#25784,.T.);
#41496=EDGE_CURVE('',#32534,#32535,#19567,.T.);
#41497=EDGE_CURVE('',#32155,#32535,#23437,.T.);
#41498=EDGE_CURVE('',#32534,#32436,#25785,.T.);
#41499=EDGE_CURVE('',#32536,#32534,#19568,.T.);
#41500=EDGE_CURVE('',#32537,#32536,#19569,.T.);
#41501=EDGE_CURVE('',#32535,#32537,#19570,.T.);
#41502=EDGE_CURVE('',#32437,#32537,#25786,.T.);
#41503=EDGE_CURVE('',#32538,#32539,#19571,.T.);
#41504=EDGE_CURVE('',#32156,#32539,#23438,.T.);
#41505=EDGE_CURVE('',#32538,#32437,#25787,.T.);
#41506=EDGE_CURVE('',#32540,#32538,#19572,.T.);
#41507=EDGE_CURVE('',#32541,#32540,#19573,.T.);
#41508=EDGE_CURVE('',#32539,#32541,#19574,.T.);
#41509=EDGE_CURVE('',#32438,#32541,#25788,.T.);
#41510=EDGE_CURVE('',#32542,#32543,#19575,.T.);
#41511=EDGE_CURVE('',#32157,#32543,#23439,.T.);
#41512=EDGE_CURVE('',#32542,#32438,#25789,.T.);
#41513=EDGE_CURVE('',#32544,#32542,#19576,.T.);
#41514=EDGE_CURVE('',#32545,#32544,#19577,.T.);
#41515=EDGE_CURVE('',#32543,#32545,#19578,.T.);
#41516=EDGE_CURVE('',#32439,#32545,#25790,.T.);
#41517=EDGE_CURVE('',#32546,#32547,#19579,.T.);
#41518=EDGE_CURVE('',#32158,#32547,#23440,.T.);
#41519=EDGE_CURVE('',#32546,#32439,#25791,.T.);
#41520=EDGE_CURVE('',#32548,#32546,#19580,.T.);
#41521=EDGE_CURVE('',#32549,#32548,#19581,.T.);
#41522=EDGE_CURVE('',#32547,#32549,#19582,.T.);
#41523=EDGE_CURVE('',#32440,#32549,#25792,.T.);
#41524=EDGE_CURVE('',#32550,#32551,#19583,.T.);
#41525=EDGE_CURVE('',#32159,#32551,#23441,.T.);
#41526=EDGE_CURVE('',#32550,#32440,#25793,.T.);
#41527=EDGE_CURVE('',#32551,#32552,#19584,.T.);
#41528=EDGE_CURVE('',#32441,#32552,#25794,.T.);
#41529=EDGE_CURVE('',#32553,#32550,#19585,.T.);
#41530=EDGE_CURVE('',#32552,#32553,#19586,.T.);
#41531=EDGE_CURVE('',#32554,#32441,#25795,.T.);
#41532=EDGE_CURVE('',#32554,#32555,#19587,.T.);
#41533=EDGE_CURVE('',#32160,#32555,#23442,.T.);
#41534=EDGE_CURVE('',#32555,#32556,#19588,.T.);
#41535=EDGE_CURVE('',#32557,#32554,#19589,.T.);
#41536=EDGE_CURVE('',#32556,#32557,#19590,.T.);
#41537=EDGE_CURVE('',#32442,#32556,#25796,.T.);
#41538=EDGE_CURVE('',#32558,#32559,#19591,.T.);
#41539=EDGE_CURVE('',#32161,#32559,#23443,.T.);
#41540=EDGE_CURVE('',#32558,#32442,#25797,.T.);
#41541=EDGE_CURVE('',#32560,#32558,#19592,.T.);
#41542=EDGE_CURVE('',#32561,#32560,#19593,.T.);
#41543=EDGE_CURVE('',#32559,#32561,#19594,.T.);
#41544=EDGE_CURVE('',#32443,#32561,#25798,.T.);
#41545=EDGE_CURVE('',#32562,#32563,#19595,.T.);
#41546=EDGE_CURVE('',#32162,#32563,#23444,.T.);
#41547=EDGE_CURVE('',#32562,#32443,#25799,.T.);
#41548=EDGE_CURVE('',#32564,#32562,#19596,.T.);
#41549=EDGE_CURVE('',#32565,#32564,#19597,.T.);
#41550=EDGE_CURVE('',#32563,#32565,#19598,.T.);
#41551=EDGE_CURVE('',#32444,#32565,#25800,.T.);
#41552=EDGE_CURVE('',#32566,#32567,#19599,.T.);
#41553=EDGE_CURVE('',#32163,#32567,#23445,.T.);
#41554=EDGE_CURVE('',#32566,#32444,#25801,.T.);
#41555=EDGE_CURVE('',#32568,#32566,#19600,.T.);
#41556=EDGE_CURVE('',#32569,#32568,#19601,.T.);
#41557=EDGE_CURVE('',#32567,#32569,#19602,.T.);
#41558=EDGE_CURVE('',#32445,#32569,#25802,.T.);
#41559=EDGE_CURVE('',#32570,#32571,#19603,.T.);
#41560=EDGE_CURVE('',#32164,#32571,#23446,.T.);
#41561=EDGE_CURVE('',#32570,#32445,#25803,.T.);
#41562=EDGE_CURVE('',#32572,#32570,#19604,.T.);
#41563=EDGE_CURVE('',#32573,#32572,#19605,.T.);
#41564=EDGE_CURVE('',#32571,#32573,#19606,.T.);
#41565=EDGE_CURVE('',#32446,#32573,#25804,.T.);
#41566=EDGE_CURVE('',#32574,#32575,#19607,.T.);
#41567=EDGE_CURVE('',#32165,#32575,#23447,.T.);
#41568=EDGE_CURVE('',#32574,#32446,#25805,.T.);
#41569=EDGE_CURVE('',#32576,#32574,#19608,.T.);
#41570=EDGE_CURVE('',#32577,#32576,#19609,.T.);
#41571=EDGE_CURVE('',#32575,#32577,#19610,.T.);
#41572=EDGE_CURVE('',#32447,#32577,#25806,.T.);
#41573=EDGE_CURVE('',#32578,#32579,#19611,.T.);
#41574=EDGE_CURVE('',#32166,#32579,#23448,.T.);
#41575=EDGE_CURVE('',#32578,#32447,#25807,.T.);
#41576=EDGE_CURVE('',#32580,#32578,#19612,.T.);
#41577=EDGE_CURVE('',#32581,#32580,#19613,.T.);
#41578=EDGE_CURVE('',#32579,#32581,#19614,.T.);
#41579=EDGE_CURVE('',#32448,#32581,#25808,.T.);
#41580=EDGE_CURVE('',#32582,#32583,#19615,.T.);
#41581=EDGE_CURVE('',#32167,#32583,#23449,.T.);
#41582=EDGE_CURVE('',#32582,#32448,#25809,.T.);
#41583=EDGE_CURVE('',#32584,#32582,#19616,.T.);
#41584=EDGE_CURVE('',#32585,#32584,#19617,.T.);
#41585=EDGE_CURVE('',#32583,#32585,#19618,.T.);
#41586=EDGE_CURVE('',#32449,#32585,#25810,.T.);
#41587=EDGE_CURVE('',#32586,#32587,#19619,.T.);
#41588=EDGE_CURVE('',#32168,#32587,#23450,.T.);
#41589=EDGE_CURVE('',#32586,#32449,#25811,.T.);
#41590=EDGE_CURVE('',#32588,#32586,#19620,.T.);
#41591=EDGE_CURVE('',#32589,#32588,#19621,.T.);
#41592=EDGE_CURVE('',#32587,#32589,#19622,.T.);
#41593=EDGE_CURVE('',#32450,#32589,#25812,.T.);
#41594=EDGE_CURVE('',#32590,#32591,#19623,.T.);
#41595=EDGE_CURVE('',#32481,#32590,#19624,.T.);
#41596=EDGE_CURVE('',#32591,#32480,#19625,.T.);
#41597=EDGE_CURVE('',#32591,#32450,#25813,.T.);
#41598=EDGE_CURVE('',#32592,#32169,#23451,.T.);
#41599=EDGE_CURVE('',#32592,#32593,#19626,.T.);
#41600=EDGE_CURVE('',#32451,#32593,#25814,.T.);
#41601=EDGE_CURVE('',#32594,#32451,#25815,.T.);
#41602=EDGE_CURVE('',#32594,#32595,#19627,.T.);
#41603=EDGE_CURVE('',#32170,#32595,#23452,.T.);
#41604=EDGE_CURVE('',#32595,#32596,#19628,.T.);
#41605=EDGE_CURVE('',#32452,#32596,#25816,.T.);
#41606=EDGE_CURVE('',#32597,#32594,#19629,.T.);
#41607=EDGE_CURVE('',#32596,#32597,#19630,.T.);
#41608=EDGE_CURVE('',#32598,#32452,#25817,.T.);
#41609=EDGE_CURVE('',#32598,#32599,#19631,.T.);
#41610=EDGE_CURVE('',#32171,#32599,#23453,.T.);
#41611=EDGE_CURVE('',#32599,#32600,#19632,.T.);
#41612=EDGE_CURVE('',#32453,#32600,#25818,.T.);
#41613=EDGE_CURVE('',#32601,#32598,#19633,.T.);
#41614=EDGE_CURVE('',#32600,#32601,#19634,.T.);
#41615=EDGE_CURVE('',#32602,#32453,#25819,.T.);
#41616=EDGE_CURVE('',#32602,#32603,#19635,.T.);
#41617=EDGE_CURVE('',#32172,#32603,#23454,.T.);
#41618=EDGE_CURVE('',#32603,#32604,#19636,.T.);
#41619=EDGE_CURVE('',#32454,#32604,#25820,.T.);
#41620=EDGE_CURVE('',#32605,#32602,#19637,.T.);
#41621=EDGE_CURVE('',#32604,#32605,#19638,.T.);
#41622=EDGE_CURVE('',#32606,#32454,#25821,.T.);
#41623=EDGE_CURVE('',#32606,#32607,#19639,.T.);
#41624=EDGE_CURVE('',#32173,#32607,#23455,.T.);
#41625=EDGE_CURVE('',#32607,#32608,#19640,.T.);
#41626=EDGE_CURVE('',#32455,#32608,#25822,.T.);
#41627=EDGE_CURVE('',#32609,#32606,#19641,.T.);
#41628=EDGE_CURVE('',#32608,#32609,#19642,.T.);
#41629=EDGE_CURVE('',#32610,#32455,#25823,.T.);
#41630=EDGE_CURVE('',#32610,#32611,#19643,.T.);
#41631=EDGE_CURVE('',#32174,#32611,#23456,.T.);
#41632=EDGE_CURVE('',#32611,#32612,#19644,.T.);
#41633=EDGE_CURVE('',#32456,#32612,#25824,.T.);
#41634=EDGE_CURVE('',#32613,#32610,#19645,.T.);
#41635=EDGE_CURVE('',#32612,#32613,#19646,.T.);
#41636=EDGE_CURVE('',#32614,#32456,#25825,.T.);
#41637=EDGE_CURVE('',#32614,#32615,#19647,.T.);
#41638=EDGE_CURVE('',#32175,#32615,#23457,.T.);
#41639=EDGE_CURVE('',#32615,#32616,#19648,.T.);
#41640=EDGE_CURVE('',#32457,#32616,#25826,.T.);
#41641=EDGE_CURVE('',#32617,#32614,#19649,.T.);
#41642=EDGE_CURVE('',#32616,#32617,#19650,.T.);
#41643=EDGE_CURVE('',#32618,#32457,#25827,.T.);
#41644=EDGE_CURVE('',#32618,#32619,#19651,.T.);
#41645=EDGE_CURVE('',#32176,#32619,#23458,.T.);
#41646=EDGE_CURVE('',#32619,#32620,#19652,.T.);
#41647=EDGE_CURVE('',#32458,#32620,#25828,.T.);
#41648=EDGE_CURVE('',#32621,#32618,#19653,.T.);
#41649=EDGE_CURVE('',#32620,#32621,#19654,.T.);
#41650=EDGE_CURVE('',#32622,#32458,#25829,.T.);
#41651=EDGE_CURVE('',#32622,#32623,#19655,.T.);
#41652=EDGE_CURVE('',#32177,#32623,#23459,.T.);
#41653=EDGE_CURVE('',#32623,#32624,#19656,.T.);
#41654=EDGE_CURVE('',#32459,#32624,#25830,.T.);
#41655=EDGE_CURVE('',#32625,#32622,#19657,.T.);
#41656=EDGE_CURVE('',#32624,#32625,#19658,.T.);
#41657=EDGE_CURVE('',#32626,#32459,#25831,.T.);
#41658=EDGE_CURVE('',#32626,#32627,#19659,.T.);
#41659=EDGE_CURVE('',#32178,#32627,#23460,.T.);
#41660=EDGE_CURVE('',#32627,#32628,#19660,.T.);
#41661=EDGE_CURVE('',#32460,#32628,#25832,.T.);
#41662=EDGE_CURVE('',#32629,#32626,#19661,.T.);
#41663=EDGE_CURVE('',#32628,#32629,#19662,.T.);
#41664=EDGE_CURVE('',#32630,#32460,#25833,.T.);
#41665=EDGE_CURVE('',#32630,#32631,#19663,.T.);
#41666=EDGE_CURVE('',#32179,#32631,#23461,.T.);
#41667=EDGE_CURVE('',#32631,#32632,#19664,.T.);
#41668=EDGE_CURVE('',#32461,#32632,#25834,.T.);
#41669=EDGE_CURVE('',#32633,#32630,#19665,.T.);
#41670=EDGE_CURVE('',#32632,#32633,#19666,.T.);
#41671=EDGE_CURVE('',#32634,#32461,#25835,.T.);
#41672=EDGE_CURVE('',#32634,#32635,#19667,.T.);
#41673=EDGE_CURVE('',#32180,#32635,#23462,.T.);
#41674=EDGE_CURVE('',#32635,#32636,#19668,.T.);
#41675=EDGE_CURVE('',#32462,#32636,#25836,.T.);
#41676=EDGE_CURVE('',#32637,#32634,#19669,.T.);
#41677=EDGE_CURVE('',#32636,#32637,#19670,.T.);
#41678=EDGE_CURVE('',#32638,#32462,#25837,.T.);
#41679=EDGE_CURVE('',#32638,#32639,#19671,.T.);
#41680=EDGE_CURVE('',#32181,#32639,#23463,.T.);
#41681=EDGE_CURVE('',#32639,#32640,#19672,.T.);
#41682=EDGE_CURVE('',#32463,#32640,#25838,.T.);
#41683=EDGE_CURVE('',#32641,#32638,#19673,.T.);
#41684=EDGE_CURVE('',#32640,#32641,#19674,.T.);
#41685=EDGE_CURVE('',#32642,#32463,#25839,.T.);
#41686=EDGE_CURVE('',#32642,#32643,#19675,.T.);
#41687=EDGE_CURVE('',#32182,#32643,#23464,.T.);
#41688=EDGE_CURVE('',#32643,#32644,#19676,.T.);
#41689=EDGE_CURVE('',#32464,#32644,#25840,.T.);
#41690=EDGE_CURVE('',#32645,#32642,#19677,.T.);
#41691=EDGE_CURVE('',#32644,#32645,#19678,.T.);
#41692=EDGE_CURVE('',#28937,#32464,#25841,.T.);
#41693=EDGE_CURVE('',#32183,#28936,#23465,.T.);
#41694=EDGE_CURVE('',#32465,#28934,#25842,.T.);
#41695=EDGE_CURVE('',#32646,#32465,#25843,.T.);
#41696=EDGE_CURVE('',#32646,#32647,#19679,.T.);
#41697=EDGE_CURVE('',#32184,#32647,#23466,.T.);
#41698=EDGE_CURVE('',#32647,#32648,#19680,.T.);
#41699=EDGE_CURVE('',#32466,#32648,#25844,.T.);
#41700=EDGE_CURVE('',#32649,#32646,#19681,.T.);
#41701=EDGE_CURVE('',#32648,#32649,#19682,.T.);
#41702=EDGE_CURVE('',#32650,#32466,#25845,.T.);
#41703=EDGE_CURVE('',#32650,#32651,#19683,.T.);
#41704=EDGE_CURVE('',#32185,#32651,#23467,.T.);
#41705=EDGE_CURVE('',#32651,#32652,#19684,.T.);
#41706=EDGE_CURVE('',#32467,#32652,#25846,.T.);
#41707=EDGE_CURVE('',#32653,#32650,#19685,.T.);
#41708=EDGE_CURVE('',#32652,#32653,#19686,.T.);
#41709=EDGE_CURVE('',#32654,#32467,#25847,.T.);
#41710=EDGE_CURVE('',#32654,#32655,#19687,.T.);
#41711=EDGE_CURVE('',#32186,#32655,#23468,.T.);
#41712=EDGE_CURVE('',#32655,#32656,#19688,.T.);
#41713=EDGE_CURVE('',#32468,#32656,#25848,.T.);
#41714=EDGE_CURVE('',#32657,#32654,#19689,.T.);
#41715=EDGE_CURVE('',#32656,#32657,#19690,.T.);
#41716=EDGE_CURVE('',#32658,#32468,#25849,.T.);
#41717=EDGE_CURVE('',#32658,#32659,#19691,.T.);
#41718=EDGE_CURVE('',#32187,#32659,#23469,.T.);
#41719=EDGE_CURVE('',#32659,#32660,#19692,.T.);
#41720=EDGE_CURVE('',#32469,#32660,#25850,.T.);
#41721=EDGE_CURVE('',#32661,#32658,#19693,.T.);
#41722=EDGE_CURVE('',#32660,#32661,#19694,.T.);
#41723=EDGE_CURVE('',#32662,#32469,#25851,.T.);
#41724=EDGE_CURVE('',#32662,#32663,#19695,.T.);
#41725=EDGE_CURVE('',#32188,#32663,#23470,.T.);
#41726=EDGE_CURVE('',#32663,#32664,#19696,.T.);
#41727=EDGE_CURVE('',#32470,#32664,#25852,.T.);
#41728=EDGE_CURVE('',#32665,#32662,#19697,.T.);
#41729=EDGE_CURVE('',#32664,#32665,#19698,.T.);
#41730=EDGE_CURVE('',#32666,#32470,#25853,.T.);
#41731=EDGE_CURVE('',#32666,#32667,#19699,.T.);
#41732=EDGE_CURVE('',#32189,#32667,#23471,.T.);
#41733=EDGE_CURVE('',#32667,#32668,#19700,.T.);
#41734=EDGE_CURVE('',#32471,#32668,#25854,.T.);
#41735=EDGE_CURVE('',#32669,#32666,#19701,.T.);
#41736=EDGE_CURVE('',#32668,#32669,#19702,.T.);
#41737=EDGE_CURVE('',#32670,#32471,#25855,.T.);
#41738=EDGE_CURVE('',#32670,#32671,#19703,.T.);
#41739=EDGE_CURVE('',#32190,#32671,#23472,.T.);
#41740=EDGE_CURVE('',#32671,#32672,#19704,.T.);
#41741=EDGE_CURVE('',#32472,#32672,#25856,.T.);
#41742=EDGE_CURVE('',#32673,#32670,#19705,.T.);
#41743=EDGE_CURVE('',#32672,#32673,#19706,.T.);
#41744=EDGE_CURVE('',#32674,#32472,#25857,.T.);
#41745=EDGE_CURVE('',#32674,#32675,#19707,.T.);
#41746=EDGE_CURVE('',#32191,#32675,#23473,.T.);
#41747=EDGE_CURVE('',#32675,#32676,#19708,.T.);
#41748=EDGE_CURVE('',#32473,#32676,#25858,.T.);
#41749=EDGE_CURVE('',#32677,#32674,#19709,.T.);
#41750=EDGE_CURVE('',#32676,#32677,#19710,.T.);
#41751=EDGE_CURVE('',#32678,#32473,#25859,.T.);
#41752=EDGE_CURVE('',#32678,#32679,#19711,.T.);
#41753=EDGE_CURVE('',#32192,#32679,#23474,.T.);
#41754=EDGE_CURVE('',#32679,#32680,#19712,.T.);
#41755=EDGE_CURVE('',#32474,#32680,#25860,.T.);
#41756=EDGE_CURVE('',#32681,#32678,#19713,.T.);
#41757=EDGE_CURVE('',#32680,#32681,#19714,.T.);
#41758=EDGE_CURVE('',#32682,#32474,#25861,.T.);
#41759=EDGE_CURVE('',#32682,#32683,#19715,.T.);
#41760=EDGE_CURVE('',#32193,#32683,#23475,.T.);
#41761=EDGE_CURVE('',#32683,#32684,#19716,.T.);
#41762=EDGE_CURVE('',#32475,#32684,#25862,.T.);
#41763=EDGE_CURVE('',#32685,#32682,#19717,.T.);
#41764=EDGE_CURVE('',#32684,#32685,#19718,.T.);
#41765=EDGE_CURVE('',#32686,#32475,#25863,.T.);
#41766=EDGE_CURVE('',#32686,#32687,#19719,.T.);
#41767=EDGE_CURVE('',#32194,#32687,#23476,.T.);
#41768=EDGE_CURVE('',#32687,#32688,#19720,.T.);
#41769=EDGE_CURVE('',#32476,#32688,#25864,.T.);
#41770=EDGE_CURVE('',#32689,#32686,#19721,.T.);
#41771=EDGE_CURVE('',#32688,#32689,#19722,.T.);
#41772=EDGE_CURVE('',#32690,#32476,#25865,.T.);
#41773=EDGE_CURVE('',#32690,#32691,#19723,.T.);
#41774=EDGE_CURVE('',#32195,#32691,#23477,.T.);
#41775=EDGE_CURVE('',#32691,#32692,#19724,.T.);
#41776=EDGE_CURVE('',#32477,#32692,#25866,.T.);
#41777=EDGE_CURVE('',#32693,#32690,#19725,.T.);
#41778=EDGE_CURVE('',#32692,#32693,#19726,.T.);
#41779=EDGE_CURVE('',#32694,#32477,#25867,.T.);
#41780=EDGE_CURVE('',#32694,#32695,#19727,.T.);
#41781=EDGE_CURVE('',#32196,#32695,#23478,.T.);
#41782=EDGE_CURVE('',#32695,#32696,#19728,.T.);
#41783=EDGE_CURVE('',#32478,#32696,#25868,.T.);
#41784=EDGE_CURVE('',#32697,#32694,#19729,.T.);
#41785=EDGE_CURVE('',#32696,#32697,#19730,.T.);
#41786=EDGE_CURVE('',#32698,#32478,#25869,.T.);
#41787=EDGE_CURVE('',#32698,#32699,#19731,.T.);
#41788=EDGE_CURVE('',#32197,#32699,#23479,.T.);
#41789=EDGE_CURVE('',#32699,#32700,#19732,.T.);
#41790=EDGE_CURVE('',#32479,#32700,#25870,.T.);
#41791=EDGE_CURVE('',#32701,#32698,#19733,.T.);
#41792=EDGE_CURVE('',#32700,#32701,#19734,.T.);
#41793=EDGE_CURVE('',#32702,#32592,#19735,.T.);
#41794=EDGE_CURVE('',#32703,#32702,#19736,.T.);
#41795=EDGE_CURVE('',#32593,#32703,#19737,.T.);
#41796=EDGE_CURVE('',#32702,#32479,#25871,.T.);
#41797=EDGE_CURVE('',#32422,#32704,#19738,.T.);
#41798=EDGE_CURVE('',#32704,#32590,#23480,.T.);
#41799=EDGE_CURVE('',#32705,#32422,#23481,.T.);
#41800=EDGE_CURVE('',#32484,#32705,#23482,.T.);
#41801=EDGE_CURVE('',#32423,#32705,#19739,.T.);
#41802=EDGE_CURVE('',#32706,#32423,#4450,.T.);
#41803=EDGE_CURVE('',#32488,#32706,#23483,.T.);
#41804=EDGE_CURVE('',#32424,#32706,#19740,.T.);
#41805=EDGE_CURVE('',#32707,#32424,#23484,.T.);
#41806=EDGE_CURVE('',#32492,#32707,#23485,.T.);
#41807=EDGE_CURVE('',#32425,#32707,#19741,.T.);
#41808=EDGE_CURVE('',#32708,#32425,#4451,.T.);
#41809=EDGE_CURVE('',#32496,#32708,#23486,.T.);
#41810=EDGE_CURVE('',#32426,#32708,#19742,.T.);
#41811=EDGE_CURVE('',#32709,#32426,#4452,.T.);
#41812=EDGE_CURVE('',#32500,#32709,#23487,.T.);
#41813=EDGE_CURVE('',#32427,#32709,#19743,.T.);
#41814=EDGE_CURVE('',#32710,#32427,#23488,.T.);
#41815=EDGE_CURVE('',#32504,#32710,#23489,.T.);
#41816=EDGE_CURVE('',#32428,#32710,#19744,.T.);
#41817=EDGE_CURVE('',#32711,#32428,#23490,.T.);
#41818=EDGE_CURVE('',#28941,#32711,#23491,.T.);
#41819=EDGE_CURVE('',#32429,#32711,#19745,.T.);
#41820=EDGE_CURVE('',#32712,#32429,#23492,.T.);
#41821=EDGE_CURVE('',#32508,#32712,#23493,.T.);
#41822=EDGE_CURVE('',#32430,#32712,#19746,.T.);
#41823=EDGE_CURVE('',#32713,#32430,#23494,.T.);
#41824=EDGE_CURVE('',#32512,#32713,#23495,.T.);
#41825=EDGE_CURVE('',#32431,#32713,#19747,.T.);
#41826=EDGE_CURVE('',#32714,#32431,#23496,.T.);
#41827=EDGE_CURVE('',#32516,#32714,#23497,.T.);
#41828=EDGE_CURVE('',#32432,#32714,#19748,.T.);
#41829=EDGE_CURVE('',#32715,#32432,#4453,.T.);
#41830=EDGE_CURVE('',#32520,#32715,#23498,.T.);
#41831=EDGE_CURVE('',#32433,#32715,#19749,.T.);
#41832=EDGE_CURVE('',#32716,#32433,#23499,.T.);
#41833=EDGE_CURVE('',#32524,#32716,#23500,.T.);
#41834=EDGE_CURVE('',#32434,#32716,#19750,.T.);
#41835=EDGE_CURVE('',#32717,#32434,#4454,.T.);
#41836=EDGE_CURVE('',#32528,#32717,#23501,.T.);
#41837=EDGE_CURVE('',#32435,#32717,#19751,.T.);
#41838=EDGE_CURVE('',#32718,#32435,#23502,.T.);
#41839=EDGE_CURVE('',#32532,#32718,#23503,.T.);
#41840=EDGE_CURVE('',#32436,#32718,#19752,.T.);
#41841=EDGE_CURVE('',#32719,#32436,#23504,.T.);
#41842=EDGE_CURVE('',#32536,#32719,#23505,.T.);
#41843=EDGE_CURVE('',#32437,#32719,#19753,.T.);
#41844=EDGE_CURVE('',#32720,#32437,#23506,.T.);
#41845=EDGE_CURVE('',#32540,#32720,#23507,.T.);
#41846=EDGE_CURVE('',#32438,#32720,#19754,.T.);
#41847=EDGE_CURVE('',#32721,#32438,#4455,.T.);
#41848=EDGE_CURVE('',#32544,#32721,#23508,.T.);
#41849=EDGE_CURVE('',#32439,#32721,#19755,.T.);
#41850=EDGE_CURVE('',#32722,#32439,#23509,.T.);
#41851=EDGE_CURVE('',#32548,#32722,#23510,.T.);
#41852=EDGE_CURVE('',#32440,#32722,#19756,.T.);
#41853=EDGE_CURVE('',#32723,#32440,#23511,.T.);
#41854=EDGE_CURVE('',#32553,#32723,#23512,.T.);
#41855=EDGE_CURVE('',#32441,#32723,#19757,.T.);
#41856=EDGE_CURVE('',#32724,#32441,#23513,.T.);
#41857=EDGE_CURVE('',#32557,#32724,#23514,.T.);
#41858=EDGE_CURVE('',#32442,#32724,#19758,.T.);
#41859=EDGE_CURVE('',#32725,#32442,#23515,.T.);
#41860=EDGE_CURVE('',#32560,#32725,#23516,.T.);
#41861=EDGE_CURVE('',#32443,#32725,#19759,.T.);
#41862=EDGE_CURVE('',#32726,#32443,#23517,.T.);
#41863=EDGE_CURVE('',#32564,#32726,#23518,.T.);
#41864=EDGE_CURVE('',#32444,#32726,#19760,.T.);
#41865=EDGE_CURVE('',#32727,#32444,#23519,.T.);
#41866=EDGE_CURVE('',#32568,#32727,#23520,.T.);
#41867=EDGE_CURVE('',#32445,#32727,#19761,.T.);
#41868=EDGE_CURVE('',#32728,#32445,#23521,.T.);
#41869=EDGE_CURVE('',#32572,#32728,#23522,.T.);
#41870=EDGE_CURVE('',#32446,#32728,#19762,.T.);
#41871=EDGE_CURVE('',#32729,#32446,#23523,.T.);
#41872=EDGE_CURVE('',#32576,#32729,#23524,.T.);
#41873=EDGE_CURVE('',#32447,#32729,#19763,.T.);
#41874=EDGE_CURVE('',#32730,#32447,#23525,.T.);
#41875=EDGE_CURVE('',#32580,#32730,#23526,.T.);
#41876=EDGE_CURVE('',#32448,#32730,#19764,.T.);
#41877=EDGE_CURVE('',#32731,#32448,#23527,.T.);
#41878=EDGE_CURVE('',#32584,#32731,#23528,.T.);
#41879=EDGE_CURVE('',#32449,#32731,#19765,.T.);
#41880=EDGE_CURVE('',#32732,#32449,#23529,.T.);
#41881=EDGE_CURVE('',#32588,#32732,#23530,.T.);
#41882=EDGE_CURVE('',#32450,#32732,#19766,.T.);
#41883=EDGE_CURVE('',#32704,#32450,#23531,.T.);
#41884=EDGE_CURVE('',#32733,#32703,#23532,.T.);
#41885=EDGE_CURVE('',#32451,#32733,#19767,.T.);
#41886=EDGE_CURVE('',#32734,#32451,#19768,.T.);
#41887=EDGE_CURVE('',#32597,#32734,#23533,.T.);
#41888=EDGE_CURVE('',#32452,#32734,#19769,.T.);
#41889=EDGE_CURVE('',#32735,#32452,#19770,.T.);
#41890=EDGE_CURVE('',#32601,#32735,#23534,.T.);
#41891=EDGE_CURVE('',#32453,#32735,#19771,.T.);
#41892=EDGE_CURVE('',#32736,#32453,#19772,.T.);
#41893=EDGE_CURVE('',#32605,#32736,#23535,.T.);
#41894=EDGE_CURVE('',#32454,#32736,#19773,.T.);
#41895=EDGE_CURVE('',#32737,#32454,#19774,.T.);
#41896=EDGE_CURVE('',#32609,#32737,#23536,.T.);
#41897=EDGE_CURVE('',#32455,#32737,#19775,.T.);
#41898=EDGE_CURVE('',#32738,#32455,#19776,.T.);
#41899=EDGE_CURVE('',#32613,#32738,#23537,.T.);
#41900=EDGE_CURVE('',#32456,#32738,#19777,.T.);
#41901=EDGE_CURVE('',#32739,#32456,#19778,.T.);
#41902=EDGE_CURVE('',#32617,#32739,#23538,.T.);
#41903=EDGE_CURVE('',#32457,#32739,#19779,.T.);
#41904=EDGE_CURVE('',#32740,#32457,#19780,.T.);
#41905=EDGE_CURVE('',#32621,#32740,#23539,.T.);
#41906=EDGE_CURVE('',#32458,#32740,#19781,.T.);
#41907=EDGE_CURVE('',#32741,#32458,#19782,.T.);
#41908=EDGE_CURVE('',#32625,#32741,#23540,.T.);
#41909=EDGE_CURVE('',#32459,#32741,#19783,.T.);
#41910=EDGE_CURVE('',#32742,#32459,#19784,.T.);
#41911=EDGE_CURVE('',#32629,#32742,#23541,.T.);
#41912=EDGE_CURVE('',#32460,#32742,#19785,.T.);
#41913=EDGE_CURVE('',#32743,#32460,#19786,.T.);
#41914=EDGE_CURVE('',#32633,#32743,#23542,.T.);
#41915=EDGE_CURVE('',#32461,#32743,#19787,.T.);
#41916=EDGE_CURVE('',#32744,#32461,#19788,.T.);
#41917=EDGE_CURVE('',#32637,#32744,#23543,.T.);
#41918=EDGE_CURVE('',#32462,#32744,#19789,.T.);
#41919=EDGE_CURVE('',#32745,#32462,#19790,.T.);
#41920=EDGE_CURVE('',#32641,#32745,#23544,.T.);
#41921=EDGE_CURVE('',#32463,#32745,#19791,.T.);
#41922=EDGE_CURVE('',#32746,#32463,#19792,.T.);
#41923=EDGE_CURVE('',#32645,#32746,#23545,.T.);
#41924=EDGE_CURVE('',#32464,#32746,#19793,.T.);
#41925=EDGE_CURVE('',#32747,#32464,#19794,.T.);
#41926=EDGE_CURVE('',#28935,#32747,#23546,.T.);
#41927=EDGE_CURVE('',#32465,#32747,#19795,.T.);
#41928=EDGE_CURVE('',#32748,#32465,#19796,.T.);
#41929=EDGE_CURVE('',#32649,#32748,#23547,.T.);
#41930=EDGE_CURVE('',#32466,#32748,#19797,.T.);
#41931=EDGE_CURVE('',#32749,#32466,#19798,.T.);
#41932=EDGE_CURVE('',#32653,#32749,#23548,.T.);
#41933=EDGE_CURVE('',#32467,#32749,#19799,.T.);
#41934=EDGE_CURVE('',#32750,#32467,#19800,.T.);
#41935=EDGE_CURVE('',#32657,#32750,#23549,.T.);
#41936=EDGE_CURVE('',#32468,#32750,#19801,.T.);
#41937=EDGE_CURVE('',#32751,#32468,#19802,.T.);
#41938=EDGE_CURVE('',#32661,#32751,#23550,.T.);
#41939=EDGE_CURVE('',#32469,#32751,#19803,.T.);
#41940=EDGE_CURVE('',#32752,#32469,#19804,.T.);
#41941=EDGE_CURVE('',#32665,#32752,#23551,.T.);
#41942=EDGE_CURVE('',#32470,#32752,#19805,.T.);
#41943=EDGE_CURVE('',#32753,#32470,#19806,.T.);
#41944=EDGE_CURVE('',#32669,#32753,#23552,.T.);
#41945=EDGE_CURVE('',#32471,#32753,#19807,.T.);
#41946=EDGE_CURVE('',#32754,#32471,#19808,.T.);
#41947=EDGE_CURVE('',#32673,#32754,#23553,.T.);
#41948=EDGE_CURVE('',#32472,#32754,#19809,.T.);
#41949=EDGE_CURVE('',#32755,#32472,#19810,.T.);
#41950=EDGE_CURVE('',#32677,#32755,#23554,.T.);
#41951=EDGE_CURVE('',#32473,#32755,#19811,.T.);
#41952=EDGE_CURVE('',#32756,#32473,#19812,.T.);
#41953=EDGE_CURVE('',#32681,#32756,#23555,.T.);
#41954=EDGE_CURVE('',#32474,#32756,#19813,.T.);
#41955=EDGE_CURVE('',#32757,#32474,#19814,.T.);
#41956=EDGE_CURVE('',#32685,#32757,#23556,.T.);
#41957=EDGE_CURVE('',#32475,#32757,#19815,.T.);
#41958=EDGE_CURVE('',#32758,#32475,#19816,.T.);
#41959=EDGE_CURVE('',#32689,#32758,#23557,.T.);
#41960=EDGE_CURVE('',#32476,#32758,#19817,.T.);
#41961=EDGE_CURVE('',#32759,#32476,#19818,.T.);
#41962=EDGE_CURVE('',#32693,#32759,#23558,.T.);
#41963=EDGE_CURVE('',#32477,#32759,#19819,.T.);
#41964=EDGE_CURVE('',#32760,#32477,#19820,.T.);
#41965=EDGE_CURVE('',#32697,#32760,#23559,.T.);
#41966=EDGE_CURVE('',#32478,#32760,#19821,.T.);
#41967=EDGE_CURVE('',#32761,#32478,#19822,.T.);
#41968=EDGE_CURVE('',#32701,#32761,#23560,.T.);
#41969=EDGE_CURVE('',#32479,#32761,#19823,.T.);
#41970=EDGE_CURVE('',#32733,#32479,#19824,.T.);
#41971=EDGE_CURVE('',#32762,#32763,#19825,.T.);
#41972=EDGE_CURVE('',#32422,#32763,#23561,.T.);
#41973=EDGE_CURVE('',#32762,#32704,#25872,.T.);
#41974=EDGE_CURVE('',#32764,#32762,#19826,.T.);
#41975=EDGE_CURVE('',#32765,#32764,#19827,.T.);
#41976=EDGE_CURVE('',#32763,#32765,#23562,.T.);
#41977=EDGE_CURVE('',#32705,#32765,#25873,.T.);
#41978=EDGE_CURVE('',#32766,#32767,#19828,.T.);
#41979=EDGE_CURVE('',#32423,#32767,#23563,.T.);
#41980=EDGE_CURVE('',#32766,#32705,#25874,.T.);
#41981=EDGE_CURVE('',#32768,#32766,#19829,.T.);
#41982=EDGE_CURVE('',#32769,#32768,#19830,.T.);
#41983=EDGE_CURVE('',#32767,#32769,#23564,.T.);
#41984=EDGE_CURVE('',#32706,#32769,#25875,.T.);
#41985=EDGE_CURVE('',#32770,#32771,#19831,.T.);
#41986=EDGE_CURVE('',#32424,#32771,#23565,.T.);
#41987=EDGE_CURVE('',#32770,#32706,#25876,.T.);
#41988=EDGE_CURVE('',#32772,#32770,#19832,.T.);
#41989=EDGE_CURVE('',#32773,#32772,#19833,.T.);
#41990=EDGE_CURVE('',#32771,#32773,#23566,.T.);
#41991=EDGE_CURVE('',#32707,#32773,#25877,.T.);
#41992=EDGE_CURVE('',#32774,#32775,#19834,.T.);
#41993=EDGE_CURVE('',#32425,#32775,#23567,.T.);
#41994=EDGE_CURVE('',#32774,#32707,#25878,.T.);
#41995=EDGE_CURVE('',#32776,#32774,#19835,.T.);
#41996=EDGE_CURVE('',#32777,#32776,#19836,.T.);
#41997=EDGE_CURVE('',#32775,#32777,#23568,.T.);
#41998=EDGE_CURVE('',#32708,#32777,#25879,.T.);
#41999=EDGE_CURVE('',#32778,#32779,#19837,.T.);
#42000=EDGE_CURVE('',#32426,#32779,#23569,.T.);
#42001=EDGE_CURVE('',#32778,#32708,#25880,.T.);
#42002=EDGE_CURVE('',#32780,#32778,#19838,.T.);
#42003=EDGE_CURVE('',#32781,#32780,#19839,.T.);
#42004=EDGE_CURVE('',#32779,#32781,#23570,.T.);
#42005=EDGE_CURVE('',#32709,#32781,#25881,.T.);
#42006=EDGE_CURVE('',#32782,#32783,#19840,.T.);
#42007=EDGE_CURVE('',#32427,#32783,#23571,.T.);
#42008=EDGE_CURVE('',#32782,#32709,#25882,.T.);
#42009=EDGE_CURVE('',#32784,#32782,#19841,.T.);
#42010=EDGE_CURVE('',#32785,#32784,#19842,.T.);
#42011=EDGE_CURVE('',#32783,#32785,#23572,.T.);
#42012=EDGE_CURVE('',#32710,#32785,#25883,.T.);
#42013=EDGE_CURVE('',#32786,#32787,#19843,.T.);
#42014=EDGE_CURVE('',#32428,#32787,#23573,.T.);
#42015=EDGE_CURVE('',#32786,#32710,#25884,.T.);
#42016=EDGE_CURVE('',#32788,#32786,#19844,.T.);
#42017=EDGE_CURVE('',#32789,#32788,#19845,.T.);
#42018=EDGE_CURVE('',#32787,#32789,#23574,.T.);
#42019=EDGE_CURVE('',#32711,#32789,#25885,.T.);
#42020=EDGE_CURVE('',#32790,#32791,#19846,.T.);
#42021=EDGE_CURVE('',#32429,#32791,#23575,.T.);
#42022=EDGE_CURVE('',#32790,#32711,#25886,.T.);
#42023=EDGE_CURVE('',#32792,#32790,#19847,.T.);
#42024=EDGE_CURVE('',#32793,#32792,#19848,.T.);
#42025=EDGE_CURVE('',#32791,#32793,#23576,.T.);
#42026=EDGE_CURVE('',#32712,#32793,#25887,.T.);
#42027=EDGE_CURVE('',#32794,#32795,#19849,.T.);
#42028=EDGE_CURVE('',#32430,#32795,#23577,.T.);
#42029=EDGE_CURVE('',#32794,#32712,#25888,.T.);
#42030=EDGE_CURVE('',#32796,#32794,#19850,.T.);
#42031=EDGE_CURVE('',#32797,#32796,#19851,.T.);
#42032=EDGE_CURVE('',#32795,#32797,#23578,.T.);
#42033=EDGE_CURVE('',#32713,#32797,#25889,.T.);
#42034=EDGE_CURVE('',#32798,#32799,#19852,.T.);
#42035=EDGE_CURVE('',#32431,#32799,#23579,.T.);
#42036=EDGE_CURVE('',#32798,#32713,#25890,.T.);
#42037=EDGE_CURVE('',#32800,#32798,#19853,.T.);
#42038=EDGE_CURVE('',#32801,#32800,#19854,.T.);
#42039=EDGE_CURVE('',#32799,#32801,#23580,.T.);
#42040=EDGE_CURVE('',#32714,#32801,#25891,.T.);
#42041=EDGE_CURVE('',#32802,#32803,#19855,.T.);
#42042=EDGE_CURVE('',#32432,#32803,#23581,.T.);
#42043=EDGE_CURVE('',#32802,#32714,#25892,.T.);
#42044=EDGE_CURVE('',#32804,#32802,#19856,.T.);
#42045=EDGE_CURVE('',#32805,#32804,#19857,.T.);
#42046=EDGE_CURVE('',#32803,#32805,#23582,.T.);
#42047=EDGE_CURVE('',#32715,#32805,#25893,.T.);
#42048=EDGE_CURVE('',#32806,#32807,#19858,.T.);
#42049=EDGE_CURVE('',#32433,#32807,#23583,.T.);
#42050=EDGE_CURVE('',#32806,#32715,#25894,.T.);
#42051=EDGE_CURVE('',#32808,#32806,#19859,.T.);
#42052=EDGE_CURVE('',#32809,#32808,#19860,.T.);
#42053=EDGE_CURVE('',#32807,#32809,#23584,.T.);
#42054=EDGE_CURVE('',#32716,#32809,#25895,.T.);
#42055=EDGE_CURVE('',#32810,#32811,#19861,.T.);
#42056=EDGE_CURVE('',#32434,#32811,#23585,.T.);
#42057=EDGE_CURVE('',#32810,#32716,#25896,.T.);
#42058=EDGE_CURVE('',#32812,#32810,#19862,.T.);
#42059=EDGE_CURVE('',#32813,#32812,#19863,.T.);
#42060=EDGE_CURVE('',#32811,#32813,#23586,.T.);
#42061=EDGE_CURVE('',#32717,#32813,#25897,.T.);
#42062=EDGE_CURVE('',#32814,#32815,#19864,.T.);
#42063=EDGE_CURVE('',#32435,#32815,#23587,.T.);
#42064=EDGE_CURVE('',#32814,#32717,#25898,.T.);
#42065=EDGE_CURVE('',#32816,#32814,#19865,.T.);
#42066=EDGE_CURVE('',#32817,#32816,#19866,.T.);
#42067=EDGE_CURVE('',#32815,#32817,#23588,.T.);
#42068=EDGE_CURVE('',#32718,#32817,#25899,.T.);
#42069=EDGE_CURVE('',#32436,#28931,#23589,.T.);
#42070=EDGE_CURVE('',#28930,#32718,#25900,.T.);
#42071=EDGE_CURVE('',#32719,#28933,#25901,.T.);
#42072=EDGE_CURVE('',#32818,#32819,#19867,.T.);
#42073=EDGE_CURVE('',#32437,#32819,#23590,.T.);
#42074=EDGE_CURVE('',#32818,#32719,#25902,.T.);
#42075=EDGE_CURVE('',#32820,#32818,#19868,.T.);
#42076=EDGE_CURVE('',#32821,#32820,#19869,.T.);
#42077=EDGE_CURVE('',#32819,#32821,#23591,.T.);
#42078=EDGE_CURVE('',#32720,#32821,#25903,.T.);
#42079=EDGE_CURVE('',#32822,#32823,#19870,.T.);
#42080=EDGE_CURVE('',#32438,#32823,#23592,.T.);
#42081=EDGE_CURVE('',#32822,#32720,#25904,.T.);
#42082=EDGE_CURVE('',#32824,#32822,#19871,.T.);
#42083=EDGE_CURVE('',#32825,#32824,#19872,.T.);
#42084=EDGE_CURVE('',#32823,#32825,#23593,.T.);
#42085=EDGE_CURVE('',#32721,#32825,#25905,.T.);
#42086=EDGE_CURVE('',#32826,#32827,#19873,.T.);
#42087=EDGE_CURVE('',#32439,#32827,#23594,.T.);
#42088=EDGE_CURVE('',#32826,#32721,#25906,.T.);
#42089=EDGE_CURVE('',#32828,#32826,#19874,.T.);
#42090=EDGE_CURVE('',#32829,#32828,#19875,.T.);
#42091=EDGE_CURVE('',#32827,#32829,#23595,.T.);
#42092=EDGE_CURVE('',#32722,#32829,#25907,.T.);
#42093=EDGE_CURVE('',#32830,#32831,#19876,.T.);
#42094=EDGE_CURVE('',#32440,#32831,#23596,.T.);
#42095=EDGE_CURVE('',#32830,#32722,#25908,.T.);
#42096=EDGE_CURVE('',#32831,#32832,#23597,.T.);
#42097=EDGE_CURVE('',#32723,#32832,#25909,.T.);
#42098=EDGE_CURVE('',#32833,#32830,#19877,.T.);
#42099=EDGE_CURVE('',#32832,#32833,#19878,.T.);
#42100=EDGE_CURVE('',#32834,#32723,#25910,.T.);
#42101=EDGE_CURVE('',#32834,#32835,#19879,.T.);
#42102=EDGE_CURVE('',#32441,#32835,#23598,.T.);
#42103=EDGE_CURVE('',#32835,#32836,#23599,.T.);
#42104=EDGE_CURVE('',#32837,#32834,#19880,.T.);
#42105=EDGE_CURVE('',#32836,#32837,#19881,.T.);
#42106=EDGE_CURVE('',#32724,#32836,#25911,.T.);
#42107=EDGE_CURVE('',#32838,#32839,#19882,.T.);
#42108=EDGE_CURVE('',#32442,#32839,#23600,.T.);
#42109=EDGE_CURVE('',#32838,#32724,#25912,.T.);
#42110=EDGE_CURVE('',#32840,#32838,#19883,.T.);
#42111=EDGE_CURVE('',#32841,#32840,#19884,.T.);
#42112=EDGE_CURVE('',#32839,#32841,#23601,.T.);
#42113=EDGE_CURVE('',#32725,#32841,#25913,.T.);
#42114=EDGE_CURVE('',#32842,#32843,#19885,.T.);
#42115=EDGE_CURVE('',#32443,#32843,#23602,.T.);
#42116=EDGE_CURVE('',#32842,#32725,#25914,.T.);
#42117=EDGE_CURVE('',#32844,#32842,#19886,.T.);
#42118=EDGE_CURVE('',#32845,#32844,#19887,.T.);
#42119=EDGE_CURVE('',#32843,#32845,#23603,.T.);
#42120=EDGE_CURVE('',#32726,#32845,#25915,.T.);
#42121=EDGE_CURVE('',#32846,#32847,#19888,.T.);
#42122=EDGE_CURVE('',#32444,#32847,#23604,.T.);
#42123=EDGE_CURVE('',#32846,#32726,#25916,.T.);
#42124=EDGE_CURVE('',#32848,#32846,#19889,.T.);
#42125=EDGE_CURVE('',#32849,#32848,#19890,.T.);
#42126=EDGE_CURVE('',#32847,#32849,#23605,.T.);
#42127=EDGE_CURVE('',#32727,#32849,#25917,.T.);
#42128=EDGE_CURVE('',#32850,#32851,#19891,.T.);
#42129=EDGE_CURVE('',#32445,#32851,#23606,.T.);
#42130=EDGE_CURVE('',#32850,#32727,#25918,.T.);
#42131=EDGE_CURVE('',#32852,#32850,#19892,.T.);
#42132=EDGE_CURVE('',#32853,#32852,#19893,.T.);
#42133=EDGE_CURVE('',#32851,#32853,#23607,.T.);
#42134=EDGE_CURVE('',#32728,#32853,#25919,.T.);
#42135=EDGE_CURVE('',#32854,#32855,#19894,.T.);
#42136=EDGE_CURVE('',#32446,#32855,#23608,.T.);
#42137=EDGE_CURVE('',#32854,#32728,#25920,.T.);
#42138=EDGE_CURVE('',#32856,#32854,#19895,.T.);
#42139=EDGE_CURVE('',#32857,#32856,#19896,.T.);
#42140=EDGE_CURVE('',#32855,#32857,#23609,.T.);
#42141=EDGE_CURVE('',#32729,#32857,#25921,.T.);
#42142=EDGE_CURVE('',#32858,#32859,#19897,.T.);
#42143=EDGE_CURVE('',#32447,#32859,#23610,.T.);
#42144=EDGE_CURVE('',#32858,#32729,#25922,.T.);
#42145=EDGE_CURVE('',#32860,#32858,#19898,.T.);
#42146=EDGE_CURVE('',#32861,#32860,#19899,.T.);
#42147=EDGE_CURVE('',#32859,#32861,#23611,.T.);
#42148=EDGE_CURVE('',#32730,#32861,#25923,.T.);
#42149=EDGE_CURVE('',#32862,#32863,#19900,.T.);
#42150=EDGE_CURVE('',#32448,#32863,#23612,.T.);
#42151=EDGE_CURVE('',#32862,#32730,#25924,.T.);
#42152=EDGE_CURVE('',#32864,#32862,#19901,.T.);
#42153=EDGE_CURVE('',#32865,#32864,#19902,.T.);
#42154=EDGE_CURVE('',#32863,#32865,#23613,.T.);
#42155=EDGE_CURVE('',#32731,#32865,#25925,.T.);
#42156=EDGE_CURVE('',#32866,#32867,#19903,.T.);
#42157=EDGE_CURVE('',#32449,#32867,#23614,.T.);
#42158=EDGE_CURVE('',#32866,#32731,#25926,.T.);
#42159=EDGE_CURVE('',#32868,#32866,#19904,.T.);
#42160=EDGE_CURVE('',#32869,#32868,#19905,.T.);
#42161=EDGE_CURVE('',#32867,#32869,#23615,.T.);
#42162=EDGE_CURVE('',#32732,#32869,#25927,.T.);
#42163=EDGE_CURVE('',#32870,#32871,#19906,.T.);
#42164=EDGE_CURVE('',#32450,#32871,#23616,.T.);
#42165=EDGE_CURVE('',#32870,#32732,#25928,.T.);
#42166=EDGE_CURVE('',#32872,#32870,#19907,.T.);
#42167=EDGE_CURVE('',#32873,#32872,#19908,.T.);
#42168=EDGE_CURVE('',#32871,#32873,#23617,.T.);
#42169=EDGE_CURVE('',#32704,#32873,#25929,.T.);
#42170=EDGE_CURVE('',#32874,#32733,#25930,.T.);
#42171=EDGE_CURVE('',#32874,#32875,#19909,.T.);
#42172=EDGE_CURVE('',#32451,#32875,#23618,.T.);
#42173=EDGE_CURVE('',#32876,#32877,#19910,.T.);
#42174=EDGE_CURVE('',#32876,#32878,#19911,.T.);
#42175=EDGE_CURVE('',#32877,#32878,#19912,.T.);
#42176=EDGE_CURVE('',#32875,#32879,#19913,.T.);
#42177=EDGE_CURVE('',#32734,#32879,#25931,.T.);
#42178=EDGE_CURVE('',#32879,#32876,#19914,.T.);
#42179=EDGE_CURVE('',#32878,#32874,#19915,.T.);
#42180=EDGE_CURVE('',#32880,#32734,#25932,.T.);
#42181=EDGE_CURVE('',#32880,#32881,#19916,.T.);
#42182=EDGE_CURVE('',#32452,#32881,#23619,.T.);
#42183=EDGE_CURVE('',#32882,#32883,#19917,.T.);
#42184=EDGE_CURVE('',#32882,#32884,#19918,.T.);
#42185=EDGE_CURVE('',#32883,#32884,#19919,.T.);
#42186=EDGE_CURVE('',#32881,#32885,#19920,.T.);
#42187=EDGE_CURVE('',#32735,#32885,#25933,.T.);
#42188=EDGE_CURVE('',#32885,#32882,#19921,.T.);
#42189=EDGE_CURVE('',#32884,#32880,#19922,.T.);
#42190=EDGE_CURVE('',#32886,#32735,#25934,.T.);
#42191=EDGE_CURVE('',#32886,#32887,#19923,.T.);
#42192=EDGE_CURVE('',#32453,#32887,#23620,.T.);
#42193=EDGE_CURVE('',#32888,#32889,#19924,.T.);
#42194=EDGE_CURVE('',#32888,#32890,#19925,.T.);
#42195=EDGE_CURVE('',#32889,#32890,#19926,.T.);
#42196=EDGE_CURVE('',#32887,#32891,#19927,.T.);
#42197=EDGE_CURVE('',#32736,#32891,#25935,.T.);
#42198=EDGE_CURVE('',#32891,#32888,#19928,.T.);
#42199=EDGE_CURVE('',#32890,#32886,#19929,.T.);
#42200=EDGE_CURVE('',#32892,#32736,#25936,.T.);
#42201=EDGE_CURVE('',#32892,#32893,#19930,.T.);
#42202=EDGE_CURVE('',#32454,#32893,#23621,.T.);
#42203=EDGE_CURVE('',#32894,#32895,#19931,.T.);
#42204=EDGE_CURVE('',#32894,#32896,#19932,.T.);
#42205=EDGE_CURVE('',#32895,#32896,#19933,.T.);
#42206=EDGE_CURVE('',#32893,#32897,#19934,.T.);
#42207=EDGE_CURVE('',#32737,#32897,#25937,.T.);
#42208=EDGE_CURVE('',#32897,#32894,#19935,.T.);
#42209=EDGE_CURVE('',#32896,#32892,#19936,.T.);
#42210=EDGE_CURVE('',#32898,#32737,#25938,.T.);
#42211=EDGE_CURVE('',#32898,#32899,#19937,.T.);
#42212=EDGE_CURVE('',#32455,#32899,#23622,.T.);
#42213=EDGE_CURVE('',#32900,#32901,#19938,.T.);
#42214=EDGE_CURVE('',#32900,#32902,#19939,.T.);
#42215=EDGE_CURVE('',#32901,#32902,#19940,.T.);
#42216=EDGE_CURVE('',#32899,#32903,#19941,.T.);
#42217=EDGE_CURVE('',#32738,#32903,#25939,.T.);
#42218=EDGE_CURVE('',#32903,#32900,#19942,.T.);
#42219=EDGE_CURVE('',#32902,#32898,#19943,.T.);
#42220=EDGE_CURVE('',#32904,#32738,#25940,.T.);
#42221=EDGE_CURVE('',#32904,#32905,#19944,.T.);
#42222=EDGE_CURVE('',#32456,#32905,#23623,.T.);
#42223=EDGE_CURVE('',#32906,#32907,#19945,.T.);
#42224=EDGE_CURVE('',#32906,#32908,#19946,.T.);
#42225=EDGE_CURVE('',#32907,#32908,#19947,.T.);
#42226=EDGE_CURVE('',#32905,#32909,#19948,.T.);
#42227=EDGE_CURVE('',#32739,#32909,#25941,.T.);
#42228=EDGE_CURVE('',#32909,#32906,#19949,.T.);
#42229=EDGE_CURVE('',#32908,#32904,#19950,.T.);
#42230=EDGE_CURVE('',#32910,#32739,#25942,.T.);
#42231=EDGE_CURVE('',#32910,#32911,#19951,.T.);
#42232=EDGE_CURVE('',#32457,#32911,#23624,.T.);
#42233=EDGE_CURVE('',#32912,#32913,#19952,.T.);
#42234=EDGE_CURVE('',#32912,#32914,#19953,.T.);
#42235=EDGE_CURVE('',#32913,#32914,#19954,.T.);
#42236=EDGE_CURVE('',#32911,#32915,#19955,.T.);
#42237=EDGE_CURVE('',#32740,#32915,#25943,.T.);
#42238=EDGE_CURVE('',#32915,#32912,#19956,.T.);
#42239=EDGE_CURVE('',#32914,#32910,#19957,.T.);
#42240=EDGE_CURVE('',#32916,#32740,#25944,.T.);
#42241=EDGE_CURVE('',#32916,#32917,#19958,.T.);
#42242=EDGE_CURVE('',#32458,#32917,#23625,.T.);
#42243=EDGE_CURVE('',#32918,#32919,#19959,.T.);
#42244=EDGE_CURVE('',#32918,#32920,#19960,.T.);
#42245=EDGE_CURVE('',#32919,#32920,#19961,.T.);
#42246=EDGE_CURVE('',#32917,#32921,#19962,.T.);
#42247=EDGE_CURVE('',#32741,#32921,#25945,.T.);
#42248=EDGE_CURVE('',#32921,#32918,#19963,.T.);
#42249=EDGE_CURVE('',#32920,#32916,#19964,.T.);
#42250=EDGE_CURVE('',#32922,#32741,#25946,.T.);
#42251=EDGE_CURVE('',#32922,#32923,#19965,.T.);
#42252=EDGE_CURVE('',#32459,#32923,#23626,.T.);
#42253=EDGE_CURVE('',#32924,#32925,#19966,.T.);
#42254=EDGE_CURVE('',#32924,#32926,#19967,.T.);
#42255=EDGE_CURVE('',#32925,#32926,#19968,.T.);
#42256=EDGE_CURVE('',#32923,#32927,#19969,.T.);
#42257=EDGE_CURVE('',#32742,#32927,#25947,.T.);
#42258=EDGE_CURVE('',#32927,#32924,#19970,.T.);
#42259=EDGE_CURVE('',#32926,#32922,#19971,.T.);
#42260=EDGE_CURVE('',#32928,#32742,#25948,.T.);
#42261=EDGE_CURVE('',#32928,#32929,#19972,.T.);
#42262=EDGE_CURVE('',#32460,#32929,#23627,.T.);
#42263=EDGE_CURVE('',#32930,#32931,#19973,.T.);
#42264=EDGE_CURVE('',#32930,#32932,#19974,.T.);
#42265=EDGE_CURVE('',#32931,#32932,#19975,.T.);
#42266=EDGE_CURVE('',#32929,#32933,#19976,.T.);
#42267=EDGE_CURVE('',#32743,#32933,#25949,.T.);
#42268=EDGE_CURVE('',#32933,#32930,#19977,.T.);
#42269=EDGE_CURVE('',#32932,#32928,#19978,.T.);
#42270=EDGE_CURVE('',#32934,#32743,#25950,.T.);
#42271=EDGE_CURVE('',#32934,#32935,#19979,.T.);
#42272=EDGE_CURVE('',#32461,#32935,#23628,.T.);
#42273=EDGE_CURVE('',#32936,#32937,#19980,.T.);
#42274=EDGE_CURVE('',#32936,#32938,#19981,.T.);
#42275=EDGE_CURVE('',#32937,#32938,#19982,.T.);
#42276=EDGE_CURVE('',#32935,#32939,#19983,.T.);
#42277=EDGE_CURVE('',#32744,#32939,#25951,.T.);
#42278=EDGE_CURVE('',#32939,#32936,#19984,.T.);
#42279=EDGE_CURVE('',#32938,#32934,#19985,.T.);
#42280=EDGE_CURVE('',#32940,#32744,#25952,.T.);
#42281=EDGE_CURVE('',#32940,#32941,#19986,.T.);
#42282=EDGE_CURVE('',#32462,#32941,#23629,.T.);
#42283=EDGE_CURVE('',#32942,#32943,#19987,.T.);
#42284=EDGE_CURVE('',#32942,#32944,#19988,.T.);
#42285=EDGE_CURVE('',#32943,#32944,#19989,.T.);
#42286=EDGE_CURVE('',#32941,#32945,#19990,.T.);
#42287=EDGE_CURVE('',#32745,#32945,#25953,.T.);
#42288=EDGE_CURVE('',#32945,#32942,#19991,.T.);
#42289=EDGE_CURVE('',#32944,#32940,#19992,.T.);
#42290=EDGE_CURVE('',#32946,#32745,#25954,.T.);
#42291=EDGE_CURVE('',#32946,#32947,#19993,.T.);
#42292=EDGE_CURVE('',#32463,#32947,#23630,.T.);
#42293=EDGE_CURVE('',#32948,#32949,#19994,.T.);
#42294=EDGE_CURVE('',#32948,#32950,#19995,.T.);
#42295=EDGE_CURVE('',#32949,#32950,#19996,.T.);
#42296=EDGE_CURVE('',#32947,#32951,#19997,.T.);
#42297=EDGE_CURVE('',#32746,#32951,#25955,.T.);
#42298=EDGE_CURVE('',#32951,#32948,#19998,.T.);
#42299=EDGE_CURVE('',#32950,#32946,#19999,.T.);
#42300=EDGE_CURVE('',#32952,#32746,#25956,.T.);
#42301=EDGE_CURVE('',#32952,#32953,#20000,.T.);
#42302=EDGE_CURVE('',#32464,#32953,#23631,.T.);
#42303=EDGE_CURVE('',#32954,#32955,#20001,.T.);
#42304=EDGE_CURVE('',#32954,#32956,#20002,.T.);
#42305=EDGE_CURVE('',#32955,#32956,#20003,.T.);
#42306=EDGE_CURVE('',#32953,#32957,#20004,.T.);
#42307=EDGE_CURVE('',#32747,#32957,#25957,.T.);
#42308=EDGE_CURVE('',#32957,#32954,#20005,.T.);
#42309=EDGE_CURVE('',#32956,#32952,#20006,.T.);
#42310=EDGE_CURVE('',#32958,#32747,#25958,.T.);
#42311=EDGE_CURVE('',#32958,#32959,#20007,.T.);
#42312=EDGE_CURVE('',#32465,#32959,#23632,.T.);
#42313=EDGE_CURVE('',#32960,#32961,#20008,.T.);
#42314=EDGE_CURVE('',#32960,#32962,#20009,.T.);
#42315=EDGE_CURVE('',#32961,#32962,#20010,.T.);
#42316=EDGE_CURVE('',#32959,#32963,#20011,.T.);
#42317=EDGE_CURVE('',#32748,#32963,#25959,.T.);
#42318=EDGE_CURVE('',#32963,#32960,#20012,.T.);
#42319=EDGE_CURVE('',#32962,#32958,#20013,.T.);
#42320=EDGE_CURVE('',#32964,#32748,#25960,.T.);
#42321=EDGE_CURVE('',#32964,#32965,#20014,.T.);
#42322=EDGE_CURVE('',#32466,#32965,#23633,.T.);
#42323=EDGE_CURVE('',#32966,#32967,#20015,.T.);
#42324=EDGE_CURVE('',#32966,#32968,#20016,.T.);
#42325=EDGE_CURVE('',#32967,#32968,#20017,.T.);
#42326=EDGE_CURVE('',#32965,#32969,#20018,.T.);
#42327=EDGE_CURVE('',#32749,#32969,#25961,.T.);
#42328=EDGE_CURVE('',#32969,#32966,#20019,.T.);
#42329=EDGE_CURVE('',#32968,#32964,#20020,.T.);
#42330=EDGE_CURVE('',#32970,#32749,#25962,.T.);
#42331=EDGE_CURVE('',#32970,#32971,#20021,.T.);
#42332=EDGE_CURVE('',#32467,#32971,#23634,.T.);
#42333=EDGE_CURVE('',#32972,#32973,#20022,.T.);
#42334=EDGE_CURVE('',#32972,#32974,#20023,.T.);
#42335=EDGE_CURVE('',#32973,#32974,#20024,.T.);
#42336=EDGE_CURVE('',#32971,#32975,#20025,.T.);
#42337=EDGE_CURVE('',#32750,#32975,#25963,.T.);
#42338=EDGE_CURVE('',#32975,#32972,#20026,.T.);
#42339=EDGE_CURVE('',#32974,#32970,#20027,.T.);
#42340=EDGE_CURVE('',#32976,#32750,#25964,.T.);
#42341=EDGE_CURVE('',#32976,#32977,#20028,.T.);
#42342=EDGE_CURVE('',#32468,#32977,#23635,.T.);
#42343=EDGE_CURVE('',#32978,#32979,#20029,.T.);
#42344=EDGE_CURVE('',#32978,#32980,#20030,.T.);
#42345=EDGE_CURVE('',#32979,#32980,#20031,.T.);
#42346=EDGE_CURVE('',#32977,#32981,#20032,.T.);
#42347=EDGE_CURVE('',#32751,#32981,#25965,.T.);
#42348=EDGE_CURVE('',#32981,#32978,#20033,.T.);
#42349=EDGE_CURVE('',#32980,#32976,#20034,.T.);
#42350=EDGE_CURVE('',#32982,#32751,#25966,.T.);
#42351=EDGE_CURVE('',#32982,#32983,#20035,.T.);
#42352=EDGE_CURVE('',#32469,#32983,#23636,.T.);
#42353=EDGE_CURVE('',#32984,#32985,#20036,.T.);
#42354=EDGE_CURVE('',#32984,#32986,#20037,.T.);
#42355=EDGE_CURVE('',#32985,#32986,#20038,.T.);
#42356=EDGE_CURVE('',#32983,#32987,#20039,.T.);
#42357=EDGE_CURVE('',#32752,#32987,#25967,.T.);
#42358=EDGE_CURVE('',#32987,#32984,#20040,.T.);
#42359=EDGE_CURVE('',#32986,#32982,#20041,.T.);
#42360=EDGE_CURVE('',#32988,#32752,#25968,.T.);
#42361=EDGE_CURVE('',#32988,#32989,#20042,.T.);
#42362=EDGE_CURVE('',#32470,#32989,#23637,.T.);
#42363=EDGE_CURVE('',#32990,#32991,#20043,.T.);
#42364=EDGE_CURVE('',#32990,#32992,#20044,.T.);
#42365=EDGE_CURVE('',#32991,#32992,#20045,.T.);
#42366=EDGE_CURVE('',#32989,#32993,#20046,.T.);
#42367=EDGE_CURVE('',#32753,#32993,#25969,.T.);
#42368=EDGE_CURVE('',#32993,#32990,#20047,.T.);
#42369=EDGE_CURVE('',#32992,#32988,#20048,.T.);
#42370=EDGE_CURVE('',#32994,#32753,#25970,.T.);
#42371=EDGE_CURVE('',#32994,#32995,#20049,.T.);
#42372=EDGE_CURVE('',#32471,#32995,#23638,.T.);
#42373=EDGE_CURVE('',#32996,#32997,#20050,.T.);
#42374=EDGE_CURVE('',#32996,#32998,#20051,.T.);
#42375=EDGE_CURVE('',#32997,#32998,#20052,.T.);
#42376=EDGE_CURVE('',#32995,#32999,#20053,.T.);
#42377=EDGE_CURVE('',#32754,#32999,#25971,.T.);
#42378=EDGE_CURVE('',#32999,#32996,#20054,.T.);
#42379=EDGE_CURVE('',#32998,#32994,#20055,.T.);
#42380=EDGE_CURVE('',#28928,#32754,#25972,.T.);
#42381=EDGE_CURVE('',#32472,#28927,#23639,.T.);
#42382=EDGE_CURVE('',#32755,#28926,#25973,.T.);
#42383=EDGE_CURVE('',#33000,#32755,#25974,.T.);
#42384=EDGE_CURVE('',#33000,#33001,#20056,.T.);
#42385=EDGE_CURVE('',#32473,#33001,#23640,.T.);
#42386=EDGE_CURVE('',#33002,#33003,#20057,.T.);
#42387=EDGE_CURVE('',#33002,#33004,#20058,.T.);
#42388=EDGE_CURVE('',#33003,#33004,#20059,.T.);
#42389=EDGE_CURVE('',#33001,#33005,#20060,.T.);
#42390=EDGE_CURVE('',#32756,#33005,#25975,.T.);
#42391=EDGE_CURVE('',#33005,#33002,#20061,.T.);
#42392=EDGE_CURVE('',#33004,#33000,#20062,.T.);
#42393=EDGE_CURVE('',#33006,#32756,#25976,.T.);
#42394=EDGE_CURVE('',#33006,#33007,#20063,.T.);
#42395=EDGE_CURVE('',#32474,#33007,#23641,.T.);
#42396=EDGE_CURVE('',#33008,#33009,#20064,.T.);
#42397=EDGE_CURVE('',#33008,#33010,#20065,.T.);
#42398=EDGE_CURVE('',#33009,#33010,#20066,.T.);
#42399=EDGE_CURVE('',#33007,#33011,#20067,.T.);
#42400=EDGE_CURVE('',#32757,#33011,#25977,.T.);
#42401=EDGE_CURVE('',#33011,#33008,#20068,.T.);
#42402=EDGE_CURVE('',#33010,#33006,#20069,.T.);
#42403=EDGE_CURVE('',#33012,#32757,#25978,.T.);
#42404=EDGE_CURVE('',#33012,#33013,#20070,.T.);
#42405=EDGE_CURVE('',#32475,#33013,#23642,.T.);
#42406=EDGE_CURVE('',#33014,#33015,#20071,.T.);
#42407=EDGE_CURVE('',#33016,#33014,#20072,.T.);
#42408=EDGE_CURVE('',#33016,#33015,#20073,.T.);
#42409=EDGE_CURVE('',#33013,#33017,#20074,.T.);
#42410=EDGE_CURVE('',#32758,#33017,#25979,.T.);
#42411=EDGE_CURVE('',#33017,#33016,#20075,.T.);
#42412=EDGE_CURVE('',#33015,#33012,#20076,.T.);
#42413=EDGE_CURVE('',#33018,#32758,#25980,.T.);
#42414=EDGE_CURVE('',#33018,#33019,#20077,.T.);
#42415=EDGE_CURVE('',#32476,#33019,#23643,.T.);
#42416=EDGE_CURVE('',#33020,#33021,#20078,.T.);
#42417=EDGE_CURVE('',#33020,#33022,#20079,.T.);
#42418=EDGE_CURVE('',#33021,#33022,#20080,.T.);
#42419=EDGE_CURVE('',#33019,#33023,#20081,.T.);
#42420=EDGE_CURVE('',#32759,#33023,#25981,.T.);
#42421=EDGE_CURVE('',#33023,#33020,#20082,.T.);
#42422=EDGE_CURVE('',#33022,#33018,#20083,.T.);
#42423=EDGE_CURVE('',#33024,#32759,#25982,.T.);
#42424=EDGE_CURVE('',#33024,#33025,#20084,.T.);
#42425=EDGE_CURVE('',#32477,#33025,#23644,.T.);
#42426=EDGE_CURVE('',#33026,#33027,#20085,.T.);
#42427=EDGE_CURVE('',#33026,#33028,#20086,.T.);
#42428=EDGE_CURVE('',#33027,#33028,#20087,.T.);
#42429=EDGE_CURVE('',#33025,#33029,#20088,.T.);
#42430=EDGE_CURVE('',#32760,#33029,#25983,.T.);
#42431=EDGE_CURVE('',#33029,#33026,#20089,.T.);
#42432=EDGE_CURVE('',#33028,#33024,#20090,.T.);
#42433=EDGE_CURVE('',#33030,#32760,#25984,.T.);
#42434=EDGE_CURVE('',#33030,#33031,#20091,.T.);
#42435=EDGE_CURVE('',#32478,#33031,#23645,.T.);
#42436=EDGE_CURVE('',#33032,#33033,#20092,.T.);
#42437=EDGE_CURVE('',#33032,#33034,#20093,.T.);
#42438=EDGE_CURVE('',#33033,#33034,#20094,.T.);
#42439=EDGE_CURVE('',#33031,#33035,#20095,.T.);
#42440=EDGE_CURVE('',#32761,#33035,#25985,.T.);
#42441=EDGE_CURVE('',#33035,#33032,#20096,.T.);
#42442=EDGE_CURVE('',#33034,#33030,#20097,.T.);
#42443=EDGE_CURVE('',#33036,#32761,#25986,.T.);
#42444=EDGE_CURVE('',#33036,#33037,#20098,.T.);
#42445=EDGE_CURVE('',#32479,#33037,#23646,.T.);
#42446=EDGE_CURVE('',#33038,#33039,#20099,.T.);
#42447=EDGE_CURVE('',#33038,#33040,#20100,.T.);
#42448=EDGE_CURVE('',#33039,#33040,#20101,.T.);
#42449=EDGE_CURVE('',#33037,#33041,#20102,.T.);
#42450=EDGE_CURVE('',#32733,#33041,#25987,.T.);
#42451=EDGE_CURVE('',#33041,#33038,#20103,.T.);
#42452=EDGE_CURVE('',#33040,#33036,#20104,.T.);
#42453=EDGE_CURVE('',#33042,#32704,#20105,.T.);
#42454=EDGE_CURVE('',#32764,#33042,#23647,.T.);
#42455=EDGE_CURVE('',#32705,#33042,#20106,.T.);
#42456=EDGE_CURVE('',#33043,#32705,#20107,.T.);
#42457=EDGE_CURVE('',#32768,#33043,#23648,.T.);
#42458=EDGE_CURVE('',#32706,#33043,#20108,.T.);
#42459=EDGE_CURVE('',#33044,#32706,#20109,.T.);
#42460=EDGE_CURVE('',#32772,#33044,#23649,.T.);
#42461=EDGE_CURVE('',#32707,#33044,#20110,.T.);
#42462=EDGE_CURVE('',#33045,#32707,#20111,.T.);
#42463=EDGE_CURVE('',#32776,#33045,#23650,.T.);
#42464=EDGE_CURVE('',#32708,#33045,#20112,.T.);
#42465=EDGE_CURVE('',#33046,#32708,#20113,.T.);
#42466=EDGE_CURVE('',#32780,#33046,#23651,.T.);
#42467=EDGE_CURVE('',#32709,#33046,#20114,.T.);
#42468=EDGE_CURVE('',#33047,#32709,#20115,.T.);
#42469=EDGE_CURVE('',#32784,#33047,#23652,.T.);
#42470=EDGE_CURVE('',#32710,#33047,#20116,.T.);
#42471=EDGE_CURVE('',#33048,#32710,#20117,.T.);
#42472=EDGE_CURVE('',#32788,#33048,#23653,.T.);
#42473=EDGE_CURVE('',#32711,#33048,#20118,.T.);
#42474=EDGE_CURVE('',#33049,#32711,#20119,.T.);
#42475=EDGE_CURVE('',#32792,#33049,#23654,.T.);
#42476=EDGE_CURVE('',#32712,#33049,#20120,.T.);
#42477=EDGE_CURVE('',#33050,#32712,#20121,.T.);
#42478=EDGE_CURVE('',#32796,#33050,#23655,.T.);
#42479=EDGE_CURVE('',#32713,#33050,#20122,.T.);
#42480=EDGE_CURVE('',#33051,#32713,#20123,.T.);
#42481=EDGE_CURVE('',#32800,#33051,#23656,.T.);
#42482=EDGE_CURVE('',#32714,#33051,#20124,.T.);
#42483=EDGE_CURVE('',#33052,#32714,#20125,.T.);
#42484=EDGE_CURVE('',#32804,#33052,#23657,.T.);
#42485=EDGE_CURVE('',#32715,#33052,#20126,.T.);
#42486=EDGE_CURVE('',#33053,#32715,#20127,.T.);
#42487=EDGE_CURVE('',#32808,#33053,#23658,.T.);
#42488=EDGE_CURVE('',#32716,#33053,#20128,.T.);
#42489=EDGE_CURVE('',#33054,#32716,#20129,.T.);
#42490=EDGE_CURVE('',#32812,#33054,#23659,.T.);
#42491=EDGE_CURVE('',#32717,#33054,#20130,.T.);
#42492=EDGE_CURVE('',#33055,#32717,#20131,.T.);
#42493=EDGE_CURVE('',#32816,#33055,#23660,.T.);
#42494=EDGE_CURVE('',#32718,#33055,#20132,.T.);
#42495=EDGE_CURVE('',#33056,#32718,#20133,.T.);
#42496=EDGE_CURVE('',#28932,#33056,#23661,.T.);
#42497=EDGE_CURVE('',#32719,#33056,#20134,.T.);
#42498=EDGE_CURVE('',#33057,#32719,#20135,.T.);
#42499=EDGE_CURVE('',#32820,#33057,#23662,.T.);
#42500=EDGE_CURVE('',#32720,#33057,#20136,.T.);
#42501=EDGE_CURVE('',#33058,#32720,#20137,.T.);
#42502=EDGE_CURVE('',#32824,#33058,#23663,.T.);
#42503=EDGE_CURVE('',#32721,#33058,#20138,.T.);
#42504=EDGE_CURVE('',#33059,#32721,#20139,.T.);
#42505=EDGE_CURVE('',#32828,#33059,#23664,.T.);
#42506=EDGE_CURVE('',#32722,#33059,#20140,.T.);
#42507=EDGE_CURVE('',#33060,#32722,#20141,.T.);
#42508=EDGE_CURVE('',#32833,#33060,#23665,.T.);
#42509=EDGE_CURVE('',#32723,#33060,#20142,.T.);
#42510=EDGE_CURVE('',#33061,#32723,#20143,.T.);
#42511=EDGE_CURVE('',#32837,#33061,#23666,.T.);
#42512=EDGE_CURVE('',#32724,#33061,#20144,.T.);
#42513=EDGE_CURVE('',#33062,#32724,#20145,.T.);
#42514=EDGE_CURVE('',#32840,#33062,#23667,.T.);
#42515=EDGE_CURVE('',#32725,#33062,#20146,.T.);
#42516=EDGE_CURVE('',#33063,#32725,#20147,.T.);
#42517=EDGE_CURVE('',#32844,#33063,#23668,.T.);
#42518=EDGE_CURVE('',#32726,#33063,#20148,.T.);
#42519=EDGE_CURVE('',#33064,#32726,#20149,.T.);
#42520=EDGE_CURVE('',#32848,#33064,#23669,.T.);
#42521=EDGE_CURVE('',#32727,#33064,#20150,.T.);
#42522=EDGE_CURVE('',#33065,#32727,#20151,.T.);
#42523=EDGE_CURVE('',#32852,#33065,#23670,.T.);
#42524=EDGE_CURVE('',#32728,#33065,#20152,.T.);
#42525=EDGE_CURVE('',#33066,#32728,#20153,.T.);
#42526=EDGE_CURVE('',#32856,#33066,#23671,.T.);
#42527=EDGE_CURVE('',#32729,#33066,#20154,.T.);
#42528=EDGE_CURVE('',#33067,#32729,#20155,.T.);
#42529=EDGE_CURVE('',#32860,#33067,#23672,.T.);
#42530=EDGE_CURVE('',#32730,#33067,#20156,.T.);
#42531=EDGE_CURVE('',#33068,#32730,#20157,.T.);
#42532=EDGE_CURVE('',#32864,#33068,#23673,.T.);
#42533=EDGE_CURVE('',#32731,#33068,#20158,.T.);
#42534=EDGE_CURVE('',#33069,#32731,#20159,.T.);
#42535=EDGE_CURVE('',#32868,#33069,#23674,.T.);
#42536=EDGE_CURVE('',#32732,#33069,#20160,.T.);
#42537=EDGE_CURVE('',#33070,#32732,#20161,.T.);
#42538=EDGE_CURVE('',#32872,#33070,#23675,.T.);
#42539=EDGE_CURVE('',#32704,#33070,#20162,.T.);
#42540=EDGE_CURVE('',#33071,#32733,#20163,.T.);
#42541=EDGE_CURVE('',#32877,#33071,#112,.T.);
#42542=EDGE_CURVE('',#32734,#33071,#20164,.T.);
#42543=EDGE_CURVE('',#33072,#32734,#20165,.T.);
#42544=EDGE_CURVE('',#32883,#33072,#113,.T.);
#42545=EDGE_CURVE('',#32735,#33072,#20166,.T.);
#42546=EDGE_CURVE('',#33073,#32735,#20167,.T.);
#42547=EDGE_CURVE('',#32889,#33073,#114,.T.);
#42548=EDGE_CURVE('',#32736,#33073,#20168,.T.);
#42549=EDGE_CURVE('',#33074,#32736,#20169,.T.);
#42550=EDGE_CURVE('',#32895,#33074,#115,.T.);
#42551=EDGE_CURVE('',#32737,#33074,#20170,.T.);
#42552=EDGE_CURVE('',#33075,#32737,#20171,.T.);
#42553=EDGE_CURVE('',#32901,#33075,#116,.T.);
#42554=EDGE_CURVE('',#32738,#33075,#20172,.T.);
#42555=EDGE_CURVE('',#33076,#32738,#20173,.T.);
#42556=EDGE_CURVE('',#32907,#33076,#117,.T.);
#42557=EDGE_CURVE('',#32739,#33076,#20174,.T.);
#42558=EDGE_CURVE('',#33077,#32739,#20175,.T.);
#42559=EDGE_CURVE('',#32913,#33077,#118,.T.);
#42560=EDGE_CURVE('',#32740,#33077,#20176,.T.);
#42561=EDGE_CURVE('',#33078,#32740,#20177,.T.);
#42562=EDGE_CURVE('',#32919,#33078,#119,.T.);
#42563=EDGE_CURVE('',#32741,#33078,#20178,.T.);
#42564=EDGE_CURVE('',#33079,#32741,#20179,.T.);
#42565=EDGE_CURVE('',#32925,#33079,#120,.T.);
#42566=EDGE_CURVE('',#32742,#33079,#20180,.T.);
#42567=EDGE_CURVE('',#33080,#32742,#20181,.T.);
#42568=EDGE_CURVE('',#32931,#33080,#121,.T.);
#42569=EDGE_CURVE('',#32743,#33080,#20182,.T.);
#42570=EDGE_CURVE('',#33081,#32743,#20183,.T.);
#42571=EDGE_CURVE('',#32937,#33081,#122,.T.);
#42572=EDGE_CURVE('',#32744,#33081,#20184,.T.);
#42573=EDGE_CURVE('',#33082,#32744,#20185,.T.);
#42574=EDGE_CURVE('',#32943,#33082,#123,.T.);
#42575=EDGE_CURVE('',#32745,#33082,#20186,.T.);
#42576=EDGE_CURVE('',#33083,#32745,#20187,.T.);
#42577=EDGE_CURVE('',#32949,#33083,#124,.T.);
#42578=EDGE_CURVE('',#32746,#33083,#20188,.T.);
#42579=EDGE_CURVE('',#33084,#32746,#20189,.T.);
#42580=EDGE_CURVE('',#32955,#33084,#125,.T.);
#42581=EDGE_CURVE('',#32747,#33084,#20190,.T.);
#42582=EDGE_CURVE('',#33085,#32747,#20191,.T.);
#42583=EDGE_CURVE('',#32961,#33085,#126,.T.);
#42584=EDGE_CURVE('',#32748,#33085,#20192,.T.);
#42585=EDGE_CURVE('',#33086,#32748,#20193,.T.);
#42586=EDGE_CURVE('',#32967,#33086,#127,.T.);
#42587=EDGE_CURVE('',#32749,#33086,#20194,.T.);
#42588=EDGE_CURVE('',#33087,#32749,#20195,.T.);
#42589=EDGE_CURVE('',#32973,#33087,#128,.T.);
#42590=EDGE_CURVE('',#32750,#33087,#20196,.T.);
#42591=EDGE_CURVE('',#33088,#32750,#20197,.T.);
#42592=EDGE_CURVE('',#32979,#33088,#129,.T.);
#42593=EDGE_CURVE('',#32751,#33088,#20198,.T.);
#42594=EDGE_CURVE('',#33089,#32751,#20199,.T.);
#42595=EDGE_CURVE('',#32985,#33089,#130,.T.);
#42596=EDGE_CURVE('',#32752,#33089,#20200,.T.);
#42597=EDGE_CURVE('',#33090,#32752,#20201,.T.);
#42598=EDGE_CURVE('',#32991,#33090,#131,.T.);
#42599=EDGE_CURVE('',#32753,#33090,#20202,.T.);
#42600=EDGE_CURVE('',#33091,#32753,#20203,.T.);
#42601=EDGE_CURVE('',#32997,#33091,#132,.T.);
#42602=EDGE_CURVE('',#32754,#33091,#20204,.T.);
#42603=EDGE_CURVE('',#33092,#32754,#20205,.T.);
#42604=EDGE_CURVE('',#28929,#33092,#133,.T.);
#42605=EDGE_CURVE('',#32755,#33092,#20206,.T.);
#42606=EDGE_CURVE('',#33093,#32755,#20207,.T.);
#42607=EDGE_CURVE('',#33003,#33093,#134,.T.);
#42608=EDGE_CURVE('',#32756,#33093,#20208,.T.);
#42609=EDGE_CURVE('',#33094,#32756,#20209,.T.);
#42610=EDGE_CURVE('',#33009,#33094,#135,.T.);
#42611=EDGE_CURVE('',#32757,#33094,#20210,.T.);
#42612=EDGE_CURVE('',#33095,#32757,#20211,.T.);
#42613=EDGE_CURVE('',#33014,#33095,#136,.T.);
#42614=EDGE_CURVE('',#32758,#33095,#20212,.T.);
#42615=EDGE_CURVE('',#33096,#32758,#20213,.T.);
#42616=EDGE_CURVE('',#33021,#33096,#137,.T.);
#42617=EDGE_CURVE('',#32759,#33096,#20214,.T.);
#42618=EDGE_CURVE('',#33097,#32759,#20215,.T.);
#42619=EDGE_CURVE('',#33027,#33097,#138,.T.);
#42620=EDGE_CURVE('',#32760,#33097,#20216,.T.);
#42621=EDGE_CURVE('',#33098,#32760,#20217,.T.);
#42622=EDGE_CURVE('',#33033,#33098,#139,.T.);
#42623=EDGE_CURVE('',#32761,#33098,#20218,.T.);
#42624=EDGE_CURVE('',#33099,#32761,#20219,.T.);
#42625=EDGE_CURVE('',#33039,#33099,#140,.T.);
#42626=EDGE_CURVE('',#32733,#33099,#20220,.T.);
#42627=EDGE_CURVE('',#33100,#33101,#20221,.T.);
#42628=EDGE_CURVE('',#33042,#33101,#25988,.T.);
#42629=EDGE_CURVE('',#33100,#32704,#23676,.T.);
#42630=EDGE_CURVE('',#33102,#33103,#20222,.T.);
#42631=EDGE_CURVE('',#32705,#33103,#23677,.T.);
#42632=EDGE_CURVE('',#33102,#33042,#25989,.T.);
#42633=EDGE_CURVE('',#33104,#33102,#20223,.T.);
#42634=EDGE_CURVE('',#33105,#33104,#20224,.T.);
#42635=EDGE_CURVE('',#33103,#33105,#20225,.T.);
#42636=EDGE_CURVE('',#33043,#33105,#25990,.T.);
#42637=EDGE_CURVE('',#33106,#33107,#20226,.T.);
#42638=EDGE_CURVE('',#32706,#33107,#23678,.T.);
#42639=EDGE_CURVE('',#33106,#33043,#25991,.T.);
#42640=EDGE_CURVE('',#33108,#33106,#20227,.T.);
#42641=EDGE_CURVE('',#33109,#33108,#20228,.T.);
#42642=EDGE_CURVE('',#33107,#33109,#20229,.T.);
#42643=EDGE_CURVE('',#33044,#33109,#25992,.T.);
#42644=EDGE_CURVE('',#33110,#33111,#20230,.T.);
#42645=EDGE_CURVE('',#32707,#33111,#23679,.T.);
#42646=EDGE_CURVE('',#33110,#33044,#25993,.T.);
#42647=EDGE_CURVE('',#33112,#33110,#20231,.T.);
#42648=EDGE_CURVE('',#33113,#33112,#20232,.T.);
#42649=EDGE_CURVE('',#33111,#33113,#20233,.T.);
#42650=EDGE_CURVE('',#33045,#33113,#25994,.T.);
#42651=EDGE_CURVE('',#33114,#33115,#20234,.T.);
#42652=EDGE_CURVE('',#32708,#33115,#23680,.T.);
#42653=EDGE_CURVE('',#33114,#33045,#25995,.T.);
#42654=EDGE_CURVE('',#33116,#33114,#20235,.T.);
#42655=EDGE_CURVE('',#33117,#33116,#20236,.T.);
#42656=EDGE_CURVE('',#33115,#33117,#20237,.T.);
#42657=EDGE_CURVE('',#33046,#33117,#25996,.T.);
#42658=EDGE_CURVE('',#33118,#33119,#20238,.T.);
#42659=EDGE_CURVE('',#32709,#33119,#23681,.T.);
#42660=EDGE_CURVE('',#33118,#33046,#25997,.T.);
#42661=EDGE_CURVE('',#33120,#33118,#20239,.T.);
#42662=EDGE_CURVE('',#33121,#33120,#20240,.T.);
#42663=EDGE_CURVE('',#33119,#33121,#20241,.T.);
#42664=EDGE_CURVE('',#33047,#33121,#25998,.T.);
#42665=EDGE_CURVE('',#33122,#33123,#20242,.T.);
#42666=EDGE_CURVE('',#32710,#33123,#23682,.T.);
#42667=EDGE_CURVE('',#33122,#33047,#25999,.T.);
#42668=EDGE_CURVE('',#33124,#33122,#20243,.T.);
#42669=EDGE_CURVE('',#33125,#33124,#20244,.T.);
#42670=EDGE_CURVE('',#33123,#33125,#20245,.T.);
#42671=EDGE_CURVE('',#33048,#33125,#26000,.T.);
#42672=EDGE_CURVE('',#32711,#28920,#23683,.T.);
#42673=EDGE_CURVE('',#28922,#33048,#26001,.T.);
#42674=EDGE_CURVE('',#33049,#28921,#26002,.T.);
#42675=EDGE_CURVE('',#33126,#33127,#20246,.T.);
#42676=EDGE_CURVE('',#32712,#33127,#23684,.T.);
#42677=EDGE_CURVE('',#33126,#33049,#26003,.T.);
#42678=EDGE_CURVE('',#33128,#33126,#20247,.T.);
#42679=EDGE_CURVE('',#33129,#33128,#20248,.T.);
#42680=EDGE_CURVE('',#33127,#33129,#20249,.T.);
#42681=EDGE_CURVE('',#33050,#33129,#26004,.T.);
#42682=EDGE_CURVE('',#33130,#33131,#20250,.T.);
#42683=EDGE_CURVE('',#32713,#33131,#23685,.T.);
#42684=EDGE_CURVE('',#33130,#33050,#26005,.T.);
#42685=EDGE_CURVE('',#33132,#33130,#20251,.T.);
#42686=EDGE_CURVE('',#33133,#33132,#20252,.T.);
#42687=EDGE_CURVE('',#33131,#33133,#20253,.T.);
#42688=EDGE_CURVE('',#33051,#33133,#26006,.T.);
#42689=EDGE_CURVE('',#33134,#33135,#20254,.T.);
#42690=EDGE_CURVE('',#32714,#33135,#23686,.T.);
#42691=EDGE_CURVE('',#33134,#33051,#26007,.T.);
#42692=EDGE_CURVE('',#33136,#33134,#20255,.T.);
#42693=EDGE_CURVE('',#33137,#33136,#20256,.T.);
#42694=EDGE_CURVE('',#33135,#33137,#20257,.T.);
#42695=EDGE_CURVE('',#33052,#33137,#26008,.T.);
#42696=EDGE_CURVE('',#33138,#33139,#20258,.T.);
#42697=EDGE_CURVE('',#32715,#33139,#23687,.T.);
#42698=EDGE_CURVE('',#33138,#33052,#26009,.T.);
#42699=EDGE_CURVE('',#33140,#33138,#20259,.T.);
#42700=EDGE_CURVE('',#33141,#33140,#20260,.T.);
#42701=EDGE_CURVE('',#33139,#33141,#20261,.T.);
#42702=EDGE_CURVE('',#33053,#33141,#26010,.T.);
#42703=EDGE_CURVE('',#33142,#33143,#20262,.T.);
#42704=EDGE_CURVE('',#32716,#33143,#23688,.T.);
#42705=EDGE_CURVE('',#33142,#33053,#26011,.T.);
#42706=EDGE_CURVE('',#33144,#33142,#20263,.T.);
#42707=EDGE_CURVE('',#33145,#33144,#20264,.T.);
#42708=EDGE_CURVE('',#33143,#33145,#20265,.T.);
#42709=EDGE_CURVE('',#33054,#33145,#26012,.T.);
#42710=EDGE_CURVE('',#33146,#33147,#20266,.T.);
#42711=EDGE_CURVE('',#32717,#33147,#23689,.T.);
#42712=EDGE_CURVE('',#33146,#33054,#26013,.T.);
#42713=EDGE_CURVE('',#33148,#33146,#20267,.T.);
#42714=EDGE_CURVE('',#33149,#33148,#20268,.T.);
#42715=EDGE_CURVE('',#33147,#33149,#20269,.T.);
#42716=EDGE_CURVE('',#33055,#33149,#26014,.T.);
#42717=EDGE_CURVE('',#33150,#33151,#20270,.T.);
#42718=EDGE_CURVE('',#32718,#33151,#23690,.T.);
#42719=EDGE_CURVE('',#33150,#33055,#26015,.T.);
#42720=EDGE_CURVE('',#33152,#33150,#20271,.T.);
#42721=EDGE_CURVE('',#33153,#33152,#20272,.T.);
#42722=EDGE_CURVE('',#33151,#33153,#20273,.T.);
#42723=EDGE_CURVE('',#33056,#33153,#26016,.T.);
#42724=EDGE_CURVE('',#33154,#33155,#20274,.T.);
#42725=EDGE_CURVE('',#32719,#33155,#23691,.T.);
#42726=EDGE_CURVE('',#33154,#33056,#26017,.T.);
#42727=EDGE_CURVE('',#33156,#33154,#20275,.T.);
#42728=EDGE_CURVE('',#33157,#33156,#20276,.T.);
#42729=EDGE_CURVE('',#33155,#33157,#20277,.T.);
#42730=EDGE_CURVE('',#33057,#33157,#26018,.T.);
#42731=EDGE_CURVE('',#33158,#33159,#20278,.T.);
#42732=EDGE_CURVE('',#32720,#33159,#23692,.T.);
#42733=EDGE_CURVE('',#33158,#33057,#26019,.T.);
#42734=EDGE_CURVE('',#33160,#33158,#20279,.T.);
#42735=EDGE_CURVE('',#33161,#33160,#20280,.T.);
#42736=EDGE_CURVE('',#33159,#33161,#20281,.T.);
#42737=EDGE_CURVE('',#33058,#33161,#26020,.T.);
#42738=EDGE_CURVE('',#33162,#33163,#20282,.T.);
#42739=EDGE_CURVE('',#32721,#33163,#23693,.T.);
#42740=EDGE_CURVE('',#33162,#33058,#26021,.T.);
#42741=EDGE_CURVE('',#33164,#33162,#20283,.T.);
#42742=EDGE_CURVE('',#33165,#33164,#20284,.T.);
#42743=EDGE_CURVE('',#33163,#33165,#20285,.T.);
#42744=EDGE_CURVE('',#33059,#33165,#26022,.T.);
#42745=EDGE_CURVE('',#33166,#33167,#20286,.T.);
#42746=EDGE_CURVE('',#32722,#33167,#23694,.T.);
#42747=EDGE_CURVE('',#33166,#33059,#26023,.T.);
#42748=EDGE_CURVE('',#33167,#33168,#20287,.T.);
#42749=EDGE_CURVE('',#33060,#33168,#26024,.T.);
#42750=EDGE_CURVE('',#33169,#33166,#20288,.T.);
#42751=EDGE_CURVE('',#33168,#33169,#20289,.T.);
#42752=EDGE_CURVE('',#33170,#33060,#26025,.T.);
#42753=EDGE_CURVE('',#33170,#33171,#20290,.T.);
#42754=EDGE_CURVE('',#32723,#33171,#23695,.T.);
#42755=EDGE_CURVE('',#33171,#33172,#20291,.T.);
#42756=EDGE_CURVE('',#33173,#33170,#20292,.T.);
#42757=EDGE_CURVE('',#33172,#33173,#20293,.T.);
#42758=EDGE_CURVE('',#33061,#33172,#26026,.T.);
#42759=EDGE_CURVE('',#33174,#33175,#20294,.T.);
#42760=EDGE_CURVE('',#32724,#33175,#23696,.T.);
#42761=EDGE_CURVE('',#33174,#33061,#26027,.T.);
#42762=EDGE_CURVE('',#33176,#33174,#20295,.T.);
#42763=EDGE_CURVE('',#33177,#33176,#20296,.T.);
#42764=EDGE_CURVE('',#33175,#33177,#20297,.T.);
#42765=EDGE_CURVE('',#33062,#33177,#26028,.T.);
#42766=EDGE_CURVE('',#33178,#33179,#20298,.T.);
#42767=EDGE_CURVE('',#32725,#33179,#23697,.T.);
#42768=EDGE_CURVE('',#33178,#33062,#26029,.T.);
#42769=EDGE_CURVE('',#33180,#33178,#20299,.T.);
#42770=EDGE_CURVE('',#33181,#33180,#20300,.T.);
#42771=EDGE_CURVE('',#33179,#33181,#20301,.T.);
#42772=EDGE_CURVE('',#33063,#33181,#26030,.T.);
#42773=EDGE_CURVE('',#33182,#33183,#20302,.T.);
#42774=EDGE_CURVE('',#32726,#33183,#23698,.T.);
#42775=EDGE_CURVE('',#33182,#33063,#26031,.T.);
#42776=EDGE_CURVE('',#33184,#33182,#20303,.T.);
#42777=EDGE_CURVE('',#33185,#33184,#20304,.T.);
#42778=EDGE_CURVE('',#33183,#33185,#20305,.T.);
#42779=EDGE_CURVE('',#33064,#33185,#26032,.T.);
#42780=EDGE_CURVE('',#33186,#33187,#20306,.T.);
#42781=EDGE_CURVE('',#32727,#33187,#23699,.T.);
#42782=EDGE_CURVE('',#33186,#33064,#26033,.T.);
#42783=EDGE_CURVE('',#33188,#33186,#20307,.T.);
#42784=EDGE_CURVE('',#33189,#33188,#20308,.T.);
#42785=EDGE_CURVE('',#33187,#33189,#20309,.T.);
#42786=EDGE_CURVE('',#33065,#33189,#26034,.T.);
#42787=EDGE_CURVE('',#33190,#33191,#20310,.T.);
#42788=EDGE_CURVE('',#32728,#33191,#23700,.T.);
#42789=EDGE_CURVE('',#33190,#33065,#26035,.T.);
#42790=EDGE_CURVE('',#33192,#33190,#20311,.T.);
#42791=EDGE_CURVE('',#33193,#33192,#20312,.T.);
#42792=EDGE_CURVE('',#33191,#33193,#20313,.T.);
#42793=EDGE_CURVE('',#33066,#33193,#26036,.T.);
#42794=EDGE_CURVE('',#33194,#33195,#20314,.T.);
#42795=EDGE_CURVE('',#32729,#33195,#23701,.T.);
#42796=EDGE_CURVE('',#33194,#33066,#26037,.T.);
#42797=EDGE_CURVE('',#33196,#33194,#20315,.T.);
#42798=EDGE_CURVE('',#33197,#33196,#20316,.T.);
#42799=EDGE_CURVE('',#33195,#33197,#20317,.T.);
#42800=EDGE_CURVE('',#33067,#33197,#26038,.T.);
#42801=EDGE_CURVE('',#33198,#33199,#20318,.T.);
#42802=EDGE_CURVE('',#32730,#33199,#23702,.T.);
#42803=EDGE_CURVE('',#33198,#33067,#26039,.T.);
#42804=EDGE_CURVE('',#33200,#33198,#20319,.T.);
#42805=EDGE_CURVE('',#33201,#33200,#20320,.T.);
#42806=EDGE_CURVE('',#33199,#33201,#20321,.T.);
#42807=EDGE_CURVE('',#33068,#33201,#26040,.T.);
#42808=EDGE_CURVE('',#33202,#33203,#20322,.T.);
#42809=EDGE_CURVE('',#32731,#33203,#23703,.T.);
#42810=EDGE_CURVE('',#33202,#33068,#26041,.T.);
#42811=EDGE_CURVE('',#33204,#33202,#20323,.T.);
#42812=EDGE_CURVE('',#33205,#33204,#20324,.T.);
#42813=EDGE_CURVE('',#33203,#33205,#20325,.T.);
#42814=EDGE_CURVE('',#33069,#33205,#26042,.T.);
#42815=EDGE_CURVE('',#33206,#33207,#20326,.T.);
#42816=EDGE_CURVE('',#32732,#33207,#23704,.T.);
#42817=EDGE_CURVE('',#33206,#33069,#26043,.T.);
#42818=EDGE_CURVE('',#33208,#33206,#20327,.T.);
#42819=EDGE_CURVE('',#33209,#33208,#20328,.T.);
#42820=EDGE_CURVE('',#33207,#33209,#20329,.T.);
#42821=EDGE_CURVE('',#33070,#33209,#26044,.T.);
#42822=EDGE_CURVE('',#33210,#33211,#20330,.T.);
#42823=EDGE_CURVE('',#33101,#33210,#20331,.T.);
#42824=EDGE_CURVE('',#33211,#33100,#20332,.T.);
#42825=EDGE_CURVE('',#33211,#33070,#26045,.T.);
#42826=EDGE_CURVE('',#33212,#32733,#23705,.T.);
#42827=EDGE_CURVE('',#33212,#33213,#23706,.T.);
#42828=EDGE_CURVE('',#33071,#33213,#26046,.T.);
#42829=EDGE_CURVE('',#33214,#33071,#26047,.T.);
#42830=EDGE_CURVE('',#33214,#33215,#23707,.T.);
#42831=EDGE_CURVE('',#32734,#33215,#23708,.T.);
#42832=EDGE_CURVE('',#33216,#33214,#23709,.T.);
#42833=EDGE_CURVE('',#33217,#33216,#23710,.T.);
#42834=EDGE_CURVE('',#33215,#33217,#23711,.T.);
#42835=EDGE_CURVE('',#33072,#33217,#26048,.T.);
#42836=EDGE_CURVE('',#33218,#33072,#26049,.T.);
#42837=EDGE_CURVE('',#33218,#33219,#23712,.T.);
#42838=EDGE_CURVE('',#32735,#33219,#23713,.T.);
#42839=EDGE_CURVE('',#33220,#33218,#23714,.T.);
#42840=EDGE_CURVE('',#33221,#33220,#23715,.T.);
#42841=EDGE_CURVE('',#33219,#33221,#23716,.T.);
#42842=EDGE_CURVE('',#33073,#33221,#26050,.T.);
#42843=EDGE_CURVE('',#33222,#33073,#26051,.T.);
#42844=EDGE_CURVE('',#33222,#33223,#23717,.T.);
#42845=EDGE_CURVE('',#32736,#33223,#23718,.T.);
#42846=EDGE_CURVE('',#33224,#33222,#23719,.T.);
#42847=EDGE_CURVE('',#33225,#33224,#23720,.T.);
#42848=EDGE_CURVE('',#33223,#33225,#23721,.T.);
#42849=EDGE_CURVE('',#33074,#33225,#26052,.T.);
#42850=EDGE_CURVE('',#33226,#33074,#26053,.T.);
#42851=EDGE_CURVE('',#33226,#33227,#23722,.T.);
#42852=EDGE_CURVE('',#32737,#33227,#23723,.T.);
#42853=EDGE_CURVE('',#33228,#33226,#23724,.T.);
#42854=EDGE_CURVE('',#33229,#33228,#23725,.T.);
#42855=EDGE_CURVE('',#33227,#33229,#23726,.T.);
#42856=EDGE_CURVE('',#33075,#33229,#26054,.T.);
#42857=EDGE_CURVE('',#33230,#33075,#26055,.T.);
#42858=EDGE_CURVE('',#33230,#33231,#23727,.T.);
#42859=EDGE_CURVE('',#32738,#33231,#23728,.T.);
#42860=EDGE_CURVE('',#33232,#33230,#23729,.T.);
#42861=EDGE_CURVE('',#33233,#33232,#23730,.T.);
#42862=EDGE_CURVE('',#33231,#33233,#23731,.T.);
#42863=EDGE_CURVE('',#33076,#33233,#26056,.T.);
#42864=EDGE_CURVE('',#33234,#33076,#26057,.T.);
#42865=EDGE_CURVE('',#33234,#33235,#23732,.T.);
#42866=EDGE_CURVE('',#32739,#33235,#23733,.T.);
#42867=EDGE_CURVE('',#33236,#33234,#23734,.T.);
#42868=EDGE_CURVE('',#33237,#33236,#23735,.T.);
#42869=EDGE_CURVE('',#33235,#33237,#23736,.T.);
#42870=EDGE_CURVE('',#33077,#33237,#26058,.T.);
#42871=EDGE_CURVE('',#33238,#33077,#26059,.T.);
#42872=EDGE_CURVE('',#33238,#33239,#23737,.T.);
#42873=EDGE_CURVE('',#32740,#33239,#23738,.T.);
#42874=EDGE_CURVE('',#33240,#33238,#23739,.T.);
#42875=EDGE_CURVE('',#33241,#33240,#23740,.T.);
#42876=EDGE_CURVE('',#33239,#33241,#23741,.T.);
#42877=EDGE_CURVE('',#33078,#33241,#26060,.T.);
#42878=EDGE_CURVE('',#33242,#33078,#26061,.T.);
#42879=EDGE_CURVE('',#33242,#33243,#23742,.T.);
#42880=EDGE_CURVE('',#32741,#33243,#23743,.T.);
#42881=EDGE_CURVE('',#33244,#33242,#23744,.T.);
#42882=EDGE_CURVE('',#33245,#33244,#23745,.T.);
#42883=EDGE_CURVE('',#33243,#33245,#23746,.T.);
#42884=EDGE_CURVE('',#33079,#33245,#26062,.T.);
#42885=EDGE_CURVE('',#33246,#33079,#26063,.T.);
#42886=EDGE_CURVE('',#33246,#33247,#23747,.T.);
#42887=EDGE_CURVE('',#32742,#33247,#23748,.T.);
#42888=EDGE_CURVE('',#33248,#33246,#23749,.T.);
#42889=EDGE_CURVE('',#33249,#33248,#23750,.T.);
#42890=EDGE_CURVE('',#33247,#33249,#23751,.T.);
#42891=EDGE_CURVE('',#33080,#33249,#26064,.T.);
#42892=EDGE_CURVE('',#33250,#33080,#26065,.T.);
#42893=EDGE_CURVE('',#33250,#33251,#23752,.T.);
#42894=EDGE_CURVE('',#32743,#33251,#23753,.T.);
#42895=EDGE_CURVE('',#33252,#33250,#23754,.T.);
#42896=EDGE_CURVE('',#33253,#33252,#23755,.T.);
#42897=EDGE_CURVE('',#33251,#33253,#23756,.T.);
#42898=EDGE_CURVE('',#33081,#33253,#26066,.T.);
#42899=EDGE_CURVE('',#33254,#33081,#26067,.T.);
#42900=EDGE_CURVE('',#33254,#33255,#23757,.T.);
#42901=EDGE_CURVE('',#32744,#33255,#23758,.T.);
#42902=EDGE_CURVE('',#33256,#33254,#23759,.T.);
#42903=EDGE_CURVE('',#33257,#33256,#23760,.T.);
#42904=EDGE_CURVE('',#33255,#33257,#23761,.T.);
#42905=EDGE_CURVE('',#33082,#33257,#26068,.T.);
#42906=EDGE_CURVE('',#33258,#33082,#26069,.T.);
#42907=EDGE_CURVE('',#33258,#33259,#23762,.T.);
#42908=EDGE_CURVE('',#32745,#33259,#23763,.T.);
#42909=EDGE_CURVE('',#33260,#33258,#23764,.T.);
#42910=EDGE_CURVE('',#33261,#33260,#23765,.T.);
#42911=EDGE_CURVE('',#33259,#33261,#23766,.T.);
#42912=EDGE_CURVE('',#33083,#33261,#26070,.T.);
#42913=EDGE_CURVE('',#33262,#33083,#26071,.T.);
#42914=EDGE_CURVE('',#33262,#33263,#23767,.T.);
#42915=EDGE_CURVE('',#32746,#33263,#23768,.T.);
#42916=EDGE_CURVE('',#33264,#33262,#23769,.T.);
#42917=EDGE_CURVE('',#33265,#33264,#23770,.T.);
#42918=EDGE_CURVE('',#33263,#33265,#23771,.T.);
#42919=EDGE_CURVE('',#33084,#33265,#26072,.T.);
#42920=EDGE_CURVE('',#28919,#33084,#26073,.T.);
#42921=EDGE_CURVE('',#32747,#28918,#23772,.T.);
#42922=EDGE_CURVE('',#33085,#28916,#26074,.T.);
#42923=EDGE_CURVE('',#33266,#33085,#26075,.T.);
#42924=EDGE_CURVE('',#33266,#33267,#23773,.T.);
#42925=EDGE_CURVE('',#32748,#33267,#23774,.T.);
#42926=EDGE_CURVE('',#33268,#33266,#23775,.T.);
#42927=EDGE_CURVE('',#33269,#33268,#23776,.T.);
#42928=EDGE_CURVE('',#33267,#33269,#23777,.T.);
#42929=EDGE_CURVE('',#33086,#33269,#26076,.T.);
#42930=EDGE_CURVE('',#33270,#33086,#26077,.T.);
#42931=EDGE_CURVE('',#33270,#33271,#23778,.T.);
#42932=EDGE_CURVE('',#32749,#33271,#23779,.T.);
#42933=EDGE_CURVE('',#33272,#33270,#23780,.T.);
#42934=EDGE_CURVE('',#33273,#33272,#23781,.T.);
#42935=EDGE_CURVE('',#33271,#33273,#23782,.T.);
#42936=EDGE_CURVE('',#33087,#33273,#26078,.T.);
#42937=EDGE_CURVE('',#33274,#33087,#26079,.T.);
#42938=EDGE_CURVE('',#33274,#33275,#23783,.T.);
#42939=EDGE_CURVE('',#32750,#33275,#23784,.T.);
#42940=EDGE_CURVE('',#33276,#33274,#23785,.T.);
#42941=EDGE_CURVE('',#33277,#33276,#23786,.T.);
#42942=EDGE_CURVE('',#33275,#33277,#23787,.T.);
#42943=EDGE_CURVE('',#33088,#33277,#26080,.T.);
#42944=EDGE_CURVE('',#33278,#33088,#26081,.T.);
#42945=EDGE_CURVE('',#33278,#33279,#23788,.T.);
#42946=EDGE_CURVE('',#32751,#33279,#23789,.T.);
#42947=EDGE_CURVE('',#33280,#33278,#23790,.T.);
#42948=EDGE_CURVE('',#33281,#33280,#23791,.T.);
#42949=EDGE_CURVE('',#33279,#33281,#23792,.T.);
#42950=EDGE_CURVE('',#33089,#33281,#26082,.T.);
#42951=EDGE_CURVE('',#33282,#33089,#26083,.T.);
#42952=EDGE_CURVE('',#33282,#33283,#23793,.T.);
#42953=EDGE_CURVE('',#32752,#33283,#23794,.T.);
#42954=EDGE_CURVE('',#33284,#33282,#23795,.T.);
#42955=EDGE_CURVE('',#33285,#33284,#23796,.T.);
#42956=EDGE_CURVE('',#33283,#33285,#23797,.T.);
#42957=EDGE_CURVE('',#33090,#33285,#26084,.T.);
#42958=EDGE_CURVE('',#33286,#33090,#26085,.T.);
#42959=EDGE_CURVE('',#33286,#33287,#23798,.T.);
#42960=EDGE_CURVE('',#32753,#33287,#23799,.T.);
#42961=EDGE_CURVE('',#33288,#33286,#23800,.T.);
#42962=EDGE_CURVE('',#33289,#33288,#23801,.T.);
#42963=EDGE_CURVE('',#33287,#33289,#23802,.T.);
#42964=EDGE_CURVE('',#33091,#33289,#26086,.T.);
#42965=EDGE_CURVE('',#28915,#33091,#26087,.T.);
#42966=EDGE_CURVE('',#32754,#28914,#23803,.T.);
#42967=EDGE_CURVE('',#33092,#28912,#26088,.T.);
#42968=EDGE_CURVE('',#33290,#33092,#26089,.T.);
#42969=EDGE_CURVE('',#33290,#33291,#23804,.T.);
#42970=EDGE_CURVE('',#32755,#33291,#23805,.T.);
#42971=EDGE_CURVE('',#33292,#33290,#23806,.T.);
#42972=EDGE_CURVE('',#33293,#33292,#23807,.T.);
#42973=EDGE_CURVE('',#33291,#33293,#23808,.T.);
#42974=EDGE_CURVE('',#33093,#33293,#26090,.T.);
#42975=EDGE_CURVE('',#33294,#33093,#26091,.T.);
#42976=EDGE_CURVE('',#33294,#33295,#23809,.T.);
#42977=EDGE_CURVE('',#32756,#33295,#23810,.T.);
#42978=EDGE_CURVE('',#33296,#33294,#23811,.T.);
#42979=EDGE_CURVE('',#33297,#33296,#23812,.T.);
#42980=EDGE_CURVE('',#33295,#33297,#23813,.T.);
#42981=EDGE_CURVE('',#33094,#33297,#26092,.T.);
#42982=EDGE_CURVE('',#33298,#33094,#26093,.T.);
#42983=EDGE_CURVE('',#33298,#33299,#23814,.T.);
#42984=EDGE_CURVE('',#32757,#33299,#23815,.T.);
#42985=EDGE_CURVE('',#33300,#33298,#23816,.T.);
#42986=EDGE_CURVE('',#33301,#33300,#23817,.T.);
#42987=EDGE_CURVE('',#33299,#33301,#23818,.T.);
#42988=EDGE_CURVE('',#33095,#33301,#26094,.T.);
#42989=EDGE_CURVE('',#33302,#33095,#26095,.T.);
#42990=EDGE_CURVE('',#33302,#33303,#23819,.T.);
#42991=EDGE_CURVE('',#32758,#33303,#23820,.T.);
#42992=EDGE_CURVE('',#33304,#33302,#23821,.T.);
#42993=EDGE_CURVE('',#33305,#33304,#23822,.T.);
#42994=EDGE_CURVE('',#33303,#33305,#23823,.T.);
#42995=EDGE_CURVE('',#33096,#33305,#26096,.T.);
#42996=EDGE_CURVE('',#33306,#33096,#26097,.T.);
#42997=EDGE_CURVE('',#33306,#33307,#23824,.T.);
#42998=EDGE_CURVE('',#32759,#33307,#23825,.T.);
#42999=EDGE_CURVE('',#33308,#33306,#23826,.T.);
#43000=EDGE_CURVE('',#33309,#33308,#23827,.T.);
#43001=EDGE_CURVE('',#33307,#33309,#23828,.T.);
#43002=EDGE_CURVE('',#33097,#33309,#26098,.T.);
#43003=EDGE_CURVE('',#33310,#33097,#26099,.T.);
#43004=EDGE_CURVE('',#33310,#33311,#23829,.T.);
#43005=EDGE_CURVE('',#32760,#33311,#23830,.T.);
#43006=EDGE_CURVE('',#33312,#33310,#23831,.T.);
#43007=EDGE_CURVE('',#33313,#33312,#23832,.T.);
#43008=EDGE_CURVE('',#33311,#33313,#23833,.T.);
#43009=EDGE_CURVE('',#33098,#33313,#26100,.T.);
#43010=EDGE_CURVE('',#33314,#33098,#26101,.T.);
#43011=EDGE_CURVE('',#33314,#33315,#23834,.T.);
#43012=EDGE_CURVE('',#32761,#33315,#23835,.T.);
#43013=EDGE_CURVE('',#33316,#33314,#23836,.T.);
#43014=EDGE_CURVE('',#33317,#33316,#23837,.T.);
#43015=EDGE_CURVE('',#33315,#33317,#23838,.T.);
#43016=EDGE_CURVE('',#33099,#33317,#26102,.T.);
#43017=EDGE_CURVE('',#33318,#33212,#23839,.T.);
#43018=EDGE_CURVE('',#33319,#33318,#23840,.T.);
#43019=EDGE_CURVE('',#33213,#33319,#23841,.T.);
#43020=EDGE_CURVE('',#33318,#33099,#26103,.T.);
#43021=EDGE_CURVE('',#33042,#33320,#20333,.T.);
#43022=EDGE_CURVE('',#33320,#33210,#23842,.T.);
#43023=EDGE_CURVE('',#33321,#33042,#20334,.T.);
#43024=EDGE_CURVE('',#33104,#33321,#23843,.T.);
#43025=EDGE_CURVE('',#33043,#33321,#20335,.T.);
#43026=EDGE_CURVE('',#33322,#33043,#20336,.T.);
#43027=EDGE_CURVE('',#33108,#33322,#23844,.T.);
#43028=EDGE_CURVE('',#33044,#33322,#20337,.T.);
#43029=EDGE_CURVE('',#33323,#33044,#20338,.T.);
#43030=EDGE_CURVE('',#33112,#33323,#23845,.T.);
#43031=EDGE_CURVE('',#33045,#33323,#20339,.T.);
#43032=EDGE_CURVE('',#33324,#33045,#20340,.T.);
#43033=EDGE_CURVE('',#33116,#33324,#23846,.T.);
#43034=EDGE_CURVE('',#33046,#33324,#20341,.T.);
#43035=EDGE_CURVE('',#33325,#33046,#20342,.T.);
#43036=EDGE_CURVE('',#33120,#33325,#23847,.T.);
#43037=EDGE_CURVE('',#33047,#33325,#20343,.T.);
#43038=EDGE_CURVE('',#33326,#33047,#20344,.T.);
#43039=EDGE_CURVE('',#33124,#33326,#23848,.T.);
#43040=EDGE_CURVE('',#33048,#33326,#20345,.T.);
#43041=EDGE_CURVE('',#33327,#33048,#20346,.T.);
#43042=EDGE_CURVE('',#28923,#33327,#23849,.T.);
#43043=EDGE_CURVE('',#33049,#33327,#20347,.T.);
#43044=EDGE_CURVE('',#33328,#33049,#20348,.T.);
#43045=EDGE_CURVE('',#33128,#33328,#23850,.T.);
#43046=EDGE_CURVE('',#33050,#33328,#20349,.T.);
#43047=EDGE_CURVE('',#33329,#33050,#20350,.T.);
#43048=EDGE_CURVE('',#33132,#33329,#23851,.T.);
#43049=EDGE_CURVE('',#33051,#33329,#20351,.T.);
#43050=EDGE_CURVE('',#33330,#33051,#20352,.T.);
#43051=EDGE_CURVE('',#33136,#33330,#23852,.T.);
#43052=EDGE_CURVE('',#33052,#33330,#20353,.T.);
#43053=EDGE_CURVE('',#33331,#33052,#20354,.T.);
#43054=EDGE_CURVE('',#33140,#33331,#23853,.T.);
#43055=EDGE_CURVE('',#33053,#33331,#20355,.T.);
#43056=EDGE_CURVE('',#33332,#33053,#20356,.T.);
#43057=EDGE_CURVE('',#33144,#33332,#23854,.T.);
#43058=EDGE_CURVE('',#33054,#33332,#20357,.T.);
#43059=EDGE_CURVE('',#33333,#33054,#20358,.T.);
#43060=EDGE_CURVE('',#33148,#33333,#23855,.T.);
#43061=EDGE_CURVE('',#33055,#33333,#20359,.T.);
#43062=EDGE_CURVE('',#33334,#33055,#20360,.T.);
#43063=EDGE_CURVE('',#33152,#33334,#23856,.T.);
#43064=EDGE_CURVE('',#33056,#33334,#20361,.T.);
#43065=EDGE_CURVE('',#33335,#33056,#20362,.T.);
#43066=EDGE_CURVE('',#33156,#33335,#23857,.T.);
#43067=EDGE_CURVE('',#33057,#33335,#20363,.T.);
#43068=EDGE_CURVE('',#33336,#33057,#20364,.T.);
#43069=EDGE_CURVE('',#33160,#33336,#23858,.T.);
#43070=EDGE_CURVE('',#33058,#33336,#20365,.T.);
#43071=EDGE_CURVE('',#33337,#33058,#20366,.T.);
#43072=EDGE_CURVE('',#33164,#33337,#23859,.T.);
#43073=EDGE_CURVE('',#33059,#33337,#20367,.T.);
#43074=EDGE_CURVE('',#33338,#33059,#20368,.T.);
#43075=EDGE_CURVE('',#33169,#33338,#23860,.T.);
#43076=EDGE_CURVE('',#33060,#33338,#20369,.T.);
#43077=EDGE_CURVE('',#33339,#33060,#20370,.T.);
#43078=EDGE_CURVE('',#33173,#33339,#23861,.T.);
#43079=EDGE_CURVE('',#33061,#33339,#20371,.T.);
#43080=EDGE_CURVE('',#33340,#33061,#20372,.T.);
#43081=EDGE_CURVE('',#33176,#33340,#23862,.T.);
#43082=EDGE_CURVE('',#33062,#33340,#20373,.T.);
#43083=EDGE_CURVE('',#33341,#33062,#20374,.T.);
#43084=EDGE_CURVE('',#33180,#33341,#23863,.T.);
#43085=EDGE_CURVE('',#33063,#33341,#20375,.T.);
#43086=EDGE_CURVE('',#33342,#33063,#20376,.T.);
#43087=EDGE_CURVE('',#33184,#33342,#23864,.T.);
#43088=EDGE_CURVE('',#33064,#33342,#20377,.T.);
#43089=EDGE_CURVE('',#33343,#33064,#20378,.T.);
#43090=EDGE_CURVE('',#33188,#33343,#23865,.T.);
#43091=EDGE_CURVE('',#33065,#33343,#20379,.T.);
#43092=EDGE_CURVE('',#33344,#33065,#20380,.T.);
#43093=EDGE_CURVE('',#33192,#33344,#23866,.T.);
#43094=EDGE_CURVE('',#33066,#33344,#20381,.T.);
#43095=EDGE_CURVE('',#33345,#33066,#20382,.T.);
#43096=EDGE_CURVE('',#33196,#33345,#23867,.T.);
#43097=EDGE_CURVE('',#33067,#33345,#20383,.T.);
#43098=EDGE_CURVE('',#33346,#33067,#20384,.T.);
#43099=EDGE_CURVE('',#33200,#33346,#23868,.T.);
#43100=EDGE_CURVE('',#33068,#33346,#20385,.T.);
#43101=EDGE_CURVE('',#33347,#33068,#20386,.T.);
#43102=EDGE_CURVE('',#33204,#33347,#23869,.T.);
#43103=EDGE_CURVE('',#33069,#33347,#20387,.T.);
#43104=EDGE_CURVE('',#33348,#33069,#20388,.T.);
#43105=EDGE_CURVE('',#33208,#33348,#23870,.T.);
#43106=EDGE_CURVE('',#33070,#33348,#20389,.T.);
#43107=EDGE_CURVE('',#33320,#33070,#20390,.T.);
#43108=EDGE_CURVE('',#33071,#33349,#20391,.T.);
#43109=EDGE_CURVE('',#33349,#33319,#23871,.T.);
#43110=EDGE_CURVE('',#33350,#33071,#20392,.T.);
#43111=EDGE_CURVE('',#33216,#33350,#23872,.T.);
#43112=EDGE_CURVE('',#33072,#33350,#20393,.T.);
#43113=EDGE_CURVE('',#33351,#33072,#20394,.T.);
#43114=EDGE_CURVE('',#33220,#33351,#23873,.T.);
#43115=EDGE_CURVE('',#33073,#33351,#20395,.T.);
#43116=EDGE_CURVE('',#33352,#33073,#20396,.T.);
#43117=EDGE_CURVE('',#33224,#33352,#23874,.T.);
#43118=EDGE_CURVE('',#33074,#33352,#20397,.T.);
#43119=EDGE_CURVE('',#33353,#33074,#20398,.T.);
#43120=EDGE_CURVE('',#33228,#33353,#23875,.T.);
#43121=EDGE_CURVE('',#33075,#33353,#20399,.T.);
#43122=EDGE_CURVE('',#33354,#33075,#20400,.T.);
#43123=EDGE_CURVE('',#33232,#33354,#23876,.T.);
#43124=EDGE_CURVE('',#33076,#33354,#20401,.T.);
#43125=EDGE_CURVE('',#33355,#33076,#20402,.T.);
#43126=EDGE_CURVE('',#33236,#33355,#23877,.T.);
#43127=EDGE_CURVE('',#33077,#33355,#20403,.T.);
#43128=EDGE_CURVE('',#33356,#33077,#20404,.T.);
#43129=EDGE_CURVE('',#33240,#33356,#23878,.T.);
#43130=EDGE_CURVE('',#33078,#33356,#20405,.T.);
#43131=EDGE_CURVE('',#33357,#33078,#20406,.T.);
#43132=EDGE_CURVE('',#33244,#33357,#23879,.T.);
#43133=EDGE_CURVE('',#33079,#33357,#20407,.T.);
#43134=EDGE_CURVE('',#33358,#33079,#20408,.T.);
#43135=EDGE_CURVE('',#33248,#33358,#23880,.T.);
#43136=EDGE_CURVE('',#33080,#33358,#20409,.T.);
#43137=EDGE_CURVE('',#33359,#33080,#20410,.T.);
#43138=EDGE_CURVE('',#33252,#33359,#23881,.T.);
#43139=EDGE_CURVE('',#33081,#33359,#20411,.T.);
#43140=EDGE_CURVE('',#33360,#33081,#20412,.T.);
#43141=EDGE_CURVE('',#33256,#33360,#23882,.T.);
#43142=EDGE_CURVE('',#33082,#33360,#20413,.T.);
#43143=EDGE_CURVE('',#33361,#33082,#20414,.T.);
#43144=EDGE_CURVE('',#33260,#33361,#23883,.T.);
#43145=EDGE_CURVE('',#33083,#33361,#20415,.T.);
#43146=EDGE_CURVE('',#33362,#33083,#20416,.T.);
#43147=EDGE_CURVE('',#33264,#33362,#23884,.T.);
#43148=EDGE_CURVE('',#33084,#33362,#20417,.T.);
#43149=EDGE_CURVE('',#33363,#33084,#20418,.T.);
#43150=EDGE_CURVE('',#28917,#33363,#23885,.T.);
#43151=EDGE_CURVE('',#33085,#33363,#20419,.T.);
#43152=EDGE_CURVE('',#33364,#33085,#20420,.T.);
#43153=EDGE_CURVE('',#33268,#33364,#23886,.T.);
#43154=EDGE_CURVE('',#33086,#33364,#20421,.T.);
#43155=EDGE_CURVE('',#33365,#33086,#20422,.T.);
#43156=EDGE_CURVE('',#33272,#33365,#23887,.T.);
#43157=EDGE_CURVE('',#33087,#33365,#20423,.T.);
#43158=EDGE_CURVE('',#33366,#33087,#20424,.T.);
#43159=EDGE_CURVE('',#33276,#33366,#23888,.T.);
#43160=EDGE_CURVE('',#33088,#33366,#20425,.T.);
#43161=EDGE_CURVE('',#33367,#33088,#20426,.T.);
#43162=EDGE_CURVE('',#33280,#33367,#23889,.T.);
#43163=EDGE_CURVE('',#33089,#33367,#20427,.T.);
#43164=EDGE_CURVE('',#33368,#33089,#20428,.T.);
#43165=EDGE_CURVE('',#33284,#33368,#23890,.T.);
#43166=EDGE_CURVE('',#33090,#33368,#20429,.T.);
#43167=EDGE_CURVE('',#33369,#33090,#20430,.T.);
#43168=EDGE_CURVE('',#33288,#33369,#23891,.T.);
#43169=EDGE_CURVE('',#33091,#33369,#20431,.T.);
#43170=EDGE_CURVE('',#33370,#33091,#20432,.T.);
#43171=EDGE_CURVE('',#28913,#33370,#23892,.T.);
#43172=EDGE_CURVE('',#33092,#33370,#20433,.T.);
#43173=EDGE_CURVE('',#33371,#33092,#20434,.T.);
#43174=EDGE_CURVE('',#33292,#33371,#23893,.T.);
#43175=EDGE_CURVE('',#33093,#33371,#20435,.T.);
#43176=EDGE_CURVE('',#33372,#33093,#20436,.T.);
#43177=EDGE_CURVE('',#33296,#33372,#23894,.T.);
#43178=EDGE_CURVE('',#33094,#33372,#20437,.T.);
#43179=EDGE_CURVE('',#33373,#33094,#20438,.T.);
#43180=EDGE_CURVE('',#33300,#33373,#23895,.T.);
#43181=EDGE_CURVE('',#33095,#33373,#20439,.T.);
#43182=EDGE_CURVE('',#33374,#33095,#20440,.T.);
#43183=EDGE_CURVE('',#33304,#33374,#23896,.T.);
#43184=EDGE_CURVE('',#33096,#33374,#20441,.T.);
#43185=EDGE_CURVE('',#33375,#33096,#20442,.T.);
#43186=EDGE_CURVE('',#33308,#33375,#23897,.T.);
#43187=EDGE_CURVE('',#33097,#33375,#20443,.T.);
#43188=EDGE_CURVE('',#33376,#33097,#20444,.T.);
#43189=EDGE_CURVE('',#33312,#33376,#23898,.T.);
#43190=EDGE_CURVE('',#33098,#33376,#20445,.T.);
#43191=EDGE_CURVE('',#33377,#33098,#20446,.T.);
#43192=EDGE_CURVE('',#33316,#33377,#23899,.T.);
#43193=EDGE_CURVE('',#33099,#33377,#20447,.T.);
#43194=EDGE_CURVE('',#33349,#33099,#20448,.T.);
#43195=EDGE_CURVE('',#33378,#33379,#20449,.T.);
#43196=EDGE_CURVE('',#33042,#33379,#23900,.T.);
#43197=EDGE_CURVE('',#33378,#33320,#26104,.T.);
#43198=EDGE_CURVE('',#33380,#33378,#20450,.T.);
#43199=EDGE_CURVE('',#33381,#33380,#20451,.T.);
#43200=EDGE_CURVE('',#33379,#33381,#20452,.T.);
#43201=EDGE_CURVE('',#33321,#33381,#26105,.T.);
#43202=EDGE_CURVE('',#33382,#33383,#20453,.T.);
#43203=EDGE_CURVE('',#33043,#33383,#23901,.T.);
#43204=EDGE_CURVE('',#33382,#33321,#26106,.T.);
#43205=EDGE_CURVE('',#33384,#33382,#20454,.T.);
#43206=EDGE_CURVE('',#33385,#33384,#20455,.T.);
#43207=EDGE_CURVE('',#33383,#33385,#20456,.T.);
#43208=EDGE_CURVE('',#33322,#33385,#26107,.T.);
#43209=EDGE_CURVE('',#33386,#33387,#20457,.T.);
#43210=EDGE_CURVE('',#33044,#33387,#23902,.T.);
#43211=EDGE_CURVE('',#33386,#33322,#26108,.T.);
#43212=EDGE_CURVE('',#33388,#33386,#20458,.T.);
#43213=EDGE_CURVE('',#33389,#33388,#20459,.T.);
#43214=EDGE_CURVE('',#33387,#33389,#20460,.T.);
#43215=EDGE_CURVE('',#33323,#33389,#26109,.T.);
#43216=EDGE_CURVE('',#33390,#33391,#20461,.T.);
#43217=EDGE_CURVE('',#33045,#33391,#23903,.T.);
#43218=EDGE_CURVE('',#33390,#33323,#26110,.T.);
#43219=EDGE_CURVE('',#33392,#33390,#20462,.T.);
#43220=EDGE_CURVE('',#33393,#33392,#20463,.T.);
#43221=EDGE_CURVE('',#33391,#33393,#20464,.T.);
#43222=EDGE_CURVE('',#33324,#33393,#26111,.T.);
#43223=EDGE_CURVE('',#33394,#33395,#20465,.T.);
#43224=EDGE_CURVE('',#33046,#33395,#23904,.T.);
#43225=EDGE_CURVE('',#33394,#33324,#26112,.T.);
#43226=EDGE_CURVE('',#33396,#33394,#20466,.T.);
#43227=EDGE_CURVE('',#33397,#33396,#20467,.T.);
#43228=EDGE_CURVE('',#33395,#33397,#20468,.T.);
#43229=EDGE_CURVE('',#33325,#33397,#26113,.T.);
#43230=EDGE_CURVE('',#33398,#33399,#20469,.T.);
#43231=EDGE_CURVE('',#33047,#33399,#23905,.T.);
#43232=EDGE_CURVE('',#33398,#33325,#26114,.T.);
#43233=EDGE_CURVE('',#33400,#33398,#20470,.T.);
#43234=EDGE_CURVE('',#33401,#33400,#20471,.T.);
#43235=EDGE_CURVE('',#33399,#33401,#20472,.T.);
#43236=EDGE_CURVE('',#33326,#33401,#26115,.T.);
#43237=EDGE_CURVE('',#33402,#33403,#20473,.T.);
#43238=EDGE_CURVE('',#33048,#33403,#23906,.T.);
#43239=EDGE_CURVE('',#33402,#33326,#26116,.T.);
#43240=EDGE_CURVE('',#33404,#33402,#20474,.T.);
#43241=EDGE_CURVE('',#33405,#33404,#20475,.T.);
#43242=EDGE_CURVE('',#33403,#33405,#20476,.T.);
#43243=EDGE_CURVE('',#33327,#33405,#26117,.T.);
#43244=EDGE_CURVE('',#33406,#33407,#20477,.T.);
#43245=EDGE_CURVE('',#33049,#33407,#23907,.T.);
#43246=EDGE_CURVE('',#33406,#33327,#26118,.T.);
#43247=EDGE_CURVE('',#33408,#33406,#20478,.T.);
#43248=EDGE_CURVE('',#33409,#33408,#20479,.T.);
#43249=EDGE_CURVE('',#33407,#33409,#20480,.T.);
#43250=EDGE_CURVE('',#33328,#33409,#26119,.T.);
#43251=EDGE_CURVE('',#33410,#33411,#20481,.T.);
#43252=EDGE_CURVE('',#33050,#33411,#23908,.T.);
#43253=EDGE_CURVE('',#33410,#33328,#26120,.T.);
#43254=EDGE_CURVE('',#33412,#33410,#20482,.T.);
#43255=EDGE_CURVE('',#33413,#33412,#20483,.T.);
#43256=EDGE_CURVE('',#33411,#33413,#20484,.T.);
#43257=EDGE_CURVE('',#33329,#33413,#26121,.T.);
#43258=EDGE_CURVE('',#33414,#33415,#20485,.T.);
#43259=EDGE_CURVE('',#33051,#33415,#23909,.T.);
#43260=EDGE_CURVE('',#33414,#33329,#26122,.T.);
#43261=EDGE_CURVE('',#33416,#33414,#20486,.T.);
#43262=EDGE_CURVE('',#33417,#33416,#20487,.T.);
#43263=EDGE_CURVE('',#33415,#33417,#20488,.T.);
#43264=EDGE_CURVE('',#33330,#33417,#26123,.T.);
#43265=EDGE_CURVE('',#33418,#33419,#20489,.T.);
#43266=EDGE_CURVE('',#33052,#33419,#23910,.T.);
#43267=EDGE_CURVE('',#33418,#33330,#26124,.T.);
#43268=EDGE_CURVE('',#33420,#33418,#20490,.T.);
#43269=EDGE_CURVE('',#33421,#33420,#20491,.T.);
#43270=EDGE_CURVE('',#33419,#33421,#20492,.T.);
#43271=EDGE_CURVE('',#33331,#33421,#26125,.T.);
#43272=EDGE_CURVE('',#33422,#33423,#20493,.T.);
#43273=EDGE_CURVE('',#33053,#33423,#23911,.T.);
#43274=EDGE_CURVE('',#33422,#33331,#26126,.T.);
#43275=EDGE_CURVE('',#33424,#33422,#20494,.T.);
#43276=EDGE_CURVE('',#33425,#33424,#20495,.T.);
#43277=EDGE_CURVE('',#33423,#33425,#20496,.T.);
#43278=EDGE_CURVE('',#33332,#33425,#26127,.T.);
#43279=EDGE_CURVE('',#33426,#33427,#20497,.T.);
#43280=EDGE_CURVE('',#33054,#33427,#23912,.T.);
#43281=EDGE_CURVE('',#33426,#33332,#26128,.T.);
#43282=EDGE_CURVE('',#33428,#33426,#20498,.T.);
#43283=EDGE_CURVE('',#33429,#33428,#20499,.T.);
#43284=EDGE_CURVE('',#33427,#33429,#20500,.T.);
#43285=EDGE_CURVE('',#33333,#33429,#26129,.T.);
#43286=EDGE_CURVE('',#33430,#33431,#20501,.T.);
#43287=EDGE_CURVE('',#33055,#33431,#23913,.T.);
#43288=EDGE_CURVE('',#33430,#33333,#26130,.T.);
#43289=EDGE_CURVE('',#33432,#33430,#20502,.T.);
#43290=EDGE_CURVE('',#33433,#33432,#20503,.T.);
#43291=EDGE_CURVE('',#33431,#33433,#20504,.T.);
#43292=EDGE_CURVE('',#33334,#33433,#26131,.T.);
#43293=EDGE_CURVE('',#33056,#28909,#23914,.T.);
#43294=EDGE_CURVE('',#28908,#33334,#26132,.T.);
#43295=EDGE_CURVE('',#33335,#28911,#26133,.T.);
#43296=EDGE_CURVE('',#33434,#33435,#20505,.T.);
#43297=EDGE_CURVE('',#33057,#33435,#23915,.T.);
#43298=EDGE_CURVE('',#33434,#33335,#26134,.T.);
#43299=EDGE_CURVE('',#33436,#33434,#20506,.T.);
#43300=EDGE_CURVE('',#33437,#33436,#20507,.T.);
#43301=EDGE_CURVE('',#33435,#33437,#20508,.T.);
#43302=EDGE_CURVE('',#33336,#33437,#26135,.T.);
#43303=EDGE_CURVE('',#33438,#33439,#20509,.T.);
#43304=EDGE_CURVE('',#33058,#33439,#23916,.T.);
#43305=EDGE_CURVE('',#33438,#33336,#26136,.T.);
#43306=EDGE_CURVE('',#33440,#33438,#20510,.T.);
#43307=EDGE_CURVE('',#33441,#33440,#20511,.T.);
#43308=EDGE_CURVE('',#33439,#33441,#20512,.T.);
#43309=EDGE_CURVE('',#33337,#33441,#26137,.T.);
#43310=EDGE_CURVE('',#33442,#33443,#20513,.T.);
#43311=EDGE_CURVE('',#33059,#33443,#23917,.T.);
#43312=EDGE_CURVE('',#33442,#33337,#26138,.T.);
#43313=EDGE_CURVE('',#33443,#33444,#20514,.T.);
#43314=EDGE_CURVE('',#33338,#33444,#26139,.T.);
#43315=EDGE_CURVE('',#33445,#33442,#20515,.T.);
#43316=EDGE_CURVE('',#33444,#33445,#20516,.T.);
#43317=EDGE_CURVE('',#33446,#33338,#26140,.T.);
#43318=EDGE_CURVE('',#33446,#33447,#20517,.T.);
#43319=EDGE_CURVE('',#33060,#33447,#23918,.T.);
#43320=EDGE_CURVE('',#33447,#33448,#20518,.T.);
#43321=EDGE_CURVE('',#33449,#33446,#20519,.T.);
#43322=EDGE_CURVE('',#33448,#33449,#20520,.T.);
#43323=EDGE_CURVE('',#33339,#33448,#26141,.T.);
#43324=EDGE_CURVE('',#33450,#33451,#20521,.T.);
#43325=EDGE_CURVE('',#33061,#33451,#23919,.T.);
#43326=EDGE_CURVE('',#33450,#33339,#26142,.T.);
#43327=EDGE_CURVE('',#33452,#33450,#20522,.T.);
#43328=EDGE_CURVE('',#33453,#33452,#20523,.T.);
#43329=EDGE_CURVE('',#33451,#33453,#20524,.T.);
#43330=EDGE_CURVE('',#33340,#33453,#26143,.T.);
#43331=EDGE_CURVE('',#33454,#33455,#20525,.T.);
#43332=EDGE_CURVE('',#33062,#33455,#23920,.T.);
#43333=EDGE_CURVE('',#33454,#33340,#26144,.T.);
#43334=EDGE_CURVE('',#33456,#33454,#20526,.T.);
#43335=EDGE_CURVE('',#33457,#33456,#20527,.T.);
#43336=EDGE_CURVE('',#33455,#33457,#20528,.T.);
#43337=EDGE_CURVE('',#33341,#33457,#26145,.T.);
#43338=EDGE_CURVE('',#33458,#33459,#20529,.T.);
#43339=EDGE_CURVE('',#33063,#33459,#23921,.T.);
#43340=EDGE_CURVE('',#33458,#33341,#26146,.T.);
#43341=EDGE_CURVE('',#33460,#33458,#20530,.T.);
#43342=EDGE_CURVE('',#33461,#33460,#20531,.T.);
#43343=EDGE_CURVE('',#33459,#33461,#20532,.T.);
#43344=EDGE_CURVE('',#33342,#33461,#26147,.T.);
#43345=EDGE_CURVE('',#33462,#33463,#20533,.T.);
#43346=EDGE_CURVE('',#33064,#33463,#23922,.T.);
#43347=EDGE_CURVE('',#33462,#33342,#26148,.T.);
#43348=EDGE_CURVE('',#33464,#33462,#20534,.T.);
#43349=EDGE_CURVE('',#33465,#33464,#20535,.T.);
#43350=EDGE_CURVE('',#33463,#33465,#20536,.T.);
#43351=EDGE_CURVE('',#33343,#33465,#26149,.T.);
#43352=EDGE_CURVE('',#33466,#33467,#20537,.T.);
#43353=EDGE_CURVE('',#33065,#33467,#23923,.T.);
#43354=EDGE_CURVE('',#33466,#33343,#26150,.T.);
#43355=EDGE_CURVE('',#33468,#33466,#20538,.T.);
#43356=EDGE_CURVE('',#33469,#33468,#20539,.T.);
#43357=EDGE_CURVE('',#33467,#33469,#20540,.T.);
#43358=EDGE_CURVE('',#33344,#33469,#26151,.T.);
#43359=EDGE_CURVE('',#33470,#33471,#20541,.T.);
#43360=EDGE_CURVE('',#33066,#33471,#23924,.T.);
#43361=EDGE_CURVE('',#33470,#33344,#26152,.T.);
#43362=EDGE_CURVE('',#33472,#33470,#20542,.T.);
#43363=EDGE_CURVE('',#33473,#33472,#20543,.T.);
#43364=EDGE_CURVE('',#33471,#33473,#20544,.T.);
#43365=EDGE_CURVE('',#33345,#33473,#26153,.T.);
#43366=EDGE_CURVE('',#33474,#33475,#20545,.T.);
#43367=EDGE_CURVE('',#33067,#33475,#23925,.T.);
#43368=EDGE_CURVE('',#33474,#33345,#26154,.T.);
#43369=EDGE_CURVE('',#33476,#33474,#20546,.T.);
#43370=EDGE_CURVE('',#33477,#33476,#20547,.T.);
#43371=EDGE_CURVE('',#33475,#33477,#20548,.T.);
#43372=EDGE_CURVE('',#33346,#33477,#26155,.T.);
#43373=EDGE_CURVE('',#33478,#33479,#20549,.T.);
#43374=EDGE_CURVE('',#33068,#33479,#23926,.T.);
#43375=EDGE_CURVE('',#33478,#33346,#26156,.T.);
#43376=EDGE_CURVE('',#33480,#33478,#20550,.T.);
#43377=EDGE_CURVE('',#33481,#33480,#20551,.T.);
#43378=EDGE_CURVE('',#33479,#33481,#20552,.T.);
#43379=EDGE_CURVE('',#33347,#33481,#26157,.T.);
#43380=EDGE_CURVE('',#33482,#33483,#20553,.T.);
#43381=EDGE_CURVE('',#33069,#33483,#23927,.T.);
#43382=EDGE_CURVE('',#33482,#33347,#26158,.T.);
#43383=EDGE_CURVE('',#33484,#33482,#20554,.T.);
#43384=EDGE_CURVE('',#33485,#33484,#20555,.T.);
#43385=EDGE_CURVE('',#33483,#33485,#20556,.T.);
#43386=EDGE_CURVE('',#33348,#33485,#26159,.T.);
#43387=EDGE_CURVE('',#33486,#33487,#20557,.T.);
#43388=EDGE_CURVE('',#33070,#33487,#23928,.T.);
#43389=EDGE_CURVE('',#33486,#33348,#26160,.T.);
#43390=EDGE_CURVE('',#33488,#33486,#20558,.T.);
#43391=EDGE_CURVE('',#33489,#33488,#20559,.T.);
#43392=EDGE_CURVE('',#33487,#33489,#20560,.T.);
#43393=EDGE_CURVE('',#33320,#33489,#26161,.T.);
#43394=EDGE_CURVE('',#33349,#28805,#20561,.T.);
#43395=EDGE_CURVE('',#28806,#33349,#26162,.T.);
#43396=EDGE_CURVE('',#33349,#28804,#23929,.T.);
#43397=EDGE_CURVE('',#33349,#28803,#23930,.T.);
#43398=EDGE_CURVE('',#33349,#28802,#26163,.T.);
#43399=EDGE_CURVE('',#33071,#28801,#23931,.T.);
#43400=EDGE_CURVE('',#33350,#28800,#26164,.T.);
#43401=EDGE_CURVE('',#33350,#28799,#20562,.T.);
#43402=EDGE_CURVE('',#33350,#28798,#23932,.T.);
#43403=EDGE_CURVE('',#33350,#28797,#23933,.T.);
#43404=EDGE_CURVE('',#33350,#28796,#26165,.T.);
#43405=EDGE_CURVE('',#33072,#28795,#23934,.T.);
#43406=EDGE_CURVE('',#33351,#28794,#26166,.T.);
#43407=EDGE_CURVE('',#33351,#28793,#20563,.T.);
#43408=EDGE_CURVE('',#33351,#28792,#23935,.T.);
#43409=EDGE_CURVE('',#33351,#28791,#23936,.T.);
#43410=EDGE_CURVE('',#33351,#28790,#26167,.T.);
#43411=EDGE_CURVE('',#33073,#28789,#23937,.T.);
#43412=EDGE_CURVE('',#33352,#28788,#26168,.T.);
#43413=EDGE_CURVE('',#33352,#28787,#20564,.T.);
#43414=EDGE_CURVE('',#33352,#28786,#23938,.T.);
#43415=EDGE_CURVE('',#33352,#28785,#23939,.T.);
#43416=EDGE_CURVE('',#33352,#28784,#26169,.T.);
#43417=EDGE_CURVE('',#33074,#28783,#23940,.T.);
#43418=EDGE_CURVE('',#33353,#28782,#26170,.T.);
#43419=EDGE_CURVE('',#33353,#28781,#20565,.T.);
#43420=EDGE_CURVE('',#33353,#28780,#23941,.T.);
#43421=EDGE_CURVE('',#33353,#28779,#4456,.T.);
#43422=EDGE_CURVE('',#33353,#28778,#26171,.T.);
#43423=EDGE_CURVE('',#33075,#28777,#23942,.T.);
#43424=EDGE_CURVE('',#33354,#28776,#26172,.T.);
#43425=EDGE_CURVE('',#33354,#28775,#20566,.T.);
#43426=EDGE_CURVE('',#33354,#28774,#23943,.T.);
#43427=EDGE_CURVE('',#33354,#28773,#23944,.T.);
#43428=EDGE_CURVE('',#33354,#28772,#26173,.T.);
#43429=EDGE_CURVE('',#33076,#28771,#23945,.T.);
#43430=EDGE_CURVE('',#33355,#28770,#26174,.T.);
#43431=EDGE_CURVE('',#33355,#28769,#20567,.T.);
#43432=EDGE_CURVE('',#33355,#28768,#23946,.T.);
#43433=EDGE_CURVE('',#33355,#28767,#23947,.T.);
#43434=EDGE_CURVE('',#33355,#28766,#26175,.T.);
#43435=EDGE_CURVE('',#33077,#28765,#23948,.T.);
#43436=EDGE_CURVE('',#33356,#28764,#26176,.T.);
#43437=EDGE_CURVE('',#33356,#28763,#20568,.T.);
#43438=EDGE_CURVE('',#33356,#28762,#23949,.T.);
#43439=EDGE_CURVE('',#33356,#28761,#23950,.T.);
#43440=EDGE_CURVE('',#33356,#28760,#26177,.T.);
#43441=EDGE_CURVE('',#33078,#28759,#23951,.T.);
#43442=EDGE_CURVE('',#33357,#28758,#26178,.T.);
#43443=EDGE_CURVE('',#33357,#28757,#20569,.T.);
#43444=EDGE_CURVE('',#33357,#28756,#23952,.T.);
#43445=EDGE_CURVE('',#33357,#28755,#23953,.T.);
#43446=EDGE_CURVE('',#33357,#28754,#26179,.T.);
#43447=EDGE_CURVE('',#33079,#28753,#23954,.T.);
#43448=EDGE_CURVE('',#33358,#28752,#26180,.T.);
#43449=EDGE_CURVE('',#33358,#28751,#20570,.T.);
#43450=EDGE_CURVE('',#33358,#28750,#23955,.T.);
#43451=EDGE_CURVE('',#33358,#28749,#23956,.T.);
#43452=EDGE_CURVE('',#33358,#28748,#26181,.T.);
#43453=EDGE_CURVE('',#33080,#28747,#23957,.T.);
#43454=EDGE_CURVE('',#33359,#28746,#26182,.T.);
#43455=EDGE_CURVE('',#33359,#28745,#20571,.T.);
#43456=EDGE_CURVE('',#33359,#28744,#23958,.T.);
#43457=EDGE_CURVE('',#33359,#28743,#23959,.T.);
#43458=EDGE_CURVE('',#33359,#28742,#26183,.T.);
#43459=EDGE_CURVE('',#33081,#28741,#23960,.T.);
#43460=EDGE_CURVE('',#33360,#28740,#26184,.T.);
#43461=EDGE_CURVE('',#33360,#28739,#20572,.T.);
#43462=EDGE_CURVE('',#33360,#28738,#23961,.T.);
#43463=EDGE_CURVE('',#33360,#28737,#23962,.T.);
#43464=EDGE_CURVE('',#33360,#28736,#26185,.T.);
#43465=EDGE_CURVE('',#33082,#28735,#23963,.T.);
#43466=EDGE_CURVE('',#33361,#28734,#26186,.T.);
#43467=EDGE_CURVE('',#33361,#28733,#20573,.T.);
#43468=EDGE_CURVE('',#33361,#28732,#23964,.T.);
#43469=EDGE_CURVE('',#33361,#28731,#23965,.T.);
#43470=EDGE_CURVE('',#33361,#28730,#26187,.T.);
#43471=EDGE_CURVE('',#33083,#28729,#23966,.T.);
#43472=EDGE_CURVE('',#33362,#28728,#26188,.T.);
#43473=EDGE_CURVE('',#33362,#28727,#20574,.T.);
#43474=EDGE_CURVE('',#33362,#28726,#23967,.T.);
#43475=EDGE_CURVE('',#33362,#28725,#23968,.T.);
#43476=EDGE_CURVE('',#33362,#28724,#26189,.T.);
#43477=EDGE_CURVE('',#33084,#28723,#23969,.T.);
#43478=EDGE_CURVE('',#33363,#28722,#26190,.T.);
#43479=EDGE_CURVE('',#33363,#28721,#20575,.T.);
#43480=EDGE_CURVE('',#33363,#28719,#23970,.T.);
#43481=EDGE_CURVE('',#33363,#28720,#23971,.T.);
#43482=EDGE_CURVE('',#33363,#28894,#26191,.T.);
#43483=EDGE_CURVE('',#33085,#28893,#23972,.T.);
#43484=EDGE_CURVE('',#33364,#28892,#26192,.T.);
#43485=EDGE_CURVE('',#33364,#28891,#20576,.T.);
#43486=EDGE_CURVE('',#33364,#28890,#23973,.T.);
#43487=EDGE_CURVE('',#33364,#28889,#23974,.T.);
#43488=EDGE_CURVE('',#33364,#28888,#26193,.T.);
#43489=EDGE_CURVE('',#33086,#28887,#23975,.T.);
#43490=EDGE_CURVE('',#33365,#28886,#26194,.T.);
#43491=EDGE_CURVE('',#33365,#28885,#20577,.T.);
#43492=EDGE_CURVE('',#33365,#28884,#23976,.T.);
#43493=EDGE_CURVE('',#33365,#28883,#23977,.T.);
#43494=EDGE_CURVE('',#33365,#28882,#26195,.T.);
#43495=EDGE_CURVE('',#33087,#28881,#23978,.T.);
#43496=EDGE_CURVE('',#33366,#28880,#26196,.T.);
#43497=EDGE_CURVE('',#33366,#28879,#20578,.T.);
#43498=EDGE_CURVE('',#33366,#28878,#23979,.T.);
#43499=EDGE_CURVE('',#33366,#28877,#23980,.T.);
#43500=EDGE_CURVE('',#33366,#28876,#26197,.T.);
#43501=EDGE_CURVE('',#33088,#28875,#23981,.T.);
#43502=EDGE_CURVE('',#33367,#28874,#26198,.T.);
#43503=EDGE_CURVE('',#33367,#28873,#20579,.T.);
#43504=EDGE_CURVE('',#33367,#28872,#23982,.T.);
#43505=EDGE_CURVE('',#33367,#28871,#23983,.T.);
#43506=EDGE_CURVE('',#33367,#28870,#26199,.T.);
#43507=EDGE_CURVE('',#33089,#28869,#23984,.T.);
#43508=EDGE_CURVE('',#33368,#28868,#26200,.T.);
#43509=EDGE_CURVE('',#33368,#28867,#20580,.T.);
#43510=EDGE_CURVE('',#33368,#28866,#23985,.T.);
#43511=EDGE_CURVE('',#33368,#28865,#23986,.T.);
#43512=EDGE_CURVE('',#33368,#28864,#26201,.T.);
#43513=EDGE_CURVE('',#33090,#28863,#23987,.T.);
#43514=EDGE_CURVE('',#33369,#28862,#26202,.T.);
#43515=EDGE_CURVE('',#33369,#28861,#20581,.T.);
#43516=EDGE_CURVE('',#33369,#28860,#23988,.T.);
#43517=EDGE_CURVE('',#33369,#28859,#23989,.T.);
#43518=EDGE_CURVE('',#33369,#28858,#26203,.T.);
#43519=EDGE_CURVE('',#33091,#28857,#23990,.T.);
#43520=EDGE_CURVE('',#33370,#28856,#26204,.T.);
#43521=EDGE_CURVE('',#33370,#28855,#20582,.T.);
#43522=EDGE_CURVE('',#33370,#28854,#23991,.T.);
#43523=EDGE_CURVE('',#33370,#28853,#23992,.T.);
#43524=EDGE_CURVE('',#33370,#28852,#26205,.T.);
#43525=EDGE_CURVE('',#33092,#28851,#23993,.T.);
#43526=EDGE_CURVE('',#33371,#28850,#26206,.T.);
#43527=EDGE_CURVE('',#33371,#28849,#20583,.T.);
#43528=EDGE_CURVE('',#33371,#28848,#23994,.T.);
#43529=EDGE_CURVE('',#33371,#28847,#23995,.T.);
#43530=EDGE_CURVE('',#33371,#28846,#26207,.T.);
#43531=EDGE_CURVE('',#33093,#28845,#23996,.T.);
#43532=EDGE_CURVE('',#33372,#28844,#26208,.T.);
#43533=EDGE_CURVE('',#33372,#28843,#20584,.T.);
#43534=EDGE_CURVE('',#33372,#28842,#23997,.T.);
#43535=EDGE_CURVE('',#33372,#28841,#23998,.T.);
#43536=EDGE_CURVE('',#33372,#28840,#26209,.T.);
#43537=EDGE_CURVE('',#33094,#28839,#23999,.T.);
#43538=EDGE_CURVE('',#33373,#28838,#26210,.T.);
#43539=EDGE_CURVE('',#33373,#28837,#20585,.T.);
#43540=EDGE_CURVE('',#33373,#28836,#24000,.T.);
#43541=EDGE_CURVE('',#33373,#28835,#24001,.T.);
#43542=EDGE_CURVE('',#33373,#28834,#26211,.T.);
#43543=EDGE_CURVE('',#33095,#28833,#24002,.T.);
#43544=EDGE_CURVE('',#33374,#28832,#26212,.T.);
#43545=EDGE_CURVE('',#33374,#28831,#20586,.T.);
#43546=EDGE_CURVE('',#33374,#28830,#24003,.T.);
#43547=EDGE_CURVE('',#33374,#28829,#24004,.T.);
#43548=EDGE_CURVE('',#33374,#28828,#26213,.T.);
#43549=EDGE_CURVE('',#33096,#28827,#24005,.T.);
#43550=EDGE_CURVE('',#33375,#28826,#26214,.T.);
#43551=EDGE_CURVE('',#33375,#28825,#20587,.T.);
#43552=EDGE_CURVE('',#33375,#28824,#24006,.T.);
#43553=EDGE_CURVE('',#33375,#28823,#24007,.T.);
#43554=EDGE_CURVE('',#33375,#28822,#26215,.T.);
#43555=EDGE_CURVE('',#33097,#28821,#24008,.T.);
#43556=EDGE_CURVE('',#33376,#28820,#26216,.T.);
#43557=EDGE_CURVE('',#33376,#28819,#20588,.T.);
#43558=EDGE_CURVE('',#33376,#28818,#24009,.T.);
#43559=EDGE_CURVE('',#33376,#28817,#24010,.T.);
#43560=EDGE_CURVE('',#33376,#28816,#26217,.T.);
#43561=EDGE_CURVE('',#33098,#28815,#24011,.T.);
#43562=EDGE_CURVE('',#33377,#28814,#26218,.T.);
#43563=EDGE_CURVE('',#33377,#28813,#20589,.T.);
#43564=EDGE_CURVE('',#33377,#28812,#24012,.T.);
#43565=EDGE_CURVE('',#33377,#28811,#24013,.T.);
#43566=EDGE_CURVE('',#33377,#28810,#26219,.T.);
#43567=EDGE_CURVE('',#33099,#28809,#24014,.T.);
#43568=EDGE_CURVE('',#33490,#33320,#20590,.T.);
#43569=EDGE_CURVE('',#33380,#33490,#24015,.T.);
#43570=EDGE_CURVE('',#33321,#33490,#20591,.T.);
#43571=EDGE_CURVE('',#33491,#33321,#20592,.T.);
#43572=EDGE_CURVE('',#33384,#33491,#24016,.T.);
#43573=EDGE_CURVE('',#33322,#33491,#20593,.T.);
#43574=EDGE_CURVE('',#33492,#33322,#20594,.T.);
#43575=EDGE_CURVE('',#33388,#33492,#24017,.T.);
#43576=EDGE_CURVE('',#33323,#33492,#20595,.T.);
#43577=EDGE_CURVE('',#33493,#33323,#20596,.T.);
#43578=EDGE_CURVE('',#33392,#33493,#24018,.T.);
#43579=EDGE_CURVE('',#33324,#33493,#20597,.T.);
#43580=EDGE_CURVE('',#33494,#33324,#20598,.T.);
#43581=EDGE_CURVE('',#33396,#33494,#24019,.T.);
#43582=EDGE_CURVE('',#33325,#33494,#20599,.T.);
#43583=EDGE_CURVE('',#33495,#33325,#20600,.T.);
#43584=EDGE_CURVE('',#33400,#33495,#24020,.T.);
#43585=EDGE_CURVE('',#33326,#33495,#20601,.T.);
#43586=EDGE_CURVE('',#33496,#33326,#20602,.T.);
#43587=EDGE_CURVE('',#33404,#33496,#24021,.T.);
#43588=EDGE_CURVE('',#33327,#33496,#20603,.T.);
#43589=EDGE_CURVE('',#33497,#33327,#20604,.T.);
#43590=EDGE_CURVE('',#33408,#33497,#24022,.T.);
#43591=EDGE_CURVE('',#33328,#33497,#20605,.T.);
#43592=EDGE_CURVE('',#33498,#33328,#20606,.T.);
#43593=EDGE_CURVE('',#33412,#33498,#24023,.T.);
#43594=EDGE_CURVE('',#33329,#33498,#20607,.T.);
#43595=EDGE_CURVE('',#33499,#33329,#20608,.T.);
#43596=EDGE_CURVE('',#33416,#33499,#24024,.T.);
#43597=EDGE_CURVE('',#33330,#33499,#20609,.T.);
#43598=EDGE_CURVE('',#33500,#33330,#20610,.T.);
#43599=EDGE_CURVE('',#33420,#33500,#24025,.T.);
#43600=EDGE_CURVE('',#33331,#33500,#20611,.T.);
#43601=EDGE_CURVE('',#33501,#33331,#20612,.T.);
#43602=EDGE_CURVE('',#33424,#33501,#24026,.T.);
#43603=EDGE_CURVE('',#33332,#33501,#20613,.T.);
#43604=EDGE_CURVE('',#33502,#33332,#20614,.T.);
#43605=EDGE_CURVE('',#33428,#33502,#24027,.T.);
#43606=EDGE_CURVE('',#33333,#33502,#20615,.T.);
#43607=EDGE_CURVE('',#33503,#33333,#20616,.T.);
#43608=EDGE_CURVE('',#33432,#33503,#24028,.T.);
#43609=EDGE_CURVE('',#33334,#33503,#20617,.T.);
#43610=EDGE_CURVE('',#33504,#33334,#20618,.T.);
#43611=EDGE_CURVE('',#28910,#33504,#24029,.T.);
#43612=EDGE_CURVE('',#33335,#33504,#20619,.T.);
#43613=EDGE_CURVE('',#33505,#33335,#20620,.T.);
#43614=EDGE_CURVE('',#33436,#33505,#24030,.T.);
#43615=EDGE_CURVE('',#33336,#33505,#20621,.T.);
#43616=EDGE_CURVE('',#33506,#33336,#20622,.T.);
#43617=EDGE_CURVE('',#33440,#33506,#24031,.T.);
#43618=EDGE_CURVE('',#33337,#33506,#20623,.T.);
#43619=EDGE_CURVE('',#33507,#33337,#20624,.T.);
#43620=EDGE_CURVE('',#33445,#33507,#24032,.T.);
#43621=EDGE_CURVE('',#33338,#33507,#20625,.T.);
#43622=EDGE_CURVE('',#33508,#33338,#20626,.T.);
#43623=EDGE_CURVE('',#33449,#33508,#24033,.T.);
#43624=EDGE_CURVE('',#33339,#33508,#20627,.T.);
#43625=EDGE_CURVE('',#33509,#33339,#20628,.T.);
#43626=EDGE_CURVE('',#33452,#33509,#24034,.T.);
#43627=EDGE_CURVE('',#33340,#33509,#20629,.T.);
#43628=EDGE_CURVE('',#33510,#33340,#20630,.T.);
#43629=EDGE_CURVE('',#33456,#33510,#24035,.T.);
#43630=EDGE_CURVE('',#33341,#33510,#20631,.T.);
#43631=EDGE_CURVE('',#33511,#33341,#20632,.T.);
#43632=EDGE_CURVE('',#33460,#33511,#24036,.T.);
#43633=EDGE_CURVE('',#33342,#33511,#20633,.T.);
#43634=EDGE_CURVE('',#33512,#33342,#20634,.T.);
#43635=EDGE_CURVE('',#33464,#33512,#24037,.T.);
#43636=EDGE_CURVE('',#33343,#33512,#20635,.T.);
#43637=EDGE_CURVE('',#33513,#33343,#20636,.T.);
#43638=EDGE_CURVE('',#33468,#33513,#24038,.T.);
#43639=EDGE_CURVE('',#33344,#33513,#20637,.T.);
#43640=EDGE_CURVE('',#33514,#33344,#20638,.T.);
#43641=EDGE_CURVE('',#33472,#33514,#24039,.T.);
#43642=EDGE_CURVE('',#33345,#33514,#20639,.T.);
#43643=EDGE_CURVE('',#33515,#33345,#20640,.T.);
#43644=EDGE_CURVE('',#33476,#33515,#24040,.T.);
#43645=EDGE_CURVE('',#33346,#33515,#20641,.T.);
#43646=EDGE_CURVE('',#33516,#33346,#20642,.T.);
#43647=EDGE_CURVE('',#33480,#33516,#24041,.T.);
#43648=EDGE_CURVE('',#33347,#33516,#20643,.T.);
#43649=EDGE_CURVE('',#33517,#33347,#20644,.T.);
#43650=EDGE_CURVE('',#33484,#33517,#24042,.T.);
#43651=EDGE_CURVE('',#33348,#33517,#20645,.T.);
#43652=EDGE_CURVE('',#33518,#33348,#20646,.T.);
#43653=EDGE_CURVE('',#33488,#33518,#24043,.T.);
#43654=EDGE_CURVE('',#33320,#33518,#20647,.T.);
#43655=EDGE_CURVE('',#33519,#33520,#20648,.T.);
#43656=EDGE_CURVE('',#33490,#33520,#26220,.T.);
#43657=EDGE_CURVE('',#33519,#33320,#24044,.T.);
#43658=EDGE_CURVE('',#33521,#33522,#20649,.T.);
#43659=EDGE_CURVE('',#33321,#33522,#24045,.T.);
#43660=EDGE_CURVE('',#33521,#33490,#26221,.T.);
#43661=EDGE_CURVE('',#33523,#33524,#20650,.T.);
#43662=EDGE_CURVE('',#33523,#33525,#20651,.T.);
#43663=EDGE_CURVE('',#33524,#33525,#20652,.T.);
#43664=EDGE_CURVE('',#33522,#33526,#20653,.T.);
#43665=EDGE_CURVE('',#33491,#33526,#26222,.T.);
#43666=EDGE_CURVE('',#33526,#33523,#20654,.T.);
#43667=EDGE_CURVE('',#33525,#33521,#20655,.T.);
#43668=EDGE_CURVE('',#33527,#33528,#20656,.T.);
#43669=EDGE_CURVE('',#33322,#33528,#24046,.T.);
#43670=EDGE_CURVE('',#33527,#33491,#26223,.T.);
#43671=EDGE_CURVE('',#33529,#33530,#20657,.T.);
#43672=EDGE_CURVE('',#33529,#33531,#20658,.T.);
#43673=EDGE_CURVE('',#33530,#33531,#20659,.T.);
#43674=EDGE_CURVE('',#33528,#33532,#20660,.T.);
#43675=EDGE_CURVE('',#33492,#33532,#26224,.T.);
#43676=EDGE_CURVE('',#33532,#33529,#20661,.T.);
#43677=EDGE_CURVE('',#33531,#33527,#20662,.T.);
#43678=EDGE_CURVE('',#33533,#33534,#20663,.T.);
#43679=EDGE_CURVE('',#33323,#33534,#24047,.T.);
#43680=EDGE_CURVE('',#33533,#33492,#26225,.T.);
#43681=EDGE_CURVE('',#33535,#33536,#20664,.T.);
#43682=EDGE_CURVE('',#33535,#33537,#20665,.T.);
#43683=EDGE_CURVE('',#33536,#33537,#20666,.T.);
#43684=EDGE_CURVE('',#33534,#33538,#20667,.T.);
#43685=EDGE_CURVE('',#33493,#33538,#26226,.T.);
#43686=EDGE_CURVE('',#33538,#33535,#20668,.T.);
#43687=EDGE_CURVE('',#33537,#33533,#20669,.T.);
#43688=EDGE_CURVE('',#33539,#33540,#20670,.T.);
#43689=EDGE_CURVE('',#33324,#33540,#24048,.T.);
#43690=EDGE_CURVE('',#33539,#33493,#26227,.T.);
#43691=EDGE_CURVE('',#33541,#33542,#20671,.T.);
#43692=EDGE_CURVE('',#33541,#33543,#20672,.T.);
#43693=EDGE_CURVE('',#33542,#33543,#20673,.T.);
#43694=EDGE_CURVE('',#33540,#33544,#20674,.T.);
#43695=EDGE_CURVE('',#33494,#33544,#26228,.T.);
#43696=EDGE_CURVE('',#33544,#33541,#20675,.T.);
#43697=EDGE_CURVE('',#33543,#33539,#20676,.T.);
#43698=EDGE_CURVE('',#33545,#33546,#20677,.T.);
#43699=EDGE_CURVE('',#33325,#33546,#24049,.T.);
#43700=EDGE_CURVE('',#33545,#33494,#26229,.T.);
#43701=EDGE_CURVE('',#33547,#33548,#20678,.T.);
#43702=EDGE_CURVE('',#33547,#33549,#20679,.T.);
#43703=EDGE_CURVE('',#33548,#33549,#20680,.T.);
#43704=EDGE_CURVE('',#33546,#33550,#20681,.T.);
#43705=EDGE_CURVE('',#33495,#33550,#26230,.T.);
#43706=EDGE_CURVE('',#33550,#33547,#20682,.T.);
#43707=EDGE_CURVE('',#33549,#33545,#20683,.T.);
#43708=EDGE_CURVE('',#33551,#33552,#20684,.T.);
#43709=EDGE_CURVE('',#33326,#33552,#24050,.T.);
#43710=EDGE_CURVE('',#33551,#33495,#26231,.T.);
#43711=EDGE_CURVE('',#33553,#33554,#20685,.T.);
#43712=EDGE_CURVE('',#33553,#33555,#20686,.T.);
#43713=EDGE_CURVE('',#33554,#33555,#20687,.T.);
#43714=EDGE_CURVE('',#33552,#33556,#20688,.T.);
#43715=EDGE_CURVE('',#33496,#33556,#26232,.T.);
#43716=EDGE_CURVE('',#33556,#33553,#20689,.T.);
#43717=EDGE_CURVE('',#33555,#33551,#20690,.T.);
#43718=EDGE_CURVE('',#33327,#28903,#24051,.T.);
#43719=EDGE_CURVE('',#28905,#33496,#26233,.T.);
#43720=EDGE_CURVE('',#28907,#33557,#20691,.T.);
#43721=EDGE_CURVE('',#33557,#28906,#20692,.T.);
#43722=EDGE_CURVE('',#33497,#28904,#26234,.T.);
#43723=EDGE_CURVE('',#33558,#33559,#20693,.T.);
#43724=EDGE_CURVE('',#33328,#33559,#24052,.T.);
#43725=EDGE_CURVE('',#33558,#33497,#26235,.T.);
#43726=EDGE_CURVE('',#33560,#33561,#20694,.T.);
#43727=EDGE_CURVE('',#33560,#33562,#20695,.T.);
#43728=EDGE_CURVE('',#33561,#33562,#20696,.T.);
#43729=EDGE_CURVE('',#33559,#33563,#20697,.T.);
#43730=EDGE_CURVE('',#33498,#33563,#26236,.T.);
#43731=EDGE_CURVE('',#33563,#33560,#20698,.T.);
#43732=EDGE_CURVE('',#33562,#33558,#20699,.T.);
#43733=EDGE_CURVE('',#33564,#33565,#20700,.T.);
#43734=EDGE_CURVE('',#33329,#33565,#24053,.T.);
#43735=EDGE_CURVE('',#33564,#33498,#26237,.T.);
#43736=EDGE_CURVE('',#33566,#33567,#20701,.T.);
#43737=EDGE_CURVE('',#33566,#33568,#20702,.T.);
#43738=EDGE_CURVE('',#33567,#33568,#20703,.T.);
#43739=EDGE_CURVE('',#33565,#33569,#20704,.T.);
#43740=EDGE_CURVE('',#33499,#33569,#26238,.T.);
#43741=EDGE_CURVE('',#33569,#33566,#20705,.T.);
#43742=EDGE_CURVE('',#33568,#33564,#20706,.T.);
#43743=EDGE_CURVE('',#33570,#33571,#20707,.T.);
#43744=EDGE_CURVE('',#33330,#33571,#24054,.T.);
#43745=EDGE_CURVE('',#33570,#33499,#26239,.T.);
#43746=EDGE_CURVE('',#33572,#33573,#20708,.T.);
#43747=EDGE_CURVE('',#33572,#33574,#20709,.T.);
#43748=EDGE_CURVE('',#33573,#33574,#20710,.T.);
#43749=EDGE_CURVE('',#33571,#33575,#20711,.T.);
#43750=EDGE_CURVE('',#33500,#33575,#26240,.T.);
#43751=EDGE_CURVE('',#33575,#33572,#20712,.T.);
#43752=EDGE_CURVE('',#33574,#33570,#20713,.T.);
#43753=EDGE_CURVE('',#33576,#33577,#20714,.T.);
#43754=EDGE_CURVE('',#33331,#33577,#24055,.T.);
#43755=EDGE_CURVE('',#33576,#33500,#26241,.T.);
#43756=EDGE_CURVE('',#33578,#33579,#20715,.T.);
#43757=EDGE_CURVE('',#33578,#33580,#20716,.T.);
#43758=EDGE_CURVE('',#33579,#33580,#20717,.T.);
#43759=EDGE_CURVE('',#33577,#33581,#20718,.T.);
#43760=EDGE_CURVE('',#33501,#33581,#26242,.T.);
#43761=EDGE_CURVE('',#33581,#33578,#20719,.T.);
#43762=EDGE_CURVE('',#33580,#33576,#20720,.T.);
#43763=EDGE_CURVE('',#33582,#33583,#20721,.T.);
#43764=EDGE_CURVE('',#33332,#33583,#24056,.T.);
#43765=EDGE_CURVE('',#33582,#33501,#26243,.T.);
#43766=EDGE_CURVE('',#33584,#33585,#20722,.T.);
#43767=EDGE_CURVE('',#33584,#33586,#20723,.T.);
#43768=EDGE_CURVE('',#33585,#33586,#20724,.T.);
#43769=EDGE_CURVE('',#33583,#33587,#20725,.T.);
#43770=EDGE_CURVE('',#33502,#33587,#26244,.T.);
#43771=EDGE_CURVE('',#33587,#33584,#20726,.T.);
#43772=EDGE_CURVE('',#33586,#33582,#20727,.T.);
#43773=EDGE_CURVE('',#33588,#33589,#20728,.T.);
#43774=EDGE_CURVE('',#33333,#33589,#24057,.T.);
#43775=EDGE_CURVE('',#33588,#33502,#26245,.T.);
#43776=EDGE_CURVE('',#33590,#33591,#20729,.T.);
#43777=EDGE_CURVE('',#33590,#33592,#20730,.T.);
#43778=EDGE_CURVE('',#33591,#33592,#20731,.T.);
#43779=EDGE_CURVE('',#33589,#33593,#20732,.T.);
#43780=EDGE_CURVE('',#33503,#33593,#26246,.T.);
#43781=EDGE_CURVE('',#33593,#33590,#20733,.T.);
#43782=EDGE_CURVE('',#33592,#33588,#20734,.T.);
#43783=EDGE_CURVE('',#33594,#33595,#20735,.T.);
#43784=EDGE_CURVE('',#33334,#33595,#24058,.T.);
#43785=EDGE_CURVE('',#33594,#33503,#26247,.T.);
#43786=EDGE_CURVE('',#33596,#33597,#20736,.T.);
#43787=EDGE_CURVE('',#33596,#33598,#20737,.T.);
#43788=EDGE_CURVE('',#33597,#33598,#20738,.T.);
#43789=EDGE_CURVE('',#33595,#33599,#20739,.T.);
#43790=EDGE_CURVE('',#33504,#33599,#26248,.T.);
#43791=EDGE_CURVE('',#33599,#33596,#20740,.T.);
#43792=EDGE_CURVE('',#33598,#33594,#20741,.T.);
#43793=EDGE_CURVE('',#33600,#33601,#20742,.T.);
#43794=EDGE_CURVE('',#33335,#33601,#24059,.T.);
#43795=EDGE_CURVE('',#33600,#33504,#26249,.T.);
#43796=EDGE_CURVE('',#33602,#33603,#20743,.T.);
#43797=EDGE_CURVE('',#33602,#33604,#20744,.T.);
#43798=EDGE_CURVE('',#33603,#33604,#20745,.T.);
#43799=EDGE_CURVE('',#33601,#33605,#20746,.T.);
#43800=EDGE_CURVE('',#33505,#33605,#26250,.T.);
#43801=EDGE_CURVE('',#33605,#33602,#20747,.T.);
#43802=EDGE_CURVE('',#33604,#33600,#20748,.T.);
#43803=EDGE_CURVE('',#33606,#33607,#20749,.T.);
#43804=EDGE_CURVE('',#33336,#33607,#24060,.T.);
#43805=EDGE_CURVE('',#33606,#33505,#26251,.T.);
#43806=EDGE_CURVE('',#33608,#33609,#20750,.T.);
#43807=EDGE_CURVE('',#33608,#33610,#20751,.T.);
#43808=EDGE_CURVE('',#33609,#33610,#20752,.T.);
#43809=EDGE_CURVE('',#33607,#33611,#20753,.T.);
#43810=EDGE_CURVE('',#33506,#33611,#26252,.T.);
#43811=EDGE_CURVE('',#33611,#33608,#20754,.T.);
#43812=EDGE_CURVE('',#33610,#33606,#20755,.T.);
#43813=EDGE_CURVE('',#33612,#33613,#20756,.T.);
#43814=EDGE_CURVE('',#33337,#33613,#24061,.T.);
#43815=EDGE_CURVE('',#33612,#33506,#26253,.T.);
#43816=EDGE_CURVE('',#33614,#33615,#20757,.T.);
#43817=EDGE_CURVE('',#33614,#33616,#20758,.T.);
#43818=EDGE_CURVE('',#33615,#33616,#20759,.T.);
#43819=EDGE_CURVE('',#33613,#33617,#20760,.T.);
#43820=EDGE_CURVE('',#33507,#33617,#26254,.T.);
#43821=EDGE_CURVE('',#33617,#33614,#20761,.T.);
#43822=EDGE_CURVE('',#33616,#33612,#20762,.T.);
#43823=EDGE_CURVE('',#33618,#33507,#26255,.T.);
#43824=EDGE_CURVE('',#33618,#33619,#20763,.T.);
#43825=EDGE_CURVE('',#33338,#33619,#24062,.T.);
#43826=EDGE_CURVE('',#33620,#33621,#20764,.T.);
#43827=EDGE_CURVE('',#33620,#33622,#20765,.T.);
#43828=EDGE_CURVE('',#33621,#33622,#20766,.T.);
#43829=EDGE_CURVE('',#33619,#33623,#20767,.T.);
#43830=EDGE_CURVE('',#33508,#33623,#26256,.T.);
#43831=EDGE_CURVE('',#33623,#33620,#20768,.T.);
#43832=EDGE_CURVE('',#33622,#33618,#20769,.T.);
#43833=EDGE_CURVE('',#33624,#33625,#20770,.T.);
#43834=EDGE_CURVE('',#33339,#33625,#24063,.T.);
#43835=EDGE_CURVE('',#33624,#33508,#26257,.T.);
#43836=EDGE_CURVE('',#33626,#33627,#20771,.T.);
#43837=EDGE_CURVE('',#33626,#33628,#20772,.T.);
#43838=EDGE_CURVE('',#33627,#33628,#20773,.T.);
#43839=EDGE_CURVE('',#33625,#33629,#20774,.T.);
#43840=EDGE_CURVE('',#33509,#33629,#26258,.T.);
#43841=EDGE_CURVE('',#33629,#33626,#20775,.T.);
#43842=EDGE_CURVE('',#33628,#33624,#20776,.T.);
#43843=EDGE_CURVE('',#33630,#33631,#20777,.T.);
#43844=EDGE_CURVE('',#33340,#33631,#24064,.T.);
#43845=EDGE_CURVE('',#33630,#33509,#26259,.T.);
#43846=EDGE_CURVE('',#33632,#33633,#20778,.T.);
#43847=EDGE_CURVE('',#33632,#33634,#20779,.T.);
#43848=EDGE_CURVE('',#33633,#33634,#20780,.T.);
#43849=EDGE_CURVE('',#33631,#33635,#20781,.T.);
#43850=EDGE_CURVE('',#33510,#33635,#26260,.T.);
#43851=EDGE_CURVE('',#33635,#33632,#20782,.T.);
#43852=EDGE_CURVE('',#33634,#33630,#20783,.T.);
#43853=EDGE_CURVE('',#33636,#33637,#20784,.T.);
#43854=EDGE_CURVE('',#33341,#33637,#24065,.T.);
#43855=EDGE_CURVE('',#33636,#33510,#26261,.T.);
#43856=EDGE_CURVE('',#33638,#33639,#20785,.T.);
#43857=EDGE_CURVE('',#33638,#33640,#20786,.T.);
#43858=EDGE_CURVE('',#33639,#33640,#20787,.T.);
#43859=EDGE_CURVE('',#33637,#33641,#20788,.T.);
#43860=EDGE_CURVE('',#33511,#33641,#26262,.T.);
#43861=EDGE_CURVE('',#33641,#33638,#20789,.T.);
#43862=EDGE_CURVE('',#33640,#33636,#20790,.T.);
#43863=EDGE_CURVE('',#33642,#33643,#20791,.T.);
#43864=EDGE_CURVE('',#33342,#33643,#24066,.T.);
#43865=EDGE_CURVE('',#33642,#33511,#26263,.T.);
#43866=EDGE_CURVE('',#33644,#33645,#20792,.T.);
#43867=EDGE_CURVE('',#33644,#33646,#20793,.T.);
#43868=EDGE_CURVE('',#33645,#33646,#20794,.T.);
#43869=EDGE_CURVE('',#33643,#33647,#20795,.T.);
#43870=EDGE_CURVE('',#33512,#33647,#26264,.T.);
#43871=EDGE_CURVE('',#33647,#33644,#20796,.T.);
#43872=EDGE_CURVE('',#33646,#33642,#20797,.T.);
#43873=EDGE_CURVE('',#33648,#33649,#20798,.T.);
#43874=EDGE_CURVE('',#33343,#33649,#24067,.T.);
#43875=EDGE_CURVE('',#33648,#33512,#26265,.T.);
#43876=EDGE_CURVE('',#33650,#33651,#20799,.T.);
#43877=EDGE_CURVE('',#33650,#33652,#20800,.T.);
#43878=EDGE_CURVE('',#33651,#33652,#20801,.T.);
#43879=EDGE_CURVE('',#33649,#33653,#20802,.T.);
#43880=EDGE_CURVE('',#33513,#33653,#26266,.T.);
#43881=EDGE_CURVE('',#33653,#33650,#20803,.T.);
#43882=EDGE_CURVE('',#33652,#33648,#20804,.T.);
#43883=EDGE_CURVE('',#33654,#33655,#20805,.T.);
#43884=EDGE_CURVE('',#33344,#33655,#24068,.T.);
#43885=EDGE_CURVE('',#33654,#33513,#26267,.T.);
#43886=EDGE_CURVE('',#33656,#33657,#20806,.T.);
#43887=EDGE_CURVE('',#33656,#33658,#20807,.T.);
#43888=EDGE_CURVE('',#33657,#33658,#20808,.T.);
#43889=EDGE_CURVE('',#33655,#33659,#20809,.T.);
#43890=EDGE_CURVE('',#33514,#33659,#26268,.T.);
#43891=EDGE_CURVE('',#33659,#33656,#20810,.T.);
#43892=EDGE_CURVE('',#33658,#33654,#20811,.T.);
#43893=EDGE_CURVE('',#33660,#33661,#20812,.T.);
#43894=EDGE_CURVE('',#33345,#33661,#24069,.T.);
#43895=EDGE_CURVE('',#33660,#33514,#26269,.T.);
#43896=EDGE_CURVE('',#33662,#33663,#20813,.T.);
#43897=EDGE_CURVE('',#33662,#33664,#20814,.T.);
#43898=EDGE_CURVE('',#33663,#33664,#20815,.T.);
#43899=EDGE_CURVE('',#33661,#33665,#20816,.T.);
#43900=EDGE_CURVE('',#33515,#33665,#26270,.T.);
#43901=EDGE_CURVE('',#33665,#33662,#20817,.T.);
#43902=EDGE_CURVE('',#33664,#33660,#20818,.T.);
#43903=EDGE_CURVE('',#33666,#33667,#20819,.T.);
#43904=EDGE_CURVE('',#33346,#33667,#24070,.T.);
#43905=EDGE_CURVE('',#33666,#33515,#26271,.T.);
#43906=EDGE_CURVE('',#33668,#33669,#20820,.T.);
#43907=EDGE_CURVE('',#33668,#33670,#20821,.T.);
#43908=EDGE_CURVE('',#33669,#33670,#20822,.T.);
#43909=EDGE_CURVE('',#33667,#33671,#20823,.T.);
#43910=EDGE_CURVE('',#33516,#33671,#26272,.T.);
#43911=EDGE_CURVE('',#33671,#33668,#20824,.T.);
#43912=EDGE_CURVE('',#33670,#33666,#20825,.T.);
#43913=EDGE_CURVE('',#33672,#33673,#20826,.T.);
#43914=EDGE_CURVE('',#33347,#33673,#24071,.T.);
#43915=EDGE_CURVE('',#33672,#33516,#26273,.T.);
#43916=EDGE_CURVE('',#33674,#33675,#20827,.T.);
#43917=EDGE_CURVE('',#33674,#33676,#20828,.T.);
#43918=EDGE_CURVE('',#33675,#33676,#20829,.T.);
#43919=EDGE_CURVE('',#33673,#33677,#20830,.T.);
#43920=EDGE_CURVE('',#33517,#33677,#26274,.T.);
#43921=EDGE_CURVE('',#33677,#33674,#20831,.T.);
#43922=EDGE_CURVE('',#33676,#33672,#20832,.T.);
#43923=EDGE_CURVE('',#33678,#33679,#20833,.T.);
#43924=EDGE_CURVE('',#33348,#33679,#24072,.T.);
#43925=EDGE_CURVE('',#33678,#33517,#26275,.T.);
#43926=EDGE_CURVE('',#33680,#33681,#20834,.T.);
#43927=EDGE_CURVE('',#33680,#33682,#20835,.T.);
#43928=EDGE_CURVE('',#33681,#33682,#20836,.T.);
#43929=EDGE_CURVE('',#33679,#33683,#20837,.T.);
#43930=EDGE_CURVE('',#33518,#33683,#26276,.T.);
#43931=EDGE_CURVE('',#33683,#33680,#20838,.T.);
#43932=EDGE_CURVE('',#33682,#33678,#20839,.T.);
#43933=EDGE_CURVE('',#33684,#33685,#20840,.T.);
#43934=EDGE_CURVE('',#33684,#33686,#20841,.T.);
#43935=EDGE_CURVE('',#33685,#33686,#20842,.T.);
#43936=EDGE_CURVE('',#33520,#33684,#20843,.T.);
#43937=EDGE_CURVE('',#33687,#33519,#20844,.T.);
#43938=EDGE_CURVE('',#33686,#33687,#20845,.T.);
#43939=EDGE_CURVE('',#33687,#33518,#26277,.T.);
#43940=EDGE_CURVE('',#33688,#33685,#141,.T.);
#43941=EDGE_CURVE('',#33490,#33688,#20846,.T.);
#43942=EDGE_CURVE('',#33689,#33490,#20847,.T.);
#43943=EDGE_CURVE('',#33524,#33689,#142,.T.);
#43944=EDGE_CURVE('',#33491,#33689,#20848,.T.);
#43945=EDGE_CURVE('',#33690,#33491,#20849,.T.);
#43946=EDGE_CURVE('',#33530,#33690,#143,.T.);
#43947=EDGE_CURVE('',#33492,#33690,#20850,.T.);
#43948=EDGE_CURVE('',#33691,#33492,#20851,.T.);
#43949=EDGE_CURVE('',#33536,#33691,#144,.T.);
#43950=EDGE_CURVE('',#33493,#33691,#20852,.T.);
#43951=EDGE_CURVE('',#33692,#33493,#20853,.T.);
#43952=EDGE_CURVE('',#33542,#33692,#145,.T.);
#43953=EDGE_CURVE('',#33494,#33692,#20854,.T.);
#43954=EDGE_CURVE('',#33693,#33494,#20855,.T.);
#43955=EDGE_CURVE('',#33548,#33693,#146,.T.);
#43956=EDGE_CURVE('',#33495,#33693,#20856,.T.);
#43957=EDGE_CURVE('',#33694,#33495,#20857,.T.);
#43958=EDGE_CURVE('',#33554,#33694,#147,.T.);
#43959=EDGE_CURVE('',#33496,#33694,#20858,.T.);
#43960=EDGE_CURVE('',#33695,#33496,#20859,.T.);
#43961=EDGE_CURVE('',#33557,#33695,#148,.T.);
#43962=EDGE_CURVE('',#33497,#33695,#20860,.T.);
#43963=EDGE_CURVE('',#33696,#33497,#20861,.T.);
#43964=EDGE_CURVE('',#33561,#33696,#149,.T.);
#43965=EDGE_CURVE('',#33498,#33696,#20862,.T.);
#43966=EDGE_CURVE('',#33697,#33498,#20863,.T.);
#43967=EDGE_CURVE('',#33567,#33697,#150,.T.);
#43968=EDGE_CURVE('',#33499,#33697,#20864,.T.);
#43969=EDGE_CURVE('',#33698,#33499,#20865,.T.);
#43970=EDGE_CURVE('',#33573,#33698,#151,.T.);
#43971=EDGE_CURVE('',#33500,#33698,#20866,.T.);
#43972=EDGE_CURVE('',#33699,#33500,#20867,.T.);
#43973=EDGE_CURVE('',#33579,#33699,#152,.T.);
#43974=EDGE_CURVE('',#33501,#33699,#20868,.T.);
#43975=EDGE_CURVE('',#33700,#33501,#20869,.T.);
#43976=EDGE_CURVE('',#33585,#33700,#153,.T.);
#43977=EDGE_CURVE('',#33502,#33700,#20870,.T.);
#43978=EDGE_CURVE('',#33701,#33502,#20871,.T.);
#43979=EDGE_CURVE('',#33591,#33701,#154,.T.);
#43980=EDGE_CURVE('',#33503,#33701,#20872,.T.);
#43981=EDGE_CURVE('',#33702,#33503,#20873,.T.);
#43982=EDGE_CURVE('',#33597,#33702,#155,.T.);
#43983=EDGE_CURVE('',#33504,#33702,#20874,.T.);
#43984=EDGE_CURVE('',#33703,#33504,#20875,.T.);
#43985=EDGE_CURVE('',#33603,#33703,#156,.T.);
#43986=EDGE_CURVE('',#33505,#33703,#20876,.T.);
#43987=EDGE_CURVE('',#33704,#33505,#20877,.T.);
#43988=EDGE_CURVE('',#33609,#33704,#157,.T.);
#43989=EDGE_CURVE('',#33506,#33704,#20878,.T.);
#43990=EDGE_CURVE('',#33705,#33506,#20879,.T.);
#43991=EDGE_CURVE('',#33615,#33705,#158,.T.);
#43992=EDGE_CURVE('',#33507,#33705,#20880,.T.);
#43993=EDGE_CURVE('',#33706,#33507,#20881,.T.);
#43994=EDGE_CURVE('',#33621,#33706,#159,.T.);
#43995=EDGE_CURVE('',#33508,#33706,#20882,.T.);
#43996=EDGE_CURVE('',#33707,#33508,#20883,.T.);
#43997=EDGE_CURVE('',#33627,#33707,#160,.T.);
#43998=EDGE_CURVE('',#33509,#33707,#20884,.T.);
#43999=EDGE_CURVE('',#33708,#33509,#20885,.T.);
#44000=EDGE_CURVE('',#33633,#33708,#161,.T.);
#44001=EDGE_CURVE('',#33510,#33708,#20886,.T.);
#44002=EDGE_CURVE('',#33709,#33510,#20887,.T.);
#44003=EDGE_CURVE('',#33639,#33709,#162,.T.);
#44004=EDGE_CURVE('',#33511,#33709,#20888,.T.);
#44005=EDGE_CURVE('',#33710,#33511,#20889,.T.);
#44006=EDGE_CURVE('',#33645,#33710,#163,.T.);
#44007=EDGE_CURVE('',#33512,#33710,#20890,.T.);
#44008=EDGE_CURVE('',#33711,#33512,#20891,.T.);
#44009=EDGE_CURVE('',#33651,#33711,#164,.T.);
#44010=EDGE_CURVE('',#33513,#33711,#20892,.T.);
#44011=EDGE_CURVE('',#33712,#33513,#20893,.T.);
#44012=EDGE_CURVE('',#33657,#33712,#165,.T.);
#44013=EDGE_CURVE('',#33514,#33712,#20894,.T.);
#44014=EDGE_CURVE('',#33713,#33514,#20895,.T.);
#44015=EDGE_CURVE('',#33663,#33713,#166,.T.);
#44016=EDGE_CURVE('',#33515,#33713,#20896,.T.);
#44017=EDGE_CURVE('',#33714,#33515,#20897,.T.);
#44018=EDGE_CURVE('',#33669,#33714,#167,.T.);
#44019=EDGE_CURVE('',#33516,#33714,#20898,.T.);
#44020=EDGE_CURVE('',#33715,#33516,#20899,.T.);
#44021=EDGE_CURVE('',#33675,#33715,#168,.T.);
#44022=EDGE_CURVE('',#33517,#33715,#20900,.T.);
#44023=EDGE_CURVE('',#33716,#33517,#20901,.T.);
#44024=EDGE_CURVE('',#33681,#33716,#169,.T.);
#44025=EDGE_CURVE('',#33518,#33716,#20902,.T.);
#44026=EDGE_CURVE('',#33688,#33518,#20903,.T.);
#44027=EDGE_CURVE('',#33717,#33688,#26278,.T.);
#44028=EDGE_CURVE('',#33717,#33718,#24073,.T.);
#44029=EDGE_CURVE('',#33490,#33718,#24074,.T.);
#44030=EDGE_CURVE('',#33719,#33720,#24075,.T.);
#44031=EDGE_CURVE('',#33718,#33719,#24076,.T.);
#44032=EDGE_CURVE('',#33720,#33717,#24077,.T.);
#44033=EDGE_CURVE('',#33689,#33719,#26279,.T.);
#44034=EDGE_CURVE('',#33721,#33689,#26280,.T.);
#44035=EDGE_CURVE('',#33721,#33722,#24078,.T.);
#44036=EDGE_CURVE('',#33491,#33722,#24079,.T.);
#44037=EDGE_CURVE('',#33723,#33724,#24080,.T.);
#44038=EDGE_CURVE('',#33722,#33723,#24081,.T.);
#44039=EDGE_CURVE('',#33724,#33721,#24082,.T.);
#44040=EDGE_CURVE('',#33690,#33723,#26281,.T.);
#44041=EDGE_CURVE('',#33725,#33690,#26282,.T.);
#44042=EDGE_CURVE('',#33725,#33726,#24083,.T.);
#44043=EDGE_CURVE('',#33492,#33726,#24084,.T.);
#44044=EDGE_CURVE('',#33727,#33728,#24085,.T.);
#44045=EDGE_CURVE('',#33726,#33727,#24086,.T.);
#44046=EDGE_CURVE('',#33728,#33725,#24087,.T.);
#44047=EDGE_CURVE('',#33691,#33727,#26283,.T.);
#44048=EDGE_CURVE('',#33729,#33691,#26284,.T.);
#44049=EDGE_CURVE('',#33729,#33730,#24088,.T.);
#44050=EDGE_CURVE('',#33493,#33730,#24089,.T.);
#44051=EDGE_CURVE('',#33731,#33732,#24090,.T.);
#44052=EDGE_CURVE('',#33730,#33731,#24091,.T.);
#44053=EDGE_CURVE('',#33732,#33729,#24092,.T.);
#44054=EDGE_CURVE('',#33692,#33731,#26285,.T.);
#44055=EDGE_CURVE('',#33733,#33692,#26286,.T.);
#44056=EDGE_CURVE('',#33733,#33734,#24093,.T.);
#44057=EDGE_CURVE('',#33494,#33734,#24094,.T.);
#44058=EDGE_CURVE('',#33735,#33736,#24095,.T.);
#44059=EDGE_CURVE('',#33734,#33735,#24096,.T.);
#44060=EDGE_CURVE('',#33736,#33733,#24097,.T.);
#44061=EDGE_CURVE('',#33693,#33735,#26287,.T.);
#44062=EDGE_CURVE('',#33737,#33693,#26288,.T.);
#44063=EDGE_CURVE('',#33737,#33738,#24098,.T.);
#44064=EDGE_CURVE('',#33495,#33738,#24099,.T.);
#44065=EDGE_CURVE('',#33739,#33740,#24100,.T.);
#44066=EDGE_CURVE('',#33738,#33739,#24101,.T.);
#44067=EDGE_CURVE('',#33740,#33737,#24102,.T.);
#44068=EDGE_CURVE('',#33694,#33739,#26289,.T.);
#44069=EDGE_CURVE('',#33741,#33694,#26290,.T.);
#44070=EDGE_CURVE('',#33741,#33742,#24103,.T.);
#44071=EDGE_CURVE('',#33496,#33742,#24104,.T.);
#44072=EDGE_CURVE('',#33743,#33744,#24105,.T.);
#44073=EDGE_CURVE('',#33742,#33743,#24106,.T.);
#44074=EDGE_CURVE('',#33744,#33741,#24107,.T.);
#44075=EDGE_CURVE('',#33695,#33743,#26291,.T.);
#44076=EDGE_CURVE('',#33745,#33695,#26292,.T.);
#44077=EDGE_CURVE('',#33745,#33746,#24108,.T.);
#44078=EDGE_CURVE('',#33497,#33746,#24109,.T.);
#44079=EDGE_CURVE('',#33747,#33748,#24110,.T.);
#44080=EDGE_CURVE('',#33746,#33747,#24111,.T.);
#44081=EDGE_CURVE('',#33748,#33745,#24112,.T.);
#44082=EDGE_CURVE('',#33696,#33747,#26293,.T.);
#44083=EDGE_CURVE('',#33749,#33696,#26294,.T.);
#44084=EDGE_CURVE('',#33749,#33750,#24113,.T.);
#44085=EDGE_CURVE('',#33498,#33750,#24114,.T.);
#44086=EDGE_CURVE('',#33751,#33752,#24115,.T.);
#44087=EDGE_CURVE('',#33750,#33751,#24116,.T.);
#44088=EDGE_CURVE('',#33752,#33749,#24117,.T.);
#44089=EDGE_CURVE('',#33697,#33751,#26295,.T.);
#44090=EDGE_CURVE('',#33753,#33697,#26296,.T.);
#44091=EDGE_CURVE('',#33753,#33754,#24118,.T.);
#44092=EDGE_CURVE('',#33499,#33754,#24119,.T.);
#44093=EDGE_CURVE('',#33755,#33756,#24120,.T.);
#44094=EDGE_CURVE('',#33754,#33755,#24121,.T.);
#44095=EDGE_CURVE('',#33756,#33753,#24122,.T.);
#44096=EDGE_CURVE('',#33698,#33755,#26297,.T.);
#44097=EDGE_CURVE('',#33757,#33698,#26298,.T.);
#44098=EDGE_CURVE('',#33757,#33758,#24123,.T.);
#44099=EDGE_CURVE('',#33500,#33758,#24124,.T.);
#44100=EDGE_CURVE('',#33759,#33760,#24125,.T.);
#44101=EDGE_CURVE('',#33758,#33759,#24126,.T.);
#44102=EDGE_CURVE('',#33760,#33757,#24127,.T.);
#44103=EDGE_CURVE('',#33699,#33759,#26299,.T.);
#44104=EDGE_CURVE('',#33761,#33699,#26300,.T.);
#44105=EDGE_CURVE('',#33761,#33762,#24128,.T.);
#44106=EDGE_CURVE('',#33501,#33762,#24129,.T.);
#44107=EDGE_CURVE('',#33763,#33764,#24130,.T.);
#44108=EDGE_CURVE('',#33762,#33763,#24131,.T.);
#44109=EDGE_CURVE('',#33764,#33761,#24132,.T.);
#44110=EDGE_CURVE('',#33700,#33763,#26301,.T.);
#44111=EDGE_CURVE('',#33765,#33700,#26302,.T.);
#44112=EDGE_CURVE('',#33765,#33766,#24133,.T.);
#44113=EDGE_CURVE('',#33502,#33766,#24134,.T.);
#44114=EDGE_CURVE('',#33767,#33768,#24135,.T.);
#44115=EDGE_CURVE('',#33766,#33767,#24136,.T.);
#44116=EDGE_CURVE('',#33768,#33765,#24137,.T.);
#44117=EDGE_CURVE('',#33701,#33767,#26303,.T.);
#44118=EDGE_CURVE('',#33769,#33701,#26304,.T.);
#44119=EDGE_CURVE('',#33769,#33770,#24138,.T.);
#44120=EDGE_CURVE('',#33503,#33770,#24139,.T.);
#44121=EDGE_CURVE('',#33771,#33772,#24140,.T.);
#44122=EDGE_CURVE('',#33770,#33771,#24141,.T.);
#44123=EDGE_CURVE('',#33772,#33769,#24142,.T.);
#44124=EDGE_CURVE('',#33702,#33771,#26305,.T.);
#44125=EDGE_CURVE('',#33773,#33702,#26306,.T.);
#44126=EDGE_CURVE('',#33773,#33774,#24143,.T.);
#44127=EDGE_CURVE('',#33504,#33774,#24144,.T.);
#44128=EDGE_CURVE('',#33775,#33776,#24145,.T.);
#44129=EDGE_CURVE('',#33774,#33775,#24146,.T.);
#44130=EDGE_CURVE('',#33776,#33773,#24147,.T.);
#44131=EDGE_CURVE('',#33703,#33775,#26307,.T.);
#44132=EDGE_CURVE('',#33777,#33703,#26308,.T.);
#44133=EDGE_CURVE('',#33777,#33778,#24148,.T.);
#44134=EDGE_CURVE('',#33505,#33778,#24149,.T.);
#44135=EDGE_CURVE('',#33779,#33780,#24150,.T.);
#44136=EDGE_CURVE('',#33778,#33779,#24151,.T.);
#44137=EDGE_CURVE('',#33780,#33777,#24152,.T.);
#44138=EDGE_CURVE('',#33704,#33779,#26309,.T.);
#44139=EDGE_CURVE('',#33781,#33704,#26310,.T.);
#44140=EDGE_CURVE('',#33781,#33782,#24153,.T.);
#44141=EDGE_CURVE('',#33506,#33782,#24154,.T.);
#44142=EDGE_CURVE('',#33783,#33784,#24155,.T.);
#44143=EDGE_CURVE('',#33782,#33783,#24156,.T.);
#44144=EDGE_CURVE('',#33784,#33781,#24157,.T.);
#44145=EDGE_CURVE('',#33705,#33783,#26311,.T.);
#44146=EDGE_CURVE('',#33785,#33705,#26312,.T.);
#44147=EDGE_CURVE('',#33785,#33786,#24158,.T.);
#44148=EDGE_CURVE('',#33507,#33786,#24159,.T.);
#44149=EDGE_CURVE('',#33787,#33785,#24160,.T.);
#44150=EDGE_CURVE('',#33788,#33787,#24161,.T.);
#44151=EDGE_CURVE('',#33786,#33788,#24162,.T.);
#44152=EDGE_CURVE('',#33706,#33788,#26313,.T.);
#44153=EDGE_CURVE('',#33789,#33706,#26314,.T.);
#44154=EDGE_CURVE('',#33789,#33790,#24163,.T.);
#44155=EDGE_CURVE('',#33508,#33790,#24164,.T.);
#44156=EDGE_CURVE('',#33791,#33792,#24165,.T.);
#44157=EDGE_CURVE('',#33790,#33791,#24166,.T.);
#44158=EDGE_CURVE('',#33792,#33789,#24167,.T.);
#44159=EDGE_CURVE('',#33707,#33791,#26315,.T.);
#44160=EDGE_CURVE('',#33793,#33707,#26316,.T.);
#44161=EDGE_CURVE('',#33793,#33794,#24168,.T.);
#44162=EDGE_CURVE('',#33509,#33794,#24169,.T.);
#44163=EDGE_CURVE('',#33795,#33796,#24170,.T.);
#44164=EDGE_CURVE('',#33794,#33795,#24171,.T.);
#44165=EDGE_CURVE('',#33796,#33793,#24172,.T.);
#44166=EDGE_CURVE('',#33708,#33795,#26317,.T.);
#44167=EDGE_CURVE('',#33797,#33708,#26318,.T.);
#44168=EDGE_CURVE('',#33797,#33798,#24173,.T.);
#44169=EDGE_CURVE('',#33510,#33798,#24174,.T.);
#44170=EDGE_CURVE('',#33799,#33800,#24175,.T.);
#44171=EDGE_CURVE('',#33798,#33799,#24176,.T.);
#44172=EDGE_CURVE('',#33800,#33797,#24177,.T.);
#44173=EDGE_CURVE('',#33709,#33799,#26319,.T.);
#44174=EDGE_CURVE('',#28902,#33709,#26320,.T.);
#44175=EDGE_CURVE('',#33511,#28901,#24178,.T.);
#44176=EDGE_CURVE('',#33710,#28899,#26321,.T.);
#44177=EDGE_CURVE('',#33801,#33710,#26322,.T.);
#44178=EDGE_CURVE('',#33801,#33802,#24179,.T.);
#44179=EDGE_CURVE('',#33512,#33802,#24180,.T.);
#44180=EDGE_CURVE('',#33803,#33804,#24181,.T.);
#44181=EDGE_CURVE('',#33802,#33803,#24182,.T.);
#44182=EDGE_CURVE('',#33804,#33801,#24183,.T.);
#44183=EDGE_CURVE('',#33711,#33803,#26323,.T.);
#44184=EDGE_CURVE('',#33805,#33711,#26324,.T.);
#44185=EDGE_CURVE('',#33805,#33806,#24184,.T.);
#44186=EDGE_CURVE('',#33513,#33806,#24185,.T.);
#44187=EDGE_CURVE('',#33807,#33808,#24186,.T.);
#44188=EDGE_CURVE('',#33806,#33807,#24187,.T.);
#44189=EDGE_CURVE('',#33808,#33805,#24188,.T.);
#44190=EDGE_CURVE('',#33712,#33807,#26325,.T.);
#44191=EDGE_CURVE('',#33809,#33712,#26326,.T.);
#44192=EDGE_CURVE('',#33809,#33810,#24189,.T.);
#44193=EDGE_CURVE('',#33514,#33810,#24190,.T.);
#44194=EDGE_CURVE('',#33811,#33812,#24191,.T.);
#44195=EDGE_CURVE('',#33810,#33811,#24192,.T.);
#44196=EDGE_CURVE('',#33812,#33809,#24193,.T.);
#44197=EDGE_CURVE('',#33713,#33811,#26327,.T.);
#44198=EDGE_CURVE('',#33813,#33713,#26328,.T.);
#44199=EDGE_CURVE('',#33813,#33814,#24194,.T.);
#44200=EDGE_CURVE('',#33515,#33814,#24195,.T.);
#44201=EDGE_CURVE('',#33815,#33816,#24196,.T.);
#44202=EDGE_CURVE('',#33814,#33815,#24197,.T.);
#44203=EDGE_CURVE('',#33816,#33813,#24198,.T.);
#44204=EDGE_CURVE('',#33714,#33815,#26329,.T.);
#44205=EDGE_CURVE('',#33817,#33714,#26330,.T.);
#44206=EDGE_CURVE('',#33817,#33818,#24199,.T.);
#44207=EDGE_CURVE('',#33516,#33818,#24200,.T.);
#44208=EDGE_CURVE('',#33819,#33820,#24201,.T.);
#44209=EDGE_CURVE('',#33818,#33819,#24202,.T.);
#44210=EDGE_CURVE('',#33820,#33817,#24203,.T.);
#44211=EDGE_CURVE('',#33715,#33819,#26331,.T.);
#44212=EDGE_CURVE('',#33821,#33715,#26332,.T.);
#44213=EDGE_CURVE('',#33821,#33822,#24204,.T.);
#44214=EDGE_CURVE('',#33517,#33822,#24205,.T.);
#44215=EDGE_CURVE('',#33823,#33824,#24206,.T.);
#44216=EDGE_CURVE('',#33822,#33823,#24207,.T.);
#44217=EDGE_CURVE('',#33824,#33821,#24208,.T.);
#44218=EDGE_CURVE('',#33716,#33823,#26333,.T.);
#44219=EDGE_CURVE('',#28898,#33716,#26334,.T.);
#44220=EDGE_CURVE('',#33518,#28897,#24209,.T.);
#44221=EDGE_CURVE('',#33688,#28895,#26335,.T.);
#44222=EDGE_CURVE('',#33825,#33688,#20904,.T.);
#44223=EDGE_CURVE('',#33720,#33825,#170,.T.);
#44224=EDGE_CURVE('',#33689,#33825,#20905,.T.);
#44225=EDGE_CURVE('',#33826,#33689,#20906,.T.);
#44226=EDGE_CURVE('',#33724,#33826,#24210,.T.);
#44227=EDGE_CURVE('',#33690,#33826,#20907,.T.);
#44228=EDGE_CURVE('',#33827,#33690,#20908,.T.);
#44229=EDGE_CURVE('',#33728,#33827,#171,.T.);
#44230=EDGE_CURVE('',#33691,#33827,#20909,.T.);
#44231=EDGE_CURVE('',#33828,#33691,#20910,.T.);
#44232=EDGE_CURVE('',#33732,#33828,#172,.T.);
#44233=EDGE_CURVE('',#33692,#33828,#20911,.T.);
#44234=EDGE_CURVE('',#33829,#33692,#20912,.T.);
#44235=EDGE_CURVE('',#33736,#33829,#173,.T.);
#44236=EDGE_CURVE('',#33693,#33829,#20913,.T.);
#44237=EDGE_CURVE('',#33830,#33693,#20914,.T.);
#44238=EDGE_CURVE('',#33740,#33830,#174,.T.);
#44239=EDGE_CURVE('',#33694,#33830,#20915,.T.);
#44240=EDGE_CURVE('',#33831,#33694,#20916,.T.);
#44241=EDGE_CURVE('',#33744,#33831,#175,.T.);
#44242=EDGE_CURVE('',#33695,#33831,#20917,.T.);
#44243=EDGE_CURVE('',#33832,#33695,#20918,.T.);
#44244=EDGE_CURVE('',#33748,#33832,#24211,.T.);
#44245=EDGE_CURVE('',#33696,#33832,#20919,.T.);
#44246=EDGE_CURVE('',#33833,#33696,#20920,.T.);
#44247=EDGE_CURVE('',#33752,#33833,#176,.T.);
#44248=EDGE_CURVE('',#33697,#33833,#20921,.T.);
#44249=EDGE_CURVE('',#33834,#33697,#20922,.T.);
#44250=EDGE_CURVE('',#33756,#33834,#177,.T.);
#44251=EDGE_CURVE('',#33698,#33834,#20923,.T.);
#44252=EDGE_CURVE('',#33835,#33698,#20924,.T.);
#44253=EDGE_CURVE('',#33760,#33835,#178,.T.);
#44254=EDGE_CURVE('',#33699,#33835,#20925,.T.);
#44255=EDGE_CURVE('',#33836,#33699,#20926,.T.);
#44256=EDGE_CURVE('',#33764,#33836,#179,.T.);
#44257=EDGE_CURVE('',#33700,#33836,#20927,.T.);
#44258=EDGE_CURVE('',#33837,#33700,#20928,.T.);
#44259=EDGE_CURVE('',#33768,#33837,#24212,.T.);
#44260=EDGE_CURVE('',#33701,#33837,#20929,.T.);
#44261=EDGE_CURVE('',#33838,#33701,#20930,.T.);
#44262=EDGE_CURVE('',#33772,#33838,#180,.T.);
#44263=EDGE_CURVE('',#33702,#33838,#20931,.T.);
#44264=EDGE_CURVE('',#33839,#33702,#20932,.T.);
#44265=EDGE_CURVE('',#33776,#33839,#181,.T.);
#44266=EDGE_CURVE('',#33703,#33839,#20933,.T.);
#44267=EDGE_CURVE('',#33840,#33703,#20934,.T.);
#44268=EDGE_CURVE('',#33780,#33840,#24213,.T.);
#44269=EDGE_CURVE('',#33704,#33840,#20935,.T.);
#44270=EDGE_CURVE('',#33841,#33704,#20936,.T.);
#44271=EDGE_CURVE('',#33784,#33841,#182,.T.);
#44272=EDGE_CURVE('',#33705,#33841,#20937,.T.);
#44273=EDGE_CURVE('',#33842,#33705,#20938,.T.);
#44274=EDGE_CURVE('',#33787,#33842,#24214,.T.);
#44275=EDGE_CURVE('',#33706,#33842,#20939,.T.);
#44276=EDGE_CURVE('',#33843,#33706,#20940,.T.);
#44277=EDGE_CURVE('',#33792,#33843,#183,.T.);
#44278=EDGE_CURVE('',#33707,#33843,#20941,.T.);
#44279=EDGE_CURVE('',#33844,#33707,#20942,.T.);
#44280=EDGE_CURVE('',#33796,#33844,#184,.T.);
#44281=EDGE_CURVE('',#33708,#33844,#20943,.T.);
#44282=EDGE_CURVE('',#33845,#33708,#20944,.T.);
#44283=EDGE_CURVE('',#33800,#33845,#24215,.T.);
#44284=EDGE_CURVE('',#33709,#33845,#20945,.T.);
#44285=EDGE_CURVE('',#33846,#33709,#20946,.T.);
#44286=EDGE_CURVE('',#28900,#33846,#24216,.T.);
#44287=EDGE_CURVE('',#33710,#33846,#20947,.T.);
#44288=EDGE_CURVE('',#33847,#33710,#20948,.T.);
#44289=EDGE_CURVE('',#33804,#33847,#185,.T.);
#44290=EDGE_CURVE('',#33711,#33847,#20949,.T.);
#44291=EDGE_CURVE('',#33848,#33711,#20950,.T.);
#44292=EDGE_CURVE('',#33808,#33848,#186,.T.);
#44293=EDGE_CURVE('',#33712,#33848,#20951,.T.);
#44294=EDGE_CURVE('',#33849,#33712,#20952,.T.);
#44295=EDGE_CURVE('',#33812,#33849,#187,.T.);
#44296=EDGE_CURVE('',#33713,#33849,#20953,.T.);
#44297=EDGE_CURVE('',#33850,#33713,#20954,.T.);
#44298=EDGE_CURVE('',#33816,#33850,#188,.T.);
#44299=EDGE_CURVE('',#33714,#33850,#20955,.T.);
#44300=EDGE_CURVE('',#33851,#33714,#20956,.T.);
#44301=EDGE_CURVE('',#33820,#33851,#189,.T.);
#44302=EDGE_CURVE('',#33715,#33851,#20957,.T.);
#44303=EDGE_CURVE('',#33852,#33715,#20958,.T.);
#44304=EDGE_CURVE('',#33824,#33852,#190,.T.);
#44305=EDGE_CURVE('',#33716,#33852,#20959,.T.);
#44306=EDGE_CURVE('',#33853,#33716,#20960,.T.);
#44307=EDGE_CURVE('',#28896,#33853,#191,.T.);
#44308=EDGE_CURVE('',#33688,#33853,#20961,.T.);
#44309=EDGE_CURVE('',#28619,#33688,#24217,.T.);
#44310=EDGE_CURVE('',#33825,#28618,#26336,.T.);
#44311=EDGE_CURVE('',#33825,#28617,#24218,.T.);
#44312=EDGE_CURVE('',#33825,#28616,#24219,.T.);
#44313=EDGE_CURVE('',#33825,#28615,#20962,.T.);
#44314=EDGE_CURVE('',#33825,#28614,#26337,.T.);
#44315=EDGE_CURVE('',#33689,#28613,#24220,.T.);
#44316=EDGE_CURVE('',#33826,#28612,#26338,.T.);
#44317=EDGE_CURVE('',#33826,#28611,#24221,.T.);
#44318=EDGE_CURVE('',#33826,#28610,#24222,.T.);
#44319=EDGE_CURVE('',#33826,#28609,#20963,.T.);
#44320=EDGE_CURVE('',#33826,#28608,#26339,.T.);
#44321=EDGE_CURVE('',#33690,#28607,#24223,.T.);
#44322=EDGE_CURVE('',#33827,#28606,#26340,.T.);
#44323=EDGE_CURVE('',#33827,#28605,#24224,.T.);
#44324=EDGE_CURVE('',#33827,#28604,#24225,.T.);
#44325=EDGE_CURVE('',#33827,#28603,#20964,.T.);
#44326=EDGE_CURVE('',#33827,#28602,#26341,.T.);
#44327=EDGE_CURVE('',#33691,#28601,#24226,.T.);
#44328=EDGE_CURVE('',#33828,#28600,#26342,.T.);
#44329=EDGE_CURVE('',#33828,#28599,#24227,.T.);
#44330=EDGE_CURVE('',#33828,#28598,#24228,.T.);
#44331=EDGE_CURVE('',#33828,#28597,#20965,.T.);
#44332=EDGE_CURVE('',#33828,#28596,#26343,.T.);
#44333=EDGE_CURVE('',#33692,#28595,#24229,.T.);
#44334=EDGE_CURVE('',#33829,#28594,#26344,.T.);
#44335=EDGE_CURVE('',#33829,#28593,#24230,.T.);
#44336=EDGE_CURVE('',#33829,#28592,#24231,.T.);
#44337=EDGE_CURVE('',#33829,#28591,#20966,.T.);
#44338=EDGE_CURVE('',#33829,#28590,#26345,.T.);
#44339=EDGE_CURVE('',#33693,#28589,#24232,.T.);
#44340=EDGE_CURVE('',#33830,#28588,#26346,.T.);
#44341=EDGE_CURVE('',#33830,#28587,#24233,.T.);
#44342=EDGE_CURVE('',#33830,#28586,#24234,.T.);
#44343=EDGE_CURVE('',#33830,#28585,#20967,.T.);
#44344=EDGE_CURVE('',#33830,#28584,#26347,.T.);
#44345=EDGE_CURVE('',#33694,#28583,#24235,.T.);
#44346=EDGE_CURVE('',#33831,#28582,#26348,.T.);
#44347=EDGE_CURVE('',#33831,#28581,#24236,.T.);
#44348=EDGE_CURVE('',#33831,#28580,#24237,.T.);
#44349=EDGE_CURVE('',#33831,#28579,#20968,.T.);
#44350=EDGE_CURVE('',#33831,#28578,#26349,.T.);
#44351=EDGE_CURVE('',#33695,#28577,#24238,.T.);
#44352=EDGE_CURVE('',#33832,#28576,#26350,.T.);
#44353=EDGE_CURVE('',#33832,#28575,#24239,.T.);
#44354=EDGE_CURVE('',#33832,#28574,#24240,.T.);
#44355=EDGE_CURVE('',#33832,#28573,#20969,.T.);
#44356=EDGE_CURVE('',#33832,#28572,#26351,.T.);
#44357=EDGE_CURVE('',#33696,#28571,#24241,.T.);
#44358=EDGE_CURVE('',#33833,#28570,#26352,.T.);
#44359=EDGE_CURVE('',#33833,#28569,#24242,.T.);
#44360=EDGE_CURVE('',#33833,#28568,#24243,.T.);
#44361=EDGE_CURVE('',#33833,#28567,#20970,.T.);
#44362=EDGE_CURVE('',#33833,#28566,#26353,.T.);
#44363=EDGE_CURVE('',#33697,#28565,#24244,.T.);
#44364=EDGE_CURVE('',#33834,#28564,#26354,.T.);
#44365=EDGE_CURVE('',#33834,#28563,#24245,.T.);
#44366=EDGE_CURVE('',#33834,#28562,#24246,.T.);
#44367=EDGE_CURVE('',#33834,#28561,#20971,.T.);
#44368=EDGE_CURVE('',#33834,#28560,#26355,.T.);
#44369=EDGE_CURVE('',#33698,#28559,#24247,.T.);
#44370=EDGE_CURVE('',#33835,#28558,#26356,.T.);
#44371=EDGE_CURVE('',#33835,#28557,#24248,.T.);
#44372=EDGE_CURVE('',#33835,#28556,#24249,.T.);
#44373=EDGE_CURVE('',#33835,#28555,#20972,.T.);
#44374=EDGE_CURVE('',#33835,#28554,#26357,.T.);
#44375=EDGE_CURVE('',#33699,#28553,#24250,.T.);
#44376=EDGE_CURVE('',#33836,#28552,#26358,.T.);
#44377=EDGE_CURVE('',#33836,#28551,#24251,.T.);
#44378=EDGE_CURVE('',#33836,#28550,#24252,.T.);
#44379=EDGE_CURVE('',#33836,#28549,#20973,.T.);
#44380=EDGE_CURVE('',#33836,#28548,#26359,.T.);
#44381=EDGE_CURVE('',#33700,#28547,#24253,.T.);
#44382=EDGE_CURVE('',#33837,#28546,#26360,.T.);
#44383=EDGE_CURVE('',#33837,#28545,#24254,.T.);
#44384=EDGE_CURVE('',#33837,#28544,#24255,.T.);
#44385=EDGE_CURVE('',#33837,#28543,#20974,.T.);
#44386=EDGE_CURVE('',#33837,#28542,#26361,.T.);
#44387=EDGE_CURVE('',#33701,#28541,#24256,.T.);
#44388=EDGE_CURVE('',#33838,#28540,#26362,.T.);
#44389=EDGE_CURVE('',#33838,#28539,#24257,.T.);
#44390=EDGE_CURVE('',#33838,#28538,#24258,.T.);
#44391=EDGE_CURVE('',#33838,#28537,#20975,.T.);
#44392=EDGE_CURVE('',#33838,#28536,#26363,.T.);
#44393=EDGE_CURVE('',#33702,#28535,#24259,.T.);
#44394=EDGE_CURVE('',#33839,#28712,#26364,.T.);
#44395=EDGE_CURVE('',#33839,#28709,#24260,.T.);
#44396=EDGE_CURVE('',#33839,#28706,#24261,.T.);
#44397=EDGE_CURVE('',#33839,#28705,#20976,.T.);
#44398=EDGE_CURVE('',#33839,#28704,#26365,.T.);
#44399=EDGE_CURVE('',#33703,#28703,#24262,.T.);
#44400=EDGE_CURVE('',#33840,#28702,#26366,.T.);
#44401=EDGE_CURVE('',#33840,#28701,#24263,.T.);
#44402=EDGE_CURVE('',#33840,#28700,#24264,.T.);
#44403=EDGE_CURVE('',#33840,#28699,#20977,.T.);
#44404=EDGE_CURVE('',#33840,#28698,#26367,.T.);
#44405=EDGE_CURVE('',#33704,#28697,#24265,.T.);
#44406=EDGE_CURVE('',#33841,#28696,#26368,.T.);
#44407=EDGE_CURVE('',#33841,#28695,#24266,.T.);
#44408=EDGE_CURVE('',#33841,#28694,#24267,.T.);
#44409=EDGE_CURVE('',#33841,#28693,#20978,.T.);
#44410=EDGE_CURVE('',#33841,#28692,#26369,.T.);
#44411=EDGE_CURVE('',#33705,#28691,#24268,.T.);
#44412=EDGE_CURVE('',#33842,#28690,#26370,.T.);
#44413=EDGE_CURVE('',#33842,#28689,#24269,.T.);
#44414=EDGE_CURVE('',#33842,#28688,#24270,.T.);
#44415=EDGE_CURVE('',#33842,#28687,#20979,.T.);
#44416=EDGE_CURVE('',#33842,#28686,#26371,.T.);
#44417=EDGE_CURVE('',#33706,#28685,#24271,.T.);
#44418=EDGE_CURVE('',#33843,#28684,#26372,.T.);
#44419=EDGE_CURVE('',#33843,#28683,#24272,.T.);
#44420=EDGE_CURVE('',#33843,#28682,#24273,.T.);
#44421=EDGE_CURVE('',#33843,#28681,#20980,.T.);
#44422=EDGE_CURVE('',#33843,#28680,#26373,.T.);
#44423=EDGE_CURVE('',#33707,#28679,#24274,.T.);
#44424=EDGE_CURVE('',#33844,#28678,#26374,.T.);
#44425=EDGE_CURVE('',#33844,#28677,#24275,.T.);
#44426=EDGE_CURVE('',#33844,#28676,#24276,.T.);
#44427=EDGE_CURVE('',#33844,#28675,#20981,.T.);
#44428=EDGE_CURVE('',#33844,#28674,#26375,.T.);
#44429=EDGE_CURVE('',#33708,#28673,#24277,.T.);
#44430=EDGE_CURVE('',#33845,#28672,#26376,.T.);
#44431=EDGE_CURVE('',#33845,#28671,#24278,.T.);
#44432=EDGE_CURVE('',#33845,#28670,#24279,.T.);
#44433=EDGE_CURVE('',#33845,#28669,#20982,.T.);
#44434=EDGE_CURVE('',#33845,#28668,#26377,.T.);
#44435=EDGE_CURVE('',#33709,#28667,#24280,.T.);
#44436=EDGE_CURVE('',#33846,#28666,#26378,.T.);
#44437=EDGE_CURVE('',#33846,#28665,#24281,.T.);
#44438=EDGE_CURVE('',#33846,#28664,#24282,.T.);
#44439=EDGE_CURVE('',#33846,#28663,#20983,.T.);
#44440=EDGE_CURVE('',#33846,#28662,#26379,.T.);
#44441=EDGE_CURVE('',#33710,#28661,#24283,.T.);
#44442=EDGE_CURVE('',#33847,#28660,#26380,.T.);
#44443=EDGE_CURVE('',#33847,#28659,#24284,.T.);
#44444=EDGE_CURVE('',#33847,#28658,#24285,.T.);
#44445=EDGE_CURVE('',#33847,#28657,#20984,.T.);
#44446=EDGE_CURVE('',#33847,#28656,#26381,.T.);
#44447=EDGE_CURVE('',#33711,#28655,#24286,.T.);
#44448=EDGE_CURVE('',#33848,#28654,#26382,.T.);
#44449=EDGE_CURVE('',#33848,#28653,#24287,.T.);
#44450=EDGE_CURVE('',#33848,#28652,#24288,.T.);
#44451=EDGE_CURVE('',#33848,#28651,#20985,.T.);
#44452=EDGE_CURVE('',#33848,#28650,#26383,.T.);
#44453=EDGE_CURVE('',#33712,#28649,#24289,.T.);
#44454=EDGE_CURVE('',#33849,#28648,#26384,.T.);
#44455=EDGE_CURVE('',#33849,#28647,#4457,.T.);
#44456=EDGE_CURVE('',#33849,#28646,#24290,.T.);
#44457=EDGE_CURVE('',#33849,#28645,#20986,.T.);
#44458=EDGE_CURVE('',#33849,#28644,#26385,.T.);
#44459=EDGE_CURVE('',#33713,#28643,#24291,.T.);
#44460=EDGE_CURVE('',#33850,#28642,#26386,.T.);
#44461=EDGE_CURVE('',#33850,#28641,#24292,.T.);
#44462=EDGE_CURVE('',#33850,#28640,#24293,.T.);
#44463=EDGE_CURVE('',#33850,#28639,#20987,.T.);
#44464=EDGE_CURVE('',#33850,#28638,#26387,.T.);
#44465=EDGE_CURVE('',#33714,#28637,#24294,.T.);
#44466=EDGE_CURVE('',#33851,#28636,#26388,.T.);
#44467=EDGE_CURVE('',#33851,#28635,#24295,.T.);
#44468=EDGE_CURVE('',#33851,#28634,#24296,.T.);
#44469=EDGE_CURVE('',#33851,#28633,#20988,.T.);
#44470=EDGE_CURVE('',#33851,#28632,#26389,.T.);
#44471=EDGE_CURVE('',#33715,#28631,#24297,.T.);
#44472=EDGE_CURVE('',#33852,#28630,#26390,.T.);
#44473=EDGE_CURVE('',#33852,#28629,#24298,.T.);
#44474=EDGE_CURVE('',#33852,#28628,#24299,.T.);
#44475=EDGE_CURVE('',#33852,#28627,#20989,.T.);
#44476=EDGE_CURVE('',#33852,#28626,#26391,.T.);
#44477=EDGE_CURVE('',#33716,#28625,#24300,.T.);
#44478=EDGE_CURVE('',#33853,#28624,#26392,.T.);
#44479=EDGE_CURVE('',#33853,#28623,#24301,.T.);
#44480=EDGE_CURVE('',#33853,#28622,#24302,.T.);
#44481=EDGE_CURVE('',#33853,#28621,#20990,.T.);
#44482=EDGE_CURVE('',#33853,#28620,#26393,.T.);
#44483=EDGE_CURVE('',#33854,#33854,#20991,.T.);
#44484=EDGE_CURVE('',#33854,#33855,#26394,.T.);
#44485=EDGE_CURVE('',#33855,#33855,#20992,.T.);
#44486=EDGE_CURVE('',#33856,#33857,#20993,.T.);
#44487=EDGE_CURVE('',#33857,#33858,#26395,.T.);
#44488=EDGE_CURVE('',#33858,#33859,#24303,.T.);
#44489=EDGE_CURVE('',#33859,#33860,#20994,.T.);
#44490=EDGE_CURVE('',#33860,#33861,#24304,.T.);
#44491=EDGE_CURVE('',#33861,#33862,#26396,.T.);
#44492=EDGE_CURVE('',#33862,#33863,#20995,.T.);
#44493=EDGE_CURVE('',#33863,#33864,#26397,.T.);
#44494=EDGE_CURVE('',#33864,#33864,#20996,.T.);
#44495=EDGE_CURVE('',#33863,#33865,#20997,.T.);
#44496=EDGE_CURVE('',#33865,#33866,#26398,.T.);
#44497=EDGE_CURVE('',#33866,#33867,#24305,.T.);
#44498=EDGE_CURVE('',#33867,#33868,#20998,.T.);
#44499=EDGE_CURVE('',#33868,#33869,#24306,.T.);
#44500=EDGE_CURVE('',#33869,#33856,#26399,.T.);
#44501=EDGE_CURVE('',#33870,#33871,#20999,.T.);
#44502=EDGE_CURVE('',#33871,#33870,#21000,.T.);
#44503=EDGE_CURVE('',#33871,#33872,#26400,.T.);
#44504=EDGE_CURVE('',#33872,#33872,#21001,.T.);
#44505=EDGE_CURVE('',#33873,#33874,#24307,.T.);
#44506=EDGE_CURVE('',#33874,#33875,#24308,.T.);
#44507=EDGE_CURVE('',#33859,#33875,#26401,.T.);
#44508=EDGE_CURVE('',#33858,#33869,#21002,.T.);
#44509=EDGE_CURVE('',#33868,#33876,#26402,.T.);
#44510=EDGE_CURVE('',#33876,#33873,#24309,.T.);
#44511=EDGE_CURVE('',#33870,#33877,#26403,.T.);
#44512=EDGE_CURVE('',#33877,#33877,#21003,.T.);
#44513=EDGE_CURVE('',#33878,#33876,#21004,.T.);
#44514=EDGE_CURVE('',#33879,#33878,#24310,.T.);
#44515=EDGE_CURVE('',#33873,#33879,#21005,.T.);
#44516=EDGE_CURVE('',#33877,#33880,#26404,.T.);
#44517=EDGE_CURVE('',#33881,#33880,#24311,.F.);
#44518=EDGE_CURVE('',#33874,#33881,#21006,.T.);
#44519=EDGE_CURVE('',#33880,#33879,#24312,.F.);
#44520=EDGE_CURVE('',#33861,#33866,#21007,.T.);
#44521=EDGE_CURVE('',#33865,#33862,#26405,.T.);
#44522=EDGE_CURVE('',#33860,#33882,#26406,.T.);
#44523=EDGE_CURVE('',#33882,#33881,#24313,.T.);
#44524=EDGE_CURVE('',#33878,#33867,#26407,.T.);
#44525=EDGE_CURVE('',#33875,#33882,#21008,.T.);
#44526=EDGE_CURVE('',#33857,#33856,#26408,.T.);
#44527=EDGE_CURVE('',#33883,#33884,#21009,.T.);
#44528=EDGE_CURVE('',#33885,#33883,#24314,.T.);
#44529=EDGE_CURVE('',#33884,#33885,#24315,.T.);
#44530=EDGE_CURVE('',#33886,#33887,#24316,.T.);
#44531=EDGE_CURVE('',#33888,#33886,#24317,.T.);
#44532=EDGE_CURVE('',#33887,#33888,#21010,.T.);
#44533=EDGE_CURVE('',#33889,#33890,#21011,.T.);
#44534=EDGE_CURVE('',#33890,#33891,#26409,.T.);
#44535=EDGE_CURVE('',#33891,#33891,#21012,.T.);
#44536=EDGE_CURVE('',#33890,#33889,#21013,.T.);
#44537=EDGE_CURVE('',#33892,#33892,#21014,.T.);
#44538=EDGE_CURVE('',#33892,#33893,#26410,.T.);
#44539=EDGE_CURVE('',#33893,#33893,#21015,.T.);
#44540=EDGE_CURVE('',#33894,#33894,#21016,.T.);
#44541=EDGE_CURVE('',#33894,#33892,#26411,.T.);
#44542=EDGE_CURVE('',#33895,#33896,#24318,.T.);
#44543=EDGE_CURVE('',#33896,#33897,#26412,.T.);
#44544=EDGE_CURVE('',#33898,#33897,#24319,.F.);
#44545=EDGE_CURVE('',#33895,#33898,#26413,.T.);
#44546=EDGE_CURVE('',#33889,#33899,#26414,.T.);
#44547=EDGE_CURVE('',#33899,#33899,#21017,.T.);
#44548=EDGE_CURVE('',#33900,#33901,#21018,.T.);
#44549=EDGE_CURVE('',#33902,#33900,#24320,.F.);
#44550=EDGE_CURVE('',#33903,#33902,#21019,.T.);
#44551=EDGE_CURVE('',#33904,#33903,#26415,.T.);
#44552=EDGE_CURVE('',#33904,#33905,#21020,.T.);
#44553=EDGE_CURVE('',#33906,#33905,#24321,.F.);
#44554=EDGE_CURVE('',#33907,#33906,#21021,.T.);
#44555=EDGE_CURVE('',#33901,#33907,#24322,.T.);
#44556=EDGE_CURVE('',#33897,#33908,#24323,.T.);
#44557=EDGE_CURVE('',#33909,#33908,#26416,.T.);
#44558=EDGE_CURVE('',#33909,#33910,#24324,.T.);
#44559=EDGE_CURVE('',#33911,#33910,#26417,.T.);
#44560=EDGE_CURVE('',#33911,#33898,#24325,.T.);
#44561=EDGE_CURVE('',#33912,#33911,#26418,.T.);
#44562=EDGE_CURVE('',#33912,#33895,#24326,.T.);
#44563=EDGE_CURVE('',#33908,#33913,#26419,.T.);
#44564=EDGE_CURVE('',#33896,#33913,#24327,.T.);
#44565=EDGE_CURVE('',#33914,#33915,#24328,.T.);
#44566=EDGE_CURVE('',#33910,#33914,#24329,.T.);
#44567=EDGE_CURVE('',#33915,#33909,#24330,.T.);
#44568=EDGE_CURVE('',#33916,#33917,#4458,.T.);
#44569=EDGE_CURVE('',#33913,#33916,#26420,.T.);
#44570=EDGE_CURVE('',#33917,#33912,#26421,.T.);
#44571=EDGE_CURVE('',#33918,#33919,#24331,.T.);
#44572=EDGE_CURVE('',#33920,#33919,#24332,.T.);
#44573=EDGE_CURVE('',#33920,#33921,#24333,.T.);
#44574=EDGE_CURVE('',#33921,#33918,#24334,.T.);
#44575=EDGE_CURVE('',#33920,#33915,#24335,.T.);
#44576=EDGE_CURVE('',#33919,#33914,#24336,.T.);
#44577=EDGE_CURVE('',#33916,#33922,#24337,.T.);
#44578=EDGE_CURVE('',#33917,#33923,#24338,.T.);
#44579=EDGE_CURVE('',#33922,#33923,#24339,.T.);
#44580=EDGE_CURVE('',#33923,#33924,#24340,.T.);
#44581=EDGE_CURVE('',#33925,#33924,#21022,.T.);
#44582=EDGE_CURVE('',#33922,#33925,#24341,.T.);
#44583=EDGE_CURVE('',#33907,#33918,#24342,.T.);
#44584=EDGE_CURVE('',#33901,#33921,#24343,.T.);
#44585=EDGE_CURVE('',#33926,#33927,#21023,.T.);
#44586=EDGE_CURVE('',#33926,#33904,#26422,.T.);
#44587=EDGE_CURVE('',#33903,#33927,#26423,.T.);
#44588=EDGE_CURVE('',#33928,#33902,#192,.T.);
#44589=EDGE_CURVE('',#33927,#33928,#26424,.T.);
#44590=EDGE_CURVE('',#33900,#33925,#24344,.T.);
#44591=EDGE_CURVE('',#33924,#33906,#24345,.T.);
#44592=EDGE_CURVE('',#33905,#33929,#193,.T.);
#44593=EDGE_CURVE('',#33928,#33929,#24346,.T.);
#44594=EDGE_CURVE('',#33929,#33926,#26425,.T.);
#44595=EDGE_CURVE('',#33930,#33930,#21024,.T.);
#44596=EDGE_CURVE('',#33930,#33931,#26426,.T.);
#44597=EDGE_CURVE('',#33931,#33932,#24347,.T.);
#44598=EDGE_CURVE('',#33932,#33933,#26427,.T.);
#44599=EDGE_CURVE('',#33933,#33933,#21025,.T.);
#44600=EDGE_CURVE('',#33932,#33934,#24348,.T.);
#44601=EDGE_CURVE('',#33934,#33931,#24349,.T.);
#44602=EDGE_CURVE('',#33935,#33936,#24350,.T.);
#44603=EDGE_CURVE('',#33936,#33935,#24351,.T.);
#44604=EDGE_CURVE('',#33937,#33938,#21026,.T.);
#44605=EDGE_CURVE('',#33937,#33939,#21027,.T.);
#44606=EDGE_CURVE('',#33940,#33939,#21028,.T.);
#44607=EDGE_CURVE('',#33941,#33940,#21029,.T.);
#44608=EDGE_CURVE('',#33941,#33938,#21030,.T.);
#44609=EDGE_CURVE('',#33942,#33942,#21031,.T.);
#44610=EDGE_CURVE('',#33943,#33944,#21032,.T.);
#44611=EDGE_CURVE('',#33944,#33943,#21033,.T.);
#44612=EDGE_CURVE('',#33944,#33940,#26428,.T.);
#44613=EDGE_CURVE('',#33939,#33945,#26429,.T.);
#44614=EDGE_CURVE('',#33946,#33945,#21034,.T.);
#44615=EDGE_CURVE('',#33946,#33937,#26430,.T.);
#44616=EDGE_CURVE('',#33938,#33947,#26431,.T.);
#44617=EDGE_CURVE('',#33948,#33947,#21035,.T.);
#44618=EDGE_CURVE('',#33948,#33941,#26432,.T.);
#44619=EDGE_CURVE('',#33949,#33949,#21036,.T.);
#44620=EDGE_CURVE('',#33949,#33950,#26433,.T.);
#44621=EDGE_CURVE('',#33950,#33950,#21037,.T.);
#44622=EDGE_CURVE('',#33943,#33951,#26434,.T.);
#44623=EDGE_CURVE('',#33951,#33951,#21038,.T.);
#44624=EDGE_CURVE('',#33936,#33949,#26435,.T.);
#44625=EDGE_CURVE('',#33945,#33946,#26436,.T.);
#44626=EDGE_CURVE('',#33947,#33948,#26437,.T.);
#44627=EDGE_CURVE('',#33942,#33934,#26438,.T.);
#44628=EDGE_CURVE('',#33952,#33953,#21039,.T.);
#44629=EDGE_CURVE('',#33953,#33952,#21040,.T.);
#44630=EDGE_CURVE('',#33953,#33954,#26439,.T.);
#44631=EDGE_CURVE('',#33955,#33954,#24352,.F.);
#44632=EDGE_CURVE('',#33956,#33955,#24353,.F.);
#44633=EDGE_CURVE('',#33956,#33957,#26440,.T.);
#44634=EDGE_CURVE('',#33957,#33957,#21041,.T.);
#44635=EDGE_CURVE('',#33954,#33956,#24354,.F.);
#44636=EDGE_CURVE('',#33958,#33959,#24355,.F.);
#44637=EDGE_CURVE('',#33959,#33958,#24356,.F.);
#44638=EDGE_CURVE('',#33957,#33960,#26441,.T.);
#44639=EDGE_CURVE('',#33960,#33960,#21042,.T.);
#44640=EDGE_CURVE('',#33952,#33961,#26442,.T.);
#44641=EDGE_CURVE('',#33961,#33961,#21043,.T.);
#44642=EDGE_CURVE('',#33955,#33959,#26443,.T.);
#44643=EDGE_CURVE('',#33962,#33962,#21044,.T.);
#44644=EDGE_CURVE('',#33962,#33963,#26444,.T.);
#44645=EDGE_CURVE('',#33963,#33963,#21045,.T.);
#44646=ORIENTED_EDGE('',*,*,#33964,.F.);
#44647=ORIENTED_EDGE('',*,*,#33965,.F.);
#44648=ORIENTED_EDGE('',*,*,#33966,.F.);
#44649=ORIENTED_EDGE('',*,*,#33967,.F.);
#44650=ORIENTED_EDGE('',*,*,#33968,.F.);
#44651=ORIENTED_EDGE('',*,*,#33969,.F.);
#44652=ORIENTED_EDGE('',*,*,#33970,.F.);
#44653=ORIENTED_EDGE('',*,*,#33971,.F.);
#44654=ORIENTED_EDGE('',*,*,#33972,.F.);
#44655=ORIENTED_EDGE('',*,*,#33973,.F.);
#44656=ORIENTED_EDGE('',*,*,#33974,.F.);
#44657=ORIENTED_EDGE('',*,*,#33975,.F.);
#44658=ORIENTED_EDGE('',*,*,#33976,.F.);
#44659=ORIENTED_EDGE('',*,*,#33977,.F.);
#44660=ORIENTED_EDGE('',*,*,#33978,.F.);
#44661=ORIENTED_EDGE('',*,*,#33979,.F.);
#44662=ORIENTED_EDGE('',*,*,#33980,.F.);
#44663=ORIENTED_EDGE('',*,*,#33981,.F.);
#44664=ORIENTED_EDGE('',*,*,#33982,.F.);
#44665=ORIENTED_EDGE('',*,*,#33983,.F.);
#44666=ORIENTED_EDGE('',*,*,#33984,.F.);
#44667=ORIENTED_EDGE('',*,*,#33985,.F.);
#44668=ORIENTED_EDGE('',*,*,#33986,.F.);
#44669=ORIENTED_EDGE('',*,*,#33987,.F.);
#44670=ORIENTED_EDGE('',*,*,#33988,.F.);
#44671=ORIENTED_EDGE('',*,*,#33989,.F.);
#44672=ORIENTED_EDGE('',*,*,#33990,.F.);
#44673=ORIENTED_EDGE('',*,*,#33991,.F.);
#44674=ORIENTED_EDGE('',*,*,#33992,.F.);
#44675=ORIENTED_EDGE('',*,*,#33993,.F.);
#44676=ORIENTED_EDGE('',*,*,#33994,.F.);
#44677=ORIENTED_EDGE('',*,*,#33995,.F.);
#44678=ORIENTED_EDGE('',*,*,#33996,.F.);
#44679=ORIENTED_EDGE('',*,*,#33997,.F.);
#44680=ORIENTED_EDGE('',*,*,#33998,.F.);
#44681=ORIENTED_EDGE('',*,*,#33999,.F.);
#44682=ORIENTED_EDGE('',*,*,#34000,.F.);
#44683=ORIENTED_EDGE('',*,*,#34001,.F.);
#44684=ORIENTED_EDGE('',*,*,#34002,.F.);
#44685=ORIENTED_EDGE('',*,*,#34003,.F.);
#44686=ORIENTED_EDGE('',*,*,#34004,.F.);
#44687=ORIENTED_EDGE('',*,*,#34005,.F.);
#44688=ORIENTED_EDGE('',*,*,#34006,.F.);
#44689=ORIENTED_EDGE('',*,*,#34007,.F.);
#44690=ORIENTED_EDGE('',*,*,#34008,.F.);
#44691=ORIENTED_EDGE('',*,*,#34009,.F.);
#44692=ORIENTED_EDGE('',*,*,#34010,.F.);
#44693=ORIENTED_EDGE('',*,*,#34011,.F.);
#44694=ORIENTED_EDGE('',*,*,#34012,.F.);
#44695=ORIENTED_EDGE('',*,*,#34013,.F.);
#44696=ORIENTED_EDGE('',*,*,#34014,.F.);
#44697=ORIENTED_EDGE('',*,*,#34015,.F.);
#44698=ORIENTED_EDGE('',*,*,#34016,.F.);
#44699=ORIENTED_EDGE('',*,*,#34017,.F.);
#44700=ORIENTED_EDGE('',*,*,#34018,.F.);
#44701=ORIENTED_EDGE('',*,*,#34019,.F.);
#44702=ORIENTED_EDGE('',*,*,#34020,.F.);
#44703=ORIENTED_EDGE('',*,*,#34021,.F.);
#44704=ORIENTED_EDGE('',*,*,#34022,.F.);
#44705=ORIENTED_EDGE('',*,*,#34023,.F.);
#44706=ORIENTED_EDGE('',*,*,#34024,.F.);
#44707=ORIENTED_EDGE('',*,*,#34025,.F.);
#44708=ORIENTED_EDGE('',*,*,#34026,.F.);
#44709=ORIENTED_EDGE('',*,*,#34027,.F.);
#44710=ORIENTED_EDGE('',*,*,#34028,.F.);
#44711=ORIENTED_EDGE('',*,*,#34029,.F.);
#44712=ORIENTED_EDGE('',*,*,#34030,.F.);
#44713=ORIENTED_EDGE('',*,*,#34031,.F.);
#44714=ORIENTED_EDGE('',*,*,#34032,.F.);
#44715=ORIENTED_EDGE('',*,*,#34033,.F.);
#44716=ORIENTED_EDGE('',*,*,#34034,.F.);
#44717=ORIENTED_EDGE('',*,*,#34035,.F.);
#44718=ORIENTED_EDGE('',*,*,#34036,.F.);
#44719=ORIENTED_EDGE('',*,*,#34037,.F.);
#44720=ORIENTED_EDGE('',*,*,#34038,.F.);
#44721=ORIENTED_EDGE('',*,*,#34039,.F.);
#44722=ORIENTED_EDGE('',*,*,#34040,.F.);
#44723=ORIENTED_EDGE('',*,*,#34041,.F.);
#44724=ORIENTED_EDGE('',*,*,#34042,.F.);
#44725=ORIENTED_EDGE('',*,*,#34043,.F.);
#44726=ORIENTED_EDGE('',*,*,#34044,.F.);
#44727=ORIENTED_EDGE('',*,*,#34045,.F.);
#44728=ORIENTED_EDGE('',*,*,#34046,.F.);
#44729=ORIENTED_EDGE('',*,*,#34047,.F.);
#44730=ORIENTED_EDGE('',*,*,#34048,.F.);
#44731=ORIENTED_EDGE('',*,*,#34049,.F.);
#44732=ORIENTED_EDGE('',*,*,#34050,.F.);
#44733=ORIENTED_EDGE('',*,*,#34051,.F.);
#44734=ORIENTED_EDGE('',*,*,#34052,.F.);
#44735=ORIENTED_EDGE('',*,*,#34053,.F.);
#44736=ORIENTED_EDGE('',*,*,#34054,.F.);
#44737=ORIENTED_EDGE('',*,*,#34055,.F.);
#44738=ORIENTED_EDGE('',*,*,#34056,.F.);
#44739=ORIENTED_EDGE('',*,*,#34057,.F.);
#44740=ORIENTED_EDGE('',*,*,#34058,.F.);
#44741=ORIENTED_EDGE('',*,*,#34059,.F.);
#44742=ORIENTED_EDGE('',*,*,#34060,.F.);
#44743=ORIENTED_EDGE('',*,*,#34061,.F.);
#44744=ORIENTED_EDGE('',*,*,#34062,.F.);
#44745=ORIENTED_EDGE('',*,*,#34063,.F.);
#44746=ORIENTED_EDGE('',*,*,#34064,.F.);
#44747=ORIENTED_EDGE('',*,*,#34065,.F.);
#44748=ORIENTED_EDGE('',*,*,#34066,.F.);
#44749=ORIENTED_EDGE('',*,*,#34067,.F.);
#44750=ORIENTED_EDGE('',*,*,#34068,.F.);
#44751=ORIENTED_EDGE('',*,*,#34069,.F.);
#44752=ORIENTED_EDGE('',*,*,#34070,.F.);
#44753=ORIENTED_EDGE('',*,*,#34071,.F.);
#44754=ORIENTED_EDGE('',*,*,#34072,.F.);
#44755=ORIENTED_EDGE('',*,*,#34073,.F.);
#44756=ORIENTED_EDGE('',*,*,#34074,.F.);
#44757=ORIENTED_EDGE('',*,*,#34075,.F.);
#44758=ORIENTED_EDGE('',*,*,#34076,.F.);
#44759=ORIENTED_EDGE('',*,*,#34077,.F.);
#44760=ORIENTED_EDGE('',*,*,#34078,.F.);
#44761=ORIENTED_EDGE('',*,*,#34079,.F.);
#44762=ORIENTED_EDGE('',*,*,#34080,.F.);
#44763=ORIENTED_EDGE('',*,*,#34081,.F.);
#44764=ORIENTED_EDGE('',*,*,#34082,.F.);
#44765=ORIENTED_EDGE('',*,*,#34083,.F.);
#44766=ORIENTED_EDGE('',*,*,#34084,.F.);
#44767=ORIENTED_EDGE('',*,*,#34085,.F.);
#44768=ORIENTED_EDGE('',*,*,#34086,.F.);
#44769=ORIENTED_EDGE('',*,*,#34087,.F.);
#44770=ORIENTED_EDGE('',*,*,#34088,.F.);
#44771=ORIENTED_EDGE('',*,*,#34089,.F.);
#44772=ORIENTED_EDGE('',*,*,#34090,.F.);
#44773=ORIENTED_EDGE('',*,*,#34091,.F.);
#44774=ORIENTED_EDGE('',*,*,#34092,.F.);
#44775=ORIENTED_EDGE('',*,*,#34093,.F.);
#44776=ORIENTED_EDGE('',*,*,#34094,.F.);
#44777=ORIENTED_EDGE('',*,*,#34095,.F.);
#44778=ORIENTED_EDGE('',*,*,#34096,.F.);
#44779=ORIENTED_EDGE('',*,*,#34097,.F.);
#44780=ORIENTED_EDGE('',*,*,#34098,.F.);
#44781=ORIENTED_EDGE('',*,*,#34099,.F.);
#44782=ORIENTED_EDGE('',*,*,#34100,.F.);
#44783=ORIENTED_EDGE('',*,*,#34101,.F.);
#44784=ORIENTED_EDGE('',*,*,#34102,.F.);
#44785=ORIENTED_EDGE('',*,*,#34103,.F.);
#44786=ORIENTED_EDGE('',*,*,#34104,.F.);
#44787=ORIENTED_EDGE('',*,*,#34105,.F.);
#44788=ORIENTED_EDGE('',*,*,#34106,.F.);
#44789=ORIENTED_EDGE('',*,*,#34107,.F.);
#44790=ORIENTED_EDGE('',*,*,#34108,.F.);
#44791=ORIENTED_EDGE('',*,*,#34109,.F.);
#44792=ORIENTED_EDGE('',*,*,#34110,.F.);
#44793=ORIENTED_EDGE('',*,*,#34111,.F.);
#44794=ORIENTED_EDGE('',*,*,#34112,.F.);
#44795=ORIENTED_EDGE('',*,*,#34113,.F.);
#44796=ORIENTED_EDGE('',*,*,#34114,.F.);
#44797=ORIENTED_EDGE('',*,*,#34115,.F.);
#44798=ORIENTED_EDGE('',*,*,#34116,.F.);
#44799=ORIENTED_EDGE('',*,*,#34117,.F.);
#44800=ORIENTED_EDGE('',*,*,#34118,.F.);
#44801=ORIENTED_EDGE('',*,*,#34119,.F.);
#44802=ORIENTED_EDGE('',*,*,#34120,.F.);
#44803=ORIENTED_EDGE('',*,*,#34121,.F.);
#44804=ORIENTED_EDGE('',*,*,#34122,.F.);
#44805=ORIENTED_EDGE('',*,*,#34123,.F.);
#44806=ORIENTED_EDGE('',*,*,#34124,.F.);
#44807=ORIENTED_EDGE('',*,*,#34125,.F.);
#44808=ORIENTED_EDGE('',*,*,#34126,.F.);
#44809=ORIENTED_EDGE('',*,*,#34127,.F.);
#44810=ORIENTED_EDGE('',*,*,#34128,.F.);
#44811=ORIENTED_EDGE('',*,*,#34129,.F.);
#44812=ORIENTED_EDGE('',*,*,#34130,.F.);
#44813=ORIENTED_EDGE('',*,*,#34131,.F.);
#44814=ORIENTED_EDGE('',*,*,#34132,.F.);
#44815=ORIENTED_EDGE('',*,*,#34133,.F.);
#44816=ORIENTED_EDGE('',*,*,#34134,.F.);
#44817=ORIENTED_EDGE('',*,*,#34135,.F.);
#44818=ORIENTED_EDGE('',*,*,#34136,.F.);
#44819=ORIENTED_EDGE('',*,*,#34137,.F.);
#44820=ORIENTED_EDGE('',*,*,#34138,.T.);
#44821=ORIENTED_EDGE('',*,*,#34139,.F.);
#44822=ORIENTED_EDGE('',*,*,#34138,.F.);
#44823=ORIENTED_EDGE('',*,*,#34140,.F.);
#44824=ORIENTED_EDGE('',*,*,#34141,.F.);
#44825=ORIENTED_EDGE('',*,*,#34142,.T.);
#44826=ORIENTED_EDGE('',*,*,#34143,.T.);
#44827=ORIENTED_EDGE('',*,*,#34144,.T.);
#44828=ORIENTED_EDGE('',*,*,#34143,.F.);
#44829=ORIENTED_EDGE('',*,*,#33964,.T.);
#44830=ORIENTED_EDGE('',*,*,#34145,.F.);
#44831=ORIENTED_EDGE('',*,*,#34146,.F.);
#44832=ORIENTED_EDGE('',*,*,#34147,.T.);
#44833=ORIENTED_EDGE('',*,*,#34148,.T.);
#44834=ORIENTED_EDGE('',*,*,#34149,.F.);
#44835=ORIENTED_EDGE('',*,*,#34148,.F.);
#44836=ORIENTED_EDGE('',*,*,#34150,.T.);
#44837=ORIENTED_EDGE('',*,*,#34151,.T.);
#44838=ORIENTED_EDGE('',*,*,#34152,.F.);
#44839=ORIENTED_EDGE('',*,*,#34151,.F.);
#44840=ORIENTED_EDGE('',*,*,#34153,.T.);
#44841=ORIENTED_EDGE('',*,*,#34150,.F.);
#44842=ORIENTED_EDGE('',*,*,#34154,.T.);
#44843=ORIENTED_EDGE('',*,*,#34155,.T.);
#44844=ORIENTED_EDGE('',*,*,#34154,.F.);
#44845=ORIENTED_EDGE('',*,*,#34153,.F.);
#44846=ORIENTED_EDGE('',*,*,#34156,.F.);
#44847=ORIENTED_EDGE('',*,*,#34157,.F.);
#44848=ORIENTED_EDGE('',*,*,#34158,.F.);
#44849=ORIENTED_EDGE('',*,*,#34159,.F.);
#44850=ORIENTED_EDGE('',*,*,#34160,.F.);
#44851=ORIENTED_EDGE('',*,*,#34161,.F.);
#44852=ORIENTED_EDGE('',*,*,#34162,.F.);
#44853=ORIENTED_EDGE('',*,*,#34163,.F.);
#44854=ORIENTED_EDGE('',*,*,#34164,.F.);
#44855=ORIENTED_EDGE('',*,*,#34165,.F.);
#44856=ORIENTED_EDGE('',*,*,#34166,.F.);
#44857=ORIENTED_EDGE('',*,*,#34167,.F.);
#44858=ORIENTED_EDGE('',*,*,#34168,.F.);
#44859=ORIENTED_EDGE('',*,*,#34169,.F.);
#44860=ORIENTED_EDGE('',*,*,#34170,.F.);
#44861=ORIENTED_EDGE('',*,*,#34171,.F.);
#44862=ORIENTED_EDGE('',*,*,#34172,.F.);
#44863=ORIENTED_EDGE('',*,*,#34173,.F.);
#44864=ORIENTED_EDGE('',*,*,#34174,.F.);
#44865=ORIENTED_EDGE('',*,*,#34175,.F.);
#44866=ORIENTED_EDGE('',*,*,#34176,.F.);
#44867=ORIENTED_EDGE('',*,*,#34177,.F.);
#44868=ORIENTED_EDGE('',*,*,#34178,.F.);
#44869=ORIENTED_EDGE('',*,*,#34179,.F.);
#44870=ORIENTED_EDGE('',*,*,#34180,.F.);
#44871=ORIENTED_EDGE('',*,*,#34181,.F.);
#44872=ORIENTED_EDGE('',*,*,#34182,.F.);
#44873=ORIENTED_EDGE('',*,*,#34183,.F.);
#44874=ORIENTED_EDGE('',*,*,#34184,.F.);
#44875=ORIENTED_EDGE('',*,*,#34185,.F.);
#44876=ORIENTED_EDGE('',*,*,#34186,.F.);
#44877=ORIENTED_EDGE('',*,*,#34187,.F.);
#44878=ORIENTED_EDGE('',*,*,#34188,.F.);
#44879=ORIENTED_EDGE('',*,*,#34189,.F.);
#44880=ORIENTED_EDGE('',*,*,#34190,.F.);
#44881=ORIENTED_EDGE('',*,*,#34191,.F.);
#44882=ORIENTED_EDGE('',*,*,#34192,.F.);
#44883=ORIENTED_EDGE('',*,*,#34193,.F.);
#44884=ORIENTED_EDGE('',*,*,#34194,.F.);
#44885=ORIENTED_EDGE('',*,*,#34195,.F.);
#44886=ORIENTED_EDGE('',*,*,#34196,.F.);
#44887=ORIENTED_EDGE('',*,*,#34197,.F.);
#44888=ORIENTED_EDGE('',*,*,#34198,.F.);
#44889=ORIENTED_EDGE('',*,*,#34199,.F.);
#44890=ORIENTED_EDGE('',*,*,#34200,.F.);
#44891=ORIENTED_EDGE('',*,*,#34201,.F.);
#44892=ORIENTED_EDGE('',*,*,#34202,.F.);
#44893=ORIENTED_EDGE('',*,*,#34203,.F.);
#44894=ORIENTED_EDGE('',*,*,#34204,.F.);
#44895=ORIENTED_EDGE('',*,*,#34205,.F.);
#44896=ORIENTED_EDGE('',*,*,#34206,.F.);
#44897=ORIENTED_EDGE('',*,*,#34207,.F.);
#44898=ORIENTED_EDGE('',*,*,#34208,.F.);
#44899=ORIENTED_EDGE('',*,*,#34209,.F.);
#44900=ORIENTED_EDGE('',*,*,#34210,.F.);
#44901=ORIENTED_EDGE('',*,*,#34211,.F.);
#44902=ORIENTED_EDGE('',*,*,#34212,.F.);
#44903=ORIENTED_EDGE('',*,*,#34213,.F.);
#44904=ORIENTED_EDGE('',*,*,#34214,.F.);
#44905=ORIENTED_EDGE('',*,*,#34215,.F.);
#44906=ORIENTED_EDGE('',*,*,#34216,.F.);
#44907=ORIENTED_EDGE('',*,*,#34217,.F.);
#44908=ORIENTED_EDGE('',*,*,#34218,.F.);
#44909=ORIENTED_EDGE('',*,*,#34219,.F.);
#44910=ORIENTED_EDGE('',*,*,#34220,.F.);
#44911=ORIENTED_EDGE('',*,*,#34221,.F.);
#44912=ORIENTED_EDGE('',*,*,#34222,.F.);
#44913=ORIENTED_EDGE('',*,*,#34223,.F.);
#44914=ORIENTED_EDGE('',*,*,#34224,.F.);
#44915=ORIENTED_EDGE('',*,*,#34225,.F.);
#44916=ORIENTED_EDGE('',*,*,#34226,.F.);
#44917=ORIENTED_EDGE('',*,*,#34227,.F.);
#44918=ORIENTED_EDGE('',*,*,#34228,.F.);
#44919=ORIENTED_EDGE('',*,*,#34229,.F.);
#44920=ORIENTED_EDGE('',*,*,#34230,.F.);
#44921=ORIENTED_EDGE('',*,*,#34231,.F.);
#44922=ORIENTED_EDGE('',*,*,#34232,.F.);
#44923=ORIENTED_EDGE('',*,*,#34233,.F.);
#44924=ORIENTED_EDGE('',*,*,#34234,.F.);
#44925=ORIENTED_EDGE('',*,*,#34235,.F.);
#44926=ORIENTED_EDGE('',*,*,#34236,.F.);
#44927=ORIENTED_EDGE('',*,*,#34237,.F.);
#44928=ORIENTED_EDGE('',*,*,#34238,.F.);
#44929=ORIENTED_EDGE('',*,*,#34239,.F.);
#44930=ORIENTED_EDGE('',*,*,#34240,.F.);
#44931=ORIENTED_EDGE('',*,*,#34241,.F.);
#44932=ORIENTED_EDGE('',*,*,#34242,.F.);
#44933=ORIENTED_EDGE('',*,*,#34243,.F.);
#44934=ORIENTED_EDGE('',*,*,#34244,.T.);
#44935=ORIENTED_EDGE('',*,*,#34245,.F.);
#44936=ORIENTED_EDGE('',*,*,#34244,.F.);
#44937=ORIENTED_EDGE('',*,*,#34246,.F.);
#44938=ORIENTED_EDGE('',*,*,#34247,.F.);
#44939=ORIENTED_EDGE('',*,*,#34248,.F.);
#44940=ORIENTED_EDGE('',*,*,#34249,.F.);
#44941=ORIENTED_EDGE('',*,*,#34250,.F.);
#44942=ORIENTED_EDGE('',*,*,#34251,.F.);
#44943=ORIENTED_EDGE('',*,*,#34252,.F.);
#44944=ORIENTED_EDGE('',*,*,#34253,.F.);
#44945=ORIENTED_EDGE('',*,*,#34254,.F.);
#44946=ORIENTED_EDGE('',*,*,#34255,.F.);
#44947=ORIENTED_EDGE('',*,*,#34256,.F.);
#44948=ORIENTED_EDGE('',*,*,#34257,.F.);
#44949=ORIENTED_EDGE('',*,*,#34258,.F.);
#44950=ORIENTED_EDGE('',*,*,#34259,.F.);
#44951=ORIENTED_EDGE('',*,*,#34260,.F.);
#44952=ORIENTED_EDGE('',*,*,#34261,.F.);
#44953=ORIENTED_EDGE('',*,*,#34262,.F.);
#44954=ORIENTED_EDGE('',*,*,#34263,.F.);
#44955=ORIENTED_EDGE('',*,*,#34264,.F.);
#44956=ORIENTED_EDGE('',*,*,#34265,.F.);
#44957=ORIENTED_EDGE('',*,*,#34266,.F.);
#44958=ORIENTED_EDGE('',*,*,#34267,.F.);
#44959=ORIENTED_EDGE('',*,*,#34268,.F.);
#44960=ORIENTED_EDGE('',*,*,#34269,.F.);
#44961=ORIENTED_EDGE('',*,*,#34270,.F.);
#44962=ORIENTED_EDGE('',*,*,#34271,.F.);
#44963=ORIENTED_EDGE('',*,*,#34272,.F.);
#44964=ORIENTED_EDGE('',*,*,#34273,.F.);
#44965=ORIENTED_EDGE('',*,*,#34274,.F.);
#44966=ORIENTED_EDGE('',*,*,#34275,.F.);
#44967=ORIENTED_EDGE('',*,*,#34276,.F.);
#44968=ORIENTED_EDGE('',*,*,#34277,.F.);
#44969=ORIENTED_EDGE('',*,*,#34278,.F.);
#44970=ORIENTED_EDGE('',*,*,#34279,.F.);
#44971=ORIENTED_EDGE('',*,*,#34280,.F.);
#44972=ORIENTED_EDGE('',*,*,#34281,.F.);
#44973=ORIENTED_EDGE('',*,*,#34282,.F.);
#44974=ORIENTED_EDGE('',*,*,#34283,.F.);
#44975=ORIENTED_EDGE('',*,*,#34284,.F.);
#44976=ORIENTED_EDGE('',*,*,#34285,.F.);
#44977=ORIENTED_EDGE('',*,*,#34286,.F.);
#44978=ORIENTED_EDGE('',*,*,#34287,.F.);
#44979=ORIENTED_EDGE('',*,*,#34288,.F.);
#44980=ORIENTED_EDGE('',*,*,#34289,.F.);
#44981=ORIENTED_EDGE('',*,*,#34290,.F.);
#44982=ORIENTED_EDGE('',*,*,#34291,.F.);
#44983=ORIENTED_EDGE('',*,*,#34292,.F.);
#44984=ORIENTED_EDGE('',*,*,#34293,.F.);
#44985=ORIENTED_EDGE('',*,*,#34294,.F.);
#44986=ORIENTED_EDGE('',*,*,#34295,.F.);
#44987=ORIENTED_EDGE('',*,*,#34296,.F.);
#44988=ORIENTED_EDGE('',*,*,#34297,.F.);
#44989=ORIENTED_EDGE('',*,*,#34298,.F.);
#44990=ORIENTED_EDGE('',*,*,#34299,.F.);
#44991=ORIENTED_EDGE('',*,*,#34300,.F.);
#44992=ORIENTED_EDGE('',*,*,#34301,.F.);
#44993=ORIENTED_EDGE('',*,*,#34302,.F.);
#44994=ORIENTED_EDGE('',*,*,#34303,.F.);
#44995=ORIENTED_EDGE('',*,*,#34304,.F.);
#44996=ORIENTED_EDGE('',*,*,#34305,.F.);
#44997=ORIENTED_EDGE('',*,*,#34306,.F.);
#44998=ORIENTED_EDGE('',*,*,#34307,.F.);
#44999=ORIENTED_EDGE('',*,*,#34308,.F.);
#45000=ORIENTED_EDGE('',*,*,#34309,.F.);
#45001=ORIENTED_EDGE('',*,*,#34310,.F.);
#45002=ORIENTED_EDGE('',*,*,#34311,.F.);
#45003=ORIENTED_EDGE('',*,*,#34312,.F.);
#45004=ORIENTED_EDGE('',*,*,#34313,.F.);
#45005=ORIENTED_EDGE('',*,*,#34314,.F.);
#45006=ORIENTED_EDGE('',*,*,#34315,.F.);
#45007=ORIENTED_EDGE('',*,*,#34316,.F.);
#45008=ORIENTED_EDGE('',*,*,#34317,.F.);
#45009=ORIENTED_EDGE('',*,*,#34318,.F.);
#45010=ORIENTED_EDGE('',*,*,#34319,.F.);
#45011=ORIENTED_EDGE('',*,*,#34320,.F.);
#45012=ORIENTED_EDGE('',*,*,#34321,.F.);
#45013=ORIENTED_EDGE('',*,*,#34322,.F.);
#45014=ORIENTED_EDGE('',*,*,#34323,.F.);
#45015=ORIENTED_EDGE('',*,*,#34324,.F.);
#45016=ORIENTED_EDGE('',*,*,#34325,.F.);
#45017=ORIENTED_EDGE('',*,*,#34326,.F.);
#45018=ORIENTED_EDGE('',*,*,#34327,.F.);
#45019=ORIENTED_EDGE('',*,*,#34328,.F.);
#45020=ORIENTED_EDGE('',*,*,#34329,.F.);
#45021=ORIENTED_EDGE('',*,*,#34330,.F.);
#45022=ORIENTED_EDGE('',*,*,#34331,.F.);
#45023=ORIENTED_EDGE('',*,*,#34332,.F.);
#45024=ORIENTED_EDGE('',*,*,#34333,.F.);
#45025=ORIENTED_EDGE('',*,*,#34334,.F.);
#45026=ORIENTED_EDGE('',*,*,#34335,.F.);
#45027=ORIENTED_EDGE('',*,*,#34336,.F.);
#45028=ORIENTED_EDGE('',*,*,#34337,.F.);
#45029=ORIENTED_EDGE('',*,*,#34338,.F.);
#45030=ORIENTED_EDGE('',*,*,#34339,.F.);
#45031=ORIENTED_EDGE('',*,*,#34340,.F.);
#45032=ORIENTED_EDGE('',*,*,#34341,.F.);
#45033=ORIENTED_EDGE('',*,*,#34342,.F.);
#45034=ORIENTED_EDGE('',*,*,#34343,.F.);
#45035=ORIENTED_EDGE('',*,*,#34344,.F.);
#45036=ORIENTED_EDGE('',*,*,#34345,.F.);
#45037=ORIENTED_EDGE('',*,*,#34346,.F.);
#45038=ORIENTED_EDGE('',*,*,#34347,.F.);
#45039=ORIENTED_EDGE('',*,*,#34348,.F.);
#45040=ORIENTED_EDGE('',*,*,#34349,.F.);
#45041=ORIENTED_EDGE('',*,*,#34350,.F.);
#45042=ORIENTED_EDGE('',*,*,#34351,.F.);
#45043=ORIENTED_EDGE('',*,*,#34352,.F.);
#45044=ORIENTED_EDGE('',*,*,#34353,.F.);
#45045=ORIENTED_EDGE('',*,*,#34354,.F.);
#45046=ORIENTED_EDGE('',*,*,#34355,.F.);
#45047=ORIENTED_EDGE('',*,*,#34356,.F.);
#45048=ORIENTED_EDGE('',*,*,#34357,.F.);
#45049=ORIENTED_EDGE('',*,*,#34358,.F.);
#45050=ORIENTED_EDGE('',*,*,#34359,.F.);
#45051=ORIENTED_EDGE('',*,*,#34360,.F.);
#45052=ORIENTED_EDGE('',*,*,#34361,.F.);
#45053=ORIENTED_EDGE('',*,*,#34362,.F.);
#45054=ORIENTED_EDGE('',*,*,#34363,.F.);
#45055=ORIENTED_EDGE('',*,*,#34364,.F.);
#45056=ORIENTED_EDGE('',*,*,#34365,.F.);
#45057=ORIENTED_EDGE('',*,*,#34366,.F.);
#45058=ORIENTED_EDGE('',*,*,#34367,.F.);
#45059=ORIENTED_EDGE('',*,*,#34368,.F.);
#45060=ORIENTED_EDGE('',*,*,#34362,.T.);
#45061=ORIENTED_EDGE('',*,*,#34369,.F.);
#45062=ORIENTED_EDGE('',*,*,#34370,.F.);
#45063=ORIENTED_EDGE('',*,*,#34371,.F.);
#45064=ORIENTED_EDGE('',*,*,#34372,.F.);
#45065=ORIENTED_EDGE('',*,*,#34373,.F.);
#45066=ORIENTED_EDGE('',*,*,#34374,.F.);
#45067=ORIENTED_EDGE('',*,*,#34375,.F.);
#45068=ORIENTED_EDGE('',*,*,#34376,.F.);
#45069=ORIENTED_EDGE('',*,*,#34377,.F.);
#45070=ORIENTED_EDGE('',*,*,#34378,.F.);
#45071=ORIENTED_EDGE('',*,*,#34379,.F.);
#45072=ORIENTED_EDGE('',*,*,#34380,.F.);
#45073=ORIENTED_EDGE('',*,*,#34381,.F.);
#45074=ORIENTED_EDGE('',*,*,#34382,.F.);
#45075=ORIENTED_EDGE('',*,*,#34383,.F.);
#45076=ORIENTED_EDGE('',*,*,#34384,.F.);
#45077=ORIENTED_EDGE('',*,*,#34385,.F.);
#45078=ORIENTED_EDGE('',*,*,#34386,.F.);
#45079=ORIENTED_EDGE('',*,*,#34387,.F.);
#45080=ORIENTED_EDGE('',*,*,#34388,.F.);
#45081=ORIENTED_EDGE('',*,*,#34389,.F.);
#45082=ORIENTED_EDGE('',*,*,#34390,.F.);
#45083=ORIENTED_EDGE('',*,*,#34391,.F.);
#45084=ORIENTED_EDGE('',*,*,#34392,.F.);
#45085=ORIENTED_EDGE('',*,*,#34393,.F.);
#45086=ORIENTED_EDGE('',*,*,#34394,.F.);
#45087=ORIENTED_EDGE('',*,*,#34395,.F.);
#45088=ORIENTED_EDGE('',*,*,#34396,.F.);
#45089=ORIENTED_EDGE('',*,*,#34397,.F.);
#45090=ORIENTED_EDGE('',*,*,#34398,.F.);
#45091=ORIENTED_EDGE('',*,*,#34399,.F.);
#45092=ORIENTED_EDGE('',*,*,#34400,.F.);
#45093=ORIENTED_EDGE('',*,*,#34401,.F.);
#45094=ORIENTED_EDGE('',*,*,#34402,.F.);
#45095=ORIENTED_EDGE('',*,*,#34403,.F.);
#45096=ORIENTED_EDGE('',*,*,#34404,.F.);
#45097=ORIENTED_EDGE('',*,*,#34405,.F.);
#45098=ORIENTED_EDGE('',*,*,#34406,.F.);
#45099=ORIENTED_EDGE('',*,*,#34407,.F.);
#45100=ORIENTED_EDGE('',*,*,#34408,.F.);
#45101=ORIENTED_EDGE('',*,*,#34409,.F.);
#45102=ORIENTED_EDGE('',*,*,#34410,.F.);
#45103=ORIENTED_EDGE('',*,*,#34411,.F.);
#45104=ORIENTED_EDGE('',*,*,#34412,.F.);
#45105=ORIENTED_EDGE('',*,*,#34413,.F.);
#45106=ORIENTED_EDGE('',*,*,#34414,.F.);
#45107=ORIENTED_EDGE('',*,*,#34415,.F.);
#45108=ORIENTED_EDGE('',*,*,#34416,.F.);
#45109=ORIENTED_EDGE('',*,*,#34417,.F.);
#45110=ORIENTED_EDGE('',*,*,#34418,.F.);
#45111=ORIENTED_EDGE('',*,*,#34419,.F.);
#45112=ORIENTED_EDGE('',*,*,#34420,.F.);
#45113=ORIENTED_EDGE('',*,*,#34421,.F.);
#45114=ORIENTED_EDGE('',*,*,#34422,.F.);
#45115=ORIENTED_EDGE('',*,*,#34423,.F.);
#45116=ORIENTED_EDGE('',*,*,#34424,.F.);
#45117=ORIENTED_EDGE('',*,*,#34425,.F.);
#45118=ORIENTED_EDGE('',*,*,#34426,.F.);
#45119=ORIENTED_EDGE('',*,*,#34427,.F.);
#45120=ORIENTED_EDGE('',*,*,#34428,.F.);
#45121=ORIENTED_EDGE('',*,*,#34429,.F.);
#45122=ORIENTED_EDGE('',*,*,#34430,.F.);
#45123=ORIENTED_EDGE('',*,*,#34431,.F.);
#45124=ORIENTED_EDGE('',*,*,#34432,.F.);
#45125=ORIENTED_EDGE('',*,*,#34433,.F.);
#45126=ORIENTED_EDGE('',*,*,#34434,.F.);
#45127=ORIENTED_EDGE('',*,*,#34435,.F.);
#45128=ORIENTED_EDGE('',*,*,#34436,.F.);
#45129=ORIENTED_EDGE('',*,*,#34437,.F.);
#45130=ORIENTED_EDGE('',*,*,#34438,.F.);
#45131=ORIENTED_EDGE('',*,*,#34439,.F.);
#45132=ORIENTED_EDGE('',*,*,#34440,.F.);
#45133=ORIENTED_EDGE('',*,*,#34441,.F.);
#45134=ORIENTED_EDGE('',*,*,#34442,.F.);
#45135=ORIENTED_EDGE('',*,*,#34443,.F.);
#45136=ORIENTED_EDGE('',*,*,#34444,.F.);
#45137=ORIENTED_EDGE('',*,*,#34445,.F.);
#45138=ORIENTED_EDGE('',*,*,#34446,.F.);
#45139=ORIENTED_EDGE('',*,*,#34447,.F.);
#45140=ORIENTED_EDGE('',*,*,#34448,.F.);
#45141=ORIENTED_EDGE('',*,*,#34449,.F.);
#45142=ORIENTED_EDGE('',*,*,#34450,.F.);
#45143=ORIENTED_EDGE('',*,*,#34451,.F.);
#45144=ORIENTED_EDGE('',*,*,#34452,.F.);
#45145=ORIENTED_EDGE('',*,*,#34453,.F.);
#45146=ORIENTED_EDGE('',*,*,#34454,.F.);
#45147=ORIENTED_EDGE('',*,*,#34455,.F.);
#45148=ORIENTED_EDGE('',*,*,#34456,.F.);
#45149=ORIENTED_EDGE('',*,*,#34457,.F.);
#45150=ORIENTED_EDGE('',*,*,#34458,.F.);
#45151=ORIENTED_EDGE('',*,*,#34459,.F.);
#45152=ORIENTED_EDGE('',*,*,#34460,.F.);
#45153=ORIENTED_EDGE('',*,*,#34461,.F.);
#45154=ORIENTED_EDGE('',*,*,#34462,.F.);
#45155=ORIENTED_EDGE('',*,*,#34463,.F.);
#45156=ORIENTED_EDGE('',*,*,#34464,.F.);
#45157=ORIENTED_EDGE('',*,*,#34465,.F.);
#45158=ORIENTED_EDGE('',*,*,#34466,.F.);
#45159=ORIENTED_EDGE('',*,*,#34467,.F.);
#45160=ORIENTED_EDGE('',*,*,#34468,.F.);
#45161=ORIENTED_EDGE('',*,*,#34469,.T.);
#45162=ORIENTED_EDGE('',*,*,#34470,.F.);
#45163=ORIENTED_EDGE('',*,*,#34471,.F.);
#45164=ORIENTED_EDGE('',*,*,#34472,.F.);
#45165=ORIENTED_EDGE('',*,*,#34473,.T.);
#45166=ORIENTED_EDGE('',*,*,#34474,.F.);
#45167=ORIENTED_EDGE('',*,*,#34475,.F.);
#45168=ORIENTED_EDGE('',*,*,#34476,.F.);
#45169=ORIENTED_EDGE('',*,*,#34477,.F.);
#45170=ORIENTED_EDGE('',*,*,#34478,.F.);
#45171=ORIENTED_EDGE('',*,*,#34479,.F.);
#45172=ORIENTED_EDGE('',*,*,#34473,.F.);
#45173=ORIENTED_EDGE('',*,*,#34479,.T.);
#45174=ORIENTED_EDGE('',*,*,#34480,.F.);
#45175=ORIENTED_EDGE('',*,*,#34481,.F.);
#45176=ORIENTED_EDGE('',*,*,#34474,.T.);
#45177=ORIENTED_EDGE('',*,*,#34482,.T.);
#45178=ORIENTED_EDGE('',*,*,#34483,.F.);
#45179=ORIENTED_EDGE('',*,*,#34484,.F.);
#45180=ORIENTED_EDGE('',*,*,#34485,.F.);
#45181=ORIENTED_EDGE('',*,*,#34486,.F.);
#45182=ORIENTED_EDGE('',*,*,#34487,.F.);
#45183=ORIENTED_EDGE('',*,*,#34488,.F.);
#45184=ORIENTED_EDGE('',*,*,#34482,.F.);
#45185=ORIENTED_EDGE('',*,*,#34488,.T.);
#45186=ORIENTED_EDGE('',*,*,#34489,.F.);
#45187=ORIENTED_EDGE('',*,*,#34490,.F.);
#45188=ORIENTED_EDGE('',*,*,#34483,.T.);
#45189=ORIENTED_EDGE('',*,*,#34491,.T.);
#45190=ORIENTED_EDGE('',*,*,#34492,.F.);
#45191=ORIENTED_EDGE('',*,*,#34493,.F.);
#45192=ORIENTED_EDGE('',*,*,#34494,.F.);
#45193=ORIENTED_EDGE('',*,*,#34495,.F.);
#45194=ORIENTED_EDGE('',*,*,#34496,.F.);
#45195=ORIENTED_EDGE('',*,*,#34497,.F.);
#45196=ORIENTED_EDGE('',*,*,#34491,.F.);
#45197=ORIENTED_EDGE('',*,*,#34497,.T.);
#45198=ORIENTED_EDGE('',*,*,#34498,.F.);
#45199=ORIENTED_EDGE('',*,*,#34499,.F.);
#45200=ORIENTED_EDGE('',*,*,#34492,.T.);
#45201=ORIENTED_EDGE('',*,*,#34500,.T.);
#45202=ORIENTED_EDGE('',*,*,#34501,.F.);
#45203=ORIENTED_EDGE('',*,*,#34502,.F.);
#45204=ORIENTED_EDGE('',*,*,#34503,.F.);
#45205=ORIENTED_EDGE('',*,*,#34504,.F.);
#45206=ORIENTED_EDGE('',*,*,#34505,.F.);
#45207=ORIENTED_EDGE('',*,*,#34506,.F.);
#45208=ORIENTED_EDGE('',*,*,#34500,.F.);
#45209=ORIENTED_EDGE('',*,*,#34506,.T.);
#45210=ORIENTED_EDGE('',*,*,#34507,.F.);
#45211=ORIENTED_EDGE('',*,*,#34508,.F.);
#45212=ORIENTED_EDGE('',*,*,#34501,.T.);
#45213=ORIENTED_EDGE('',*,*,#34509,.T.);
#45214=ORIENTED_EDGE('',*,*,#34510,.F.);
#45215=ORIENTED_EDGE('',*,*,#34511,.F.);
#45216=ORIENTED_EDGE('',*,*,#34512,.F.);
#45217=ORIENTED_EDGE('',*,*,#34513,.F.);
#45218=ORIENTED_EDGE('',*,*,#34514,.F.);
#45219=ORIENTED_EDGE('',*,*,#34515,.F.);
#45220=ORIENTED_EDGE('',*,*,#34509,.F.);
#45221=ORIENTED_EDGE('',*,*,#34515,.T.);
#45222=ORIENTED_EDGE('',*,*,#34516,.F.);
#45223=ORIENTED_EDGE('',*,*,#34517,.F.);
#45224=ORIENTED_EDGE('',*,*,#34510,.T.);
#45225=ORIENTED_EDGE('',*,*,#34518,.T.);
#45226=ORIENTED_EDGE('',*,*,#34519,.F.);
#45227=ORIENTED_EDGE('',*,*,#34520,.F.);
#45228=ORIENTED_EDGE('',*,*,#34521,.F.);
#45229=ORIENTED_EDGE('',*,*,#34522,.F.);
#45230=ORIENTED_EDGE('',*,*,#34523,.F.);
#45231=ORIENTED_EDGE('',*,*,#34524,.F.);
#45232=ORIENTED_EDGE('',*,*,#34518,.F.);
#45233=ORIENTED_EDGE('',*,*,#34524,.T.);
#45234=ORIENTED_EDGE('',*,*,#34525,.F.);
#45235=ORIENTED_EDGE('',*,*,#34526,.F.);
#45236=ORIENTED_EDGE('',*,*,#34519,.T.);
#45237=ORIENTED_EDGE('',*,*,#34466,.T.);
#45238=ORIENTED_EDGE('',*,*,#34527,.F.);
#45239=ORIENTED_EDGE('',*,*,#34528,.F.);
#45240=ORIENTED_EDGE('',*,*,#34529,.F.);
#45241=ORIENTED_EDGE('',*,*,#34465,.T.);
#45242=ORIENTED_EDGE('',*,*,#34530,.F.);
#45243=ORIENTED_EDGE('',*,*,#34531,.F.);
#45244=ORIENTED_EDGE('',*,*,#34527,.T.);
#45245=ORIENTED_EDGE('',*,*,#34532,.T.);
#45246=ORIENTED_EDGE('',*,*,#34533,.F.);
#45247=ORIENTED_EDGE('',*,*,#34534,.F.);
#45248=ORIENTED_EDGE('',*,*,#34535,.F.);
#45249=ORIENTED_EDGE('',*,*,#34536,.F.);
#45250=ORIENTED_EDGE('',*,*,#34537,.F.);
#45251=ORIENTED_EDGE('',*,*,#34538,.F.);
#45252=ORIENTED_EDGE('',*,*,#34532,.F.);
#45253=ORIENTED_EDGE('',*,*,#34538,.T.);
#45254=ORIENTED_EDGE('',*,*,#34539,.F.);
#45255=ORIENTED_EDGE('',*,*,#34540,.F.);
#45256=ORIENTED_EDGE('',*,*,#34533,.T.);
#45257=ORIENTED_EDGE('',*,*,#34541,.T.);
#45258=ORIENTED_EDGE('',*,*,#34542,.F.);
#45259=ORIENTED_EDGE('',*,*,#34543,.F.);
#45260=ORIENTED_EDGE('',*,*,#34544,.F.);
#45261=ORIENTED_EDGE('',*,*,#34545,.F.);
#45262=ORIENTED_EDGE('',*,*,#34546,.F.);
#45263=ORIENTED_EDGE('',*,*,#34547,.F.);
#45264=ORIENTED_EDGE('',*,*,#34541,.F.);
#45265=ORIENTED_EDGE('',*,*,#34547,.T.);
#45266=ORIENTED_EDGE('',*,*,#34548,.F.);
#45267=ORIENTED_EDGE('',*,*,#34549,.F.);
#45268=ORIENTED_EDGE('',*,*,#34542,.T.);
#45269=ORIENTED_EDGE('',*,*,#34550,.T.);
#45270=ORIENTED_EDGE('',*,*,#34551,.F.);
#45271=ORIENTED_EDGE('',*,*,#34552,.F.);
#45272=ORIENTED_EDGE('',*,*,#34553,.F.);
#45273=ORIENTED_EDGE('',*,*,#34554,.F.);
#45274=ORIENTED_EDGE('',*,*,#34555,.F.);
#45275=ORIENTED_EDGE('',*,*,#34556,.F.);
#45276=ORIENTED_EDGE('',*,*,#34550,.F.);
#45277=ORIENTED_EDGE('',*,*,#34556,.T.);
#45278=ORIENTED_EDGE('',*,*,#34557,.F.);
#45279=ORIENTED_EDGE('',*,*,#34558,.F.);
#45280=ORIENTED_EDGE('',*,*,#34551,.T.);
#45281=ORIENTED_EDGE('',*,*,#34559,.T.);
#45282=ORIENTED_EDGE('',*,*,#34560,.F.);
#45283=ORIENTED_EDGE('',*,*,#34561,.F.);
#45284=ORIENTED_EDGE('',*,*,#34562,.F.);
#45285=ORIENTED_EDGE('',*,*,#34563,.F.);
#45286=ORIENTED_EDGE('',*,*,#34564,.F.);
#45287=ORIENTED_EDGE('',*,*,#34565,.F.);
#45288=ORIENTED_EDGE('',*,*,#34559,.F.);
#45289=ORIENTED_EDGE('',*,*,#34565,.T.);
#45290=ORIENTED_EDGE('',*,*,#34566,.F.);
#45291=ORIENTED_EDGE('',*,*,#34567,.F.);
#45292=ORIENTED_EDGE('',*,*,#34560,.T.);
#45293=ORIENTED_EDGE('',*,*,#34568,.T.);
#45294=ORIENTED_EDGE('',*,*,#34569,.F.);
#45295=ORIENTED_EDGE('',*,*,#34570,.F.);
#45296=ORIENTED_EDGE('',*,*,#34571,.F.);
#45297=ORIENTED_EDGE('',*,*,#34572,.F.);
#45298=ORIENTED_EDGE('',*,*,#34573,.F.);
#45299=ORIENTED_EDGE('',*,*,#34574,.F.);
#45300=ORIENTED_EDGE('',*,*,#34568,.F.);
#45301=ORIENTED_EDGE('',*,*,#34574,.T.);
#45302=ORIENTED_EDGE('',*,*,#34575,.F.);
#45303=ORIENTED_EDGE('',*,*,#34576,.F.);
#45304=ORIENTED_EDGE('',*,*,#34569,.T.);
#45305=ORIENTED_EDGE('',*,*,#34577,.T.);
#45306=ORIENTED_EDGE('',*,*,#34578,.F.);
#45307=ORIENTED_EDGE('',*,*,#34579,.F.);
#45308=ORIENTED_EDGE('',*,*,#34580,.F.);
#45309=ORIENTED_EDGE('',*,*,#34581,.F.);
#45310=ORIENTED_EDGE('',*,*,#34582,.F.);
#45311=ORIENTED_EDGE('',*,*,#34583,.F.);
#45312=ORIENTED_EDGE('',*,*,#34577,.F.);
#45313=ORIENTED_EDGE('',*,*,#34583,.T.);
#45314=ORIENTED_EDGE('',*,*,#34584,.F.);
#45315=ORIENTED_EDGE('',*,*,#34585,.F.);
#45316=ORIENTED_EDGE('',*,*,#34578,.T.);
#45317=ORIENTED_EDGE('',*,*,#34586,.T.);
#45318=ORIENTED_EDGE('',*,*,#34587,.F.);
#45319=ORIENTED_EDGE('',*,*,#34588,.F.);
#45320=ORIENTED_EDGE('',*,*,#34589,.F.);
#45321=ORIENTED_EDGE('',*,*,#34590,.F.);
#45322=ORIENTED_EDGE('',*,*,#34591,.F.);
#45323=ORIENTED_EDGE('',*,*,#34592,.F.);
#45324=ORIENTED_EDGE('',*,*,#34586,.F.);
#45325=ORIENTED_EDGE('',*,*,#34592,.T.);
#45326=ORIENTED_EDGE('',*,*,#34593,.F.);
#45327=ORIENTED_EDGE('',*,*,#34594,.F.);
#45328=ORIENTED_EDGE('',*,*,#34587,.T.);
#45329=ORIENTED_EDGE('',*,*,#34595,.T.);
#45330=ORIENTED_EDGE('',*,*,#34596,.F.);
#45331=ORIENTED_EDGE('',*,*,#34597,.F.);
#45332=ORIENTED_EDGE('',*,*,#34598,.F.);
#45333=ORIENTED_EDGE('',*,*,#34599,.F.);
#45334=ORIENTED_EDGE('',*,*,#34600,.F.);
#45335=ORIENTED_EDGE('',*,*,#34601,.F.);
#45336=ORIENTED_EDGE('',*,*,#34595,.F.);
#45337=ORIENTED_EDGE('',*,*,#34601,.T.);
#45338=ORIENTED_EDGE('',*,*,#34602,.F.);
#45339=ORIENTED_EDGE('',*,*,#34603,.F.);
#45340=ORIENTED_EDGE('',*,*,#34596,.T.);
#45341=ORIENTED_EDGE('',*,*,#34604,.T.);
#45342=ORIENTED_EDGE('',*,*,#34605,.F.);
#45343=ORIENTED_EDGE('',*,*,#34606,.F.);
#45344=ORIENTED_EDGE('',*,*,#34607,.F.);
#45345=ORIENTED_EDGE('',*,*,#34608,.F.);
#45346=ORIENTED_EDGE('',*,*,#34609,.F.);
#45347=ORIENTED_EDGE('',*,*,#34610,.F.);
#45348=ORIENTED_EDGE('',*,*,#34604,.F.);
#45349=ORIENTED_EDGE('',*,*,#34610,.T.);
#45350=ORIENTED_EDGE('',*,*,#34611,.F.);
#45351=ORIENTED_EDGE('',*,*,#34612,.F.);
#45352=ORIENTED_EDGE('',*,*,#34605,.T.);
#45353=ORIENTED_EDGE('',*,*,#34613,.T.);
#45354=ORIENTED_EDGE('',*,*,#34614,.F.);
#45355=ORIENTED_EDGE('',*,*,#34615,.F.);
#45356=ORIENTED_EDGE('',*,*,#34616,.F.);
#45357=ORIENTED_EDGE('',*,*,#34617,.F.);
#45358=ORIENTED_EDGE('',*,*,#34618,.F.);
#45359=ORIENTED_EDGE('',*,*,#34619,.F.);
#45360=ORIENTED_EDGE('',*,*,#34613,.F.);
#45361=ORIENTED_EDGE('',*,*,#34619,.T.);
#45362=ORIENTED_EDGE('',*,*,#34620,.F.);
#45363=ORIENTED_EDGE('',*,*,#34621,.F.);
#45364=ORIENTED_EDGE('',*,*,#34614,.T.);
#45365=ORIENTED_EDGE('',*,*,#34622,.T.);
#45366=ORIENTED_EDGE('',*,*,#34623,.F.);
#45367=ORIENTED_EDGE('',*,*,#34624,.F.);
#45368=ORIENTED_EDGE('',*,*,#34625,.F.);
#45369=ORIENTED_EDGE('',*,*,#34626,.F.);
#45370=ORIENTED_EDGE('',*,*,#34627,.F.);
#45371=ORIENTED_EDGE('',*,*,#34628,.F.);
#45372=ORIENTED_EDGE('',*,*,#34622,.F.);
#45373=ORIENTED_EDGE('',*,*,#34628,.T.);
#45374=ORIENTED_EDGE('',*,*,#34629,.F.);
#45375=ORIENTED_EDGE('',*,*,#34630,.F.);
#45376=ORIENTED_EDGE('',*,*,#34623,.T.);
#45377=ORIENTED_EDGE('',*,*,#34631,.T.);
#45378=ORIENTED_EDGE('',*,*,#34632,.F.);
#45379=ORIENTED_EDGE('',*,*,#34633,.F.);
#45380=ORIENTED_EDGE('',*,*,#34634,.F.);
#45381=ORIENTED_EDGE('',*,*,#34635,.F.);
#45382=ORIENTED_EDGE('',*,*,#34636,.F.);
#45383=ORIENTED_EDGE('',*,*,#34637,.F.);
#45384=ORIENTED_EDGE('',*,*,#34631,.F.);
#45385=ORIENTED_EDGE('',*,*,#34637,.T.);
#45386=ORIENTED_EDGE('',*,*,#34638,.F.);
#45387=ORIENTED_EDGE('',*,*,#34639,.F.);
#45388=ORIENTED_EDGE('',*,*,#34632,.T.);
#45389=ORIENTED_EDGE('',*,*,#34640,.T.);
#45390=ORIENTED_EDGE('',*,*,#34641,.F.);
#45391=ORIENTED_EDGE('',*,*,#34642,.F.);
#45392=ORIENTED_EDGE('',*,*,#34643,.F.);
#45393=ORIENTED_EDGE('',*,*,#34644,.F.);
#45394=ORIENTED_EDGE('',*,*,#34645,.F.);
#45395=ORIENTED_EDGE('',*,*,#34646,.F.);
#45396=ORIENTED_EDGE('',*,*,#34640,.F.);
#45397=ORIENTED_EDGE('',*,*,#34646,.T.);
#45398=ORIENTED_EDGE('',*,*,#34647,.F.);
#45399=ORIENTED_EDGE('',*,*,#34648,.F.);
#45400=ORIENTED_EDGE('',*,*,#34641,.T.);
#45401=ORIENTED_EDGE('',*,*,#34649,.T.);
#45402=ORIENTED_EDGE('',*,*,#34650,.F.);
#45403=ORIENTED_EDGE('',*,*,#34651,.F.);
#45404=ORIENTED_EDGE('',*,*,#34652,.F.);
#45405=ORIENTED_EDGE('',*,*,#34653,.F.);
#45406=ORIENTED_EDGE('',*,*,#34654,.F.);
#45407=ORIENTED_EDGE('',*,*,#34655,.F.);
#45408=ORIENTED_EDGE('',*,*,#34649,.F.);
#45409=ORIENTED_EDGE('',*,*,#34655,.T.);
#45410=ORIENTED_EDGE('',*,*,#34656,.F.);
#45411=ORIENTED_EDGE('',*,*,#34657,.F.);
#45412=ORIENTED_EDGE('',*,*,#34650,.T.);
#45413=ORIENTED_EDGE('',*,*,#34658,.T.);
#45414=ORIENTED_EDGE('',*,*,#34659,.F.);
#45415=ORIENTED_EDGE('',*,*,#34660,.F.);
#45416=ORIENTED_EDGE('',*,*,#34661,.F.);
#45417=ORIENTED_EDGE('',*,*,#34662,.F.);
#45418=ORIENTED_EDGE('',*,*,#34663,.F.);
#45419=ORIENTED_EDGE('',*,*,#34664,.F.);
#45420=ORIENTED_EDGE('',*,*,#34658,.F.);
#45421=ORIENTED_EDGE('',*,*,#34664,.T.);
#45422=ORIENTED_EDGE('',*,*,#34665,.F.);
#45423=ORIENTED_EDGE('',*,*,#34666,.F.);
#45424=ORIENTED_EDGE('',*,*,#34659,.T.);
#45425=ORIENTED_EDGE('',*,*,#34667,.T.);
#45426=ORIENTED_EDGE('',*,*,#34668,.F.);
#45427=ORIENTED_EDGE('',*,*,#34669,.F.);
#45428=ORIENTED_EDGE('',*,*,#34670,.F.);
#45429=ORIENTED_EDGE('',*,*,#34671,.F.);
#45430=ORIENTED_EDGE('',*,*,#34672,.F.);
#45431=ORIENTED_EDGE('',*,*,#34673,.F.);
#45432=ORIENTED_EDGE('',*,*,#34667,.F.);
#45433=ORIENTED_EDGE('',*,*,#34673,.T.);
#45434=ORIENTED_EDGE('',*,*,#34674,.F.);
#45435=ORIENTED_EDGE('',*,*,#34675,.F.);
#45436=ORIENTED_EDGE('',*,*,#34668,.T.);
#45437=ORIENTED_EDGE('',*,*,#34676,.T.);
#45438=ORIENTED_EDGE('',*,*,#34677,.F.);
#45439=ORIENTED_EDGE('',*,*,#34678,.F.);
#45440=ORIENTED_EDGE('',*,*,#34679,.F.);
#45441=ORIENTED_EDGE('',*,*,#34680,.F.);
#45442=ORIENTED_EDGE('',*,*,#34681,.F.);
#45443=ORIENTED_EDGE('',*,*,#34682,.F.);
#45444=ORIENTED_EDGE('',*,*,#34676,.F.);
#45445=ORIENTED_EDGE('',*,*,#34682,.T.);
#45446=ORIENTED_EDGE('',*,*,#34683,.F.);
#45447=ORIENTED_EDGE('',*,*,#34684,.F.);
#45448=ORIENTED_EDGE('',*,*,#34677,.T.);
#45449=ORIENTED_EDGE('',*,*,#34685,.T.);
#45450=ORIENTED_EDGE('',*,*,#34686,.F.);
#45451=ORIENTED_EDGE('',*,*,#34687,.F.);
#45452=ORIENTED_EDGE('',*,*,#34688,.F.);
#45453=ORIENTED_EDGE('',*,*,#34689,.T.);
#45454=ORIENTED_EDGE('',*,*,#34690,.F.);
#45455=ORIENTED_EDGE('',*,*,#34691,.F.);
#45456=ORIENTED_EDGE('',*,*,#34686,.T.);
#45457=ORIENTED_EDGE('',*,*,#34692,.F.);
#45458=ORIENTED_EDGE('',*,*,#34693,.F.);
#45459=ORIENTED_EDGE('',*,*,#34689,.F.);
#45460=ORIENTED_EDGE('',*,*,#34685,.F.);
#45461=ORIENTED_EDGE('',*,*,#34694,.T.);
#45462=ORIENTED_EDGE('',*,*,#34695,.F.);
#45463=ORIENTED_EDGE('',*,*,#34696,.F.);
#45464=ORIENTED_EDGE('',*,*,#34697,.F.);
#45465=ORIENTED_EDGE('',*,*,#34698,.F.);
#45466=ORIENTED_EDGE('',*,*,#34694,.F.);
#45467=ORIENTED_EDGE('',*,*,#34699,.F.);
#45468=ORIENTED_EDGE('',*,*,#34700,.F.);
#45469=ORIENTED_EDGE('',*,*,#34701,.F.);
#45470=ORIENTED_EDGE('',*,*,#34695,.T.);
#45471=ORIENTED_EDGE('',*,*,#34698,.T.);
#45472=ORIENTED_EDGE('',*,*,#34702,.F.);
#45473=ORIENTED_EDGE('',*,*,#34703,.T.);
#45474=ORIENTED_EDGE('',*,*,#34704,.F.);
#45475=ORIENTED_EDGE('',*,*,#34705,.F.);
#45476=ORIENTED_EDGE('',*,*,#34706,.F.);
#45477=ORIENTED_EDGE('',*,*,#34707,.F.);
#45478=ORIENTED_EDGE('',*,*,#34708,.F.);
#45479=ORIENTED_EDGE('',*,*,#34709,.F.);
#45480=ORIENTED_EDGE('',*,*,#34703,.F.);
#45481=ORIENTED_EDGE('',*,*,#34709,.T.);
#45482=ORIENTED_EDGE('',*,*,#34710,.F.);
#45483=ORIENTED_EDGE('',*,*,#34711,.F.);
#45484=ORIENTED_EDGE('',*,*,#34704,.T.);
#45485=ORIENTED_EDGE('',*,*,#34712,.T.);
#45486=ORIENTED_EDGE('',*,*,#34713,.F.);
#45487=ORIENTED_EDGE('',*,*,#34714,.F.);
#45488=ORIENTED_EDGE('',*,*,#34715,.F.);
#45489=ORIENTED_EDGE('',*,*,#34716,.F.);
#45490=ORIENTED_EDGE('',*,*,#34717,.F.);
#45491=ORIENTED_EDGE('',*,*,#34718,.F.);
#45492=ORIENTED_EDGE('',*,*,#34712,.F.);
#45493=ORIENTED_EDGE('',*,*,#34718,.T.);
#45494=ORIENTED_EDGE('',*,*,#34719,.F.);
#45495=ORIENTED_EDGE('',*,*,#34720,.F.);
#45496=ORIENTED_EDGE('',*,*,#34713,.T.);
#45497=ORIENTED_EDGE('',*,*,#34721,.F.);
#45498=ORIENTED_EDGE('',*,*,#34722,.F.);
#45499=ORIENTED_EDGE('',*,*,#34469,.F.);
#45500=ORIENTED_EDGE('',*,*,#34723,.F.);
#45501=ORIENTED_EDGE('',*,*,#34723,.T.);
#45502=ORIENTED_EDGE('',*,*,#34472,.T.);
#45503=ORIENTED_EDGE('',*,*,#34724,.F.);
#45504=ORIENTED_EDGE('',*,*,#34725,.F.);
#45505=ORIENTED_EDGE('',*,*,#34720,.T.);
#45506=ORIENTED_EDGE('',*,*,#34726,.F.);
#45507=ORIENTED_EDGE('',*,*,#34727,.T.);
#45508=ORIENTED_EDGE('',*,*,#34728,.F.);
#45509=ORIENTED_EDGE('',*,*,#34714,.T.);
#45510=ORIENTED_EDGE('',*,*,#34729,.F.);
#45511=ORIENTED_EDGE('',*,*,#34730,.T.);
#45512=ORIENTED_EDGE('',*,*,#34731,.F.);
#45513=ORIENTED_EDGE('',*,*,#34711,.T.);
#45514=ORIENTED_EDGE('',*,*,#34731,.T.);
#45515=ORIENTED_EDGE('',*,*,#34732,.T.);
#45516=ORIENTED_EDGE('',*,*,#34733,.F.);
#45517=ORIENTED_EDGE('',*,*,#34732,.F.);
#45518=ORIENTED_EDGE('',*,*,#34730,.F.);
#45519=ORIENTED_EDGE('',*,*,#34734,.F.);
#45520=ORIENTED_EDGE('',*,*,#34735,.F.);
#45521=ORIENTED_EDGE('',*,*,#34705,.T.);
#45522=ORIENTED_EDGE('',*,*,#34736,.F.);
#45523=ORIENTED_EDGE('',*,*,#34737,.T.);
#45524=ORIENTED_EDGE('',*,*,#34738,.F.);
#45525=ORIENTED_EDGE('',*,*,#34739,.T.);
#45526=ORIENTED_EDGE('',*,*,#34740,.F.);
#45527=ORIENTED_EDGE('',*,*,#34701,.T.);
#45528=ORIENTED_EDGE('',*,*,#34738,.T.);
#45529=ORIENTED_EDGE('',*,*,#34741,.F.);
#45530=ORIENTED_EDGE('',*,*,#34742,.F.);
#45531=ORIENTED_EDGE('',*,*,#34739,.F.);
#45532=ORIENTED_EDGE('',*,*,#34737,.F.);
#45533=ORIENTED_EDGE('',*,*,#34696,.T.);
#45534=ORIENTED_EDGE('',*,*,#34743,.F.);
#45535=ORIENTED_EDGE('',*,*,#34744,.T.);
#45536=ORIENTED_EDGE('',*,*,#34745,.F.);
#45537=ORIENTED_EDGE('',*,*,#34691,.T.);
#45538=ORIENTED_EDGE('',*,*,#34745,.T.);
#45539=ORIENTED_EDGE('',*,*,#34746,.T.);
#45540=ORIENTED_EDGE('',*,*,#34747,.F.);
#45541=ORIENTED_EDGE('',*,*,#34746,.F.);
#45542=ORIENTED_EDGE('',*,*,#34744,.F.);
#45543=ORIENTED_EDGE('',*,*,#34748,.F.);
#45544=ORIENTED_EDGE('',*,*,#34749,.F.);
#45545=ORIENTED_EDGE('',*,*,#34687,.T.);
#45546=ORIENTED_EDGE('',*,*,#34750,.F.);
#45547=ORIENTED_EDGE('',*,*,#34751,.T.);
#45548=ORIENTED_EDGE('',*,*,#34752,.F.);
#45549=ORIENTED_EDGE('',*,*,#34684,.T.);
#45550=ORIENTED_EDGE('',*,*,#34752,.T.);
#45551=ORIENTED_EDGE('',*,*,#34753,.T.);
#45552=ORIENTED_EDGE('',*,*,#34754,.F.);
#45553=ORIENTED_EDGE('',*,*,#34753,.F.);
#45554=ORIENTED_EDGE('',*,*,#34751,.F.);
#45555=ORIENTED_EDGE('',*,*,#34755,.F.);
#45556=ORIENTED_EDGE('',*,*,#34756,.F.);
#45557=ORIENTED_EDGE('',*,*,#34678,.T.);
#45558=ORIENTED_EDGE('',*,*,#34757,.F.);
#45559=ORIENTED_EDGE('',*,*,#34758,.T.);
#45560=ORIENTED_EDGE('',*,*,#34759,.F.);
#45561=ORIENTED_EDGE('',*,*,#34675,.T.);
#45562=ORIENTED_EDGE('',*,*,#34759,.T.);
#45563=ORIENTED_EDGE('',*,*,#34760,.T.);
#45564=ORIENTED_EDGE('',*,*,#34761,.F.);
#45565=ORIENTED_EDGE('',*,*,#34760,.F.);
#45566=ORIENTED_EDGE('',*,*,#34758,.F.);
#45567=ORIENTED_EDGE('',*,*,#34762,.F.);
#45568=ORIENTED_EDGE('',*,*,#34763,.F.);
#45569=ORIENTED_EDGE('',*,*,#34669,.T.);
#45570=ORIENTED_EDGE('',*,*,#34764,.F.);
#45571=ORIENTED_EDGE('',*,*,#34765,.T.);
#45572=ORIENTED_EDGE('',*,*,#34766,.F.);
#45573=ORIENTED_EDGE('',*,*,#34666,.T.);
#45574=ORIENTED_EDGE('',*,*,#34766,.T.);
#45575=ORIENTED_EDGE('',*,*,#34767,.T.);
#45576=ORIENTED_EDGE('',*,*,#34768,.F.);
#45577=ORIENTED_EDGE('',*,*,#34767,.F.);
#45578=ORIENTED_EDGE('',*,*,#34765,.F.);
#45579=ORIENTED_EDGE('',*,*,#34769,.F.);
#45580=ORIENTED_EDGE('',*,*,#34770,.F.);
#45581=ORIENTED_EDGE('',*,*,#34660,.T.);
#45582=ORIENTED_EDGE('',*,*,#34771,.F.);
#45583=ORIENTED_EDGE('',*,*,#34772,.T.);
#45584=ORIENTED_EDGE('',*,*,#34773,.F.);
#45585=ORIENTED_EDGE('',*,*,#34657,.T.);
#45586=ORIENTED_EDGE('',*,*,#34773,.T.);
#45587=ORIENTED_EDGE('',*,*,#34774,.T.);
#45588=ORIENTED_EDGE('',*,*,#34775,.F.);
#45589=ORIENTED_EDGE('',*,*,#34774,.F.);
#45590=ORIENTED_EDGE('',*,*,#34772,.F.);
#45591=ORIENTED_EDGE('',*,*,#34776,.F.);
#45592=ORIENTED_EDGE('',*,*,#34777,.F.);
#45593=ORIENTED_EDGE('',*,*,#34651,.T.);
#45594=ORIENTED_EDGE('',*,*,#34778,.F.);
#45595=ORIENTED_EDGE('',*,*,#34779,.T.);
#45596=ORIENTED_EDGE('',*,*,#34780,.F.);
#45597=ORIENTED_EDGE('',*,*,#34648,.T.);
#45598=ORIENTED_EDGE('',*,*,#34780,.T.);
#45599=ORIENTED_EDGE('',*,*,#34781,.T.);
#45600=ORIENTED_EDGE('',*,*,#34782,.F.);
#45601=ORIENTED_EDGE('',*,*,#34781,.F.);
#45602=ORIENTED_EDGE('',*,*,#34779,.F.);
#45603=ORIENTED_EDGE('',*,*,#34783,.F.);
#45604=ORIENTED_EDGE('',*,*,#34784,.F.);
#45605=ORIENTED_EDGE('',*,*,#34642,.T.);
#45606=ORIENTED_EDGE('',*,*,#34785,.F.);
#45607=ORIENTED_EDGE('',*,*,#34786,.T.);
#45608=ORIENTED_EDGE('',*,*,#34787,.F.);
#45609=ORIENTED_EDGE('',*,*,#34639,.T.);
#45610=ORIENTED_EDGE('',*,*,#34787,.T.);
#45611=ORIENTED_EDGE('',*,*,#34788,.T.);
#45612=ORIENTED_EDGE('',*,*,#34789,.F.);
#45613=ORIENTED_EDGE('',*,*,#34788,.F.);
#45614=ORIENTED_EDGE('',*,*,#34786,.F.);
#45615=ORIENTED_EDGE('',*,*,#34790,.F.);
#45616=ORIENTED_EDGE('',*,*,#34791,.F.);
#45617=ORIENTED_EDGE('',*,*,#34633,.T.);
#45618=ORIENTED_EDGE('',*,*,#34792,.F.);
#45619=ORIENTED_EDGE('',*,*,#34793,.T.);
#45620=ORIENTED_EDGE('',*,*,#34794,.F.);
#45621=ORIENTED_EDGE('',*,*,#34630,.T.);
#45622=ORIENTED_EDGE('',*,*,#34794,.T.);
#45623=ORIENTED_EDGE('',*,*,#34795,.T.);
#45624=ORIENTED_EDGE('',*,*,#34796,.F.);
#45625=ORIENTED_EDGE('',*,*,#34795,.F.);
#45626=ORIENTED_EDGE('',*,*,#34793,.F.);
#45627=ORIENTED_EDGE('',*,*,#34797,.F.);
#45628=ORIENTED_EDGE('',*,*,#34798,.F.);
#45629=ORIENTED_EDGE('',*,*,#34624,.T.);
#45630=ORIENTED_EDGE('',*,*,#34799,.F.);
#45631=ORIENTED_EDGE('',*,*,#34800,.T.);
#45632=ORIENTED_EDGE('',*,*,#34801,.F.);
#45633=ORIENTED_EDGE('',*,*,#34621,.T.);
#45634=ORIENTED_EDGE('',*,*,#34801,.T.);
#45635=ORIENTED_EDGE('',*,*,#34802,.T.);
#45636=ORIENTED_EDGE('',*,*,#34803,.F.);
#45637=ORIENTED_EDGE('',*,*,#34802,.F.);
#45638=ORIENTED_EDGE('',*,*,#34800,.F.);
#45639=ORIENTED_EDGE('',*,*,#34804,.F.);
#45640=ORIENTED_EDGE('',*,*,#34805,.F.);
#45641=ORIENTED_EDGE('',*,*,#34615,.T.);
#45642=ORIENTED_EDGE('',*,*,#34806,.F.);
#45643=ORIENTED_EDGE('',*,*,#34807,.T.);
#45644=ORIENTED_EDGE('',*,*,#34808,.F.);
#45645=ORIENTED_EDGE('',*,*,#34612,.T.);
#45646=ORIENTED_EDGE('',*,*,#34808,.T.);
#45647=ORIENTED_EDGE('',*,*,#34809,.T.);
#45648=ORIENTED_EDGE('',*,*,#34810,.F.);
#45649=ORIENTED_EDGE('',*,*,#34809,.F.);
#45650=ORIENTED_EDGE('',*,*,#34807,.F.);
#45651=ORIENTED_EDGE('',*,*,#34811,.F.);
#45652=ORIENTED_EDGE('',*,*,#34812,.F.);
#45653=ORIENTED_EDGE('',*,*,#34606,.T.);
#45654=ORIENTED_EDGE('',*,*,#34813,.F.);
#45655=ORIENTED_EDGE('',*,*,#34814,.T.);
#45656=ORIENTED_EDGE('',*,*,#34815,.F.);
#45657=ORIENTED_EDGE('',*,*,#34603,.T.);
#45658=ORIENTED_EDGE('',*,*,#34815,.T.);
#45659=ORIENTED_EDGE('',*,*,#34816,.T.);
#45660=ORIENTED_EDGE('',*,*,#34817,.F.);
#45661=ORIENTED_EDGE('',*,*,#34816,.F.);
#45662=ORIENTED_EDGE('',*,*,#34814,.F.);
#45663=ORIENTED_EDGE('',*,*,#34818,.F.);
#45664=ORIENTED_EDGE('',*,*,#34819,.F.);
#45665=ORIENTED_EDGE('',*,*,#34597,.T.);
#45666=ORIENTED_EDGE('',*,*,#34820,.F.);
#45667=ORIENTED_EDGE('',*,*,#34463,.T.);
#45668=ORIENTED_EDGE('',*,*,#34821,.F.);
#45669=ORIENTED_EDGE('',*,*,#34594,.T.);
#45670=ORIENTED_EDGE('',*,*,#34821,.T.);
#45671=ORIENTED_EDGE('',*,*,#34462,.T.);
#45672=ORIENTED_EDGE('',*,*,#34822,.F.);
#45673=ORIENTED_EDGE('',*,*,#34588,.T.);
#45674=ORIENTED_EDGE('',*,*,#34823,.F.);
#45675=ORIENTED_EDGE('',*,*,#34824,.T.);
#45676=ORIENTED_EDGE('',*,*,#34825,.F.);
#45677=ORIENTED_EDGE('',*,*,#34585,.T.);
#45678=ORIENTED_EDGE('',*,*,#34825,.T.);
#45679=ORIENTED_EDGE('',*,*,#34826,.T.);
#45680=ORIENTED_EDGE('',*,*,#34827,.F.);
#45681=ORIENTED_EDGE('',*,*,#34826,.F.);
#45682=ORIENTED_EDGE('',*,*,#34824,.F.);
#45683=ORIENTED_EDGE('',*,*,#34828,.F.);
#45684=ORIENTED_EDGE('',*,*,#34829,.F.);
#45685=ORIENTED_EDGE('',*,*,#34579,.T.);
#45686=ORIENTED_EDGE('',*,*,#34830,.F.);
#45687=ORIENTED_EDGE('',*,*,#34831,.T.);
#45688=ORIENTED_EDGE('',*,*,#34832,.F.);
#45689=ORIENTED_EDGE('',*,*,#34576,.T.);
#45690=ORIENTED_EDGE('',*,*,#34832,.T.);
#45691=ORIENTED_EDGE('',*,*,#34833,.T.);
#45692=ORIENTED_EDGE('',*,*,#34834,.F.);
#45693=ORIENTED_EDGE('',*,*,#34833,.F.);
#45694=ORIENTED_EDGE('',*,*,#34831,.F.);
#45695=ORIENTED_EDGE('',*,*,#34835,.F.);
#45696=ORIENTED_EDGE('',*,*,#34836,.F.);
#45697=ORIENTED_EDGE('',*,*,#34570,.T.);
#45698=ORIENTED_EDGE('',*,*,#34837,.F.);
#45699=ORIENTED_EDGE('',*,*,#34838,.T.);
#45700=ORIENTED_EDGE('',*,*,#34839,.F.);
#45701=ORIENTED_EDGE('',*,*,#34567,.T.);
#45702=ORIENTED_EDGE('',*,*,#34839,.T.);
#45703=ORIENTED_EDGE('',*,*,#34840,.T.);
#45704=ORIENTED_EDGE('',*,*,#34841,.F.);
#45705=ORIENTED_EDGE('',*,*,#34840,.F.);
#45706=ORIENTED_EDGE('',*,*,#34838,.F.);
#45707=ORIENTED_EDGE('',*,*,#34842,.F.);
#45708=ORIENTED_EDGE('',*,*,#34843,.F.);
#45709=ORIENTED_EDGE('',*,*,#34561,.T.);
#45710=ORIENTED_EDGE('',*,*,#34844,.F.);
#45711=ORIENTED_EDGE('',*,*,#34845,.T.);
#45712=ORIENTED_EDGE('',*,*,#34846,.F.);
#45713=ORIENTED_EDGE('',*,*,#34558,.T.);
#45714=ORIENTED_EDGE('',*,*,#34846,.T.);
#45715=ORIENTED_EDGE('',*,*,#34847,.T.);
#45716=ORIENTED_EDGE('',*,*,#34848,.F.);
#45717=ORIENTED_EDGE('',*,*,#34847,.F.);
#45718=ORIENTED_EDGE('',*,*,#34845,.F.);
#45719=ORIENTED_EDGE('',*,*,#34849,.F.);
#45720=ORIENTED_EDGE('',*,*,#34850,.F.);
#45721=ORIENTED_EDGE('',*,*,#34552,.T.);
#45722=ORIENTED_EDGE('',*,*,#34851,.F.);
#45723=ORIENTED_EDGE('',*,*,#34852,.T.);
#45724=ORIENTED_EDGE('',*,*,#34853,.F.);
#45725=ORIENTED_EDGE('',*,*,#34549,.T.);
#45726=ORIENTED_EDGE('',*,*,#34853,.T.);
#45727=ORIENTED_EDGE('',*,*,#34854,.T.);
#45728=ORIENTED_EDGE('',*,*,#34855,.F.);
#45729=ORIENTED_EDGE('',*,*,#34854,.F.);
#45730=ORIENTED_EDGE('',*,*,#34852,.F.);
#45731=ORIENTED_EDGE('',*,*,#34856,.F.);
#45732=ORIENTED_EDGE('',*,*,#34857,.F.);
#45733=ORIENTED_EDGE('',*,*,#34543,.T.);
#45734=ORIENTED_EDGE('',*,*,#34858,.F.);
#45735=ORIENTED_EDGE('',*,*,#34859,.T.);
#45736=ORIENTED_EDGE('',*,*,#34860,.F.);
#45737=ORIENTED_EDGE('',*,*,#34540,.T.);
#45738=ORIENTED_EDGE('',*,*,#34860,.T.);
#45739=ORIENTED_EDGE('',*,*,#34861,.T.);
#45740=ORIENTED_EDGE('',*,*,#34862,.F.);
#45741=ORIENTED_EDGE('',*,*,#34861,.F.);
#45742=ORIENTED_EDGE('',*,*,#34859,.F.);
#45743=ORIENTED_EDGE('',*,*,#34863,.F.);
#45744=ORIENTED_EDGE('',*,*,#34864,.F.);
#45745=ORIENTED_EDGE('',*,*,#34534,.T.);
#45746=ORIENTED_EDGE('',*,*,#34865,.F.);
#45747=ORIENTED_EDGE('',*,*,#34866,.T.);
#45748=ORIENTED_EDGE('',*,*,#34867,.F.);
#45749=ORIENTED_EDGE('',*,*,#34531,.T.);
#45750=ORIENTED_EDGE('',*,*,#34867,.T.);
#45751=ORIENTED_EDGE('',*,*,#34868,.T.);
#45752=ORIENTED_EDGE('',*,*,#34869,.F.);
#45753=ORIENTED_EDGE('',*,*,#34868,.F.);
#45754=ORIENTED_EDGE('',*,*,#34866,.F.);
#45755=ORIENTED_EDGE('',*,*,#34870,.F.);
#45756=ORIENTED_EDGE('',*,*,#34871,.F.);
#45757=ORIENTED_EDGE('',*,*,#34528,.T.);
#45758=ORIENTED_EDGE('',*,*,#34872,.F.);
#45759=ORIENTED_EDGE('',*,*,#34873,.T.);
#45760=ORIENTED_EDGE('',*,*,#34874,.F.);
#45761=ORIENTED_EDGE('',*,*,#34526,.T.);
#45762=ORIENTED_EDGE('',*,*,#34874,.T.);
#45763=ORIENTED_EDGE('',*,*,#34875,.T.);
#45764=ORIENTED_EDGE('',*,*,#34876,.F.);
#45765=ORIENTED_EDGE('',*,*,#34875,.F.);
#45766=ORIENTED_EDGE('',*,*,#34873,.F.);
#45767=ORIENTED_EDGE('',*,*,#34877,.F.);
#45768=ORIENTED_EDGE('',*,*,#34878,.F.);
#45769=ORIENTED_EDGE('',*,*,#34520,.T.);
#45770=ORIENTED_EDGE('',*,*,#34879,.F.);
#45771=ORIENTED_EDGE('',*,*,#34880,.T.);
#45772=ORIENTED_EDGE('',*,*,#34881,.F.);
#45773=ORIENTED_EDGE('',*,*,#34517,.T.);
#45774=ORIENTED_EDGE('',*,*,#34881,.T.);
#45775=ORIENTED_EDGE('',*,*,#34882,.T.);
#45776=ORIENTED_EDGE('',*,*,#34883,.F.);
#45777=ORIENTED_EDGE('',*,*,#34882,.F.);
#45778=ORIENTED_EDGE('',*,*,#34880,.F.);
#45779=ORIENTED_EDGE('',*,*,#34884,.F.);
#45780=ORIENTED_EDGE('',*,*,#34885,.F.);
#45781=ORIENTED_EDGE('',*,*,#34511,.T.);
#45782=ORIENTED_EDGE('',*,*,#34886,.F.);
#45783=ORIENTED_EDGE('',*,*,#34887,.T.);
#45784=ORIENTED_EDGE('',*,*,#34888,.F.);
#45785=ORIENTED_EDGE('',*,*,#34508,.T.);
#45786=ORIENTED_EDGE('',*,*,#34888,.T.);
#45787=ORIENTED_EDGE('',*,*,#34889,.T.);
#45788=ORIENTED_EDGE('',*,*,#34890,.F.);
#45789=ORIENTED_EDGE('',*,*,#34889,.F.);
#45790=ORIENTED_EDGE('',*,*,#34887,.F.);
#45791=ORIENTED_EDGE('',*,*,#34891,.F.);
#45792=ORIENTED_EDGE('',*,*,#34892,.F.);
#45793=ORIENTED_EDGE('',*,*,#34502,.T.);
#45794=ORIENTED_EDGE('',*,*,#34893,.F.);
#45795=ORIENTED_EDGE('',*,*,#34894,.T.);
#45796=ORIENTED_EDGE('',*,*,#34895,.F.);
#45797=ORIENTED_EDGE('',*,*,#34499,.T.);
#45798=ORIENTED_EDGE('',*,*,#34895,.T.);
#45799=ORIENTED_EDGE('',*,*,#34896,.T.);
#45800=ORIENTED_EDGE('',*,*,#34897,.F.);
#45801=ORIENTED_EDGE('',*,*,#34896,.F.);
#45802=ORIENTED_EDGE('',*,*,#34894,.F.);
#45803=ORIENTED_EDGE('',*,*,#34898,.F.);
#45804=ORIENTED_EDGE('',*,*,#34899,.F.);
#45805=ORIENTED_EDGE('',*,*,#34493,.T.);
#45806=ORIENTED_EDGE('',*,*,#34900,.F.);
#45807=ORIENTED_EDGE('',*,*,#34901,.T.);
#45808=ORIENTED_EDGE('',*,*,#34902,.F.);
#45809=ORIENTED_EDGE('',*,*,#34490,.T.);
#45810=ORIENTED_EDGE('',*,*,#34902,.T.);
#45811=ORIENTED_EDGE('',*,*,#34903,.T.);
#45812=ORIENTED_EDGE('',*,*,#34904,.F.);
#45813=ORIENTED_EDGE('',*,*,#34903,.F.);
#45814=ORIENTED_EDGE('',*,*,#34901,.F.);
#45815=ORIENTED_EDGE('',*,*,#34905,.F.);
#45816=ORIENTED_EDGE('',*,*,#34906,.F.);
#45817=ORIENTED_EDGE('',*,*,#34484,.T.);
#45818=ORIENTED_EDGE('',*,*,#34907,.F.);
#45819=ORIENTED_EDGE('',*,*,#34908,.T.);
#45820=ORIENTED_EDGE('',*,*,#34909,.F.);
#45821=ORIENTED_EDGE('',*,*,#34481,.T.);
#45822=ORIENTED_EDGE('',*,*,#34909,.T.);
#45823=ORIENTED_EDGE('',*,*,#34910,.T.);
#45824=ORIENTED_EDGE('',*,*,#34911,.F.);
#45825=ORIENTED_EDGE('',*,*,#34910,.F.);
#45826=ORIENTED_EDGE('',*,*,#34908,.F.);
#45827=ORIENTED_EDGE('',*,*,#34912,.F.);
#45828=ORIENTED_EDGE('',*,*,#34913,.F.);
#45829=ORIENTED_EDGE('',*,*,#34475,.T.);
#45830=ORIENTED_EDGE('',*,*,#34914,.F.);
#45831=ORIENTED_EDGE('',*,*,#34915,.T.);
#45832=ORIENTED_EDGE('',*,*,#34916,.F.);
#45833=ORIENTED_EDGE('',*,*,#34471,.T.);
#45834=ORIENTED_EDGE('',*,*,#34916,.T.);
#45835=ORIENTED_EDGE('',*,*,#34917,.T.);
#45836=ORIENTED_EDGE('',*,*,#34918,.F.);
#45837=ORIENTED_EDGE('',*,*,#34917,.F.);
#45838=ORIENTED_EDGE('',*,*,#34915,.F.);
#45839=ORIENTED_EDGE('',*,*,#34919,.F.);
#45840=ORIENTED_EDGE('',*,*,#34920,.F.);
#45841=ORIENTED_EDGE('',*,*,#34727,.F.);
#45842=ORIENTED_EDGE('',*,*,#34921,.F.);
#45843=ORIENTED_EDGE('',*,*,#34922,.F.);
#45844=ORIENTED_EDGE('',*,*,#34923,.F.);
#45845=ORIENTED_EDGE('',*,*,#34724,.T.);
#45846=ORIENTED_EDGE('',*,*,#34924,.F.);
#45847=ORIENTED_EDGE('',*,*,#34921,.T.);
#45848=ORIENTED_EDGE('',*,*,#34726,.T.);
#45849=ORIENTED_EDGE('',*,*,#34925,.F.);
#45850=ORIENTED_EDGE('',*,*,#34470,.T.);
#45851=ORIENTED_EDGE('',*,*,#34722,.T.);
#45852=ORIENTED_EDGE('',*,*,#34926,.F.);
#45853=ORIENTED_EDGE('',*,*,#34927,.F.);
#45854=ORIENTED_EDGE('',*,*,#34928,.F.);
#45855=ORIENTED_EDGE('',*,*,#34477,.T.);
#45856=ORIENTED_EDGE('',*,*,#34476,.T.);
#45857=ORIENTED_EDGE('',*,*,#34929,.F.);
#45858=ORIENTED_EDGE('',*,*,#34480,.T.);
#45859=ORIENTED_EDGE('',*,*,#34478,.T.);
#45860=ORIENTED_EDGE('',*,*,#34928,.T.);
#45861=ORIENTED_EDGE('',*,*,#34930,.F.);
#45862=ORIENTED_EDGE('',*,*,#34931,.F.);
#45863=ORIENTED_EDGE('',*,*,#34486,.T.);
#45864=ORIENTED_EDGE('',*,*,#34485,.T.);
#45865=ORIENTED_EDGE('',*,*,#34932,.F.);
#45866=ORIENTED_EDGE('',*,*,#34489,.T.);
#45867=ORIENTED_EDGE('',*,*,#34487,.T.);
#45868=ORIENTED_EDGE('',*,*,#34931,.T.);
#45869=ORIENTED_EDGE('',*,*,#34933,.F.);
#45870=ORIENTED_EDGE('',*,*,#34934,.F.);
#45871=ORIENTED_EDGE('',*,*,#34495,.T.);
#45872=ORIENTED_EDGE('',*,*,#34494,.T.);
#45873=ORIENTED_EDGE('',*,*,#34935,.F.);
#45874=ORIENTED_EDGE('',*,*,#34498,.T.);
#45875=ORIENTED_EDGE('',*,*,#34496,.T.);
#45876=ORIENTED_EDGE('',*,*,#34934,.T.);
#45877=ORIENTED_EDGE('',*,*,#34936,.F.);
#45878=ORIENTED_EDGE('',*,*,#34937,.F.);
#45879=ORIENTED_EDGE('',*,*,#34504,.T.);
#45880=ORIENTED_EDGE('',*,*,#34503,.T.);
#45881=ORIENTED_EDGE('',*,*,#34938,.F.);
#45882=ORIENTED_EDGE('',*,*,#34507,.T.);
#45883=ORIENTED_EDGE('',*,*,#34505,.T.);
#45884=ORIENTED_EDGE('',*,*,#34937,.T.);
#45885=ORIENTED_EDGE('',*,*,#34939,.F.);
#45886=ORIENTED_EDGE('',*,*,#34940,.F.);
#45887=ORIENTED_EDGE('',*,*,#34513,.T.);
#45888=ORIENTED_EDGE('',*,*,#34512,.T.);
#45889=ORIENTED_EDGE('',*,*,#34941,.F.);
#45890=ORIENTED_EDGE('',*,*,#34516,.T.);
#45891=ORIENTED_EDGE('',*,*,#34514,.T.);
#45892=ORIENTED_EDGE('',*,*,#34940,.T.);
#45893=ORIENTED_EDGE('',*,*,#34942,.F.);
#45894=ORIENTED_EDGE('',*,*,#34943,.F.);
#45895=ORIENTED_EDGE('',*,*,#34522,.T.);
#45896=ORIENTED_EDGE('',*,*,#34521,.T.);
#45897=ORIENTED_EDGE('',*,*,#34944,.F.);
#45898=ORIENTED_EDGE('',*,*,#34525,.T.);
#45899=ORIENTED_EDGE('',*,*,#34523,.T.);
#45900=ORIENTED_EDGE('',*,*,#34943,.T.);
#45901=ORIENTED_EDGE('',*,*,#34945,.F.);
#45902=ORIENTED_EDGE('',*,*,#34946,.F.);
#45903=ORIENTED_EDGE('',*,*,#34467,.T.);
#45904=ORIENTED_EDGE('',*,*,#34529,.T.);
#45905=ORIENTED_EDGE('',*,*,#34947,.F.);
#45906=ORIENTED_EDGE('',*,*,#34530,.T.);
#45907=ORIENTED_EDGE('',*,*,#34468,.T.);
#45908=ORIENTED_EDGE('',*,*,#34946,.T.);
#45909=ORIENTED_EDGE('',*,*,#34948,.F.);
#45910=ORIENTED_EDGE('',*,*,#34949,.F.);
#45911=ORIENTED_EDGE('',*,*,#34536,.T.);
#45912=ORIENTED_EDGE('',*,*,#34535,.T.);
#45913=ORIENTED_EDGE('',*,*,#34950,.F.);
#45914=ORIENTED_EDGE('',*,*,#34539,.T.);
#45915=ORIENTED_EDGE('',*,*,#34537,.T.);
#45916=ORIENTED_EDGE('',*,*,#34949,.T.);
#45917=ORIENTED_EDGE('',*,*,#34951,.F.);
#45918=ORIENTED_EDGE('',*,*,#34952,.F.);
#45919=ORIENTED_EDGE('',*,*,#34545,.T.);
#45920=ORIENTED_EDGE('',*,*,#34544,.T.);
#45921=ORIENTED_EDGE('',*,*,#34953,.F.);
#45922=ORIENTED_EDGE('',*,*,#34548,.T.);
#45923=ORIENTED_EDGE('',*,*,#34546,.T.);
#45924=ORIENTED_EDGE('',*,*,#34952,.T.);
#45925=ORIENTED_EDGE('',*,*,#34954,.F.);
#45926=ORIENTED_EDGE('',*,*,#34955,.F.);
#45927=ORIENTED_EDGE('',*,*,#34554,.T.);
#45928=ORIENTED_EDGE('',*,*,#34553,.T.);
#45929=ORIENTED_EDGE('',*,*,#34956,.F.);
#45930=ORIENTED_EDGE('',*,*,#34557,.T.);
#45931=ORIENTED_EDGE('',*,*,#34555,.T.);
#45932=ORIENTED_EDGE('',*,*,#34955,.T.);
#45933=ORIENTED_EDGE('',*,*,#34957,.F.);
#45934=ORIENTED_EDGE('',*,*,#34958,.F.);
#45935=ORIENTED_EDGE('',*,*,#34563,.T.);
#45936=ORIENTED_EDGE('',*,*,#34562,.T.);
#45937=ORIENTED_EDGE('',*,*,#34959,.F.);
#45938=ORIENTED_EDGE('',*,*,#34566,.T.);
#45939=ORIENTED_EDGE('',*,*,#34564,.T.);
#45940=ORIENTED_EDGE('',*,*,#34958,.T.);
#45941=ORIENTED_EDGE('',*,*,#34960,.F.);
#45942=ORIENTED_EDGE('',*,*,#34961,.F.);
#45943=ORIENTED_EDGE('',*,*,#34572,.T.);
#45944=ORIENTED_EDGE('',*,*,#34571,.T.);
#45945=ORIENTED_EDGE('',*,*,#34962,.F.);
#45946=ORIENTED_EDGE('',*,*,#34575,.T.);
#45947=ORIENTED_EDGE('',*,*,#34573,.T.);
#45948=ORIENTED_EDGE('',*,*,#34961,.T.);
#45949=ORIENTED_EDGE('',*,*,#34963,.F.);
#45950=ORIENTED_EDGE('',*,*,#34964,.F.);
#45951=ORIENTED_EDGE('',*,*,#34581,.T.);
#45952=ORIENTED_EDGE('',*,*,#34580,.T.);
#45953=ORIENTED_EDGE('',*,*,#34965,.F.);
#45954=ORIENTED_EDGE('',*,*,#34584,.T.);
#45955=ORIENTED_EDGE('',*,*,#34582,.T.);
#45956=ORIENTED_EDGE('',*,*,#34964,.T.);
#45957=ORIENTED_EDGE('',*,*,#34966,.F.);
#45958=ORIENTED_EDGE('',*,*,#34967,.F.);
#45959=ORIENTED_EDGE('',*,*,#34590,.T.);
#45960=ORIENTED_EDGE('',*,*,#34589,.T.);
#45961=ORIENTED_EDGE('',*,*,#34968,.F.);
#45962=ORIENTED_EDGE('',*,*,#34593,.T.);
#45963=ORIENTED_EDGE('',*,*,#34591,.T.);
#45964=ORIENTED_EDGE('',*,*,#34967,.T.);
#45965=ORIENTED_EDGE('',*,*,#34969,.F.);
#45966=ORIENTED_EDGE('',*,*,#34970,.F.);
#45967=ORIENTED_EDGE('',*,*,#34599,.T.);
#45968=ORIENTED_EDGE('',*,*,#34598,.T.);
#45969=ORIENTED_EDGE('',*,*,#34971,.F.);
#45970=ORIENTED_EDGE('',*,*,#34602,.T.);
#45971=ORIENTED_EDGE('',*,*,#34600,.T.);
#45972=ORIENTED_EDGE('',*,*,#34970,.T.);
#45973=ORIENTED_EDGE('',*,*,#34972,.F.);
#45974=ORIENTED_EDGE('',*,*,#34973,.F.);
#45975=ORIENTED_EDGE('',*,*,#34608,.T.);
#45976=ORIENTED_EDGE('',*,*,#34607,.T.);
#45977=ORIENTED_EDGE('',*,*,#34974,.F.);
#45978=ORIENTED_EDGE('',*,*,#34611,.T.);
#45979=ORIENTED_EDGE('',*,*,#34609,.T.);
#45980=ORIENTED_EDGE('',*,*,#34973,.T.);
#45981=ORIENTED_EDGE('',*,*,#34975,.F.);
#45982=ORIENTED_EDGE('',*,*,#34976,.F.);
#45983=ORIENTED_EDGE('',*,*,#34617,.T.);
#45984=ORIENTED_EDGE('',*,*,#34616,.T.);
#45985=ORIENTED_EDGE('',*,*,#34977,.F.);
#45986=ORIENTED_EDGE('',*,*,#34620,.T.);
#45987=ORIENTED_EDGE('',*,*,#34618,.T.);
#45988=ORIENTED_EDGE('',*,*,#34976,.T.);
#45989=ORIENTED_EDGE('',*,*,#34978,.F.);
#45990=ORIENTED_EDGE('',*,*,#34979,.F.);
#45991=ORIENTED_EDGE('',*,*,#34626,.T.);
#45992=ORIENTED_EDGE('',*,*,#34625,.T.);
#45993=ORIENTED_EDGE('',*,*,#34980,.F.);
#45994=ORIENTED_EDGE('',*,*,#34629,.T.);
#45995=ORIENTED_EDGE('',*,*,#34627,.T.);
#45996=ORIENTED_EDGE('',*,*,#34979,.T.);
#45997=ORIENTED_EDGE('',*,*,#34981,.F.);
#45998=ORIENTED_EDGE('',*,*,#34982,.F.);
#45999=ORIENTED_EDGE('',*,*,#34635,.T.);
#46000=ORIENTED_EDGE('',*,*,#34634,.T.);
#46001=ORIENTED_EDGE('',*,*,#34983,.F.);
#46002=ORIENTED_EDGE('',*,*,#34638,.T.);
#46003=ORIENTED_EDGE('',*,*,#34636,.T.);
#46004=ORIENTED_EDGE('',*,*,#34982,.T.);
#46005=ORIENTED_EDGE('',*,*,#34984,.F.);
#46006=ORIENTED_EDGE('',*,*,#34985,.F.);
#46007=ORIENTED_EDGE('',*,*,#34644,.T.);
#46008=ORIENTED_EDGE('',*,*,#34643,.T.);
#46009=ORIENTED_EDGE('',*,*,#34986,.F.);
#46010=ORIENTED_EDGE('',*,*,#34647,.T.);
#46011=ORIENTED_EDGE('',*,*,#34645,.T.);
#46012=ORIENTED_EDGE('',*,*,#34985,.T.);
#46013=ORIENTED_EDGE('',*,*,#34987,.F.);
#46014=ORIENTED_EDGE('',*,*,#34988,.F.);
#46015=ORIENTED_EDGE('',*,*,#34653,.T.);
#46016=ORIENTED_EDGE('',*,*,#34652,.T.);
#46017=ORIENTED_EDGE('',*,*,#34989,.F.);
#46018=ORIENTED_EDGE('',*,*,#34656,.T.);
#46019=ORIENTED_EDGE('',*,*,#34654,.T.);
#46020=ORIENTED_EDGE('',*,*,#34988,.T.);
#46021=ORIENTED_EDGE('',*,*,#34990,.F.);
#46022=ORIENTED_EDGE('',*,*,#34991,.F.);
#46023=ORIENTED_EDGE('',*,*,#34662,.T.);
#46024=ORIENTED_EDGE('',*,*,#34661,.T.);
#46025=ORIENTED_EDGE('',*,*,#34992,.F.);
#46026=ORIENTED_EDGE('',*,*,#34665,.T.);
#46027=ORIENTED_EDGE('',*,*,#34663,.T.);
#46028=ORIENTED_EDGE('',*,*,#34991,.T.);
#46029=ORIENTED_EDGE('',*,*,#34993,.F.);
#46030=ORIENTED_EDGE('',*,*,#34994,.F.);
#46031=ORIENTED_EDGE('',*,*,#34671,.T.);
#46032=ORIENTED_EDGE('',*,*,#34670,.T.);
#46033=ORIENTED_EDGE('',*,*,#34995,.F.);
#46034=ORIENTED_EDGE('',*,*,#34674,.T.);
#46035=ORIENTED_EDGE('',*,*,#34672,.T.);
#46036=ORIENTED_EDGE('',*,*,#34994,.T.);
#46037=ORIENTED_EDGE('',*,*,#34996,.F.);
#46038=ORIENTED_EDGE('',*,*,#34997,.F.);
#46039=ORIENTED_EDGE('',*,*,#34680,.T.);
#46040=ORIENTED_EDGE('',*,*,#34679,.T.);
#46041=ORIENTED_EDGE('',*,*,#34998,.F.);
#46042=ORIENTED_EDGE('',*,*,#34683,.T.);
#46043=ORIENTED_EDGE('',*,*,#34681,.T.);
#46044=ORIENTED_EDGE('',*,*,#34997,.T.);
#46045=ORIENTED_EDGE('',*,*,#34999,.F.);
#46046=ORIENTED_EDGE('',*,*,#35000,.F.);
#46047=ORIENTED_EDGE('',*,*,#34692,.T.);
#46048=ORIENTED_EDGE('',*,*,#34688,.T.);
#46049=ORIENTED_EDGE('',*,*,#34693,.T.);
#46050=ORIENTED_EDGE('',*,*,#35000,.T.);
#46051=ORIENTED_EDGE('',*,*,#35001,.F.);
#46052=ORIENTED_EDGE('',*,*,#34690,.T.);
#46053=ORIENTED_EDGE('',*,*,#34699,.T.);
#46054=ORIENTED_EDGE('',*,*,#34697,.T.);
#46055=ORIENTED_EDGE('',*,*,#35002,.F.);
#46056=ORIENTED_EDGE('',*,*,#35003,.F.);
#46057=ORIENTED_EDGE('',*,*,#35004,.F.);
#46058=ORIENTED_EDGE('',*,*,#34702,.T.);
#46059=ORIENTED_EDGE('',*,*,#34700,.T.);
#46060=ORIENTED_EDGE('',*,*,#35003,.T.);
#46061=ORIENTED_EDGE('',*,*,#35005,.F.);
#46062=ORIENTED_EDGE('',*,*,#35006,.F.);
#46063=ORIENTED_EDGE('',*,*,#34707,.T.);
#46064=ORIENTED_EDGE('',*,*,#34706,.T.);
#46065=ORIENTED_EDGE('',*,*,#35007,.F.);
#46066=ORIENTED_EDGE('',*,*,#34710,.T.);
#46067=ORIENTED_EDGE('',*,*,#34708,.T.);
#46068=ORIENTED_EDGE('',*,*,#35006,.T.);
#46069=ORIENTED_EDGE('',*,*,#35008,.F.);
#46070=ORIENTED_EDGE('',*,*,#35009,.F.);
#46071=ORIENTED_EDGE('',*,*,#34716,.T.);
#46072=ORIENTED_EDGE('',*,*,#34715,.T.);
#46073=ORIENTED_EDGE('',*,*,#35010,.F.);
#46074=ORIENTED_EDGE('',*,*,#34719,.T.);
#46075=ORIENTED_EDGE('',*,*,#34717,.T.);
#46076=ORIENTED_EDGE('',*,*,#35009,.T.);
#46077=ORIENTED_EDGE('',*,*,#35011,.F.);
#46078=ORIENTED_EDGE('',*,*,#34926,.T.);
#46079=ORIENTED_EDGE('',*,*,#34721,.T.);
#46080=ORIENTED_EDGE('',*,*,#34725,.T.);
#46081=ORIENTED_EDGE('',*,*,#34923,.T.);
#46082=ORIENTED_EDGE('',*,*,#35012,.F.);
#46083=ORIENTED_EDGE('',*,*,#35013,.F.);
#46084=ORIENTED_EDGE('',*,*,#34728,.T.);
#46085=ORIENTED_EDGE('',*,*,#34734,.T.);
#46086=ORIENTED_EDGE('',*,*,#34729,.T.);
#46087=ORIENTED_EDGE('',*,*,#35014,.F.);
#46088=ORIENTED_EDGE('',*,*,#35015,.F.);
#46089=ORIENTED_EDGE('',*,*,#34735,.T.);
#46090=ORIENTED_EDGE('',*,*,#35015,.T.);
#46091=ORIENTED_EDGE('',*,*,#35016,.F.);
#46092=ORIENTED_EDGE('',*,*,#34733,.T.);
#46093=ORIENTED_EDGE('',*,*,#35017,.F.);
#46094=ORIENTED_EDGE('',*,*,#35018,.F.);
#46095=ORIENTED_EDGE('',*,*,#34741,.T.);
#46096=ORIENTED_EDGE('',*,*,#34736,.T.);
#46097=ORIENTED_EDGE('',*,*,#34742,.T.);
#46098=ORIENTED_EDGE('',*,*,#35018,.T.);
#46099=ORIENTED_EDGE('',*,*,#35019,.F.);
#46100=ORIENTED_EDGE('',*,*,#34740,.T.);
#46101=ORIENTED_EDGE('',*,*,#34748,.T.);
#46102=ORIENTED_EDGE('',*,*,#34743,.T.);
#46103=ORIENTED_EDGE('',*,*,#35020,.F.);
#46104=ORIENTED_EDGE('',*,*,#35021,.F.);
#46105=ORIENTED_EDGE('',*,*,#34749,.T.);
#46106=ORIENTED_EDGE('',*,*,#35021,.T.);
#46107=ORIENTED_EDGE('',*,*,#35022,.F.);
#46108=ORIENTED_EDGE('',*,*,#34747,.T.);
#46109=ORIENTED_EDGE('',*,*,#34755,.T.);
#46110=ORIENTED_EDGE('',*,*,#34750,.T.);
#46111=ORIENTED_EDGE('',*,*,#35023,.F.);
#46112=ORIENTED_EDGE('',*,*,#35024,.F.);
#46113=ORIENTED_EDGE('',*,*,#34756,.T.);
#46114=ORIENTED_EDGE('',*,*,#35024,.T.);
#46115=ORIENTED_EDGE('',*,*,#35025,.F.);
#46116=ORIENTED_EDGE('',*,*,#34754,.T.);
#46117=ORIENTED_EDGE('',*,*,#34762,.T.);
#46118=ORIENTED_EDGE('',*,*,#34757,.T.);
#46119=ORIENTED_EDGE('',*,*,#35026,.F.);
#46120=ORIENTED_EDGE('',*,*,#35027,.F.);
#46121=ORIENTED_EDGE('',*,*,#34763,.T.);
#46122=ORIENTED_EDGE('',*,*,#35027,.T.);
#46123=ORIENTED_EDGE('',*,*,#35028,.F.);
#46124=ORIENTED_EDGE('',*,*,#34761,.T.);
#46125=ORIENTED_EDGE('',*,*,#34769,.T.);
#46126=ORIENTED_EDGE('',*,*,#34764,.T.);
#46127=ORIENTED_EDGE('',*,*,#35029,.F.);
#46128=ORIENTED_EDGE('',*,*,#35030,.F.);
#46129=ORIENTED_EDGE('',*,*,#34770,.T.);
#46130=ORIENTED_EDGE('',*,*,#35030,.T.);
#46131=ORIENTED_EDGE('',*,*,#35031,.F.);
#46132=ORIENTED_EDGE('',*,*,#34768,.T.);
#46133=ORIENTED_EDGE('',*,*,#34776,.T.);
#46134=ORIENTED_EDGE('',*,*,#34771,.T.);
#46135=ORIENTED_EDGE('',*,*,#35032,.F.);
#46136=ORIENTED_EDGE('',*,*,#35033,.F.);
#46137=ORIENTED_EDGE('',*,*,#34777,.T.);
#46138=ORIENTED_EDGE('',*,*,#35033,.T.);
#46139=ORIENTED_EDGE('',*,*,#35034,.F.);
#46140=ORIENTED_EDGE('',*,*,#34775,.T.);
#46141=ORIENTED_EDGE('',*,*,#34783,.T.);
#46142=ORIENTED_EDGE('',*,*,#34778,.T.);
#46143=ORIENTED_EDGE('',*,*,#35035,.F.);
#46144=ORIENTED_EDGE('',*,*,#35036,.F.);
#46145=ORIENTED_EDGE('',*,*,#34784,.T.);
#46146=ORIENTED_EDGE('',*,*,#35036,.T.);
#46147=ORIENTED_EDGE('',*,*,#35037,.F.);
#46148=ORIENTED_EDGE('',*,*,#34782,.T.);
#46149=ORIENTED_EDGE('',*,*,#34790,.T.);
#46150=ORIENTED_EDGE('',*,*,#34785,.T.);
#46151=ORIENTED_EDGE('',*,*,#35038,.F.);
#46152=ORIENTED_EDGE('',*,*,#35039,.F.);
#46153=ORIENTED_EDGE('',*,*,#34791,.T.);
#46154=ORIENTED_EDGE('',*,*,#35039,.T.);
#46155=ORIENTED_EDGE('',*,*,#35040,.F.);
#46156=ORIENTED_EDGE('',*,*,#34789,.T.);
#46157=ORIENTED_EDGE('',*,*,#34797,.T.);
#46158=ORIENTED_EDGE('',*,*,#34792,.T.);
#46159=ORIENTED_EDGE('',*,*,#35041,.F.);
#46160=ORIENTED_EDGE('',*,*,#35042,.F.);
#46161=ORIENTED_EDGE('',*,*,#34798,.T.);
#46162=ORIENTED_EDGE('',*,*,#35042,.T.);
#46163=ORIENTED_EDGE('',*,*,#35043,.F.);
#46164=ORIENTED_EDGE('',*,*,#34796,.T.);
#46165=ORIENTED_EDGE('',*,*,#34804,.T.);
#46166=ORIENTED_EDGE('',*,*,#34799,.T.);
#46167=ORIENTED_EDGE('',*,*,#35044,.F.);
#46168=ORIENTED_EDGE('',*,*,#35045,.F.);
#46169=ORIENTED_EDGE('',*,*,#34805,.T.);
#46170=ORIENTED_EDGE('',*,*,#35045,.T.);
#46171=ORIENTED_EDGE('',*,*,#35046,.F.);
#46172=ORIENTED_EDGE('',*,*,#34803,.T.);
#46173=ORIENTED_EDGE('',*,*,#34811,.T.);
#46174=ORIENTED_EDGE('',*,*,#34806,.T.);
#46175=ORIENTED_EDGE('',*,*,#35047,.F.);
#46176=ORIENTED_EDGE('',*,*,#35048,.F.);
#46177=ORIENTED_EDGE('',*,*,#34812,.T.);
#46178=ORIENTED_EDGE('',*,*,#35048,.T.);
#46179=ORIENTED_EDGE('',*,*,#35049,.F.);
#46180=ORIENTED_EDGE('',*,*,#34810,.T.);
#46181=ORIENTED_EDGE('',*,*,#34818,.T.);
#46182=ORIENTED_EDGE('',*,*,#34813,.T.);
#46183=ORIENTED_EDGE('',*,*,#35050,.F.);
#46184=ORIENTED_EDGE('',*,*,#35051,.F.);
#46185=ORIENTED_EDGE('',*,*,#34819,.T.);
#46186=ORIENTED_EDGE('',*,*,#35051,.T.);
#46187=ORIENTED_EDGE('',*,*,#35052,.F.);
#46188=ORIENTED_EDGE('',*,*,#34817,.T.);
#46189=ORIENTED_EDGE('',*,*,#34464,.T.);
#46190=ORIENTED_EDGE('',*,*,#34820,.T.);
#46191=ORIENTED_EDGE('',*,*,#35053,.F.);
#46192=ORIENTED_EDGE('',*,*,#35054,.F.);
#46193=ORIENTED_EDGE('',*,*,#34461,.T.);
#46194=ORIENTED_EDGE('',*,*,#35054,.T.);
#46195=ORIENTED_EDGE('',*,*,#35055,.F.);
#46196=ORIENTED_EDGE('',*,*,#34822,.T.);
#46197=ORIENTED_EDGE('',*,*,#34828,.T.);
#46198=ORIENTED_EDGE('',*,*,#34823,.T.);
#46199=ORIENTED_EDGE('',*,*,#35056,.F.);
#46200=ORIENTED_EDGE('',*,*,#35057,.F.);
#46201=ORIENTED_EDGE('',*,*,#34829,.T.);
#46202=ORIENTED_EDGE('',*,*,#35057,.T.);
#46203=ORIENTED_EDGE('',*,*,#35058,.F.);
#46204=ORIENTED_EDGE('',*,*,#34827,.T.);
#46205=ORIENTED_EDGE('',*,*,#34835,.T.);
#46206=ORIENTED_EDGE('',*,*,#34830,.T.);
#46207=ORIENTED_EDGE('',*,*,#35059,.F.);
#46208=ORIENTED_EDGE('',*,*,#35060,.F.);
#46209=ORIENTED_EDGE('',*,*,#34836,.T.);
#46210=ORIENTED_EDGE('',*,*,#35060,.T.);
#46211=ORIENTED_EDGE('',*,*,#35061,.F.);
#46212=ORIENTED_EDGE('',*,*,#34834,.T.);
#46213=ORIENTED_EDGE('',*,*,#34842,.T.);
#46214=ORIENTED_EDGE('',*,*,#34837,.T.);
#46215=ORIENTED_EDGE('',*,*,#35062,.F.);
#46216=ORIENTED_EDGE('',*,*,#35063,.F.);
#46217=ORIENTED_EDGE('',*,*,#34843,.T.);
#46218=ORIENTED_EDGE('',*,*,#35063,.T.);
#46219=ORIENTED_EDGE('',*,*,#35064,.F.);
#46220=ORIENTED_EDGE('',*,*,#34841,.T.);
#46221=ORIENTED_EDGE('',*,*,#34849,.T.);
#46222=ORIENTED_EDGE('',*,*,#34844,.T.);
#46223=ORIENTED_EDGE('',*,*,#35065,.F.);
#46224=ORIENTED_EDGE('',*,*,#35066,.F.);
#46225=ORIENTED_EDGE('',*,*,#34850,.T.);
#46226=ORIENTED_EDGE('',*,*,#35066,.T.);
#46227=ORIENTED_EDGE('',*,*,#35067,.F.);
#46228=ORIENTED_EDGE('',*,*,#34848,.T.);
#46229=ORIENTED_EDGE('',*,*,#34856,.T.);
#46230=ORIENTED_EDGE('',*,*,#34851,.T.);
#46231=ORIENTED_EDGE('',*,*,#35068,.F.);
#46232=ORIENTED_EDGE('',*,*,#35069,.F.);
#46233=ORIENTED_EDGE('',*,*,#34857,.T.);
#46234=ORIENTED_EDGE('',*,*,#35069,.T.);
#46235=ORIENTED_EDGE('',*,*,#35070,.F.);
#46236=ORIENTED_EDGE('',*,*,#34855,.T.);
#46237=ORIENTED_EDGE('',*,*,#34863,.T.);
#46238=ORIENTED_EDGE('',*,*,#34858,.T.);
#46239=ORIENTED_EDGE('',*,*,#35071,.F.);
#46240=ORIENTED_EDGE('',*,*,#35072,.F.);
#46241=ORIENTED_EDGE('',*,*,#34864,.T.);
#46242=ORIENTED_EDGE('',*,*,#35072,.T.);
#46243=ORIENTED_EDGE('',*,*,#35073,.F.);
#46244=ORIENTED_EDGE('',*,*,#34862,.T.);
#46245=ORIENTED_EDGE('',*,*,#34870,.T.);
#46246=ORIENTED_EDGE('',*,*,#34865,.T.);
#46247=ORIENTED_EDGE('',*,*,#35074,.F.);
#46248=ORIENTED_EDGE('',*,*,#35075,.F.);
#46249=ORIENTED_EDGE('',*,*,#34871,.T.);
#46250=ORIENTED_EDGE('',*,*,#35075,.T.);
#46251=ORIENTED_EDGE('',*,*,#35076,.F.);
#46252=ORIENTED_EDGE('',*,*,#34869,.T.);
#46253=ORIENTED_EDGE('',*,*,#34877,.T.);
#46254=ORIENTED_EDGE('',*,*,#34872,.T.);
#46255=ORIENTED_EDGE('',*,*,#35077,.F.);
#46256=ORIENTED_EDGE('',*,*,#35078,.F.);
#46257=ORIENTED_EDGE('',*,*,#34878,.T.);
#46258=ORIENTED_EDGE('',*,*,#35078,.T.);
#46259=ORIENTED_EDGE('',*,*,#35079,.F.);
#46260=ORIENTED_EDGE('',*,*,#34876,.T.);
#46261=ORIENTED_EDGE('',*,*,#34884,.T.);
#46262=ORIENTED_EDGE('',*,*,#34879,.T.);
#46263=ORIENTED_EDGE('',*,*,#35080,.F.);
#46264=ORIENTED_EDGE('',*,*,#35081,.F.);
#46265=ORIENTED_EDGE('',*,*,#34885,.T.);
#46266=ORIENTED_EDGE('',*,*,#35081,.T.);
#46267=ORIENTED_EDGE('',*,*,#35082,.F.);
#46268=ORIENTED_EDGE('',*,*,#34883,.T.);
#46269=ORIENTED_EDGE('',*,*,#34891,.T.);
#46270=ORIENTED_EDGE('',*,*,#34886,.T.);
#46271=ORIENTED_EDGE('',*,*,#35083,.F.);
#46272=ORIENTED_EDGE('',*,*,#35084,.F.);
#46273=ORIENTED_EDGE('',*,*,#34892,.T.);
#46274=ORIENTED_EDGE('',*,*,#35084,.T.);
#46275=ORIENTED_EDGE('',*,*,#35085,.F.);
#46276=ORIENTED_EDGE('',*,*,#34890,.T.);
#46277=ORIENTED_EDGE('',*,*,#34898,.T.);
#46278=ORIENTED_EDGE('',*,*,#34893,.T.);
#46279=ORIENTED_EDGE('',*,*,#35086,.F.);
#46280=ORIENTED_EDGE('',*,*,#35087,.F.);
#46281=ORIENTED_EDGE('',*,*,#34899,.T.);
#46282=ORIENTED_EDGE('',*,*,#35087,.T.);
#46283=ORIENTED_EDGE('',*,*,#35088,.F.);
#46284=ORIENTED_EDGE('',*,*,#34897,.T.);
#46285=ORIENTED_EDGE('',*,*,#34905,.T.);
#46286=ORIENTED_EDGE('',*,*,#34900,.T.);
#46287=ORIENTED_EDGE('',*,*,#35089,.F.);
#46288=ORIENTED_EDGE('',*,*,#35090,.F.);
#46289=ORIENTED_EDGE('',*,*,#34906,.T.);
#46290=ORIENTED_EDGE('',*,*,#35090,.T.);
#46291=ORIENTED_EDGE('',*,*,#35091,.F.);
#46292=ORIENTED_EDGE('',*,*,#34904,.T.);
#46293=ORIENTED_EDGE('',*,*,#34912,.T.);
#46294=ORIENTED_EDGE('',*,*,#34907,.T.);
#46295=ORIENTED_EDGE('',*,*,#35092,.F.);
#46296=ORIENTED_EDGE('',*,*,#35093,.F.);
#46297=ORIENTED_EDGE('',*,*,#34913,.T.);
#46298=ORIENTED_EDGE('',*,*,#35093,.T.);
#46299=ORIENTED_EDGE('',*,*,#35094,.F.);
#46300=ORIENTED_EDGE('',*,*,#34911,.T.);
#46301=ORIENTED_EDGE('',*,*,#34919,.T.);
#46302=ORIENTED_EDGE('',*,*,#34914,.T.);
#46303=ORIENTED_EDGE('',*,*,#35095,.F.);
#46304=ORIENTED_EDGE('',*,*,#35096,.F.);
#46305=ORIENTED_EDGE('',*,*,#34920,.T.);
#46306=ORIENTED_EDGE('',*,*,#35096,.T.);
#46307=ORIENTED_EDGE('',*,*,#35097,.F.);
#46308=ORIENTED_EDGE('',*,*,#34918,.T.);
#46309=ORIENTED_EDGE('',*,*,#34922,.T.);
#46310=ORIENTED_EDGE('',*,*,#34924,.T.);
#46311=ORIENTED_EDGE('',*,*,#35098,.F.);
#46312=ORIENTED_EDGE('',*,*,#35012,.T.);
#46313=ORIENTED_EDGE('',*,*,#35099,.T.);
#46314=ORIENTED_EDGE('',*,*,#35100,.F.);
#46315=ORIENTED_EDGE('',*,*,#34925,.T.);
#46316=ORIENTED_EDGE('',*,*,#35101,.F.);
#46317=ORIENTED_EDGE('',*,*,#35102,.F.);
#46318=ORIENTED_EDGE('',*,*,#35103,.F.);
#46319=ORIENTED_EDGE('',*,*,#35104,.F.);
#46320=ORIENTED_EDGE('',*,*,#35099,.F.);
#46321=ORIENTED_EDGE('',*,*,#35104,.T.);
#46322=ORIENTED_EDGE('',*,*,#35105,.F.);
#46323=ORIENTED_EDGE('',*,*,#34927,.T.);
#46324=ORIENTED_EDGE('',*,*,#35100,.T.);
#46325=ORIENTED_EDGE('',*,*,#35106,.T.);
#46326=ORIENTED_EDGE('',*,*,#35107,.F.);
#46327=ORIENTED_EDGE('',*,*,#34929,.T.);
#46328=ORIENTED_EDGE('',*,*,#35108,.F.);
#46329=ORIENTED_EDGE('',*,*,#35109,.F.);
#46330=ORIENTED_EDGE('',*,*,#35110,.F.);
#46331=ORIENTED_EDGE('',*,*,#35111,.F.);
#46332=ORIENTED_EDGE('',*,*,#35106,.F.);
#46333=ORIENTED_EDGE('',*,*,#35111,.T.);
#46334=ORIENTED_EDGE('',*,*,#35112,.F.);
#46335=ORIENTED_EDGE('',*,*,#34930,.T.);
#46336=ORIENTED_EDGE('',*,*,#35107,.T.);
#46337=ORIENTED_EDGE('',*,*,#35113,.T.);
#46338=ORIENTED_EDGE('',*,*,#35114,.F.);
#46339=ORIENTED_EDGE('',*,*,#34932,.T.);
#46340=ORIENTED_EDGE('',*,*,#35115,.F.);
#46341=ORIENTED_EDGE('',*,*,#35116,.F.);
#46342=ORIENTED_EDGE('',*,*,#35117,.F.);
#46343=ORIENTED_EDGE('',*,*,#35118,.F.);
#46344=ORIENTED_EDGE('',*,*,#35113,.F.);
#46345=ORIENTED_EDGE('',*,*,#35118,.T.);
#46346=ORIENTED_EDGE('',*,*,#35119,.F.);
#46347=ORIENTED_EDGE('',*,*,#34933,.T.);
#46348=ORIENTED_EDGE('',*,*,#35114,.T.);
#46349=ORIENTED_EDGE('',*,*,#35120,.T.);
#46350=ORIENTED_EDGE('',*,*,#35121,.F.);
#46351=ORIENTED_EDGE('',*,*,#34935,.T.);
#46352=ORIENTED_EDGE('',*,*,#35122,.F.);
#46353=ORIENTED_EDGE('',*,*,#35123,.F.);
#46354=ORIENTED_EDGE('',*,*,#35124,.F.);
#46355=ORIENTED_EDGE('',*,*,#35125,.F.);
#46356=ORIENTED_EDGE('',*,*,#35120,.F.);
#46357=ORIENTED_EDGE('',*,*,#35125,.T.);
#46358=ORIENTED_EDGE('',*,*,#35126,.F.);
#46359=ORIENTED_EDGE('',*,*,#34936,.T.);
#46360=ORIENTED_EDGE('',*,*,#35121,.T.);
#46361=ORIENTED_EDGE('',*,*,#35127,.T.);
#46362=ORIENTED_EDGE('',*,*,#35128,.F.);
#46363=ORIENTED_EDGE('',*,*,#34938,.T.);
#46364=ORIENTED_EDGE('',*,*,#35129,.F.);
#46365=ORIENTED_EDGE('',*,*,#35130,.F.);
#46366=ORIENTED_EDGE('',*,*,#35131,.F.);
#46367=ORIENTED_EDGE('',*,*,#35132,.F.);
#46368=ORIENTED_EDGE('',*,*,#35127,.F.);
#46369=ORIENTED_EDGE('',*,*,#35132,.T.);
#46370=ORIENTED_EDGE('',*,*,#35133,.F.);
#46371=ORIENTED_EDGE('',*,*,#34939,.T.);
#46372=ORIENTED_EDGE('',*,*,#35128,.T.);
#46373=ORIENTED_EDGE('',*,*,#35134,.T.);
#46374=ORIENTED_EDGE('',*,*,#35135,.F.);
#46375=ORIENTED_EDGE('',*,*,#34941,.T.);
#46376=ORIENTED_EDGE('',*,*,#35136,.F.);
#46377=ORIENTED_EDGE('',*,*,#35137,.F.);
#46378=ORIENTED_EDGE('',*,*,#35138,.F.);
#46379=ORIENTED_EDGE('',*,*,#35139,.F.);
#46380=ORIENTED_EDGE('',*,*,#35134,.F.);
#46381=ORIENTED_EDGE('',*,*,#35139,.T.);
#46382=ORIENTED_EDGE('',*,*,#35140,.F.);
#46383=ORIENTED_EDGE('',*,*,#34942,.T.);
#46384=ORIENTED_EDGE('',*,*,#35135,.T.);
#46385=ORIENTED_EDGE('',*,*,#35141,.T.);
#46386=ORIENTED_EDGE('',*,*,#35142,.F.);
#46387=ORIENTED_EDGE('',*,*,#34944,.T.);
#46388=ORIENTED_EDGE('',*,*,#35143,.F.);
#46389=ORIENTED_EDGE('',*,*,#35144,.F.);
#46390=ORIENTED_EDGE('',*,*,#35145,.F.);
#46391=ORIENTED_EDGE('',*,*,#35146,.F.);
#46392=ORIENTED_EDGE('',*,*,#35141,.F.);
#46393=ORIENTED_EDGE('',*,*,#35146,.T.);
#46394=ORIENTED_EDGE('',*,*,#35147,.F.);
#46395=ORIENTED_EDGE('',*,*,#34945,.T.);
#46396=ORIENTED_EDGE('',*,*,#35142,.T.);
#46397=ORIENTED_EDGE('',*,*,#35148,.T.);
#46398=ORIENTED_EDGE('',*,*,#35149,.F.);
#46399=ORIENTED_EDGE('',*,*,#34947,.T.);
#46400=ORIENTED_EDGE('',*,*,#35150,.F.);
#46401=ORIENTED_EDGE('',*,*,#35151,.F.);
#46402=ORIENTED_EDGE('',*,*,#35152,.F.);
#46403=ORIENTED_EDGE('',*,*,#35153,.F.);
#46404=ORIENTED_EDGE('',*,*,#35148,.F.);
#46405=ORIENTED_EDGE('',*,*,#35153,.T.);
#46406=ORIENTED_EDGE('',*,*,#35154,.F.);
#46407=ORIENTED_EDGE('',*,*,#34948,.T.);
#46408=ORIENTED_EDGE('',*,*,#35149,.T.);
#46409=ORIENTED_EDGE('',*,*,#35155,.T.);
#46410=ORIENTED_EDGE('',*,*,#35156,.F.);
#46411=ORIENTED_EDGE('',*,*,#34950,.T.);
#46412=ORIENTED_EDGE('',*,*,#35157,.F.);
#46413=ORIENTED_EDGE('',*,*,#35158,.F.);
#46414=ORIENTED_EDGE('',*,*,#35159,.F.);
#46415=ORIENTED_EDGE('',*,*,#35160,.F.);
#46416=ORIENTED_EDGE('',*,*,#35155,.F.);
#46417=ORIENTED_EDGE('',*,*,#35160,.T.);
#46418=ORIENTED_EDGE('',*,*,#35161,.F.);
#46419=ORIENTED_EDGE('',*,*,#34951,.T.);
#46420=ORIENTED_EDGE('',*,*,#35156,.T.);
#46421=ORIENTED_EDGE('',*,*,#35162,.T.);
#46422=ORIENTED_EDGE('',*,*,#35163,.F.);
#46423=ORIENTED_EDGE('',*,*,#34953,.T.);
#46424=ORIENTED_EDGE('',*,*,#35164,.F.);
#46425=ORIENTED_EDGE('',*,*,#35165,.F.);
#46426=ORIENTED_EDGE('',*,*,#35166,.F.);
#46427=ORIENTED_EDGE('',*,*,#35167,.F.);
#46428=ORIENTED_EDGE('',*,*,#35162,.F.);
#46429=ORIENTED_EDGE('',*,*,#35167,.T.);
#46430=ORIENTED_EDGE('',*,*,#35168,.F.);
#46431=ORIENTED_EDGE('',*,*,#34954,.T.);
#46432=ORIENTED_EDGE('',*,*,#35163,.T.);
#46433=ORIENTED_EDGE('',*,*,#35169,.T.);
#46434=ORIENTED_EDGE('',*,*,#35170,.F.);
#46435=ORIENTED_EDGE('',*,*,#34956,.T.);
#46436=ORIENTED_EDGE('',*,*,#35171,.F.);
#46437=ORIENTED_EDGE('',*,*,#35172,.F.);
#46438=ORIENTED_EDGE('',*,*,#35173,.F.);
#46439=ORIENTED_EDGE('',*,*,#35174,.F.);
#46440=ORIENTED_EDGE('',*,*,#35169,.F.);
#46441=ORIENTED_EDGE('',*,*,#35174,.T.);
#46442=ORIENTED_EDGE('',*,*,#35175,.F.);
#46443=ORIENTED_EDGE('',*,*,#34957,.T.);
#46444=ORIENTED_EDGE('',*,*,#35170,.T.);
#46445=ORIENTED_EDGE('',*,*,#35176,.T.);
#46446=ORIENTED_EDGE('',*,*,#35177,.F.);
#46447=ORIENTED_EDGE('',*,*,#34959,.T.);
#46448=ORIENTED_EDGE('',*,*,#35178,.F.);
#46449=ORIENTED_EDGE('',*,*,#35179,.F.);
#46450=ORIENTED_EDGE('',*,*,#35180,.F.);
#46451=ORIENTED_EDGE('',*,*,#35181,.F.);
#46452=ORIENTED_EDGE('',*,*,#35176,.F.);
#46453=ORIENTED_EDGE('',*,*,#35181,.T.);
#46454=ORIENTED_EDGE('',*,*,#35182,.F.);
#46455=ORIENTED_EDGE('',*,*,#34960,.T.);
#46456=ORIENTED_EDGE('',*,*,#35177,.T.);
#46457=ORIENTED_EDGE('',*,*,#35183,.T.);
#46458=ORIENTED_EDGE('',*,*,#35184,.F.);
#46459=ORIENTED_EDGE('',*,*,#34962,.T.);
#46460=ORIENTED_EDGE('',*,*,#35185,.F.);
#46461=ORIENTED_EDGE('',*,*,#35186,.F.);
#46462=ORIENTED_EDGE('',*,*,#35187,.F.);
#46463=ORIENTED_EDGE('',*,*,#35188,.F.);
#46464=ORIENTED_EDGE('',*,*,#35183,.F.);
#46465=ORIENTED_EDGE('',*,*,#35188,.T.);
#46466=ORIENTED_EDGE('',*,*,#35189,.F.);
#46467=ORIENTED_EDGE('',*,*,#34963,.T.);
#46468=ORIENTED_EDGE('',*,*,#35184,.T.);
#46469=ORIENTED_EDGE('',*,*,#35190,.T.);
#46470=ORIENTED_EDGE('',*,*,#35191,.F.);
#46471=ORIENTED_EDGE('',*,*,#34965,.T.);
#46472=ORIENTED_EDGE('',*,*,#35192,.F.);
#46473=ORIENTED_EDGE('',*,*,#35193,.F.);
#46474=ORIENTED_EDGE('',*,*,#35194,.F.);
#46475=ORIENTED_EDGE('',*,*,#35195,.F.);
#46476=ORIENTED_EDGE('',*,*,#35190,.F.);
#46477=ORIENTED_EDGE('',*,*,#35195,.T.);
#46478=ORIENTED_EDGE('',*,*,#35196,.F.);
#46479=ORIENTED_EDGE('',*,*,#34966,.T.);
#46480=ORIENTED_EDGE('',*,*,#35191,.T.);
#46481=ORIENTED_EDGE('',*,*,#34457,.T.);
#46482=ORIENTED_EDGE('',*,*,#35197,.F.);
#46483=ORIENTED_EDGE('',*,*,#34968,.T.);
#46484=ORIENTED_EDGE('',*,*,#35198,.F.);
#46485=ORIENTED_EDGE('',*,*,#34460,.T.);
#46486=ORIENTED_EDGE('',*,*,#35199,.F.);
#46487=ORIENTED_EDGE('',*,*,#34969,.T.);
#46488=ORIENTED_EDGE('',*,*,#35197,.T.);
#46489=ORIENTED_EDGE('',*,*,#35200,.T.);
#46490=ORIENTED_EDGE('',*,*,#35201,.F.);
#46491=ORIENTED_EDGE('',*,*,#34971,.T.);
#46492=ORIENTED_EDGE('',*,*,#35202,.F.);
#46493=ORIENTED_EDGE('',*,*,#35203,.F.);
#46494=ORIENTED_EDGE('',*,*,#35204,.F.);
#46495=ORIENTED_EDGE('',*,*,#35205,.F.);
#46496=ORIENTED_EDGE('',*,*,#35200,.F.);
#46497=ORIENTED_EDGE('',*,*,#35205,.T.);
#46498=ORIENTED_EDGE('',*,*,#35206,.F.);
#46499=ORIENTED_EDGE('',*,*,#34972,.T.);
#46500=ORIENTED_EDGE('',*,*,#35201,.T.);
#46501=ORIENTED_EDGE('',*,*,#35207,.T.);
#46502=ORIENTED_EDGE('',*,*,#35208,.F.);
#46503=ORIENTED_EDGE('',*,*,#34974,.T.);
#46504=ORIENTED_EDGE('',*,*,#35209,.F.);
#46505=ORIENTED_EDGE('',*,*,#35210,.F.);
#46506=ORIENTED_EDGE('',*,*,#35211,.F.);
#46507=ORIENTED_EDGE('',*,*,#35212,.F.);
#46508=ORIENTED_EDGE('',*,*,#35207,.F.);
#46509=ORIENTED_EDGE('',*,*,#35212,.T.);
#46510=ORIENTED_EDGE('',*,*,#35213,.F.);
#46511=ORIENTED_EDGE('',*,*,#34975,.T.);
#46512=ORIENTED_EDGE('',*,*,#35208,.T.);
#46513=ORIENTED_EDGE('',*,*,#35214,.T.);
#46514=ORIENTED_EDGE('',*,*,#35215,.F.);
#46515=ORIENTED_EDGE('',*,*,#34977,.T.);
#46516=ORIENTED_EDGE('',*,*,#35216,.F.);
#46517=ORIENTED_EDGE('',*,*,#35217,.F.);
#46518=ORIENTED_EDGE('',*,*,#35218,.F.);
#46519=ORIENTED_EDGE('',*,*,#35219,.F.);
#46520=ORIENTED_EDGE('',*,*,#35214,.F.);
#46521=ORIENTED_EDGE('',*,*,#35219,.T.);
#46522=ORIENTED_EDGE('',*,*,#35220,.F.);
#46523=ORIENTED_EDGE('',*,*,#34978,.T.);
#46524=ORIENTED_EDGE('',*,*,#35215,.T.);
#46525=ORIENTED_EDGE('',*,*,#35221,.T.);
#46526=ORIENTED_EDGE('',*,*,#35222,.F.);
#46527=ORIENTED_EDGE('',*,*,#34980,.T.);
#46528=ORIENTED_EDGE('',*,*,#35223,.F.);
#46529=ORIENTED_EDGE('',*,*,#35224,.F.);
#46530=ORIENTED_EDGE('',*,*,#35225,.F.);
#46531=ORIENTED_EDGE('',*,*,#35226,.F.);
#46532=ORIENTED_EDGE('',*,*,#35221,.F.);
#46533=ORIENTED_EDGE('',*,*,#35226,.T.);
#46534=ORIENTED_EDGE('',*,*,#35227,.F.);
#46535=ORIENTED_EDGE('',*,*,#34981,.T.);
#46536=ORIENTED_EDGE('',*,*,#35222,.T.);
#46537=ORIENTED_EDGE('',*,*,#35228,.T.);
#46538=ORIENTED_EDGE('',*,*,#35229,.F.);
#46539=ORIENTED_EDGE('',*,*,#34983,.T.);
#46540=ORIENTED_EDGE('',*,*,#35230,.F.);
#46541=ORIENTED_EDGE('',*,*,#35231,.F.);
#46542=ORIENTED_EDGE('',*,*,#35232,.F.);
#46543=ORIENTED_EDGE('',*,*,#35233,.F.);
#46544=ORIENTED_EDGE('',*,*,#35228,.F.);
#46545=ORIENTED_EDGE('',*,*,#35233,.T.);
#46546=ORIENTED_EDGE('',*,*,#35234,.F.);
#46547=ORIENTED_EDGE('',*,*,#34984,.T.);
#46548=ORIENTED_EDGE('',*,*,#35229,.T.);
#46549=ORIENTED_EDGE('',*,*,#35235,.T.);
#46550=ORIENTED_EDGE('',*,*,#35236,.F.);
#46551=ORIENTED_EDGE('',*,*,#34986,.T.);
#46552=ORIENTED_EDGE('',*,*,#35237,.F.);
#46553=ORIENTED_EDGE('',*,*,#35238,.F.);
#46554=ORIENTED_EDGE('',*,*,#35239,.F.);
#46555=ORIENTED_EDGE('',*,*,#35240,.F.);
#46556=ORIENTED_EDGE('',*,*,#35235,.F.);
#46557=ORIENTED_EDGE('',*,*,#35240,.T.);
#46558=ORIENTED_EDGE('',*,*,#35241,.F.);
#46559=ORIENTED_EDGE('',*,*,#34987,.T.);
#46560=ORIENTED_EDGE('',*,*,#35236,.T.);
#46561=ORIENTED_EDGE('',*,*,#35242,.T.);
#46562=ORIENTED_EDGE('',*,*,#35243,.F.);
#46563=ORIENTED_EDGE('',*,*,#34989,.T.);
#46564=ORIENTED_EDGE('',*,*,#35244,.F.);
#46565=ORIENTED_EDGE('',*,*,#35245,.F.);
#46566=ORIENTED_EDGE('',*,*,#35246,.F.);
#46567=ORIENTED_EDGE('',*,*,#35247,.F.);
#46568=ORIENTED_EDGE('',*,*,#35242,.F.);
#46569=ORIENTED_EDGE('',*,*,#35247,.T.);
#46570=ORIENTED_EDGE('',*,*,#35248,.F.);
#46571=ORIENTED_EDGE('',*,*,#34990,.T.);
#46572=ORIENTED_EDGE('',*,*,#35243,.T.);
#46573=ORIENTED_EDGE('',*,*,#35249,.T.);
#46574=ORIENTED_EDGE('',*,*,#35250,.F.);
#46575=ORIENTED_EDGE('',*,*,#34992,.T.);
#46576=ORIENTED_EDGE('',*,*,#35251,.F.);
#46577=ORIENTED_EDGE('',*,*,#35252,.F.);
#46578=ORIENTED_EDGE('',*,*,#35253,.F.);
#46579=ORIENTED_EDGE('',*,*,#35254,.F.);
#46580=ORIENTED_EDGE('',*,*,#35249,.F.);
#46581=ORIENTED_EDGE('',*,*,#35254,.T.);
#46582=ORIENTED_EDGE('',*,*,#35255,.F.);
#46583=ORIENTED_EDGE('',*,*,#34993,.T.);
#46584=ORIENTED_EDGE('',*,*,#35250,.T.);
#46585=ORIENTED_EDGE('',*,*,#35256,.T.);
#46586=ORIENTED_EDGE('',*,*,#35257,.F.);
#46587=ORIENTED_EDGE('',*,*,#34995,.T.);
#46588=ORIENTED_EDGE('',*,*,#35258,.F.);
#46589=ORIENTED_EDGE('',*,*,#35259,.F.);
#46590=ORIENTED_EDGE('',*,*,#35260,.F.);
#46591=ORIENTED_EDGE('',*,*,#35261,.F.);
#46592=ORIENTED_EDGE('',*,*,#35256,.F.);
#46593=ORIENTED_EDGE('',*,*,#35261,.T.);
#46594=ORIENTED_EDGE('',*,*,#35262,.F.);
#46595=ORIENTED_EDGE('',*,*,#34996,.T.);
#46596=ORIENTED_EDGE('',*,*,#35257,.T.);
#46597=ORIENTED_EDGE('',*,*,#35263,.T.);
#46598=ORIENTED_EDGE('',*,*,#35264,.F.);
#46599=ORIENTED_EDGE('',*,*,#34998,.T.);
#46600=ORIENTED_EDGE('',*,*,#35265,.F.);
#46601=ORIENTED_EDGE('',*,*,#35266,.T.);
#46602=ORIENTED_EDGE('',*,*,#35267,.F.);
#46603=ORIENTED_EDGE('',*,*,#34999,.T.);
#46604=ORIENTED_EDGE('',*,*,#35264,.T.);
#46605=ORIENTED_EDGE('',*,*,#35268,.F.);
#46606=ORIENTED_EDGE('',*,*,#35269,.F.);
#46607=ORIENTED_EDGE('',*,*,#35266,.F.);
#46608=ORIENTED_EDGE('',*,*,#35263,.F.);
#46609=ORIENTED_EDGE('',*,*,#35001,.T.);
#46610=ORIENTED_EDGE('',*,*,#35270,.F.);
#46611=ORIENTED_EDGE('',*,*,#35271,.T.);
#46612=ORIENTED_EDGE('',*,*,#35272,.F.);
#46613=ORIENTED_EDGE('',*,*,#35273,.F.);
#46614=ORIENTED_EDGE('',*,*,#35271,.F.);
#46615=ORIENTED_EDGE('',*,*,#35274,.F.);
#46616=ORIENTED_EDGE('',*,*,#35275,.F.);
#46617=ORIENTED_EDGE('',*,*,#35002,.T.);
#46618=ORIENTED_EDGE('',*,*,#35272,.T.);
#46619=ORIENTED_EDGE('',*,*,#35273,.T.);
#46620=ORIENTED_EDGE('',*,*,#35276,.F.);
#46621=ORIENTED_EDGE('',*,*,#35277,.T.);
#46622=ORIENTED_EDGE('',*,*,#35278,.F.);
#46623=ORIENTED_EDGE('',*,*,#35004,.T.);
#46624=ORIENTED_EDGE('',*,*,#35279,.F.);
#46625=ORIENTED_EDGE('',*,*,#35280,.F.);
#46626=ORIENTED_EDGE('',*,*,#35281,.F.);
#46627=ORIENTED_EDGE('',*,*,#35282,.F.);
#46628=ORIENTED_EDGE('',*,*,#35277,.F.);
#46629=ORIENTED_EDGE('',*,*,#35282,.T.);
#46630=ORIENTED_EDGE('',*,*,#35283,.F.);
#46631=ORIENTED_EDGE('',*,*,#35005,.T.);
#46632=ORIENTED_EDGE('',*,*,#35278,.T.);
#46633=ORIENTED_EDGE('',*,*,#35284,.T.);
#46634=ORIENTED_EDGE('',*,*,#35285,.F.);
#46635=ORIENTED_EDGE('',*,*,#35007,.T.);
#46636=ORIENTED_EDGE('',*,*,#35286,.F.);
#46637=ORIENTED_EDGE('',*,*,#35287,.F.);
#46638=ORIENTED_EDGE('',*,*,#35288,.F.);
#46639=ORIENTED_EDGE('',*,*,#35289,.F.);
#46640=ORIENTED_EDGE('',*,*,#35284,.F.);
#46641=ORIENTED_EDGE('',*,*,#35289,.T.);
#46642=ORIENTED_EDGE('',*,*,#35290,.F.);
#46643=ORIENTED_EDGE('',*,*,#35008,.T.);
#46644=ORIENTED_EDGE('',*,*,#35285,.T.);
#46645=ORIENTED_EDGE('',*,*,#35291,.T.);
#46646=ORIENTED_EDGE('',*,*,#35292,.F.);
#46647=ORIENTED_EDGE('',*,*,#35010,.T.);
#46648=ORIENTED_EDGE('',*,*,#35293,.F.);
#46649=ORIENTED_EDGE('',*,*,#35294,.F.);
#46650=ORIENTED_EDGE('',*,*,#35295,.F.);
#46651=ORIENTED_EDGE('',*,*,#35296,.F.);
#46652=ORIENTED_EDGE('',*,*,#35291,.F.);
#46653=ORIENTED_EDGE('',*,*,#35296,.T.);
#46654=ORIENTED_EDGE('',*,*,#35297,.F.);
#46655=ORIENTED_EDGE('',*,*,#35011,.T.);
#46656=ORIENTED_EDGE('',*,*,#35292,.T.);
#46657=ORIENTED_EDGE('',*,*,#35013,.T.);
#46658=ORIENTED_EDGE('',*,*,#35298,.F.);
#46659=ORIENTED_EDGE('',*,*,#35299,.T.);
#46660=ORIENTED_EDGE('',*,*,#35300,.F.);
#46661=ORIENTED_EDGE('',*,*,#35014,.T.);
#46662=ORIENTED_EDGE('',*,*,#35300,.T.);
#46663=ORIENTED_EDGE('',*,*,#35301,.T.);
#46664=ORIENTED_EDGE('',*,*,#35302,.F.);
#46665=ORIENTED_EDGE('',*,*,#35301,.F.);
#46666=ORIENTED_EDGE('',*,*,#35299,.F.);
#46667=ORIENTED_EDGE('',*,*,#35303,.F.);
#46668=ORIENTED_EDGE('',*,*,#35304,.F.);
#46669=ORIENTED_EDGE('',*,*,#35016,.T.);
#46670=ORIENTED_EDGE('',*,*,#35305,.F.);
#46671=ORIENTED_EDGE('',*,*,#35306,.T.);
#46672=ORIENTED_EDGE('',*,*,#35307,.F.);
#46673=ORIENTED_EDGE('',*,*,#35308,.T.);
#46674=ORIENTED_EDGE('',*,*,#35309,.F.);
#46675=ORIENTED_EDGE('',*,*,#35017,.T.);
#46676=ORIENTED_EDGE('',*,*,#35307,.T.);
#46677=ORIENTED_EDGE('',*,*,#35310,.F.);
#46678=ORIENTED_EDGE('',*,*,#35311,.F.);
#46679=ORIENTED_EDGE('',*,*,#35308,.F.);
#46680=ORIENTED_EDGE('',*,*,#35306,.F.);
#46681=ORIENTED_EDGE('',*,*,#35019,.T.);
#46682=ORIENTED_EDGE('',*,*,#35312,.F.);
#46683=ORIENTED_EDGE('',*,*,#35313,.T.);
#46684=ORIENTED_EDGE('',*,*,#35314,.F.);
#46685=ORIENTED_EDGE('',*,*,#35020,.T.);
#46686=ORIENTED_EDGE('',*,*,#35314,.T.);
#46687=ORIENTED_EDGE('',*,*,#35315,.T.);
#46688=ORIENTED_EDGE('',*,*,#35316,.F.);
#46689=ORIENTED_EDGE('',*,*,#35315,.F.);
#46690=ORIENTED_EDGE('',*,*,#35313,.F.);
#46691=ORIENTED_EDGE('',*,*,#35317,.F.);
#46692=ORIENTED_EDGE('',*,*,#35318,.F.);
#46693=ORIENTED_EDGE('',*,*,#35022,.T.);
#46694=ORIENTED_EDGE('',*,*,#35319,.F.);
#46695=ORIENTED_EDGE('',*,*,#35320,.T.);
#46696=ORIENTED_EDGE('',*,*,#35321,.F.);
#46697=ORIENTED_EDGE('',*,*,#35023,.T.);
#46698=ORIENTED_EDGE('',*,*,#35321,.T.);
#46699=ORIENTED_EDGE('',*,*,#35322,.T.);
#46700=ORIENTED_EDGE('',*,*,#35323,.F.);
#46701=ORIENTED_EDGE('',*,*,#35322,.F.);
#46702=ORIENTED_EDGE('',*,*,#35320,.F.);
#46703=ORIENTED_EDGE('',*,*,#35324,.F.);
#46704=ORIENTED_EDGE('',*,*,#35325,.F.);
#46705=ORIENTED_EDGE('',*,*,#35025,.T.);
#46706=ORIENTED_EDGE('',*,*,#35326,.F.);
#46707=ORIENTED_EDGE('',*,*,#35327,.T.);
#46708=ORIENTED_EDGE('',*,*,#35328,.F.);
#46709=ORIENTED_EDGE('',*,*,#35026,.T.);
#46710=ORIENTED_EDGE('',*,*,#35328,.T.);
#46711=ORIENTED_EDGE('',*,*,#35329,.T.);
#46712=ORIENTED_EDGE('',*,*,#35330,.F.);
#46713=ORIENTED_EDGE('',*,*,#35329,.F.);
#46714=ORIENTED_EDGE('',*,*,#35327,.F.);
#46715=ORIENTED_EDGE('',*,*,#35331,.F.);
#46716=ORIENTED_EDGE('',*,*,#35332,.F.);
#46717=ORIENTED_EDGE('',*,*,#35028,.T.);
#46718=ORIENTED_EDGE('',*,*,#35333,.F.);
#46719=ORIENTED_EDGE('',*,*,#35334,.T.);
#46720=ORIENTED_EDGE('',*,*,#35335,.F.);
#46721=ORIENTED_EDGE('',*,*,#35029,.T.);
#46722=ORIENTED_EDGE('',*,*,#35335,.T.);
#46723=ORIENTED_EDGE('',*,*,#35336,.T.);
#46724=ORIENTED_EDGE('',*,*,#35337,.F.);
#46725=ORIENTED_EDGE('',*,*,#35336,.F.);
#46726=ORIENTED_EDGE('',*,*,#35334,.F.);
#46727=ORIENTED_EDGE('',*,*,#35338,.F.);
#46728=ORIENTED_EDGE('',*,*,#35339,.F.);
#46729=ORIENTED_EDGE('',*,*,#35031,.T.);
#46730=ORIENTED_EDGE('',*,*,#35340,.F.);
#46731=ORIENTED_EDGE('',*,*,#35341,.T.);
#46732=ORIENTED_EDGE('',*,*,#35342,.F.);
#46733=ORIENTED_EDGE('',*,*,#35032,.T.);
#46734=ORIENTED_EDGE('',*,*,#35342,.T.);
#46735=ORIENTED_EDGE('',*,*,#35343,.T.);
#46736=ORIENTED_EDGE('',*,*,#35344,.F.);
#46737=ORIENTED_EDGE('',*,*,#35343,.F.);
#46738=ORIENTED_EDGE('',*,*,#35341,.F.);
#46739=ORIENTED_EDGE('',*,*,#35345,.F.);
#46740=ORIENTED_EDGE('',*,*,#35346,.F.);
#46741=ORIENTED_EDGE('',*,*,#35034,.T.);
#46742=ORIENTED_EDGE('',*,*,#35347,.F.);
#46743=ORIENTED_EDGE('',*,*,#35348,.T.);
#46744=ORIENTED_EDGE('',*,*,#35349,.F.);
#46745=ORIENTED_EDGE('',*,*,#35035,.T.);
#46746=ORIENTED_EDGE('',*,*,#35349,.T.);
#46747=ORIENTED_EDGE('',*,*,#35350,.T.);
#46748=ORIENTED_EDGE('',*,*,#35351,.F.);
#46749=ORIENTED_EDGE('',*,*,#35350,.F.);
#46750=ORIENTED_EDGE('',*,*,#35348,.F.);
#46751=ORIENTED_EDGE('',*,*,#35352,.F.);
#46752=ORIENTED_EDGE('',*,*,#35353,.F.);
#46753=ORIENTED_EDGE('',*,*,#35037,.T.);
#46754=ORIENTED_EDGE('',*,*,#35354,.F.);
#46755=ORIENTED_EDGE('',*,*,#35355,.T.);
#46756=ORIENTED_EDGE('',*,*,#35356,.F.);
#46757=ORIENTED_EDGE('',*,*,#35038,.T.);
#46758=ORIENTED_EDGE('',*,*,#35356,.T.);
#46759=ORIENTED_EDGE('',*,*,#35357,.T.);
#46760=ORIENTED_EDGE('',*,*,#35358,.F.);
#46761=ORIENTED_EDGE('',*,*,#35357,.F.);
#46762=ORIENTED_EDGE('',*,*,#35355,.F.);
#46763=ORIENTED_EDGE('',*,*,#35359,.F.);
#46764=ORIENTED_EDGE('',*,*,#35360,.F.);
#46765=ORIENTED_EDGE('',*,*,#35040,.T.);
#46766=ORIENTED_EDGE('',*,*,#35361,.F.);
#46767=ORIENTED_EDGE('',*,*,#35362,.T.);
#46768=ORIENTED_EDGE('',*,*,#35363,.F.);
#46769=ORIENTED_EDGE('',*,*,#35041,.T.);
#46770=ORIENTED_EDGE('',*,*,#35363,.T.);
#46771=ORIENTED_EDGE('',*,*,#35364,.T.);
#46772=ORIENTED_EDGE('',*,*,#35365,.F.);
#46773=ORIENTED_EDGE('',*,*,#35364,.F.);
#46774=ORIENTED_EDGE('',*,*,#35362,.F.);
#46775=ORIENTED_EDGE('',*,*,#35366,.F.);
#46776=ORIENTED_EDGE('',*,*,#35367,.F.);
#46777=ORIENTED_EDGE('',*,*,#35043,.T.);
#46778=ORIENTED_EDGE('',*,*,#35368,.F.);
#46779=ORIENTED_EDGE('',*,*,#35369,.T.);
#46780=ORIENTED_EDGE('',*,*,#35370,.F.);
#46781=ORIENTED_EDGE('',*,*,#35044,.T.);
#46782=ORIENTED_EDGE('',*,*,#35370,.T.);
#46783=ORIENTED_EDGE('',*,*,#35371,.T.);
#46784=ORIENTED_EDGE('',*,*,#35372,.F.);
#46785=ORIENTED_EDGE('',*,*,#35371,.F.);
#46786=ORIENTED_EDGE('',*,*,#35369,.F.);
#46787=ORIENTED_EDGE('',*,*,#35373,.F.);
#46788=ORIENTED_EDGE('',*,*,#35374,.F.);
#46789=ORIENTED_EDGE('',*,*,#35046,.T.);
#46790=ORIENTED_EDGE('',*,*,#35375,.F.);
#46791=ORIENTED_EDGE('',*,*,#35376,.T.);
#46792=ORIENTED_EDGE('',*,*,#35377,.F.);
#46793=ORIENTED_EDGE('',*,*,#35047,.T.);
#46794=ORIENTED_EDGE('',*,*,#35377,.T.);
#46795=ORIENTED_EDGE('',*,*,#35378,.T.);
#46796=ORIENTED_EDGE('',*,*,#35379,.F.);
#46797=ORIENTED_EDGE('',*,*,#35378,.F.);
#46798=ORIENTED_EDGE('',*,*,#35376,.F.);
#46799=ORIENTED_EDGE('',*,*,#35380,.F.);
#46800=ORIENTED_EDGE('',*,*,#35381,.F.);
#46801=ORIENTED_EDGE('',*,*,#35049,.T.);
#46802=ORIENTED_EDGE('',*,*,#35382,.F.);
#46803=ORIENTED_EDGE('',*,*,#35383,.T.);
#46804=ORIENTED_EDGE('',*,*,#35384,.F.);
#46805=ORIENTED_EDGE('',*,*,#35050,.T.);
#46806=ORIENTED_EDGE('',*,*,#35384,.T.);
#46807=ORIENTED_EDGE('',*,*,#35385,.T.);
#46808=ORIENTED_EDGE('',*,*,#35386,.F.);
#46809=ORIENTED_EDGE('',*,*,#35385,.F.);
#46810=ORIENTED_EDGE('',*,*,#35383,.F.);
#46811=ORIENTED_EDGE('',*,*,#35387,.F.);
#46812=ORIENTED_EDGE('',*,*,#35388,.F.);
#46813=ORIENTED_EDGE('',*,*,#35052,.T.);
#46814=ORIENTED_EDGE('',*,*,#35389,.F.);
#46815=ORIENTED_EDGE('',*,*,#35390,.T.);
#46816=ORIENTED_EDGE('',*,*,#35391,.F.);
#46817=ORIENTED_EDGE('',*,*,#35053,.T.);
#46818=ORIENTED_EDGE('',*,*,#35391,.T.);
#46819=ORIENTED_EDGE('',*,*,#35392,.T.);
#46820=ORIENTED_EDGE('',*,*,#35393,.F.);
#46821=ORIENTED_EDGE('',*,*,#35392,.F.);
#46822=ORIENTED_EDGE('',*,*,#35390,.F.);
#46823=ORIENTED_EDGE('',*,*,#35394,.F.);
#46824=ORIENTED_EDGE('',*,*,#35395,.F.);
#46825=ORIENTED_EDGE('',*,*,#35055,.T.);
#46826=ORIENTED_EDGE('',*,*,#35396,.F.);
#46827=ORIENTED_EDGE('',*,*,#35397,.T.);
#46828=ORIENTED_EDGE('',*,*,#35398,.F.);
#46829=ORIENTED_EDGE('',*,*,#35056,.T.);
#46830=ORIENTED_EDGE('',*,*,#35398,.T.);
#46831=ORIENTED_EDGE('',*,*,#35399,.T.);
#46832=ORIENTED_EDGE('',*,*,#35400,.F.);
#46833=ORIENTED_EDGE('',*,*,#35399,.F.);
#46834=ORIENTED_EDGE('',*,*,#35397,.F.);
#46835=ORIENTED_EDGE('',*,*,#35401,.F.);
#46836=ORIENTED_EDGE('',*,*,#35402,.F.);
#46837=ORIENTED_EDGE('',*,*,#35058,.T.);
#46838=ORIENTED_EDGE('',*,*,#35403,.F.);
#46839=ORIENTED_EDGE('',*,*,#35404,.T.);
#46840=ORIENTED_EDGE('',*,*,#35405,.F.);
#46841=ORIENTED_EDGE('',*,*,#35059,.T.);
#46842=ORIENTED_EDGE('',*,*,#35405,.T.);
#46843=ORIENTED_EDGE('',*,*,#35406,.T.);
#46844=ORIENTED_EDGE('',*,*,#35407,.F.);
#46845=ORIENTED_EDGE('',*,*,#35406,.F.);
#46846=ORIENTED_EDGE('',*,*,#35404,.F.);
#46847=ORIENTED_EDGE('',*,*,#35408,.F.);
#46848=ORIENTED_EDGE('',*,*,#35409,.F.);
#46849=ORIENTED_EDGE('',*,*,#35061,.T.);
#46850=ORIENTED_EDGE('',*,*,#35410,.F.);
#46851=ORIENTED_EDGE('',*,*,#35411,.T.);
#46852=ORIENTED_EDGE('',*,*,#35412,.F.);
#46853=ORIENTED_EDGE('',*,*,#35062,.T.);
#46854=ORIENTED_EDGE('',*,*,#35412,.T.);
#46855=ORIENTED_EDGE('',*,*,#35413,.T.);
#46856=ORIENTED_EDGE('',*,*,#35414,.F.);
#46857=ORIENTED_EDGE('',*,*,#35413,.F.);
#46858=ORIENTED_EDGE('',*,*,#35411,.F.);
#46859=ORIENTED_EDGE('',*,*,#35415,.F.);
#46860=ORIENTED_EDGE('',*,*,#35416,.F.);
#46861=ORIENTED_EDGE('',*,*,#35064,.T.);
#46862=ORIENTED_EDGE('',*,*,#35417,.F.);
#46863=ORIENTED_EDGE('',*,*,#35418,.T.);
#46864=ORIENTED_EDGE('',*,*,#35419,.F.);
#46865=ORIENTED_EDGE('',*,*,#35065,.T.);
#46866=ORIENTED_EDGE('',*,*,#35419,.T.);
#46867=ORIENTED_EDGE('',*,*,#35420,.T.);
#46868=ORIENTED_EDGE('',*,*,#35421,.F.);
#46869=ORIENTED_EDGE('',*,*,#35420,.F.);
#46870=ORIENTED_EDGE('',*,*,#35418,.F.);
#46871=ORIENTED_EDGE('',*,*,#35422,.F.);
#46872=ORIENTED_EDGE('',*,*,#35423,.F.);
#46873=ORIENTED_EDGE('',*,*,#35067,.T.);
#46874=ORIENTED_EDGE('',*,*,#35424,.F.);
#46875=ORIENTED_EDGE('',*,*,#35425,.T.);
#46876=ORIENTED_EDGE('',*,*,#35426,.F.);
#46877=ORIENTED_EDGE('',*,*,#35068,.T.);
#46878=ORIENTED_EDGE('',*,*,#35426,.T.);
#46879=ORIENTED_EDGE('',*,*,#35427,.T.);
#46880=ORIENTED_EDGE('',*,*,#35428,.F.);
#46881=ORIENTED_EDGE('',*,*,#35427,.F.);
#46882=ORIENTED_EDGE('',*,*,#35425,.F.);
#46883=ORIENTED_EDGE('',*,*,#35429,.F.);
#46884=ORIENTED_EDGE('',*,*,#35430,.F.);
#46885=ORIENTED_EDGE('',*,*,#35070,.T.);
#46886=ORIENTED_EDGE('',*,*,#35431,.F.);
#46887=ORIENTED_EDGE('',*,*,#35432,.T.);
#46888=ORIENTED_EDGE('',*,*,#35433,.F.);
#46889=ORIENTED_EDGE('',*,*,#35071,.T.);
#46890=ORIENTED_EDGE('',*,*,#35433,.T.);
#46891=ORIENTED_EDGE('',*,*,#35434,.T.);
#46892=ORIENTED_EDGE('',*,*,#35435,.F.);
#46893=ORIENTED_EDGE('',*,*,#35434,.F.);
#46894=ORIENTED_EDGE('',*,*,#35432,.F.);
#46895=ORIENTED_EDGE('',*,*,#35436,.F.);
#46896=ORIENTED_EDGE('',*,*,#35437,.F.);
#46897=ORIENTED_EDGE('',*,*,#35073,.T.);
#46898=ORIENTED_EDGE('',*,*,#35438,.F.);
#46899=ORIENTED_EDGE('',*,*,#35439,.T.);
#46900=ORIENTED_EDGE('',*,*,#35440,.F.);
#46901=ORIENTED_EDGE('',*,*,#35074,.T.);
#46902=ORIENTED_EDGE('',*,*,#35440,.T.);
#46903=ORIENTED_EDGE('',*,*,#35441,.T.);
#46904=ORIENTED_EDGE('',*,*,#35442,.F.);
#46905=ORIENTED_EDGE('',*,*,#35441,.F.);
#46906=ORIENTED_EDGE('',*,*,#35439,.F.);
#46907=ORIENTED_EDGE('',*,*,#35443,.F.);
#46908=ORIENTED_EDGE('',*,*,#35444,.F.);
#46909=ORIENTED_EDGE('',*,*,#35076,.T.);
#46910=ORIENTED_EDGE('',*,*,#35445,.F.);
#46911=ORIENTED_EDGE('',*,*,#34456,.T.);
#46912=ORIENTED_EDGE('',*,*,#35446,.F.);
#46913=ORIENTED_EDGE('',*,*,#35077,.T.);
#46914=ORIENTED_EDGE('',*,*,#35446,.T.);
#46915=ORIENTED_EDGE('',*,*,#34455,.T.);
#46916=ORIENTED_EDGE('',*,*,#35447,.F.);
#46917=ORIENTED_EDGE('',*,*,#35079,.T.);
#46918=ORIENTED_EDGE('',*,*,#35448,.F.);
#46919=ORIENTED_EDGE('',*,*,#35449,.T.);
#46920=ORIENTED_EDGE('',*,*,#35450,.F.);
#46921=ORIENTED_EDGE('',*,*,#35080,.T.);
#46922=ORIENTED_EDGE('',*,*,#35450,.T.);
#46923=ORIENTED_EDGE('',*,*,#35451,.T.);
#46924=ORIENTED_EDGE('',*,*,#35452,.F.);
#46925=ORIENTED_EDGE('',*,*,#35451,.F.);
#46926=ORIENTED_EDGE('',*,*,#35449,.F.);
#46927=ORIENTED_EDGE('',*,*,#35453,.F.);
#46928=ORIENTED_EDGE('',*,*,#35454,.F.);
#46929=ORIENTED_EDGE('',*,*,#35082,.T.);
#46930=ORIENTED_EDGE('',*,*,#35455,.F.);
#46931=ORIENTED_EDGE('',*,*,#35456,.T.);
#46932=ORIENTED_EDGE('',*,*,#35457,.F.);
#46933=ORIENTED_EDGE('',*,*,#35083,.T.);
#46934=ORIENTED_EDGE('',*,*,#35457,.T.);
#46935=ORIENTED_EDGE('',*,*,#35458,.T.);
#46936=ORIENTED_EDGE('',*,*,#35459,.F.);
#46937=ORIENTED_EDGE('',*,*,#35458,.F.);
#46938=ORIENTED_EDGE('',*,*,#35456,.F.);
#46939=ORIENTED_EDGE('',*,*,#35460,.F.);
#46940=ORIENTED_EDGE('',*,*,#35461,.F.);
#46941=ORIENTED_EDGE('',*,*,#35085,.T.);
#46942=ORIENTED_EDGE('',*,*,#35462,.F.);
#46943=ORIENTED_EDGE('',*,*,#35463,.T.);
#46944=ORIENTED_EDGE('',*,*,#35464,.F.);
#46945=ORIENTED_EDGE('',*,*,#35086,.T.);
#46946=ORIENTED_EDGE('',*,*,#35464,.T.);
#46947=ORIENTED_EDGE('',*,*,#35465,.T.);
#46948=ORIENTED_EDGE('',*,*,#35466,.F.);
#46949=ORIENTED_EDGE('',*,*,#35465,.F.);
#46950=ORIENTED_EDGE('',*,*,#35463,.F.);
#46951=ORIENTED_EDGE('',*,*,#35467,.F.);
#46952=ORIENTED_EDGE('',*,*,#35468,.F.);
#46953=ORIENTED_EDGE('',*,*,#35088,.T.);
#46954=ORIENTED_EDGE('',*,*,#35469,.F.);
#46955=ORIENTED_EDGE('',*,*,#35470,.T.);
#46956=ORIENTED_EDGE('',*,*,#35471,.F.);
#46957=ORIENTED_EDGE('',*,*,#35089,.T.);
#46958=ORIENTED_EDGE('',*,*,#35471,.T.);
#46959=ORIENTED_EDGE('',*,*,#35472,.T.);
#46960=ORIENTED_EDGE('',*,*,#35473,.F.);
#46961=ORIENTED_EDGE('',*,*,#35472,.F.);
#46962=ORIENTED_EDGE('',*,*,#35470,.F.);
#46963=ORIENTED_EDGE('',*,*,#35474,.F.);
#46964=ORIENTED_EDGE('',*,*,#35475,.F.);
#46965=ORIENTED_EDGE('',*,*,#35091,.T.);
#46966=ORIENTED_EDGE('',*,*,#35476,.F.);
#46967=ORIENTED_EDGE('',*,*,#35477,.T.);
#46968=ORIENTED_EDGE('',*,*,#35478,.F.);
#46969=ORIENTED_EDGE('',*,*,#35092,.T.);
#46970=ORIENTED_EDGE('',*,*,#35478,.T.);
#46971=ORIENTED_EDGE('',*,*,#35479,.T.);
#46972=ORIENTED_EDGE('',*,*,#35480,.F.);
#46973=ORIENTED_EDGE('',*,*,#35479,.F.);
#46974=ORIENTED_EDGE('',*,*,#35477,.F.);
#46975=ORIENTED_EDGE('',*,*,#35481,.F.);
#46976=ORIENTED_EDGE('',*,*,#35482,.F.);
#46977=ORIENTED_EDGE('',*,*,#35094,.T.);
#46978=ORIENTED_EDGE('',*,*,#35483,.F.);
#46979=ORIENTED_EDGE('',*,*,#35484,.T.);
#46980=ORIENTED_EDGE('',*,*,#35485,.F.);
#46981=ORIENTED_EDGE('',*,*,#35095,.T.);
#46982=ORIENTED_EDGE('',*,*,#35485,.T.);
#46983=ORIENTED_EDGE('',*,*,#35486,.T.);
#46984=ORIENTED_EDGE('',*,*,#35487,.F.);
#46985=ORIENTED_EDGE('',*,*,#35486,.F.);
#46986=ORIENTED_EDGE('',*,*,#35484,.F.);
#46987=ORIENTED_EDGE('',*,*,#35488,.F.);
#46988=ORIENTED_EDGE('',*,*,#35489,.F.);
#46989=ORIENTED_EDGE('',*,*,#35097,.T.);
#46990=ORIENTED_EDGE('',*,*,#35490,.F.);
#46991=ORIENTED_EDGE('',*,*,#35491,.T.);
#46992=ORIENTED_EDGE('',*,*,#35492,.F.);
#46993=ORIENTED_EDGE('',*,*,#35098,.T.);
#46994=ORIENTED_EDGE('',*,*,#35492,.T.);
#46995=ORIENTED_EDGE('',*,*,#35493,.T.);
#46996=ORIENTED_EDGE('',*,*,#35494,.F.);
#46997=ORIENTED_EDGE('',*,*,#35493,.F.);
#46998=ORIENTED_EDGE('',*,*,#35491,.F.);
#46999=ORIENTED_EDGE('',*,*,#35495,.F.);
#47000=ORIENTED_EDGE('',*,*,#35496,.F.);
#47001=ORIENTED_EDGE('',*,*,#35497,.F.);
#47002=ORIENTED_EDGE('',*,*,#35498,.F.);
#47003=ORIENTED_EDGE('',*,*,#35102,.T.);
#47004=ORIENTED_EDGE('',*,*,#35101,.T.);
#47005=ORIENTED_EDGE('',*,*,#35499,.F.);
#47006=ORIENTED_EDGE('',*,*,#35105,.T.);
#47007=ORIENTED_EDGE('',*,*,#35103,.T.);
#47008=ORIENTED_EDGE('',*,*,#35498,.T.);
#47009=ORIENTED_EDGE('',*,*,#35500,.F.);
#47010=ORIENTED_EDGE('',*,*,#35501,.F.);
#47011=ORIENTED_EDGE('',*,*,#35109,.T.);
#47012=ORIENTED_EDGE('',*,*,#35108,.T.);
#47013=ORIENTED_EDGE('',*,*,#35502,.F.);
#47014=ORIENTED_EDGE('',*,*,#35112,.T.);
#47015=ORIENTED_EDGE('',*,*,#35110,.T.);
#47016=ORIENTED_EDGE('',*,*,#35501,.T.);
#47017=ORIENTED_EDGE('',*,*,#35503,.F.);
#47018=ORIENTED_EDGE('',*,*,#35504,.F.);
#47019=ORIENTED_EDGE('',*,*,#35116,.T.);
#47020=ORIENTED_EDGE('',*,*,#35115,.T.);
#47021=ORIENTED_EDGE('',*,*,#35505,.F.);
#47022=ORIENTED_EDGE('',*,*,#35119,.T.);
#47023=ORIENTED_EDGE('',*,*,#35117,.T.);
#47024=ORIENTED_EDGE('',*,*,#35504,.T.);
#47025=ORIENTED_EDGE('',*,*,#35506,.F.);
#47026=ORIENTED_EDGE('',*,*,#35507,.F.);
#47027=ORIENTED_EDGE('',*,*,#35123,.T.);
#47028=ORIENTED_EDGE('',*,*,#35122,.T.);
#47029=ORIENTED_EDGE('',*,*,#35508,.F.);
#47030=ORIENTED_EDGE('',*,*,#35126,.T.);
#47031=ORIENTED_EDGE('',*,*,#35124,.T.);
#47032=ORIENTED_EDGE('',*,*,#35507,.T.);
#47033=ORIENTED_EDGE('',*,*,#35509,.F.);
#47034=ORIENTED_EDGE('',*,*,#35510,.F.);
#47035=ORIENTED_EDGE('',*,*,#35130,.T.);
#47036=ORIENTED_EDGE('',*,*,#35129,.T.);
#47037=ORIENTED_EDGE('',*,*,#35511,.F.);
#47038=ORIENTED_EDGE('',*,*,#35133,.T.);
#47039=ORIENTED_EDGE('',*,*,#35131,.T.);
#47040=ORIENTED_EDGE('',*,*,#35510,.T.);
#47041=ORIENTED_EDGE('',*,*,#35512,.F.);
#47042=ORIENTED_EDGE('',*,*,#35513,.F.);
#47043=ORIENTED_EDGE('',*,*,#35137,.T.);
#47044=ORIENTED_EDGE('',*,*,#35136,.T.);
#47045=ORIENTED_EDGE('',*,*,#35514,.F.);
#47046=ORIENTED_EDGE('',*,*,#35140,.T.);
#47047=ORIENTED_EDGE('',*,*,#35138,.T.);
#47048=ORIENTED_EDGE('',*,*,#35513,.T.);
#47049=ORIENTED_EDGE('',*,*,#35515,.F.);
#47050=ORIENTED_EDGE('',*,*,#35516,.F.);
#47051=ORIENTED_EDGE('',*,*,#35144,.T.);
#47052=ORIENTED_EDGE('',*,*,#35143,.T.);
#47053=ORIENTED_EDGE('',*,*,#35517,.F.);
#47054=ORIENTED_EDGE('',*,*,#35147,.T.);
#47055=ORIENTED_EDGE('',*,*,#35145,.T.);
#47056=ORIENTED_EDGE('',*,*,#35516,.T.);
#47057=ORIENTED_EDGE('',*,*,#35518,.F.);
#47058=ORIENTED_EDGE('',*,*,#35519,.F.);
#47059=ORIENTED_EDGE('',*,*,#35151,.T.);
#47060=ORIENTED_EDGE('',*,*,#35150,.T.);
#47061=ORIENTED_EDGE('',*,*,#35520,.F.);
#47062=ORIENTED_EDGE('',*,*,#35154,.T.);
#47063=ORIENTED_EDGE('',*,*,#35152,.T.);
#47064=ORIENTED_EDGE('',*,*,#35519,.T.);
#47065=ORIENTED_EDGE('',*,*,#35521,.F.);
#47066=ORIENTED_EDGE('',*,*,#35522,.F.);
#47067=ORIENTED_EDGE('',*,*,#35158,.T.);
#47068=ORIENTED_EDGE('',*,*,#35157,.T.);
#47069=ORIENTED_EDGE('',*,*,#35523,.F.);
#47070=ORIENTED_EDGE('',*,*,#35161,.T.);
#47071=ORIENTED_EDGE('',*,*,#35159,.T.);
#47072=ORIENTED_EDGE('',*,*,#35522,.T.);
#47073=ORIENTED_EDGE('',*,*,#35524,.F.);
#47074=ORIENTED_EDGE('',*,*,#35525,.F.);
#47075=ORIENTED_EDGE('',*,*,#35165,.T.);
#47076=ORIENTED_EDGE('',*,*,#35164,.T.);
#47077=ORIENTED_EDGE('',*,*,#35526,.F.);
#47078=ORIENTED_EDGE('',*,*,#35168,.T.);
#47079=ORIENTED_EDGE('',*,*,#35166,.T.);
#47080=ORIENTED_EDGE('',*,*,#35525,.T.);
#47081=ORIENTED_EDGE('',*,*,#35527,.F.);
#47082=ORIENTED_EDGE('',*,*,#35528,.F.);
#47083=ORIENTED_EDGE('',*,*,#35172,.T.);
#47084=ORIENTED_EDGE('',*,*,#35171,.T.);
#47085=ORIENTED_EDGE('',*,*,#35529,.F.);
#47086=ORIENTED_EDGE('',*,*,#35175,.T.);
#47087=ORIENTED_EDGE('',*,*,#35173,.T.);
#47088=ORIENTED_EDGE('',*,*,#35528,.T.);
#47089=ORIENTED_EDGE('',*,*,#35530,.F.);
#47090=ORIENTED_EDGE('',*,*,#35531,.F.);
#47091=ORIENTED_EDGE('',*,*,#35179,.T.);
#47092=ORIENTED_EDGE('',*,*,#35178,.T.);
#47093=ORIENTED_EDGE('',*,*,#35532,.F.);
#47094=ORIENTED_EDGE('',*,*,#35182,.T.);
#47095=ORIENTED_EDGE('',*,*,#35180,.T.);
#47096=ORIENTED_EDGE('',*,*,#35531,.T.);
#47097=ORIENTED_EDGE('',*,*,#35533,.F.);
#47098=ORIENTED_EDGE('',*,*,#35534,.F.);
#47099=ORIENTED_EDGE('',*,*,#35186,.T.);
#47100=ORIENTED_EDGE('',*,*,#35185,.T.);
#47101=ORIENTED_EDGE('',*,*,#35535,.F.);
#47102=ORIENTED_EDGE('',*,*,#35189,.T.);
#47103=ORIENTED_EDGE('',*,*,#35187,.T.);
#47104=ORIENTED_EDGE('',*,*,#35534,.T.);
#47105=ORIENTED_EDGE('',*,*,#35536,.F.);
#47106=ORIENTED_EDGE('',*,*,#35537,.F.);
#47107=ORIENTED_EDGE('',*,*,#35193,.T.);
#47108=ORIENTED_EDGE('',*,*,#35192,.T.);
#47109=ORIENTED_EDGE('',*,*,#35538,.F.);
#47110=ORIENTED_EDGE('',*,*,#35196,.T.);
#47111=ORIENTED_EDGE('',*,*,#35194,.T.);
#47112=ORIENTED_EDGE('',*,*,#35537,.T.);
#47113=ORIENTED_EDGE('',*,*,#35539,.F.);
#47114=ORIENTED_EDGE('',*,*,#35540,.F.);
#47115=ORIENTED_EDGE('',*,*,#34458,.T.);
#47116=ORIENTED_EDGE('',*,*,#35198,.T.);
#47117=ORIENTED_EDGE('',*,*,#35541,.F.);
#47118=ORIENTED_EDGE('',*,*,#35199,.T.);
#47119=ORIENTED_EDGE('',*,*,#34459,.T.);
#47120=ORIENTED_EDGE('',*,*,#35540,.T.);
#47121=ORIENTED_EDGE('',*,*,#35542,.F.);
#47122=ORIENTED_EDGE('',*,*,#35543,.F.);
#47123=ORIENTED_EDGE('',*,*,#35203,.T.);
#47124=ORIENTED_EDGE('',*,*,#35202,.T.);
#47125=ORIENTED_EDGE('',*,*,#35544,.F.);
#47126=ORIENTED_EDGE('',*,*,#35206,.T.);
#47127=ORIENTED_EDGE('',*,*,#35204,.T.);
#47128=ORIENTED_EDGE('',*,*,#35543,.T.);
#47129=ORIENTED_EDGE('',*,*,#35545,.F.);
#47130=ORIENTED_EDGE('',*,*,#35546,.F.);
#47131=ORIENTED_EDGE('',*,*,#35210,.T.);
#47132=ORIENTED_EDGE('',*,*,#35209,.T.);
#47133=ORIENTED_EDGE('',*,*,#35547,.F.);
#47134=ORIENTED_EDGE('',*,*,#35213,.T.);
#47135=ORIENTED_EDGE('',*,*,#35211,.T.);
#47136=ORIENTED_EDGE('',*,*,#35546,.T.);
#47137=ORIENTED_EDGE('',*,*,#35548,.F.);
#47138=ORIENTED_EDGE('',*,*,#35549,.F.);
#47139=ORIENTED_EDGE('',*,*,#35217,.T.);
#47140=ORIENTED_EDGE('',*,*,#35216,.T.);
#47141=ORIENTED_EDGE('',*,*,#35550,.F.);
#47142=ORIENTED_EDGE('',*,*,#35220,.T.);
#47143=ORIENTED_EDGE('',*,*,#35218,.T.);
#47144=ORIENTED_EDGE('',*,*,#35549,.T.);
#47145=ORIENTED_EDGE('',*,*,#35551,.F.);
#47146=ORIENTED_EDGE('',*,*,#35552,.F.);
#47147=ORIENTED_EDGE('',*,*,#35224,.T.);
#47148=ORIENTED_EDGE('',*,*,#35223,.T.);
#47149=ORIENTED_EDGE('',*,*,#35553,.F.);
#47150=ORIENTED_EDGE('',*,*,#35227,.T.);
#47151=ORIENTED_EDGE('',*,*,#35225,.T.);
#47152=ORIENTED_EDGE('',*,*,#35552,.T.);
#47153=ORIENTED_EDGE('',*,*,#35554,.F.);
#47154=ORIENTED_EDGE('',*,*,#35555,.F.);
#47155=ORIENTED_EDGE('',*,*,#35231,.T.);
#47156=ORIENTED_EDGE('',*,*,#35230,.T.);
#47157=ORIENTED_EDGE('',*,*,#35556,.F.);
#47158=ORIENTED_EDGE('',*,*,#35234,.T.);
#47159=ORIENTED_EDGE('',*,*,#35232,.T.);
#47160=ORIENTED_EDGE('',*,*,#35555,.T.);
#47161=ORIENTED_EDGE('',*,*,#35557,.F.);
#47162=ORIENTED_EDGE('',*,*,#35558,.F.);
#47163=ORIENTED_EDGE('',*,*,#35238,.T.);
#47164=ORIENTED_EDGE('',*,*,#35237,.T.);
#47165=ORIENTED_EDGE('',*,*,#35559,.F.);
#47166=ORIENTED_EDGE('',*,*,#35241,.T.);
#47167=ORIENTED_EDGE('',*,*,#35239,.T.);
#47168=ORIENTED_EDGE('',*,*,#35558,.T.);
#47169=ORIENTED_EDGE('',*,*,#35560,.F.);
#47170=ORIENTED_EDGE('',*,*,#35561,.F.);
#47171=ORIENTED_EDGE('',*,*,#35245,.T.);
#47172=ORIENTED_EDGE('',*,*,#35244,.T.);
#47173=ORIENTED_EDGE('',*,*,#35562,.F.);
#47174=ORIENTED_EDGE('',*,*,#35248,.T.);
#47175=ORIENTED_EDGE('',*,*,#35246,.T.);
#47176=ORIENTED_EDGE('',*,*,#35561,.T.);
#47177=ORIENTED_EDGE('',*,*,#35563,.F.);
#47178=ORIENTED_EDGE('',*,*,#35564,.F.);
#47179=ORIENTED_EDGE('',*,*,#35252,.T.);
#47180=ORIENTED_EDGE('',*,*,#35251,.T.);
#47181=ORIENTED_EDGE('',*,*,#35565,.F.);
#47182=ORIENTED_EDGE('',*,*,#35255,.T.);
#47183=ORIENTED_EDGE('',*,*,#35253,.T.);
#47184=ORIENTED_EDGE('',*,*,#35564,.T.);
#47185=ORIENTED_EDGE('',*,*,#35566,.F.);
#47186=ORIENTED_EDGE('',*,*,#35567,.F.);
#47187=ORIENTED_EDGE('',*,*,#35259,.T.);
#47188=ORIENTED_EDGE('',*,*,#35258,.T.);
#47189=ORIENTED_EDGE('',*,*,#35568,.F.);
#47190=ORIENTED_EDGE('',*,*,#35262,.T.);
#47191=ORIENTED_EDGE('',*,*,#35260,.T.);
#47192=ORIENTED_EDGE('',*,*,#35567,.T.);
#47193=ORIENTED_EDGE('',*,*,#35569,.F.);
#47194=ORIENTED_EDGE('',*,*,#35570,.F.);
#47195=ORIENTED_EDGE('',*,*,#35268,.T.);
#47196=ORIENTED_EDGE('',*,*,#35265,.T.);
#47197=ORIENTED_EDGE('',*,*,#35269,.T.);
#47198=ORIENTED_EDGE('',*,*,#35570,.T.);
#47199=ORIENTED_EDGE('',*,*,#35571,.F.);
#47200=ORIENTED_EDGE('',*,*,#35267,.T.);
#47201=ORIENTED_EDGE('',*,*,#35274,.T.);
#47202=ORIENTED_EDGE('',*,*,#35270,.T.);
#47203=ORIENTED_EDGE('',*,*,#35572,.F.);
#47204=ORIENTED_EDGE('',*,*,#35573,.F.);
#47205=ORIENTED_EDGE('',*,*,#35574,.F.);
#47206=ORIENTED_EDGE('',*,*,#35276,.T.);
#47207=ORIENTED_EDGE('',*,*,#35275,.T.);
#47208=ORIENTED_EDGE('',*,*,#35573,.T.);
#47209=ORIENTED_EDGE('',*,*,#35575,.F.);
#47210=ORIENTED_EDGE('',*,*,#35576,.F.);
#47211=ORIENTED_EDGE('',*,*,#35280,.T.);
#47212=ORIENTED_EDGE('',*,*,#35279,.T.);
#47213=ORIENTED_EDGE('',*,*,#35577,.F.);
#47214=ORIENTED_EDGE('',*,*,#35283,.T.);
#47215=ORIENTED_EDGE('',*,*,#35281,.T.);
#47216=ORIENTED_EDGE('',*,*,#35576,.T.);
#47217=ORIENTED_EDGE('',*,*,#35578,.F.);
#47218=ORIENTED_EDGE('',*,*,#35579,.F.);
#47219=ORIENTED_EDGE('',*,*,#35287,.T.);
#47220=ORIENTED_EDGE('',*,*,#35286,.T.);
#47221=ORIENTED_EDGE('',*,*,#35580,.F.);
#47222=ORIENTED_EDGE('',*,*,#35290,.T.);
#47223=ORIENTED_EDGE('',*,*,#35288,.T.);
#47224=ORIENTED_EDGE('',*,*,#35579,.T.);
#47225=ORIENTED_EDGE('',*,*,#35581,.F.);
#47226=ORIENTED_EDGE('',*,*,#35582,.F.);
#47227=ORIENTED_EDGE('',*,*,#35294,.T.);
#47228=ORIENTED_EDGE('',*,*,#35293,.T.);
#47229=ORIENTED_EDGE('',*,*,#35583,.F.);
#47230=ORIENTED_EDGE('',*,*,#35297,.T.);
#47231=ORIENTED_EDGE('',*,*,#35295,.T.);
#47232=ORIENTED_EDGE('',*,*,#35582,.T.);
#47233=ORIENTED_EDGE('',*,*,#35303,.T.);
#47234=ORIENTED_EDGE('',*,*,#35298,.T.);
#47235=ORIENTED_EDGE('',*,*,#35584,.F.);
#47236=ORIENTED_EDGE('',*,*,#35585,.F.);
#47237=ORIENTED_EDGE('',*,*,#35304,.T.);
#47238=ORIENTED_EDGE('',*,*,#35585,.T.);
#47239=ORIENTED_EDGE('',*,*,#35586,.F.);
#47240=ORIENTED_EDGE('',*,*,#35302,.T.);
#47241=ORIENTED_EDGE('',*,*,#35587,.F.);
#47242=ORIENTED_EDGE('',*,*,#35588,.F.);
#47243=ORIENTED_EDGE('',*,*,#35310,.T.);
#47244=ORIENTED_EDGE('',*,*,#35305,.T.);
#47245=ORIENTED_EDGE('',*,*,#35311,.T.);
#47246=ORIENTED_EDGE('',*,*,#35588,.T.);
#47247=ORIENTED_EDGE('',*,*,#35589,.F.);
#47248=ORIENTED_EDGE('',*,*,#35309,.T.);
#47249=ORIENTED_EDGE('',*,*,#35317,.T.);
#47250=ORIENTED_EDGE('',*,*,#35312,.T.);
#47251=ORIENTED_EDGE('',*,*,#35590,.F.);
#47252=ORIENTED_EDGE('',*,*,#35591,.F.);
#47253=ORIENTED_EDGE('',*,*,#35318,.T.);
#47254=ORIENTED_EDGE('',*,*,#35591,.T.);
#47255=ORIENTED_EDGE('',*,*,#35592,.F.);
#47256=ORIENTED_EDGE('',*,*,#35316,.T.);
#47257=ORIENTED_EDGE('',*,*,#35324,.T.);
#47258=ORIENTED_EDGE('',*,*,#35319,.T.);
#47259=ORIENTED_EDGE('',*,*,#35593,.F.);
#47260=ORIENTED_EDGE('',*,*,#35594,.F.);
#47261=ORIENTED_EDGE('',*,*,#35325,.T.);
#47262=ORIENTED_EDGE('',*,*,#35594,.T.);
#47263=ORIENTED_EDGE('',*,*,#35595,.F.);
#47264=ORIENTED_EDGE('',*,*,#35323,.T.);
#47265=ORIENTED_EDGE('',*,*,#35331,.T.);
#47266=ORIENTED_EDGE('',*,*,#35326,.T.);
#47267=ORIENTED_EDGE('',*,*,#35596,.F.);
#47268=ORIENTED_EDGE('',*,*,#35597,.F.);
#47269=ORIENTED_EDGE('',*,*,#35332,.T.);
#47270=ORIENTED_EDGE('',*,*,#35597,.T.);
#47271=ORIENTED_EDGE('',*,*,#35598,.F.);
#47272=ORIENTED_EDGE('',*,*,#35330,.T.);
#47273=ORIENTED_EDGE('',*,*,#35338,.T.);
#47274=ORIENTED_EDGE('',*,*,#35333,.T.);
#47275=ORIENTED_EDGE('',*,*,#35599,.F.);
#47276=ORIENTED_EDGE('',*,*,#35600,.F.);
#47277=ORIENTED_EDGE('',*,*,#35339,.T.);
#47278=ORIENTED_EDGE('',*,*,#35600,.T.);
#47279=ORIENTED_EDGE('',*,*,#35601,.F.);
#47280=ORIENTED_EDGE('',*,*,#35337,.T.);
#47281=ORIENTED_EDGE('',*,*,#35345,.T.);
#47282=ORIENTED_EDGE('',*,*,#35340,.T.);
#47283=ORIENTED_EDGE('',*,*,#35602,.F.);
#47284=ORIENTED_EDGE('',*,*,#35603,.F.);
#47285=ORIENTED_EDGE('',*,*,#35346,.T.);
#47286=ORIENTED_EDGE('',*,*,#35603,.T.);
#47287=ORIENTED_EDGE('',*,*,#35604,.F.);
#47288=ORIENTED_EDGE('',*,*,#35344,.T.);
#47289=ORIENTED_EDGE('',*,*,#35352,.T.);
#47290=ORIENTED_EDGE('',*,*,#35347,.T.);
#47291=ORIENTED_EDGE('',*,*,#35605,.F.);
#47292=ORIENTED_EDGE('',*,*,#35606,.F.);
#47293=ORIENTED_EDGE('',*,*,#35353,.T.);
#47294=ORIENTED_EDGE('',*,*,#35606,.T.);
#47295=ORIENTED_EDGE('',*,*,#35607,.F.);
#47296=ORIENTED_EDGE('',*,*,#35351,.T.);
#47297=ORIENTED_EDGE('',*,*,#35359,.T.);
#47298=ORIENTED_EDGE('',*,*,#35354,.T.);
#47299=ORIENTED_EDGE('',*,*,#35608,.F.);
#47300=ORIENTED_EDGE('',*,*,#35609,.F.);
#47301=ORIENTED_EDGE('',*,*,#35360,.T.);
#47302=ORIENTED_EDGE('',*,*,#35609,.T.);
#47303=ORIENTED_EDGE('',*,*,#35610,.F.);
#47304=ORIENTED_EDGE('',*,*,#35358,.T.);
#47305=ORIENTED_EDGE('',*,*,#35366,.T.);
#47306=ORIENTED_EDGE('',*,*,#35361,.T.);
#47307=ORIENTED_EDGE('',*,*,#35611,.F.);
#47308=ORIENTED_EDGE('',*,*,#35612,.F.);
#47309=ORIENTED_EDGE('',*,*,#35367,.T.);
#47310=ORIENTED_EDGE('',*,*,#35612,.T.);
#47311=ORIENTED_EDGE('',*,*,#35613,.F.);
#47312=ORIENTED_EDGE('',*,*,#35365,.T.);
#47313=ORIENTED_EDGE('',*,*,#35373,.T.);
#47314=ORIENTED_EDGE('',*,*,#35368,.T.);
#47315=ORIENTED_EDGE('',*,*,#35614,.F.);
#47316=ORIENTED_EDGE('',*,*,#35615,.F.);
#47317=ORIENTED_EDGE('',*,*,#35374,.T.);
#47318=ORIENTED_EDGE('',*,*,#35615,.T.);
#47319=ORIENTED_EDGE('',*,*,#35616,.F.);
#47320=ORIENTED_EDGE('',*,*,#35372,.T.);
#47321=ORIENTED_EDGE('',*,*,#35380,.T.);
#47322=ORIENTED_EDGE('',*,*,#35375,.T.);
#47323=ORIENTED_EDGE('',*,*,#35617,.F.);
#47324=ORIENTED_EDGE('',*,*,#35618,.F.);
#47325=ORIENTED_EDGE('',*,*,#35381,.T.);
#47326=ORIENTED_EDGE('',*,*,#35618,.T.);
#47327=ORIENTED_EDGE('',*,*,#35619,.F.);
#47328=ORIENTED_EDGE('',*,*,#35379,.T.);
#47329=ORIENTED_EDGE('',*,*,#35387,.T.);
#47330=ORIENTED_EDGE('',*,*,#35382,.T.);
#47331=ORIENTED_EDGE('',*,*,#35620,.F.);
#47332=ORIENTED_EDGE('',*,*,#35621,.F.);
#47333=ORIENTED_EDGE('',*,*,#35388,.T.);
#47334=ORIENTED_EDGE('',*,*,#35621,.T.);
#47335=ORIENTED_EDGE('',*,*,#35622,.F.);
#47336=ORIENTED_EDGE('',*,*,#35386,.T.);
#47337=ORIENTED_EDGE('',*,*,#35394,.T.);
#47338=ORIENTED_EDGE('',*,*,#35389,.T.);
#47339=ORIENTED_EDGE('',*,*,#35623,.F.);
#47340=ORIENTED_EDGE('',*,*,#35624,.F.);
#47341=ORIENTED_EDGE('',*,*,#35395,.T.);
#47342=ORIENTED_EDGE('',*,*,#35624,.T.);
#47343=ORIENTED_EDGE('',*,*,#35625,.F.);
#47344=ORIENTED_EDGE('',*,*,#35393,.T.);
#47345=ORIENTED_EDGE('',*,*,#35401,.T.);
#47346=ORIENTED_EDGE('',*,*,#35396,.T.);
#47347=ORIENTED_EDGE('',*,*,#35626,.F.);
#47348=ORIENTED_EDGE('',*,*,#35627,.F.);
#47349=ORIENTED_EDGE('',*,*,#35402,.T.);
#47350=ORIENTED_EDGE('',*,*,#35627,.T.);
#47351=ORIENTED_EDGE('',*,*,#35628,.F.);
#47352=ORIENTED_EDGE('',*,*,#35400,.T.);
#47353=ORIENTED_EDGE('',*,*,#35408,.T.);
#47354=ORIENTED_EDGE('',*,*,#35403,.T.);
#47355=ORIENTED_EDGE('',*,*,#35629,.F.);
#47356=ORIENTED_EDGE('',*,*,#35630,.F.);
#47357=ORIENTED_EDGE('',*,*,#35409,.T.);
#47358=ORIENTED_EDGE('',*,*,#35630,.T.);
#47359=ORIENTED_EDGE('',*,*,#35631,.F.);
#47360=ORIENTED_EDGE('',*,*,#35407,.T.);
#47361=ORIENTED_EDGE('',*,*,#35415,.T.);
#47362=ORIENTED_EDGE('',*,*,#35410,.T.);
#47363=ORIENTED_EDGE('',*,*,#35632,.F.);
#47364=ORIENTED_EDGE('',*,*,#35633,.F.);
#47365=ORIENTED_EDGE('',*,*,#35416,.T.);
#47366=ORIENTED_EDGE('',*,*,#35633,.T.);
#47367=ORIENTED_EDGE('',*,*,#35634,.F.);
#47368=ORIENTED_EDGE('',*,*,#35414,.T.);
#47369=ORIENTED_EDGE('',*,*,#35422,.T.);
#47370=ORIENTED_EDGE('',*,*,#35417,.T.);
#47371=ORIENTED_EDGE('',*,*,#35635,.F.);
#47372=ORIENTED_EDGE('',*,*,#35636,.F.);
#47373=ORIENTED_EDGE('',*,*,#35423,.T.);
#47374=ORIENTED_EDGE('',*,*,#35636,.T.);
#47375=ORIENTED_EDGE('',*,*,#35637,.F.);
#47376=ORIENTED_EDGE('',*,*,#35421,.T.);
#47377=ORIENTED_EDGE('',*,*,#35429,.T.);
#47378=ORIENTED_EDGE('',*,*,#35424,.T.);
#47379=ORIENTED_EDGE('',*,*,#35638,.F.);
#47380=ORIENTED_EDGE('',*,*,#35639,.F.);
#47381=ORIENTED_EDGE('',*,*,#35430,.T.);
#47382=ORIENTED_EDGE('',*,*,#35639,.T.);
#47383=ORIENTED_EDGE('',*,*,#35640,.F.);
#47384=ORIENTED_EDGE('',*,*,#35428,.T.);
#47385=ORIENTED_EDGE('',*,*,#35436,.T.);
#47386=ORIENTED_EDGE('',*,*,#35431,.T.);
#47387=ORIENTED_EDGE('',*,*,#35641,.F.);
#47388=ORIENTED_EDGE('',*,*,#35642,.F.);
#47389=ORIENTED_EDGE('',*,*,#35437,.T.);
#47390=ORIENTED_EDGE('',*,*,#35642,.T.);
#47391=ORIENTED_EDGE('',*,*,#35643,.F.);
#47392=ORIENTED_EDGE('',*,*,#35435,.T.);
#47393=ORIENTED_EDGE('',*,*,#35443,.T.);
#47394=ORIENTED_EDGE('',*,*,#35438,.T.);
#47395=ORIENTED_EDGE('',*,*,#35644,.F.);
#47396=ORIENTED_EDGE('',*,*,#35645,.F.);
#47397=ORIENTED_EDGE('',*,*,#35444,.T.);
#47398=ORIENTED_EDGE('',*,*,#35645,.T.);
#47399=ORIENTED_EDGE('',*,*,#35646,.F.);
#47400=ORIENTED_EDGE('',*,*,#35442,.T.);
#47401=ORIENTED_EDGE('',*,*,#34453,.T.);
#47402=ORIENTED_EDGE('',*,*,#35445,.T.);
#47403=ORIENTED_EDGE('',*,*,#35647,.F.);
#47404=ORIENTED_EDGE('',*,*,#35648,.F.);
#47405=ORIENTED_EDGE('',*,*,#34454,.T.);
#47406=ORIENTED_EDGE('',*,*,#35648,.T.);
#47407=ORIENTED_EDGE('',*,*,#35649,.F.);
#47408=ORIENTED_EDGE('',*,*,#35447,.T.);
#47409=ORIENTED_EDGE('',*,*,#35453,.T.);
#47410=ORIENTED_EDGE('',*,*,#35448,.T.);
#47411=ORIENTED_EDGE('',*,*,#35650,.F.);
#47412=ORIENTED_EDGE('',*,*,#35651,.F.);
#47413=ORIENTED_EDGE('',*,*,#35454,.T.);
#47414=ORIENTED_EDGE('',*,*,#35651,.T.);
#47415=ORIENTED_EDGE('',*,*,#35652,.F.);
#47416=ORIENTED_EDGE('',*,*,#35452,.T.);
#47417=ORIENTED_EDGE('',*,*,#35460,.T.);
#47418=ORIENTED_EDGE('',*,*,#35455,.T.);
#47419=ORIENTED_EDGE('',*,*,#35653,.F.);
#47420=ORIENTED_EDGE('',*,*,#35654,.F.);
#47421=ORIENTED_EDGE('',*,*,#35461,.T.);
#47422=ORIENTED_EDGE('',*,*,#35654,.T.);
#47423=ORIENTED_EDGE('',*,*,#35655,.F.);
#47424=ORIENTED_EDGE('',*,*,#35459,.T.);
#47425=ORIENTED_EDGE('',*,*,#35467,.T.);
#47426=ORIENTED_EDGE('',*,*,#35462,.T.);
#47427=ORIENTED_EDGE('',*,*,#35656,.F.);
#47428=ORIENTED_EDGE('',*,*,#35657,.F.);
#47429=ORIENTED_EDGE('',*,*,#35468,.T.);
#47430=ORIENTED_EDGE('',*,*,#35657,.T.);
#47431=ORIENTED_EDGE('',*,*,#35658,.F.);
#47432=ORIENTED_EDGE('',*,*,#35466,.T.);
#47433=ORIENTED_EDGE('',*,*,#35474,.T.);
#47434=ORIENTED_EDGE('',*,*,#35469,.T.);
#47435=ORIENTED_EDGE('',*,*,#35659,.F.);
#47436=ORIENTED_EDGE('',*,*,#35660,.F.);
#47437=ORIENTED_EDGE('',*,*,#35475,.T.);
#47438=ORIENTED_EDGE('',*,*,#35660,.T.);
#47439=ORIENTED_EDGE('',*,*,#35661,.F.);
#47440=ORIENTED_EDGE('',*,*,#35473,.T.);
#47441=ORIENTED_EDGE('',*,*,#35481,.T.);
#47442=ORIENTED_EDGE('',*,*,#35476,.T.);
#47443=ORIENTED_EDGE('',*,*,#35662,.F.);
#47444=ORIENTED_EDGE('',*,*,#35663,.F.);
#47445=ORIENTED_EDGE('',*,*,#35482,.T.);
#47446=ORIENTED_EDGE('',*,*,#35663,.T.);
#47447=ORIENTED_EDGE('',*,*,#35664,.F.);
#47448=ORIENTED_EDGE('',*,*,#35480,.T.);
#47449=ORIENTED_EDGE('',*,*,#35488,.T.);
#47450=ORIENTED_EDGE('',*,*,#35483,.T.);
#47451=ORIENTED_EDGE('',*,*,#35665,.F.);
#47452=ORIENTED_EDGE('',*,*,#35666,.F.);
#47453=ORIENTED_EDGE('',*,*,#35489,.T.);
#47454=ORIENTED_EDGE('',*,*,#35666,.T.);
#47455=ORIENTED_EDGE('',*,*,#35667,.F.);
#47456=ORIENTED_EDGE('',*,*,#35487,.T.);
#47457=ORIENTED_EDGE('',*,*,#35495,.T.);
#47458=ORIENTED_EDGE('',*,*,#35490,.T.);
#47459=ORIENTED_EDGE('',*,*,#35668,.F.);
#47460=ORIENTED_EDGE('',*,*,#35669,.F.);
#47461=ORIENTED_EDGE('',*,*,#35496,.T.);
#47462=ORIENTED_EDGE('',*,*,#35669,.T.);
#47463=ORIENTED_EDGE('',*,*,#35670,.F.);
#47464=ORIENTED_EDGE('',*,*,#35494,.T.);
#47465=ORIENTED_EDGE('',*,*,#35671,.T.);
#47466=ORIENTED_EDGE('',*,*,#35672,.F.);
#47467=ORIENTED_EDGE('',*,*,#35497,.T.);
#47468=ORIENTED_EDGE('',*,*,#35673,.F.);
#47469=ORIENTED_EDGE('',*,*,#35674,.T.);
#47470=ORIENTED_EDGE('',*,*,#35675,.F.);
#47471=ORIENTED_EDGE('',*,*,#35499,.T.);
#47472=ORIENTED_EDGE('',*,*,#35676,.F.);
#47473=ORIENTED_EDGE('',*,*,#35677,.F.);
#47474=ORIENTED_EDGE('',*,*,#35678,.F.);
#47475=ORIENTED_EDGE('',*,*,#35679,.F.);
#47476=ORIENTED_EDGE('',*,*,#35674,.F.);
#47477=ORIENTED_EDGE('',*,*,#35679,.T.);
#47478=ORIENTED_EDGE('',*,*,#35680,.F.);
#47479=ORIENTED_EDGE('',*,*,#35500,.T.);
#47480=ORIENTED_EDGE('',*,*,#35675,.T.);
#47481=ORIENTED_EDGE('',*,*,#35681,.T.);
#47482=ORIENTED_EDGE('',*,*,#35682,.F.);
#47483=ORIENTED_EDGE('',*,*,#35502,.T.);
#47484=ORIENTED_EDGE('',*,*,#35683,.F.);
#47485=ORIENTED_EDGE('',*,*,#35684,.F.);
#47486=ORIENTED_EDGE('',*,*,#35685,.F.);
#47487=ORIENTED_EDGE('',*,*,#35686,.F.);
#47488=ORIENTED_EDGE('',*,*,#35681,.F.);
#47489=ORIENTED_EDGE('',*,*,#35686,.T.);
#47490=ORIENTED_EDGE('',*,*,#35687,.F.);
#47491=ORIENTED_EDGE('',*,*,#35503,.T.);
#47492=ORIENTED_EDGE('',*,*,#35682,.T.);
#47493=ORIENTED_EDGE('',*,*,#35688,.T.);
#47494=ORIENTED_EDGE('',*,*,#35689,.F.);
#47495=ORIENTED_EDGE('',*,*,#35505,.T.);
#47496=ORIENTED_EDGE('',*,*,#35690,.F.);
#47497=ORIENTED_EDGE('',*,*,#35691,.F.);
#47498=ORIENTED_EDGE('',*,*,#35692,.F.);
#47499=ORIENTED_EDGE('',*,*,#35693,.F.);
#47500=ORIENTED_EDGE('',*,*,#35688,.F.);
#47501=ORIENTED_EDGE('',*,*,#35693,.T.);
#47502=ORIENTED_EDGE('',*,*,#35694,.F.);
#47503=ORIENTED_EDGE('',*,*,#35506,.T.);
#47504=ORIENTED_EDGE('',*,*,#35689,.T.);
#47505=ORIENTED_EDGE('',*,*,#35695,.T.);
#47506=ORIENTED_EDGE('',*,*,#35696,.F.);
#47507=ORIENTED_EDGE('',*,*,#35508,.T.);
#47508=ORIENTED_EDGE('',*,*,#35697,.F.);
#47509=ORIENTED_EDGE('',*,*,#35698,.F.);
#47510=ORIENTED_EDGE('',*,*,#35699,.F.);
#47511=ORIENTED_EDGE('',*,*,#35700,.F.);
#47512=ORIENTED_EDGE('',*,*,#35695,.F.);
#47513=ORIENTED_EDGE('',*,*,#35700,.T.);
#47514=ORIENTED_EDGE('',*,*,#35701,.F.);
#47515=ORIENTED_EDGE('',*,*,#35509,.T.);
#47516=ORIENTED_EDGE('',*,*,#35696,.T.);
#47517=ORIENTED_EDGE('',*,*,#35702,.T.);
#47518=ORIENTED_EDGE('',*,*,#35703,.F.);
#47519=ORIENTED_EDGE('',*,*,#35511,.T.);
#47520=ORIENTED_EDGE('',*,*,#35704,.F.);
#47521=ORIENTED_EDGE('',*,*,#35705,.F.);
#47522=ORIENTED_EDGE('',*,*,#35706,.F.);
#47523=ORIENTED_EDGE('',*,*,#35707,.F.);
#47524=ORIENTED_EDGE('',*,*,#35702,.F.);
#47525=ORIENTED_EDGE('',*,*,#35707,.T.);
#47526=ORIENTED_EDGE('',*,*,#35708,.F.);
#47527=ORIENTED_EDGE('',*,*,#35512,.T.);
#47528=ORIENTED_EDGE('',*,*,#35703,.T.);
#47529=ORIENTED_EDGE('',*,*,#35709,.T.);
#47530=ORIENTED_EDGE('',*,*,#35710,.F.);
#47531=ORIENTED_EDGE('',*,*,#35514,.T.);
#47532=ORIENTED_EDGE('',*,*,#35711,.F.);
#47533=ORIENTED_EDGE('',*,*,#35712,.F.);
#47534=ORIENTED_EDGE('',*,*,#35713,.F.);
#47535=ORIENTED_EDGE('',*,*,#35714,.F.);
#47536=ORIENTED_EDGE('',*,*,#35709,.F.);
#47537=ORIENTED_EDGE('',*,*,#35714,.T.);
#47538=ORIENTED_EDGE('',*,*,#35715,.F.);
#47539=ORIENTED_EDGE('',*,*,#35515,.T.);
#47540=ORIENTED_EDGE('',*,*,#35710,.T.);
#47541=ORIENTED_EDGE('',*,*,#34450,.T.);
#47542=ORIENTED_EDGE('',*,*,#35716,.F.);
#47543=ORIENTED_EDGE('',*,*,#35517,.T.);
#47544=ORIENTED_EDGE('',*,*,#35717,.F.);
#47545=ORIENTED_EDGE('',*,*,#34449,.T.);
#47546=ORIENTED_EDGE('',*,*,#35718,.F.);
#47547=ORIENTED_EDGE('',*,*,#35518,.T.);
#47548=ORIENTED_EDGE('',*,*,#35716,.T.);
#47549=ORIENTED_EDGE('',*,*,#35719,.T.);
#47550=ORIENTED_EDGE('',*,*,#35720,.F.);
#47551=ORIENTED_EDGE('',*,*,#35520,.T.);
#47552=ORIENTED_EDGE('',*,*,#35721,.F.);
#47553=ORIENTED_EDGE('',*,*,#35722,.F.);
#47554=ORIENTED_EDGE('',*,*,#35723,.F.);
#47555=ORIENTED_EDGE('',*,*,#35724,.F.);
#47556=ORIENTED_EDGE('',*,*,#35719,.F.);
#47557=ORIENTED_EDGE('',*,*,#35724,.T.);
#47558=ORIENTED_EDGE('',*,*,#35725,.F.);
#47559=ORIENTED_EDGE('',*,*,#35521,.T.);
#47560=ORIENTED_EDGE('',*,*,#35720,.T.);
#47561=ORIENTED_EDGE('',*,*,#35726,.T.);
#47562=ORIENTED_EDGE('',*,*,#35727,.F.);
#47563=ORIENTED_EDGE('',*,*,#35523,.T.);
#47564=ORIENTED_EDGE('',*,*,#35728,.F.);
#47565=ORIENTED_EDGE('',*,*,#35729,.F.);
#47566=ORIENTED_EDGE('',*,*,#35730,.F.);
#47567=ORIENTED_EDGE('',*,*,#35731,.F.);
#47568=ORIENTED_EDGE('',*,*,#35726,.F.);
#47569=ORIENTED_EDGE('',*,*,#35731,.T.);
#47570=ORIENTED_EDGE('',*,*,#35732,.F.);
#47571=ORIENTED_EDGE('',*,*,#35524,.T.);
#47572=ORIENTED_EDGE('',*,*,#35727,.T.);
#47573=ORIENTED_EDGE('',*,*,#35733,.T.);
#47574=ORIENTED_EDGE('',*,*,#35734,.F.);
#47575=ORIENTED_EDGE('',*,*,#35526,.T.);
#47576=ORIENTED_EDGE('',*,*,#35735,.F.);
#47577=ORIENTED_EDGE('',*,*,#35736,.F.);
#47578=ORIENTED_EDGE('',*,*,#35737,.F.);
#47579=ORIENTED_EDGE('',*,*,#35738,.F.);
#47580=ORIENTED_EDGE('',*,*,#35733,.F.);
#47581=ORIENTED_EDGE('',*,*,#35738,.T.);
#47582=ORIENTED_EDGE('',*,*,#35739,.F.);
#47583=ORIENTED_EDGE('',*,*,#35527,.T.);
#47584=ORIENTED_EDGE('',*,*,#35734,.T.);
#47585=ORIENTED_EDGE('',*,*,#35740,.T.);
#47586=ORIENTED_EDGE('',*,*,#35741,.F.);
#47587=ORIENTED_EDGE('',*,*,#35529,.T.);
#47588=ORIENTED_EDGE('',*,*,#35742,.F.);
#47589=ORIENTED_EDGE('',*,*,#35743,.F.);
#47590=ORIENTED_EDGE('',*,*,#35744,.F.);
#47591=ORIENTED_EDGE('',*,*,#35745,.F.);
#47592=ORIENTED_EDGE('',*,*,#35740,.F.);
#47593=ORIENTED_EDGE('',*,*,#35745,.T.);
#47594=ORIENTED_EDGE('',*,*,#35746,.F.);
#47595=ORIENTED_EDGE('',*,*,#35530,.T.);
#47596=ORIENTED_EDGE('',*,*,#35741,.T.);
#47597=ORIENTED_EDGE('',*,*,#35747,.T.);
#47598=ORIENTED_EDGE('',*,*,#35748,.F.);
#47599=ORIENTED_EDGE('',*,*,#35532,.T.);
#47600=ORIENTED_EDGE('',*,*,#35749,.F.);
#47601=ORIENTED_EDGE('',*,*,#35750,.F.);
#47602=ORIENTED_EDGE('',*,*,#35751,.F.);
#47603=ORIENTED_EDGE('',*,*,#35752,.F.);
#47604=ORIENTED_EDGE('',*,*,#35747,.F.);
#47605=ORIENTED_EDGE('',*,*,#35752,.T.);
#47606=ORIENTED_EDGE('',*,*,#35753,.F.);
#47607=ORIENTED_EDGE('',*,*,#35533,.T.);
#47608=ORIENTED_EDGE('',*,*,#35748,.T.);
#47609=ORIENTED_EDGE('',*,*,#35754,.T.);
#47610=ORIENTED_EDGE('',*,*,#35755,.F.);
#47611=ORIENTED_EDGE('',*,*,#35535,.T.);
#47612=ORIENTED_EDGE('',*,*,#35756,.F.);
#47613=ORIENTED_EDGE('',*,*,#35757,.F.);
#47614=ORIENTED_EDGE('',*,*,#35758,.F.);
#47615=ORIENTED_EDGE('',*,*,#35759,.F.);
#47616=ORIENTED_EDGE('',*,*,#35754,.F.);
#47617=ORIENTED_EDGE('',*,*,#35759,.T.);
#47618=ORIENTED_EDGE('',*,*,#35760,.F.);
#47619=ORIENTED_EDGE('',*,*,#35536,.T.);
#47620=ORIENTED_EDGE('',*,*,#35755,.T.);
#47621=ORIENTED_EDGE('',*,*,#35761,.T.);
#47622=ORIENTED_EDGE('',*,*,#35762,.F.);
#47623=ORIENTED_EDGE('',*,*,#35538,.T.);
#47624=ORIENTED_EDGE('',*,*,#35763,.F.);
#47625=ORIENTED_EDGE('',*,*,#35764,.F.);
#47626=ORIENTED_EDGE('',*,*,#35765,.F.);
#47627=ORIENTED_EDGE('',*,*,#35766,.F.);
#47628=ORIENTED_EDGE('',*,*,#35761,.F.);
#47629=ORIENTED_EDGE('',*,*,#35766,.T.);
#47630=ORIENTED_EDGE('',*,*,#35767,.F.);
#47631=ORIENTED_EDGE('',*,*,#35539,.T.);
#47632=ORIENTED_EDGE('',*,*,#35762,.T.);
#47633=ORIENTED_EDGE('',*,*,#35768,.T.);
#47634=ORIENTED_EDGE('',*,*,#35769,.F.);
#47635=ORIENTED_EDGE('',*,*,#35541,.T.);
#47636=ORIENTED_EDGE('',*,*,#35770,.F.);
#47637=ORIENTED_EDGE('',*,*,#35771,.F.);
#47638=ORIENTED_EDGE('',*,*,#35772,.F.);
#47639=ORIENTED_EDGE('',*,*,#35773,.F.);
#47640=ORIENTED_EDGE('',*,*,#35768,.F.);
#47641=ORIENTED_EDGE('',*,*,#35773,.T.);
#47642=ORIENTED_EDGE('',*,*,#35774,.F.);
#47643=ORIENTED_EDGE('',*,*,#35542,.T.);
#47644=ORIENTED_EDGE('',*,*,#35769,.T.);
#47645=ORIENTED_EDGE('',*,*,#35775,.T.);
#47646=ORIENTED_EDGE('',*,*,#35776,.F.);
#47647=ORIENTED_EDGE('',*,*,#35544,.T.);
#47648=ORIENTED_EDGE('',*,*,#35777,.F.);
#47649=ORIENTED_EDGE('',*,*,#35778,.F.);
#47650=ORIENTED_EDGE('',*,*,#35779,.F.);
#47651=ORIENTED_EDGE('',*,*,#35780,.F.);
#47652=ORIENTED_EDGE('',*,*,#35775,.F.);
#47653=ORIENTED_EDGE('',*,*,#35780,.T.);
#47654=ORIENTED_EDGE('',*,*,#35781,.F.);
#47655=ORIENTED_EDGE('',*,*,#35545,.T.);
#47656=ORIENTED_EDGE('',*,*,#35776,.T.);
#47657=ORIENTED_EDGE('',*,*,#35782,.T.);
#47658=ORIENTED_EDGE('',*,*,#35783,.F.);
#47659=ORIENTED_EDGE('',*,*,#35547,.T.);
#47660=ORIENTED_EDGE('',*,*,#35784,.F.);
#47661=ORIENTED_EDGE('',*,*,#35785,.F.);
#47662=ORIENTED_EDGE('',*,*,#35786,.F.);
#47663=ORIENTED_EDGE('',*,*,#35787,.F.);
#47664=ORIENTED_EDGE('',*,*,#35782,.F.);
#47665=ORIENTED_EDGE('',*,*,#35787,.T.);
#47666=ORIENTED_EDGE('',*,*,#35788,.F.);
#47667=ORIENTED_EDGE('',*,*,#35548,.T.);
#47668=ORIENTED_EDGE('',*,*,#35783,.T.);
#47669=ORIENTED_EDGE('',*,*,#35789,.T.);
#47670=ORIENTED_EDGE('',*,*,#35790,.F.);
#47671=ORIENTED_EDGE('',*,*,#35550,.T.);
#47672=ORIENTED_EDGE('',*,*,#35791,.F.);
#47673=ORIENTED_EDGE('',*,*,#35792,.F.);
#47674=ORIENTED_EDGE('',*,*,#35793,.F.);
#47675=ORIENTED_EDGE('',*,*,#35794,.F.);
#47676=ORIENTED_EDGE('',*,*,#35789,.F.);
#47677=ORIENTED_EDGE('',*,*,#35794,.T.);
#47678=ORIENTED_EDGE('',*,*,#35795,.F.);
#47679=ORIENTED_EDGE('',*,*,#35551,.T.);
#47680=ORIENTED_EDGE('',*,*,#35790,.T.);
#47681=ORIENTED_EDGE('',*,*,#35796,.T.);
#47682=ORIENTED_EDGE('',*,*,#35797,.F.);
#47683=ORIENTED_EDGE('',*,*,#35553,.T.);
#47684=ORIENTED_EDGE('',*,*,#35798,.F.);
#47685=ORIENTED_EDGE('',*,*,#35799,.F.);
#47686=ORIENTED_EDGE('',*,*,#35800,.F.);
#47687=ORIENTED_EDGE('',*,*,#35801,.F.);
#47688=ORIENTED_EDGE('',*,*,#35796,.F.);
#47689=ORIENTED_EDGE('',*,*,#35801,.T.);
#47690=ORIENTED_EDGE('',*,*,#35802,.F.);
#47691=ORIENTED_EDGE('',*,*,#35554,.T.);
#47692=ORIENTED_EDGE('',*,*,#35797,.T.);
#47693=ORIENTED_EDGE('',*,*,#35803,.T.);
#47694=ORIENTED_EDGE('',*,*,#35804,.F.);
#47695=ORIENTED_EDGE('',*,*,#35556,.T.);
#47696=ORIENTED_EDGE('',*,*,#35805,.F.);
#47697=ORIENTED_EDGE('',*,*,#35806,.F.);
#47698=ORIENTED_EDGE('',*,*,#35807,.F.);
#47699=ORIENTED_EDGE('',*,*,#35808,.F.);
#47700=ORIENTED_EDGE('',*,*,#35803,.F.);
#47701=ORIENTED_EDGE('',*,*,#35808,.T.);
#47702=ORIENTED_EDGE('',*,*,#35809,.F.);
#47703=ORIENTED_EDGE('',*,*,#35557,.T.);
#47704=ORIENTED_EDGE('',*,*,#35804,.T.);
#47705=ORIENTED_EDGE('',*,*,#35810,.T.);
#47706=ORIENTED_EDGE('',*,*,#35811,.F.);
#47707=ORIENTED_EDGE('',*,*,#35559,.T.);
#47708=ORIENTED_EDGE('',*,*,#35812,.F.);
#47709=ORIENTED_EDGE('',*,*,#35813,.F.);
#47710=ORIENTED_EDGE('',*,*,#35814,.F.);
#47711=ORIENTED_EDGE('',*,*,#35815,.F.);
#47712=ORIENTED_EDGE('',*,*,#35810,.F.);
#47713=ORIENTED_EDGE('',*,*,#35815,.T.);
#47714=ORIENTED_EDGE('',*,*,#35816,.F.);
#47715=ORIENTED_EDGE('',*,*,#35560,.T.);
#47716=ORIENTED_EDGE('',*,*,#35811,.T.);
#47717=ORIENTED_EDGE('',*,*,#35817,.T.);
#47718=ORIENTED_EDGE('',*,*,#35818,.F.);
#47719=ORIENTED_EDGE('',*,*,#35562,.T.);
#47720=ORIENTED_EDGE('',*,*,#35819,.F.);
#47721=ORIENTED_EDGE('',*,*,#35820,.F.);
#47722=ORIENTED_EDGE('',*,*,#35821,.F.);
#47723=ORIENTED_EDGE('',*,*,#35822,.F.);
#47724=ORIENTED_EDGE('',*,*,#35817,.F.);
#47725=ORIENTED_EDGE('',*,*,#35822,.T.);
#47726=ORIENTED_EDGE('',*,*,#35823,.F.);
#47727=ORIENTED_EDGE('',*,*,#35563,.T.);
#47728=ORIENTED_EDGE('',*,*,#35818,.T.);
#47729=ORIENTED_EDGE('',*,*,#35824,.T.);
#47730=ORIENTED_EDGE('',*,*,#35825,.F.);
#47731=ORIENTED_EDGE('',*,*,#35565,.T.);
#47732=ORIENTED_EDGE('',*,*,#35826,.F.);
#47733=ORIENTED_EDGE('',*,*,#35827,.F.);
#47734=ORIENTED_EDGE('',*,*,#35828,.F.);
#47735=ORIENTED_EDGE('',*,*,#35829,.F.);
#47736=ORIENTED_EDGE('',*,*,#35824,.F.);
#47737=ORIENTED_EDGE('',*,*,#35829,.T.);
#47738=ORIENTED_EDGE('',*,*,#35830,.F.);
#47739=ORIENTED_EDGE('',*,*,#35566,.T.);
#47740=ORIENTED_EDGE('',*,*,#35825,.T.);
#47741=ORIENTED_EDGE('',*,*,#35831,.T.);
#47742=ORIENTED_EDGE('',*,*,#35832,.F.);
#47743=ORIENTED_EDGE('',*,*,#35568,.T.);
#47744=ORIENTED_EDGE('',*,*,#35833,.F.);
#47745=ORIENTED_EDGE('',*,*,#35834,.T.);
#47746=ORIENTED_EDGE('',*,*,#35835,.F.);
#47747=ORIENTED_EDGE('',*,*,#35569,.T.);
#47748=ORIENTED_EDGE('',*,*,#35832,.T.);
#47749=ORIENTED_EDGE('',*,*,#35836,.F.);
#47750=ORIENTED_EDGE('',*,*,#35837,.F.);
#47751=ORIENTED_EDGE('',*,*,#35834,.F.);
#47752=ORIENTED_EDGE('',*,*,#35831,.F.);
#47753=ORIENTED_EDGE('',*,*,#35571,.T.);
#47754=ORIENTED_EDGE('',*,*,#35838,.F.);
#47755=ORIENTED_EDGE('',*,*,#35839,.T.);
#47756=ORIENTED_EDGE('',*,*,#35840,.F.);
#47757=ORIENTED_EDGE('',*,*,#35841,.F.);
#47758=ORIENTED_EDGE('',*,*,#35839,.F.);
#47759=ORIENTED_EDGE('',*,*,#35842,.F.);
#47760=ORIENTED_EDGE('',*,*,#35843,.F.);
#47761=ORIENTED_EDGE('',*,*,#35572,.T.);
#47762=ORIENTED_EDGE('',*,*,#35840,.T.);
#47763=ORIENTED_EDGE('',*,*,#35841,.T.);
#47764=ORIENTED_EDGE('',*,*,#35844,.F.);
#47765=ORIENTED_EDGE('',*,*,#35845,.T.);
#47766=ORIENTED_EDGE('',*,*,#35846,.F.);
#47767=ORIENTED_EDGE('',*,*,#35574,.T.);
#47768=ORIENTED_EDGE('',*,*,#35847,.F.);
#47769=ORIENTED_EDGE('',*,*,#35848,.F.);
#47770=ORIENTED_EDGE('',*,*,#35849,.F.);
#47771=ORIENTED_EDGE('',*,*,#35850,.F.);
#47772=ORIENTED_EDGE('',*,*,#35845,.F.);
#47773=ORIENTED_EDGE('',*,*,#35850,.T.);
#47774=ORIENTED_EDGE('',*,*,#35851,.F.);
#47775=ORIENTED_EDGE('',*,*,#35575,.T.);
#47776=ORIENTED_EDGE('',*,*,#35846,.T.);
#47777=ORIENTED_EDGE('',*,*,#35852,.T.);
#47778=ORIENTED_EDGE('',*,*,#35853,.F.);
#47779=ORIENTED_EDGE('',*,*,#35577,.T.);
#47780=ORIENTED_EDGE('',*,*,#35854,.F.);
#47781=ORIENTED_EDGE('',*,*,#35855,.F.);
#47782=ORIENTED_EDGE('',*,*,#35856,.F.);
#47783=ORIENTED_EDGE('',*,*,#35857,.F.);
#47784=ORIENTED_EDGE('',*,*,#35852,.F.);
#47785=ORIENTED_EDGE('',*,*,#35857,.T.);
#47786=ORIENTED_EDGE('',*,*,#35858,.F.);
#47787=ORIENTED_EDGE('',*,*,#35578,.T.);
#47788=ORIENTED_EDGE('',*,*,#35853,.T.);
#47789=ORIENTED_EDGE('',*,*,#35859,.T.);
#47790=ORIENTED_EDGE('',*,*,#35860,.F.);
#47791=ORIENTED_EDGE('',*,*,#35580,.T.);
#47792=ORIENTED_EDGE('',*,*,#35861,.F.);
#47793=ORIENTED_EDGE('',*,*,#35862,.F.);
#47794=ORIENTED_EDGE('',*,*,#35863,.F.);
#47795=ORIENTED_EDGE('',*,*,#35864,.F.);
#47796=ORIENTED_EDGE('',*,*,#35859,.F.);
#47797=ORIENTED_EDGE('',*,*,#35864,.T.);
#47798=ORIENTED_EDGE('',*,*,#35865,.F.);
#47799=ORIENTED_EDGE('',*,*,#35581,.T.);
#47800=ORIENTED_EDGE('',*,*,#35860,.T.);
#47801=ORIENTED_EDGE('',*,*,#35866,.F.);
#47802=ORIENTED_EDGE('',*,*,#35867,.F.);
#47803=ORIENTED_EDGE('',*,*,#35671,.F.);
#47804=ORIENTED_EDGE('',*,*,#35868,.F.);
#47805=ORIENTED_EDGE('',*,*,#35868,.T.);
#47806=ORIENTED_EDGE('',*,*,#35673,.T.);
#47807=ORIENTED_EDGE('',*,*,#35583,.T.);
#47808=ORIENTED_EDGE('',*,*,#35869,.F.);
#47809=ORIENTED_EDGE('',*,*,#35584,.T.);
#47810=ORIENTED_EDGE('',*,*,#35870,.F.);
#47811=ORIENTED_EDGE('',*,*,#35871,.T.);
#47812=ORIENTED_EDGE('',*,*,#35872,.F.);
#47813=ORIENTED_EDGE('',*,*,#35586,.T.);
#47814=ORIENTED_EDGE('',*,*,#35873,.F.);
#47815=ORIENTED_EDGE('',*,*,#35874,.T.);
#47816=ORIENTED_EDGE('',*,*,#35875,.F.);
#47817=ORIENTED_EDGE('',*,*,#35876,.T.);
#47818=ORIENTED_EDGE('',*,*,#35877,.F.);
#47819=ORIENTED_EDGE('',*,*,#35587,.T.);
#47820=ORIENTED_EDGE('',*,*,#35875,.T.);
#47821=ORIENTED_EDGE('',*,*,#35878,.F.);
#47822=ORIENTED_EDGE('',*,*,#35879,.F.);
#47823=ORIENTED_EDGE('',*,*,#35876,.F.);
#47824=ORIENTED_EDGE('',*,*,#35874,.F.);
#47825=ORIENTED_EDGE('',*,*,#35589,.T.);
#47826=ORIENTED_EDGE('',*,*,#35880,.F.);
#47827=ORIENTED_EDGE('',*,*,#35881,.T.);
#47828=ORIENTED_EDGE('',*,*,#35882,.F.);
#47829=ORIENTED_EDGE('',*,*,#35590,.T.);
#47830=ORIENTED_EDGE('',*,*,#35882,.T.);
#47831=ORIENTED_EDGE('',*,*,#35883,.T.);
#47832=ORIENTED_EDGE('',*,*,#35884,.F.);
#47833=ORIENTED_EDGE('',*,*,#35883,.F.);
#47834=ORIENTED_EDGE('',*,*,#35881,.F.);
#47835=ORIENTED_EDGE('',*,*,#35885,.F.);
#47836=ORIENTED_EDGE('',*,*,#35886,.F.);
#47837=ORIENTED_EDGE('',*,*,#35592,.T.);
#47838=ORIENTED_EDGE('',*,*,#35887,.F.);
#47839=ORIENTED_EDGE('',*,*,#35888,.T.);
#47840=ORIENTED_EDGE('',*,*,#35889,.F.);
#47841=ORIENTED_EDGE('',*,*,#35593,.T.);
#47842=ORIENTED_EDGE('',*,*,#35889,.T.);
#47843=ORIENTED_EDGE('',*,*,#35890,.T.);
#47844=ORIENTED_EDGE('',*,*,#35891,.F.);
#47845=ORIENTED_EDGE('',*,*,#35890,.F.);
#47846=ORIENTED_EDGE('',*,*,#35888,.F.);
#47847=ORIENTED_EDGE('',*,*,#35892,.F.);
#47848=ORIENTED_EDGE('',*,*,#35893,.F.);
#47849=ORIENTED_EDGE('',*,*,#35595,.T.);
#47850=ORIENTED_EDGE('',*,*,#35894,.F.);
#47851=ORIENTED_EDGE('',*,*,#35895,.T.);
#47852=ORIENTED_EDGE('',*,*,#35896,.F.);
#47853=ORIENTED_EDGE('',*,*,#35596,.T.);
#47854=ORIENTED_EDGE('',*,*,#35896,.T.);
#47855=ORIENTED_EDGE('',*,*,#35897,.T.);
#47856=ORIENTED_EDGE('',*,*,#35898,.F.);
#47857=ORIENTED_EDGE('',*,*,#35897,.F.);
#47858=ORIENTED_EDGE('',*,*,#35895,.F.);
#47859=ORIENTED_EDGE('',*,*,#35899,.F.);
#47860=ORIENTED_EDGE('',*,*,#35900,.F.);
#47861=ORIENTED_EDGE('',*,*,#35598,.T.);
#47862=ORIENTED_EDGE('',*,*,#35901,.F.);
#47863=ORIENTED_EDGE('',*,*,#35902,.T.);
#47864=ORIENTED_EDGE('',*,*,#35903,.F.);
#47865=ORIENTED_EDGE('',*,*,#35599,.T.);
#47866=ORIENTED_EDGE('',*,*,#35903,.T.);
#47867=ORIENTED_EDGE('',*,*,#35904,.T.);
#47868=ORIENTED_EDGE('',*,*,#35905,.F.);
#47869=ORIENTED_EDGE('',*,*,#35904,.F.);
#47870=ORIENTED_EDGE('',*,*,#35902,.F.);
#47871=ORIENTED_EDGE('',*,*,#35906,.F.);
#47872=ORIENTED_EDGE('',*,*,#35907,.F.);
#47873=ORIENTED_EDGE('',*,*,#35601,.T.);
#47874=ORIENTED_EDGE('',*,*,#35908,.F.);
#47875=ORIENTED_EDGE('',*,*,#35909,.T.);
#47876=ORIENTED_EDGE('',*,*,#35910,.F.);
#47877=ORIENTED_EDGE('',*,*,#35602,.T.);
#47878=ORIENTED_EDGE('',*,*,#35910,.T.);
#47879=ORIENTED_EDGE('',*,*,#35911,.T.);
#47880=ORIENTED_EDGE('',*,*,#35912,.F.);
#47881=ORIENTED_EDGE('',*,*,#35911,.F.);
#47882=ORIENTED_EDGE('',*,*,#35909,.F.);
#47883=ORIENTED_EDGE('',*,*,#35913,.F.);
#47884=ORIENTED_EDGE('',*,*,#35914,.F.);
#47885=ORIENTED_EDGE('',*,*,#35604,.T.);
#47886=ORIENTED_EDGE('',*,*,#35915,.F.);
#47887=ORIENTED_EDGE('',*,*,#35916,.T.);
#47888=ORIENTED_EDGE('',*,*,#35917,.F.);
#47889=ORIENTED_EDGE('',*,*,#35605,.T.);
#47890=ORIENTED_EDGE('',*,*,#35917,.T.);
#47891=ORIENTED_EDGE('',*,*,#35918,.T.);
#47892=ORIENTED_EDGE('',*,*,#35919,.F.);
#47893=ORIENTED_EDGE('',*,*,#35918,.F.);
#47894=ORIENTED_EDGE('',*,*,#35916,.F.);
#47895=ORIENTED_EDGE('',*,*,#35920,.F.);
#47896=ORIENTED_EDGE('',*,*,#35921,.F.);
#47897=ORIENTED_EDGE('',*,*,#35607,.T.);
#47898=ORIENTED_EDGE('',*,*,#35922,.F.);
#47899=ORIENTED_EDGE('',*,*,#35923,.T.);
#47900=ORIENTED_EDGE('',*,*,#35924,.F.);
#47901=ORIENTED_EDGE('',*,*,#35608,.T.);
#47902=ORIENTED_EDGE('',*,*,#35924,.T.);
#47903=ORIENTED_EDGE('',*,*,#35925,.T.);
#47904=ORIENTED_EDGE('',*,*,#35926,.F.);
#47905=ORIENTED_EDGE('',*,*,#35925,.F.);
#47906=ORIENTED_EDGE('',*,*,#35923,.F.);
#47907=ORIENTED_EDGE('',*,*,#35927,.F.);
#47908=ORIENTED_EDGE('',*,*,#35928,.F.);
#47909=ORIENTED_EDGE('',*,*,#35610,.T.);
#47910=ORIENTED_EDGE('',*,*,#35929,.F.);
#47911=ORIENTED_EDGE('',*,*,#35930,.T.);
#47912=ORIENTED_EDGE('',*,*,#35931,.F.);
#47913=ORIENTED_EDGE('',*,*,#35611,.T.);
#47914=ORIENTED_EDGE('',*,*,#35931,.T.);
#47915=ORIENTED_EDGE('',*,*,#35932,.T.);
#47916=ORIENTED_EDGE('',*,*,#35933,.F.);
#47917=ORIENTED_EDGE('',*,*,#35932,.F.);
#47918=ORIENTED_EDGE('',*,*,#35930,.F.);
#47919=ORIENTED_EDGE('',*,*,#35934,.F.);
#47920=ORIENTED_EDGE('',*,*,#35935,.F.);
#47921=ORIENTED_EDGE('',*,*,#35613,.T.);
#47922=ORIENTED_EDGE('',*,*,#35936,.F.);
#47923=ORIENTED_EDGE('',*,*,#35937,.T.);
#47924=ORIENTED_EDGE('',*,*,#35938,.F.);
#47925=ORIENTED_EDGE('',*,*,#35614,.T.);
#47926=ORIENTED_EDGE('',*,*,#35938,.T.);
#47927=ORIENTED_EDGE('',*,*,#35939,.T.);
#47928=ORIENTED_EDGE('',*,*,#35940,.F.);
#47929=ORIENTED_EDGE('',*,*,#35939,.F.);
#47930=ORIENTED_EDGE('',*,*,#35937,.F.);
#47931=ORIENTED_EDGE('',*,*,#35941,.F.);
#47932=ORIENTED_EDGE('',*,*,#35942,.F.);
#47933=ORIENTED_EDGE('',*,*,#35616,.T.);
#47934=ORIENTED_EDGE('',*,*,#35943,.F.);
#47935=ORIENTED_EDGE('',*,*,#35944,.T.);
#47936=ORIENTED_EDGE('',*,*,#35945,.F.);
#47937=ORIENTED_EDGE('',*,*,#35617,.T.);
#47938=ORIENTED_EDGE('',*,*,#35945,.T.);
#47939=ORIENTED_EDGE('',*,*,#35946,.T.);
#47940=ORIENTED_EDGE('',*,*,#35947,.F.);
#47941=ORIENTED_EDGE('',*,*,#35946,.F.);
#47942=ORIENTED_EDGE('',*,*,#35944,.F.);
#47943=ORIENTED_EDGE('',*,*,#35948,.F.);
#47944=ORIENTED_EDGE('',*,*,#35949,.F.);
#47945=ORIENTED_EDGE('',*,*,#35619,.T.);
#47946=ORIENTED_EDGE('',*,*,#35950,.F.);
#47947=ORIENTED_EDGE('',*,*,#35951,.T.);
#47948=ORIENTED_EDGE('',*,*,#35952,.F.);
#47949=ORIENTED_EDGE('',*,*,#35620,.T.);
#47950=ORIENTED_EDGE('',*,*,#35952,.T.);
#47951=ORIENTED_EDGE('',*,*,#35953,.T.);
#47952=ORIENTED_EDGE('',*,*,#35954,.F.);
#47953=ORIENTED_EDGE('',*,*,#35953,.F.);
#47954=ORIENTED_EDGE('',*,*,#35951,.F.);
#47955=ORIENTED_EDGE('',*,*,#35955,.F.);
#47956=ORIENTED_EDGE('',*,*,#35956,.F.);
#47957=ORIENTED_EDGE('',*,*,#35622,.T.);
#47958=ORIENTED_EDGE('',*,*,#35957,.F.);
#47959=ORIENTED_EDGE('',*,*,#35958,.T.);
#47960=ORIENTED_EDGE('',*,*,#35959,.F.);
#47961=ORIENTED_EDGE('',*,*,#35623,.T.);
#47962=ORIENTED_EDGE('',*,*,#35959,.T.);
#47963=ORIENTED_EDGE('',*,*,#35960,.T.);
#47964=ORIENTED_EDGE('',*,*,#35961,.F.);
#47965=ORIENTED_EDGE('',*,*,#35960,.F.);
#47966=ORIENTED_EDGE('',*,*,#35958,.F.);
#47967=ORIENTED_EDGE('',*,*,#35962,.F.);
#47968=ORIENTED_EDGE('',*,*,#35963,.F.);
#47969=ORIENTED_EDGE('',*,*,#35625,.T.);
#47970=ORIENTED_EDGE('',*,*,#35964,.F.);
#47971=ORIENTED_EDGE('',*,*,#34447,.T.);
#47972=ORIENTED_EDGE('',*,*,#35965,.F.);
#47973=ORIENTED_EDGE('',*,*,#35626,.T.);
#47974=ORIENTED_EDGE('',*,*,#35965,.T.);
#47975=ORIENTED_EDGE('',*,*,#34446,.T.);
#47976=ORIENTED_EDGE('',*,*,#35966,.F.);
#47977=ORIENTED_EDGE('',*,*,#35628,.T.);
#47978=ORIENTED_EDGE('',*,*,#35967,.F.);
#47979=ORIENTED_EDGE('',*,*,#35968,.T.);
#47980=ORIENTED_EDGE('',*,*,#35969,.F.);
#47981=ORIENTED_EDGE('',*,*,#35629,.T.);
#47982=ORIENTED_EDGE('',*,*,#35969,.T.);
#47983=ORIENTED_EDGE('',*,*,#35970,.T.);
#47984=ORIENTED_EDGE('',*,*,#35971,.F.);
#47985=ORIENTED_EDGE('',*,*,#35970,.F.);
#47986=ORIENTED_EDGE('',*,*,#35968,.F.);
#47987=ORIENTED_EDGE('',*,*,#35972,.F.);
#47988=ORIENTED_EDGE('',*,*,#35973,.F.);
#47989=ORIENTED_EDGE('',*,*,#35631,.T.);
#47990=ORIENTED_EDGE('',*,*,#35974,.F.);
#47991=ORIENTED_EDGE('',*,*,#35975,.T.);
#47992=ORIENTED_EDGE('',*,*,#35976,.F.);
#47993=ORIENTED_EDGE('',*,*,#35632,.T.);
#47994=ORIENTED_EDGE('',*,*,#35976,.T.);
#47995=ORIENTED_EDGE('',*,*,#35977,.T.);
#47996=ORIENTED_EDGE('',*,*,#35978,.F.);
#47997=ORIENTED_EDGE('',*,*,#35977,.F.);
#47998=ORIENTED_EDGE('',*,*,#35975,.F.);
#47999=ORIENTED_EDGE('',*,*,#35979,.F.);
#48000=ORIENTED_EDGE('',*,*,#35980,.F.);
#48001=ORIENTED_EDGE('',*,*,#35634,.T.);
#48002=ORIENTED_EDGE('',*,*,#35981,.F.);
#48003=ORIENTED_EDGE('',*,*,#35982,.T.);
#48004=ORIENTED_EDGE('',*,*,#35983,.F.);
#48005=ORIENTED_EDGE('',*,*,#35635,.T.);
#48006=ORIENTED_EDGE('',*,*,#35983,.T.);
#48007=ORIENTED_EDGE('',*,*,#35984,.T.);
#48008=ORIENTED_EDGE('',*,*,#35985,.F.);
#48009=ORIENTED_EDGE('',*,*,#35984,.F.);
#48010=ORIENTED_EDGE('',*,*,#35982,.F.);
#48011=ORIENTED_EDGE('',*,*,#35986,.F.);
#48012=ORIENTED_EDGE('',*,*,#35987,.F.);
#48013=ORIENTED_EDGE('',*,*,#35637,.T.);
#48014=ORIENTED_EDGE('',*,*,#35988,.F.);
#48015=ORIENTED_EDGE('',*,*,#35989,.T.);
#48016=ORIENTED_EDGE('',*,*,#35990,.F.);
#48017=ORIENTED_EDGE('',*,*,#35638,.T.);
#48018=ORIENTED_EDGE('',*,*,#35990,.T.);
#48019=ORIENTED_EDGE('',*,*,#35991,.T.);
#48020=ORIENTED_EDGE('',*,*,#35992,.F.);
#48021=ORIENTED_EDGE('',*,*,#35991,.F.);
#48022=ORIENTED_EDGE('',*,*,#35989,.F.);
#48023=ORIENTED_EDGE('',*,*,#35993,.F.);
#48024=ORIENTED_EDGE('',*,*,#35994,.F.);
#48025=ORIENTED_EDGE('',*,*,#35640,.T.);
#48026=ORIENTED_EDGE('',*,*,#35995,.F.);
#48027=ORIENTED_EDGE('',*,*,#35996,.T.);
#48028=ORIENTED_EDGE('',*,*,#35997,.F.);
#48029=ORIENTED_EDGE('',*,*,#35641,.T.);
#48030=ORIENTED_EDGE('',*,*,#35997,.T.);
#48031=ORIENTED_EDGE('',*,*,#35998,.T.);
#48032=ORIENTED_EDGE('',*,*,#35999,.F.);
#48033=ORIENTED_EDGE('',*,*,#35998,.F.);
#48034=ORIENTED_EDGE('',*,*,#35996,.F.);
#48035=ORIENTED_EDGE('',*,*,#36000,.F.);
#48036=ORIENTED_EDGE('',*,*,#36001,.F.);
#48037=ORIENTED_EDGE('',*,*,#35643,.T.);
#48038=ORIENTED_EDGE('',*,*,#36002,.F.);
#48039=ORIENTED_EDGE('',*,*,#36003,.T.);
#48040=ORIENTED_EDGE('',*,*,#36004,.F.);
#48041=ORIENTED_EDGE('',*,*,#35644,.T.);
#48042=ORIENTED_EDGE('',*,*,#36004,.T.);
#48043=ORIENTED_EDGE('',*,*,#36005,.T.);
#48044=ORIENTED_EDGE('',*,*,#36006,.F.);
#48045=ORIENTED_EDGE('',*,*,#36005,.F.);
#48046=ORIENTED_EDGE('',*,*,#36003,.F.);
#48047=ORIENTED_EDGE('',*,*,#36007,.F.);
#48048=ORIENTED_EDGE('',*,*,#36008,.F.);
#48049=ORIENTED_EDGE('',*,*,#35646,.T.);
#48050=ORIENTED_EDGE('',*,*,#36009,.F.);
#48051=ORIENTED_EDGE('',*,*,#36010,.T.);
#48052=ORIENTED_EDGE('',*,*,#36011,.F.);
#48053=ORIENTED_EDGE('',*,*,#35647,.T.);
#48054=ORIENTED_EDGE('',*,*,#36011,.T.);
#48055=ORIENTED_EDGE('',*,*,#36012,.T.);
#48056=ORIENTED_EDGE('',*,*,#36013,.F.);
#48057=ORIENTED_EDGE('',*,*,#36012,.F.);
#48058=ORIENTED_EDGE('',*,*,#36010,.F.);
#48059=ORIENTED_EDGE('',*,*,#36014,.F.);
#48060=ORIENTED_EDGE('',*,*,#36015,.F.);
#48061=ORIENTED_EDGE('',*,*,#35649,.T.);
#48062=ORIENTED_EDGE('',*,*,#36016,.F.);
#48063=ORIENTED_EDGE('',*,*,#36017,.T.);
#48064=ORIENTED_EDGE('',*,*,#36018,.F.);
#48065=ORIENTED_EDGE('',*,*,#35650,.T.);
#48066=ORIENTED_EDGE('',*,*,#36018,.T.);
#48067=ORIENTED_EDGE('',*,*,#36019,.T.);
#48068=ORIENTED_EDGE('',*,*,#36020,.F.);
#48069=ORIENTED_EDGE('',*,*,#36019,.F.);
#48070=ORIENTED_EDGE('',*,*,#36017,.F.);
#48071=ORIENTED_EDGE('',*,*,#36021,.F.);
#48072=ORIENTED_EDGE('',*,*,#36022,.F.);
#48073=ORIENTED_EDGE('',*,*,#35652,.T.);
#48074=ORIENTED_EDGE('',*,*,#36023,.F.);
#48075=ORIENTED_EDGE('',*,*,#36024,.T.);
#48076=ORIENTED_EDGE('',*,*,#36025,.F.);
#48077=ORIENTED_EDGE('',*,*,#35653,.T.);
#48078=ORIENTED_EDGE('',*,*,#36025,.T.);
#48079=ORIENTED_EDGE('',*,*,#36026,.T.);
#48080=ORIENTED_EDGE('',*,*,#36027,.F.);
#48081=ORIENTED_EDGE('',*,*,#36026,.F.);
#48082=ORIENTED_EDGE('',*,*,#36024,.F.);
#48083=ORIENTED_EDGE('',*,*,#36028,.F.);
#48084=ORIENTED_EDGE('',*,*,#36029,.F.);
#48085=ORIENTED_EDGE('',*,*,#35655,.T.);
#48086=ORIENTED_EDGE('',*,*,#36030,.F.);
#48087=ORIENTED_EDGE('',*,*,#36031,.T.);
#48088=ORIENTED_EDGE('',*,*,#36032,.F.);
#48089=ORIENTED_EDGE('',*,*,#35656,.T.);
#48090=ORIENTED_EDGE('',*,*,#36032,.T.);
#48091=ORIENTED_EDGE('',*,*,#36033,.T.);
#48092=ORIENTED_EDGE('',*,*,#36034,.F.);
#48093=ORIENTED_EDGE('',*,*,#36033,.F.);
#48094=ORIENTED_EDGE('',*,*,#36031,.F.);
#48095=ORIENTED_EDGE('',*,*,#36035,.F.);
#48096=ORIENTED_EDGE('',*,*,#36036,.F.);
#48097=ORIENTED_EDGE('',*,*,#35658,.T.);
#48098=ORIENTED_EDGE('',*,*,#36037,.F.);
#48099=ORIENTED_EDGE('',*,*,#36038,.T.);
#48100=ORIENTED_EDGE('',*,*,#36039,.F.);
#48101=ORIENTED_EDGE('',*,*,#35659,.T.);
#48102=ORIENTED_EDGE('',*,*,#36039,.T.);
#48103=ORIENTED_EDGE('',*,*,#36040,.T.);
#48104=ORIENTED_EDGE('',*,*,#36041,.F.);
#48105=ORIENTED_EDGE('',*,*,#36040,.F.);
#48106=ORIENTED_EDGE('',*,*,#36038,.F.);
#48107=ORIENTED_EDGE('',*,*,#36042,.F.);
#48108=ORIENTED_EDGE('',*,*,#36043,.F.);
#48109=ORIENTED_EDGE('',*,*,#35661,.T.);
#48110=ORIENTED_EDGE('',*,*,#36044,.F.);
#48111=ORIENTED_EDGE('',*,*,#36045,.T.);
#48112=ORIENTED_EDGE('',*,*,#36046,.F.);
#48113=ORIENTED_EDGE('',*,*,#35662,.T.);
#48114=ORIENTED_EDGE('',*,*,#36046,.T.);
#48115=ORIENTED_EDGE('',*,*,#36047,.T.);
#48116=ORIENTED_EDGE('',*,*,#36048,.F.);
#48117=ORIENTED_EDGE('',*,*,#36047,.F.);
#48118=ORIENTED_EDGE('',*,*,#36045,.F.);
#48119=ORIENTED_EDGE('',*,*,#36049,.F.);
#48120=ORIENTED_EDGE('',*,*,#36050,.F.);
#48121=ORIENTED_EDGE('',*,*,#35664,.T.);
#48122=ORIENTED_EDGE('',*,*,#36051,.F.);
#48123=ORIENTED_EDGE('',*,*,#36052,.T.);
#48124=ORIENTED_EDGE('',*,*,#36053,.F.);
#48125=ORIENTED_EDGE('',*,*,#35665,.T.);
#48126=ORIENTED_EDGE('',*,*,#36053,.T.);
#48127=ORIENTED_EDGE('',*,*,#36054,.T.);
#48128=ORIENTED_EDGE('',*,*,#36055,.F.);
#48129=ORIENTED_EDGE('',*,*,#36054,.F.);
#48130=ORIENTED_EDGE('',*,*,#36052,.F.);
#48131=ORIENTED_EDGE('',*,*,#36056,.F.);
#48132=ORIENTED_EDGE('',*,*,#36057,.F.);
#48133=ORIENTED_EDGE('',*,*,#35667,.T.);
#48134=ORIENTED_EDGE('',*,*,#36058,.F.);
#48135=ORIENTED_EDGE('',*,*,#36059,.T.);
#48136=ORIENTED_EDGE('',*,*,#36060,.F.);
#48137=ORIENTED_EDGE('',*,*,#35668,.T.);
#48138=ORIENTED_EDGE('',*,*,#36060,.T.);
#48139=ORIENTED_EDGE('',*,*,#36061,.T.);
#48140=ORIENTED_EDGE('',*,*,#36062,.F.);
#48141=ORIENTED_EDGE('',*,*,#36061,.F.);
#48142=ORIENTED_EDGE('',*,*,#36059,.F.);
#48143=ORIENTED_EDGE('',*,*,#36063,.F.);
#48144=ORIENTED_EDGE('',*,*,#36064,.F.);
#48145=ORIENTED_EDGE('',*,*,#35871,.F.);
#48146=ORIENTED_EDGE('',*,*,#36065,.F.);
#48147=ORIENTED_EDGE('',*,*,#36066,.F.);
#48148=ORIENTED_EDGE('',*,*,#36067,.F.);
#48149=ORIENTED_EDGE('',*,*,#35670,.T.);
#48150=ORIENTED_EDGE('',*,*,#36068,.F.);
#48151=ORIENTED_EDGE('',*,*,#36065,.T.);
#48152=ORIENTED_EDGE('',*,*,#35870,.T.);
#48153=ORIENTED_EDGE('',*,*,#36069,.F.);
#48154=ORIENTED_EDGE('',*,*,#35672,.T.);
#48155=ORIENTED_EDGE('',*,*,#35867,.T.);
#48156=ORIENTED_EDGE('',*,*,#36070,.F.);
#48157=ORIENTED_EDGE('',*,*,#36071,.F.);
#48158=ORIENTED_EDGE('',*,*,#36072,.F.);
#48159=ORIENTED_EDGE('',*,*,#35677,.T.);
#48160=ORIENTED_EDGE('',*,*,#35676,.T.);
#48161=ORIENTED_EDGE('',*,*,#36073,.F.);
#48162=ORIENTED_EDGE('',*,*,#35680,.T.);
#48163=ORIENTED_EDGE('',*,*,#35678,.T.);
#48164=ORIENTED_EDGE('',*,*,#36072,.T.);
#48165=ORIENTED_EDGE('',*,*,#36074,.F.);
#48166=ORIENTED_EDGE('',*,*,#36075,.F.);
#48167=ORIENTED_EDGE('',*,*,#35684,.T.);
#48168=ORIENTED_EDGE('',*,*,#35683,.T.);
#48169=ORIENTED_EDGE('',*,*,#36076,.F.);
#48170=ORIENTED_EDGE('',*,*,#35687,.T.);
#48171=ORIENTED_EDGE('',*,*,#35685,.T.);
#48172=ORIENTED_EDGE('',*,*,#36075,.T.);
#48173=ORIENTED_EDGE('',*,*,#36077,.F.);
#48174=ORIENTED_EDGE('',*,*,#36078,.F.);
#48175=ORIENTED_EDGE('',*,*,#35691,.T.);
#48176=ORIENTED_EDGE('',*,*,#35690,.T.);
#48177=ORIENTED_EDGE('',*,*,#36079,.F.);
#48178=ORIENTED_EDGE('',*,*,#35694,.T.);
#48179=ORIENTED_EDGE('',*,*,#35692,.T.);
#48180=ORIENTED_EDGE('',*,*,#36078,.T.);
#48181=ORIENTED_EDGE('',*,*,#36080,.F.);
#48182=ORIENTED_EDGE('',*,*,#36081,.F.);
#48183=ORIENTED_EDGE('',*,*,#35698,.T.);
#48184=ORIENTED_EDGE('',*,*,#35697,.T.);
#48185=ORIENTED_EDGE('',*,*,#36082,.F.);
#48186=ORIENTED_EDGE('',*,*,#35701,.T.);
#48187=ORIENTED_EDGE('',*,*,#35699,.T.);
#48188=ORIENTED_EDGE('',*,*,#36081,.T.);
#48189=ORIENTED_EDGE('',*,*,#36083,.F.);
#48190=ORIENTED_EDGE('',*,*,#36084,.F.);
#48191=ORIENTED_EDGE('',*,*,#35705,.T.);
#48192=ORIENTED_EDGE('',*,*,#35704,.T.);
#48193=ORIENTED_EDGE('',*,*,#36085,.F.);
#48194=ORIENTED_EDGE('',*,*,#35708,.T.);
#48195=ORIENTED_EDGE('',*,*,#35706,.T.);
#48196=ORIENTED_EDGE('',*,*,#36084,.T.);
#48197=ORIENTED_EDGE('',*,*,#36086,.F.);
#48198=ORIENTED_EDGE('',*,*,#36087,.F.);
#48199=ORIENTED_EDGE('',*,*,#35712,.T.);
#48200=ORIENTED_EDGE('',*,*,#35711,.T.);
#48201=ORIENTED_EDGE('',*,*,#36088,.F.);
#48202=ORIENTED_EDGE('',*,*,#35715,.T.);
#48203=ORIENTED_EDGE('',*,*,#35713,.T.);
#48204=ORIENTED_EDGE('',*,*,#36087,.T.);
#48205=ORIENTED_EDGE('',*,*,#36089,.F.);
#48206=ORIENTED_EDGE('',*,*,#36090,.F.);
#48207=ORIENTED_EDGE('',*,*,#34451,.T.);
#48208=ORIENTED_EDGE('',*,*,#35717,.T.);
#48209=ORIENTED_EDGE('',*,*,#36091,.F.);
#48210=ORIENTED_EDGE('',*,*,#35718,.T.);
#48211=ORIENTED_EDGE('',*,*,#34452,.T.);
#48212=ORIENTED_EDGE('',*,*,#36090,.T.);
#48213=ORIENTED_EDGE('',*,*,#36092,.F.);
#48214=ORIENTED_EDGE('',*,*,#36093,.F.);
#48215=ORIENTED_EDGE('',*,*,#35722,.T.);
#48216=ORIENTED_EDGE('',*,*,#35721,.T.);
#48217=ORIENTED_EDGE('',*,*,#36094,.F.);
#48218=ORIENTED_EDGE('',*,*,#35725,.T.);
#48219=ORIENTED_EDGE('',*,*,#35723,.T.);
#48220=ORIENTED_EDGE('',*,*,#36093,.T.);
#48221=ORIENTED_EDGE('',*,*,#36095,.F.);
#48222=ORIENTED_EDGE('',*,*,#36096,.F.);
#48223=ORIENTED_EDGE('',*,*,#35729,.T.);
#48224=ORIENTED_EDGE('',*,*,#35728,.T.);
#48225=ORIENTED_EDGE('',*,*,#36097,.F.);
#48226=ORIENTED_EDGE('',*,*,#35732,.T.);
#48227=ORIENTED_EDGE('',*,*,#35730,.T.);
#48228=ORIENTED_EDGE('',*,*,#36096,.T.);
#48229=ORIENTED_EDGE('',*,*,#36098,.F.);
#48230=ORIENTED_EDGE('',*,*,#36099,.F.);
#48231=ORIENTED_EDGE('',*,*,#35736,.T.);
#48232=ORIENTED_EDGE('',*,*,#35735,.T.);
#48233=ORIENTED_EDGE('',*,*,#36100,.F.);
#48234=ORIENTED_EDGE('',*,*,#35739,.T.);
#48235=ORIENTED_EDGE('',*,*,#35737,.T.);
#48236=ORIENTED_EDGE('',*,*,#36099,.T.);
#48237=ORIENTED_EDGE('',*,*,#36101,.F.);
#48238=ORIENTED_EDGE('',*,*,#36102,.F.);
#48239=ORIENTED_EDGE('',*,*,#35743,.T.);
#48240=ORIENTED_EDGE('',*,*,#35742,.T.);
#48241=ORIENTED_EDGE('',*,*,#36103,.F.);
#48242=ORIENTED_EDGE('',*,*,#35746,.T.);
#48243=ORIENTED_EDGE('',*,*,#35744,.T.);
#48244=ORIENTED_EDGE('',*,*,#36102,.T.);
#48245=ORIENTED_EDGE('',*,*,#36104,.F.);
#48246=ORIENTED_EDGE('',*,*,#36105,.F.);
#48247=ORIENTED_EDGE('',*,*,#35750,.T.);
#48248=ORIENTED_EDGE('',*,*,#35749,.T.);
#48249=ORIENTED_EDGE('',*,*,#36106,.F.);
#48250=ORIENTED_EDGE('',*,*,#35753,.T.);
#48251=ORIENTED_EDGE('',*,*,#35751,.T.);
#48252=ORIENTED_EDGE('',*,*,#36105,.T.);
#48253=ORIENTED_EDGE('',*,*,#36107,.F.);
#48254=ORIENTED_EDGE('',*,*,#36108,.F.);
#48255=ORIENTED_EDGE('',*,*,#35757,.T.);
#48256=ORIENTED_EDGE('',*,*,#35756,.T.);
#48257=ORIENTED_EDGE('',*,*,#36109,.F.);
#48258=ORIENTED_EDGE('',*,*,#35760,.T.);
#48259=ORIENTED_EDGE('',*,*,#35758,.T.);
#48260=ORIENTED_EDGE('',*,*,#36108,.T.);
#48261=ORIENTED_EDGE('',*,*,#36110,.F.);
#48262=ORIENTED_EDGE('',*,*,#36111,.F.);
#48263=ORIENTED_EDGE('',*,*,#35764,.T.);
#48264=ORIENTED_EDGE('',*,*,#35763,.T.);
#48265=ORIENTED_EDGE('',*,*,#36112,.F.);
#48266=ORIENTED_EDGE('',*,*,#35767,.T.);
#48267=ORIENTED_EDGE('',*,*,#35765,.T.);
#48268=ORIENTED_EDGE('',*,*,#36111,.T.);
#48269=ORIENTED_EDGE('',*,*,#36113,.F.);
#48270=ORIENTED_EDGE('',*,*,#36114,.F.);
#48271=ORIENTED_EDGE('',*,*,#35771,.T.);
#48272=ORIENTED_EDGE('',*,*,#35770,.T.);
#48273=ORIENTED_EDGE('',*,*,#36115,.F.);
#48274=ORIENTED_EDGE('',*,*,#35774,.T.);
#48275=ORIENTED_EDGE('',*,*,#35772,.T.);
#48276=ORIENTED_EDGE('',*,*,#36114,.T.);
#48277=ORIENTED_EDGE('',*,*,#36116,.F.);
#48278=ORIENTED_EDGE('',*,*,#36117,.F.);
#48279=ORIENTED_EDGE('',*,*,#35778,.T.);
#48280=ORIENTED_EDGE('',*,*,#35777,.T.);
#48281=ORIENTED_EDGE('',*,*,#36118,.F.);
#48282=ORIENTED_EDGE('',*,*,#35781,.T.);
#48283=ORIENTED_EDGE('',*,*,#35779,.T.);
#48284=ORIENTED_EDGE('',*,*,#36117,.T.);
#48285=ORIENTED_EDGE('',*,*,#36119,.F.);
#48286=ORIENTED_EDGE('',*,*,#36120,.F.);
#48287=ORIENTED_EDGE('',*,*,#35785,.T.);
#48288=ORIENTED_EDGE('',*,*,#35784,.T.);
#48289=ORIENTED_EDGE('',*,*,#36121,.F.);
#48290=ORIENTED_EDGE('',*,*,#35788,.T.);
#48291=ORIENTED_EDGE('',*,*,#35786,.T.);
#48292=ORIENTED_EDGE('',*,*,#36120,.T.);
#48293=ORIENTED_EDGE('',*,*,#36122,.F.);
#48294=ORIENTED_EDGE('',*,*,#36123,.F.);
#48295=ORIENTED_EDGE('',*,*,#35792,.T.);
#48296=ORIENTED_EDGE('',*,*,#35791,.T.);
#48297=ORIENTED_EDGE('',*,*,#36124,.F.);
#48298=ORIENTED_EDGE('',*,*,#35795,.T.);
#48299=ORIENTED_EDGE('',*,*,#35793,.T.);
#48300=ORIENTED_EDGE('',*,*,#36123,.T.);
#48301=ORIENTED_EDGE('',*,*,#36125,.F.);
#48302=ORIENTED_EDGE('',*,*,#36126,.F.);
#48303=ORIENTED_EDGE('',*,*,#35799,.T.);
#48304=ORIENTED_EDGE('',*,*,#35798,.T.);
#48305=ORIENTED_EDGE('',*,*,#36127,.F.);
#48306=ORIENTED_EDGE('',*,*,#35802,.T.);
#48307=ORIENTED_EDGE('',*,*,#35800,.T.);
#48308=ORIENTED_EDGE('',*,*,#36126,.T.);
#48309=ORIENTED_EDGE('',*,*,#36128,.F.);
#48310=ORIENTED_EDGE('',*,*,#36129,.F.);
#48311=ORIENTED_EDGE('',*,*,#35806,.T.);
#48312=ORIENTED_EDGE('',*,*,#35805,.T.);
#48313=ORIENTED_EDGE('',*,*,#36130,.F.);
#48314=ORIENTED_EDGE('',*,*,#35809,.T.);
#48315=ORIENTED_EDGE('',*,*,#35807,.T.);
#48316=ORIENTED_EDGE('',*,*,#36129,.T.);
#48317=ORIENTED_EDGE('',*,*,#36131,.F.);
#48318=ORIENTED_EDGE('',*,*,#36132,.F.);
#48319=ORIENTED_EDGE('',*,*,#35813,.T.);
#48320=ORIENTED_EDGE('',*,*,#35812,.T.);
#48321=ORIENTED_EDGE('',*,*,#36133,.F.);
#48322=ORIENTED_EDGE('',*,*,#35816,.T.);
#48323=ORIENTED_EDGE('',*,*,#35814,.T.);
#48324=ORIENTED_EDGE('',*,*,#36132,.T.);
#48325=ORIENTED_EDGE('',*,*,#36134,.F.);
#48326=ORIENTED_EDGE('',*,*,#36135,.F.);
#48327=ORIENTED_EDGE('',*,*,#35820,.T.);
#48328=ORIENTED_EDGE('',*,*,#35819,.T.);
#48329=ORIENTED_EDGE('',*,*,#36136,.F.);
#48330=ORIENTED_EDGE('',*,*,#35823,.T.);
#48331=ORIENTED_EDGE('',*,*,#35821,.T.);
#48332=ORIENTED_EDGE('',*,*,#36135,.T.);
#48333=ORIENTED_EDGE('',*,*,#36137,.F.);
#48334=ORIENTED_EDGE('',*,*,#36138,.F.);
#48335=ORIENTED_EDGE('',*,*,#35827,.T.);
#48336=ORIENTED_EDGE('',*,*,#35826,.T.);
#48337=ORIENTED_EDGE('',*,*,#36139,.F.);
#48338=ORIENTED_EDGE('',*,*,#35830,.T.);
#48339=ORIENTED_EDGE('',*,*,#35828,.T.);
#48340=ORIENTED_EDGE('',*,*,#36138,.T.);
#48341=ORIENTED_EDGE('',*,*,#36140,.F.);
#48342=ORIENTED_EDGE('',*,*,#36141,.F.);
#48343=ORIENTED_EDGE('',*,*,#35836,.T.);
#48344=ORIENTED_EDGE('',*,*,#35833,.T.);
#48345=ORIENTED_EDGE('',*,*,#35837,.T.);
#48346=ORIENTED_EDGE('',*,*,#36141,.T.);
#48347=ORIENTED_EDGE('',*,*,#36142,.F.);
#48348=ORIENTED_EDGE('',*,*,#35835,.T.);
#48349=ORIENTED_EDGE('',*,*,#35842,.T.);
#48350=ORIENTED_EDGE('',*,*,#35838,.T.);
#48351=ORIENTED_EDGE('',*,*,#36143,.F.);
#48352=ORIENTED_EDGE('',*,*,#36144,.F.);
#48353=ORIENTED_EDGE('',*,*,#36145,.F.);
#48354=ORIENTED_EDGE('',*,*,#35844,.T.);
#48355=ORIENTED_EDGE('',*,*,#35843,.T.);
#48356=ORIENTED_EDGE('',*,*,#36144,.T.);
#48357=ORIENTED_EDGE('',*,*,#36146,.F.);
#48358=ORIENTED_EDGE('',*,*,#36147,.F.);
#48359=ORIENTED_EDGE('',*,*,#35848,.T.);
#48360=ORIENTED_EDGE('',*,*,#35847,.T.);
#48361=ORIENTED_EDGE('',*,*,#36148,.F.);
#48362=ORIENTED_EDGE('',*,*,#35851,.T.);
#48363=ORIENTED_EDGE('',*,*,#35849,.T.);
#48364=ORIENTED_EDGE('',*,*,#36147,.T.);
#48365=ORIENTED_EDGE('',*,*,#36149,.F.);
#48366=ORIENTED_EDGE('',*,*,#36150,.F.);
#48367=ORIENTED_EDGE('',*,*,#35855,.T.);
#48368=ORIENTED_EDGE('',*,*,#35854,.T.);
#48369=ORIENTED_EDGE('',*,*,#36151,.F.);
#48370=ORIENTED_EDGE('',*,*,#35858,.T.);
#48371=ORIENTED_EDGE('',*,*,#35856,.T.);
#48372=ORIENTED_EDGE('',*,*,#36150,.T.);
#48373=ORIENTED_EDGE('',*,*,#36152,.F.);
#48374=ORIENTED_EDGE('',*,*,#36153,.F.);
#48375=ORIENTED_EDGE('',*,*,#35862,.T.);
#48376=ORIENTED_EDGE('',*,*,#35861,.T.);
#48377=ORIENTED_EDGE('',*,*,#36154,.F.);
#48378=ORIENTED_EDGE('',*,*,#35865,.T.);
#48379=ORIENTED_EDGE('',*,*,#35863,.T.);
#48380=ORIENTED_EDGE('',*,*,#36153,.T.);
#48381=ORIENTED_EDGE('',*,*,#36155,.F.);
#48382=ORIENTED_EDGE('',*,*,#36070,.T.);
#48383=ORIENTED_EDGE('',*,*,#35866,.T.);
#48384=ORIENTED_EDGE('',*,*,#35869,.T.);
#48385=ORIENTED_EDGE('',*,*,#36067,.T.);
#48386=ORIENTED_EDGE('',*,*,#36156,.F.);
#48387=ORIENTED_EDGE('',*,*,#36157,.F.);
#48388=ORIENTED_EDGE('',*,*,#35872,.T.);
#48389=ORIENTED_EDGE('',*,*,#36158,.F.);
#48390=ORIENTED_EDGE('',*,*,#36159,.F.);
#48391=ORIENTED_EDGE('',*,*,#35878,.T.);
#48392=ORIENTED_EDGE('',*,*,#35873,.T.);
#48393=ORIENTED_EDGE('',*,*,#35879,.T.);
#48394=ORIENTED_EDGE('',*,*,#36159,.T.);
#48395=ORIENTED_EDGE('',*,*,#36160,.F.);
#48396=ORIENTED_EDGE('',*,*,#35877,.T.);
#48397=ORIENTED_EDGE('',*,*,#35885,.T.);
#48398=ORIENTED_EDGE('',*,*,#35880,.T.);
#48399=ORIENTED_EDGE('',*,*,#36161,.F.);
#48400=ORIENTED_EDGE('',*,*,#36162,.F.);
#48401=ORIENTED_EDGE('',*,*,#35886,.T.);
#48402=ORIENTED_EDGE('',*,*,#36162,.T.);
#48403=ORIENTED_EDGE('',*,*,#36163,.F.);
#48404=ORIENTED_EDGE('',*,*,#35884,.T.);
#48405=ORIENTED_EDGE('',*,*,#35892,.T.);
#48406=ORIENTED_EDGE('',*,*,#35887,.T.);
#48407=ORIENTED_EDGE('',*,*,#36164,.F.);
#48408=ORIENTED_EDGE('',*,*,#36165,.F.);
#48409=ORIENTED_EDGE('',*,*,#35893,.T.);
#48410=ORIENTED_EDGE('',*,*,#36165,.T.);
#48411=ORIENTED_EDGE('',*,*,#36166,.F.);
#48412=ORIENTED_EDGE('',*,*,#35891,.T.);
#48413=ORIENTED_EDGE('',*,*,#35899,.T.);
#48414=ORIENTED_EDGE('',*,*,#35894,.T.);
#48415=ORIENTED_EDGE('',*,*,#36167,.F.);
#48416=ORIENTED_EDGE('',*,*,#36168,.F.);
#48417=ORIENTED_EDGE('',*,*,#35900,.T.);
#48418=ORIENTED_EDGE('',*,*,#36168,.T.);
#48419=ORIENTED_EDGE('',*,*,#36169,.F.);
#48420=ORIENTED_EDGE('',*,*,#35898,.T.);
#48421=ORIENTED_EDGE('',*,*,#35906,.T.);
#48422=ORIENTED_EDGE('',*,*,#35901,.T.);
#48423=ORIENTED_EDGE('',*,*,#36170,.F.);
#48424=ORIENTED_EDGE('',*,*,#36171,.F.);
#48425=ORIENTED_EDGE('',*,*,#35907,.T.);
#48426=ORIENTED_EDGE('',*,*,#36171,.T.);
#48427=ORIENTED_EDGE('',*,*,#36172,.F.);
#48428=ORIENTED_EDGE('',*,*,#35905,.T.);
#48429=ORIENTED_EDGE('',*,*,#35913,.T.);
#48430=ORIENTED_EDGE('',*,*,#35908,.T.);
#48431=ORIENTED_EDGE('',*,*,#36173,.F.);
#48432=ORIENTED_EDGE('',*,*,#36174,.F.);
#48433=ORIENTED_EDGE('',*,*,#35914,.T.);
#48434=ORIENTED_EDGE('',*,*,#36174,.T.);
#48435=ORIENTED_EDGE('',*,*,#36175,.F.);
#48436=ORIENTED_EDGE('',*,*,#35912,.T.);
#48437=ORIENTED_EDGE('',*,*,#35920,.T.);
#48438=ORIENTED_EDGE('',*,*,#35915,.T.);
#48439=ORIENTED_EDGE('',*,*,#36176,.F.);
#48440=ORIENTED_EDGE('',*,*,#36177,.F.);
#48441=ORIENTED_EDGE('',*,*,#35921,.T.);
#48442=ORIENTED_EDGE('',*,*,#36177,.T.);
#48443=ORIENTED_EDGE('',*,*,#36178,.F.);
#48444=ORIENTED_EDGE('',*,*,#35919,.T.);
#48445=ORIENTED_EDGE('',*,*,#35927,.T.);
#48446=ORIENTED_EDGE('',*,*,#35922,.T.);
#48447=ORIENTED_EDGE('',*,*,#36179,.F.);
#48448=ORIENTED_EDGE('',*,*,#36180,.F.);
#48449=ORIENTED_EDGE('',*,*,#35928,.T.);
#48450=ORIENTED_EDGE('',*,*,#36180,.T.);
#48451=ORIENTED_EDGE('',*,*,#36181,.F.);
#48452=ORIENTED_EDGE('',*,*,#35926,.T.);
#48453=ORIENTED_EDGE('',*,*,#35934,.T.);
#48454=ORIENTED_EDGE('',*,*,#35929,.T.);
#48455=ORIENTED_EDGE('',*,*,#36182,.F.);
#48456=ORIENTED_EDGE('',*,*,#36183,.F.);
#48457=ORIENTED_EDGE('',*,*,#35935,.T.);
#48458=ORIENTED_EDGE('',*,*,#36183,.T.);
#48459=ORIENTED_EDGE('',*,*,#36184,.F.);
#48460=ORIENTED_EDGE('',*,*,#35933,.T.);
#48461=ORIENTED_EDGE('',*,*,#35941,.T.);
#48462=ORIENTED_EDGE('',*,*,#35936,.T.);
#48463=ORIENTED_EDGE('',*,*,#36185,.F.);
#48464=ORIENTED_EDGE('',*,*,#36186,.F.);
#48465=ORIENTED_EDGE('',*,*,#35942,.T.);
#48466=ORIENTED_EDGE('',*,*,#36186,.T.);
#48467=ORIENTED_EDGE('',*,*,#36187,.F.);
#48468=ORIENTED_EDGE('',*,*,#35940,.T.);
#48469=ORIENTED_EDGE('',*,*,#35948,.T.);
#48470=ORIENTED_EDGE('',*,*,#35943,.T.);
#48471=ORIENTED_EDGE('',*,*,#36188,.F.);
#48472=ORIENTED_EDGE('',*,*,#36189,.F.);
#48473=ORIENTED_EDGE('',*,*,#35949,.T.);
#48474=ORIENTED_EDGE('',*,*,#36189,.T.);
#48475=ORIENTED_EDGE('',*,*,#36190,.F.);
#48476=ORIENTED_EDGE('',*,*,#35947,.T.);
#48477=ORIENTED_EDGE('',*,*,#35955,.T.);
#48478=ORIENTED_EDGE('',*,*,#35950,.T.);
#48479=ORIENTED_EDGE('',*,*,#36191,.F.);
#48480=ORIENTED_EDGE('',*,*,#36192,.F.);
#48481=ORIENTED_EDGE('',*,*,#35956,.T.);
#48482=ORIENTED_EDGE('',*,*,#36192,.T.);
#48483=ORIENTED_EDGE('',*,*,#36193,.F.);
#48484=ORIENTED_EDGE('',*,*,#35954,.T.);
#48485=ORIENTED_EDGE('',*,*,#35962,.T.);
#48486=ORIENTED_EDGE('',*,*,#35957,.T.);
#48487=ORIENTED_EDGE('',*,*,#36194,.F.);
#48488=ORIENTED_EDGE('',*,*,#36195,.F.);
#48489=ORIENTED_EDGE('',*,*,#35963,.T.);
#48490=ORIENTED_EDGE('',*,*,#36195,.T.);
#48491=ORIENTED_EDGE('',*,*,#36196,.F.);
#48492=ORIENTED_EDGE('',*,*,#35961,.T.);
#48493=ORIENTED_EDGE('',*,*,#34448,.T.);
#48494=ORIENTED_EDGE('',*,*,#35964,.T.);
#48495=ORIENTED_EDGE('',*,*,#36197,.F.);
#48496=ORIENTED_EDGE('',*,*,#36198,.F.);
#48497=ORIENTED_EDGE('',*,*,#34445,.T.);
#48498=ORIENTED_EDGE('',*,*,#36198,.T.);
#48499=ORIENTED_EDGE('',*,*,#36199,.F.);
#48500=ORIENTED_EDGE('',*,*,#35966,.T.);
#48501=ORIENTED_EDGE('',*,*,#35972,.T.);
#48502=ORIENTED_EDGE('',*,*,#35967,.T.);
#48503=ORIENTED_EDGE('',*,*,#36200,.F.);
#48504=ORIENTED_EDGE('',*,*,#36201,.F.);
#48505=ORIENTED_EDGE('',*,*,#35973,.T.);
#48506=ORIENTED_EDGE('',*,*,#36201,.T.);
#48507=ORIENTED_EDGE('',*,*,#36202,.F.);
#48508=ORIENTED_EDGE('',*,*,#35971,.T.);
#48509=ORIENTED_EDGE('',*,*,#35979,.T.);
#48510=ORIENTED_EDGE('',*,*,#35974,.T.);
#48511=ORIENTED_EDGE('',*,*,#36203,.F.);
#48512=ORIENTED_EDGE('',*,*,#36204,.F.);
#48513=ORIENTED_EDGE('',*,*,#35980,.T.);
#48514=ORIENTED_EDGE('',*,*,#36204,.T.);
#48515=ORIENTED_EDGE('',*,*,#36205,.F.);
#48516=ORIENTED_EDGE('',*,*,#35978,.T.);
#48517=ORIENTED_EDGE('',*,*,#35986,.T.);
#48518=ORIENTED_EDGE('',*,*,#35981,.T.);
#48519=ORIENTED_EDGE('',*,*,#36206,.F.);
#48520=ORIENTED_EDGE('',*,*,#36207,.F.);
#48521=ORIENTED_EDGE('',*,*,#35987,.T.);
#48522=ORIENTED_EDGE('',*,*,#36207,.T.);
#48523=ORIENTED_EDGE('',*,*,#36208,.F.);
#48524=ORIENTED_EDGE('',*,*,#35985,.T.);
#48525=ORIENTED_EDGE('',*,*,#35993,.T.);
#48526=ORIENTED_EDGE('',*,*,#35988,.T.);
#48527=ORIENTED_EDGE('',*,*,#36209,.F.);
#48528=ORIENTED_EDGE('',*,*,#36210,.F.);
#48529=ORIENTED_EDGE('',*,*,#35994,.T.);
#48530=ORIENTED_EDGE('',*,*,#36210,.T.);
#48531=ORIENTED_EDGE('',*,*,#36211,.F.);
#48532=ORIENTED_EDGE('',*,*,#35992,.T.);
#48533=ORIENTED_EDGE('',*,*,#36000,.T.);
#48534=ORIENTED_EDGE('',*,*,#35995,.T.);
#48535=ORIENTED_EDGE('',*,*,#36212,.F.);
#48536=ORIENTED_EDGE('',*,*,#36213,.F.);
#48537=ORIENTED_EDGE('',*,*,#36001,.T.);
#48538=ORIENTED_EDGE('',*,*,#36213,.T.);
#48539=ORIENTED_EDGE('',*,*,#36214,.F.);
#48540=ORIENTED_EDGE('',*,*,#35999,.T.);
#48541=ORIENTED_EDGE('',*,*,#36007,.T.);
#48542=ORIENTED_EDGE('',*,*,#36002,.T.);
#48543=ORIENTED_EDGE('',*,*,#36215,.F.);
#48544=ORIENTED_EDGE('',*,*,#36216,.F.);
#48545=ORIENTED_EDGE('',*,*,#36008,.T.);
#48546=ORIENTED_EDGE('',*,*,#36216,.T.);
#48547=ORIENTED_EDGE('',*,*,#36217,.F.);
#48548=ORIENTED_EDGE('',*,*,#36006,.T.);
#48549=ORIENTED_EDGE('',*,*,#36014,.T.);
#48550=ORIENTED_EDGE('',*,*,#36009,.T.);
#48551=ORIENTED_EDGE('',*,*,#36218,.F.);
#48552=ORIENTED_EDGE('',*,*,#36219,.F.);
#48553=ORIENTED_EDGE('',*,*,#36015,.T.);
#48554=ORIENTED_EDGE('',*,*,#36219,.T.);
#48555=ORIENTED_EDGE('',*,*,#36220,.F.);
#48556=ORIENTED_EDGE('',*,*,#36013,.T.);
#48557=ORIENTED_EDGE('',*,*,#36021,.T.);
#48558=ORIENTED_EDGE('',*,*,#36016,.T.);
#48559=ORIENTED_EDGE('',*,*,#36221,.F.);
#48560=ORIENTED_EDGE('',*,*,#36222,.F.);
#48561=ORIENTED_EDGE('',*,*,#36022,.T.);
#48562=ORIENTED_EDGE('',*,*,#36222,.T.);
#48563=ORIENTED_EDGE('',*,*,#36223,.F.);
#48564=ORIENTED_EDGE('',*,*,#36020,.T.);
#48565=ORIENTED_EDGE('',*,*,#36028,.T.);
#48566=ORIENTED_EDGE('',*,*,#36023,.T.);
#48567=ORIENTED_EDGE('',*,*,#36224,.F.);
#48568=ORIENTED_EDGE('',*,*,#36225,.F.);
#48569=ORIENTED_EDGE('',*,*,#36029,.T.);
#48570=ORIENTED_EDGE('',*,*,#36225,.T.);
#48571=ORIENTED_EDGE('',*,*,#36226,.F.);
#48572=ORIENTED_EDGE('',*,*,#36027,.T.);
#48573=ORIENTED_EDGE('',*,*,#36035,.T.);
#48574=ORIENTED_EDGE('',*,*,#36030,.T.);
#48575=ORIENTED_EDGE('',*,*,#36227,.F.);
#48576=ORIENTED_EDGE('',*,*,#36228,.F.);
#48577=ORIENTED_EDGE('',*,*,#36036,.T.);
#48578=ORIENTED_EDGE('',*,*,#36228,.T.);
#48579=ORIENTED_EDGE('',*,*,#36229,.F.);
#48580=ORIENTED_EDGE('',*,*,#36034,.T.);
#48581=ORIENTED_EDGE('',*,*,#36042,.T.);
#48582=ORIENTED_EDGE('',*,*,#36037,.T.);
#48583=ORIENTED_EDGE('',*,*,#36230,.F.);
#48584=ORIENTED_EDGE('',*,*,#36231,.F.);
#48585=ORIENTED_EDGE('',*,*,#36043,.T.);
#48586=ORIENTED_EDGE('',*,*,#36231,.T.);
#48587=ORIENTED_EDGE('',*,*,#36232,.F.);
#48588=ORIENTED_EDGE('',*,*,#36041,.T.);
#48589=ORIENTED_EDGE('',*,*,#36049,.T.);
#48590=ORIENTED_EDGE('',*,*,#36044,.T.);
#48591=ORIENTED_EDGE('',*,*,#36233,.F.);
#48592=ORIENTED_EDGE('',*,*,#36234,.F.);
#48593=ORIENTED_EDGE('',*,*,#36050,.T.);
#48594=ORIENTED_EDGE('',*,*,#36234,.T.);
#48595=ORIENTED_EDGE('',*,*,#36235,.F.);
#48596=ORIENTED_EDGE('',*,*,#36048,.T.);
#48597=ORIENTED_EDGE('',*,*,#36056,.T.);
#48598=ORIENTED_EDGE('',*,*,#36051,.T.);
#48599=ORIENTED_EDGE('',*,*,#36236,.F.);
#48600=ORIENTED_EDGE('',*,*,#36237,.F.);
#48601=ORIENTED_EDGE('',*,*,#36057,.T.);
#48602=ORIENTED_EDGE('',*,*,#36237,.T.);
#48603=ORIENTED_EDGE('',*,*,#36238,.F.);
#48604=ORIENTED_EDGE('',*,*,#36055,.T.);
#48605=ORIENTED_EDGE('',*,*,#36063,.T.);
#48606=ORIENTED_EDGE('',*,*,#36058,.T.);
#48607=ORIENTED_EDGE('',*,*,#36239,.F.);
#48608=ORIENTED_EDGE('',*,*,#36240,.F.);
#48609=ORIENTED_EDGE('',*,*,#36064,.T.);
#48610=ORIENTED_EDGE('',*,*,#36240,.T.);
#48611=ORIENTED_EDGE('',*,*,#36241,.F.);
#48612=ORIENTED_EDGE('',*,*,#36062,.T.);
#48613=ORIENTED_EDGE('',*,*,#36066,.T.);
#48614=ORIENTED_EDGE('',*,*,#36068,.T.);
#48615=ORIENTED_EDGE('',*,*,#36242,.F.);
#48616=ORIENTED_EDGE('',*,*,#36156,.T.);
#48617=ORIENTED_EDGE('',*,*,#36243,.T.);
#48618=ORIENTED_EDGE('',*,*,#36244,.F.);
#48619=ORIENTED_EDGE('',*,*,#36069,.T.);
#48620=ORIENTED_EDGE('',*,*,#36245,.F.);
#48621=ORIENTED_EDGE('',*,*,#36246,.F.);
#48622=ORIENTED_EDGE('',*,*,#36247,.F.);
#48623=ORIENTED_EDGE('',*,*,#36248,.F.);
#48624=ORIENTED_EDGE('',*,*,#36243,.F.);
#48625=ORIENTED_EDGE('',*,*,#36248,.T.);
#48626=ORIENTED_EDGE('',*,*,#36249,.F.);
#48627=ORIENTED_EDGE('',*,*,#36071,.T.);
#48628=ORIENTED_EDGE('',*,*,#36244,.T.);
#48629=ORIENTED_EDGE('',*,*,#36250,.T.);
#48630=ORIENTED_EDGE('',*,*,#36251,.F.);
#48631=ORIENTED_EDGE('',*,*,#36073,.T.);
#48632=ORIENTED_EDGE('',*,*,#36252,.F.);
#48633=ORIENTED_EDGE('',*,*,#36253,.F.);
#48634=ORIENTED_EDGE('',*,*,#36254,.F.);
#48635=ORIENTED_EDGE('',*,*,#36255,.F.);
#48636=ORIENTED_EDGE('',*,*,#36250,.F.);
#48637=ORIENTED_EDGE('',*,*,#36255,.T.);
#48638=ORIENTED_EDGE('',*,*,#36256,.F.);
#48639=ORIENTED_EDGE('',*,*,#36074,.T.);
#48640=ORIENTED_EDGE('',*,*,#36251,.T.);
#48641=ORIENTED_EDGE('',*,*,#36257,.T.);
#48642=ORIENTED_EDGE('',*,*,#36258,.F.);
#48643=ORIENTED_EDGE('',*,*,#36076,.T.);
#48644=ORIENTED_EDGE('',*,*,#36259,.F.);
#48645=ORIENTED_EDGE('',*,*,#36260,.F.);
#48646=ORIENTED_EDGE('',*,*,#36261,.F.);
#48647=ORIENTED_EDGE('',*,*,#36262,.F.);
#48648=ORIENTED_EDGE('',*,*,#36257,.F.);
#48649=ORIENTED_EDGE('',*,*,#36262,.T.);
#48650=ORIENTED_EDGE('',*,*,#36263,.F.);
#48651=ORIENTED_EDGE('',*,*,#36077,.T.);
#48652=ORIENTED_EDGE('',*,*,#36258,.T.);
#48653=ORIENTED_EDGE('',*,*,#36264,.T.);
#48654=ORIENTED_EDGE('',*,*,#36265,.F.);
#48655=ORIENTED_EDGE('',*,*,#36079,.T.);
#48656=ORIENTED_EDGE('',*,*,#36266,.F.);
#48657=ORIENTED_EDGE('',*,*,#36267,.F.);
#48658=ORIENTED_EDGE('',*,*,#36268,.F.);
#48659=ORIENTED_EDGE('',*,*,#36269,.F.);
#48660=ORIENTED_EDGE('',*,*,#36264,.F.);
#48661=ORIENTED_EDGE('',*,*,#36269,.T.);
#48662=ORIENTED_EDGE('',*,*,#36270,.F.);
#48663=ORIENTED_EDGE('',*,*,#36080,.T.);
#48664=ORIENTED_EDGE('',*,*,#36265,.T.);
#48665=ORIENTED_EDGE('',*,*,#36271,.T.);
#48666=ORIENTED_EDGE('',*,*,#36272,.F.);
#48667=ORIENTED_EDGE('',*,*,#36082,.T.);
#48668=ORIENTED_EDGE('',*,*,#36273,.F.);
#48669=ORIENTED_EDGE('',*,*,#36274,.F.);
#48670=ORIENTED_EDGE('',*,*,#36275,.F.);
#48671=ORIENTED_EDGE('',*,*,#36276,.F.);
#48672=ORIENTED_EDGE('',*,*,#36271,.F.);
#48673=ORIENTED_EDGE('',*,*,#36276,.T.);
#48674=ORIENTED_EDGE('',*,*,#36277,.F.);
#48675=ORIENTED_EDGE('',*,*,#36083,.T.);
#48676=ORIENTED_EDGE('',*,*,#36272,.T.);
#48677=ORIENTED_EDGE('',*,*,#36278,.T.);
#48678=ORIENTED_EDGE('',*,*,#36279,.F.);
#48679=ORIENTED_EDGE('',*,*,#36085,.T.);
#48680=ORIENTED_EDGE('',*,*,#36280,.F.);
#48681=ORIENTED_EDGE('',*,*,#36281,.F.);
#48682=ORIENTED_EDGE('',*,*,#36282,.F.);
#48683=ORIENTED_EDGE('',*,*,#36283,.F.);
#48684=ORIENTED_EDGE('',*,*,#36278,.F.);
#48685=ORIENTED_EDGE('',*,*,#36283,.T.);
#48686=ORIENTED_EDGE('',*,*,#36284,.F.);
#48687=ORIENTED_EDGE('',*,*,#36086,.T.);
#48688=ORIENTED_EDGE('',*,*,#36279,.T.);
#48689=ORIENTED_EDGE('',*,*,#36285,.T.);
#48690=ORIENTED_EDGE('',*,*,#36286,.F.);
#48691=ORIENTED_EDGE('',*,*,#36088,.T.);
#48692=ORIENTED_EDGE('',*,*,#36287,.F.);
#48693=ORIENTED_EDGE('',*,*,#36288,.F.);
#48694=ORIENTED_EDGE('',*,*,#36289,.F.);
#48695=ORIENTED_EDGE('',*,*,#36290,.F.);
#48696=ORIENTED_EDGE('',*,*,#36285,.F.);
#48697=ORIENTED_EDGE('',*,*,#36290,.T.);
#48698=ORIENTED_EDGE('',*,*,#36291,.F.);
#48699=ORIENTED_EDGE('',*,*,#36089,.T.);
#48700=ORIENTED_EDGE('',*,*,#36286,.T.);
#48701=ORIENTED_EDGE('',*,*,#36292,.T.);
#48702=ORIENTED_EDGE('',*,*,#36293,.F.);
#48703=ORIENTED_EDGE('',*,*,#36091,.T.);
#48704=ORIENTED_EDGE('',*,*,#36294,.F.);
#48705=ORIENTED_EDGE('',*,*,#36295,.F.);
#48706=ORIENTED_EDGE('',*,*,#36296,.F.);
#48707=ORIENTED_EDGE('',*,*,#36297,.F.);
#48708=ORIENTED_EDGE('',*,*,#36292,.F.);
#48709=ORIENTED_EDGE('',*,*,#36297,.T.);
#48710=ORIENTED_EDGE('',*,*,#36298,.F.);
#48711=ORIENTED_EDGE('',*,*,#36092,.T.);
#48712=ORIENTED_EDGE('',*,*,#36293,.T.);
#48713=ORIENTED_EDGE('',*,*,#36299,.T.);
#48714=ORIENTED_EDGE('',*,*,#36300,.F.);
#48715=ORIENTED_EDGE('',*,*,#36094,.T.);
#48716=ORIENTED_EDGE('',*,*,#36301,.F.);
#48717=ORIENTED_EDGE('',*,*,#36302,.F.);
#48718=ORIENTED_EDGE('',*,*,#36303,.F.);
#48719=ORIENTED_EDGE('',*,*,#36304,.F.);
#48720=ORIENTED_EDGE('',*,*,#36299,.F.);
#48721=ORIENTED_EDGE('',*,*,#36304,.T.);
#48722=ORIENTED_EDGE('',*,*,#36305,.F.);
#48723=ORIENTED_EDGE('',*,*,#36095,.T.);
#48724=ORIENTED_EDGE('',*,*,#36300,.T.);
#48725=ORIENTED_EDGE('',*,*,#36306,.T.);
#48726=ORIENTED_EDGE('',*,*,#36307,.F.);
#48727=ORIENTED_EDGE('',*,*,#36097,.T.);
#48728=ORIENTED_EDGE('',*,*,#36308,.F.);
#48729=ORIENTED_EDGE('',*,*,#36309,.F.);
#48730=ORIENTED_EDGE('',*,*,#36310,.F.);
#48731=ORIENTED_EDGE('',*,*,#36311,.F.);
#48732=ORIENTED_EDGE('',*,*,#36306,.F.);
#48733=ORIENTED_EDGE('',*,*,#36311,.T.);
#48734=ORIENTED_EDGE('',*,*,#36312,.F.);
#48735=ORIENTED_EDGE('',*,*,#36098,.T.);
#48736=ORIENTED_EDGE('',*,*,#36307,.T.);
#48737=ORIENTED_EDGE('',*,*,#36313,.T.);
#48738=ORIENTED_EDGE('',*,*,#36314,.F.);
#48739=ORIENTED_EDGE('',*,*,#36100,.T.);
#48740=ORIENTED_EDGE('',*,*,#36315,.F.);
#48741=ORIENTED_EDGE('',*,*,#36316,.F.);
#48742=ORIENTED_EDGE('',*,*,#36317,.F.);
#48743=ORIENTED_EDGE('',*,*,#36318,.F.);
#48744=ORIENTED_EDGE('',*,*,#36313,.F.);
#48745=ORIENTED_EDGE('',*,*,#36318,.T.);
#48746=ORIENTED_EDGE('',*,*,#36319,.F.);
#48747=ORIENTED_EDGE('',*,*,#36101,.T.);
#48748=ORIENTED_EDGE('',*,*,#36314,.T.);
#48749=ORIENTED_EDGE('',*,*,#36320,.T.);
#48750=ORIENTED_EDGE('',*,*,#36321,.F.);
#48751=ORIENTED_EDGE('',*,*,#36103,.T.);
#48752=ORIENTED_EDGE('',*,*,#36322,.F.);
#48753=ORIENTED_EDGE('',*,*,#36323,.F.);
#48754=ORIENTED_EDGE('',*,*,#36324,.F.);
#48755=ORIENTED_EDGE('',*,*,#36325,.F.);
#48756=ORIENTED_EDGE('',*,*,#36320,.F.);
#48757=ORIENTED_EDGE('',*,*,#36325,.T.);
#48758=ORIENTED_EDGE('',*,*,#36326,.F.);
#48759=ORIENTED_EDGE('',*,*,#36104,.T.);
#48760=ORIENTED_EDGE('',*,*,#36321,.T.);
#48761=ORIENTED_EDGE('',*,*,#36327,.T.);
#48762=ORIENTED_EDGE('',*,*,#36328,.F.);
#48763=ORIENTED_EDGE('',*,*,#36106,.T.);
#48764=ORIENTED_EDGE('',*,*,#36329,.F.);
#48765=ORIENTED_EDGE('',*,*,#36330,.F.);
#48766=ORIENTED_EDGE('',*,*,#36331,.F.);
#48767=ORIENTED_EDGE('',*,*,#36332,.F.);
#48768=ORIENTED_EDGE('',*,*,#36327,.F.);
#48769=ORIENTED_EDGE('',*,*,#36332,.T.);
#48770=ORIENTED_EDGE('',*,*,#36333,.F.);
#48771=ORIENTED_EDGE('',*,*,#36107,.T.);
#48772=ORIENTED_EDGE('',*,*,#36328,.T.);
#48773=ORIENTED_EDGE('',*,*,#36334,.T.);
#48774=ORIENTED_EDGE('',*,*,#36335,.F.);
#48775=ORIENTED_EDGE('',*,*,#36109,.T.);
#48776=ORIENTED_EDGE('',*,*,#36336,.F.);
#48777=ORIENTED_EDGE('',*,*,#36337,.F.);
#48778=ORIENTED_EDGE('',*,*,#36338,.F.);
#48779=ORIENTED_EDGE('',*,*,#36339,.F.);
#48780=ORIENTED_EDGE('',*,*,#36334,.F.);
#48781=ORIENTED_EDGE('',*,*,#36339,.T.);
#48782=ORIENTED_EDGE('',*,*,#36340,.F.);
#48783=ORIENTED_EDGE('',*,*,#36110,.T.);
#48784=ORIENTED_EDGE('',*,*,#36335,.T.);
#48785=ORIENTED_EDGE('',*,*,#34441,.T.);
#48786=ORIENTED_EDGE('',*,*,#36341,.F.);
#48787=ORIENTED_EDGE('',*,*,#36112,.T.);
#48788=ORIENTED_EDGE('',*,*,#36342,.F.);
#48789=ORIENTED_EDGE('',*,*,#34444,.T.);
#48790=ORIENTED_EDGE('',*,*,#36343,.F.);
#48791=ORIENTED_EDGE('',*,*,#36113,.T.);
#48792=ORIENTED_EDGE('',*,*,#36341,.T.);
#48793=ORIENTED_EDGE('',*,*,#36344,.T.);
#48794=ORIENTED_EDGE('',*,*,#36345,.F.);
#48795=ORIENTED_EDGE('',*,*,#36115,.T.);
#48796=ORIENTED_EDGE('',*,*,#36346,.F.);
#48797=ORIENTED_EDGE('',*,*,#36347,.F.);
#48798=ORIENTED_EDGE('',*,*,#36348,.F.);
#48799=ORIENTED_EDGE('',*,*,#36349,.F.);
#48800=ORIENTED_EDGE('',*,*,#36344,.F.);
#48801=ORIENTED_EDGE('',*,*,#36349,.T.);
#48802=ORIENTED_EDGE('',*,*,#36350,.F.);
#48803=ORIENTED_EDGE('',*,*,#36116,.T.);
#48804=ORIENTED_EDGE('',*,*,#36345,.T.);
#48805=ORIENTED_EDGE('',*,*,#36351,.T.);
#48806=ORIENTED_EDGE('',*,*,#36352,.F.);
#48807=ORIENTED_EDGE('',*,*,#36118,.T.);
#48808=ORIENTED_EDGE('',*,*,#36353,.F.);
#48809=ORIENTED_EDGE('',*,*,#36354,.F.);
#48810=ORIENTED_EDGE('',*,*,#36355,.F.);
#48811=ORIENTED_EDGE('',*,*,#36356,.F.);
#48812=ORIENTED_EDGE('',*,*,#36351,.F.);
#48813=ORIENTED_EDGE('',*,*,#36356,.T.);
#48814=ORIENTED_EDGE('',*,*,#36357,.F.);
#48815=ORIENTED_EDGE('',*,*,#36119,.T.);
#48816=ORIENTED_EDGE('',*,*,#36352,.T.);
#48817=ORIENTED_EDGE('',*,*,#36358,.T.);
#48818=ORIENTED_EDGE('',*,*,#36359,.F.);
#48819=ORIENTED_EDGE('',*,*,#36121,.T.);
#48820=ORIENTED_EDGE('',*,*,#36360,.F.);
#48821=ORIENTED_EDGE('',*,*,#36361,.F.);
#48822=ORIENTED_EDGE('',*,*,#36362,.F.);
#48823=ORIENTED_EDGE('',*,*,#36363,.F.);
#48824=ORIENTED_EDGE('',*,*,#36358,.F.);
#48825=ORIENTED_EDGE('',*,*,#36363,.T.);
#48826=ORIENTED_EDGE('',*,*,#36364,.F.);
#48827=ORIENTED_EDGE('',*,*,#36122,.T.);
#48828=ORIENTED_EDGE('',*,*,#36359,.T.);
#48829=ORIENTED_EDGE('',*,*,#36365,.T.);
#48830=ORIENTED_EDGE('',*,*,#36366,.F.);
#48831=ORIENTED_EDGE('',*,*,#36124,.T.);
#48832=ORIENTED_EDGE('',*,*,#36367,.F.);
#48833=ORIENTED_EDGE('',*,*,#36368,.F.);
#48834=ORIENTED_EDGE('',*,*,#36369,.F.);
#48835=ORIENTED_EDGE('',*,*,#36370,.F.);
#48836=ORIENTED_EDGE('',*,*,#36365,.F.);
#48837=ORIENTED_EDGE('',*,*,#36370,.T.);
#48838=ORIENTED_EDGE('',*,*,#36371,.F.);
#48839=ORIENTED_EDGE('',*,*,#36125,.T.);
#48840=ORIENTED_EDGE('',*,*,#36366,.T.);
#48841=ORIENTED_EDGE('',*,*,#36372,.T.);
#48842=ORIENTED_EDGE('',*,*,#36373,.F.);
#48843=ORIENTED_EDGE('',*,*,#36127,.T.);
#48844=ORIENTED_EDGE('',*,*,#36374,.F.);
#48845=ORIENTED_EDGE('',*,*,#36375,.F.);
#48846=ORIENTED_EDGE('',*,*,#36376,.F.);
#48847=ORIENTED_EDGE('',*,*,#36377,.F.);
#48848=ORIENTED_EDGE('',*,*,#36372,.F.);
#48849=ORIENTED_EDGE('',*,*,#36377,.T.);
#48850=ORIENTED_EDGE('',*,*,#36378,.F.);
#48851=ORIENTED_EDGE('',*,*,#36128,.T.);
#48852=ORIENTED_EDGE('',*,*,#36373,.T.);
#48853=ORIENTED_EDGE('',*,*,#36379,.T.);
#48854=ORIENTED_EDGE('',*,*,#36380,.F.);
#48855=ORIENTED_EDGE('',*,*,#36130,.T.);
#48856=ORIENTED_EDGE('',*,*,#36381,.F.);
#48857=ORIENTED_EDGE('',*,*,#36382,.F.);
#48858=ORIENTED_EDGE('',*,*,#36383,.F.);
#48859=ORIENTED_EDGE('',*,*,#36384,.F.);
#48860=ORIENTED_EDGE('',*,*,#36379,.F.);
#48861=ORIENTED_EDGE('',*,*,#36384,.T.);
#48862=ORIENTED_EDGE('',*,*,#36385,.F.);
#48863=ORIENTED_EDGE('',*,*,#36131,.T.);
#48864=ORIENTED_EDGE('',*,*,#36380,.T.);
#48865=ORIENTED_EDGE('',*,*,#36386,.T.);
#48866=ORIENTED_EDGE('',*,*,#36387,.F.);
#48867=ORIENTED_EDGE('',*,*,#36133,.T.);
#48868=ORIENTED_EDGE('',*,*,#36388,.F.);
#48869=ORIENTED_EDGE('',*,*,#36389,.F.);
#48870=ORIENTED_EDGE('',*,*,#36390,.F.);
#48871=ORIENTED_EDGE('',*,*,#36391,.F.);
#48872=ORIENTED_EDGE('',*,*,#36386,.F.);
#48873=ORIENTED_EDGE('',*,*,#36391,.T.);
#48874=ORIENTED_EDGE('',*,*,#36392,.F.);
#48875=ORIENTED_EDGE('',*,*,#36134,.T.);
#48876=ORIENTED_EDGE('',*,*,#36387,.T.);
#48877=ORIENTED_EDGE('',*,*,#36393,.T.);
#48878=ORIENTED_EDGE('',*,*,#36394,.F.);
#48879=ORIENTED_EDGE('',*,*,#36136,.T.);
#48880=ORIENTED_EDGE('',*,*,#36395,.F.);
#48881=ORIENTED_EDGE('',*,*,#36396,.F.);
#48882=ORIENTED_EDGE('',*,*,#36397,.F.);
#48883=ORIENTED_EDGE('',*,*,#36398,.F.);
#48884=ORIENTED_EDGE('',*,*,#36393,.F.);
#48885=ORIENTED_EDGE('',*,*,#36398,.T.);
#48886=ORIENTED_EDGE('',*,*,#36399,.F.);
#48887=ORIENTED_EDGE('',*,*,#36137,.T.);
#48888=ORIENTED_EDGE('',*,*,#36394,.T.);
#48889=ORIENTED_EDGE('',*,*,#36400,.T.);
#48890=ORIENTED_EDGE('',*,*,#36401,.F.);
#48891=ORIENTED_EDGE('',*,*,#36139,.T.);
#48892=ORIENTED_EDGE('',*,*,#36402,.F.);
#48893=ORIENTED_EDGE('',*,*,#36403,.T.);
#48894=ORIENTED_EDGE('',*,*,#36404,.F.);
#48895=ORIENTED_EDGE('',*,*,#36140,.T.);
#48896=ORIENTED_EDGE('',*,*,#36401,.T.);
#48897=ORIENTED_EDGE('',*,*,#36405,.F.);
#48898=ORIENTED_EDGE('',*,*,#36406,.F.);
#48899=ORIENTED_EDGE('',*,*,#36403,.F.);
#48900=ORIENTED_EDGE('',*,*,#36400,.F.);
#48901=ORIENTED_EDGE('',*,*,#36142,.T.);
#48902=ORIENTED_EDGE('',*,*,#36407,.F.);
#48903=ORIENTED_EDGE('',*,*,#36408,.T.);
#48904=ORIENTED_EDGE('',*,*,#36409,.F.);
#48905=ORIENTED_EDGE('',*,*,#36410,.F.);
#48906=ORIENTED_EDGE('',*,*,#36408,.F.);
#48907=ORIENTED_EDGE('',*,*,#36411,.F.);
#48908=ORIENTED_EDGE('',*,*,#36412,.F.);
#48909=ORIENTED_EDGE('',*,*,#36143,.T.);
#48910=ORIENTED_EDGE('',*,*,#36409,.T.);
#48911=ORIENTED_EDGE('',*,*,#36410,.T.);
#48912=ORIENTED_EDGE('',*,*,#36413,.F.);
#48913=ORIENTED_EDGE('',*,*,#36414,.T.);
#48914=ORIENTED_EDGE('',*,*,#36415,.F.);
#48915=ORIENTED_EDGE('',*,*,#36145,.T.);
#48916=ORIENTED_EDGE('',*,*,#36416,.F.);
#48917=ORIENTED_EDGE('',*,*,#36417,.F.);
#48918=ORIENTED_EDGE('',*,*,#36418,.F.);
#48919=ORIENTED_EDGE('',*,*,#36419,.F.);
#48920=ORIENTED_EDGE('',*,*,#36414,.F.);
#48921=ORIENTED_EDGE('',*,*,#36419,.T.);
#48922=ORIENTED_EDGE('',*,*,#36420,.F.);
#48923=ORIENTED_EDGE('',*,*,#36146,.T.);
#48924=ORIENTED_EDGE('',*,*,#36415,.T.);
#48925=ORIENTED_EDGE('',*,*,#36421,.T.);
#48926=ORIENTED_EDGE('',*,*,#36422,.F.);
#48927=ORIENTED_EDGE('',*,*,#36148,.T.);
#48928=ORIENTED_EDGE('',*,*,#36423,.F.);
#48929=ORIENTED_EDGE('',*,*,#36424,.F.);
#48930=ORIENTED_EDGE('',*,*,#36425,.F.);
#48931=ORIENTED_EDGE('',*,*,#36426,.F.);
#48932=ORIENTED_EDGE('',*,*,#36421,.F.);
#48933=ORIENTED_EDGE('',*,*,#36426,.T.);
#48934=ORIENTED_EDGE('',*,*,#36427,.F.);
#48935=ORIENTED_EDGE('',*,*,#36149,.T.);
#48936=ORIENTED_EDGE('',*,*,#36422,.T.);
#48937=ORIENTED_EDGE('',*,*,#36428,.T.);
#48938=ORIENTED_EDGE('',*,*,#36429,.F.);
#48939=ORIENTED_EDGE('',*,*,#36151,.T.);
#48940=ORIENTED_EDGE('',*,*,#36430,.F.);
#48941=ORIENTED_EDGE('',*,*,#36431,.F.);
#48942=ORIENTED_EDGE('',*,*,#36432,.F.);
#48943=ORIENTED_EDGE('',*,*,#36433,.F.);
#48944=ORIENTED_EDGE('',*,*,#36428,.F.);
#48945=ORIENTED_EDGE('',*,*,#36433,.T.);
#48946=ORIENTED_EDGE('',*,*,#36434,.F.);
#48947=ORIENTED_EDGE('',*,*,#36152,.T.);
#48948=ORIENTED_EDGE('',*,*,#36429,.T.);
#48949=ORIENTED_EDGE('',*,*,#36435,.T.);
#48950=ORIENTED_EDGE('',*,*,#36436,.F.);
#48951=ORIENTED_EDGE('',*,*,#36154,.T.);
#48952=ORIENTED_EDGE('',*,*,#36437,.F.);
#48953=ORIENTED_EDGE('',*,*,#36438,.F.);
#48954=ORIENTED_EDGE('',*,*,#36439,.F.);
#48955=ORIENTED_EDGE('',*,*,#36440,.F.);
#48956=ORIENTED_EDGE('',*,*,#36435,.F.);
#48957=ORIENTED_EDGE('',*,*,#36440,.T.);
#48958=ORIENTED_EDGE('',*,*,#36441,.F.);
#48959=ORIENTED_EDGE('',*,*,#36155,.T.);
#48960=ORIENTED_EDGE('',*,*,#36436,.T.);
#48961=ORIENTED_EDGE('',*,*,#36157,.T.);
#48962=ORIENTED_EDGE('',*,*,#36442,.F.);
#48963=ORIENTED_EDGE('',*,*,#36443,.T.);
#48964=ORIENTED_EDGE('',*,*,#36444,.F.);
#48965=ORIENTED_EDGE('',*,*,#36445,.T.);
#48966=ORIENTED_EDGE('',*,*,#36446,.F.);
#48967=ORIENTED_EDGE('',*,*,#36158,.T.);
#48968=ORIENTED_EDGE('',*,*,#36444,.T.);
#48969=ORIENTED_EDGE('',*,*,#36447,.F.);
#48970=ORIENTED_EDGE('',*,*,#36448,.F.);
#48971=ORIENTED_EDGE('',*,*,#36445,.F.);
#48972=ORIENTED_EDGE('',*,*,#36443,.F.);
#48973=ORIENTED_EDGE('',*,*,#36160,.T.);
#48974=ORIENTED_EDGE('',*,*,#36449,.F.);
#48975=ORIENTED_EDGE('',*,*,#36450,.T.);
#48976=ORIENTED_EDGE('',*,*,#36451,.F.);
#48977=ORIENTED_EDGE('',*,*,#36161,.T.);
#48978=ORIENTED_EDGE('',*,*,#36451,.T.);
#48979=ORIENTED_EDGE('',*,*,#36452,.T.);
#48980=ORIENTED_EDGE('',*,*,#36453,.F.);
#48981=ORIENTED_EDGE('',*,*,#36452,.F.);
#48982=ORIENTED_EDGE('',*,*,#36450,.F.);
#48983=ORIENTED_EDGE('',*,*,#36454,.F.);
#48984=ORIENTED_EDGE('',*,*,#36455,.F.);
#48985=ORIENTED_EDGE('',*,*,#36163,.T.);
#48986=ORIENTED_EDGE('',*,*,#36456,.F.);
#48987=ORIENTED_EDGE('',*,*,#36457,.T.);
#48988=ORIENTED_EDGE('',*,*,#36458,.F.);
#48989=ORIENTED_EDGE('',*,*,#36164,.T.);
#48990=ORIENTED_EDGE('',*,*,#36458,.T.);
#48991=ORIENTED_EDGE('',*,*,#36459,.T.);
#48992=ORIENTED_EDGE('',*,*,#36460,.F.);
#48993=ORIENTED_EDGE('',*,*,#36459,.F.);
#48994=ORIENTED_EDGE('',*,*,#36457,.F.);
#48995=ORIENTED_EDGE('',*,*,#36461,.F.);
#48996=ORIENTED_EDGE('',*,*,#36462,.F.);
#48997=ORIENTED_EDGE('',*,*,#36166,.T.);
#48998=ORIENTED_EDGE('',*,*,#36463,.F.);
#48999=ORIENTED_EDGE('',*,*,#36464,.T.);
#49000=ORIENTED_EDGE('',*,*,#36465,.F.);
#49001=ORIENTED_EDGE('',*,*,#36167,.T.);
#49002=ORIENTED_EDGE('',*,*,#36465,.T.);
#49003=ORIENTED_EDGE('',*,*,#36466,.T.);
#49004=ORIENTED_EDGE('',*,*,#36467,.F.);
#49005=ORIENTED_EDGE('',*,*,#36466,.F.);
#49006=ORIENTED_EDGE('',*,*,#36464,.F.);
#49007=ORIENTED_EDGE('',*,*,#36468,.F.);
#49008=ORIENTED_EDGE('',*,*,#36469,.F.);
#49009=ORIENTED_EDGE('',*,*,#36169,.T.);
#49010=ORIENTED_EDGE('',*,*,#36470,.F.);
#49011=ORIENTED_EDGE('',*,*,#36471,.T.);
#49012=ORIENTED_EDGE('',*,*,#36472,.F.);
#49013=ORIENTED_EDGE('',*,*,#36170,.T.);
#49014=ORIENTED_EDGE('',*,*,#36472,.T.);
#49015=ORIENTED_EDGE('',*,*,#36473,.T.);
#49016=ORIENTED_EDGE('',*,*,#36474,.F.);
#49017=ORIENTED_EDGE('',*,*,#36473,.F.);
#49018=ORIENTED_EDGE('',*,*,#36471,.F.);
#49019=ORIENTED_EDGE('',*,*,#36475,.F.);
#49020=ORIENTED_EDGE('',*,*,#36476,.F.);
#49021=ORIENTED_EDGE('',*,*,#36172,.T.);
#49022=ORIENTED_EDGE('',*,*,#36477,.F.);
#49023=ORIENTED_EDGE('',*,*,#36478,.T.);
#49024=ORIENTED_EDGE('',*,*,#36479,.F.);
#49025=ORIENTED_EDGE('',*,*,#36173,.T.);
#49026=ORIENTED_EDGE('',*,*,#36479,.T.);
#49027=ORIENTED_EDGE('',*,*,#36480,.T.);
#49028=ORIENTED_EDGE('',*,*,#36481,.F.);
#49029=ORIENTED_EDGE('',*,*,#36480,.F.);
#49030=ORIENTED_EDGE('',*,*,#36478,.F.);
#49031=ORIENTED_EDGE('',*,*,#36482,.F.);
#49032=ORIENTED_EDGE('',*,*,#36483,.F.);
#49033=ORIENTED_EDGE('',*,*,#36175,.T.);
#49034=ORIENTED_EDGE('',*,*,#36484,.F.);
#49035=ORIENTED_EDGE('',*,*,#36485,.T.);
#49036=ORIENTED_EDGE('',*,*,#36486,.F.);
#49037=ORIENTED_EDGE('',*,*,#36176,.T.);
#49038=ORIENTED_EDGE('',*,*,#36486,.T.);
#49039=ORIENTED_EDGE('',*,*,#36487,.T.);
#49040=ORIENTED_EDGE('',*,*,#36488,.F.);
#49041=ORIENTED_EDGE('',*,*,#36487,.F.);
#49042=ORIENTED_EDGE('',*,*,#36485,.F.);
#49043=ORIENTED_EDGE('',*,*,#36489,.F.);
#49044=ORIENTED_EDGE('',*,*,#36490,.F.);
#49045=ORIENTED_EDGE('',*,*,#36178,.T.);
#49046=ORIENTED_EDGE('',*,*,#36491,.F.);
#49047=ORIENTED_EDGE('',*,*,#36492,.T.);
#49048=ORIENTED_EDGE('',*,*,#36493,.F.);
#49049=ORIENTED_EDGE('',*,*,#36179,.T.);
#49050=ORIENTED_EDGE('',*,*,#36493,.T.);
#49051=ORIENTED_EDGE('',*,*,#36494,.T.);
#49052=ORIENTED_EDGE('',*,*,#36495,.F.);
#49053=ORIENTED_EDGE('',*,*,#36494,.F.);
#49054=ORIENTED_EDGE('',*,*,#36492,.F.);
#49055=ORIENTED_EDGE('',*,*,#36496,.F.);
#49056=ORIENTED_EDGE('',*,*,#36497,.F.);
#49057=ORIENTED_EDGE('',*,*,#36181,.T.);
#49058=ORIENTED_EDGE('',*,*,#36498,.F.);
#49059=ORIENTED_EDGE('',*,*,#36499,.T.);
#49060=ORIENTED_EDGE('',*,*,#36500,.F.);
#49061=ORIENTED_EDGE('',*,*,#36182,.T.);
#49062=ORIENTED_EDGE('',*,*,#36500,.T.);
#49063=ORIENTED_EDGE('',*,*,#36501,.T.);
#49064=ORIENTED_EDGE('',*,*,#36502,.F.);
#49065=ORIENTED_EDGE('',*,*,#36501,.F.);
#49066=ORIENTED_EDGE('',*,*,#36499,.F.);
#49067=ORIENTED_EDGE('',*,*,#36503,.F.);
#49068=ORIENTED_EDGE('',*,*,#36504,.F.);
#49069=ORIENTED_EDGE('',*,*,#36184,.T.);
#49070=ORIENTED_EDGE('',*,*,#36505,.F.);
#49071=ORIENTED_EDGE('',*,*,#36506,.T.);
#49072=ORIENTED_EDGE('',*,*,#36507,.F.);
#49073=ORIENTED_EDGE('',*,*,#36185,.T.);
#49074=ORIENTED_EDGE('',*,*,#36507,.T.);
#49075=ORIENTED_EDGE('',*,*,#36508,.T.);
#49076=ORIENTED_EDGE('',*,*,#36509,.F.);
#49077=ORIENTED_EDGE('',*,*,#36508,.F.);
#49078=ORIENTED_EDGE('',*,*,#36506,.F.);
#49079=ORIENTED_EDGE('',*,*,#36510,.F.);
#49080=ORIENTED_EDGE('',*,*,#36511,.F.);
#49081=ORIENTED_EDGE('',*,*,#36187,.T.);
#49082=ORIENTED_EDGE('',*,*,#36512,.F.);
#49083=ORIENTED_EDGE('',*,*,#36513,.T.);
#49084=ORIENTED_EDGE('',*,*,#36514,.F.);
#49085=ORIENTED_EDGE('',*,*,#36188,.T.);
#49086=ORIENTED_EDGE('',*,*,#36514,.T.);
#49087=ORIENTED_EDGE('',*,*,#36515,.T.);
#49088=ORIENTED_EDGE('',*,*,#36516,.F.);
#49089=ORIENTED_EDGE('',*,*,#36515,.F.);
#49090=ORIENTED_EDGE('',*,*,#36513,.F.);
#49091=ORIENTED_EDGE('',*,*,#36517,.F.);
#49092=ORIENTED_EDGE('',*,*,#36518,.F.);
#49093=ORIENTED_EDGE('',*,*,#36190,.T.);
#49094=ORIENTED_EDGE('',*,*,#36519,.F.);
#49095=ORIENTED_EDGE('',*,*,#36520,.T.);
#49096=ORIENTED_EDGE('',*,*,#36521,.F.);
#49097=ORIENTED_EDGE('',*,*,#36191,.T.);
#49098=ORIENTED_EDGE('',*,*,#36521,.T.);
#49099=ORIENTED_EDGE('',*,*,#36522,.T.);
#49100=ORIENTED_EDGE('',*,*,#36523,.F.);
#49101=ORIENTED_EDGE('',*,*,#36522,.F.);
#49102=ORIENTED_EDGE('',*,*,#36520,.F.);
#49103=ORIENTED_EDGE('',*,*,#36524,.F.);
#49104=ORIENTED_EDGE('',*,*,#36525,.F.);
#49105=ORIENTED_EDGE('',*,*,#36193,.T.);
#49106=ORIENTED_EDGE('',*,*,#36526,.F.);
#49107=ORIENTED_EDGE('',*,*,#36527,.T.);
#49108=ORIENTED_EDGE('',*,*,#36528,.F.);
#49109=ORIENTED_EDGE('',*,*,#36194,.T.);
#49110=ORIENTED_EDGE('',*,*,#36528,.T.);
#49111=ORIENTED_EDGE('',*,*,#36529,.T.);
#49112=ORIENTED_EDGE('',*,*,#36530,.F.);
#49113=ORIENTED_EDGE('',*,*,#36529,.F.);
#49114=ORIENTED_EDGE('',*,*,#36527,.F.);
#49115=ORIENTED_EDGE('',*,*,#36531,.F.);
#49116=ORIENTED_EDGE('',*,*,#36532,.F.);
#49117=ORIENTED_EDGE('',*,*,#36196,.T.);
#49118=ORIENTED_EDGE('',*,*,#36533,.F.);
#49119=ORIENTED_EDGE('',*,*,#36534,.T.);
#49120=ORIENTED_EDGE('',*,*,#36535,.F.);
#49121=ORIENTED_EDGE('',*,*,#36197,.T.);
#49122=ORIENTED_EDGE('',*,*,#36535,.T.);
#49123=ORIENTED_EDGE('',*,*,#36536,.T.);
#49124=ORIENTED_EDGE('',*,*,#36537,.F.);
#49125=ORIENTED_EDGE('',*,*,#36536,.F.);
#49126=ORIENTED_EDGE('',*,*,#36534,.F.);
#49127=ORIENTED_EDGE('',*,*,#36538,.F.);
#49128=ORIENTED_EDGE('',*,*,#36539,.F.);
#49129=ORIENTED_EDGE('',*,*,#36199,.T.);
#49130=ORIENTED_EDGE('',*,*,#36540,.F.);
#49131=ORIENTED_EDGE('',*,*,#36541,.T.);
#49132=ORIENTED_EDGE('',*,*,#36542,.F.);
#49133=ORIENTED_EDGE('',*,*,#36200,.T.);
#49134=ORIENTED_EDGE('',*,*,#36542,.T.);
#49135=ORIENTED_EDGE('',*,*,#36543,.T.);
#49136=ORIENTED_EDGE('',*,*,#36544,.F.);
#49137=ORIENTED_EDGE('',*,*,#36543,.F.);
#49138=ORIENTED_EDGE('',*,*,#36541,.F.);
#49139=ORIENTED_EDGE('',*,*,#36545,.F.);
#49140=ORIENTED_EDGE('',*,*,#36546,.F.);
#49141=ORIENTED_EDGE('',*,*,#36202,.T.);
#49142=ORIENTED_EDGE('',*,*,#36547,.F.);
#49143=ORIENTED_EDGE('',*,*,#36548,.T.);
#49144=ORIENTED_EDGE('',*,*,#36549,.F.);
#49145=ORIENTED_EDGE('',*,*,#36203,.T.);
#49146=ORIENTED_EDGE('',*,*,#36549,.T.);
#49147=ORIENTED_EDGE('',*,*,#36550,.T.);
#49148=ORIENTED_EDGE('',*,*,#36551,.F.);
#49149=ORIENTED_EDGE('',*,*,#36550,.F.);
#49150=ORIENTED_EDGE('',*,*,#36548,.F.);
#49151=ORIENTED_EDGE('',*,*,#36552,.F.);
#49152=ORIENTED_EDGE('',*,*,#36553,.F.);
#49153=ORIENTED_EDGE('',*,*,#36205,.T.);
#49154=ORIENTED_EDGE('',*,*,#36554,.F.);
#49155=ORIENTED_EDGE('',*,*,#36555,.T.);
#49156=ORIENTED_EDGE('',*,*,#36556,.F.);
#49157=ORIENTED_EDGE('',*,*,#36206,.T.);
#49158=ORIENTED_EDGE('',*,*,#36556,.T.);
#49159=ORIENTED_EDGE('',*,*,#36557,.T.);
#49160=ORIENTED_EDGE('',*,*,#36558,.F.);
#49161=ORIENTED_EDGE('',*,*,#36557,.F.);
#49162=ORIENTED_EDGE('',*,*,#36555,.F.);
#49163=ORIENTED_EDGE('',*,*,#36559,.F.);
#49164=ORIENTED_EDGE('',*,*,#36560,.F.);
#49165=ORIENTED_EDGE('',*,*,#36208,.T.);
#49166=ORIENTED_EDGE('',*,*,#36561,.F.);
#49167=ORIENTED_EDGE('',*,*,#36562,.T.);
#49168=ORIENTED_EDGE('',*,*,#36563,.F.);
#49169=ORIENTED_EDGE('',*,*,#36209,.T.);
#49170=ORIENTED_EDGE('',*,*,#36563,.T.);
#49171=ORIENTED_EDGE('',*,*,#36564,.T.);
#49172=ORIENTED_EDGE('',*,*,#36565,.F.);
#49173=ORIENTED_EDGE('',*,*,#36564,.F.);
#49174=ORIENTED_EDGE('',*,*,#36562,.F.);
#49175=ORIENTED_EDGE('',*,*,#36566,.F.);
#49176=ORIENTED_EDGE('',*,*,#36567,.F.);
#49177=ORIENTED_EDGE('',*,*,#36211,.T.);
#49178=ORIENTED_EDGE('',*,*,#36568,.F.);
#49179=ORIENTED_EDGE('',*,*,#36569,.T.);
#49180=ORIENTED_EDGE('',*,*,#36570,.F.);
#49181=ORIENTED_EDGE('',*,*,#36212,.T.);
#49182=ORIENTED_EDGE('',*,*,#36570,.T.);
#49183=ORIENTED_EDGE('',*,*,#36571,.T.);
#49184=ORIENTED_EDGE('',*,*,#36572,.F.);
#49185=ORIENTED_EDGE('',*,*,#36571,.F.);
#49186=ORIENTED_EDGE('',*,*,#36569,.F.);
#49187=ORIENTED_EDGE('',*,*,#36573,.F.);
#49188=ORIENTED_EDGE('',*,*,#36574,.F.);
#49189=ORIENTED_EDGE('',*,*,#36214,.T.);
#49190=ORIENTED_EDGE('',*,*,#36575,.F.);
#49191=ORIENTED_EDGE('',*,*,#36576,.T.);
#49192=ORIENTED_EDGE('',*,*,#36577,.F.);
#49193=ORIENTED_EDGE('',*,*,#36215,.T.);
#49194=ORIENTED_EDGE('',*,*,#36577,.T.);
#49195=ORIENTED_EDGE('',*,*,#36578,.T.);
#49196=ORIENTED_EDGE('',*,*,#36579,.F.);
#49197=ORIENTED_EDGE('',*,*,#36578,.F.);
#49198=ORIENTED_EDGE('',*,*,#36576,.F.);
#49199=ORIENTED_EDGE('',*,*,#36580,.F.);
#49200=ORIENTED_EDGE('',*,*,#36581,.F.);
#49201=ORIENTED_EDGE('',*,*,#36217,.T.);
#49202=ORIENTED_EDGE('',*,*,#36582,.F.);
#49203=ORIENTED_EDGE('',*,*,#36583,.T.);
#49204=ORIENTED_EDGE('',*,*,#36584,.F.);
#49205=ORIENTED_EDGE('',*,*,#36218,.T.);
#49206=ORIENTED_EDGE('',*,*,#36584,.T.);
#49207=ORIENTED_EDGE('',*,*,#36585,.T.);
#49208=ORIENTED_EDGE('',*,*,#36586,.F.);
#49209=ORIENTED_EDGE('',*,*,#36585,.F.);
#49210=ORIENTED_EDGE('',*,*,#36583,.F.);
#49211=ORIENTED_EDGE('',*,*,#36587,.F.);
#49212=ORIENTED_EDGE('',*,*,#36588,.F.);
#49213=ORIENTED_EDGE('',*,*,#36220,.T.);
#49214=ORIENTED_EDGE('',*,*,#36589,.F.);
#49215=ORIENTED_EDGE('',*,*,#36590,.T.);
#49216=ORIENTED_EDGE('',*,*,#36591,.F.);
#49217=ORIENTED_EDGE('',*,*,#36221,.T.);
#49218=ORIENTED_EDGE('',*,*,#36591,.T.);
#49219=ORIENTED_EDGE('',*,*,#36592,.T.);
#49220=ORIENTED_EDGE('',*,*,#36593,.F.);
#49221=ORIENTED_EDGE('',*,*,#36592,.F.);
#49222=ORIENTED_EDGE('',*,*,#36590,.F.);
#49223=ORIENTED_EDGE('',*,*,#36594,.F.);
#49224=ORIENTED_EDGE('',*,*,#36595,.F.);
#49225=ORIENTED_EDGE('',*,*,#36223,.T.);
#49226=ORIENTED_EDGE('',*,*,#36596,.F.);
#49227=ORIENTED_EDGE('',*,*,#36597,.T.);
#49228=ORIENTED_EDGE('',*,*,#36598,.F.);
#49229=ORIENTED_EDGE('',*,*,#36224,.T.);
#49230=ORIENTED_EDGE('',*,*,#36598,.T.);
#49231=ORIENTED_EDGE('',*,*,#36599,.T.);
#49232=ORIENTED_EDGE('',*,*,#36600,.F.);
#49233=ORIENTED_EDGE('',*,*,#36599,.F.);
#49234=ORIENTED_EDGE('',*,*,#36597,.F.);
#49235=ORIENTED_EDGE('',*,*,#36601,.F.);
#49236=ORIENTED_EDGE('',*,*,#36602,.F.);
#49237=ORIENTED_EDGE('',*,*,#36226,.T.);
#49238=ORIENTED_EDGE('',*,*,#36603,.F.);
#49239=ORIENTED_EDGE('',*,*,#36604,.T.);
#49240=ORIENTED_EDGE('',*,*,#36605,.F.);
#49241=ORIENTED_EDGE('',*,*,#36227,.T.);
#49242=ORIENTED_EDGE('',*,*,#36605,.T.);
#49243=ORIENTED_EDGE('',*,*,#36606,.T.);
#49244=ORIENTED_EDGE('',*,*,#36607,.F.);
#49245=ORIENTED_EDGE('',*,*,#36606,.F.);
#49246=ORIENTED_EDGE('',*,*,#36604,.F.);
#49247=ORIENTED_EDGE('',*,*,#36608,.F.);
#49248=ORIENTED_EDGE('',*,*,#36609,.F.);
#49249=ORIENTED_EDGE('',*,*,#36229,.T.);
#49250=ORIENTED_EDGE('',*,*,#36610,.F.);
#49251=ORIENTED_EDGE('',*,*,#36611,.T.);
#49252=ORIENTED_EDGE('',*,*,#36612,.F.);
#49253=ORIENTED_EDGE('',*,*,#36230,.T.);
#49254=ORIENTED_EDGE('',*,*,#36612,.T.);
#49255=ORIENTED_EDGE('',*,*,#36613,.T.);
#49256=ORIENTED_EDGE('',*,*,#36614,.F.);
#49257=ORIENTED_EDGE('',*,*,#36613,.F.);
#49258=ORIENTED_EDGE('',*,*,#36611,.F.);
#49259=ORIENTED_EDGE('',*,*,#36615,.F.);
#49260=ORIENTED_EDGE('',*,*,#36616,.F.);
#49261=ORIENTED_EDGE('',*,*,#36232,.T.);
#49262=ORIENTED_EDGE('',*,*,#36617,.F.);
#49263=ORIENTED_EDGE('',*,*,#36618,.T.);
#49264=ORIENTED_EDGE('',*,*,#36619,.F.);
#49265=ORIENTED_EDGE('',*,*,#36233,.T.);
#49266=ORIENTED_EDGE('',*,*,#36619,.T.);
#49267=ORIENTED_EDGE('',*,*,#36620,.T.);
#49268=ORIENTED_EDGE('',*,*,#36621,.F.);
#49269=ORIENTED_EDGE('',*,*,#36620,.F.);
#49270=ORIENTED_EDGE('',*,*,#36618,.F.);
#49271=ORIENTED_EDGE('',*,*,#36622,.F.);
#49272=ORIENTED_EDGE('',*,*,#36623,.F.);
#49273=ORIENTED_EDGE('',*,*,#36235,.T.);
#49274=ORIENTED_EDGE('',*,*,#36624,.F.);
#49275=ORIENTED_EDGE('',*,*,#36625,.T.);
#49276=ORIENTED_EDGE('',*,*,#36626,.F.);
#49277=ORIENTED_EDGE('',*,*,#36236,.T.);
#49278=ORIENTED_EDGE('',*,*,#36626,.T.);
#49279=ORIENTED_EDGE('',*,*,#36627,.T.);
#49280=ORIENTED_EDGE('',*,*,#36628,.F.);
#49281=ORIENTED_EDGE('',*,*,#36627,.F.);
#49282=ORIENTED_EDGE('',*,*,#36625,.F.);
#49283=ORIENTED_EDGE('',*,*,#36629,.F.);
#49284=ORIENTED_EDGE('',*,*,#36630,.F.);
#49285=ORIENTED_EDGE('',*,*,#36238,.T.);
#49286=ORIENTED_EDGE('',*,*,#36631,.F.);
#49287=ORIENTED_EDGE('',*,*,#36632,.T.);
#49288=ORIENTED_EDGE('',*,*,#36633,.F.);
#49289=ORIENTED_EDGE('',*,*,#36239,.T.);
#49290=ORIENTED_EDGE('',*,*,#36633,.T.);
#49291=ORIENTED_EDGE('',*,*,#36634,.T.);
#49292=ORIENTED_EDGE('',*,*,#36635,.F.);
#49293=ORIENTED_EDGE('',*,*,#36634,.F.);
#49294=ORIENTED_EDGE('',*,*,#36632,.F.);
#49295=ORIENTED_EDGE('',*,*,#36636,.F.);
#49296=ORIENTED_EDGE('',*,*,#36637,.F.);
#49297=ORIENTED_EDGE('',*,*,#36241,.T.);
#49298=ORIENTED_EDGE('',*,*,#36638,.F.);
#49299=ORIENTED_EDGE('',*,*,#36639,.T.);
#49300=ORIENTED_EDGE('',*,*,#36640,.F.);
#49301=ORIENTED_EDGE('',*,*,#36242,.T.);
#49302=ORIENTED_EDGE('',*,*,#36640,.T.);
#49303=ORIENTED_EDGE('',*,*,#36641,.T.);
#49304=ORIENTED_EDGE('',*,*,#36642,.F.);
#49305=ORIENTED_EDGE('',*,*,#36641,.F.);
#49306=ORIENTED_EDGE('',*,*,#36639,.F.);
#49307=ORIENTED_EDGE('',*,*,#36643,.F.);
#49308=ORIENTED_EDGE('',*,*,#36644,.F.);
#49309=ORIENTED_EDGE('',*,*,#36645,.F.);
#49310=ORIENTED_EDGE('',*,*,#36646,.F.);
#49311=ORIENTED_EDGE('',*,*,#36246,.T.);
#49312=ORIENTED_EDGE('',*,*,#36245,.T.);
#49313=ORIENTED_EDGE('',*,*,#36647,.F.);
#49314=ORIENTED_EDGE('',*,*,#36249,.T.);
#49315=ORIENTED_EDGE('',*,*,#36247,.T.);
#49316=ORIENTED_EDGE('',*,*,#36646,.T.);
#49317=ORIENTED_EDGE('',*,*,#36648,.F.);
#49318=ORIENTED_EDGE('',*,*,#36649,.F.);
#49319=ORIENTED_EDGE('',*,*,#36253,.T.);
#49320=ORIENTED_EDGE('',*,*,#36252,.T.);
#49321=ORIENTED_EDGE('',*,*,#36650,.F.);
#49322=ORIENTED_EDGE('',*,*,#36256,.T.);
#49323=ORIENTED_EDGE('',*,*,#36254,.T.);
#49324=ORIENTED_EDGE('',*,*,#36649,.T.);
#49325=ORIENTED_EDGE('',*,*,#36651,.F.);
#49326=ORIENTED_EDGE('',*,*,#36652,.F.);
#49327=ORIENTED_EDGE('',*,*,#36260,.T.);
#49328=ORIENTED_EDGE('',*,*,#36259,.T.);
#49329=ORIENTED_EDGE('',*,*,#36653,.F.);
#49330=ORIENTED_EDGE('',*,*,#36263,.T.);
#49331=ORIENTED_EDGE('',*,*,#36261,.T.);
#49332=ORIENTED_EDGE('',*,*,#36652,.T.);
#49333=ORIENTED_EDGE('',*,*,#36654,.F.);
#49334=ORIENTED_EDGE('',*,*,#36655,.F.);
#49335=ORIENTED_EDGE('',*,*,#36267,.T.);
#49336=ORIENTED_EDGE('',*,*,#36266,.T.);
#49337=ORIENTED_EDGE('',*,*,#36656,.F.);
#49338=ORIENTED_EDGE('',*,*,#36270,.T.);
#49339=ORIENTED_EDGE('',*,*,#36268,.T.);
#49340=ORIENTED_EDGE('',*,*,#36655,.T.);
#49341=ORIENTED_EDGE('',*,*,#36657,.F.);
#49342=ORIENTED_EDGE('',*,*,#36658,.F.);
#49343=ORIENTED_EDGE('',*,*,#36274,.T.);
#49344=ORIENTED_EDGE('',*,*,#36273,.T.);
#49345=ORIENTED_EDGE('',*,*,#36659,.F.);
#49346=ORIENTED_EDGE('',*,*,#36277,.T.);
#49347=ORIENTED_EDGE('',*,*,#36275,.T.);
#49348=ORIENTED_EDGE('',*,*,#36658,.T.);
#49349=ORIENTED_EDGE('',*,*,#36660,.F.);
#49350=ORIENTED_EDGE('',*,*,#36661,.F.);
#49351=ORIENTED_EDGE('',*,*,#36281,.T.);
#49352=ORIENTED_EDGE('',*,*,#36280,.T.);
#49353=ORIENTED_EDGE('',*,*,#36662,.F.);
#49354=ORIENTED_EDGE('',*,*,#36284,.T.);
#49355=ORIENTED_EDGE('',*,*,#36282,.T.);
#49356=ORIENTED_EDGE('',*,*,#36661,.T.);
#49357=ORIENTED_EDGE('',*,*,#36663,.F.);
#49358=ORIENTED_EDGE('',*,*,#36664,.F.);
#49359=ORIENTED_EDGE('',*,*,#36288,.T.);
#49360=ORIENTED_EDGE('',*,*,#36287,.T.);
#49361=ORIENTED_EDGE('',*,*,#36665,.F.);
#49362=ORIENTED_EDGE('',*,*,#36291,.T.);
#49363=ORIENTED_EDGE('',*,*,#36289,.T.);
#49364=ORIENTED_EDGE('',*,*,#36664,.T.);
#49365=ORIENTED_EDGE('',*,*,#36666,.F.);
#49366=ORIENTED_EDGE('',*,*,#36667,.F.);
#49367=ORIENTED_EDGE('',*,*,#36295,.T.);
#49368=ORIENTED_EDGE('',*,*,#36294,.T.);
#49369=ORIENTED_EDGE('',*,*,#36668,.F.);
#49370=ORIENTED_EDGE('',*,*,#36298,.T.);
#49371=ORIENTED_EDGE('',*,*,#36296,.T.);
#49372=ORIENTED_EDGE('',*,*,#36667,.T.);
#49373=ORIENTED_EDGE('',*,*,#36669,.F.);
#49374=ORIENTED_EDGE('',*,*,#36670,.F.);
#49375=ORIENTED_EDGE('',*,*,#36302,.T.);
#49376=ORIENTED_EDGE('',*,*,#36301,.T.);
#49377=ORIENTED_EDGE('',*,*,#36671,.F.);
#49378=ORIENTED_EDGE('',*,*,#36305,.T.);
#49379=ORIENTED_EDGE('',*,*,#36303,.T.);
#49380=ORIENTED_EDGE('',*,*,#36670,.T.);
#49381=ORIENTED_EDGE('',*,*,#36672,.F.);
#49382=ORIENTED_EDGE('',*,*,#36673,.F.);
#49383=ORIENTED_EDGE('',*,*,#36309,.T.);
#49384=ORIENTED_EDGE('',*,*,#36308,.T.);
#49385=ORIENTED_EDGE('',*,*,#36674,.F.);
#49386=ORIENTED_EDGE('',*,*,#36312,.T.);
#49387=ORIENTED_EDGE('',*,*,#36310,.T.);
#49388=ORIENTED_EDGE('',*,*,#36673,.T.);
#49389=ORIENTED_EDGE('',*,*,#36675,.F.);
#49390=ORIENTED_EDGE('',*,*,#36676,.F.);
#49391=ORIENTED_EDGE('',*,*,#36316,.T.);
#49392=ORIENTED_EDGE('',*,*,#36315,.T.);
#49393=ORIENTED_EDGE('',*,*,#36677,.F.);
#49394=ORIENTED_EDGE('',*,*,#36319,.T.);
#49395=ORIENTED_EDGE('',*,*,#36317,.T.);
#49396=ORIENTED_EDGE('',*,*,#36676,.T.);
#49397=ORIENTED_EDGE('',*,*,#36678,.F.);
#49398=ORIENTED_EDGE('',*,*,#36679,.F.);
#49399=ORIENTED_EDGE('',*,*,#36323,.T.);
#49400=ORIENTED_EDGE('',*,*,#36322,.T.);
#49401=ORIENTED_EDGE('',*,*,#36680,.F.);
#49402=ORIENTED_EDGE('',*,*,#36326,.T.);
#49403=ORIENTED_EDGE('',*,*,#36324,.T.);
#49404=ORIENTED_EDGE('',*,*,#36679,.T.);
#49405=ORIENTED_EDGE('',*,*,#36681,.F.);
#49406=ORIENTED_EDGE('',*,*,#36682,.F.);
#49407=ORIENTED_EDGE('',*,*,#36330,.T.);
#49408=ORIENTED_EDGE('',*,*,#36329,.T.);
#49409=ORIENTED_EDGE('',*,*,#36683,.F.);
#49410=ORIENTED_EDGE('',*,*,#36333,.T.);
#49411=ORIENTED_EDGE('',*,*,#36331,.T.);
#49412=ORIENTED_EDGE('',*,*,#36682,.T.);
#49413=ORIENTED_EDGE('',*,*,#36684,.F.);
#49414=ORIENTED_EDGE('',*,*,#36685,.F.);
#49415=ORIENTED_EDGE('',*,*,#36337,.T.);
#49416=ORIENTED_EDGE('',*,*,#36336,.T.);
#49417=ORIENTED_EDGE('',*,*,#36686,.F.);
#49418=ORIENTED_EDGE('',*,*,#36340,.T.);
#49419=ORIENTED_EDGE('',*,*,#36338,.T.);
#49420=ORIENTED_EDGE('',*,*,#36685,.T.);
#49421=ORIENTED_EDGE('',*,*,#36687,.F.);
#49422=ORIENTED_EDGE('',*,*,#36688,.F.);
#49423=ORIENTED_EDGE('',*,*,#34442,.T.);
#49424=ORIENTED_EDGE('',*,*,#36342,.T.);
#49425=ORIENTED_EDGE('',*,*,#36689,.F.);
#49426=ORIENTED_EDGE('',*,*,#36343,.T.);
#49427=ORIENTED_EDGE('',*,*,#34443,.T.);
#49428=ORIENTED_EDGE('',*,*,#36688,.T.);
#49429=ORIENTED_EDGE('',*,*,#36690,.F.);
#49430=ORIENTED_EDGE('',*,*,#36691,.F.);
#49431=ORIENTED_EDGE('',*,*,#36347,.T.);
#49432=ORIENTED_EDGE('',*,*,#36346,.T.);
#49433=ORIENTED_EDGE('',*,*,#36692,.F.);
#49434=ORIENTED_EDGE('',*,*,#36350,.T.);
#49435=ORIENTED_EDGE('',*,*,#36348,.T.);
#49436=ORIENTED_EDGE('',*,*,#36691,.T.);
#49437=ORIENTED_EDGE('',*,*,#36693,.F.);
#49438=ORIENTED_EDGE('',*,*,#36694,.F.);
#49439=ORIENTED_EDGE('',*,*,#36354,.T.);
#49440=ORIENTED_EDGE('',*,*,#36353,.T.);
#49441=ORIENTED_EDGE('',*,*,#36695,.F.);
#49442=ORIENTED_EDGE('',*,*,#36357,.T.);
#49443=ORIENTED_EDGE('',*,*,#36355,.T.);
#49444=ORIENTED_EDGE('',*,*,#36694,.T.);
#49445=ORIENTED_EDGE('',*,*,#36696,.F.);
#49446=ORIENTED_EDGE('',*,*,#36697,.F.);
#49447=ORIENTED_EDGE('',*,*,#36361,.T.);
#49448=ORIENTED_EDGE('',*,*,#36360,.T.);
#49449=ORIENTED_EDGE('',*,*,#36698,.F.);
#49450=ORIENTED_EDGE('',*,*,#36364,.T.);
#49451=ORIENTED_EDGE('',*,*,#36362,.T.);
#49452=ORIENTED_EDGE('',*,*,#36697,.T.);
#49453=ORIENTED_EDGE('',*,*,#36699,.F.);
#49454=ORIENTED_EDGE('',*,*,#36700,.F.);
#49455=ORIENTED_EDGE('',*,*,#36368,.T.);
#49456=ORIENTED_EDGE('',*,*,#36367,.T.);
#49457=ORIENTED_EDGE('',*,*,#36701,.F.);
#49458=ORIENTED_EDGE('',*,*,#36371,.T.);
#49459=ORIENTED_EDGE('',*,*,#36369,.T.);
#49460=ORIENTED_EDGE('',*,*,#36700,.T.);
#49461=ORIENTED_EDGE('',*,*,#36702,.F.);
#49462=ORIENTED_EDGE('',*,*,#36703,.F.);
#49463=ORIENTED_EDGE('',*,*,#36375,.T.);
#49464=ORIENTED_EDGE('',*,*,#36374,.T.);
#49465=ORIENTED_EDGE('',*,*,#36704,.F.);
#49466=ORIENTED_EDGE('',*,*,#36378,.T.);
#49467=ORIENTED_EDGE('',*,*,#36376,.T.);
#49468=ORIENTED_EDGE('',*,*,#36703,.T.);
#49469=ORIENTED_EDGE('',*,*,#36705,.F.);
#49470=ORIENTED_EDGE('',*,*,#36706,.F.);
#49471=ORIENTED_EDGE('',*,*,#36382,.T.);
#49472=ORIENTED_EDGE('',*,*,#36381,.T.);
#49473=ORIENTED_EDGE('',*,*,#36707,.F.);
#49474=ORIENTED_EDGE('',*,*,#36385,.T.);
#49475=ORIENTED_EDGE('',*,*,#36383,.T.);
#49476=ORIENTED_EDGE('',*,*,#36706,.T.);
#49477=ORIENTED_EDGE('',*,*,#36708,.F.);
#49478=ORIENTED_EDGE('',*,*,#36709,.F.);
#49479=ORIENTED_EDGE('',*,*,#36389,.T.);
#49480=ORIENTED_EDGE('',*,*,#36388,.T.);
#49481=ORIENTED_EDGE('',*,*,#36710,.F.);
#49482=ORIENTED_EDGE('',*,*,#36392,.T.);
#49483=ORIENTED_EDGE('',*,*,#36390,.T.);
#49484=ORIENTED_EDGE('',*,*,#36709,.T.);
#49485=ORIENTED_EDGE('',*,*,#36711,.F.);
#49486=ORIENTED_EDGE('',*,*,#36712,.F.);
#49487=ORIENTED_EDGE('',*,*,#36396,.T.);
#49488=ORIENTED_EDGE('',*,*,#36395,.T.);
#49489=ORIENTED_EDGE('',*,*,#36713,.F.);
#49490=ORIENTED_EDGE('',*,*,#36399,.T.);
#49491=ORIENTED_EDGE('',*,*,#36397,.T.);
#49492=ORIENTED_EDGE('',*,*,#36712,.T.);
#49493=ORIENTED_EDGE('',*,*,#36714,.F.);
#49494=ORIENTED_EDGE('',*,*,#36715,.F.);
#49495=ORIENTED_EDGE('',*,*,#36405,.T.);
#49496=ORIENTED_EDGE('',*,*,#36402,.T.);
#49497=ORIENTED_EDGE('',*,*,#36406,.T.);
#49498=ORIENTED_EDGE('',*,*,#36715,.T.);
#49499=ORIENTED_EDGE('',*,*,#36716,.F.);
#49500=ORIENTED_EDGE('',*,*,#36404,.T.);
#49501=ORIENTED_EDGE('',*,*,#36411,.T.);
#49502=ORIENTED_EDGE('',*,*,#36407,.T.);
#49503=ORIENTED_EDGE('',*,*,#36717,.F.);
#49504=ORIENTED_EDGE('',*,*,#36718,.F.);
#49505=ORIENTED_EDGE('',*,*,#36719,.F.);
#49506=ORIENTED_EDGE('',*,*,#36413,.T.);
#49507=ORIENTED_EDGE('',*,*,#36412,.T.);
#49508=ORIENTED_EDGE('',*,*,#36718,.T.);
#49509=ORIENTED_EDGE('',*,*,#36720,.F.);
#49510=ORIENTED_EDGE('',*,*,#36721,.F.);
#49511=ORIENTED_EDGE('',*,*,#36417,.T.);
#49512=ORIENTED_EDGE('',*,*,#36416,.T.);
#49513=ORIENTED_EDGE('',*,*,#36722,.F.);
#49514=ORIENTED_EDGE('',*,*,#36420,.T.);
#49515=ORIENTED_EDGE('',*,*,#36418,.T.);
#49516=ORIENTED_EDGE('',*,*,#36721,.T.);
#49517=ORIENTED_EDGE('',*,*,#36723,.F.);
#49518=ORIENTED_EDGE('',*,*,#36724,.F.);
#49519=ORIENTED_EDGE('',*,*,#36424,.T.);
#49520=ORIENTED_EDGE('',*,*,#36423,.T.);
#49521=ORIENTED_EDGE('',*,*,#36725,.F.);
#49522=ORIENTED_EDGE('',*,*,#36427,.T.);
#49523=ORIENTED_EDGE('',*,*,#36425,.T.);
#49524=ORIENTED_EDGE('',*,*,#36724,.T.);
#49525=ORIENTED_EDGE('',*,*,#36726,.F.);
#49526=ORIENTED_EDGE('',*,*,#36727,.F.);
#49527=ORIENTED_EDGE('',*,*,#36431,.T.);
#49528=ORIENTED_EDGE('',*,*,#36430,.T.);
#49529=ORIENTED_EDGE('',*,*,#36728,.F.);
#49530=ORIENTED_EDGE('',*,*,#36434,.T.);
#49531=ORIENTED_EDGE('',*,*,#36432,.T.);
#49532=ORIENTED_EDGE('',*,*,#36727,.T.);
#49533=ORIENTED_EDGE('',*,*,#36729,.F.);
#49534=ORIENTED_EDGE('',*,*,#36730,.F.);
#49535=ORIENTED_EDGE('',*,*,#36438,.T.);
#49536=ORIENTED_EDGE('',*,*,#36437,.T.);
#49537=ORIENTED_EDGE('',*,*,#36731,.F.);
#49538=ORIENTED_EDGE('',*,*,#36441,.T.);
#49539=ORIENTED_EDGE('',*,*,#36439,.T.);
#49540=ORIENTED_EDGE('',*,*,#36730,.T.);
#49541=ORIENTED_EDGE('',*,*,#36732,.F.);
#49542=ORIENTED_EDGE('',*,*,#36733,.F.);
#49543=ORIENTED_EDGE('',*,*,#36447,.T.);
#49544=ORIENTED_EDGE('',*,*,#36442,.T.);
#49545=ORIENTED_EDGE('',*,*,#36448,.T.);
#49546=ORIENTED_EDGE('',*,*,#36733,.T.);
#49547=ORIENTED_EDGE('',*,*,#36734,.F.);
#49548=ORIENTED_EDGE('',*,*,#36446,.T.);
#49549=ORIENTED_EDGE('',*,*,#36454,.T.);
#49550=ORIENTED_EDGE('',*,*,#36449,.T.);
#49551=ORIENTED_EDGE('',*,*,#36735,.F.);
#49552=ORIENTED_EDGE('',*,*,#36736,.F.);
#49553=ORIENTED_EDGE('',*,*,#36455,.T.);
#49554=ORIENTED_EDGE('',*,*,#36736,.T.);
#49555=ORIENTED_EDGE('',*,*,#36737,.F.);
#49556=ORIENTED_EDGE('',*,*,#36453,.T.);
#49557=ORIENTED_EDGE('',*,*,#36461,.T.);
#49558=ORIENTED_EDGE('',*,*,#36456,.T.);
#49559=ORIENTED_EDGE('',*,*,#36738,.F.);
#49560=ORIENTED_EDGE('',*,*,#36739,.F.);
#49561=ORIENTED_EDGE('',*,*,#36462,.T.);
#49562=ORIENTED_EDGE('',*,*,#36739,.T.);
#49563=ORIENTED_EDGE('',*,*,#36740,.F.);
#49564=ORIENTED_EDGE('',*,*,#36460,.T.);
#49565=ORIENTED_EDGE('',*,*,#36468,.T.);
#49566=ORIENTED_EDGE('',*,*,#36463,.T.);
#49567=ORIENTED_EDGE('',*,*,#36741,.F.);
#49568=ORIENTED_EDGE('',*,*,#36742,.F.);
#49569=ORIENTED_EDGE('',*,*,#36469,.T.);
#49570=ORIENTED_EDGE('',*,*,#36742,.T.);
#49571=ORIENTED_EDGE('',*,*,#36743,.F.);
#49572=ORIENTED_EDGE('',*,*,#36467,.T.);
#49573=ORIENTED_EDGE('',*,*,#36475,.T.);
#49574=ORIENTED_EDGE('',*,*,#36470,.T.);
#49575=ORIENTED_EDGE('',*,*,#36744,.F.);
#49576=ORIENTED_EDGE('',*,*,#36745,.F.);
#49577=ORIENTED_EDGE('',*,*,#36476,.T.);
#49578=ORIENTED_EDGE('',*,*,#36745,.T.);
#49579=ORIENTED_EDGE('',*,*,#36746,.F.);
#49580=ORIENTED_EDGE('',*,*,#36474,.T.);
#49581=ORIENTED_EDGE('',*,*,#36482,.T.);
#49582=ORIENTED_EDGE('',*,*,#36477,.T.);
#49583=ORIENTED_EDGE('',*,*,#36747,.F.);
#49584=ORIENTED_EDGE('',*,*,#36748,.F.);
#49585=ORIENTED_EDGE('',*,*,#36483,.T.);
#49586=ORIENTED_EDGE('',*,*,#36748,.T.);
#49587=ORIENTED_EDGE('',*,*,#36749,.F.);
#49588=ORIENTED_EDGE('',*,*,#36481,.T.);
#49589=ORIENTED_EDGE('',*,*,#36489,.T.);
#49590=ORIENTED_EDGE('',*,*,#36484,.T.);
#49591=ORIENTED_EDGE('',*,*,#36750,.F.);
#49592=ORIENTED_EDGE('',*,*,#36751,.F.);
#49593=ORIENTED_EDGE('',*,*,#36490,.T.);
#49594=ORIENTED_EDGE('',*,*,#36751,.T.);
#49595=ORIENTED_EDGE('',*,*,#36752,.F.);
#49596=ORIENTED_EDGE('',*,*,#36488,.T.);
#49597=ORIENTED_EDGE('',*,*,#36496,.T.);
#49598=ORIENTED_EDGE('',*,*,#36491,.T.);
#49599=ORIENTED_EDGE('',*,*,#36753,.F.);
#49600=ORIENTED_EDGE('',*,*,#36754,.F.);
#49601=ORIENTED_EDGE('',*,*,#36497,.T.);
#49602=ORIENTED_EDGE('',*,*,#36754,.T.);
#49603=ORIENTED_EDGE('',*,*,#36755,.F.);
#49604=ORIENTED_EDGE('',*,*,#36495,.T.);
#49605=ORIENTED_EDGE('',*,*,#36503,.T.);
#49606=ORIENTED_EDGE('',*,*,#36498,.T.);
#49607=ORIENTED_EDGE('',*,*,#36756,.F.);
#49608=ORIENTED_EDGE('',*,*,#36757,.F.);
#49609=ORIENTED_EDGE('',*,*,#36504,.T.);
#49610=ORIENTED_EDGE('',*,*,#36757,.T.);
#49611=ORIENTED_EDGE('',*,*,#36758,.F.);
#49612=ORIENTED_EDGE('',*,*,#36502,.T.);
#49613=ORIENTED_EDGE('',*,*,#36510,.T.);
#49614=ORIENTED_EDGE('',*,*,#36505,.T.);
#49615=ORIENTED_EDGE('',*,*,#36759,.F.);
#49616=ORIENTED_EDGE('',*,*,#36760,.F.);
#49617=ORIENTED_EDGE('',*,*,#36511,.T.);
#49618=ORIENTED_EDGE('',*,*,#36760,.T.);
#49619=ORIENTED_EDGE('',*,*,#36761,.F.);
#49620=ORIENTED_EDGE('',*,*,#36509,.T.);
#49621=ORIENTED_EDGE('',*,*,#36517,.T.);
#49622=ORIENTED_EDGE('',*,*,#36512,.T.);
#49623=ORIENTED_EDGE('',*,*,#36762,.F.);
#49624=ORIENTED_EDGE('',*,*,#36763,.F.);
#49625=ORIENTED_EDGE('',*,*,#36518,.T.);
#49626=ORIENTED_EDGE('',*,*,#36763,.T.);
#49627=ORIENTED_EDGE('',*,*,#36764,.F.);
#49628=ORIENTED_EDGE('',*,*,#36516,.T.);
#49629=ORIENTED_EDGE('',*,*,#36524,.T.);
#49630=ORIENTED_EDGE('',*,*,#36519,.T.);
#49631=ORIENTED_EDGE('',*,*,#36765,.F.);
#49632=ORIENTED_EDGE('',*,*,#36766,.F.);
#49633=ORIENTED_EDGE('',*,*,#36525,.T.);
#49634=ORIENTED_EDGE('',*,*,#36766,.T.);
#49635=ORIENTED_EDGE('',*,*,#36767,.F.);
#49636=ORIENTED_EDGE('',*,*,#36523,.T.);
#49637=ORIENTED_EDGE('',*,*,#36531,.T.);
#49638=ORIENTED_EDGE('',*,*,#36526,.T.);
#49639=ORIENTED_EDGE('',*,*,#36768,.F.);
#49640=ORIENTED_EDGE('',*,*,#36769,.F.);
#49641=ORIENTED_EDGE('',*,*,#36532,.T.);
#49642=ORIENTED_EDGE('',*,*,#36769,.T.);
#49643=ORIENTED_EDGE('',*,*,#36770,.F.);
#49644=ORIENTED_EDGE('',*,*,#36530,.T.);
#49645=ORIENTED_EDGE('',*,*,#36538,.T.);
#49646=ORIENTED_EDGE('',*,*,#36533,.T.);
#49647=ORIENTED_EDGE('',*,*,#36771,.F.);
#49648=ORIENTED_EDGE('',*,*,#36772,.F.);
#49649=ORIENTED_EDGE('',*,*,#36539,.T.);
#49650=ORIENTED_EDGE('',*,*,#36772,.T.);
#49651=ORIENTED_EDGE('',*,*,#36773,.F.);
#49652=ORIENTED_EDGE('',*,*,#36537,.T.);
#49653=ORIENTED_EDGE('',*,*,#36545,.T.);
#49654=ORIENTED_EDGE('',*,*,#36540,.T.);
#49655=ORIENTED_EDGE('',*,*,#36774,.F.);
#49656=ORIENTED_EDGE('',*,*,#36775,.F.);
#49657=ORIENTED_EDGE('',*,*,#36546,.T.);
#49658=ORIENTED_EDGE('',*,*,#36775,.T.);
#49659=ORIENTED_EDGE('',*,*,#36776,.F.);
#49660=ORIENTED_EDGE('',*,*,#36544,.T.);
#49661=ORIENTED_EDGE('',*,*,#36552,.T.);
#49662=ORIENTED_EDGE('',*,*,#36547,.T.);
#49663=ORIENTED_EDGE('',*,*,#36777,.F.);
#49664=ORIENTED_EDGE('',*,*,#36778,.F.);
#49665=ORIENTED_EDGE('',*,*,#36553,.T.);
#49666=ORIENTED_EDGE('',*,*,#36778,.T.);
#49667=ORIENTED_EDGE('',*,*,#36779,.F.);
#49668=ORIENTED_EDGE('',*,*,#36551,.T.);
#49669=ORIENTED_EDGE('',*,*,#36559,.T.);
#49670=ORIENTED_EDGE('',*,*,#36554,.T.);
#49671=ORIENTED_EDGE('',*,*,#36780,.F.);
#49672=ORIENTED_EDGE('',*,*,#36781,.F.);
#49673=ORIENTED_EDGE('',*,*,#36560,.T.);
#49674=ORIENTED_EDGE('',*,*,#36781,.T.);
#49675=ORIENTED_EDGE('',*,*,#36782,.F.);
#49676=ORIENTED_EDGE('',*,*,#36558,.T.);
#49677=ORIENTED_EDGE('',*,*,#36566,.T.);
#49678=ORIENTED_EDGE('',*,*,#36561,.T.);
#49679=ORIENTED_EDGE('',*,*,#36783,.F.);
#49680=ORIENTED_EDGE('',*,*,#36784,.F.);
#49681=ORIENTED_EDGE('',*,*,#36567,.T.);
#49682=ORIENTED_EDGE('',*,*,#36784,.T.);
#49683=ORIENTED_EDGE('',*,*,#36785,.F.);
#49684=ORIENTED_EDGE('',*,*,#36565,.T.);
#49685=ORIENTED_EDGE('',*,*,#36573,.T.);
#49686=ORIENTED_EDGE('',*,*,#36568,.T.);
#49687=ORIENTED_EDGE('',*,*,#36786,.F.);
#49688=ORIENTED_EDGE('',*,*,#36787,.F.);
#49689=ORIENTED_EDGE('',*,*,#36574,.T.);
#49690=ORIENTED_EDGE('',*,*,#36787,.T.);
#49691=ORIENTED_EDGE('',*,*,#36788,.F.);
#49692=ORIENTED_EDGE('',*,*,#36572,.T.);
#49693=ORIENTED_EDGE('',*,*,#36580,.T.);
#49694=ORIENTED_EDGE('',*,*,#36575,.T.);
#49695=ORIENTED_EDGE('',*,*,#36789,.F.);
#49696=ORIENTED_EDGE('',*,*,#36790,.F.);
#49697=ORIENTED_EDGE('',*,*,#36581,.T.);
#49698=ORIENTED_EDGE('',*,*,#36790,.T.);
#49699=ORIENTED_EDGE('',*,*,#36791,.F.);
#49700=ORIENTED_EDGE('',*,*,#36579,.T.);
#49701=ORIENTED_EDGE('',*,*,#36587,.T.);
#49702=ORIENTED_EDGE('',*,*,#36582,.T.);
#49703=ORIENTED_EDGE('',*,*,#36792,.F.);
#49704=ORIENTED_EDGE('',*,*,#36793,.F.);
#49705=ORIENTED_EDGE('',*,*,#36588,.T.);
#49706=ORIENTED_EDGE('',*,*,#36793,.T.);
#49707=ORIENTED_EDGE('',*,*,#36794,.F.);
#49708=ORIENTED_EDGE('',*,*,#36586,.T.);
#49709=ORIENTED_EDGE('',*,*,#36594,.T.);
#49710=ORIENTED_EDGE('',*,*,#36589,.T.);
#49711=ORIENTED_EDGE('',*,*,#36795,.F.);
#49712=ORIENTED_EDGE('',*,*,#36796,.F.);
#49713=ORIENTED_EDGE('',*,*,#36595,.T.);
#49714=ORIENTED_EDGE('',*,*,#36796,.T.);
#49715=ORIENTED_EDGE('',*,*,#36797,.F.);
#49716=ORIENTED_EDGE('',*,*,#36593,.T.);
#49717=ORIENTED_EDGE('',*,*,#36601,.T.);
#49718=ORIENTED_EDGE('',*,*,#36596,.T.);
#49719=ORIENTED_EDGE('',*,*,#36798,.F.);
#49720=ORIENTED_EDGE('',*,*,#36799,.F.);
#49721=ORIENTED_EDGE('',*,*,#36602,.T.);
#49722=ORIENTED_EDGE('',*,*,#36799,.T.);
#49723=ORIENTED_EDGE('',*,*,#36800,.F.);
#49724=ORIENTED_EDGE('',*,*,#36600,.T.);
#49725=ORIENTED_EDGE('',*,*,#36608,.T.);
#49726=ORIENTED_EDGE('',*,*,#36603,.T.);
#49727=ORIENTED_EDGE('',*,*,#36801,.F.);
#49728=ORIENTED_EDGE('',*,*,#36802,.F.);
#49729=ORIENTED_EDGE('',*,*,#36609,.T.);
#49730=ORIENTED_EDGE('',*,*,#36802,.T.);
#49731=ORIENTED_EDGE('',*,*,#36803,.F.);
#49732=ORIENTED_EDGE('',*,*,#36607,.T.);
#49733=ORIENTED_EDGE('',*,*,#36615,.T.);
#49734=ORIENTED_EDGE('',*,*,#36610,.T.);
#49735=ORIENTED_EDGE('',*,*,#36804,.F.);
#49736=ORIENTED_EDGE('',*,*,#36805,.F.);
#49737=ORIENTED_EDGE('',*,*,#36616,.T.);
#49738=ORIENTED_EDGE('',*,*,#36805,.T.);
#49739=ORIENTED_EDGE('',*,*,#36806,.F.);
#49740=ORIENTED_EDGE('',*,*,#36614,.T.);
#49741=ORIENTED_EDGE('',*,*,#36622,.T.);
#49742=ORIENTED_EDGE('',*,*,#36617,.T.);
#49743=ORIENTED_EDGE('',*,*,#36807,.F.);
#49744=ORIENTED_EDGE('',*,*,#36808,.F.);
#49745=ORIENTED_EDGE('',*,*,#36623,.T.);
#49746=ORIENTED_EDGE('',*,*,#36808,.T.);
#49747=ORIENTED_EDGE('',*,*,#36809,.F.);
#49748=ORIENTED_EDGE('',*,*,#36621,.T.);
#49749=ORIENTED_EDGE('',*,*,#36629,.T.);
#49750=ORIENTED_EDGE('',*,*,#36624,.T.);
#49751=ORIENTED_EDGE('',*,*,#36810,.F.);
#49752=ORIENTED_EDGE('',*,*,#36811,.F.);
#49753=ORIENTED_EDGE('',*,*,#36630,.T.);
#49754=ORIENTED_EDGE('',*,*,#36811,.T.);
#49755=ORIENTED_EDGE('',*,*,#36812,.F.);
#49756=ORIENTED_EDGE('',*,*,#36628,.T.);
#49757=ORIENTED_EDGE('',*,*,#36636,.T.);
#49758=ORIENTED_EDGE('',*,*,#36631,.T.);
#49759=ORIENTED_EDGE('',*,*,#36813,.F.);
#49760=ORIENTED_EDGE('',*,*,#36814,.F.);
#49761=ORIENTED_EDGE('',*,*,#36637,.T.);
#49762=ORIENTED_EDGE('',*,*,#36814,.T.);
#49763=ORIENTED_EDGE('',*,*,#36815,.F.);
#49764=ORIENTED_EDGE('',*,*,#36635,.T.);
#49765=ORIENTED_EDGE('',*,*,#36643,.T.);
#49766=ORIENTED_EDGE('',*,*,#36638,.T.);
#49767=ORIENTED_EDGE('',*,*,#36816,.F.);
#49768=ORIENTED_EDGE('',*,*,#36817,.F.);
#49769=ORIENTED_EDGE('',*,*,#36644,.T.);
#49770=ORIENTED_EDGE('',*,*,#36817,.T.);
#49771=ORIENTED_EDGE('',*,*,#36818,.F.);
#49772=ORIENTED_EDGE('',*,*,#36642,.T.);
#49773=ORIENTED_EDGE('',*,*,#36819,.T.);
#49774=ORIENTED_EDGE('',*,*,#36820,.F.);
#49775=ORIENTED_EDGE('',*,*,#36645,.T.);
#49776=ORIENTED_EDGE('',*,*,#36821,.F.);
#49777=ORIENTED_EDGE('',*,*,#36822,.T.);
#49778=ORIENTED_EDGE('',*,*,#36823,.F.);
#49779=ORIENTED_EDGE('',*,*,#36647,.T.);
#49780=ORIENTED_EDGE('',*,*,#36824,.F.);
#49781=ORIENTED_EDGE('',*,*,#36825,.F.);
#49782=ORIENTED_EDGE('',*,*,#36826,.F.);
#49783=ORIENTED_EDGE('',*,*,#36827,.F.);
#49784=ORIENTED_EDGE('',*,*,#36822,.F.);
#49785=ORIENTED_EDGE('',*,*,#36827,.T.);
#49786=ORIENTED_EDGE('',*,*,#36828,.F.);
#49787=ORIENTED_EDGE('',*,*,#36648,.T.);
#49788=ORIENTED_EDGE('',*,*,#36823,.T.);
#49789=ORIENTED_EDGE('',*,*,#36829,.T.);
#49790=ORIENTED_EDGE('',*,*,#36830,.F.);
#49791=ORIENTED_EDGE('',*,*,#36650,.T.);
#49792=ORIENTED_EDGE('',*,*,#36831,.F.);
#49793=ORIENTED_EDGE('',*,*,#36832,.F.);
#49794=ORIENTED_EDGE('',*,*,#36833,.F.);
#49795=ORIENTED_EDGE('',*,*,#36834,.F.);
#49796=ORIENTED_EDGE('',*,*,#36829,.F.);
#49797=ORIENTED_EDGE('',*,*,#36834,.T.);
#49798=ORIENTED_EDGE('',*,*,#36835,.F.);
#49799=ORIENTED_EDGE('',*,*,#36651,.T.);
#49800=ORIENTED_EDGE('',*,*,#36830,.T.);
#49801=ORIENTED_EDGE('',*,*,#36836,.T.);
#49802=ORIENTED_EDGE('',*,*,#36837,.F.);
#49803=ORIENTED_EDGE('',*,*,#36653,.T.);
#49804=ORIENTED_EDGE('',*,*,#36838,.F.);
#49805=ORIENTED_EDGE('',*,*,#36839,.F.);
#49806=ORIENTED_EDGE('',*,*,#36840,.F.);
#49807=ORIENTED_EDGE('',*,*,#36841,.F.);
#49808=ORIENTED_EDGE('',*,*,#36836,.F.);
#49809=ORIENTED_EDGE('',*,*,#36841,.T.);
#49810=ORIENTED_EDGE('',*,*,#36842,.F.);
#49811=ORIENTED_EDGE('',*,*,#36654,.T.);
#49812=ORIENTED_EDGE('',*,*,#36837,.T.);
#49813=ORIENTED_EDGE('',*,*,#36843,.T.);
#49814=ORIENTED_EDGE('',*,*,#36844,.F.);
#49815=ORIENTED_EDGE('',*,*,#36656,.T.);
#49816=ORIENTED_EDGE('',*,*,#36845,.F.);
#49817=ORIENTED_EDGE('',*,*,#36846,.F.);
#49818=ORIENTED_EDGE('',*,*,#36847,.F.);
#49819=ORIENTED_EDGE('',*,*,#36848,.F.);
#49820=ORIENTED_EDGE('',*,*,#36843,.F.);
#49821=ORIENTED_EDGE('',*,*,#36848,.T.);
#49822=ORIENTED_EDGE('',*,*,#36849,.F.);
#49823=ORIENTED_EDGE('',*,*,#36657,.T.);
#49824=ORIENTED_EDGE('',*,*,#36844,.T.);
#49825=ORIENTED_EDGE('',*,*,#36850,.T.);
#49826=ORIENTED_EDGE('',*,*,#36851,.F.);
#49827=ORIENTED_EDGE('',*,*,#36659,.T.);
#49828=ORIENTED_EDGE('',*,*,#36852,.F.);
#49829=ORIENTED_EDGE('',*,*,#36853,.F.);
#49830=ORIENTED_EDGE('',*,*,#36854,.F.);
#49831=ORIENTED_EDGE('',*,*,#36855,.F.);
#49832=ORIENTED_EDGE('',*,*,#36850,.F.);
#49833=ORIENTED_EDGE('',*,*,#36855,.T.);
#49834=ORIENTED_EDGE('',*,*,#36856,.F.);
#49835=ORIENTED_EDGE('',*,*,#36660,.T.);
#49836=ORIENTED_EDGE('',*,*,#36851,.T.);
#49837=ORIENTED_EDGE('',*,*,#36857,.T.);
#49838=ORIENTED_EDGE('',*,*,#36858,.F.);
#49839=ORIENTED_EDGE('',*,*,#36662,.T.);
#49840=ORIENTED_EDGE('',*,*,#36859,.F.);
#49841=ORIENTED_EDGE('',*,*,#36860,.F.);
#49842=ORIENTED_EDGE('',*,*,#36861,.F.);
#49843=ORIENTED_EDGE('',*,*,#36862,.F.);
#49844=ORIENTED_EDGE('',*,*,#36857,.F.);
#49845=ORIENTED_EDGE('',*,*,#36862,.T.);
#49846=ORIENTED_EDGE('',*,*,#36863,.F.);
#49847=ORIENTED_EDGE('',*,*,#36663,.T.);
#49848=ORIENTED_EDGE('',*,*,#36858,.T.);
#49849=ORIENTED_EDGE('',*,*,#34438,.T.);
#49850=ORIENTED_EDGE('',*,*,#36864,.F.);
#49851=ORIENTED_EDGE('',*,*,#36665,.T.);
#49852=ORIENTED_EDGE('',*,*,#36865,.F.);
#49853=ORIENTED_EDGE('',*,*,#34437,.T.);
#49854=ORIENTED_EDGE('',*,*,#36866,.F.);
#49855=ORIENTED_EDGE('',*,*,#36666,.T.);
#49856=ORIENTED_EDGE('',*,*,#36864,.T.);
#49857=ORIENTED_EDGE('',*,*,#36867,.T.);
#49858=ORIENTED_EDGE('',*,*,#36868,.F.);
#49859=ORIENTED_EDGE('',*,*,#36668,.T.);
#49860=ORIENTED_EDGE('',*,*,#36869,.F.);
#49861=ORIENTED_EDGE('',*,*,#36870,.F.);
#49862=ORIENTED_EDGE('',*,*,#36871,.F.);
#49863=ORIENTED_EDGE('',*,*,#36872,.F.);
#49864=ORIENTED_EDGE('',*,*,#36867,.F.);
#49865=ORIENTED_EDGE('',*,*,#36872,.T.);
#49866=ORIENTED_EDGE('',*,*,#36873,.F.);
#49867=ORIENTED_EDGE('',*,*,#36669,.T.);
#49868=ORIENTED_EDGE('',*,*,#36868,.T.);
#49869=ORIENTED_EDGE('',*,*,#36874,.T.);
#49870=ORIENTED_EDGE('',*,*,#36875,.F.);
#49871=ORIENTED_EDGE('',*,*,#36671,.T.);
#49872=ORIENTED_EDGE('',*,*,#36876,.F.);
#49873=ORIENTED_EDGE('',*,*,#36877,.F.);
#49874=ORIENTED_EDGE('',*,*,#36878,.F.);
#49875=ORIENTED_EDGE('',*,*,#36879,.F.);
#49876=ORIENTED_EDGE('',*,*,#36874,.F.);
#49877=ORIENTED_EDGE('',*,*,#36879,.T.);
#49878=ORIENTED_EDGE('',*,*,#36880,.F.);
#49879=ORIENTED_EDGE('',*,*,#36672,.T.);
#49880=ORIENTED_EDGE('',*,*,#36875,.T.);
#49881=ORIENTED_EDGE('',*,*,#36881,.T.);
#49882=ORIENTED_EDGE('',*,*,#36882,.F.);
#49883=ORIENTED_EDGE('',*,*,#36674,.T.);
#49884=ORIENTED_EDGE('',*,*,#36883,.F.);
#49885=ORIENTED_EDGE('',*,*,#36884,.F.);
#49886=ORIENTED_EDGE('',*,*,#36885,.F.);
#49887=ORIENTED_EDGE('',*,*,#36886,.F.);
#49888=ORIENTED_EDGE('',*,*,#36881,.F.);
#49889=ORIENTED_EDGE('',*,*,#36886,.T.);
#49890=ORIENTED_EDGE('',*,*,#36887,.F.);
#49891=ORIENTED_EDGE('',*,*,#36675,.T.);
#49892=ORIENTED_EDGE('',*,*,#36882,.T.);
#49893=ORIENTED_EDGE('',*,*,#36888,.T.);
#49894=ORIENTED_EDGE('',*,*,#36889,.F.);
#49895=ORIENTED_EDGE('',*,*,#36677,.T.);
#49896=ORIENTED_EDGE('',*,*,#36890,.F.);
#49897=ORIENTED_EDGE('',*,*,#36891,.F.);
#49898=ORIENTED_EDGE('',*,*,#36892,.F.);
#49899=ORIENTED_EDGE('',*,*,#36893,.F.);
#49900=ORIENTED_EDGE('',*,*,#36888,.F.);
#49901=ORIENTED_EDGE('',*,*,#36893,.T.);
#49902=ORIENTED_EDGE('',*,*,#36894,.F.);
#49903=ORIENTED_EDGE('',*,*,#36678,.T.);
#49904=ORIENTED_EDGE('',*,*,#36889,.T.);
#49905=ORIENTED_EDGE('',*,*,#36895,.T.);
#49906=ORIENTED_EDGE('',*,*,#36896,.F.);
#49907=ORIENTED_EDGE('',*,*,#36680,.T.);
#49908=ORIENTED_EDGE('',*,*,#36897,.F.);
#49909=ORIENTED_EDGE('',*,*,#36898,.F.);
#49910=ORIENTED_EDGE('',*,*,#36899,.F.);
#49911=ORIENTED_EDGE('',*,*,#36900,.F.);
#49912=ORIENTED_EDGE('',*,*,#36895,.F.);
#49913=ORIENTED_EDGE('',*,*,#36900,.T.);
#49914=ORIENTED_EDGE('',*,*,#36901,.F.);
#49915=ORIENTED_EDGE('',*,*,#36681,.T.);
#49916=ORIENTED_EDGE('',*,*,#36896,.T.);
#49917=ORIENTED_EDGE('',*,*,#36902,.T.);
#49918=ORIENTED_EDGE('',*,*,#36903,.F.);
#49919=ORIENTED_EDGE('',*,*,#36683,.T.);
#49920=ORIENTED_EDGE('',*,*,#36904,.F.);
#49921=ORIENTED_EDGE('',*,*,#36905,.F.);
#49922=ORIENTED_EDGE('',*,*,#36906,.F.);
#49923=ORIENTED_EDGE('',*,*,#36907,.F.);
#49924=ORIENTED_EDGE('',*,*,#36902,.F.);
#49925=ORIENTED_EDGE('',*,*,#36907,.T.);
#49926=ORIENTED_EDGE('',*,*,#36908,.F.);
#49927=ORIENTED_EDGE('',*,*,#36684,.T.);
#49928=ORIENTED_EDGE('',*,*,#36903,.T.);
#49929=ORIENTED_EDGE('',*,*,#36909,.T.);
#49930=ORIENTED_EDGE('',*,*,#36910,.F.);
#49931=ORIENTED_EDGE('',*,*,#36686,.T.);
#49932=ORIENTED_EDGE('',*,*,#36911,.F.);
#49933=ORIENTED_EDGE('',*,*,#36912,.F.);
#49934=ORIENTED_EDGE('',*,*,#36913,.F.);
#49935=ORIENTED_EDGE('',*,*,#36914,.F.);
#49936=ORIENTED_EDGE('',*,*,#36909,.F.);
#49937=ORIENTED_EDGE('',*,*,#36914,.T.);
#49938=ORIENTED_EDGE('',*,*,#36915,.F.);
#49939=ORIENTED_EDGE('',*,*,#36687,.T.);
#49940=ORIENTED_EDGE('',*,*,#36910,.T.);
#49941=ORIENTED_EDGE('',*,*,#36916,.T.);
#49942=ORIENTED_EDGE('',*,*,#36917,.F.);
#49943=ORIENTED_EDGE('',*,*,#36689,.T.);
#49944=ORIENTED_EDGE('',*,*,#36918,.F.);
#49945=ORIENTED_EDGE('',*,*,#36919,.F.);
#49946=ORIENTED_EDGE('',*,*,#36920,.F.);
#49947=ORIENTED_EDGE('',*,*,#36921,.F.);
#49948=ORIENTED_EDGE('',*,*,#36916,.F.);
#49949=ORIENTED_EDGE('',*,*,#36921,.T.);
#49950=ORIENTED_EDGE('',*,*,#36922,.F.);
#49951=ORIENTED_EDGE('',*,*,#36690,.T.);
#49952=ORIENTED_EDGE('',*,*,#36917,.T.);
#49953=ORIENTED_EDGE('',*,*,#36923,.T.);
#49954=ORIENTED_EDGE('',*,*,#36924,.F.);
#49955=ORIENTED_EDGE('',*,*,#36692,.T.);
#49956=ORIENTED_EDGE('',*,*,#36925,.F.);
#49957=ORIENTED_EDGE('',*,*,#36926,.F.);
#49958=ORIENTED_EDGE('',*,*,#36927,.F.);
#49959=ORIENTED_EDGE('',*,*,#36928,.F.);
#49960=ORIENTED_EDGE('',*,*,#36923,.F.);
#49961=ORIENTED_EDGE('',*,*,#36928,.T.);
#49962=ORIENTED_EDGE('',*,*,#36929,.F.);
#49963=ORIENTED_EDGE('',*,*,#36693,.T.);
#49964=ORIENTED_EDGE('',*,*,#36924,.T.);
#49965=ORIENTED_EDGE('',*,*,#36930,.T.);
#49966=ORIENTED_EDGE('',*,*,#36931,.F.);
#49967=ORIENTED_EDGE('',*,*,#36695,.T.);
#49968=ORIENTED_EDGE('',*,*,#36932,.F.);
#49969=ORIENTED_EDGE('',*,*,#36933,.F.);
#49970=ORIENTED_EDGE('',*,*,#36934,.F.);
#49971=ORIENTED_EDGE('',*,*,#36935,.F.);
#49972=ORIENTED_EDGE('',*,*,#36930,.F.);
#49973=ORIENTED_EDGE('',*,*,#36935,.T.);
#49974=ORIENTED_EDGE('',*,*,#36936,.F.);
#49975=ORIENTED_EDGE('',*,*,#36696,.T.);
#49976=ORIENTED_EDGE('',*,*,#36931,.T.);
#49977=ORIENTED_EDGE('',*,*,#36937,.T.);
#49978=ORIENTED_EDGE('',*,*,#36938,.F.);
#49979=ORIENTED_EDGE('',*,*,#36698,.T.);
#49980=ORIENTED_EDGE('',*,*,#36939,.F.);
#49981=ORIENTED_EDGE('',*,*,#36940,.F.);
#49982=ORIENTED_EDGE('',*,*,#36941,.F.);
#49983=ORIENTED_EDGE('',*,*,#36942,.F.);
#49984=ORIENTED_EDGE('',*,*,#36937,.F.);
#49985=ORIENTED_EDGE('',*,*,#36942,.T.);
#49986=ORIENTED_EDGE('',*,*,#36943,.F.);
#49987=ORIENTED_EDGE('',*,*,#36699,.T.);
#49988=ORIENTED_EDGE('',*,*,#36938,.T.);
#49989=ORIENTED_EDGE('',*,*,#36944,.T.);
#49990=ORIENTED_EDGE('',*,*,#36945,.F.);
#49991=ORIENTED_EDGE('',*,*,#36701,.T.);
#49992=ORIENTED_EDGE('',*,*,#36946,.F.);
#49993=ORIENTED_EDGE('',*,*,#36947,.F.);
#49994=ORIENTED_EDGE('',*,*,#36948,.F.);
#49995=ORIENTED_EDGE('',*,*,#36949,.F.);
#49996=ORIENTED_EDGE('',*,*,#36944,.F.);
#49997=ORIENTED_EDGE('',*,*,#36949,.T.);
#49998=ORIENTED_EDGE('',*,*,#36950,.F.);
#49999=ORIENTED_EDGE('',*,*,#36702,.T.);
#50000=ORIENTED_EDGE('',*,*,#36945,.T.);
#50001=ORIENTED_EDGE('',*,*,#36951,.T.);
#50002=ORIENTED_EDGE('',*,*,#36952,.F.);
#50003=ORIENTED_EDGE('',*,*,#36704,.T.);
#50004=ORIENTED_EDGE('',*,*,#36953,.F.);
#50005=ORIENTED_EDGE('',*,*,#36954,.F.);
#50006=ORIENTED_EDGE('',*,*,#36955,.F.);
#50007=ORIENTED_EDGE('',*,*,#36956,.F.);
#50008=ORIENTED_EDGE('',*,*,#36951,.F.);
#50009=ORIENTED_EDGE('',*,*,#36956,.T.);
#50010=ORIENTED_EDGE('',*,*,#36957,.F.);
#50011=ORIENTED_EDGE('',*,*,#36705,.T.);
#50012=ORIENTED_EDGE('',*,*,#36952,.T.);
#50013=ORIENTED_EDGE('',*,*,#36958,.T.);
#50014=ORIENTED_EDGE('',*,*,#36959,.F.);
#50015=ORIENTED_EDGE('',*,*,#36707,.T.);
#50016=ORIENTED_EDGE('',*,*,#36960,.F.);
#50017=ORIENTED_EDGE('',*,*,#36961,.F.);
#50018=ORIENTED_EDGE('',*,*,#36962,.F.);
#50019=ORIENTED_EDGE('',*,*,#36963,.F.);
#50020=ORIENTED_EDGE('',*,*,#36958,.F.);
#50021=ORIENTED_EDGE('',*,*,#36963,.T.);
#50022=ORIENTED_EDGE('',*,*,#36964,.F.);
#50023=ORIENTED_EDGE('',*,*,#36708,.T.);
#50024=ORIENTED_EDGE('',*,*,#36959,.T.);
#50025=ORIENTED_EDGE('',*,*,#36965,.T.);
#50026=ORIENTED_EDGE('',*,*,#36966,.F.);
#50027=ORIENTED_EDGE('',*,*,#36710,.T.);
#50028=ORIENTED_EDGE('',*,*,#36967,.F.);
#50029=ORIENTED_EDGE('',*,*,#36968,.F.);
#50030=ORIENTED_EDGE('',*,*,#36969,.F.);
#50031=ORIENTED_EDGE('',*,*,#36970,.F.);
#50032=ORIENTED_EDGE('',*,*,#36965,.F.);
#50033=ORIENTED_EDGE('',*,*,#36970,.T.);
#50034=ORIENTED_EDGE('',*,*,#36971,.F.);
#50035=ORIENTED_EDGE('',*,*,#36711,.T.);
#50036=ORIENTED_EDGE('',*,*,#36966,.T.);
#50037=ORIENTED_EDGE('',*,*,#36972,.T.);
#50038=ORIENTED_EDGE('',*,*,#36973,.F.);
#50039=ORIENTED_EDGE('',*,*,#36713,.T.);
#50040=ORIENTED_EDGE('',*,*,#36974,.F.);
#50041=ORIENTED_EDGE('',*,*,#36975,.T.);
#50042=ORIENTED_EDGE('',*,*,#36976,.F.);
#50043=ORIENTED_EDGE('',*,*,#36714,.T.);
#50044=ORIENTED_EDGE('',*,*,#36973,.T.);
#50045=ORIENTED_EDGE('',*,*,#36977,.F.);
#50046=ORIENTED_EDGE('',*,*,#36978,.F.);
#50047=ORIENTED_EDGE('',*,*,#36975,.F.);
#50048=ORIENTED_EDGE('',*,*,#36972,.F.);
#50049=ORIENTED_EDGE('',*,*,#36716,.T.);
#50050=ORIENTED_EDGE('',*,*,#36979,.F.);
#50051=ORIENTED_EDGE('',*,*,#36980,.T.);
#50052=ORIENTED_EDGE('',*,*,#36981,.F.);
#50053=ORIENTED_EDGE('',*,*,#36982,.F.);
#50054=ORIENTED_EDGE('',*,*,#36980,.F.);
#50055=ORIENTED_EDGE('',*,*,#36983,.F.);
#50056=ORIENTED_EDGE('',*,*,#36984,.F.);
#50057=ORIENTED_EDGE('',*,*,#36717,.T.);
#50058=ORIENTED_EDGE('',*,*,#36981,.T.);
#50059=ORIENTED_EDGE('',*,*,#36982,.T.);
#50060=ORIENTED_EDGE('',*,*,#36985,.F.);
#50061=ORIENTED_EDGE('',*,*,#36986,.T.);
#50062=ORIENTED_EDGE('',*,*,#36987,.F.);
#50063=ORIENTED_EDGE('',*,*,#36719,.T.);
#50064=ORIENTED_EDGE('',*,*,#36988,.F.);
#50065=ORIENTED_EDGE('',*,*,#36989,.F.);
#50066=ORIENTED_EDGE('',*,*,#36990,.F.);
#50067=ORIENTED_EDGE('',*,*,#36991,.F.);
#50068=ORIENTED_EDGE('',*,*,#36986,.F.);
#50069=ORIENTED_EDGE('',*,*,#36991,.T.);
#50070=ORIENTED_EDGE('',*,*,#36992,.F.);
#50071=ORIENTED_EDGE('',*,*,#36720,.T.);
#50072=ORIENTED_EDGE('',*,*,#36987,.T.);
#50073=ORIENTED_EDGE('',*,*,#36993,.T.);
#50074=ORIENTED_EDGE('',*,*,#36994,.F.);
#50075=ORIENTED_EDGE('',*,*,#36722,.T.);
#50076=ORIENTED_EDGE('',*,*,#36995,.F.);
#50077=ORIENTED_EDGE('',*,*,#36996,.F.);
#50078=ORIENTED_EDGE('',*,*,#36997,.F.);
#50079=ORIENTED_EDGE('',*,*,#36998,.F.);
#50080=ORIENTED_EDGE('',*,*,#36993,.F.);
#50081=ORIENTED_EDGE('',*,*,#36998,.T.);
#50082=ORIENTED_EDGE('',*,*,#36999,.F.);
#50083=ORIENTED_EDGE('',*,*,#36723,.T.);
#50084=ORIENTED_EDGE('',*,*,#36994,.T.);
#50085=ORIENTED_EDGE('',*,*,#37000,.T.);
#50086=ORIENTED_EDGE('',*,*,#37001,.F.);
#50087=ORIENTED_EDGE('',*,*,#36725,.T.);
#50088=ORIENTED_EDGE('',*,*,#37002,.F.);
#50089=ORIENTED_EDGE('',*,*,#37003,.F.);
#50090=ORIENTED_EDGE('',*,*,#37004,.F.);
#50091=ORIENTED_EDGE('',*,*,#37005,.F.);
#50092=ORIENTED_EDGE('',*,*,#37000,.F.);
#50093=ORIENTED_EDGE('',*,*,#37005,.T.);
#50094=ORIENTED_EDGE('',*,*,#37006,.F.);
#50095=ORIENTED_EDGE('',*,*,#36726,.T.);
#50096=ORIENTED_EDGE('',*,*,#37001,.T.);
#50097=ORIENTED_EDGE('',*,*,#37007,.T.);
#50098=ORIENTED_EDGE('',*,*,#37008,.F.);
#50099=ORIENTED_EDGE('',*,*,#36728,.T.);
#50100=ORIENTED_EDGE('',*,*,#37009,.F.);
#50101=ORIENTED_EDGE('',*,*,#37010,.F.);
#50102=ORIENTED_EDGE('',*,*,#37011,.F.);
#50103=ORIENTED_EDGE('',*,*,#37012,.F.);
#50104=ORIENTED_EDGE('',*,*,#37007,.F.);
#50105=ORIENTED_EDGE('',*,*,#37012,.T.);
#50106=ORIENTED_EDGE('',*,*,#37013,.F.);
#50107=ORIENTED_EDGE('',*,*,#36729,.T.);
#50108=ORIENTED_EDGE('',*,*,#37008,.T.);
#50109=ORIENTED_EDGE('',*,*,#37014,.F.);
#50110=ORIENTED_EDGE('',*,*,#37015,.F.);
#50111=ORIENTED_EDGE('',*,*,#36819,.F.);
#50112=ORIENTED_EDGE('',*,*,#37016,.F.);
#50113=ORIENTED_EDGE('',*,*,#37016,.T.);
#50114=ORIENTED_EDGE('',*,*,#36821,.T.);
#50115=ORIENTED_EDGE('',*,*,#36731,.T.);
#50116=ORIENTED_EDGE('',*,*,#37017,.F.);
#50117=ORIENTED_EDGE('',*,*,#37018,.T.);
#50118=ORIENTED_EDGE('',*,*,#37019,.F.);
#50119=ORIENTED_EDGE('',*,*,#36732,.T.);
#50120=ORIENTED_EDGE('',*,*,#37020,.F.);
#50121=ORIENTED_EDGE('',*,*,#36734,.T.);
#50122=ORIENTED_EDGE('',*,*,#37021,.F.);
#50123=ORIENTED_EDGE('',*,*,#37022,.T.);
#50124=ORIENTED_EDGE('',*,*,#37023,.F.);
#50125=ORIENTED_EDGE('',*,*,#36735,.T.);
#50126=ORIENTED_EDGE('',*,*,#37023,.T.);
#50127=ORIENTED_EDGE('',*,*,#37024,.T.);
#50128=ORIENTED_EDGE('',*,*,#37025,.F.);
#50129=ORIENTED_EDGE('',*,*,#37024,.F.);
#50130=ORIENTED_EDGE('',*,*,#37022,.F.);
#50131=ORIENTED_EDGE('',*,*,#37026,.F.);
#50132=ORIENTED_EDGE('',*,*,#37027,.F.);
#50133=ORIENTED_EDGE('',*,*,#36737,.T.);
#50134=ORIENTED_EDGE('',*,*,#37028,.F.);
#50135=ORIENTED_EDGE('',*,*,#37029,.T.);
#50136=ORIENTED_EDGE('',*,*,#37030,.F.);
#50137=ORIENTED_EDGE('',*,*,#36738,.T.);
#50138=ORIENTED_EDGE('',*,*,#37030,.T.);
#50139=ORIENTED_EDGE('',*,*,#37031,.T.);
#50140=ORIENTED_EDGE('',*,*,#37032,.F.);
#50141=ORIENTED_EDGE('',*,*,#37031,.F.);
#50142=ORIENTED_EDGE('',*,*,#37029,.F.);
#50143=ORIENTED_EDGE('',*,*,#37033,.F.);
#50144=ORIENTED_EDGE('',*,*,#37034,.F.);
#50145=ORIENTED_EDGE('',*,*,#36740,.T.);
#50146=ORIENTED_EDGE('',*,*,#37035,.F.);
#50147=ORIENTED_EDGE('',*,*,#37036,.T.);
#50148=ORIENTED_EDGE('',*,*,#37037,.F.);
#50149=ORIENTED_EDGE('',*,*,#36741,.T.);
#50150=ORIENTED_EDGE('',*,*,#37037,.T.);
#50151=ORIENTED_EDGE('',*,*,#37038,.T.);
#50152=ORIENTED_EDGE('',*,*,#37039,.F.);
#50153=ORIENTED_EDGE('',*,*,#37038,.F.);
#50154=ORIENTED_EDGE('',*,*,#37036,.F.);
#50155=ORIENTED_EDGE('',*,*,#37040,.F.);
#50156=ORIENTED_EDGE('',*,*,#37041,.F.);
#50157=ORIENTED_EDGE('',*,*,#36743,.T.);
#50158=ORIENTED_EDGE('',*,*,#37042,.F.);
#50159=ORIENTED_EDGE('',*,*,#37043,.T.);
#50160=ORIENTED_EDGE('',*,*,#37044,.F.);
#50161=ORIENTED_EDGE('',*,*,#36744,.T.);
#50162=ORIENTED_EDGE('',*,*,#37044,.T.);
#50163=ORIENTED_EDGE('',*,*,#37045,.T.);
#50164=ORIENTED_EDGE('',*,*,#37046,.F.);
#50165=ORIENTED_EDGE('',*,*,#37045,.F.);
#50166=ORIENTED_EDGE('',*,*,#37043,.F.);
#50167=ORIENTED_EDGE('',*,*,#37047,.F.);
#50168=ORIENTED_EDGE('',*,*,#37048,.F.);
#50169=ORIENTED_EDGE('',*,*,#36746,.T.);
#50170=ORIENTED_EDGE('',*,*,#37049,.F.);
#50171=ORIENTED_EDGE('',*,*,#37050,.T.);
#50172=ORIENTED_EDGE('',*,*,#37051,.F.);
#50173=ORIENTED_EDGE('',*,*,#36747,.T.);
#50174=ORIENTED_EDGE('',*,*,#37051,.T.);
#50175=ORIENTED_EDGE('',*,*,#37052,.T.);
#50176=ORIENTED_EDGE('',*,*,#37053,.F.);
#50177=ORIENTED_EDGE('',*,*,#37052,.F.);
#50178=ORIENTED_EDGE('',*,*,#37050,.F.);
#50179=ORIENTED_EDGE('',*,*,#37054,.F.);
#50180=ORIENTED_EDGE('',*,*,#37055,.F.);
#50181=ORIENTED_EDGE('',*,*,#36749,.T.);
#50182=ORIENTED_EDGE('',*,*,#37056,.F.);
#50183=ORIENTED_EDGE('',*,*,#37057,.T.);
#50184=ORIENTED_EDGE('',*,*,#37058,.F.);
#50185=ORIENTED_EDGE('',*,*,#36750,.T.);
#50186=ORIENTED_EDGE('',*,*,#37058,.T.);
#50187=ORIENTED_EDGE('',*,*,#37059,.T.);
#50188=ORIENTED_EDGE('',*,*,#37060,.F.);
#50189=ORIENTED_EDGE('',*,*,#37059,.F.);
#50190=ORIENTED_EDGE('',*,*,#37057,.F.);
#50191=ORIENTED_EDGE('',*,*,#37061,.F.);
#50192=ORIENTED_EDGE('',*,*,#37062,.F.);
#50193=ORIENTED_EDGE('',*,*,#36752,.T.);
#50194=ORIENTED_EDGE('',*,*,#37063,.F.);
#50195=ORIENTED_EDGE('',*,*,#37064,.T.);
#50196=ORIENTED_EDGE('',*,*,#37065,.F.);
#50197=ORIENTED_EDGE('',*,*,#36753,.T.);
#50198=ORIENTED_EDGE('',*,*,#37065,.T.);
#50199=ORIENTED_EDGE('',*,*,#37066,.T.);
#50200=ORIENTED_EDGE('',*,*,#37067,.F.);
#50201=ORIENTED_EDGE('',*,*,#37066,.F.);
#50202=ORIENTED_EDGE('',*,*,#37064,.F.);
#50203=ORIENTED_EDGE('',*,*,#37068,.F.);
#50204=ORIENTED_EDGE('',*,*,#37069,.F.);
#50205=ORIENTED_EDGE('',*,*,#36755,.T.);
#50206=ORIENTED_EDGE('',*,*,#37070,.F.);
#50207=ORIENTED_EDGE('',*,*,#37071,.T.);
#50208=ORIENTED_EDGE('',*,*,#37072,.F.);
#50209=ORIENTED_EDGE('',*,*,#36756,.T.);
#50210=ORIENTED_EDGE('',*,*,#37072,.T.);
#50211=ORIENTED_EDGE('',*,*,#37073,.T.);
#50212=ORIENTED_EDGE('',*,*,#37074,.F.);
#50213=ORIENTED_EDGE('',*,*,#37073,.F.);
#50214=ORIENTED_EDGE('',*,*,#37071,.F.);
#50215=ORIENTED_EDGE('',*,*,#37075,.F.);
#50216=ORIENTED_EDGE('',*,*,#37076,.F.);
#50217=ORIENTED_EDGE('',*,*,#36758,.T.);
#50218=ORIENTED_EDGE('',*,*,#37077,.F.);
#50219=ORIENTED_EDGE('',*,*,#37078,.T.);
#50220=ORIENTED_EDGE('',*,*,#37079,.F.);
#50221=ORIENTED_EDGE('',*,*,#36759,.T.);
#50222=ORIENTED_EDGE('',*,*,#37079,.T.);
#50223=ORIENTED_EDGE('',*,*,#37080,.T.);
#50224=ORIENTED_EDGE('',*,*,#37081,.F.);
#50225=ORIENTED_EDGE('',*,*,#37080,.F.);
#50226=ORIENTED_EDGE('',*,*,#37078,.F.);
#50227=ORIENTED_EDGE('',*,*,#37082,.F.);
#50228=ORIENTED_EDGE('',*,*,#37083,.F.);
#50229=ORIENTED_EDGE('',*,*,#36761,.T.);
#50230=ORIENTED_EDGE('',*,*,#37084,.F.);
#50231=ORIENTED_EDGE('',*,*,#37085,.T.);
#50232=ORIENTED_EDGE('',*,*,#37086,.F.);
#50233=ORIENTED_EDGE('',*,*,#36762,.T.);
#50234=ORIENTED_EDGE('',*,*,#37086,.T.);
#50235=ORIENTED_EDGE('',*,*,#37087,.T.);
#50236=ORIENTED_EDGE('',*,*,#37088,.F.);
#50237=ORIENTED_EDGE('',*,*,#37087,.F.);
#50238=ORIENTED_EDGE('',*,*,#37085,.F.);
#50239=ORIENTED_EDGE('',*,*,#37089,.F.);
#50240=ORIENTED_EDGE('',*,*,#37090,.F.);
#50241=ORIENTED_EDGE('',*,*,#36764,.T.);
#50242=ORIENTED_EDGE('',*,*,#37091,.F.);
#50243=ORIENTED_EDGE('',*,*,#37092,.T.);
#50244=ORIENTED_EDGE('',*,*,#37093,.F.);
#50245=ORIENTED_EDGE('',*,*,#36765,.T.);
#50246=ORIENTED_EDGE('',*,*,#37093,.T.);
#50247=ORIENTED_EDGE('',*,*,#37094,.T.);
#50248=ORIENTED_EDGE('',*,*,#37095,.F.);
#50249=ORIENTED_EDGE('',*,*,#37094,.F.);
#50250=ORIENTED_EDGE('',*,*,#37092,.F.);
#50251=ORIENTED_EDGE('',*,*,#37096,.F.);
#50252=ORIENTED_EDGE('',*,*,#37097,.F.);
#50253=ORIENTED_EDGE('',*,*,#36767,.T.);
#50254=ORIENTED_EDGE('',*,*,#37098,.F.);
#50255=ORIENTED_EDGE('',*,*,#37099,.T.);
#50256=ORIENTED_EDGE('',*,*,#37100,.F.);
#50257=ORIENTED_EDGE('',*,*,#36768,.T.);
#50258=ORIENTED_EDGE('',*,*,#37100,.T.);
#50259=ORIENTED_EDGE('',*,*,#37101,.T.);
#50260=ORIENTED_EDGE('',*,*,#37102,.F.);
#50261=ORIENTED_EDGE('',*,*,#37101,.F.);
#50262=ORIENTED_EDGE('',*,*,#37099,.F.);
#50263=ORIENTED_EDGE('',*,*,#37103,.F.);
#50264=ORIENTED_EDGE('',*,*,#37104,.F.);
#50265=ORIENTED_EDGE('',*,*,#36770,.T.);
#50266=ORIENTED_EDGE('',*,*,#37105,.F.);
#50267=ORIENTED_EDGE('',*,*,#37106,.T.);
#50268=ORIENTED_EDGE('',*,*,#37107,.F.);
#50269=ORIENTED_EDGE('',*,*,#36771,.T.);
#50270=ORIENTED_EDGE('',*,*,#37107,.T.);
#50271=ORIENTED_EDGE('',*,*,#37108,.T.);
#50272=ORIENTED_EDGE('',*,*,#37109,.F.);
#50273=ORIENTED_EDGE('',*,*,#37108,.F.);
#50274=ORIENTED_EDGE('',*,*,#37106,.F.);
#50275=ORIENTED_EDGE('',*,*,#37110,.F.);
#50276=ORIENTED_EDGE('',*,*,#37111,.F.);
#50277=ORIENTED_EDGE('',*,*,#36773,.T.);
#50278=ORIENTED_EDGE('',*,*,#37112,.F.);
#50279=ORIENTED_EDGE('',*,*,#34435,.T.);
#50280=ORIENTED_EDGE('',*,*,#37113,.F.);
#50281=ORIENTED_EDGE('',*,*,#36774,.T.);
#50282=ORIENTED_EDGE('',*,*,#37113,.T.);
#50283=ORIENTED_EDGE('',*,*,#34434,.T.);
#50284=ORIENTED_EDGE('',*,*,#37114,.F.);
#50285=ORIENTED_EDGE('',*,*,#36776,.T.);
#50286=ORIENTED_EDGE('',*,*,#37115,.F.);
#50287=ORIENTED_EDGE('',*,*,#37116,.T.);
#50288=ORIENTED_EDGE('',*,*,#37117,.F.);
#50289=ORIENTED_EDGE('',*,*,#36777,.T.);
#50290=ORIENTED_EDGE('',*,*,#37117,.T.);
#50291=ORIENTED_EDGE('',*,*,#37118,.T.);
#50292=ORIENTED_EDGE('',*,*,#37119,.F.);
#50293=ORIENTED_EDGE('',*,*,#37118,.F.);
#50294=ORIENTED_EDGE('',*,*,#37116,.F.);
#50295=ORIENTED_EDGE('',*,*,#37120,.F.);
#50296=ORIENTED_EDGE('',*,*,#37121,.F.);
#50297=ORIENTED_EDGE('',*,*,#36779,.T.);
#50298=ORIENTED_EDGE('',*,*,#37122,.F.);
#50299=ORIENTED_EDGE('',*,*,#37123,.T.);
#50300=ORIENTED_EDGE('',*,*,#37124,.F.);
#50301=ORIENTED_EDGE('',*,*,#36780,.T.);
#50302=ORIENTED_EDGE('',*,*,#37124,.T.);
#50303=ORIENTED_EDGE('',*,*,#37125,.T.);
#50304=ORIENTED_EDGE('',*,*,#37126,.F.);
#50305=ORIENTED_EDGE('',*,*,#37125,.F.);
#50306=ORIENTED_EDGE('',*,*,#37123,.F.);
#50307=ORIENTED_EDGE('',*,*,#37127,.F.);
#50308=ORIENTED_EDGE('',*,*,#37128,.F.);
#50309=ORIENTED_EDGE('',*,*,#36782,.T.);
#50310=ORIENTED_EDGE('',*,*,#37129,.F.);
#50311=ORIENTED_EDGE('',*,*,#37130,.T.);
#50312=ORIENTED_EDGE('',*,*,#37131,.F.);
#50313=ORIENTED_EDGE('',*,*,#36783,.T.);
#50314=ORIENTED_EDGE('',*,*,#37131,.T.);
#50315=ORIENTED_EDGE('',*,*,#37132,.T.);
#50316=ORIENTED_EDGE('',*,*,#37133,.F.);
#50317=ORIENTED_EDGE('',*,*,#37132,.F.);
#50318=ORIENTED_EDGE('',*,*,#37130,.F.);
#50319=ORIENTED_EDGE('',*,*,#37134,.F.);
#50320=ORIENTED_EDGE('',*,*,#37135,.F.);
#50321=ORIENTED_EDGE('',*,*,#36785,.T.);
#50322=ORIENTED_EDGE('',*,*,#37136,.F.);
#50323=ORIENTED_EDGE('',*,*,#37137,.T.);
#50324=ORIENTED_EDGE('',*,*,#37138,.F.);
#50325=ORIENTED_EDGE('',*,*,#36786,.T.);
#50326=ORIENTED_EDGE('',*,*,#37138,.T.);
#50327=ORIENTED_EDGE('',*,*,#37139,.T.);
#50328=ORIENTED_EDGE('',*,*,#37140,.F.);
#50329=ORIENTED_EDGE('',*,*,#37139,.F.);
#50330=ORIENTED_EDGE('',*,*,#37137,.F.);
#50331=ORIENTED_EDGE('',*,*,#37141,.F.);
#50332=ORIENTED_EDGE('',*,*,#37142,.F.);
#50333=ORIENTED_EDGE('',*,*,#36788,.T.);
#50334=ORIENTED_EDGE('',*,*,#37143,.F.);
#50335=ORIENTED_EDGE('',*,*,#37144,.T.);
#50336=ORIENTED_EDGE('',*,*,#37145,.F.);
#50337=ORIENTED_EDGE('',*,*,#36789,.T.);
#50338=ORIENTED_EDGE('',*,*,#37145,.T.);
#50339=ORIENTED_EDGE('',*,*,#37146,.T.);
#50340=ORIENTED_EDGE('',*,*,#37147,.F.);
#50341=ORIENTED_EDGE('',*,*,#37146,.F.);
#50342=ORIENTED_EDGE('',*,*,#37144,.F.);
#50343=ORIENTED_EDGE('',*,*,#37148,.F.);
#50344=ORIENTED_EDGE('',*,*,#37149,.F.);
#50345=ORIENTED_EDGE('',*,*,#36791,.T.);
#50346=ORIENTED_EDGE('',*,*,#37150,.F.);
#50347=ORIENTED_EDGE('',*,*,#37151,.T.);
#50348=ORIENTED_EDGE('',*,*,#37152,.F.);
#50349=ORIENTED_EDGE('',*,*,#36792,.T.);
#50350=ORIENTED_EDGE('',*,*,#37152,.T.);
#50351=ORIENTED_EDGE('',*,*,#37153,.T.);
#50352=ORIENTED_EDGE('',*,*,#37154,.F.);
#50353=ORIENTED_EDGE('',*,*,#37153,.F.);
#50354=ORIENTED_EDGE('',*,*,#37151,.F.);
#50355=ORIENTED_EDGE('',*,*,#37155,.F.);
#50356=ORIENTED_EDGE('',*,*,#37156,.F.);
#50357=ORIENTED_EDGE('',*,*,#36794,.T.);
#50358=ORIENTED_EDGE('',*,*,#37157,.F.);
#50359=ORIENTED_EDGE('',*,*,#37158,.T.);
#50360=ORIENTED_EDGE('',*,*,#37159,.F.);
#50361=ORIENTED_EDGE('',*,*,#36795,.T.);
#50362=ORIENTED_EDGE('',*,*,#37159,.T.);
#50363=ORIENTED_EDGE('',*,*,#37160,.T.);
#50364=ORIENTED_EDGE('',*,*,#37161,.F.);
#50365=ORIENTED_EDGE('',*,*,#37160,.F.);
#50366=ORIENTED_EDGE('',*,*,#37158,.F.);
#50367=ORIENTED_EDGE('',*,*,#37162,.F.);
#50368=ORIENTED_EDGE('',*,*,#37163,.F.);
#50369=ORIENTED_EDGE('',*,*,#36797,.T.);
#50370=ORIENTED_EDGE('',*,*,#37164,.F.);
#50371=ORIENTED_EDGE('',*,*,#37165,.T.);
#50372=ORIENTED_EDGE('',*,*,#37166,.F.);
#50373=ORIENTED_EDGE('',*,*,#36798,.T.);
#50374=ORIENTED_EDGE('',*,*,#37166,.T.);
#50375=ORIENTED_EDGE('',*,*,#37167,.T.);
#50376=ORIENTED_EDGE('',*,*,#37168,.F.);
#50377=ORIENTED_EDGE('',*,*,#37167,.F.);
#50378=ORIENTED_EDGE('',*,*,#37165,.F.);
#50379=ORIENTED_EDGE('',*,*,#37169,.F.);
#50380=ORIENTED_EDGE('',*,*,#37170,.F.);
#50381=ORIENTED_EDGE('',*,*,#36800,.T.);
#50382=ORIENTED_EDGE('',*,*,#37171,.F.);
#50383=ORIENTED_EDGE('',*,*,#37172,.T.);
#50384=ORIENTED_EDGE('',*,*,#37173,.F.);
#50385=ORIENTED_EDGE('',*,*,#36801,.T.);
#50386=ORIENTED_EDGE('',*,*,#37173,.T.);
#50387=ORIENTED_EDGE('',*,*,#37174,.T.);
#50388=ORIENTED_EDGE('',*,*,#37175,.F.);
#50389=ORIENTED_EDGE('',*,*,#37174,.F.);
#50390=ORIENTED_EDGE('',*,*,#37172,.F.);
#50391=ORIENTED_EDGE('',*,*,#37176,.F.);
#50392=ORIENTED_EDGE('',*,*,#37177,.F.);
#50393=ORIENTED_EDGE('',*,*,#36803,.T.);
#50394=ORIENTED_EDGE('',*,*,#37178,.F.);
#50395=ORIENTED_EDGE('',*,*,#37179,.T.);
#50396=ORIENTED_EDGE('',*,*,#37180,.F.);
#50397=ORIENTED_EDGE('',*,*,#36804,.T.);
#50398=ORIENTED_EDGE('',*,*,#37180,.T.);
#50399=ORIENTED_EDGE('',*,*,#37181,.T.);
#50400=ORIENTED_EDGE('',*,*,#37182,.F.);
#50401=ORIENTED_EDGE('',*,*,#37181,.F.);
#50402=ORIENTED_EDGE('',*,*,#37179,.F.);
#50403=ORIENTED_EDGE('',*,*,#37183,.F.);
#50404=ORIENTED_EDGE('',*,*,#37184,.F.);
#50405=ORIENTED_EDGE('',*,*,#36806,.T.);
#50406=ORIENTED_EDGE('',*,*,#37185,.F.);
#50407=ORIENTED_EDGE('',*,*,#37186,.T.);
#50408=ORIENTED_EDGE('',*,*,#37187,.F.);
#50409=ORIENTED_EDGE('',*,*,#36807,.T.);
#50410=ORIENTED_EDGE('',*,*,#37187,.T.);
#50411=ORIENTED_EDGE('',*,*,#37188,.T.);
#50412=ORIENTED_EDGE('',*,*,#37189,.F.);
#50413=ORIENTED_EDGE('',*,*,#37188,.F.);
#50414=ORIENTED_EDGE('',*,*,#37186,.F.);
#50415=ORIENTED_EDGE('',*,*,#37190,.F.);
#50416=ORIENTED_EDGE('',*,*,#37191,.F.);
#50417=ORIENTED_EDGE('',*,*,#36809,.T.);
#50418=ORIENTED_EDGE('',*,*,#37192,.F.);
#50419=ORIENTED_EDGE('',*,*,#37193,.T.);
#50420=ORIENTED_EDGE('',*,*,#37194,.F.);
#50421=ORIENTED_EDGE('',*,*,#36810,.T.);
#50422=ORIENTED_EDGE('',*,*,#37194,.T.);
#50423=ORIENTED_EDGE('',*,*,#37195,.T.);
#50424=ORIENTED_EDGE('',*,*,#37196,.F.);
#50425=ORIENTED_EDGE('',*,*,#37195,.F.);
#50426=ORIENTED_EDGE('',*,*,#37193,.F.);
#50427=ORIENTED_EDGE('',*,*,#37197,.F.);
#50428=ORIENTED_EDGE('',*,*,#37198,.F.);
#50429=ORIENTED_EDGE('',*,*,#36812,.T.);
#50430=ORIENTED_EDGE('',*,*,#37199,.F.);
#50431=ORIENTED_EDGE('',*,*,#37200,.T.);
#50432=ORIENTED_EDGE('',*,*,#37201,.F.);
#50433=ORIENTED_EDGE('',*,*,#36813,.T.);
#50434=ORIENTED_EDGE('',*,*,#37201,.T.);
#50435=ORIENTED_EDGE('',*,*,#37202,.T.);
#50436=ORIENTED_EDGE('',*,*,#37203,.F.);
#50437=ORIENTED_EDGE('',*,*,#37202,.F.);
#50438=ORIENTED_EDGE('',*,*,#37200,.F.);
#50439=ORIENTED_EDGE('',*,*,#37204,.F.);
#50440=ORIENTED_EDGE('',*,*,#37205,.F.);
#50441=ORIENTED_EDGE('',*,*,#36815,.T.);
#50442=ORIENTED_EDGE('',*,*,#37206,.F.);
#50443=ORIENTED_EDGE('',*,*,#37207,.T.);
#50444=ORIENTED_EDGE('',*,*,#37208,.F.);
#50445=ORIENTED_EDGE('',*,*,#36816,.T.);
#50446=ORIENTED_EDGE('',*,*,#37208,.T.);
#50447=ORIENTED_EDGE('',*,*,#37209,.T.);
#50448=ORIENTED_EDGE('',*,*,#37210,.F.);
#50449=ORIENTED_EDGE('',*,*,#37209,.F.);
#50450=ORIENTED_EDGE('',*,*,#37207,.F.);
#50451=ORIENTED_EDGE('',*,*,#37211,.F.);
#50452=ORIENTED_EDGE('',*,*,#37212,.F.);
#50453=ORIENTED_EDGE('',*,*,#37213,.F.);
#50454=ORIENTED_EDGE('',*,*,#37214,.F.);
#50455=ORIENTED_EDGE('',*,*,#37018,.F.);
#50456=ORIENTED_EDGE('',*,*,#37215,.F.);
#50457=ORIENTED_EDGE('',*,*,#36818,.T.);
#50458=ORIENTED_EDGE('',*,*,#37216,.F.);
#50459=ORIENTED_EDGE('',*,*,#37215,.T.);
#50460=ORIENTED_EDGE('',*,*,#37020,.T.);
#50461=ORIENTED_EDGE('',*,*,#37217,.F.);
#50462=ORIENTED_EDGE('',*,*,#36820,.T.);
#50463=ORIENTED_EDGE('',*,*,#37015,.T.);
#50464=ORIENTED_EDGE('',*,*,#37218,.F.);
#50465=ORIENTED_EDGE('',*,*,#37219,.F.);
#50466=ORIENTED_EDGE('',*,*,#37220,.F.);
#50467=ORIENTED_EDGE('',*,*,#36825,.T.);
#50468=ORIENTED_EDGE('',*,*,#36824,.T.);
#50469=ORIENTED_EDGE('',*,*,#37221,.F.);
#50470=ORIENTED_EDGE('',*,*,#36828,.T.);
#50471=ORIENTED_EDGE('',*,*,#36826,.T.);
#50472=ORIENTED_EDGE('',*,*,#37220,.T.);
#50473=ORIENTED_EDGE('',*,*,#37222,.F.);
#50474=ORIENTED_EDGE('',*,*,#37223,.F.);
#50475=ORIENTED_EDGE('',*,*,#36832,.T.);
#50476=ORIENTED_EDGE('',*,*,#36831,.T.);
#50477=ORIENTED_EDGE('',*,*,#37224,.F.);
#50478=ORIENTED_EDGE('',*,*,#36835,.T.);
#50479=ORIENTED_EDGE('',*,*,#36833,.T.);
#50480=ORIENTED_EDGE('',*,*,#37223,.T.);
#50481=ORIENTED_EDGE('',*,*,#37225,.F.);
#50482=ORIENTED_EDGE('',*,*,#37226,.F.);
#50483=ORIENTED_EDGE('',*,*,#36839,.T.);
#50484=ORIENTED_EDGE('',*,*,#36838,.T.);
#50485=ORIENTED_EDGE('',*,*,#37227,.F.);
#50486=ORIENTED_EDGE('',*,*,#36842,.T.);
#50487=ORIENTED_EDGE('',*,*,#36840,.T.);
#50488=ORIENTED_EDGE('',*,*,#37226,.T.);
#50489=ORIENTED_EDGE('',*,*,#37228,.F.);
#50490=ORIENTED_EDGE('',*,*,#37229,.F.);
#50491=ORIENTED_EDGE('',*,*,#36846,.T.);
#50492=ORIENTED_EDGE('',*,*,#36845,.T.);
#50493=ORIENTED_EDGE('',*,*,#37230,.F.);
#50494=ORIENTED_EDGE('',*,*,#36849,.T.);
#50495=ORIENTED_EDGE('',*,*,#36847,.T.);
#50496=ORIENTED_EDGE('',*,*,#37229,.T.);
#50497=ORIENTED_EDGE('',*,*,#37231,.F.);
#50498=ORIENTED_EDGE('',*,*,#37232,.F.);
#50499=ORIENTED_EDGE('',*,*,#36853,.T.);
#50500=ORIENTED_EDGE('',*,*,#36852,.T.);
#50501=ORIENTED_EDGE('',*,*,#37233,.F.);
#50502=ORIENTED_EDGE('',*,*,#36856,.T.);
#50503=ORIENTED_EDGE('',*,*,#36854,.T.);
#50504=ORIENTED_EDGE('',*,*,#37232,.T.);
#50505=ORIENTED_EDGE('',*,*,#37234,.F.);
#50506=ORIENTED_EDGE('',*,*,#37235,.F.);
#50507=ORIENTED_EDGE('',*,*,#36860,.T.);
#50508=ORIENTED_EDGE('',*,*,#36859,.T.);
#50509=ORIENTED_EDGE('',*,*,#37236,.F.);
#50510=ORIENTED_EDGE('',*,*,#36863,.T.);
#50511=ORIENTED_EDGE('',*,*,#36861,.T.);
#50512=ORIENTED_EDGE('',*,*,#37235,.T.);
#50513=ORIENTED_EDGE('',*,*,#37237,.F.);
#50514=ORIENTED_EDGE('',*,*,#37238,.F.);
#50515=ORIENTED_EDGE('',*,*,#34439,.T.);
#50516=ORIENTED_EDGE('',*,*,#36865,.T.);
#50517=ORIENTED_EDGE('',*,*,#37239,.F.);
#50518=ORIENTED_EDGE('',*,*,#36866,.T.);
#50519=ORIENTED_EDGE('',*,*,#34440,.T.);
#50520=ORIENTED_EDGE('',*,*,#37238,.T.);
#50521=ORIENTED_EDGE('',*,*,#37240,.F.);
#50522=ORIENTED_EDGE('',*,*,#37241,.F.);
#50523=ORIENTED_EDGE('',*,*,#36870,.T.);
#50524=ORIENTED_EDGE('',*,*,#36869,.T.);
#50525=ORIENTED_EDGE('',*,*,#37242,.F.);
#50526=ORIENTED_EDGE('',*,*,#36873,.T.);
#50527=ORIENTED_EDGE('',*,*,#36871,.T.);
#50528=ORIENTED_EDGE('',*,*,#37241,.T.);
#50529=ORIENTED_EDGE('',*,*,#37243,.F.);
#50530=ORIENTED_EDGE('',*,*,#37244,.F.);
#50531=ORIENTED_EDGE('',*,*,#36877,.T.);
#50532=ORIENTED_EDGE('',*,*,#36876,.T.);
#50533=ORIENTED_EDGE('',*,*,#37245,.F.);
#50534=ORIENTED_EDGE('',*,*,#36880,.T.);
#50535=ORIENTED_EDGE('',*,*,#36878,.T.);
#50536=ORIENTED_EDGE('',*,*,#37244,.T.);
#50537=ORIENTED_EDGE('',*,*,#37246,.F.);
#50538=ORIENTED_EDGE('',*,*,#37247,.F.);
#50539=ORIENTED_EDGE('',*,*,#36884,.T.);
#50540=ORIENTED_EDGE('',*,*,#36883,.T.);
#50541=ORIENTED_EDGE('',*,*,#37248,.F.);
#50542=ORIENTED_EDGE('',*,*,#36887,.T.);
#50543=ORIENTED_EDGE('',*,*,#36885,.T.);
#50544=ORIENTED_EDGE('',*,*,#37247,.T.);
#50545=ORIENTED_EDGE('',*,*,#37249,.F.);
#50546=ORIENTED_EDGE('',*,*,#37250,.F.);
#50547=ORIENTED_EDGE('',*,*,#36891,.T.);
#50548=ORIENTED_EDGE('',*,*,#36890,.T.);
#50549=ORIENTED_EDGE('',*,*,#37251,.F.);
#50550=ORIENTED_EDGE('',*,*,#36894,.T.);
#50551=ORIENTED_EDGE('',*,*,#36892,.T.);
#50552=ORIENTED_EDGE('',*,*,#37250,.T.);
#50553=ORIENTED_EDGE('',*,*,#37252,.F.);
#50554=ORIENTED_EDGE('',*,*,#37253,.F.);
#50555=ORIENTED_EDGE('',*,*,#36898,.T.);
#50556=ORIENTED_EDGE('',*,*,#36897,.T.);
#50557=ORIENTED_EDGE('',*,*,#37254,.F.);
#50558=ORIENTED_EDGE('',*,*,#36901,.T.);
#50559=ORIENTED_EDGE('',*,*,#36899,.T.);
#50560=ORIENTED_EDGE('',*,*,#37253,.T.);
#50561=ORIENTED_EDGE('',*,*,#37255,.F.);
#50562=ORIENTED_EDGE('',*,*,#37256,.F.);
#50563=ORIENTED_EDGE('',*,*,#36905,.T.);
#50564=ORIENTED_EDGE('',*,*,#36904,.T.);
#50565=ORIENTED_EDGE('',*,*,#37257,.F.);
#50566=ORIENTED_EDGE('',*,*,#36908,.T.);
#50567=ORIENTED_EDGE('',*,*,#36906,.T.);
#50568=ORIENTED_EDGE('',*,*,#37256,.T.);
#50569=ORIENTED_EDGE('',*,*,#37258,.F.);
#50570=ORIENTED_EDGE('',*,*,#37259,.F.);
#50571=ORIENTED_EDGE('',*,*,#36912,.T.);
#50572=ORIENTED_EDGE('',*,*,#36911,.T.);
#50573=ORIENTED_EDGE('',*,*,#37260,.F.);
#50574=ORIENTED_EDGE('',*,*,#36915,.T.);
#50575=ORIENTED_EDGE('',*,*,#36913,.T.);
#50576=ORIENTED_EDGE('',*,*,#37259,.T.);
#50577=ORIENTED_EDGE('',*,*,#37261,.F.);
#50578=ORIENTED_EDGE('',*,*,#37262,.F.);
#50579=ORIENTED_EDGE('',*,*,#36919,.T.);
#50580=ORIENTED_EDGE('',*,*,#36918,.T.);
#50581=ORIENTED_EDGE('',*,*,#37263,.F.);
#50582=ORIENTED_EDGE('',*,*,#36922,.T.);
#50583=ORIENTED_EDGE('',*,*,#36920,.T.);
#50584=ORIENTED_EDGE('',*,*,#37262,.T.);
#50585=ORIENTED_EDGE('',*,*,#37264,.F.);
#50586=ORIENTED_EDGE('',*,*,#37265,.F.);
#50587=ORIENTED_EDGE('',*,*,#36926,.T.);
#50588=ORIENTED_EDGE('',*,*,#36925,.T.);
#50589=ORIENTED_EDGE('',*,*,#37266,.F.);
#50590=ORIENTED_EDGE('',*,*,#36929,.T.);
#50591=ORIENTED_EDGE('',*,*,#36927,.T.);
#50592=ORIENTED_EDGE('',*,*,#37265,.T.);
#50593=ORIENTED_EDGE('',*,*,#37267,.F.);
#50594=ORIENTED_EDGE('',*,*,#37268,.F.);
#50595=ORIENTED_EDGE('',*,*,#36933,.T.);
#50596=ORIENTED_EDGE('',*,*,#36932,.T.);
#50597=ORIENTED_EDGE('',*,*,#37269,.F.);
#50598=ORIENTED_EDGE('',*,*,#36936,.T.);
#50599=ORIENTED_EDGE('',*,*,#36934,.T.);
#50600=ORIENTED_EDGE('',*,*,#37268,.T.);
#50601=ORIENTED_EDGE('',*,*,#37270,.F.);
#50602=ORIENTED_EDGE('',*,*,#37271,.F.);
#50603=ORIENTED_EDGE('',*,*,#36940,.T.);
#50604=ORIENTED_EDGE('',*,*,#36939,.T.);
#50605=ORIENTED_EDGE('',*,*,#37272,.F.);
#50606=ORIENTED_EDGE('',*,*,#36943,.T.);
#50607=ORIENTED_EDGE('',*,*,#36941,.T.);
#50608=ORIENTED_EDGE('',*,*,#37271,.T.);
#50609=ORIENTED_EDGE('',*,*,#37273,.F.);
#50610=ORIENTED_EDGE('',*,*,#37274,.F.);
#50611=ORIENTED_EDGE('',*,*,#36947,.T.);
#50612=ORIENTED_EDGE('',*,*,#36946,.T.);
#50613=ORIENTED_EDGE('',*,*,#37275,.F.);
#50614=ORIENTED_EDGE('',*,*,#36950,.T.);
#50615=ORIENTED_EDGE('',*,*,#36948,.T.);
#50616=ORIENTED_EDGE('',*,*,#37274,.T.);
#50617=ORIENTED_EDGE('',*,*,#37276,.F.);
#50618=ORIENTED_EDGE('',*,*,#37277,.F.);
#50619=ORIENTED_EDGE('',*,*,#36954,.T.);
#50620=ORIENTED_EDGE('',*,*,#36953,.T.);
#50621=ORIENTED_EDGE('',*,*,#37278,.F.);
#50622=ORIENTED_EDGE('',*,*,#36957,.T.);
#50623=ORIENTED_EDGE('',*,*,#36955,.T.);
#50624=ORIENTED_EDGE('',*,*,#37277,.T.);
#50625=ORIENTED_EDGE('',*,*,#37279,.F.);
#50626=ORIENTED_EDGE('',*,*,#37280,.F.);
#50627=ORIENTED_EDGE('',*,*,#36961,.T.);
#50628=ORIENTED_EDGE('',*,*,#36960,.T.);
#50629=ORIENTED_EDGE('',*,*,#37281,.F.);
#50630=ORIENTED_EDGE('',*,*,#36964,.T.);
#50631=ORIENTED_EDGE('',*,*,#36962,.T.);
#50632=ORIENTED_EDGE('',*,*,#37280,.T.);
#50633=ORIENTED_EDGE('',*,*,#37282,.F.);
#50634=ORIENTED_EDGE('',*,*,#37283,.F.);
#50635=ORIENTED_EDGE('',*,*,#36968,.T.);
#50636=ORIENTED_EDGE('',*,*,#36967,.T.);
#50637=ORIENTED_EDGE('',*,*,#37284,.F.);
#50638=ORIENTED_EDGE('',*,*,#36971,.T.);
#50639=ORIENTED_EDGE('',*,*,#36969,.T.);
#50640=ORIENTED_EDGE('',*,*,#37283,.T.);
#50641=ORIENTED_EDGE('',*,*,#37285,.F.);
#50642=ORIENTED_EDGE('',*,*,#37286,.F.);
#50643=ORIENTED_EDGE('',*,*,#36977,.T.);
#50644=ORIENTED_EDGE('',*,*,#36974,.T.);
#50645=ORIENTED_EDGE('',*,*,#36978,.T.);
#50646=ORIENTED_EDGE('',*,*,#37286,.T.);
#50647=ORIENTED_EDGE('',*,*,#37287,.F.);
#50648=ORIENTED_EDGE('',*,*,#36976,.T.);
#50649=ORIENTED_EDGE('',*,*,#36983,.T.);
#50650=ORIENTED_EDGE('',*,*,#36979,.T.);
#50651=ORIENTED_EDGE('',*,*,#37288,.F.);
#50652=ORIENTED_EDGE('',*,*,#37289,.F.);
#50653=ORIENTED_EDGE('',*,*,#37290,.F.);
#50654=ORIENTED_EDGE('',*,*,#36985,.T.);
#50655=ORIENTED_EDGE('',*,*,#36984,.T.);
#50656=ORIENTED_EDGE('',*,*,#37289,.T.);
#50657=ORIENTED_EDGE('',*,*,#37291,.F.);
#50658=ORIENTED_EDGE('',*,*,#37292,.F.);
#50659=ORIENTED_EDGE('',*,*,#36989,.T.);
#50660=ORIENTED_EDGE('',*,*,#36988,.T.);
#50661=ORIENTED_EDGE('',*,*,#37293,.F.);
#50662=ORIENTED_EDGE('',*,*,#36992,.T.);
#50663=ORIENTED_EDGE('',*,*,#36990,.T.);
#50664=ORIENTED_EDGE('',*,*,#37292,.T.);
#50665=ORIENTED_EDGE('',*,*,#37294,.F.);
#50666=ORIENTED_EDGE('',*,*,#37295,.F.);
#50667=ORIENTED_EDGE('',*,*,#36996,.T.);
#50668=ORIENTED_EDGE('',*,*,#36995,.T.);
#50669=ORIENTED_EDGE('',*,*,#37296,.F.);
#50670=ORIENTED_EDGE('',*,*,#36999,.T.);
#50671=ORIENTED_EDGE('',*,*,#36997,.T.);
#50672=ORIENTED_EDGE('',*,*,#37295,.T.);
#50673=ORIENTED_EDGE('',*,*,#37297,.F.);
#50674=ORIENTED_EDGE('',*,*,#37298,.F.);
#50675=ORIENTED_EDGE('',*,*,#37003,.T.);
#50676=ORIENTED_EDGE('',*,*,#37002,.T.);
#50677=ORIENTED_EDGE('',*,*,#37299,.F.);
#50678=ORIENTED_EDGE('',*,*,#37006,.T.);
#50679=ORIENTED_EDGE('',*,*,#37004,.T.);
#50680=ORIENTED_EDGE('',*,*,#37298,.T.);
#50681=ORIENTED_EDGE('',*,*,#37300,.F.);
#50682=ORIENTED_EDGE('',*,*,#37301,.F.);
#50683=ORIENTED_EDGE('',*,*,#37010,.T.);
#50684=ORIENTED_EDGE('',*,*,#37009,.T.);
#50685=ORIENTED_EDGE('',*,*,#37302,.F.);
#50686=ORIENTED_EDGE('',*,*,#37013,.T.);
#50687=ORIENTED_EDGE('',*,*,#37011,.T.);
#50688=ORIENTED_EDGE('',*,*,#37301,.T.);
#50689=ORIENTED_EDGE('',*,*,#37303,.F.);
#50690=ORIENTED_EDGE('',*,*,#37218,.T.);
#50691=ORIENTED_EDGE('',*,*,#37014,.T.);
#50692=ORIENTED_EDGE('',*,*,#37017,.T.);
#50693=ORIENTED_EDGE('',*,*,#37214,.T.);
#50694=ORIENTED_EDGE('',*,*,#37304,.F.);
#50695=ORIENTED_EDGE('',*,*,#37305,.F.);
#50696=ORIENTED_EDGE('',*,*,#37019,.T.);
#50697=ORIENTED_EDGE('',*,*,#37026,.T.);
#50698=ORIENTED_EDGE('',*,*,#37021,.T.);
#50699=ORIENTED_EDGE('',*,*,#37306,.F.);
#50700=ORIENTED_EDGE('',*,*,#37307,.F.);
#50701=ORIENTED_EDGE('',*,*,#37027,.T.);
#50702=ORIENTED_EDGE('',*,*,#37307,.T.);
#50703=ORIENTED_EDGE('',*,*,#37308,.F.);
#50704=ORIENTED_EDGE('',*,*,#37025,.T.);
#50705=ORIENTED_EDGE('',*,*,#37033,.T.);
#50706=ORIENTED_EDGE('',*,*,#37028,.T.);
#50707=ORIENTED_EDGE('',*,*,#37309,.F.);
#50708=ORIENTED_EDGE('',*,*,#37310,.F.);
#50709=ORIENTED_EDGE('',*,*,#37034,.T.);
#50710=ORIENTED_EDGE('',*,*,#37310,.T.);
#50711=ORIENTED_EDGE('',*,*,#37311,.F.);
#50712=ORIENTED_EDGE('',*,*,#37032,.T.);
#50713=ORIENTED_EDGE('',*,*,#37040,.T.);
#50714=ORIENTED_EDGE('',*,*,#37035,.T.);
#50715=ORIENTED_EDGE('',*,*,#37312,.F.);
#50716=ORIENTED_EDGE('',*,*,#37313,.F.);
#50717=ORIENTED_EDGE('',*,*,#37041,.T.);
#50718=ORIENTED_EDGE('',*,*,#37313,.T.);
#50719=ORIENTED_EDGE('',*,*,#37314,.F.);
#50720=ORIENTED_EDGE('',*,*,#37039,.T.);
#50721=ORIENTED_EDGE('',*,*,#37047,.T.);
#50722=ORIENTED_EDGE('',*,*,#37042,.T.);
#50723=ORIENTED_EDGE('',*,*,#37315,.F.);
#50724=ORIENTED_EDGE('',*,*,#37316,.F.);
#50725=ORIENTED_EDGE('',*,*,#37048,.T.);
#50726=ORIENTED_EDGE('',*,*,#37316,.T.);
#50727=ORIENTED_EDGE('',*,*,#37317,.F.);
#50728=ORIENTED_EDGE('',*,*,#37046,.T.);
#50729=ORIENTED_EDGE('',*,*,#37054,.T.);
#50730=ORIENTED_EDGE('',*,*,#37049,.T.);
#50731=ORIENTED_EDGE('',*,*,#37318,.F.);
#50732=ORIENTED_EDGE('',*,*,#37319,.F.);
#50733=ORIENTED_EDGE('',*,*,#37055,.T.);
#50734=ORIENTED_EDGE('',*,*,#37319,.T.);
#50735=ORIENTED_EDGE('',*,*,#37320,.F.);
#50736=ORIENTED_EDGE('',*,*,#37053,.T.);
#50737=ORIENTED_EDGE('',*,*,#37061,.T.);
#50738=ORIENTED_EDGE('',*,*,#37056,.T.);
#50739=ORIENTED_EDGE('',*,*,#37321,.F.);
#50740=ORIENTED_EDGE('',*,*,#37322,.F.);
#50741=ORIENTED_EDGE('',*,*,#37062,.T.);
#50742=ORIENTED_EDGE('',*,*,#37322,.T.);
#50743=ORIENTED_EDGE('',*,*,#37323,.F.);
#50744=ORIENTED_EDGE('',*,*,#37060,.T.);
#50745=ORIENTED_EDGE('',*,*,#37068,.T.);
#50746=ORIENTED_EDGE('',*,*,#37063,.T.);
#50747=ORIENTED_EDGE('',*,*,#37324,.F.);
#50748=ORIENTED_EDGE('',*,*,#37325,.F.);
#50749=ORIENTED_EDGE('',*,*,#37069,.T.);
#50750=ORIENTED_EDGE('',*,*,#37325,.T.);
#50751=ORIENTED_EDGE('',*,*,#37326,.F.);
#50752=ORIENTED_EDGE('',*,*,#37067,.T.);
#50753=ORIENTED_EDGE('',*,*,#37075,.T.);
#50754=ORIENTED_EDGE('',*,*,#37070,.T.);
#50755=ORIENTED_EDGE('',*,*,#37327,.F.);
#50756=ORIENTED_EDGE('',*,*,#37328,.F.);
#50757=ORIENTED_EDGE('',*,*,#37076,.T.);
#50758=ORIENTED_EDGE('',*,*,#37328,.T.);
#50759=ORIENTED_EDGE('',*,*,#37329,.F.);
#50760=ORIENTED_EDGE('',*,*,#37074,.T.);
#50761=ORIENTED_EDGE('',*,*,#37082,.T.);
#50762=ORIENTED_EDGE('',*,*,#37077,.T.);
#50763=ORIENTED_EDGE('',*,*,#37330,.F.);
#50764=ORIENTED_EDGE('',*,*,#37331,.F.);
#50765=ORIENTED_EDGE('',*,*,#37083,.T.);
#50766=ORIENTED_EDGE('',*,*,#37331,.T.);
#50767=ORIENTED_EDGE('',*,*,#37332,.F.);
#50768=ORIENTED_EDGE('',*,*,#37081,.T.);
#50769=ORIENTED_EDGE('',*,*,#37089,.T.);
#50770=ORIENTED_EDGE('',*,*,#37084,.T.);
#50771=ORIENTED_EDGE('',*,*,#37333,.F.);
#50772=ORIENTED_EDGE('',*,*,#37334,.F.);
#50773=ORIENTED_EDGE('',*,*,#37090,.T.);
#50774=ORIENTED_EDGE('',*,*,#37334,.T.);
#50775=ORIENTED_EDGE('',*,*,#37335,.F.);
#50776=ORIENTED_EDGE('',*,*,#37088,.T.);
#50777=ORIENTED_EDGE('',*,*,#37096,.T.);
#50778=ORIENTED_EDGE('',*,*,#37091,.T.);
#50779=ORIENTED_EDGE('',*,*,#37336,.F.);
#50780=ORIENTED_EDGE('',*,*,#37337,.F.);
#50781=ORIENTED_EDGE('',*,*,#37097,.T.);
#50782=ORIENTED_EDGE('',*,*,#37337,.T.);
#50783=ORIENTED_EDGE('',*,*,#37338,.F.);
#50784=ORIENTED_EDGE('',*,*,#37095,.T.);
#50785=ORIENTED_EDGE('',*,*,#37103,.T.);
#50786=ORIENTED_EDGE('',*,*,#37098,.T.);
#50787=ORIENTED_EDGE('',*,*,#37339,.F.);
#50788=ORIENTED_EDGE('',*,*,#37340,.F.);
#50789=ORIENTED_EDGE('',*,*,#37104,.T.);
#50790=ORIENTED_EDGE('',*,*,#37340,.T.);
#50791=ORIENTED_EDGE('',*,*,#37341,.F.);
#50792=ORIENTED_EDGE('',*,*,#37102,.T.);
#50793=ORIENTED_EDGE('',*,*,#37110,.T.);
#50794=ORIENTED_EDGE('',*,*,#37105,.T.);
#50795=ORIENTED_EDGE('',*,*,#37342,.F.);
#50796=ORIENTED_EDGE('',*,*,#37343,.F.);
#50797=ORIENTED_EDGE('',*,*,#37111,.T.);
#50798=ORIENTED_EDGE('',*,*,#37343,.T.);
#50799=ORIENTED_EDGE('',*,*,#37344,.F.);
#50800=ORIENTED_EDGE('',*,*,#37109,.T.);
#50801=ORIENTED_EDGE('',*,*,#34436,.T.);
#50802=ORIENTED_EDGE('',*,*,#37112,.T.);
#50803=ORIENTED_EDGE('',*,*,#37345,.F.);
#50804=ORIENTED_EDGE('',*,*,#37346,.F.);
#50805=ORIENTED_EDGE('',*,*,#34433,.T.);
#50806=ORIENTED_EDGE('',*,*,#37346,.T.);
#50807=ORIENTED_EDGE('',*,*,#37347,.F.);
#50808=ORIENTED_EDGE('',*,*,#37114,.T.);
#50809=ORIENTED_EDGE('',*,*,#37120,.T.);
#50810=ORIENTED_EDGE('',*,*,#37115,.T.);
#50811=ORIENTED_EDGE('',*,*,#37348,.F.);
#50812=ORIENTED_EDGE('',*,*,#37349,.F.);
#50813=ORIENTED_EDGE('',*,*,#37121,.T.);
#50814=ORIENTED_EDGE('',*,*,#37349,.T.);
#50815=ORIENTED_EDGE('',*,*,#37350,.F.);
#50816=ORIENTED_EDGE('',*,*,#37119,.T.);
#50817=ORIENTED_EDGE('',*,*,#37127,.T.);
#50818=ORIENTED_EDGE('',*,*,#37122,.T.);
#50819=ORIENTED_EDGE('',*,*,#37351,.F.);
#50820=ORIENTED_EDGE('',*,*,#37352,.F.);
#50821=ORIENTED_EDGE('',*,*,#37128,.T.);
#50822=ORIENTED_EDGE('',*,*,#37352,.T.);
#50823=ORIENTED_EDGE('',*,*,#37353,.F.);
#50824=ORIENTED_EDGE('',*,*,#37126,.T.);
#50825=ORIENTED_EDGE('',*,*,#37134,.T.);
#50826=ORIENTED_EDGE('',*,*,#37129,.T.);
#50827=ORIENTED_EDGE('',*,*,#37354,.F.);
#50828=ORIENTED_EDGE('',*,*,#37355,.F.);
#50829=ORIENTED_EDGE('',*,*,#37135,.T.);
#50830=ORIENTED_EDGE('',*,*,#37355,.T.);
#50831=ORIENTED_EDGE('',*,*,#37356,.F.);
#50832=ORIENTED_EDGE('',*,*,#37133,.T.);
#50833=ORIENTED_EDGE('',*,*,#37141,.T.);
#50834=ORIENTED_EDGE('',*,*,#37136,.T.);
#50835=ORIENTED_EDGE('',*,*,#37357,.F.);
#50836=ORIENTED_EDGE('',*,*,#37358,.F.);
#50837=ORIENTED_EDGE('',*,*,#37142,.T.);
#50838=ORIENTED_EDGE('',*,*,#37358,.T.);
#50839=ORIENTED_EDGE('',*,*,#37359,.F.);
#50840=ORIENTED_EDGE('',*,*,#37140,.T.);
#50841=ORIENTED_EDGE('',*,*,#37148,.T.);
#50842=ORIENTED_EDGE('',*,*,#37143,.T.);
#50843=ORIENTED_EDGE('',*,*,#37360,.F.);
#50844=ORIENTED_EDGE('',*,*,#37361,.F.);
#50845=ORIENTED_EDGE('',*,*,#37149,.T.);
#50846=ORIENTED_EDGE('',*,*,#37361,.T.);
#50847=ORIENTED_EDGE('',*,*,#37362,.F.);
#50848=ORIENTED_EDGE('',*,*,#37147,.T.);
#50849=ORIENTED_EDGE('',*,*,#37155,.T.);
#50850=ORIENTED_EDGE('',*,*,#37150,.T.);
#50851=ORIENTED_EDGE('',*,*,#37363,.F.);
#50852=ORIENTED_EDGE('',*,*,#37364,.F.);
#50853=ORIENTED_EDGE('',*,*,#37156,.T.);
#50854=ORIENTED_EDGE('',*,*,#37364,.T.);
#50855=ORIENTED_EDGE('',*,*,#37365,.F.);
#50856=ORIENTED_EDGE('',*,*,#37154,.T.);
#50857=ORIENTED_EDGE('',*,*,#37162,.T.);
#50858=ORIENTED_EDGE('',*,*,#37157,.T.);
#50859=ORIENTED_EDGE('',*,*,#37366,.F.);
#50860=ORIENTED_EDGE('',*,*,#37367,.F.);
#50861=ORIENTED_EDGE('',*,*,#37163,.T.);
#50862=ORIENTED_EDGE('',*,*,#37367,.T.);
#50863=ORIENTED_EDGE('',*,*,#37368,.F.);
#50864=ORIENTED_EDGE('',*,*,#37161,.T.);
#50865=ORIENTED_EDGE('',*,*,#37169,.T.);
#50866=ORIENTED_EDGE('',*,*,#37164,.T.);
#50867=ORIENTED_EDGE('',*,*,#37369,.F.);
#50868=ORIENTED_EDGE('',*,*,#37370,.F.);
#50869=ORIENTED_EDGE('',*,*,#37170,.T.);
#50870=ORIENTED_EDGE('',*,*,#37370,.T.);
#50871=ORIENTED_EDGE('',*,*,#37371,.F.);
#50872=ORIENTED_EDGE('',*,*,#37168,.T.);
#50873=ORIENTED_EDGE('',*,*,#37176,.T.);
#50874=ORIENTED_EDGE('',*,*,#37171,.T.);
#50875=ORIENTED_EDGE('',*,*,#37372,.F.);
#50876=ORIENTED_EDGE('',*,*,#37373,.F.);
#50877=ORIENTED_EDGE('',*,*,#37177,.T.);
#50878=ORIENTED_EDGE('',*,*,#37373,.T.);
#50879=ORIENTED_EDGE('',*,*,#37374,.F.);
#50880=ORIENTED_EDGE('',*,*,#37175,.T.);
#50881=ORIENTED_EDGE('',*,*,#37183,.T.);
#50882=ORIENTED_EDGE('',*,*,#37178,.T.);
#50883=ORIENTED_EDGE('',*,*,#37375,.F.);
#50884=ORIENTED_EDGE('',*,*,#37376,.F.);
#50885=ORIENTED_EDGE('',*,*,#37184,.T.);
#50886=ORIENTED_EDGE('',*,*,#37376,.T.);
#50887=ORIENTED_EDGE('',*,*,#37377,.F.);
#50888=ORIENTED_EDGE('',*,*,#37182,.T.);
#50889=ORIENTED_EDGE('',*,*,#37190,.T.);
#50890=ORIENTED_EDGE('',*,*,#37185,.T.);
#50891=ORIENTED_EDGE('',*,*,#37378,.F.);
#50892=ORIENTED_EDGE('',*,*,#37379,.F.);
#50893=ORIENTED_EDGE('',*,*,#37191,.T.);
#50894=ORIENTED_EDGE('',*,*,#37379,.T.);
#50895=ORIENTED_EDGE('',*,*,#37380,.F.);
#50896=ORIENTED_EDGE('',*,*,#37189,.T.);
#50897=ORIENTED_EDGE('',*,*,#37197,.T.);
#50898=ORIENTED_EDGE('',*,*,#37192,.T.);
#50899=ORIENTED_EDGE('',*,*,#37381,.F.);
#50900=ORIENTED_EDGE('',*,*,#37382,.F.);
#50901=ORIENTED_EDGE('',*,*,#37198,.T.);
#50902=ORIENTED_EDGE('',*,*,#37382,.T.);
#50903=ORIENTED_EDGE('',*,*,#37383,.F.);
#50904=ORIENTED_EDGE('',*,*,#37196,.T.);
#50905=ORIENTED_EDGE('',*,*,#37204,.T.);
#50906=ORIENTED_EDGE('',*,*,#37199,.T.);
#50907=ORIENTED_EDGE('',*,*,#37384,.F.);
#50908=ORIENTED_EDGE('',*,*,#37385,.F.);
#50909=ORIENTED_EDGE('',*,*,#37205,.T.);
#50910=ORIENTED_EDGE('',*,*,#37385,.T.);
#50911=ORIENTED_EDGE('',*,*,#37386,.F.);
#50912=ORIENTED_EDGE('',*,*,#37203,.T.);
#50913=ORIENTED_EDGE('',*,*,#37211,.T.);
#50914=ORIENTED_EDGE('',*,*,#37206,.T.);
#50915=ORIENTED_EDGE('',*,*,#37387,.F.);
#50916=ORIENTED_EDGE('',*,*,#37388,.F.);
#50917=ORIENTED_EDGE('',*,*,#37212,.T.);
#50918=ORIENTED_EDGE('',*,*,#37388,.T.);
#50919=ORIENTED_EDGE('',*,*,#37389,.F.);
#50920=ORIENTED_EDGE('',*,*,#37210,.T.);
#50921=ORIENTED_EDGE('',*,*,#37390,.F.);
#50922=ORIENTED_EDGE('',*,*,#37304,.T.);
#50923=ORIENTED_EDGE('',*,*,#37213,.T.);
#50924=ORIENTED_EDGE('',*,*,#37216,.T.);
#50925=ORIENTED_EDGE('',*,*,#37391,.T.);
#50926=ORIENTED_EDGE('',*,*,#37392,.F.);
#50927=ORIENTED_EDGE('',*,*,#37217,.T.);
#50928=ORIENTED_EDGE('',*,*,#37393,.F.);
#50929=ORIENTED_EDGE('',*,*,#37394,.F.);
#50930=ORIENTED_EDGE('',*,*,#37395,.F.);
#50931=ORIENTED_EDGE('',*,*,#37396,.F.);
#50932=ORIENTED_EDGE('',*,*,#37391,.F.);
#50933=ORIENTED_EDGE('',*,*,#37396,.T.);
#50934=ORIENTED_EDGE('',*,*,#37397,.F.);
#50935=ORIENTED_EDGE('',*,*,#37219,.T.);
#50936=ORIENTED_EDGE('',*,*,#37392,.T.);
#50937=ORIENTED_EDGE('',*,*,#37398,.T.);
#50938=ORIENTED_EDGE('',*,*,#37399,.F.);
#50939=ORIENTED_EDGE('',*,*,#37221,.T.);
#50940=ORIENTED_EDGE('',*,*,#37400,.F.);
#50941=ORIENTED_EDGE('',*,*,#37401,.F.);
#50942=ORIENTED_EDGE('',*,*,#37402,.F.);
#50943=ORIENTED_EDGE('',*,*,#37403,.F.);
#50944=ORIENTED_EDGE('',*,*,#37398,.F.);
#50945=ORIENTED_EDGE('',*,*,#37403,.T.);
#50946=ORIENTED_EDGE('',*,*,#37404,.F.);
#50947=ORIENTED_EDGE('',*,*,#37222,.T.);
#50948=ORIENTED_EDGE('',*,*,#37399,.T.);
#50949=ORIENTED_EDGE('',*,*,#37405,.T.);
#50950=ORIENTED_EDGE('',*,*,#37406,.F.);
#50951=ORIENTED_EDGE('',*,*,#37224,.T.);
#50952=ORIENTED_EDGE('',*,*,#37407,.F.);
#50953=ORIENTED_EDGE('',*,*,#37408,.F.);
#50954=ORIENTED_EDGE('',*,*,#37409,.F.);
#50955=ORIENTED_EDGE('',*,*,#37410,.F.);
#50956=ORIENTED_EDGE('',*,*,#37405,.F.);
#50957=ORIENTED_EDGE('',*,*,#37410,.T.);
#50958=ORIENTED_EDGE('',*,*,#37411,.F.);
#50959=ORIENTED_EDGE('',*,*,#37225,.T.);
#50960=ORIENTED_EDGE('',*,*,#37406,.T.);
#50961=ORIENTED_EDGE('',*,*,#37412,.T.);
#50962=ORIENTED_EDGE('',*,*,#37413,.F.);
#50963=ORIENTED_EDGE('',*,*,#37227,.T.);
#50964=ORIENTED_EDGE('',*,*,#37414,.F.);
#50965=ORIENTED_EDGE('',*,*,#37415,.F.);
#50966=ORIENTED_EDGE('',*,*,#37416,.F.);
#50967=ORIENTED_EDGE('',*,*,#37417,.F.);
#50968=ORIENTED_EDGE('',*,*,#37412,.F.);
#50969=ORIENTED_EDGE('',*,*,#37417,.T.);
#50970=ORIENTED_EDGE('',*,*,#37418,.F.);
#50971=ORIENTED_EDGE('',*,*,#37228,.T.);
#50972=ORIENTED_EDGE('',*,*,#37413,.T.);
#50973=ORIENTED_EDGE('',*,*,#37419,.T.);
#50974=ORIENTED_EDGE('',*,*,#37420,.F.);
#50975=ORIENTED_EDGE('',*,*,#37230,.T.);
#50976=ORIENTED_EDGE('',*,*,#37421,.F.);
#50977=ORIENTED_EDGE('',*,*,#37422,.F.);
#50978=ORIENTED_EDGE('',*,*,#37423,.F.);
#50979=ORIENTED_EDGE('',*,*,#37424,.F.);
#50980=ORIENTED_EDGE('',*,*,#37419,.F.);
#50981=ORIENTED_EDGE('',*,*,#37424,.T.);
#50982=ORIENTED_EDGE('',*,*,#37425,.F.);
#50983=ORIENTED_EDGE('',*,*,#37231,.T.);
#50984=ORIENTED_EDGE('',*,*,#37420,.T.);
#50985=ORIENTED_EDGE('',*,*,#37426,.T.);
#50986=ORIENTED_EDGE('',*,*,#37427,.F.);
#50987=ORIENTED_EDGE('',*,*,#37233,.T.);
#50988=ORIENTED_EDGE('',*,*,#37428,.F.);
#50989=ORIENTED_EDGE('',*,*,#37429,.F.);
#50990=ORIENTED_EDGE('',*,*,#37430,.F.);
#50991=ORIENTED_EDGE('',*,*,#37431,.F.);
#50992=ORIENTED_EDGE('',*,*,#37426,.F.);
#50993=ORIENTED_EDGE('',*,*,#37431,.T.);
#50994=ORIENTED_EDGE('',*,*,#37432,.F.);
#50995=ORIENTED_EDGE('',*,*,#37234,.T.);
#50996=ORIENTED_EDGE('',*,*,#37427,.T.);
#50997=ORIENTED_EDGE('',*,*,#37433,.T.);
#50998=ORIENTED_EDGE('',*,*,#37434,.F.);
#50999=ORIENTED_EDGE('',*,*,#37236,.T.);
#51000=ORIENTED_EDGE('',*,*,#37435,.F.);
#51001=ORIENTED_EDGE('',*,*,#37436,.F.);
#51002=ORIENTED_EDGE('',*,*,#37437,.F.);
#51003=ORIENTED_EDGE('',*,*,#37438,.F.);
#51004=ORIENTED_EDGE('',*,*,#37433,.F.);
#51005=ORIENTED_EDGE('',*,*,#37438,.T.);
#51006=ORIENTED_EDGE('',*,*,#37439,.F.);
#51007=ORIENTED_EDGE('',*,*,#37237,.T.);
#51008=ORIENTED_EDGE('',*,*,#37434,.T.);
#51009=ORIENTED_EDGE('',*,*,#37440,.T.);
#51010=ORIENTED_EDGE('',*,*,#37441,.F.);
#51011=ORIENTED_EDGE('',*,*,#37239,.T.);
#51012=ORIENTED_EDGE('',*,*,#37442,.F.);
#51013=ORIENTED_EDGE('',*,*,#37443,.F.);
#51014=ORIENTED_EDGE('',*,*,#37444,.F.);
#51015=ORIENTED_EDGE('',*,*,#37445,.F.);
#51016=ORIENTED_EDGE('',*,*,#37440,.F.);
#51017=ORIENTED_EDGE('',*,*,#37445,.T.);
#51018=ORIENTED_EDGE('',*,*,#37446,.F.);
#51019=ORIENTED_EDGE('',*,*,#37240,.T.);
#51020=ORIENTED_EDGE('',*,*,#37441,.T.);
#51021=ORIENTED_EDGE('',*,*,#37447,.T.);
#51022=ORIENTED_EDGE('',*,*,#37448,.F.);
#51023=ORIENTED_EDGE('',*,*,#37242,.T.);
#51024=ORIENTED_EDGE('',*,*,#37449,.F.);
#51025=ORIENTED_EDGE('',*,*,#37450,.F.);
#51026=ORIENTED_EDGE('',*,*,#37451,.F.);
#51027=ORIENTED_EDGE('',*,*,#37452,.F.);
#51028=ORIENTED_EDGE('',*,*,#37447,.F.);
#51029=ORIENTED_EDGE('',*,*,#37452,.T.);
#51030=ORIENTED_EDGE('',*,*,#37453,.F.);
#51031=ORIENTED_EDGE('',*,*,#37243,.T.);
#51032=ORIENTED_EDGE('',*,*,#37448,.T.);
#51033=ORIENTED_EDGE('',*,*,#37454,.T.);
#51034=ORIENTED_EDGE('',*,*,#37455,.F.);
#51035=ORIENTED_EDGE('',*,*,#37245,.T.);
#51036=ORIENTED_EDGE('',*,*,#37456,.F.);
#51037=ORIENTED_EDGE('',*,*,#37457,.F.);
#51038=ORIENTED_EDGE('',*,*,#37458,.F.);
#51039=ORIENTED_EDGE('',*,*,#37459,.F.);
#51040=ORIENTED_EDGE('',*,*,#37454,.F.);
#51041=ORIENTED_EDGE('',*,*,#37459,.T.);
#51042=ORIENTED_EDGE('',*,*,#37460,.F.);
#51043=ORIENTED_EDGE('',*,*,#37246,.T.);
#51044=ORIENTED_EDGE('',*,*,#37455,.T.);
#51045=ORIENTED_EDGE('',*,*,#37461,.T.);
#51046=ORIENTED_EDGE('',*,*,#37462,.F.);
#51047=ORIENTED_EDGE('',*,*,#37248,.T.);
#51048=ORIENTED_EDGE('',*,*,#37463,.F.);
#51049=ORIENTED_EDGE('',*,*,#37464,.F.);
#51050=ORIENTED_EDGE('',*,*,#37465,.F.);
#51051=ORIENTED_EDGE('',*,*,#37466,.F.);
#51052=ORIENTED_EDGE('',*,*,#37461,.F.);
#51053=ORIENTED_EDGE('',*,*,#37466,.T.);
#51054=ORIENTED_EDGE('',*,*,#37467,.F.);
#51055=ORIENTED_EDGE('',*,*,#37249,.T.);
#51056=ORIENTED_EDGE('',*,*,#37462,.T.);
#51057=ORIENTED_EDGE('',*,*,#37468,.T.);
#51058=ORIENTED_EDGE('',*,*,#37469,.F.);
#51059=ORIENTED_EDGE('',*,*,#37251,.T.);
#51060=ORIENTED_EDGE('',*,*,#37470,.F.);
#51061=ORIENTED_EDGE('',*,*,#37471,.F.);
#51062=ORIENTED_EDGE('',*,*,#37472,.F.);
#51063=ORIENTED_EDGE('',*,*,#37473,.F.);
#51064=ORIENTED_EDGE('',*,*,#37468,.F.);
#51065=ORIENTED_EDGE('',*,*,#37473,.T.);
#51066=ORIENTED_EDGE('',*,*,#37474,.F.);
#51067=ORIENTED_EDGE('',*,*,#37252,.T.);
#51068=ORIENTED_EDGE('',*,*,#37469,.T.);
#51069=ORIENTED_EDGE('',*,*,#37475,.T.);
#51070=ORIENTED_EDGE('',*,*,#37476,.F.);
#51071=ORIENTED_EDGE('',*,*,#37254,.T.);
#51072=ORIENTED_EDGE('',*,*,#37477,.F.);
#51073=ORIENTED_EDGE('',*,*,#37478,.F.);
#51074=ORIENTED_EDGE('',*,*,#37479,.F.);
#51075=ORIENTED_EDGE('',*,*,#37480,.F.);
#51076=ORIENTED_EDGE('',*,*,#37475,.F.);
#51077=ORIENTED_EDGE('',*,*,#37480,.T.);
#51078=ORIENTED_EDGE('',*,*,#37481,.F.);
#51079=ORIENTED_EDGE('',*,*,#37255,.T.);
#51080=ORIENTED_EDGE('',*,*,#37476,.T.);
#51081=ORIENTED_EDGE('',*,*,#37482,.T.);
#51082=ORIENTED_EDGE('',*,*,#37483,.F.);
#51083=ORIENTED_EDGE('',*,*,#37257,.T.);
#51084=ORIENTED_EDGE('',*,*,#37484,.F.);
#51085=ORIENTED_EDGE('',*,*,#37485,.F.);
#51086=ORIENTED_EDGE('',*,*,#37486,.F.);
#51087=ORIENTED_EDGE('',*,*,#37487,.F.);
#51088=ORIENTED_EDGE('',*,*,#37482,.F.);
#51089=ORIENTED_EDGE('',*,*,#37487,.T.);
#51090=ORIENTED_EDGE('',*,*,#37488,.F.);
#51091=ORIENTED_EDGE('',*,*,#37258,.T.);
#51092=ORIENTED_EDGE('',*,*,#37483,.T.);
#51093=ORIENTED_EDGE('',*,*,#34429,.T.);
#51094=ORIENTED_EDGE('',*,*,#37489,.F.);
#51095=ORIENTED_EDGE('',*,*,#37260,.T.);
#51096=ORIENTED_EDGE('',*,*,#37490,.F.);
#51097=ORIENTED_EDGE('',*,*,#34432,.T.);
#51098=ORIENTED_EDGE('',*,*,#37491,.F.);
#51099=ORIENTED_EDGE('',*,*,#37261,.T.);
#51100=ORIENTED_EDGE('',*,*,#37489,.T.);
#51101=ORIENTED_EDGE('',*,*,#37492,.T.);
#51102=ORIENTED_EDGE('',*,*,#37493,.F.);
#51103=ORIENTED_EDGE('',*,*,#37263,.T.);
#51104=ORIENTED_EDGE('',*,*,#37494,.F.);
#51105=ORIENTED_EDGE('',*,*,#37495,.F.);
#51106=ORIENTED_EDGE('',*,*,#37496,.F.);
#51107=ORIENTED_EDGE('',*,*,#37497,.F.);
#51108=ORIENTED_EDGE('',*,*,#37492,.F.);
#51109=ORIENTED_EDGE('',*,*,#37497,.T.);
#51110=ORIENTED_EDGE('',*,*,#37498,.F.);
#51111=ORIENTED_EDGE('',*,*,#37264,.T.);
#51112=ORIENTED_EDGE('',*,*,#37493,.T.);
#51113=ORIENTED_EDGE('',*,*,#37499,.T.);
#51114=ORIENTED_EDGE('',*,*,#37500,.F.);
#51115=ORIENTED_EDGE('',*,*,#37266,.T.);
#51116=ORIENTED_EDGE('',*,*,#37501,.F.);
#51117=ORIENTED_EDGE('',*,*,#37502,.F.);
#51118=ORIENTED_EDGE('',*,*,#37503,.F.);
#51119=ORIENTED_EDGE('',*,*,#37504,.F.);
#51120=ORIENTED_EDGE('',*,*,#37499,.F.);
#51121=ORIENTED_EDGE('',*,*,#37504,.T.);
#51122=ORIENTED_EDGE('',*,*,#37505,.F.);
#51123=ORIENTED_EDGE('',*,*,#37267,.T.);
#51124=ORIENTED_EDGE('',*,*,#37500,.T.);
#51125=ORIENTED_EDGE('',*,*,#37506,.T.);
#51126=ORIENTED_EDGE('',*,*,#37507,.F.);
#51127=ORIENTED_EDGE('',*,*,#37269,.T.);
#51128=ORIENTED_EDGE('',*,*,#37508,.F.);
#51129=ORIENTED_EDGE('',*,*,#37509,.F.);
#51130=ORIENTED_EDGE('',*,*,#37510,.F.);
#51131=ORIENTED_EDGE('',*,*,#37511,.F.);
#51132=ORIENTED_EDGE('',*,*,#37506,.F.);
#51133=ORIENTED_EDGE('',*,*,#37511,.T.);
#51134=ORIENTED_EDGE('',*,*,#37512,.F.);
#51135=ORIENTED_EDGE('',*,*,#37270,.T.);
#51136=ORIENTED_EDGE('',*,*,#37507,.T.);
#51137=ORIENTED_EDGE('',*,*,#37513,.T.);
#51138=ORIENTED_EDGE('',*,*,#37514,.F.);
#51139=ORIENTED_EDGE('',*,*,#37272,.T.);
#51140=ORIENTED_EDGE('',*,*,#37515,.F.);
#51141=ORIENTED_EDGE('',*,*,#37516,.F.);
#51142=ORIENTED_EDGE('',*,*,#37517,.F.);
#51143=ORIENTED_EDGE('',*,*,#37518,.F.);
#51144=ORIENTED_EDGE('',*,*,#37513,.F.);
#51145=ORIENTED_EDGE('',*,*,#37518,.T.);
#51146=ORIENTED_EDGE('',*,*,#37519,.F.);
#51147=ORIENTED_EDGE('',*,*,#37273,.T.);
#51148=ORIENTED_EDGE('',*,*,#37514,.T.);
#51149=ORIENTED_EDGE('',*,*,#37520,.T.);
#51150=ORIENTED_EDGE('',*,*,#37521,.F.);
#51151=ORIENTED_EDGE('',*,*,#37275,.T.);
#51152=ORIENTED_EDGE('',*,*,#37522,.F.);
#51153=ORIENTED_EDGE('',*,*,#37523,.F.);
#51154=ORIENTED_EDGE('',*,*,#37524,.F.);
#51155=ORIENTED_EDGE('',*,*,#37525,.F.);
#51156=ORIENTED_EDGE('',*,*,#37520,.F.);
#51157=ORIENTED_EDGE('',*,*,#37525,.T.);
#51158=ORIENTED_EDGE('',*,*,#37526,.F.);
#51159=ORIENTED_EDGE('',*,*,#37276,.T.);
#51160=ORIENTED_EDGE('',*,*,#37521,.T.);
#51161=ORIENTED_EDGE('',*,*,#37527,.T.);
#51162=ORIENTED_EDGE('',*,*,#37528,.F.);
#51163=ORIENTED_EDGE('',*,*,#37278,.T.);
#51164=ORIENTED_EDGE('',*,*,#37529,.F.);
#51165=ORIENTED_EDGE('',*,*,#37530,.F.);
#51166=ORIENTED_EDGE('',*,*,#37531,.F.);
#51167=ORIENTED_EDGE('',*,*,#37532,.F.);
#51168=ORIENTED_EDGE('',*,*,#37527,.F.);
#51169=ORIENTED_EDGE('',*,*,#37532,.T.);
#51170=ORIENTED_EDGE('',*,*,#37533,.F.);
#51171=ORIENTED_EDGE('',*,*,#37279,.T.);
#51172=ORIENTED_EDGE('',*,*,#37528,.T.);
#51173=ORIENTED_EDGE('',*,*,#37534,.T.);
#51174=ORIENTED_EDGE('',*,*,#37535,.F.);
#51175=ORIENTED_EDGE('',*,*,#37281,.T.);
#51176=ORIENTED_EDGE('',*,*,#37536,.F.);
#51177=ORIENTED_EDGE('',*,*,#37537,.F.);
#51178=ORIENTED_EDGE('',*,*,#37538,.F.);
#51179=ORIENTED_EDGE('',*,*,#37539,.F.);
#51180=ORIENTED_EDGE('',*,*,#37534,.F.);
#51181=ORIENTED_EDGE('',*,*,#37539,.T.);
#51182=ORIENTED_EDGE('',*,*,#37540,.F.);
#51183=ORIENTED_EDGE('',*,*,#37282,.T.);
#51184=ORIENTED_EDGE('',*,*,#37535,.T.);
#51185=ORIENTED_EDGE('',*,*,#37541,.T.);
#51186=ORIENTED_EDGE('',*,*,#37542,.F.);
#51187=ORIENTED_EDGE('',*,*,#37284,.T.);
#51188=ORIENTED_EDGE('',*,*,#37543,.F.);
#51189=ORIENTED_EDGE('',*,*,#37544,.T.);
#51190=ORIENTED_EDGE('',*,*,#37545,.F.);
#51191=ORIENTED_EDGE('',*,*,#37285,.T.);
#51192=ORIENTED_EDGE('',*,*,#37542,.T.);
#51193=ORIENTED_EDGE('',*,*,#37546,.F.);
#51194=ORIENTED_EDGE('',*,*,#37547,.F.);
#51195=ORIENTED_EDGE('',*,*,#37544,.F.);
#51196=ORIENTED_EDGE('',*,*,#37541,.F.);
#51197=ORIENTED_EDGE('',*,*,#37287,.T.);
#51198=ORIENTED_EDGE('',*,*,#37548,.F.);
#51199=ORIENTED_EDGE('',*,*,#37549,.T.);
#51200=ORIENTED_EDGE('',*,*,#37550,.F.);
#51201=ORIENTED_EDGE('',*,*,#37551,.F.);
#51202=ORIENTED_EDGE('',*,*,#37549,.F.);
#51203=ORIENTED_EDGE('',*,*,#37552,.F.);
#51204=ORIENTED_EDGE('',*,*,#37553,.F.);
#51205=ORIENTED_EDGE('',*,*,#37288,.T.);
#51206=ORIENTED_EDGE('',*,*,#37550,.T.);
#51207=ORIENTED_EDGE('',*,*,#37551,.T.);
#51208=ORIENTED_EDGE('',*,*,#37554,.F.);
#51209=ORIENTED_EDGE('',*,*,#37555,.T.);
#51210=ORIENTED_EDGE('',*,*,#37556,.F.);
#51211=ORIENTED_EDGE('',*,*,#37290,.T.);
#51212=ORIENTED_EDGE('',*,*,#37557,.F.);
#51213=ORIENTED_EDGE('',*,*,#37558,.F.);
#51214=ORIENTED_EDGE('',*,*,#37559,.F.);
#51215=ORIENTED_EDGE('',*,*,#37560,.F.);
#51216=ORIENTED_EDGE('',*,*,#37555,.F.);
#51217=ORIENTED_EDGE('',*,*,#37560,.T.);
#51218=ORIENTED_EDGE('',*,*,#37561,.F.);
#51219=ORIENTED_EDGE('',*,*,#37291,.T.);
#51220=ORIENTED_EDGE('',*,*,#37556,.T.);
#51221=ORIENTED_EDGE('',*,*,#37562,.T.);
#51222=ORIENTED_EDGE('',*,*,#37563,.F.);
#51223=ORIENTED_EDGE('',*,*,#37293,.T.);
#51224=ORIENTED_EDGE('',*,*,#37564,.F.);
#51225=ORIENTED_EDGE('',*,*,#37565,.F.);
#51226=ORIENTED_EDGE('',*,*,#37566,.F.);
#51227=ORIENTED_EDGE('',*,*,#37567,.F.);
#51228=ORIENTED_EDGE('',*,*,#37562,.F.);
#51229=ORIENTED_EDGE('',*,*,#37567,.T.);
#51230=ORIENTED_EDGE('',*,*,#37568,.F.);
#51231=ORIENTED_EDGE('',*,*,#37294,.T.);
#51232=ORIENTED_EDGE('',*,*,#37563,.T.);
#51233=ORIENTED_EDGE('',*,*,#37569,.T.);
#51234=ORIENTED_EDGE('',*,*,#37570,.F.);
#51235=ORIENTED_EDGE('',*,*,#37296,.T.);
#51236=ORIENTED_EDGE('',*,*,#37571,.F.);
#51237=ORIENTED_EDGE('',*,*,#37572,.F.);
#51238=ORIENTED_EDGE('',*,*,#37573,.F.);
#51239=ORIENTED_EDGE('',*,*,#37574,.F.);
#51240=ORIENTED_EDGE('',*,*,#37569,.F.);
#51241=ORIENTED_EDGE('',*,*,#37574,.T.);
#51242=ORIENTED_EDGE('',*,*,#37575,.F.);
#51243=ORIENTED_EDGE('',*,*,#37297,.T.);
#51244=ORIENTED_EDGE('',*,*,#37570,.T.);
#51245=ORIENTED_EDGE('',*,*,#37576,.T.);
#51246=ORIENTED_EDGE('',*,*,#37577,.F.);
#51247=ORIENTED_EDGE('',*,*,#37299,.T.);
#51248=ORIENTED_EDGE('',*,*,#37578,.F.);
#51249=ORIENTED_EDGE('',*,*,#37579,.F.);
#51250=ORIENTED_EDGE('',*,*,#37580,.F.);
#51251=ORIENTED_EDGE('',*,*,#37581,.F.);
#51252=ORIENTED_EDGE('',*,*,#37576,.F.);
#51253=ORIENTED_EDGE('',*,*,#37581,.T.);
#51254=ORIENTED_EDGE('',*,*,#37582,.F.);
#51255=ORIENTED_EDGE('',*,*,#37300,.T.);
#51256=ORIENTED_EDGE('',*,*,#37577,.T.);
#51257=ORIENTED_EDGE('',*,*,#37583,.T.);
#51258=ORIENTED_EDGE('',*,*,#37584,.F.);
#51259=ORIENTED_EDGE('',*,*,#37302,.T.);
#51260=ORIENTED_EDGE('',*,*,#37585,.F.);
#51261=ORIENTED_EDGE('',*,*,#37586,.F.);
#51262=ORIENTED_EDGE('',*,*,#37587,.F.);
#51263=ORIENTED_EDGE('',*,*,#37588,.F.);
#51264=ORIENTED_EDGE('',*,*,#37583,.F.);
#51265=ORIENTED_EDGE('',*,*,#37588,.T.);
#51266=ORIENTED_EDGE('',*,*,#37589,.F.);
#51267=ORIENTED_EDGE('',*,*,#37303,.T.);
#51268=ORIENTED_EDGE('',*,*,#37584,.T.);
#51269=ORIENTED_EDGE('',*,*,#37305,.T.);
#51270=ORIENTED_EDGE('',*,*,#37590,.F.);
#51271=ORIENTED_EDGE('',*,*,#37591,.T.);
#51272=ORIENTED_EDGE('',*,*,#37592,.F.);
#51273=ORIENTED_EDGE('',*,*,#37306,.T.);
#51274=ORIENTED_EDGE('',*,*,#37592,.T.);
#51275=ORIENTED_EDGE('',*,*,#37593,.T.);
#51276=ORIENTED_EDGE('',*,*,#37594,.F.);
#51277=ORIENTED_EDGE('',*,*,#37593,.F.);
#51278=ORIENTED_EDGE('',*,*,#37591,.F.);
#51279=ORIENTED_EDGE('',*,*,#37595,.F.);
#51280=ORIENTED_EDGE('',*,*,#37596,.F.);
#51281=ORIENTED_EDGE('',*,*,#37308,.T.);
#51282=ORIENTED_EDGE('',*,*,#37597,.F.);
#51283=ORIENTED_EDGE('',*,*,#37598,.T.);
#51284=ORIENTED_EDGE('',*,*,#37599,.F.);
#51285=ORIENTED_EDGE('',*,*,#37309,.T.);
#51286=ORIENTED_EDGE('',*,*,#37599,.T.);
#51287=ORIENTED_EDGE('',*,*,#37600,.T.);
#51288=ORIENTED_EDGE('',*,*,#37601,.F.);
#51289=ORIENTED_EDGE('',*,*,#37600,.F.);
#51290=ORIENTED_EDGE('',*,*,#37598,.F.);
#51291=ORIENTED_EDGE('',*,*,#37602,.F.);
#51292=ORIENTED_EDGE('',*,*,#37603,.F.);
#51293=ORIENTED_EDGE('',*,*,#37311,.T.);
#51294=ORIENTED_EDGE('',*,*,#37604,.F.);
#51295=ORIENTED_EDGE('',*,*,#37605,.T.);
#51296=ORIENTED_EDGE('',*,*,#37606,.F.);
#51297=ORIENTED_EDGE('',*,*,#37312,.T.);
#51298=ORIENTED_EDGE('',*,*,#37606,.T.);
#51299=ORIENTED_EDGE('',*,*,#37607,.T.);
#51300=ORIENTED_EDGE('',*,*,#37608,.F.);
#51301=ORIENTED_EDGE('',*,*,#37607,.F.);
#51302=ORIENTED_EDGE('',*,*,#37605,.F.);
#51303=ORIENTED_EDGE('',*,*,#37609,.F.);
#51304=ORIENTED_EDGE('',*,*,#37610,.F.);
#51305=ORIENTED_EDGE('',*,*,#37314,.T.);
#51306=ORIENTED_EDGE('',*,*,#37611,.F.);
#51307=ORIENTED_EDGE('',*,*,#37612,.T.);
#51308=ORIENTED_EDGE('',*,*,#37613,.F.);
#51309=ORIENTED_EDGE('',*,*,#37315,.T.);
#51310=ORIENTED_EDGE('',*,*,#37613,.T.);
#51311=ORIENTED_EDGE('',*,*,#37614,.T.);
#51312=ORIENTED_EDGE('',*,*,#37615,.F.);
#51313=ORIENTED_EDGE('',*,*,#37614,.F.);
#51314=ORIENTED_EDGE('',*,*,#37612,.F.);
#51315=ORIENTED_EDGE('',*,*,#37616,.F.);
#51316=ORIENTED_EDGE('',*,*,#37617,.F.);
#51317=ORIENTED_EDGE('',*,*,#37317,.T.);
#51318=ORIENTED_EDGE('',*,*,#37618,.F.);
#51319=ORIENTED_EDGE('',*,*,#37619,.T.);
#51320=ORIENTED_EDGE('',*,*,#37620,.F.);
#51321=ORIENTED_EDGE('',*,*,#37318,.T.);
#51322=ORIENTED_EDGE('',*,*,#37620,.T.);
#51323=ORIENTED_EDGE('',*,*,#37621,.T.);
#51324=ORIENTED_EDGE('',*,*,#37622,.F.);
#51325=ORIENTED_EDGE('',*,*,#37621,.F.);
#51326=ORIENTED_EDGE('',*,*,#37619,.F.);
#51327=ORIENTED_EDGE('',*,*,#37623,.F.);
#51328=ORIENTED_EDGE('',*,*,#37624,.F.);
#51329=ORIENTED_EDGE('',*,*,#37320,.T.);
#51330=ORIENTED_EDGE('',*,*,#37625,.F.);
#51331=ORIENTED_EDGE('',*,*,#37626,.T.);
#51332=ORIENTED_EDGE('',*,*,#37627,.F.);
#51333=ORIENTED_EDGE('',*,*,#37321,.T.);
#51334=ORIENTED_EDGE('',*,*,#37627,.T.);
#51335=ORIENTED_EDGE('',*,*,#37628,.T.);
#51336=ORIENTED_EDGE('',*,*,#37629,.F.);
#51337=ORIENTED_EDGE('',*,*,#37628,.F.);
#51338=ORIENTED_EDGE('',*,*,#37626,.F.);
#51339=ORIENTED_EDGE('',*,*,#37630,.F.);
#51340=ORIENTED_EDGE('',*,*,#37631,.F.);
#51341=ORIENTED_EDGE('',*,*,#37323,.T.);
#51342=ORIENTED_EDGE('',*,*,#37632,.F.);
#51343=ORIENTED_EDGE('',*,*,#37633,.T.);
#51344=ORIENTED_EDGE('',*,*,#37634,.F.);
#51345=ORIENTED_EDGE('',*,*,#37324,.T.);
#51346=ORIENTED_EDGE('',*,*,#37634,.T.);
#51347=ORIENTED_EDGE('',*,*,#37635,.T.);
#51348=ORIENTED_EDGE('',*,*,#37636,.F.);
#51349=ORIENTED_EDGE('',*,*,#37635,.F.);
#51350=ORIENTED_EDGE('',*,*,#37633,.F.);
#51351=ORIENTED_EDGE('',*,*,#37637,.F.);
#51352=ORIENTED_EDGE('',*,*,#37638,.F.);
#51353=ORIENTED_EDGE('',*,*,#37326,.T.);
#51354=ORIENTED_EDGE('',*,*,#37639,.F.);
#51355=ORIENTED_EDGE('',*,*,#37640,.T.);
#51356=ORIENTED_EDGE('',*,*,#37641,.F.);
#51357=ORIENTED_EDGE('',*,*,#37327,.T.);
#51358=ORIENTED_EDGE('',*,*,#37641,.T.);
#51359=ORIENTED_EDGE('',*,*,#37642,.T.);
#51360=ORIENTED_EDGE('',*,*,#37643,.F.);
#51361=ORIENTED_EDGE('',*,*,#37642,.F.);
#51362=ORIENTED_EDGE('',*,*,#37640,.F.);
#51363=ORIENTED_EDGE('',*,*,#37644,.F.);
#51364=ORIENTED_EDGE('',*,*,#37645,.F.);
#51365=ORIENTED_EDGE('',*,*,#37329,.T.);
#51366=ORIENTED_EDGE('',*,*,#37646,.F.);
#51367=ORIENTED_EDGE('',*,*,#37647,.T.);
#51368=ORIENTED_EDGE('',*,*,#37648,.F.);
#51369=ORIENTED_EDGE('',*,*,#37330,.T.);
#51370=ORIENTED_EDGE('',*,*,#37648,.T.);
#51371=ORIENTED_EDGE('',*,*,#37649,.T.);
#51372=ORIENTED_EDGE('',*,*,#37650,.F.);
#51373=ORIENTED_EDGE('',*,*,#37649,.F.);
#51374=ORIENTED_EDGE('',*,*,#37647,.F.);
#51375=ORIENTED_EDGE('',*,*,#37651,.F.);
#51376=ORIENTED_EDGE('',*,*,#37652,.F.);
#51377=ORIENTED_EDGE('',*,*,#37332,.T.);
#51378=ORIENTED_EDGE('',*,*,#37653,.F.);
#51379=ORIENTED_EDGE('',*,*,#37654,.T.);
#51380=ORIENTED_EDGE('',*,*,#37655,.F.);
#51381=ORIENTED_EDGE('',*,*,#37333,.T.);
#51382=ORIENTED_EDGE('',*,*,#37655,.T.);
#51383=ORIENTED_EDGE('',*,*,#37656,.T.);
#51384=ORIENTED_EDGE('',*,*,#37657,.F.);
#51385=ORIENTED_EDGE('',*,*,#37656,.F.);
#51386=ORIENTED_EDGE('',*,*,#37654,.F.);
#51387=ORIENTED_EDGE('',*,*,#37658,.F.);
#51388=ORIENTED_EDGE('',*,*,#37659,.F.);
#51389=ORIENTED_EDGE('',*,*,#37335,.T.);
#51390=ORIENTED_EDGE('',*,*,#37660,.F.);
#51391=ORIENTED_EDGE('',*,*,#37661,.T.);
#51392=ORIENTED_EDGE('',*,*,#37662,.F.);
#51393=ORIENTED_EDGE('',*,*,#37336,.T.);
#51394=ORIENTED_EDGE('',*,*,#37662,.T.);
#51395=ORIENTED_EDGE('',*,*,#37663,.T.);
#51396=ORIENTED_EDGE('',*,*,#37664,.F.);
#51397=ORIENTED_EDGE('',*,*,#37663,.F.);
#51398=ORIENTED_EDGE('',*,*,#37661,.F.);
#51399=ORIENTED_EDGE('',*,*,#37665,.F.);
#51400=ORIENTED_EDGE('',*,*,#37666,.F.);
#51401=ORIENTED_EDGE('',*,*,#37338,.T.);
#51402=ORIENTED_EDGE('',*,*,#37667,.F.);
#51403=ORIENTED_EDGE('',*,*,#37668,.T.);
#51404=ORIENTED_EDGE('',*,*,#37669,.F.);
#51405=ORIENTED_EDGE('',*,*,#37339,.T.);
#51406=ORIENTED_EDGE('',*,*,#37669,.T.);
#51407=ORIENTED_EDGE('',*,*,#37670,.T.);
#51408=ORIENTED_EDGE('',*,*,#37671,.F.);
#51409=ORIENTED_EDGE('',*,*,#37670,.F.);
#51410=ORIENTED_EDGE('',*,*,#37668,.F.);
#51411=ORIENTED_EDGE('',*,*,#37672,.F.);
#51412=ORIENTED_EDGE('',*,*,#37673,.F.);
#51413=ORIENTED_EDGE('',*,*,#37341,.T.);
#51414=ORIENTED_EDGE('',*,*,#37674,.F.);
#51415=ORIENTED_EDGE('',*,*,#37675,.T.);
#51416=ORIENTED_EDGE('',*,*,#37676,.F.);
#51417=ORIENTED_EDGE('',*,*,#37342,.T.);
#51418=ORIENTED_EDGE('',*,*,#37676,.T.);
#51419=ORIENTED_EDGE('',*,*,#37677,.T.);
#51420=ORIENTED_EDGE('',*,*,#37678,.F.);
#51421=ORIENTED_EDGE('',*,*,#37677,.F.);
#51422=ORIENTED_EDGE('',*,*,#37675,.F.);
#51423=ORIENTED_EDGE('',*,*,#37679,.F.);
#51424=ORIENTED_EDGE('',*,*,#37680,.F.);
#51425=ORIENTED_EDGE('',*,*,#37344,.T.);
#51426=ORIENTED_EDGE('',*,*,#37681,.F.);
#51427=ORIENTED_EDGE('',*,*,#37682,.T.);
#51428=ORIENTED_EDGE('',*,*,#37683,.F.);
#51429=ORIENTED_EDGE('',*,*,#37345,.T.);
#51430=ORIENTED_EDGE('',*,*,#37683,.T.);
#51431=ORIENTED_EDGE('',*,*,#37684,.T.);
#51432=ORIENTED_EDGE('',*,*,#37685,.F.);
#51433=ORIENTED_EDGE('',*,*,#37684,.F.);
#51434=ORIENTED_EDGE('',*,*,#37682,.F.);
#51435=ORIENTED_EDGE('',*,*,#37686,.F.);
#51436=ORIENTED_EDGE('',*,*,#37687,.F.);
#51437=ORIENTED_EDGE('',*,*,#37347,.T.);
#51438=ORIENTED_EDGE('',*,*,#37688,.F.);
#51439=ORIENTED_EDGE('',*,*,#37689,.T.);
#51440=ORIENTED_EDGE('',*,*,#37690,.F.);
#51441=ORIENTED_EDGE('',*,*,#37348,.T.);
#51442=ORIENTED_EDGE('',*,*,#37690,.T.);
#51443=ORIENTED_EDGE('',*,*,#37691,.T.);
#51444=ORIENTED_EDGE('',*,*,#37692,.F.);
#51445=ORIENTED_EDGE('',*,*,#37691,.F.);
#51446=ORIENTED_EDGE('',*,*,#37689,.F.);
#51447=ORIENTED_EDGE('',*,*,#37693,.F.);
#51448=ORIENTED_EDGE('',*,*,#37694,.F.);
#51449=ORIENTED_EDGE('',*,*,#37350,.T.);
#51450=ORIENTED_EDGE('',*,*,#37695,.F.);
#51451=ORIENTED_EDGE('',*,*,#37696,.T.);
#51452=ORIENTED_EDGE('',*,*,#37697,.F.);
#51453=ORIENTED_EDGE('',*,*,#37351,.T.);
#51454=ORIENTED_EDGE('',*,*,#37697,.T.);
#51455=ORIENTED_EDGE('',*,*,#37698,.T.);
#51456=ORIENTED_EDGE('',*,*,#37699,.F.);
#51457=ORIENTED_EDGE('',*,*,#37698,.F.);
#51458=ORIENTED_EDGE('',*,*,#37696,.F.);
#51459=ORIENTED_EDGE('',*,*,#37700,.F.);
#51460=ORIENTED_EDGE('',*,*,#37701,.F.);
#51461=ORIENTED_EDGE('',*,*,#37353,.T.);
#51462=ORIENTED_EDGE('',*,*,#37702,.F.);
#51463=ORIENTED_EDGE('',*,*,#37703,.T.);
#51464=ORIENTED_EDGE('',*,*,#37704,.F.);
#51465=ORIENTED_EDGE('',*,*,#37354,.T.);
#51466=ORIENTED_EDGE('',*,*,#37704,.T.);
#51467=ORIENTED_EDGE('',*,*,#37705,.T.);
#51468=ORIENTED_EDGE('',*,*,#37706,.F.);
#51469=ORIENTED_EDGE('',*,*,#37705,.F.);
#51470=ORIENTED_EDGE('',*,*,#37703,.F.);
#51471=ORIENTED_EDGE('',*,*,#37707,.F.);
#51472=ORIENTED_EDGE('',*,*,#37708,.F.);
#51473=ORIENTED_EDGE('',*,*,#37356,.T.);
#51474=ORIENTED_EDGE('',*,*,#37709,.F.);
#51475=ORIENTED_EDGE('',*,*,#37710,.T.);
#51476=ORIENTED_EDGE('',*,*,#37711,.F.);
#51477=ORIENTED_EDGE('',*,*,#37357,.T.);
#51478=ORIENTED_EDGE('',*,*,#37711,.T.);
#51479=ORIENTED_EDGE('',*,*,#37712,.T.);
#51480=ORIENTED_EDGE('',*,*,#37713,.F.);
#51481=ORIENTED_EDGE('',*,*,#37712,.F.);
#51482=ORIENTED_EDGE('',*,*,#37710,.F.);
#51483=ORIENTED_EDGE('',*,*,#37714,.F.);
#51484=ORIENTED_EDGE('',*,*,#37715,.F.);
#51485=ORIENTED_EDGE('',*,*,#37359,.T.);
#51486=ORIENTED_EDGE('',*,*,#37716,.F.);
#51487=ORIENTED_EDGE('',*,*,#37717,.T.);
#51488=ORIENTED_EDGE('',*,*,#37718,.F.);
#51489=ORIENTED_EDGE('',*,*,#37360,.T.);
#51490=ORIENTED_EDGE('',*,*,#37718,.T.);
#51491=ORIENTED_EDGE('',*,*,#37719,.T.);
#51492=ORIENTED_EDGE('',*,*,#37720,.F.);
#51493=ORIENTED_EDGE('',*,*,#37719,.F.);
#51494=ORIENTED_EDGE('',*,*,#37717,.F.);
#51495=ORIENTED_EDGE('',*,*,#37721,.F.);
#51496=ORIENTED_EDGE('',*,*,#37722,.F.);
#51497=ORIENTED_EDGE('',*,*,#37362,.T.);
#51498=ORIENTED_EDGE('',*,*,#37723,.F.);
#51499=ORIENTED_EDGE('',*,*,#37724,.T.);
#51500=ORIENTED_EDGE('',*,*,#37725,.F.);
#51501=ORIENTED_EDGE('',*,*,#37363,.T.);
#51502=ORIENTED_EDGE('',*,*,#37725,.T.);
#51503=ORIENTED_EDGE('',*,*,#37726,.T.);
#51504=ORIENTED_EDGE('',*,*,#37727,.F.);
#51505=ORIENTED_EDGE('',*,*,#37726,.F.);
#51506=ORIENTED_EDGE('',*,*,#37724,.F.);
#51507=ORIENTED_EDGE('',*,*,#37728,.F.);
#51508=ORIENTED_EDGE('',*,*,#37729,.F.);
#51509=ORIENTED_EDGE('',*,*,#37365,.T.);
#51510=ORIENTED_EDGE('',*,*,#37730,.F.);
#51511=ORIENTED_EDGE('',*,*,#37731,.T.);
#51512=ORIENTED_EDGE('',*,*,#37732,.F.);
#51513=ORIENTED_EDGE('',*,*,#37366,.T.);
#51514=ORIENTED_EDGE('',*,*,#37732,.T.);
#51515=ORIENTED_EDGE('',*,*,#37733,.T.);
#51516=ORIENTED_EDGE('',*,*,#37734,.F.);
#51517=ORIENTED_EDGE('',*,*,#37733,.F.);
#51518=ORIENTED_EDGE('',*,*,#37731,.F.);
#51519=ORIENTED_EDGE('',*,*,#37735,.F.);
#51520=ORIENTED_EDGE('',*,*,#37736,.F.);
#51521=ORIENTED_EDGE('',*,*,#37368,.T.);
#51522=ORIENTED_EDGE('',*,*,#37737,.F.);
#51523=ORIENTED_EDGE('',*,*,#34428,.T.);
#51524=ORIENTED_EDGE('',*,*,#37738,.F.);
#51525=ORIENTED_EDGE('',*,*,#37369,.T.);
#51526=ORIENTED_EDGE('',*,*,#37738,.T.);
#51527=ORIENTED_EDGE('',*,*,#34427,.T.);
#51528=ORIENTED_EDGE('',*,*,#37739,.F.);
#51529=ORIENTED_EDGE('',*,*,#37371,.T.);
#51530=ORIENTED_EDGE('',*,*,#37740,.F.);
#51531=ORIENTED_EDGE('',*,*,#37741,.T.);
#51532=ORIENTED_EDGE('',*,*,#37742,.F.);
#51533=ORIENTED_EDGE('',*,*,#37372,.T.);
#51534=ORIENTED_EDGE('',*,*,#37742,.T.);
#51535=ORIENTED_EDGE('',*,*,#37743,.T.);
#51536=ORIENTED_EDGE('',*,*,#37744,.F.);
#51537=ORIENTED_EDGE('',*,*,#37743,.F.);
#51538=ORIENTED_EDGE('',*,*,#37741,.F.);
#51539=ORIENTED_EDGE('',*,*,#37745,.F.);
#51540=ORIENTED_EDGE('',*,*,#37746,.F.);
#51541=ORIENTED_EDGE('',*,*,#37374,.T.);
#51542=ORIENTED_EDGE('',*,*,#37747,.F.);
#51543=ORIENTED_EDGE('',*,*,#37748,.T.);
#51544=ORIENTED_EDGE('',*,*,#37749,.F.);
#51545=ORIENTED_EDGE('',*,*,#37375,.T.);
#51546=ORIENTED_EDGE('',*,*,#37749,.T.);
#51547=ORIENTED_EDGE('',*,*,#37750,.T.);
#51548=ORIENTED_EDGE('',*,*,#37751,.F.);
#51549=ORIENTED_EDGE('',*,*,#37750,.F.);
#51550=ORIENTED_EDGE('',*,*,#37748,.F.);
#51551=ORIENTED_EDGE('',*,*,#37752,.F.);
#51552=ORIENTED_EDGE('',*,*,#37753,.F.);
#51553=ORIENTED_EDGE('',*,*,#37377,.T.);
#51554=ORIENTED_EDGE('',*,*,#37754,.F.);
#51555=ORIENTED_EDGE('',*,*,#37755,.T.);
#51556=ORIENTED_EDGE('',*,*,#37756,.F.);
#51557=ORIENTED_EDGE('',*,*,#37378,.T.);
#51558=ORIENTED_EDGE('',*,*,#37756,.T.);
#51559=ORIENTED_EDGE('',*,*,#37757,.T.);
#51560=ORIENTED_EDGE('',*,*,#37758,.F.);
#51561=ORIENTED_EDGE('',*,*,#37757,.F.);
#51562=ORIENTED_EDGE('',*,*,#37755,.F.);
#51563=ORIENTED_EDGE('',*,*,#37759,.F.);
#51564=ORIENTED_EDGE('',*,*,#37760,.F.);
#51565=ORIENTED_EDGE('',*,*,#37380,.T.);
#51566=ORIENTED_EDGE('',*,*,#37761,.F.);
#51567=ORIENTED_EDGE('',*,*,#37762,.T.);
#51568=ORIENTED_EDGE('',*,*,#37763,.F.);
#51569=ORIENTED_EDGE('',*,*,#37381,.T.);
#51570=ORIENTED_EDGE('',*,*,#37763,.T.);
#51571=ORIENTED_EDGE('',*,*,#37764,.T.);
#51572=ORIENTED_EDGE('',*,*,#37765,.F.);
#51573=ORIENTED_EDGE('',*,*,#37764,.F.);
#51574=ORIENTED_EDGE('',*,*,#37762,.F.);
#51575=ORIENTED_EDGE('',*,*,#37766,.F.);
#51576=ORIENTED_EDGE('',*,*,#37767,.F.);
#51577=ORIENTED_EDGE('',*,*,#37383,.T.);
#51578=ORIENTED_EDGE('',*,*,#37768,.F.);
#51579=ORIENTED_EDGE('',*,*,#37769,.T.);
#51580=ORIENTED_EDGE('',*,*,#37770,.F.);
#51581=ORIENTED_EDGE('',*,*,#37384,.T.);
#51582=ORIENTED_EDGE('',*,*,#37770,.T.);
#51583=ORIENTED_EDGE('',*,*,#37771,.T.);
#51584=ORIENTED_EDGE('',*,*,#37772,.F.);
#51585=ORIENTED_EDGE('',*,*,#37771,.F.);
#51586=ORIENTED_EDGE('',*,*,#37769,.F.);
#51587=ORIENTED_EDGE('',*,*,#37773,.F.);
#51588=ORIENTED_EDGE('',*,*,#37774,.F.);
#51589=ORIENTED_EDGE('',*,*,#37386,.T.);
#51590=ORIENTED_EDGE('',*,*,#37775,.F.);
#51591=ORIENTED_EDGE('',*,*,#37776,.T.);
#51592=ORIENTED_EDGE('',*,*,#37777,.F.);
#51593=ORIENTED_EDGE('',*,*,#37387,.T.);
#51594=ORIENTED_EDGE('',*,*,#37777,.T.);
#51595=ORIENTED_EDGE('',*,*,#37778,.T.);
#51596=ORIENTED_EDGE('',*,*,#37779,.F.);
#51597=ORIENTED_EDGE('',*,*,#37778,.F.);
#51598=ORIENTED_EDGE('',*,*,#37776,.F.);
#51599=ORIENTED_EDGE('',*,*,#37780,.F.);
#51600=ORIENTED_EDGE('',*,*,#37781,.F.);
#51601=ORIENTED_EDGE('',*,*,#37389,.T.);
#51602=ORIENTED_EDGE('',*,*,#37782,.F.);
#51603=ORIENTED_EDGE('',*,*,#37783,.T.);
#51604=ORIENTED_EDGE('',*,*,#37784,.F.);
#51605=ORIENTED_EDGE('',*,*,#37785,.T.);
#51606=ORIENTED_EDGE('',*,*,#37786,.F.);
#51607=ORIENTED_EDGE('',*,*,#37390,.T.);
#51608=ORIENTED_EDGE('',*,*,#37784,.T.);
#51609=ORIENTED_EDGE('',*,*,#37787,.F.);
#51610=ORIENTED_EDGE('',*,*,#37788,.F.);
#51611=ORIENTED_EDGE('',*,*,#37785,.F.);
#51612=ORIENTED_EDGE('',*,*,#37783,.F.);
#51613=ORIENTED_EDGE('',*,*,#37789,.F.);
#51614=ORIENTED_EDGE('',*,*,#37790,.F.);
#51615=ORIENTED_EDGE('',*,*,#37394,.T.);
#51616=ORIENTED_EDGE('',*,*,#37393,.T.);
#51617=ORIENTED_EDGE('',*,*,#37791,.F.);
#51618=ORIENTED_EDGE('',*,*,#37397,.T.);
#51619=ORIENTED_EDGE('',*,*,#37395,.T.);
#51620=ORIENTED_EDGE('',*,*,#37790,.T.);
#51621=ORIENTED_EDGE('',*,*,#37792,.F.);
#51622=ORIENTED_EDGE('',*,*,#37793,.F.);
#51623=ORIENTED_EDGE('',*,*,#37401,.T.);
#51624=ORIENTED_EDGE('',*,*,#37400,.T.);
#51625=ORIENTED_EDGE('',*,*,#37794,.F.);
#51626=ORIENTED_EDGE('',*,*,#37404,.T.);
#51627=ORIENTED_EDGE('',*,*,#37402,.T.);
#51628=ORIENTED_EDGE('',*,*,#37793,.T.);
#51629=ORIENTED_EDGE('',*,*,#37795,.F.);
#51630=ORIENTED_EDGE('',*,*,#37796,.F.);
#51631=ORIENTED_EDGE('',*,*,#37408,.T.);
#51632=ORIENTED_EDGE('',*,*,#37407,.T.);
#51633=ORIENTED_EDGE('',*,*,#37797,.F.);
#51634=ORIENTED_EDGE('',*,*,#37411,.T.);
#51635=ORIENTED_EDGE('',*,*,#37409,.T.);
#51636=ORIENTED_EDGE('',*,*,#37796,.T.);
#51637=ORIENTED_EDGE('',*,*,#37798,.F.);
#51638=ORIENTED_EDGE('',*,*,#37799,.F.);
#51639=ORIENTED_EDGE('',*,*,#37415,.T.);
#51640=ORIENTED_EDGE('',*,*,#37414,.T.);
#51641=ORIENTED_EDGE('',*,*,#37800,.F.);
#51642=ORIENTED_EDGE('',*,*,#37418,.T.);
#51643=ORIENTED_EDGE('',*,*,#37416,.T.);
#51644=ORIENTED_EDGE('',*,*,#37799,.T.);
#51645=ORIENTED_EDGE('',*,*,#37801,.F.);
#51646=ORIENTED_EDGE('',*,*,#37802,.F.);
#51647=ORIENTED_EDGE('',*,*,#37422,.T.);
#51648=ORIENTED_EDGE('',*,*,#37421,.T.);
#51649=ORIENTED_EDGE('',*,*,#37803,.F.);
#51650=ORIENTED_EDGE('',*,*,#37425,.T.);
#51651=ORIENTED_EDGE('',*,*,#37423,.T.);
#51652=ORIENTED_EDGE('',*,*,#37802,.T.);
#51653=ORIENTED_EDGE('',*,*,#37804,.F.);
#51654=ORIENTED_EDGE('',*,*,#37805,.F.);
#51655=ORIENTED_EDGE('',*,*,#37429,.T.);
#51656=ORIENTED_EDGE('',*,*,#37428,.T.);
#51657=ORIENTED_EDGE('',*,*,#37806,.F.);
#51658=ORIENTED_EDGE('',*,*,#37432,.T.);
#51659=ORIENTED_EDGE('',*,*,#37430,.T.);
#51660=ORIENTED_EDGE('',*,*,#37805,.T.);
#51661=ORIENTED_EDGE('',*,*,#37807,.F.);
#51662=ORIENTED_EDGE('',*,*,#37808,.F.);
#51663=ORIENTED_EDGE('',*,*,#37436,.T.);
#51664=ORIENTED_EDGE('',*,*,#37435,.T.);
#51665=ORIENTED_EDGE('',*,*,#37809,.F.);
#51666=ORIENTED_EDGE('',*,*,#37439,.T.);
#51667=ORIENTED_EDGE('',*,*,#37437,.T.);
#51668=ORIENTED_EDGE('',*,*,#37808,.T.);
#51669=ORIENTED_EDGE('',*,*,#37810,.F.);
#51670=ORIENTED_EDGE('',*,*,#37811,.F.);
#51671=ORIENTED_EDGE('',*,*,#37443,.T.);
#51672=ORIENTED_EDGE('',*,*,#37442,.T.);
#51673=ORIENTED_EDGE('',*,*,#37812,.F.);
#51674=ORIENTED_EDGE('',*,*,#37446,.T.);
#51675=ORIENTED_EDGE('',*,*,#37444,.T.);
#51676=ORIENTED_EDGE('',*,*,#37811,.T.);
#51677=ORIENTED_EDGE('',*,*,#37813,.F.);
#51678=ORIENTED_EDGE('',*,*,#37814,.F.);
#51679=ORIENTED_EDGE('',*,*,#37450,.T.);
#51680=ORIENTED_EDGE('',*,*,#37449,.T.);
#51681=ORIENTED_EDGE('',*,*,#37815,.F.);
#51682=ORIENTED_EDGE('',*,*,#37453,.T.);
#51683=ORIENTED_EDGE('',*,*,#37451,.T.);
#51684=ORIENTED_EDGE('',*,*,#37814,.T.);
#51685=ORIENTED_EDGE('',*,*,#37816,.F.);
#51686=ORIENTED_EDGE('',*,*,#37817,.F.);
#51687=ORIENTED_EDGE('',*,*,#37457,.T.);
#51688=ORIENTED_EDGE('',*,*,#37456,.T.);
#51689=ORIENTED_EDGE('',*,*,#37818,.F.);
#51690=ORIENTED_EDGE('',*,*,#37460,.T.);
#51691=ORIENTED_EDGE('',*,*,#37458,.T.);
#51692=ORIENTED_EDGE('',*,*,#37817,.T.);
#51693=ORIENTED_EDGE('',*,*,#37819,.F.);
#51694=ORIENTED_EDGE('',*,*,#37820,.F.);
#51695=ORIENTED_EDGE('',*,*,#37464,.T.);
#51696=ORIENTED_EDGE('',*,*,#37463,.T.);
#51697=ORIENTED_EDGE('',*,*,#37821,.F.);
#51698=ORIENTED_EDGE('',*,*,#37467,.T.);
#51699=ORIENTED_EDGE('',*,*,#37465,.T.);
#51700=ORIENTED_EDGE('',*,*,#37820,.T.);
#51701=ORIENTED_EDGE('',*,*,#37822,.F.);
#51702=ORIENTED_EDGE('',*,*,#37823,.F.);
#51703=ORIENTED_EDGE('',*,*,#37471,.T.);
#51704=ORIENTED_EDGE('',*,*,#37470,.T.);
#51705=ORIENTED_EDGE('',*,*,#37824,.F.);
#51706=ORIENTED_EDGE('',*,*,#37474,.T.);
#51707=ORIENTED_EDGE('',*,*,#37472,.T.);
#51708=ORIENTED_EDGE('',*,*,#37823,.T.);
#51709=ORIENTED_EDGE('',*,*,#37825,.F.);
#51710=ORIENTED_EDGE('',*,*,#37826,.F.);
#51711=ORIENTED_EDGE('',*,*,#37478,.T.);
#51712=ORIENTED_EDGE('',*,*,#37477,.T.);
#51713=ORIENTED_EDGE('',*,*,#37827,.F.);
#51714=ORIENTED_EDGE('',*,*,#37481,.T.);
#51715=ORIENTED_EDGE('',*,*,#37479,.T.);
#51716=ORIENTED_EDGE('',*,*,#37826,.T.);
#51717=ORIENTED_EDGE('',*,*,#37828,.F.);
#51718=ORIENTED_EDGE('',*,*,#37829,.F.);
#51719=ORIENTED_EDGE('',*,*,#37485,.T.);
#51720=ORIENTED_EDGE('',*,*,#37484,.T.);
#51721=ORIENTED_EDGE('',*,*,#37830,.F.);
#51722=ORIENTED_EDGE('',*,*,#37488,.T.);
#51723=ORIENTED_EDGE('',*,*,#37486,.T.);
#51724=ORIENTED_EDGE('',*,*,#37829,.T.);
#51725=ORIENTED_EDGE('',*,*,#37831,.F.);
#51726=ORIENTED_EDGE('',*,*,#37832,.F.);
#51727=ORIENTED_EDGE('',*,*,#34430,.T.);
#51728=ORIENTED_EDGE('',*,*,#37490,.T.);
#51729=ORIENTED_EDGE('',*,*,#37833,.F.);
#51730=ORIENTED_EDGE('',*,*,#37491,.T.);
#51731=ORIENTED_EDGE('',*,*,#34431,.T.);
#51732=ORIENTED_EDGE('',*,*,#37832,.T.);
#51733=ORIENTED_EDGE('',*,*,#37834,.F.);
#51734=ORIENTED_EDGE('',*,*,#37835,.F.);
#51735=ORIENTED_EDGE('',*,*,#37495,.T.);
#51736=ORIENTED_EDGE('',*,*,#37494,.T.);
#51737=ORIENTED_EDGE('',*,*,#37836,.F.);
#51738=ORIENTED_EDGE('',*,*,#37498,.T.);
#51739=ORIENTED_EDGE('',*,*,#37496,.T.);
#51740=ORIENTED_EDGE('',*,*,#37835,.T.);
#51741=ORIENTED_EDGE('',*,*,#37837,.F.);
#51742=ORIENTED_EDGE('',*,*,#37838,.F.);
#51743=ORIENTED_EDGE('',*,*,#37502,.T.);
#51744=ORIENTED_EDGE('',*,*,#37501,.T.);
#51745=ORIENTED_EDGE('',*,*,#37839,.F.);
#51746=ORIENTED_EDGE('',*,*,#37505,.T.);
#51747=ORIENTED_EDGE('',*,*,#37503,.T.);
#51748=ORIENTED_EDGE('',*,*,#37838,.T.);
#51749=ORIENTED_EDGE('',*,*,#37840,.F.);
#51750=ORIENTED_EDGE('',*,*,#37841,.F.);
#51751=ORIENTED_EDGE('',*,*,#37509,.T.);
#51752=ORIENTED_EDGE('',*,*,#37508,.T.);
#51753=ORIENTED_EDGE('',*,*,#37842,.F.);
#51754=ORIENTED_EDGE('',*,*,#37512,.T.);
#51755=ORIENTED_EDGE('',*,*,#37510,.T.);
#51756=ORIENTED_EDGE('',*,*,#37841,.T.);
#51757=ORIENTED_EDGE('',*,*,#37843,.F.);
#51758=ORIENTED_EDGE('',*,*,#37844,.F.);
#51759=ORIENTED_EDGE('',*,*,#37516,.T.);
#51760=ORIENTED_EDGE('',*,*,#37515,.T.);
#51761=ORIENTED_EDGE('',*,*,#37845,.F.);
#51762=ORIENTED_EDGE('',*,*,#37519,.T.);
#51763=ORIENTED_EDGE('',*,*,#37517,.T.);
#51764=ORIENTED_EDGE('',*,*,#37844,.T.);
#51765=ORIENTED_EDGE('',*,*,#37846,.F.);
#51766=ORIENTED_EDGE('',*,*,#37847,.F.);
#51767=ORIENTED_EDGE('',*,*,#37523,.T.);
#51768=ORIENTED_EDGE('',*,*,#37522,.T.);
#51769=ORIENTED_EDGE('',*,*,#37848,.F.);
#51770=ORIENTED_EDGE('',*,*,#37526,.T.);
#51771=ORIENTED_EDGE('',*,*,#37524,.T.);
#51772=ORIENTED_EDGE('',*,*,#37847,.T.);
#51773=ORIENTED_EDGE('',*,*,#37849,.F.);
#51774=ORIENTED_EDGE('',*,*,#37850,.F.);
#51775=ORIENTED_EDGE('',*,*,#37530,.T.);
#51776=ORIENTED_EDGE('',*,*,#37529,.T.);
#51777=ORIENTED_EDGE('',*,*,#37851,.F.);
#51778=ORIENTED_EDGE('',*,*,#37533,.T.);
#51779=ORIENTED_EDGE('',*,*,#37531,.T.);
#51780=ORIENTED_EDGE('',*,*,#37850,.T.);
#51781=ORIENTED_EDGE('',*,*,#37852,.F.);
#51782=ORIENTED_EDGE('',*,*,#37853,.F.);
#51783=ORIENTED_EDGE('',*,*,#37537,.T.);
#51784=ORIENTED_EDGE('',*,*,#37536,.T.);
#51785=ORIENTED_EDGE('',*,*,#37854,.F.);
#51786=ORIENTED_EDGE('',*,*,#37540,.T.);
#51787=ORIENTED_EDGE('',*,*,#37538,.T.);
#51788=ORIENTED_EDGE('',*,*,#37853,.T.);
#51789=ORIENTED_EDGE('',*,*,#37855,.F.);
#51790=ORIENTED_EDGE('',*,*,#37856,.F.);
#51791=ORIENTED_EDGE('',*,*,#37546,.T.);
#51792=ORIENTED_EDGE('',*,*,#37543,.T.);
#51793=ORIENTED_EDGE('',*,*,#37547,.T.);
#51794=ORIENTED_EDGE('',*,*,#37856,.T.);
#51795=ORIENTED_EDGE('',*,*,#37857,.F.);
#51796=ORIENTED_EDGE('',*,*,#37545,.T.);
#51797=ORIENTED_EDGE('',*,*,#37552,.T.);
#51798=ORIENTED_EDGE('',*,*,#37548,.T.);
#51799=ORIENTED_EDGE('',*,*,#37858,.F.);
#51800=ORIENTED_EDGE('',*,*,#37859,.F.);
#51801=ORIENTED_EDGE('',*,*,#37860,.F.);
#51802=ORIENTED_EDGE('',*,*,#37554,.T.);
#51803=ORIENTED_EDGE('',*,*,#37553,.T.);
#51804=ORIENTED_EDGE('',*,*,#37859,.T.);
#51805=ORIENTED_EDGE('',*,*,#37861,.F.);
#51806=ORIENTED_EDGE('',*,*,#37862,.F.);
#51807=ORIENTED_EDGE('',*,*,#37558,.T.);
#51808=ORIENTED_EDGE('',*,*,#37557,.T.);
#51809=ORIENTED_EDGE('',*,*,#37863,.F.);
#51810=ORIENTED_EDGE('',*,*,#37561,.T.);
#51811=ORIENTED_EDGE('',*,*,#37559,.T.);
#51812=ORIENTED_EDGE('',*,*,#37862,.T.);
#51813=ORIENTED_EDGE('',*,*,#37864,.F.);
#51814=ORIENTED_EDGE('',*,*,#37865,.F.);
#51815=ORIENTED_EDGE('',*,*,#37565,.T.);
#51816=ORIENTED_EDGE('',*,*,#37564,.T.);
#51817=ORIENTED_EDGE('',*,*,#37866,.F.);
#51818=ORIENTED_EDGE('',*,*,#37568,.T.);
#51819=ORIENTED_EDGE('',*,*,#37566,.T.);
#51820=ORIENTED_EDGE('',*,*,#37865,.T.);
#51821=ORIENTED_EDGE('',*,*,#37867,.F.);
#51822=ORIENTED_EDGE('',*,*,#37868,.F.);
#51823=ORIENTED_EDGE('',*,*,#37572,.T.);
#51824=ORIENTED_EDGE('',*,*,#37571,.T.);
#51825=ORIENTED_EDGE('',*,*,#37869,.F.);
#51826=ORIENTED_EDGE('',*,*,#37575,.T.);
#51827=ORIENTED_EDGE('',*,*,#37573,.T.);
#51828=ORIENTED_EDGE('',*,*,#37868,.T.);
#51829=ORIENTED_EDGE('',*,*,#37870,.F.);
#51830=ORIENTED_EDGE('',*,*,#37871,.F.);
#51831=ORIENTED_EDGE('',*,*,#37579,.T.);
#51832=ORIENTED_EDGE('',*,*,#37578,.T.);
#51833=ORIENTED_EDGE('',*,*,#37872,.F.);
#51834=ORIENTED_EDGE('',*,*,#37582,.T.);
#51835=ORIENTED_EDGE('',*,*,#37580,.T.);
#51836=ORIENTED_EDGE('',*,*,#37871,.T.);
#51837=ORIENTED_EDGE('',*,*,#37873,.F.);
#51838=ORIENTED_EDGE('',*,*,#37874,.F.);
#51839=ORIENTED_EDGE('',*,*,#37586,.T.);
#51840=ORIENTED_EDGE('',*,*,#37585,.T.);
#51841=ORIENTED_EDGE('',*,*,#37875,.F.);
#51842=ORIENTED_EDGE('',*,*,#37589,.T.);
#51843=ORIENTED_EDGE('',*,*,#37587,.T.);
#51844=ORIENTED_EDGE('',*,*,#37874,.T.);
#51845=ORIENTED_EDGE('',*,*,#37595,.T.);
#51846=ORIENTED_EDGE('',*,*,#37590,.T.);
#51847=ORIENTED_EDGE('',*,*,#37876,.F.);
#51848=ORIENTED_EDGE('',*,*,#37877,.F.);
#51849=ORIENTED_EDGE('',*,*,#37596,.T.);
#51850=ORIENTED_EDGE('',*,*,#37877,.T.);
#51851=ORIENTED_EDGE('',*,*,#37878,.F.);
#51852=ORIENTED_EDGE('',*,*,#37594,.T.);
#51853=ORIENTED_EDGE('',*,*,#37602,.T.);
#51854=ORIENTED_EDGE('',*,*,#37597,.T.);
#51855=ORIENTED_EDGE('',*,*,#37879,.F.);
#51856=ORIENTED_EDGE('',*,*,#37880,.F.);
#51857=ORIENTED_EDGE('',*,*,#37603,.T.);
#51858=ORIENTED_EDGE('',*,*,#37880,.T.);
#51859=ORIENTED_EDGE('',*,*,#37881,.F.);
#51860=ORIENTED_EDGE('',*,*,#37601,.T.);
#51861=ORIENTED_EDGE('',*,*,#37609,.T.);
#51862=ORIENTED_EDGE('',*,*,#37604,.T.);
#51863=ORIENTED_EDGE('',*,*,#37882,.F.);
#51864=ORIENTED_EDGE('',*,*,#37883,.F.);
#51865=ORIENTED_EDGE('',*,*,#37610,.T.);
#51866=ORIENTED_EDGE('',*,*,#37883,.T.);
#51867=ORIENTED_EDGE('',*,*,#37884,.F.);
#51868=ORIENTED_EDGE('',*,*,#37608,.T.);
#51869=ORIENTED_EDGE('',*,*,#37616,.T.);
#51870=ORIENTED_EDGE('',*,*,#37611,.T.);
#51871=ORIENTED_EDGE('',*,*,#37885,.F.);
#51872=ORIENTED_EDGE('',*,*,#37886,.F.);
#51873=ORIENTED_EDGE('',*,*,#37617,.T.);
#51874=ORIENTED_EDGE('',*,*,#37886,.T.);
#51875=ORIENTED_EDGE('',*,*,#37887,.F.);
#51876=ORIENTED_EDGE('',*,*,#37615,.T.);
#51877=ORIENTED_EDGE('',*,*,#37623,.T.);
#51878=ORIENTED_EDGE('',*,*,#37618,.T.);
#51879=ORIENTED_EDGE('',*,*,#37888,.F.);
#51880=ORIENTED_EDGE('',*,*,#37889,.F.);
#51881=ORIENTED_EDGE('',*,*,#37624,.T.);
#51882=ORIENTED_EDGE('',*,*,#37889,.T.);
#51883=ORIENTED_EDGE('',*,*,#37890,.F.);
#51884=ORIENTED_EDGE('',*,*,#37622,.T.);
#51885=ORIENTED_EDGE('',*,*,#37630,.T.);
#51886=ORIENTED_EDGE('',*,*,#37625,.T.);
#51887=ORIENTED_EDGE('',*,*,#37891,.F.);
#51888=ORIENTED_EDGE('',*,*,#37892,.F.);
#51889=ORIENTED_EDGE('',*,*,#37631,.T.);
#51890=ORIENTED_EDGE('',*,*,#37892,.T.);
#51891=ORIENTED_EDGE('',*,*,#37893,.F.);
#51892=ORIENTED_EDGE('',*,*,#37629,.T.);
#51893=ORIENTED_EDGE('',*,*,#37637,.T.);
#51894=ORIENTED_EDGE('',*,*,#37632,.T.);
#51895=ORIENTED_EDGE('',*,*,#37894,.F.);
#51896=ORIENTED_EDGE('',*,*,#37895,.F.);
#51897=ORIENTED_EDGE('',*,*,#37638,.T.);
#51898=ORIENTED_EDGE('',*,*,#37895,.T.);
#51899=ORIENTED_EDGE('',*,*,#37896,.F.);
#51900=ORIENTED_EDGE('',*,*,#37636,.T.);
#51901=ORIENTED_EDGE('',*,*,#37644,.T.);
#51902=ORIENTED_EDGE('',*,*,#37639,.T.);
#51903=ORIENTED_EDGE('',*,*,#37897,.F.);
#51904=ORIENTED_EDGE('',*,*,#37898,.F.);
#51905=ORIENTED_EDGE('',*,*,#37645,.T.);
#51906=ORIENTED_EDGE('',*,*,#37898,.T.);
#51907=ORIENTED_EDGE('',*,*,#37899,.F.);
#51908=ORIENTED_EDGE('',*,*,#37643,.T.);
#51909=ORIENTED_EDGE('',*,*,#37651,.T.);
#51910=ORIENTED_EDGE('',*,*,#37646,.T.);
#51911=ORIENTED_EDGE('',*,*,#37900,.F.);
#51912=ORIENTED_EDGE('',*,*,#37901,.F.);
#51913=ORIENTED_EDGE('',*,*,#37652,.T.);
#51914=ORIENTED_EDGE('',*,*,#37901,.T.);
#51915=ORIENTED_EDGE('',*,*,#37902,.F.);
#51916=ORIENTED_EDGE('',*,*,#37650,.T.);
#51917=ORIENTED_EDGE('',*,*,#37658,.T.);
#51918=ORIENTED_EDGE('',*,*,#37653,.T.);
#51919=ORIENTED_EDGE('',*,*,#37903,.F.);
#51920=ORIENTED_EDGE('',*,*,#37904,.F.);
#51921=ORIENTED_EDGE('',*,*,#37659,.T.);
#51922=ORIENTED_EDGE('',*,*,#37904,.T.);
#51923=ORIENTED_EDGE('',*,*,#37905,.F.);
#51924=ORIENTED_EDGE('',*,*,#37657,.T.);
#51925=ORIENTED_EDGE('',*,*,#37665,.T.);
#51926=ORIENTED_EDGE('',*,*,#37660,.T.);
#51927=ORIENTED_EDGE('',*,*,#37906,.F.);
#51928=ORIENTED_EDGE('',*,*,#37907,.F.);
#51929=ORIENTED_EDGE('',*,*,#37666,.T.);
#51930=ORIENTED_EDGE('',*,*,#37907,.T.);
#51931=ORIENTED_EDGE('',*,*,#37908,.F.);
#51932=ORIENTED_EDGE('',*,*,#37664,.T.);
#51933=ORIENTED_EDGE('',*,*,#37672,.T.);
#51934=ORIENTED_EDGE('',*,*,#37667,.T.);
#51935=ORIENTED_EDGE('',*,*,#37909,.F.);
#51936=ORIENTED_EDGE('',*,*,#37910,.F.);
#51937=ORIENTED_EDGE('',*,*,#37673,.T.);
#51938=ORIENTED_EDGE('',*,*,#37910,.T.);
#51939=ORIENTED_EDGE('',*,*,#37911,.F.);
#51940=ORIENTED_EDGE('',*,*,#37671,.T.);
#51941=ORIENTED_EDGE('',*,*,#37679,.T.);
#51942=ORIENTED_EDGE('',*,*,#37674,.T.);
#51943=ORIENTED_EDGE('',*,*,#37912,.F.);
#51944=ORIENTED_EDGE('',*,*,#37913,.F.);
#51945=ORIENTED_EDGE('',*,*,#37680,.T.);
#51946=ORIENTED_EDGE('',*,*,#37913,.T.);
#51947=ORIENTED_EDGE('',*,*,#37914,.F.);
#51948=ORIENTED_EDGE('',*,*,#37678,.T.);
#51949=ORIENTED_EDGE('',*,*,#37686,.T.);
#51950=ORIENTED_EDGE('',*,*,#37681,.T.);
#51951=ORIENTED_EDGE('',*,*,#37915,.F.);
#51952=ORIENTED_EDGE('',*,*,#37916,.F.);
#51953=ORIENTED_EDGE('',*,*,#37687,.T.);
#51954=ORIENTED_EDGE('',*,*,#37916,.T.);
#51955=ORIENTED_EDGE('',*,*,#37917,.F.);
#51956=ORIENTED_EDGE('',*,*,#37685,.T.);
#51957=ORIENTED_EDGE('',*,*,#37693,.T.);
#51958=ORIENTED_EDGE('',*,*,#37688,.T.);
#51959=ORIENTED_EDGE('',*,*,#37918,.F.);
#51960=ORIENTED_EDGE('',*,*,#37919,.F.);
#51961=ORIENTED_EDGE('',*,*,#37694,.T.);
#51962=ORIENTED_EDGE('',*,*,#37919,.T.);
#51963=ORIENTED_EDGE('',*,*,#37920,.F.);
#51964=ORIENTED_EDGE('',*,*,#37692,.T.);
#51965=ORIENTED_EDGE('',*,*,#37700,.T.);
#51966=ORIENTED_EDGE('',*,*,#37695,.T.);
#51967=ORIENTED_EDGE('',*,*,#37921,.F.);
#51968=ORIENTED_EDGE('',*,*,#37922,.F.);
#51969=ORIENTED_EDGE('',*,*,#37701,.T.);
#51970=ORIENTED_EDGE('',*,*,#37922,.T.);
#51971=ORIENTED_EDGE('',*,*,#37923,.F.);
#51972=ORIENTED_EDGE('',*,*,#37699,.T.);
#51973=ORIENTED_EDGE('',*,*,#37707,.T.);
#51974=ORIENTED_EDGE('',*,*,#37702,.T.);
#51975=ORIENTED_EDGE('',*,*,#37924,.F.);
#51976=ORIENTED_EDGE('',*,*,#37925,.F.);
#51977=ORIENTED_EDGE('',*,*,#37708,.T.);
#51978=ORIENTED_EDGE('',*,*,#37925,.T.);
#51979=ORIENTED_EDGE('',*,*,#37926,.F.);
#51980=ORIENTED_EDGE('',*,*,#37706,.T.);
#51981=ORIENTED_EDGE('',*,*,#37714,.T.);
#51982=ORIENTED_EDGE('',*,*,#37709,.T.);
#51983=ORIENTED_EDGE('',*,*,#37927,.F.);
#51984=ORIENTED_EDGE('',*,*,#37928,.F.);
#51985=ORIENTED_EDGE('',*,*,#37715,.T.);
#51986=ORIENTED_EDGE('',*,*,#37928,.T.);
#51987=ORIENTED_EDGE('',*,*,#37929,.F.);
#51988=ORIENTED_EDGE('',*,*,#37713,.T.);
#51989=ORIENTED_EDGE('',*,*,#37721,.T.);
#51990=ORIENTED_EDGE('',*,*,#37716,.T.);
#51991=ORIENTED_EDGE('',*,*,#37930,.F.);
#51992=ORIENTED_EDGE('',*,*,#37931,.F.);
#51993=ORIENTED_EDGE('',*,*,#37722,.T.);
#51994=ORIENTED_EDGE('',*,*,#37931,.T.);
#51995=ORIENTED_EDGE('',*,*,#37932,.F.);
#51996=ORIENTED_EDGE('',*,*,#37720,.T.);
#51997=ORIENTED_EDGE('',*,*,#37728,.T.);
#51998=ORIENTED_EDGE('',*,*,#37723,.T.);
#51999=ORIENTED_EDGE('',*,*,#37933,.F.);
#52000=ORIENTED_EDGE('',*,*,#37934,.F.);
#52001=ORIENTED_EDGE('',*,*,#37729,.T.);
#52002=ORIENTED_EDGE('',*,*,#37934,.T.);
#52003=ORIENTED_EDGE('',*,*,#37935,.F.);
#52004=ORIENTED_EDGE('',*,*,#37727,.T.);
#52005=ORIENTED_EDGE('',*,*,#37735,.T.);
#52006=ORIENTED_EDGE('',*,*,#37730,.T.);
#52007=ORIENTED_EDGE('',*,*,#37936,.F.);
#52008=ORIENTED_EDGE('',*,*,#37937,.F.);
#52009=ORIENTED_EDGE('',*,*,#37736,.T.);
#52010=ORIENTED_EDGE('',*,*,#37937,.T.);
#52011=ORIENTED_EDGE('',*,*,#37938,.F.);
#52012=ORIENTED_EDGE('',*,*,#37734,.T.);
#52013=ORIENTED_EDGE('',*,*,#34425,.T.);
#52014=ORIENTED_EDGE('',*,*,#37737,.T.);
#52015=ORIENTED_EDGE('',*,*,#37939,.F.);
#52016=ORIENTED_EDGE('',*,*,#37940,.F.);
#52017=ORIENTED_EDGE('',*,*,#34426,.T.);
#52018=ORIENTED_EDGE('',*,*,#37940,.T.);
#52019=ORIENTED_EDGE('',*,*,#37941,.F.);
#52020=ORIENTED_EDGE('',*,*,#37739,.T.);
#52021=ORIENTED_EDGE('',*,*,#37745,.T.);
#52022=ORIENTED_EDGE('',*,*,#37740,.T.);
#52023=ORIENTED_EDGE('',*,*,#37942,.F.);
#52024=ORIENTED_EDGE('',*,*,#37943,.F.);
#52025=ORIENTED_EDGE('',*,*,#37746,.T.);
#52026=ORIENTED_EDGE('',*,*,#37943,.T.);
#52027=ORIENTED_EDGE('',*,*,#37944,.F.);
#52028=ORIENTED_EDGE('',*,*,#37744,.T.);
#52029=ORIENTED_EDGE('',*,*,#37752,.T.);
#52030=ORIENTED_EDGE('',*,*,#37747,.T.);
#52031=ORIENTED_EDGE('',*,*,#37945,.F.);
#52032=ORIENTED_EDGE('',*,*,#37946,.F.);
#52033=ORIENTED_EDGE('',*,*,#37753,.T.);
#52034=ORIENTED_EDGE('',*,*,#37946,.T.);
#52035=ORIENTED_EDGE('',*,*,#37947,.F.);
#52036=ORIENTED_EDGE('',*,*,#37751,.T.);
#52037=ORIENTED_EDGE('',*,*,#37759,.T.);
#52038=ORIENTED_EDGE('',*,*,#37754,.T.);
#52039=ORIENTED_EDGE('',*,*,#37948,.F.);
#52040=ORIENTED_EDGE('',*,*,#37949,.F.);
#52041=ORIENTED_EDGE('',*,*,#37760,.T.);
#52042=ORIENTED_EDGE('',*,*,#37949,.T.);
#52043=ORIENTED_EDGE('',*,*,#37950,.F.);
#52044=ORIENTED_EDGE('',*,*,#37758,.T.);
#52045=ORIENTED_EDGE('',*,*,#37766,.T.);
#52046=ORIENTED_EDGE('',*,*,#37761,.T.);
#52047=ORIENTED_EDGE('',*,*,#37951,.F.);
#52048=ORIENTED_EDGE('',*,*,#37952,.F.);
#52049=ORIENTED_EDGE('',*,*,#37767,.T.);
#52050=ORIENTED_EDGE('',*,*,#37952,.T.);
#52051=ORIENTED_EDGE('',*,*,#37953,.F.);
#52052=ORIENTED_EDGE('',*,*,#37765,.T.);
#52053=ORIENTED_EDGE('',*,*,#37773,.T.);
#52054=ORIENTED_EDGE('',*,*,#37768,.T.);
#52055=ORIENTED_EDGE('',*,*,#37954,.F.);
#52056=ORIENTED_EDGE('',*,*,#37955,.F.);
#52057=ORIENTED_EDGE('',*,*,#37774,.T.);
#52058=ORIENTED_EDGE('',*,*,#37955,.T.);
#52059=ORIENTED_EDGE('',*,*,#37956,.F.);
#52060=ORIENTED_EDGE('',*,*,#37772,.T.);
#52061=ORIENTED_EDGE('',*,*,#37780,.T.);
#52062=ORIENTED_EDGE('',*,*,#37775,.T.);
#52063=ORIENTED_EDGE('',*,*,#37957,.F.);
#52064=ORIENTED_EDGE('',*,*,#37958,.F.);
#52065=ORIENTED_EDGE('',*,*,#37781,.T.);
#52066=ORIENTED_EDGE('',*,*,#37958,.T.);
#52067=ORIENTED_EDGE('',*,*,#37959,.F.);
#52068=ORIENTED_EDGE('',*,*,#37779,.T.);
#52069=ORIENTED_EDGE('',*,*,#37960,.F.);
#52070=ORIENTED_EDGE('',*,*,#37961,.F.);
#52071=ORIENTED_EDGE('',*,*,#37787,.T.);
#52072=ORIENTED_EDGE('',*,*,#37782,.T.);
#52073=ORIENTED_EDGE('',*,*,#37788,.T.);
#52074=ORIENTED_EDGE('',*,*,#37961,.T.);
#52075=ORIENTED_EDGE('',*,*,#37962,.F.);
#52076=ORIENTED_EDGE('',*,*,#37786,.T.);
#52077=ORIENTED_EDGE('',*,*,#37963,.T.);
#52078=ORIENTED_EDGE('',*,*,#37964,.F.);
#52079=ORIENTED_EDGE('',*,*,#37789,.T.);
#52080=ORIENTED_EDGE('',*,*,#37965,.F.);
#52081=ORIENTED_EDGE('',*,*,#37966,.T.);
#52082=ORIENTED_EDGE('',*,*,#37967,.F.);
#52083=ORIENTED_EDGE('',*,*,#37791,.T.);
#52084=ORIENTED_EDGE('',*,*,#37968,.F.);
#52085=ORIENTED_EDGE('',*,*,#37969,.F.);
#52086=ORIENTED_EDGE('',*,*,#37970,.F.);
#52087=ORIENTED_EDGE('',*,*,#37971,.F.);
#52088=ORIENTED_EDGE('',*,*,#37966,.F.);
#52089=ORIENTED_EDGE('',*,*,#37971,.T.);
#52090=ORIENTED_EDGE('',*,*,#37972,.F.);
#52091=ORIENTED_EDGE('',*,*,#37792,.T.);
#52092=ORIENTED_EDGE('',*,*,#37967,.T.);
#52093=ORIENTED_EDGE('',*,*,#37973,.T.);
#52094=ORIENTED_EDGE('',*,*,#37974,.F.);
#52095=ORIENTED_EDGE('',*,*,#37794,.T.);
#52096=ORIENTED_EDGE('',*,*,#37975,.F.);
#52097=ORIENTED_EDGE('',*,*,#37976,.F.);
#52098=ORIENTED_EDGE('',*,*,#37977,.F.);
#52099=ORIENTED_EDGE('',*,*,#37978,.F.);
#52100=ORIENTED_EDGE('',*,*,#37973,.F.);
#52101=ORIENTED_EDGE('',*,*,#37978,.T.);
#52102=ORIENTED_EDGE('',*,*,#37979,.F.);
#52103=ORIENTED_EDGE('',*,*,#37795,.T.);
#52104=ORIENTED_EDGE('',*,*,#37974,.T.);
#52105=ORIENTED_EDGE('',*,*,#37980,.T.);
#52106=ORIENTED_EDGE('',*,*,#37981,.F.);
#52107=ORIENTED_EDGE('',*,*,#37797,.T.);
#52108=ORIENTED_EDGE('',*,*,#37982,.F.);
#52109=ORIENTED_EDGE('',*,*,#37983,.F.);
#52110=ORIENTED_EDGE('',*,*,#37984,.F.);
#52111=ORIENTED_EDGE('',*,*,#37985,.F.);
#52112=ORIENTED_EDGE('',*,*,#37980,.F.);
#52113=ORIENTED_EDGE('',*,*,#37985,.T.);
#52114=ORIENTED_EDGE('',*,*,#37986,.F.);
#52115=ORIENTED_EDGE('',*,*,#37798,.T.);
#52116=ORIENTED_EDGE('',*,*,#37981,.T.);
#52117=ORIENTED_EDGE('',*,*,#37987,.T.);
#52118=ORIENTED_EDGE('',*,*,#37988,.F.);
#52119=ORIENTED_EDGE('',*,*,#37800,.T.);
#52120=ORIENTED_EDGE('',*,*,#37989,.F.);
#52121=ORIENTED_EDGE('',*,*,#37990,.F.);
#52122=ORIENTED_EDGE('',*,*,#37991,.F.);
#52123=ORIENTED_EDGE('',*,*,#37992,.F.);
#52124=ORIENTED_EDGE('',*,*,#37987,.F.);
#52125=ORIENTED_EDGE('',*,*,#37992,.T.);
#52126=ORIENTED_EDGE('',*,*,#37993,.F.);
#52127=ORIENTED_EDGE('',*,*,#37801,.T.);
#52128=ORIENTED_EDGE('',*,*,#37988,.T.);
#52129=ORIENTED_EDGE('',*,*,#37994,.T.);
#52130=ORIENTED_EDGE('',*,*,#37995,.F.);
#52131=ORIENTED_EDGE('',*,*,#37803,.T.);
#52132=ORIENTED_EDGE('',*,*,#37996,.F.);
#52133=ORIENTED_EDGE('',*,*,#37997,.F.);
#52134=ORIENTED_EDGE('',*,*,#37998,.F.);
#52135=ORIENTED_EDGE('',*,*,#37999,.F.);
#52136=ORIENTED_EDGE('',*,*,#37994,.F.);
#52137=ORIENTED_EDGE('',*,*,#37999,.T.);
#52138=ORIENTED_EDGE('',*,*,#38000,.F.);
#52139=ORIENTED_EDGE('',*,*,#37804,.T.);
#52140=ORIENTED_EDGE('',*,*,#37995,.T.);
#52141=ORIENTED_EDGE('',*,*,#38001,.T.);
#52142=ORIENTED_EDGE('',*,*,#38002,.F.);
#52143=ORIENTED_EDGE('',*,*,#37806,.T.);
#52144=ORIENTED_EDGE('',*,*,#38003,.F.);
#52145=ORIENTED_EDGE('',*,*,#38004,.F.);
#52146=ORIENTED_EDGE('',*,*,#38005,.F.);
#52147=ORIENTED_EDGE('',*,*,#38006,.F.);
#52148=ORIENTED_EDGE('',*,*,#38001,.F.);
#52149=ORIENTED_EDGE('',*,*,#38006,.T.);
#52150=ORIENTED_EDGE('',*,*,#38007,.F.);
#52151=ORIENTED_EDGE('',*,*,#37807,.T.);
#52152=ORIENTED_EDGE('',*,*,#38002,.T.);
#52153=ORIENTED_EDGE('',*,*,#34422,.T.);
#52154=ORIENTED_EDGE('',*,*,#38008,.F.);
#52155=ORIENTED_EDGE('',*,*,#37809,.T.);
#52156=ORIENTED_EDGE('',*,*,#38009,.F.);
#52157=ORIENTED_EDGE('',*,*,#34421,.T.);
#52158=ORIENTED_EDGE('',*,*,#38010,.F.);
#52159=ORIENTED_EDGE('',*,*,#37810,.T.);
#52160=ORIENTED_EDGE('',*,*,#38008,.T.);
#52161=ORIENTED_EDGE('',*,*,#38011,.T.);
#52162=ORIENTED_EDGE('',*,*,#38012,.F.);
#52163=ORIENTED_EDGE('',*,*,#37812,.T.);
#52164=ORIENTED_EDGE('',*,*,#38013,.F.);
#52165=ORIENTED_EDGE('',*,*,#38014,.F.);
#52166=ORIENTED_EDGE('',*,*,#38015,.F.);
#52167=ORIENTED_EDGE('',*,*,#38016,.F.);
#52168=ORIENTED_EDGE('',*,*,#38011,.F.);
#52169=ORIENTED_EDGE('',*,*,#38016,.T.);
#52170=ORIENTED_EDGE('',*,*,#38017,.F.);
#52171=ORIENTED_EDGE('',*,*,#37813,.T.);
#52172=ORIENTED_EDGE('',*,*,#38012,.T.);
#52173=ORIENTED_EDGE('',*,*,#38018,.T.);
#52174=ORIENTED_EDGE('',*,*,#38019,.F.);
#52175=ORIENTED_EDGE('',*,*,#37815,.T.);
#52176=ORIENTED_EDGE('',*,*,#38020,.F.);
#52177=ORIENTED_EDGE('',*,*,#38021,.F.);
#52178=ORIENTED_EDGE('',*,*,#38022,.F.);
#52179=ORIENTED_EDGE('',*,*,#38023,.F.);
#52180=ORIENTED_EDGE('',*,*,#38018,.F.);
#52181=ORIENTED_EDGE('',*,*,#38023,.T.);
#52182=ORIENTED_EDGE('',*,*,#38024,.F.);
#52183=ORIENTED_EDGE('',*,*,#37816,.T.);
#52184=ORIENTED_EDGE('',*,*,#38019,.T.);
#52185=ORIENTED_EDGE('',*,*,#38025,.T.);
#52186=ORIENTED_EDGE('',*,*,#38026,.F.);
#52187=ORIENTED_EDGE('',*,*,#37818,.T.);
#52188=ORIENTED_EDGE('',*,*,#38027,.F.);
#52189=ORIENTED_EDGE('',*,*,#38028,.F.);
#52190=ORIENTED_EDGE('',*,*,#38029,.F.);
#52191=ORIENTED_EDGE('',*,*,#38030,.F.);
#52192=ORIENTED_EDGE('',*,*,#38025,.F.);
#52193=ORIENTED_EDGE('',*,*,#38030,.T.);
#52194=ORIENTED_EDGE('',*,*,#38031,.F.);
#52195=ORIENTED_EDGE('',*,*,#37819,.T.);
#52196=ORIENTED_EDGE('',*,*,#38026,.T.);
#52197=ORIENTED_EDGE('',*,*,#38032,.T.);
#52198=ORIENTED_EDGE('',*,*,#38033,.F.);
#52199=ORIENTED_EDGE('',*,*,#37821,.T.);
#52200=ORIENTED_EDGE('',*,*,#38034,.F.);
#52201=ORIENTED_EDGE('',*,*,#38035,.F.);
#52202=ORIENTED_EDGE('',*,*,#38036,.F.);
#52203=ORIENTED_EDGE('',*,*,#38037,.F.);
#52204=ORIENTED_EDGE('',*,*,#38032,.F.);
#52205=ORIENTED_EDGE('',*,*,#38037,.T.);
#52206=ORIENTED_EDGE('',*,*,#38038,.F.);
#52207=ORIENTED_EDGE('',*,*,#37822,.T.);
#52208=ORIENTED_EDGE('',*,*,#38033,.T.);
#52209=ORIENTED_EDGE('',*,*,#38039,.T.);
#52210=ORIENTED_EDGE('',*,*,#38040,.F.);
#52211=ORIENTED_EDGE('',*,*,#37824,.T.);
#52212=ORIENTED_EDGE('',*,*,#38041,.F.);
#52213=ORIENTED_EDGE('',*,*,#38042,.F.);
#52214=ORIENTED_EDGE('',*,*,#38043,.F.);
#52215=ORIENTED_EDGE('',*,*,#38044,.F.);
#52216=ORIENTED_EDGE('',*,*,#38039,.F.);
#52217=ORIENTED_EDGE('',*,*,#38044,.T.);
#52218=ORIENTED_EDGE('',*,*,#38045,.F.);
#52219=ORIENTED_EDGE('',*,*,#37825,.T.);
#52220=ORIENTED_EDGE('',*,*,#38040,.T.);
#52221=ORIENTED_EDGE('',*,*,#38046,.T.);
#52222=ORIENTED_EDGE('',*,*,#38047,.F.);
#52223=ORIENTED_EDGE('',*,*,#37827,.T.);
#52224=ORIENTED_EDGE('',*,*,#38048,.F.);
#52225=ORIENTED_EDGE('',*,*,#38049,.F.);
#52226=ORIENTED_EDGE('',*,*,#38050,.F.);
#52227=ORIENTED_EDGE('',*,*,#38051,.F.);
#52228=ORIENTED_EDGE('',*,*,#38046,.F.);
#52229=ORIENTED_EDGE('',*,*,#38051,.T.);
#52230=ORIENTED_EDGE('',*,*,#38052,.F.);
#52231=ORIENTED_EDGE('',*,*,#37828,.T.);
#52232=ORIENTED_EDGE('',*,*,#38047,.T.);
#52233=ORIENTED_EDGE('',*,*,#38053,.T.);
#52234=ORIENTED_EDGE('',*,*,#38054,.F.);
#52235=ORIENTED_EDGE('',*,*,#37830,.T.);
#52236=ORIENTED_EDGE('',*,*,#38055,.F.);
#52237=ORIENTED_EDGE('',*,*,#38056,.F.);
#52238=ORIENTED_EDGE('',*,*,#38057,.F.);
#52239=ORIENTED_EDGE('',*,*,#38058,.F.);
#52240=ORIENTED_EDGE('',*,*,#38053,.F.);
#52241=ORIENTED_EDGE('',*,*,#38058,.T.);
#52242=ORIENTED_EDGE('',*,*,#38059,.F.);
#52243=ORIENTED_EDGE('',*,*,#37831,.T.);
#52244=ORIENTED_EDGE('',*,*,#38054,.T.);
#52245=ORIENTED_EDGE('',*,*,#38060,.T.);
#52246=ORIENTED_EDGE('',*,*,#38061,.F.);
#52247=ORIENTED_EDGE('',*,*,#37833,.T.);
#52248=ORIENTED_EDGE('',*,*,#38062,.F.);
#52249=ORIENTED_EDGE('',*,*,#38063,.F.);
#52250=ORIENTED_EDGE('',*,*,#38064,.F.);
#52251=ORIENTED_EDGE('',*,*,#38065,.F.);
#52252=ORIENTED_EDGE('',*,*,#38060,.F.);
#52253=ORIENTED_EDGE('',*,*,#38065,.T.);
#52254=ORIENTED_EDGE('',*,*,#38066,.F.);
#52255=ORIENTED_EDGE('',*,*,#37834,.T.);
#52256=ORIENTED_EDGE('',*,*,#38061,.T.);
#52257=ORIENTED_EDGE('',*,*,#38067,.T.);
#52258=ORIENTED_EDGE('',*,*,#38068,.F.);
#52259=ORIENTED_EDGE('',*,*,#37836,.T.);
#52260=ORIENTED_EDGE('',*,*,#38069,.F.);
#52261=ORIENTED_EDGE('',*,*,#38070,.F.);
#52262=ORIENTED_EDGE('',*,*,#38071,.F.);
#52263=ORIENTED_EDGE('',*,*,#38072,.F.);
#52264=ORIENTED_EDGE('',*,*,#38067,.F.);
#52265=ORIENTED_EDGE('',*,*,#38072,.T.);
#52266=ORIENTED_EDGE('',*,*,#38073,.F.);
#52267=ORIENTED_EDGE('',*,*,#37837,.T.);
#52268=ORIENTED_EDGE('',*,*,#38068,.T.);
#52269=ORIENTED_EDGE('',*,*,#38074,.T.);
#52270=ORIENTED_EDGE('',*,*,#38075,.F.);
#52271=ORIENTED_EDGE('',*,*,#37839,.T.);
#52272=ORIENTED_EDGE('',*,*,#38076,.F.);
#52273=ORIENTED_EDGE('',*,*,#38077,.F.);
#52274=ORIENTED_EDGE('',*,*,#38078,.F.);
#52275=ORIENTED_EDGE('',*,*,#38079,.F.);
#52276=ORIENTED_EDGE('',*,*,#38074,.F.);
#52277=ORIENTED_EDGE('',*,*,#38079,.T.);
#52278=ORIENTED_EDGE('',*,*,#38080,.F.);
#52279=ORIENTED_EDGE('',*,*,#37840,.T.);
#52280=ORIENTED_EDGE('',*,*,#38075,.T.);
#52281=ORIENTED_EDGE('',*,*,#38081,.T.);
#52282=ORIENTED_EDGE('',*,*,#38082,.F.);
#52283=ORIENTED_EDGE('',*,*,#37842,.T.);
#52284=ORIENTED_EDGE('',*,*,#38083,.F.);
#52285=ORIENTED_EDGE('',*,*,#38084,.F.);
#52286=ORIENTED_EDGE('',*,*,#38085,.F.);
#52287=ORIENTED_EDGE('',*,*,#38086,.F.);
#52288=ORIENTED_EDGE('',*,*,#38081,.F.);
#52289=ORIENTED_EDGE('',*,*,#38086,.T.);
#52290=ORIENTED_EDGE('',*,*,#38087,.F.);
#52291=ORIENTED_EDGE('',*,*,#37843,.T.);
#52292=ORIENTED_EDGE('',*,*,#38082,.T.);
#52293=ORIENTED_EDGE('',*,*,#38088,.T.);
#52294=ORIENTED_EDGE('',*,*,#38089,.F.);
#52295=ORIENTED_EDGE('',*,*,#37845,.T.);
#52296=ORIENTED_EDGE('',*,*,#38090,.F.);
#52297=ORIENTED_EDGE('',*,*,#38091,.F.);
#52298=ORIENTED_EDGE('',*,*,#38092,.F.);
#52299=ORIENTED_EDGE('',*,*,#38093,.F.);
#52300=ORIENTED_EDGE('',*,*,#38088,.F.);
#52301=ORIENTED_EDGE('',*,*,#38093,.T.);
#52302=ORIENTED_EDGE('',*,*,#38094,.F.);
#52303=ORIENTED_EDGE('',*,*,#37846,.T.);
#52304=ORIENTED_EDGE('',*,*,#38089,.T.);
#52305=ORIENTED_EDGE('',*,*,#38095,.T.);
#52306=ORIENTED_EDGE('',*,*,#38096,.F.);
#52307=ORIENTED_EDGE('',*,*,#37848,.T.);
#52308=ORIENTED_EDGE('',*,*,#38097,.F.);
#52309=ORIENTED_EDGE('',*,*,#38098,.F.);
#52310=ORIENTED_EDGE('',*,*,#38099,.F.);
#52311=ORIENTED_EDGE('',*,*,#38100,.F.);
#52312=ORIENTED_EDGE('',*,*,#38095,.F.);
#52313=ORIENTED_EDGE('',*,*,#38100,.T.);
#52314=ORIENTED_EDGE('',*,*,#38101,.F.);
#52315=ORIENTED_EDGE('',*,*,#37849,.T.);
#52316=ORIENTED_EDGE('',*,*,#38096,.T.);
#52317=ORIENTED_EDGE('',*,*,#38102,.T.);
#52318=ORIENTED_EDGE('',*,*,#38103,.F.);
#52319=ORIENTED_EDGE('',*,*,#37851,.T.);
#52320=ORIENTED_EDGE('',*,*,#38104,.F.);
#52321=ORIENTED_EDGE('',*,*,#38105,.F.);
#52322=ORIENTED_EDGE('',*,*,#38106,.F.);
#52323=ORIENTED_EDGE('',*,*,#38107,.F.);
#52324=ORIENTED_EDGE('',*,*,#38102,.F.);
#52325=ORIENTED_EDGE('',*,*,#38107,.T.);
#52326=ORIENTED_EDGE('',*,*,#38108,.F.);
#52327=ORIENTED_EDGE('',*,*,#37852,.T.);
#52328=ORIENTED_EDGE('',*,*,#38103,.T.);
#52329=ORIENTED_EDGE('',*,*,#38109,.T.);
#52330=ORIENTED_EDGE('',*,*,#38110,.F.);
#52331=ORIENTED_EDGE('',*,*,#37854,.T.);
#52332=ORIENTED_EDGE('',*,*,#38111,.F.);
#52333=ORIENTED_EDGE('',*,*,#38112,.T.);
#52334=ORIENTED_EDGE('',*,*,#38113,.F.);
#52335=ORIENTED_EDGE('',*,*,#37855,.T.);
#52336=ORIENTED_EDGE('',*,*,#38110,.T.);
#52337=ORIENTED_EDGE('',*,*,#38114,.F.);
#52338=ORIENTED_EDGE('',*,*,#38115,.F.);
#52339=ORIENTED_EDGE('',*,*,#38112,.F.);
#52340=ORIENTED_EDGE('',*,*,#38109,.F.);
#52341=ORIENTED_EDGE('',*,*,#37857,.T.);
#52342=ORIENTED_EDGE('',*,*,#38116,.F.);
#52343=ORIENTED_EDGE('',*,*,#38117,.T.);
#52344=ORIENTED_EDGE('',*,*,#38118,.F.);
#52345=ORIENTED_EDGE('',*,*,#38119,.F.);
#52346=ORIENTED_EDGE('',*,*,#38117,.F.);
#52347=ORIENTED_EDGE('',*,*,#38120,.F.);
#52348=ORIENTED_EDGE('',*,*,#38121,.F.);
#52349=ORIENTED_EDGE('',*,*,#37858,.T.);
#52350=ORIENTED_EDGE('',*,*,#38118,.T.);
#52351=ORIENTED_EDGE('',*,*,#38119,.T.);
#52352=ORIENTED_EDGE('',*,*,#38122,.F.);
#52353=ORIENTED_EDGE('',*,*,#38123,.T.);
#52354=ORIENTED_EDGE('',*,*,#38124,.F.);
#52355=ORIENTED_EDGE('',*,*,#37860,.T.);
#52356=ORIENTED_EDGE('',*,*,#38125,.F.);
#52357=ORIENTED_EDGE('',*,*,#38126,.F.);
#52358=ORIENTED_EDGE('',*,*,#38127,.F.);
#52359=ORIENTED_EDGE('',*,*,#38128,.F.);
#52360=ORIENTED_EDGE('',*,*,#38123,.F.);
#52361=ORIENTED_EDGE('',*,*,#38128,.T.);
#52362=ORIENTED_EDGE('',*,*,#38129,.F.);
#52363=ORIENTED_EDGE('',*,*,#37861,.T.);
#52364=ORIENTED_EDGE('',*,*,#38124,.T.);
#52365=ORIENTED_EDGE('',*,*,#38130,.T.);
#52366=ORIENTED_EDGE('',*,*,#38131,.F.);
#52367=ORIENTED_EDGE('',*,*,#37863,.T.);
#52368=ORIENTED_EDGE('',*,*,#38132,.F.);
#52369=ORIENTED_EDGE('',*,*,#38133,.F.);
#52370=ORIENTED_EDGE('',*,*,#38134,.F.);
#52371=ORIENTED_EDGE('',*,*,#38135,.F.);
#52372=ORIENTED_EDGE('',*,*,#38130,.F.);
#52373=ORIENTED_EDGE('',*,*,#38135,.T.);
#52374=ORIENTED_EDGE('',*,*,#38136,.F.);
#52375=ORIENTED_EDGE('',*,*,#37864,.T.);
#52376=ORIENTED_EDGE('',*,*,#38131,.T.);
#52377=ORIENTED_EDGE('',*,*,#38137,.T.);
#52378=ORIENTED_EDGE('',*,*,#38138,.F.);
#52379=ORIENTED_EDGE('',*,*,#37866,.T.);
#52380=ORIENTED_EDGE('',*,*,#38139,.F.);
#52381=ORIENTED_EDGE('',*,*,#38140,.F.);
#52382=ORIENTED_EDGE('',*,*,#38141,.F.);
#52383=ORIENTED_EDGE('',*,*,#38142,.F.);
#52384=ORIENTED_EDGE('',*,*,#38137,.F.);
#52385=ORIENTED_EDGE('',*,*,#38142,.T.);
#52386=ORIENTED_EDGE('',*,*,#38143,.F.);
#52387=ORIENTED_EDGE('',*,*,#37867,.T.);
#52388=ORIENTED_EDGE('',*,*,#38138,.T.);
#52389=ORIENTED_EDGE('',*,*,#38144,.T.);
#52390=ORIENTED_EDGE('',*,*,#38145,.F.);
#52391=ORIENTED_EDGE('',*,*,#37869,.T.);
#52392=ORIENTED_EDGE('',*,*,#38146,.F.);
#52393=ORIENTED_EDGE('',*,*,#38147,.F.);
#52394=ORIENTED_EDGE('',*,*,#38148,.F.);
#52395=ORIENTED_EDGE('',*,*,#38149,.F.);
#52396=ORIENTED_EDGE('',*,*,#38144,.F.);
#52397=ORIENTED_EDGE('',*,*,#38149,.T.);
#52398=ORIENTED_EDGE('',*,*,#38150,.F.);
#52399=ORIENTED_EDGE('',*,*,#37870,.T.);
#52400=ORIENTED_EDGE('',*,*,#38145,.T.);
#52401=ORIENTED_EDGE('',*,*,#38151,.T.);
#52402=ORIENTED_EDGE('',*,*,#38152,.F.);
#52403=ORIENTED_EDGE('',*,*,#37872,.T.);
#52404=ORIENTED_EDGE('',*,*,#38153,.F.);
#52405=ORIENTED_EDGE('',*,*,#38154,.F.);
#52406=ORIENTED_EDGE('',*,*,#38155,.F.);
#52407=ORIENTED_EDGE('',*,*,#38156,.F.);
#52408=ORIENTED_EDGE('',*,*,#38151,.F.);
#52409=ORIENTED_EDGE('',*,*,#38156,.T.);
#52410=ORIENTED_EDGE('',*,*,#38157,.F.);
#52411=ORIENTED_EDGE('',*,*,#37873,.T.);
#52412=ORIENTED_EDGE('',*,*,#38152,.T.);
#52413=ORIENTED_EDGE('',*,*,#38158,.F.);
#52414=ORIENTED_EDGE('',*,*,#38159,.F.);
#52415=ORIENTED_EDGE('',*,*,#37963,.F.);
#52416=ORIENTED_EDGE('',*,*,#38160,.F.);
#52417=ORIENTED_EDGE('',*,*,#38160,.T.);
#52418=ORIENTED_EDGE('',*,*,#37965,.T.);
#52419=ORIENTED_EDGE('',*,*,#37875,.T.);
#52420=ORIENTED_EDGE('',*,*,#38161,.F.);
#52421=ORIENTED_EDGE('',*,*,#37876,.T.);
#52422=ORIENTED_EDGE('',*,*,#38162,.F.);
#52423=ORIENTED_EDGE('',*,*,#38163,.T.);
#52424=ORIENTED_EDGE('',*,*,#38164,.F.);
#52425=ORIENTED_EDGE('',*,*,#37878,.T.);
#52426=ORIENTED_EDGE('',*,*,#38165,.F.);
#52427=ORIENTED_EDGE('',*,*,#38166,.T.);
#52428=ORIENTED_EDGE('',*,*,#38167,.F.);
#52429=ORIENTED_EDGE('',*,*,#37879,.T.);
#52430=ORIENTED_EDGE('',*,*,#38167,.T.);
#52431=ORIENTED_EDGE('',*,*,#38168,.T.);
#52432=ORIENTED_EDGE('',*,*,#38169,.F.);
#52433=ORIENTED_EDGE('',*,*,#38168,.F.);
#52434=ORIENTED_EDGE('',*,*,#38166,.F.);
#52435=ORIENTED_EDGE('',*,*,#38170,.F.);
#52436=ORIENTED_EDGE('',*,*,#38171,.F.);
#52437=ORIENTED_EDGE('',*,*,#37881,.T.);
#52438=ORIENTED_EDGE('',*,*,#38172,.F.);
#52439=ORIENTED_EDGE('',*,*,#38173,.T.);
#52440=ORIENTED_EDGE('',*,*,#38174,.F.);
#52441=ORIENTED_EDGE('',*,*,#37882,.T.);
#52442=ORIENTED_EDGE('',*,*,#38174,.T.);
#52443=ORIENTED_EDGE('',*,*,#38175,.T.);
#52444=ORIENTED_EDGE('',*,*,#38176,.F.);
#52445=ORIENTED_EDGE('',*,*,#38175,.F.);
#52446=ORIENTED_EDGE('',*,*,#38173,.F.);
#52447=ORIENTED_EDGE('',*,*,#38177,.F.);
#52448=ORIENTED_EDGE('',*,*,#38178,.F.);
#52449=ORIENTED_EDGE('',*,*,#37884,.T.);
#52450=ORIENTED_EDGE('',*,*,#38179,.F.);
#52451=ORIENTED_EDGE('',*,*,#38180,.T.);
#52452=ORIENTED_EDGE('',*,*,#38181,.F.);
#52453=ORIENTED_EDGE('',*,*,#37885,.T.);
#52454=ORIENTED_EDGE('',*,*,#38181,.T.);
#52455=ORIENTED_EDGE('',*,*,#38182,.T.);
#52456=ORIENTED_EDGE('',*,*,#38183,.F.);
#52457=ORIENTED_EDGE('',*,*,#38182,.F.);
#52458=ORIENTED_EDGE('',*,*,#38180,.F.);
#52459=ORIENTED_EDGE('',*,*,#38184,.F.);
#52460=ORIENTED_EDGE('',*,*,#38185,.F.);
#52461=ORIENTED_EDGE('',*,*,#37887,.T.);
#52462=ORIENTED_EDGE('',*,*,#38186,.F.);
#52463=ORIENTED_EDGE('',*,*,#38187,.T.);
#52464=ORIENTED_EDGE('',*,*,#38188,.F.);
#52465=ORIENTED_EDGE('',*,*,#37888,.T.);
#52466=ORIENTED_EDGE('',*,*,#38188,.T.);
#52467=ORIENTED_EDGE('',*,*,#38189,.T.);
#52468=ORIENTED_EDGE('',*,*,#38190,.F.);
#52469=ORIENTED_EDGE('',*,*,#38189,.F.);
#52470=ORIENTED_EDGE('',*,*,#38187,.F.);
#52471=ORIENTED_EDGE('',*,*,#38191,.F.);
#52472=ORIENTED_EDGE('',*,*,#38192,.F.);
#52473=ORIENTED_EDGE('',*,*,#37890,.T.);
#52474=ORIENTED_EDGE('',*,*,#38193,.F.);
#52475=ORIENTED_EDGE('',*,*,#38194,.T.);
#52476=ORIENTED_EDGE('',*,*,#38195,.F.);
#52477=ORIENTED_EDGE('',*,*,#37891,.T.);
#52478=ORIENTED_EDGE('',*,*,#38195,.T.);
#52479=ORIENTED_EDGE('',*,*,#38196,.T.);
#52480=ORIENTED_EDGE('',*,*,#38197,.F.);
#52481=ORIENTED_EDGE('',*,*,#38196,.F.);
#52482=ORIENTED_EDGE('',*,*,#38194,.F.);
#52483=ORIENTED_EDGE('',*,*,#38198,.F.);
#52484=ORIENTED_EDGE('',*,*,#38199,.F.);
#52485=ORIENTED_EDGE('',*,*,#37893,.T.);
#52486=ORIENTED_EDGE('',*,*,#38200,.F.);
#52487=ORIENTED_EDGE('',*,*,#38201,.T.);
#52488=ORIENTED_EDGE('',*,*,#38202,.F.);
#52489=ORIENTED_EDGE('',*,*,#37894,.T.);
#52490=ORIENTED_EDGE('',*,*,#38202,.T.);
#52491=ORIENTED_EDGE('',*,*,#38203,.T.);
#52492=ORIENTED_EDGE('',*,*,#38204,.F.);
#52493=ORIENTED_EDGE('',*,*,#38203,.F.);
#52494=ORIENTED_EDGE('',*,*,#38201,.F.);
#52495=ORIENTED_EDGE('',*,*,#38205,.F.);
#52496=ORIENTED_EDGE('',*,*,#38206,.F.);
#52497=ORIENTED_EDGE('',*,*,#37896,.T.);
#52498=ORIENTED_EDGE('',*,*,#38207,.F.);
#52499=ORIENTED_EDGE('',*,*,#38208,.T.);
#52500=ORIENTED_EDGE('',*,*,#38209,.F.);
#52501=ORIENTED_EDGE('',*,*,#37897,.T.);
#52502=ORIENTED_EDGE('',*,*,#38209,.T.);
#52503=ORIENTED_EDGE('',*,*,#38210,.T.);
#52504=ORIENTED_EDGE('',*,*,#38211,.F.);
#52505=ORIENTED_EDGE('',*,*,#38210,.F.);
#52506=ORIENTED_EDGE('',*,*,#38208,.F.);
#52507=ORIENTED_EDGE('',*,*,#38212,.F.);
#52508=ORIENTED_EDGE('',*,*,#38213,.F.);
#52509=ORIENTED_EDGE('',*,*,#37899,.T.);
#52510=ORIENTED_EDGE('',*,*,#38214,.F.);
#52511=ORIENTED_EDGE('',*,*,#38215,.T.);
#52512=ORIENTED_EDGE('',*,*,#38216,.F.);
#52513=ORIENTED_EDGE('',*,*,#37900,.T.);
#52514=ORIENTED_EDGE('',*,*,#38216,.T.);
#52515=ORIENTED_EDGE('',*,*,#38217,.T.);
#52516=ORIENTED_EDGE('',*,*,#38218,.F.);
#52517=ORIENTED_EDGE('',*,*,#38217,.F.);
#52518=ORIENTED_EDGE('',*,*,#38215,.F.);
#52519=ORIENTED_EDGE('',*,*,#38219,.F.);
#52520=ORIENTED_EDGE('',*,*,#38220,.F.);
#52521=ORIENTED_EDGE('',*,*,#37902,.T.);
#52522=ORIENTED_EDGE('',*,*,#38221,.F.);
#52523=ORIENTED_EDGE('',*,*,#38222,.T.);
#52524=ORIENTED_EDGE('',*,*,#38223,.F.);
#52525=ORIENTED_EDGE('',*,*,#37903,.T.);
#52526=ORIENTED_EDGE('',*,*,#38223,.T.);
#52527=ORIENTED_EDGE('',*,*,#38224,.T.);
#52528=ORIENTED_EDGE('',*,*,#38225,.F.);
#52529=ORIENTED_EDGE('',*,*,#38224,.F.);
#52530=ORIENTED_EDGE('',*,*,#38222,.F.);
#52531=ORIENTED_EDGE('',*,*,#38226,.F.);
#52532=ORIENTED_EDGE('',*,*,#38227,.F.);
#52533=ORIENTED_EDGE('',*,*,#37905,.T.);
#52534=ORIENTED_EDGE('',*,*,#38228,.F.);
#52535=ORIENTED_EDGE('',*,*,#38229,.T.);
#52536=ORIENTED_EDGE('',*,*,#38230,.F.);
#52537=ORIENTED_EDGE('',*,*,#37906,.T.);
#52538=ORIENTED_EDGE('',*,*,#38230,.T.);
#52539=ORIENTED_EDGE('',*,*,#38231,.T.);
#52540=ORIENTED_EDGE('',*,*,#38232,.F.);
#52541=ORIENTED_EDGE('',*,*,#38231,.F.);
#52542=ORIENTED_EDGE('',*,*,#38229,.F.);
#52543=ORIENTED_EDGE('',*,*,#38233,.F.);
#52544=ORIENTED_EDGE('',*,*,#38234,.F.);
#52545=ORIENTED_EDGE('',*,*,#37908,.T.);
#52546=ORIENTED_EDGE('',*,*,#38235,.F.);
#52547=ORIENTED_EDGE('',*,*,#38236,.T.);
#52548=ORIENTED_EDGE('',*,*,#38237,.F.);
#52549=ORIENTED_EDGE('',*,*,#37909,.T.);
#52550=ORIENTED_EDGE('',*,*,#38237,.T.);
#52551=ORIENTED_EDGE('',*,*,#38238,.T.);
#52552=ORIENTED_EDGE('',*,*,#38239,.F.);
#52553=ORIENTED_EDGE('',*,*,#38238,.F.);
#52554=ORIENTED_EDGE('',*,*,#38236,.F.);
#52555=ORIENTED_EDGE('',*,*,#38240,.F.);
#52556=ORIENTED_EDGE('',*,*,#38241,.F.);
#52557=ORIENTED_EDGE('',*,*,#37911,.T.);
#52558=ORIENTED_EDGE('',*,*,#38242,.F.);
#52559=ORIENTED_EDGE('',*,*,#38243,.T.);
#52560=ORIENTED_EDGE('',*,*,#38244,.F.);
#52561=ORIENTED_EDGE('',*,*,#37912,.T.);
#52562=ORIENTED_EDGE('',*,*,#38244,.T.);
#52563=ORIENTED_EDGE('',*,*,#38245,.T.);
#52564=ORIENTED_EDGE('',*,*,#38246,.F.);
#52565=ORIENTED_EDGE('',*,*,#38245,.F.);
#52566=ORIENTED_EDGE('',*,*,#38243,.F.);
#52567=ORIENTED_EDGE('',*,*,#38247,.F.);
#52568=ORIENTED_EDGE('',*,*,#38248,.F.);
#52569=ORIENTED_EDGE('',*,*,#37914,.T.);
#52570=ORIENTED_EDGE('',*,*,#38249,.F.);
#52571=ORIENTED_EDGE('',*,*,#38250,.T.);
#52572=ORIENTED_EDGE('',*,*,#38251,.F.);
#52573=ORIENTED_EDGE('',*,*,#37915,.T.);
#52574=ORIENTED_EDGE('',*,*,#38251,.T.);
#52575=ORIENTED_EDGE('',*,*,#38252,.T.);
#52576=ORIENTED_EDGE('',*,*,#38253,.F.);
#52577=ORIENTED_EDGE('',*,*,#38252,.F.);
#52578=ORIENTED_EDGE('',*,*,#38250,.F.);
#52579=ORIENTED_EDGE('',*,*,#38254,.F.);
#52580=ORIENTED_EDGE('',*,*,#38255,.F.);
#52581=ORIENTED_EDGE('',*,*,#37917,.T.);
#52582=ORIENTED_EDGE('',*,*,#38256,.F.);
#52583=ORIENTED_EDGE('',*,*,#34419,.T.);
#52584=ORIENTED_EDGE('',*,*,#38257,.F.);
#52585=ORIENTED_EDGE('',*,*,#37918,.T.);
#52586=ORIENTED_EDGE('',*,*,#38257,.T.);
#52587=ORIENTED_EDGE('',*,*,#34418,.T.);
#52588=ORIENTED_EDGE('',*,*,#38258,.F.);
#52589=ORIENTED_EDGE('',*,*,#37920,.T.);
#52590=ORIENTED_EDGE('',*,*,#38259,.F.);
#52591=ORIENTED_EDGE('',*,*,#38260,.T.);
#52592=ORIENTED_EDGE('',*,*,#38261,.F.);
#52593=ORIENTED_EDGE('',*,*,#37921,.T.);
#52594=ORIENTED_EDGE('',*,*,#38261,.T.);
#52595=ORIENTED_EDGE('',*,*,#38262,.T.);
#52596=ORIENTED_EDGE('',*,*,#38263,.F.);
#52597=ORIENTED_EDGE('',*,*,#38262,.F.);
#52598=ORIENTED_EDGE('',*,*,#38260,.F.);
#52599=ORIENTED_EDGE('',*,*,#38264,.F.);
#52600=ORIENTED_EDGE('',*,*,#38265,.F.);
#52601=ORIENTED_EDGE('',*,*,#37923,.T.);
#52602=ORIENTED_EDGE('',*,*,#38266,.F.);
#52603=ORIENTED_EDGE('',*,*,#38267,.T.);
#52604=ORIENTED_EDGE('',*,*,#38268,.F.);
#52605=ORIENTED_EDGE('',*,*,#37924,.T.);
#52606=ORIENTED_EDGE('',*,*,#38268,.T.);
#52607=ORIENTED_EDGE('',*,*,#38269,.T.);
#52608=ORIENTED_EDGE('',*,*,#38270,.F.);
#52609=ORIENTED_EDGE('',*,*,#38269,.F.);
#52610=ORIENTED_EDGE('',*,*,#38267,.F.);
#52611=ORIENTED_EDGE('',*,*,#38271,.F.);
#52612=ORIENTED_EDGE('',*,*,#38272,.F.);
#52613=ORIENTED_EDGE('',*,*,#37926,.T.);
#52614=ORIENTED_EDGE('',*,*,#38273,.F.);
#52615=ORIENTED_EDGE('',*,*,#38274,.T.);
#52616=ORIENTED_EDGE('',*,*,#38275,.F.);
#52617=ORIENTED_EDGE('',*,*,#37927,.T.);
#52618=ORIENTED_EDGE('',*,*,#38275,.T.);
#52619=ORIENTED_EDGE('',*,*,#38276,.T.);
#52620=ORIENTED_EDGE('',*,*,#38277,.F.);
#52621=ORIENTED_EDGE('',*,*,#38276,.F.);
#52622=ORIENTED_EDGE('',*,*,#38274,.F.);
#52623=ORIENTED_EDGE('',*,*,#38278,.F.);
#52624=ORIENTED_EDGE('',*,*,#38279,.F.);
#52625=ORIENTED_EDGE('',*,*,#37929,.T.);
#52626=ORIENTED_EDGE('',*,*,#38280,.F.);
#52627=ORIENTED_EDGE('',*,*,#38281,.T.);
#52628=ORIENTED_EDGE('',*,*,#38282,.F.);
#52629=ORIENTED_EDGE('',*,*,#37930,.T.);
#52630=ORIENTED_EDGE('',*,*,#38282,.T.);
#52631=ORIENTED_EDGE('',*,*,#38283,.T.);
#52632=ORIENTED_EDGE('',*,*,#38284,.F.);
#52633=ORIENTED_EDGE('',*,*,#38283,.F.);
#52634=ORIENTED_EDGE('',*,*,#38281,.F.);
#52635=ORIENTED_EDGE('',*,*,#38285,.F.);
#52636=ORIENTED_EDGE('',*,*,#38286,.F.);
#52637=ORIENTED_EDGE('',*,*,#37932,.T.);
#52638=ORIENTED_EDGE('',*,*,#38287,.F.);
#52639=ORIENTED_EDGE('',*,*,#38288,.T.);
#52640=ORIENTED_EDGE('',*,*,#38289,.F.);
#52641=ORIENTED_EDGE('',*,*,#37933,.T.);
#52642=ORIENTED_EDGE('',*,*,#38289,.T.);
#52643=ORIENTED_EDGE('',*,*,#38290,.T.);
#52644=ORIENTED_EDGE('',*,*,#38291,.F.);
#52645=ORIENTED_EDGE('',*,*,#38290,.F.);
#52646=ORIENTED_EDGE('',*,*,#38288,.F.);
#52647=ORIENTED_EDGE('',*,*,#38292,.F.);
#52648=ORIENTED_EDGE('',*,*,#38293,.F.);
#52649=ORIENTED_EDGE('',*,*,#37935,.T.);
#52650=ORIENTED_EDGE('',*,*,#38294,.F.);
#52651=ORIENTED_EDGE('',*,*,#38295,.T.);
#52652=ORIENTED_EDGE('',*,*,#38296,.F.);
#52653=ORIENTED_EDGE('',*,*,#37936,.T.);
#52654=ORIENTED_EDGE('',*,*,#38296,.T.);
#52655=ORIENTED_EDGE('',*,*,#38297,.T.);
#52656=ORIENTED_EDGE('',*,*,#38298,.F.);
#52657=ORIENTED_EDGE('',*,*,#38297,.F.);
#52658=ORIENTED_EDGE('',*,*,#38295,.F.);
#52659=ORIENTED_EDGE('',*,*,#38299,.F.);
#52660=ORIENTED_EDGE('',*,*,#38300,.F.);
#52661=ORIENTED_EDGE('',*,*,#37938,.T.);
#52662=ORIENTED_EDGE('',*,*,#38301,.F.);
#52663=ORIENTED_EDGE('',*,*,#38302,.T.);
#52664=ORIENTED_EDGE('',*,*,#38303,.F.);
#52665=ORIENTED_EDGE('',*,*,#37939,.T.);
#52666=ORIENTED_EDGE('',*,*,#38303,.T.);
#52667=ORIENTED_EDGE('',*,*,#38304,.T.);
#52668=ORIENTED_EDGE('',*,*,#38305,.F.);
#52669=ORIENTED_EDGE('',*,*,#38304,.F.);
#52670=ORIENTED_EDGE('',*,*,#38302,.F.);
#52671=ORIENTED_EDGE('',*,*,#38306,.F.);
#52672=ORIENTED_EDGE('',*,*,#38307,.F.);
#52673=ORIENTED_EDGE('',*,*,#37941,.T.);
#52674=ORIENTED_EDGE('',*,*,#38308,.F.);
#52675=ORIENTED_EDGE('',*,*,#38309,.T.);
#52676=ORIENTED_EDGE('',*,*,#38310,.F.);
#52677=ORIENTED_EDGE('',*,*,#37942,.T.);
#52678=ORIENTED_EDGE('',*,*,#38310,.T.);
#52679=ORIENTED_EDGE('',*,*,#38311,.T.);
#52680=ORIENTED_EDGE('',*,*,#38312,.F.);
#52681=ORIENTED_EDGE('',*,*,#38311,.F.);
#52682=ORIENTED_EDGE('',*,*,#38309,.F.);
#52683=ORIENTED_EDGE('',*,*,#38313,.F.);
#52684=ORIENTED_EDGE('',*,*,#38314,.F.);
#52685=ORIENTED_EDGE('',*,*,#37944,.T.);
#52686=ORIENTED_EDGE('',*,*,#38315,.F.);
#52687=ORIENTED_EDGE('',*,*,#38316,.T.);
#52688=ORIENTED_EDGE('',*,*,#38317,.F.);
#52689=ORIENTED_EDGE('',*,*,#37945,.T.);
#52690=ORIENTED_EDGE('',*,*,#38317,.T.);
#52691=ORIENTED_EDGE('',*,*,#38318,.T.);
#52692=ORIENTED_EDGE('',*,*,#38319,.F.);
#52693=ORIENTED_EDGE('',*,*,#38318,.F.);
#52694=ORIENTED_EDGE('',*,*,#38316,.F.);
#52695=ORIENTED_EDGE('',*,*,#38320,.F.);
#52696=ORIENTED_EDGE('',*,*,#38321,.F.);
#52697=ORIENTED_EDGE('',*,*,#37947,.T.);
#52698=ORIENTED_EDGE('',*,*,#38322,.F.);
#52699=ORIENTED_EDGE('',*,*,#38323,.T.);
#52700=ORIENTED_EDGE('',*,*,#38324,.F.);
#52701=ORIENTED_EDGE('',*,*,#37948,.T.);
#52702=ORIENTED_EDGE('',*,*,#38324,.T.);
#52703=ORIENTED_EDGE('',*,*,#38325,.T.);
#52704=ORIENTED_EDGE('',*,*,#38326,.F.);
#52705=ORIENTED_EDGE('',*,*,#38325,.F.);
#52706=ORIENTED_EDGE('',*,*,#38323,.F.);
#52707=ORIENTED_EDGE('',*,*,#38327,.F.);
#52708=ORIENTED_EDGE('',*,*,#38328,.F.);
#52709=ORIENTED_EDGE('',*,*,#37950,.T.);
#52710=ORIENTED_EDGE('',*,*,#38329,.F.);
#52711=ORIENTED_EDGE('',*,*,#38330,.T.);
#52712=ORIENTED_EDGE('',*,*,#38331,.F.);
#52713=ORIENTED_EDGE('',*,*,#37951,.T.);
#52714=ORIENTED_EDGE('',*,*,#38331,.T.);
#52715=ORIENTED_EDGE('',*,*,#38332,.T.);
#52716=ORIENTED_EDGE('',*,*,#38333,.F.);
#52717=ORIENTED_EDGE('',*,*,#38332,.F.);
#52718=ORIENTED_EDGE('',*,*,#38330,.F.);
#52719=ORIENTED_EDGE('',*,*,#38334,.F.);
#52720=ORIENTED_EDGE('',*,*,#38335,.F.);
#52721=ORIENTED_EDGE('',*,*,#37953,.T.);
#52722=ORIENTED_EDGE('',*,*,#38336,.F.);
#52723=ORIENTED_EDGE('',*,*,#38337,.T.);
#52724=ORIENTED_EDGE('',*,*,#38338,.F.);
#52725=ORIENTED_EDGE('',*,*,#37954,.T.);
#52726=ORIENTED_EDGE('',*,*,#38338,.T.);
#52727=ORIENTED_EDGE('',*,*,#38339,.T.);
#52728=ORIENTED_EDGE('',*,*,#38340,.F.);
#52729=ORIENTED_EDGE('',*,*,#38339,.F.);
#52730=ORIENTED_EDGE('',*,*,#38337,.F.);
#52731=ORIENTED_EDGE('',*,*,#38341,.F.);
#52732=ORIENTED_EDGE('',*,*,#38342,.F.);
#52733=ORIENTED_EDGE('',*,*,#37956,.T.);
#52734=ORIENTED_EDGE('',*,*,#38343,.F.);
#52735=ORIENTED_EDGE('',*,*,#38344,.T.);
#52736=ORIENTED_EDGE('',*,*,#38345,.F.);
#52737=ORIENTED_EDGE('',*,*,#37957,.T.);
#52738=ORIENTED_EDGE('',*,*,#38345,.T.);
#52739=ORIENTED_EDGE('',*,*,#38346,.T.);
#52740=ORIENTED_EDGE('',*,*,#38347,.F.);
#52741=ORIENTED_EDGE('',*,*,#38346,.F.);
#52742=ORIENTED_EDGE('',*,*,#38344,.F.);
#52743=ORIENTED_EDGE('',*,*,#38348,.F.);
#52744=ORIENTED_EDGE('',*,*,#38349,.F.);
#52745=ORIENTED_EDGE('',*,*,#37959,.T.);
#52746=ORIENTED_EDGE('',*,*,#38350,.F.);
#52747=ORIENTED_EDGE('',*,*,#38351,.T.);
#52748=ORIENTED_EDGE('',*,*,#38352,.F.);
#52749=ORIENTED_EDGE('',*,*,#38353,.T.);
#52750=ORIENTED_EDGE('',*,*,#38354,.F.);
#52751=ORIENTED_EDGE('',*,*,#37960,.T.);
#52752=ORIENTED_EDGE('',*,*,#38352,.T.);
#52753=ORIENTED_EDGE('',*,*,#38355,.F.);
#52754=ORIENTED_EDGE('',*,*,#38356,.F.);
#52755=ORIENTED_EDGE('',*,*,#38353,.F.);
#52756=ORIENTED_EDGE('',*,*,#38351,.F.);
#52757=ORIENTED_EDGE('',*,*,#38163,.F.);
#52758=ORIENTED_EDGE('',*,*,#38357,.F.);
#52759=ORIENTED_EDGE('',*,*,#38358,.F.);
#52760=ORIENTED_EDGE('',*,*,#38359,.F.);
#52761=ORIENTED_EDGE('',*,*,#37962,.T.);
#52762=ORIENTED_EDGE('',*,*,#38360,.F.);
#52763=ORIENTED_EDGE('',*,*,#38357,.T.);
#52764=ORIENTED_EDGE('',*,*,#38162,.T.);
#52765=ORIENTED_EDGE('',*,*,#38361,.F.);
#52766=ORIENTED_EDGE('',*,*,#37964,.T.);
#52767=ORIENTED_EDGE('',*,*,#38159,.T.);
#52768=ORIENTED_EDGE('',*,*,#38362,.F.);
#52769=ORIENTED_EDGE('',*,*,#38363,.F.);
#52770=ORIENTED_EDGE('',*,*,#38364,.F.);
#52771=ORIENTED_EDGE('',*,*,#37969,.T.);
#52772=ORIENTED_EDGE('',*,*,#37968,.T.);
#52773=ORIENTED_EDGE('',*,*,#38365,.F.);
#52774=ORIENTED_EDGE('',*,*,#37972,.T.);
#52775=ORIENTED_EDGE('',*,*,#37970,.T.);
#52776=ORIENTED_EDGE('',*,*,#38364,.T.);
#52777=ORIENTED_EDGE('',*,*,#38366,.F.);
#52778=ORIENTED_EDGE('',*,*,#38367,.F.);
#52779=ORIENTED_EDGE('',*,*,#37976,.T.);
#52780=ORIENTED_EDGE('',*,*,#37975,.T.);
#52781=ORIENTED_EDGE('',*,*,#38368,.F.);
#52782=ORIENTED_EDGE('',*,*,#37979,.T.);
#52783=ORIENTED_EDGE('',*,*,#37977,.T.);
#52784=ORIENTED_EDGE('',*,*,#38367,.T.);
#52785=ORIENTED_EDGE('',*,*,#38369,.F.);
#52786=ORIENTED_EDGE('',*,*,#38370,.F.);
#52787=ORIENTED_EDGE('',*,*,#37983,.T.);
#52788=ORIENTED_EDGE('',*,*,#37982,.T.);
#52789=ORIENTED_EDGE('',*,*,#38371,.F.);
#52790=ORIENTED_EDGE('',*,*,#37986,.T.);
#52791=ORIENTED_EDGE('',*,*,#37984,.T.);
#52792=ORIENTED_EDGE('',*,*,#38370,.T.);
#52793=ORIENTED_EDGE('',*,*,#38372,.F.);
#52794=ORIENTED_EDGE('',*,*,#38373,.F.);
#52795=ORIENTED_EDGE('',*,*,#37990,.T.);
#52796=ORIENTED_EDGE('',*,*,#37989,.T.);
#52797=ORIENTED_EDGE('',*,*,#38374,.F.);
#52798=ORIENTED_EDGE('',*,*,#37993,.T.);
#52799=ORIENTED_EDGE('',*,*,#37991,.T.);
#52800=ORIENTED_EDGE('',*,*,#38373,.T.);
#52801=ORIENTED_EDGE('',*,*,#38375,.F.);
#52802=ORIENTED_EDGE('',*,*,#38376,.F.);
#52803=ORIENTED_EDGE('',*,*,#37997,.T.);
#52804=ORIENTED_EDGE('',*,*,#37996,.T.);
#52805=ORIENTED_EDGE('',*,*,#38377,.F.);
#52806=ORIENTED_EDGE('',*,*,#38000,.T.);
#52807=ORIENTED_EDGE('',*,*,#37998,.T.);
#52808=ORIENTED_EDGE('',*,*,#38376,.T.);
#52809=ORIENTED_EDGE('',*,*,#38378,.F.);
#52810=ORIENTED_EDGE('',*,*,#38379,.F.);
#52811=ORIENTED_EDGE('',*,*,#38004,.T.);
#52812=ORIENTED_EDGE('',*,*,#38003,.T.);
#52813=ORIENTED_EDGE('',*,*,#38380,.F.);
#52814=ORIENTED_EDGE('',*,*,#38007,.T.);
#52815=ORIENTED_EDGE('',*,*,#38005,.T.);
#52816=ORIENTED_EDGE('',*,*,#38379,.T.);
#52817=ORIENTED_EDGE('',*,*,#38381,.F.);
#52818=ORIENTED_EDGE('',*,*,#38382,.F.);
#52819=ORIENTED_EDGE('',*,*,#34423,.T.);
#52820=ORIENTED_EDGE('',*,*,#38009,.T.);
#52821=ORIENTED_EDGE('',*,*,#38383,.F.);
#52822=ORIENTED_EDGE('',*,*,#38010,.T.);
#52823=ORIENTED_EDGE('',*,*,#34424,.T.);
#52824=ORIENTED_EDGE('',*,*,#38382,.T.);
#52825=ORIENTED_EDGE('',*,*,#38384,.F.);
#52826=ORIENTED_EDGE('',*,*,#38385,.F.);
#52827=ORIENTED_EDGE('',*,*,#38014,.T.);
#52828=ORIENTED_EDGE('',*,*,#38013,.T.);
#52829=ORIENTED_EDGE('',*,*,#38386,.F.);
#52830=ORIENTED_EDGE('',*,*,#38017,.T.);
#52831=ORIENTED_EDGE('',*,*,#38015,.T.);
#52832=ORIENTED_EDGE('',*,*,#38385,.T.);
#52833=ORIENTED_EDGE('',*,*,#38387,.F.);
#52834=ORIENTED_EDGE('',*,*,#38388,.F.);
#52835=ORIENTED_EDGE('',*,*,#38021,.T.);
#52836=ORIENTED_EDGE('',*,*,#38020,.T.);
#52837=ORIENTED_EDGE('',*,*,#38389,.F.);
#52838=ORIENTED_EDGE('',*,*,#38024,.T.);
#52839=ORIENTED_EDGE('',*,*,#38022,.T.);
#52840=ORIENTED_EDGE('',*,*,#38388,.T.);
#52841=ORIENTED_EDGE('',*,*,#38390,.F.);
#52842=ORIENTED_EDGE('',*,*,#38391,.F.);
#52843=ORIENTED_EDGE('',*,*,#38028,.T.);
#52844=ORIENTED_EDGE('',*,*,#38027,.T.);
#52845=ORIENTED_EDGE('',*,*,#38392,.F.);
#52846=ORIENTED_EDGE('',*,*,#38031,.T.);
#52847=ORIENTED_EDGE('',*,*,#38029,.T.);
#52848=ORIENTED_EDGE('',*,*,#38391,.T.);
#52849=ORIENTED_EDGE('',*,*,#38393,.F.);
#52850=ORIENTED_EDGE('',*,*,#38394,.F.);
#52851=ORIENTED_EDGE('',*,*,#38035,.T.);
#52852=ORIENTED_EDGE('',*,*,#38034,.T.);
#52853=ORIENTED_EDGE('',*,*,#38395,.F.);
#52854=ORIENTED_EDGE('',*,*,#38038,.T.);
#52855=ORIENTED_EDGE('',*,*,#38036,.T.);
#52856=ORIENTED_EDGE('',*,*,#38394,.T.);
#52857=ORIENTED_EDGE('',*,*,#38396,.F.);
#52858=ORIENTED_EDGE('',*,*,#38397,.F.);
#52859=ORIENTED_EDGE('',*,*,#38042,.T.);
#52860=ORIENTED_EDGE('',*,*,#38041,.T.);
#52861=ORIENTED_EDGE('',*,*,#38398,.F.);
#52862=ORIENTED_EDGE('',*,*,#38045,.T.);
#52863=ORIENTED_EDGE('',*,*,#38043,.T.);
#52864=ORIENTED_EDGE('',*,*,#38397,.T.);
#52865=ORIENTED_EDGE('',*,*,#38399,.F.);
#52866=ORIENTED_EDGE('',*,*,#38400,.F.);
#52867=ORIENTED_EDGE('',*,*,#38049,.T.);
#52868=ORIENTED_EDGE('',*,*,#38048,.T.);
#52869=ORIENTED_EDGE('',*,*,#38401,.F.);
#52870=ORIENTED_EDGE('',*,*,#38052,.T.);
#52871=ORIENTED_EDGE('',*,*,#38050,.T.);
#52872=ORIENTED_EDGE('',*,*,#38400,.T.);
#52873=ORIENTED_EDGE('',*,*,#38402,.F.);
#52874=ORIENTED_EDGE('',*,*,#38403,.F.);
#52875=ORIENTED_EDGE('',*,*,#38056,.T.);
#52876=ORIENTED_EDGE('',*,*,#38055,.T.);
#52877=ORIENTED_EDGE('',*,*,#38404,.F.);
#52878=ORIENTED_EDGE('',*,*,#38059,.T.);
#52879=ORIENTED_EDGE('',*,*,#38057,.T.);
#52880=ORIENTED_EDGE('',*,*,#38403,.T.);
#52881=ORIENTED_EDGE('',*,*,#38405,.F.);
#52882=ORIENTED_EDGE('',*,*,#38406,.F.);
#52883=ORIENTED_EDGE('',*,*,#38063,.T.);
#52884=ORIENTED_EDGE('',*,*,#38062,.T.);
#52885=ORIENTED_EDGE('',*,*,#38407,.F.);
#52886=ORIENTED_EDGE('',*,*,#38066,.T.);
#52887=ORIENTED_EDGE('',*,*,#38064,.T.);
#52888=ORIENTED_EDGE('',*,*,#38406,.T.);
#52889=ORIENTED_EDGE('',*,*,#38408,.F.);
#52890=ORIENTED_EDGE('',*,*,#38409,.F.);
#52891=ORIENTED_EDGE('',*,*,#38070,.T.);
#52892=ORIENTED_EDGE('',*,*,#38069,.T.);
#52893=ORIENTED_EDGE('',*,*,#38410,.F.);
#52894=ORIENTED_EDGE('',*,*,#38073,.T.);
#52895=ORIENTED_EDGE('',*,*,#38071,.T.);
#52896=ORIENTED_EDGE('',*,*,#38409,.T.);
#52897=ORIENTED_EDGE('',*,*,#38411,.F.);
#52898=ORIENTED_EDGE('',*,*,#38412,.F.);
#52899=ORIENTED_EDGE('',*,*,#38077,.T.);
#52900=ORIENTED_EDGE('',*,*,#38076,.T.);
#52901=ORIENTED_EDGE('',*,*,#38413,.F.);
#52902=ORIENTED_EDGE('',*,*,#38080,.T.);
#52903=ORIENTED_EDGE('',*,*,#38078,.T.);
#52904=ORIENTED_EDGE('',*,*,#38412,.T.);
#52905=ORIENTED_EDGE('',*,*,#38414,.F.);
#52906=ORIENTED_EDGE('',*,*,#38415,.F.);
#52907=ORIENTED_EDGE('',*,*,#38084,.T.);
#52908=ORIENTED_EDGE('',*,*,#38083,.T.);
#52909=ORIENTED_EDGE('',*,*,#38416,.F.);
#52910=ORIENTED_EDGE('',*,*,#38087,.T.);
#52911=ORIENTED_EDGE('',*,*,#38085,.T.);
#52912=ORIENTED_EDGE('',*,*,#38415,.T.);
#52913=ORIENTED_EDGE('',*,*,#38417,.F.);
#52914=ORIENTED_EDGE('',*,*,#38418,.F.);
#52915=ORIENTED_EDGE('',*,*,#38091,.T.);
#52916=ORIENTED_EDGE('',*,*,#38090,.T.);
#52917=ORIENTED_EDGE('',*,*,#38419,.F.);
#52918=ORIENTED_EDGE('',*,*,#38094,.T.);
#52919=ORIENTED_EDGE('',*,*,#38092,.T.);
#52920=ORIENTED_EDGE('',*,*,#38418,.T.);
#52921=ORIENTED_EDGE('',*,*,#38420,.F.);
#52922=ORIENTED_EDGE('',*,*,#38421,.F.);
#52923=ORIENTED_EDGE('',*,*,#38098,.T.);
#52924=ORIENTED_EDGE('',*,*,#38097,.T.);
#52925=ORIENTED_EDGE('',*,*,#38422,.F.);
#52926=ORIENTED_EDGE('',*,*,#38101,.T.);
#52927=ORIENTED_EDGE('',*,*,#38099,.T.);
#52928=ORIENTED_EDGE('',*,*,#38421,.T.);
#52929=ORIENTED_EDGE('',*,*,#38423,.F.);
#52930=ORIENTED_EDGE('',*,*,#38424,.F.);
#52931=ORIENTED_EDGE('',*,*,#38105,.T.);
#52932=ORIENTED_EDGE('',*,*,#38104,.T.);
#52933=ORIENTED_EDGE('',*,*,#38425,.F.);
#52934=ORIENTED_EDGE('',*,*,#38108,.T.);
#52935=ORIENTED_EDGE('',*,*,#38106,.T.);
#52936=ORIENTED_EDGE('',*,*,#38424,.T.);
#52937=ORIENTED_EDGE('',*,*,#38426,.F.);
#52938=ORIENTED_EDGE('',*,*,#38427,.F.);
#52939=ORIENTED_EDGE('',*,*,#38114,.T.);
#52940=ORIENTED_EDGE('',*,*,#38111,.T.);
#52941=ORIENTED_EDGE('',*,*,#38115,.T.);
#52942=ORIENTED_EDGE('',*,*,#38427,.T.);
#52943=ORIENTED_EDGE('',*,*,#38428,.F.);
#52944=ORIENTED_EDGE('',*,*,#38113,.T.);
#52945=ORIENTED_EDGE('',*,*,#38120,.T.);
#52946=ORIENTED_EDGE('',*,*,#38116,.T.);
#52947=ORIENTED_EDGE('',*,*,#38429,.F.);
#52948=ORIENTED_EDGE('',*,*,#38430,.F.);
#52949=ORIENTED_EDGE('',*,*,#38431,.F.);
#52950=ORIENTED_EDGE('',*,*,#38122,.T.);
#52951=ORIENTED_EDGE('',*,*,#38121,.T.);
#52952=ORIENTED_EDGE('',*,*,#38430,.T.);
#52953=ORIENTED_EDGE('',*,*,#38432,.F.);
#52954=ORIENTED_EDGE('',*,*,#38433,.F.);
#52955=ORIENTED_EDGE('',*,*,#38126,.T.);
#52956=ORIENTED_EDGE('',*,*,#38125,.T.);
#52957=ORIENTED_EDGE('',*,*,#38434,.F.);
#52958=ORIENTED_EDGE('',*,*,#38129,.T.);
#52959=ORIENTED_EDGE('',*,*,#38127,.T.);
#52960=ORIENTED_EDGE('',*,*,#38433,.T.);
#52961=ORIENTED_EDGE('',*,*,#38435,.F.);
#52962=ORIENTED_EDGE('',*,*,#38436,.F.);
#52963=ORIENTED_EDGE('',*,*,#38133,.T.);
#52964=ORIENTED_EDGE('',*,*,#38132,.T.);
#52965=ORIENTED_EDGE('',*,*,#38437,.F.);
#52966=ORIENTED_EDGE('',*,*,#38136,.T.);
#52967=ORIENTED_EDGE('',*,*,#38134,.T.);
#52968=ORIENTED_EDGE('',*,*,#38436,.T.);
#52969=ORIENTED_EDGE('',*,*,#38438,.F.);
#52970=ORIENTED_EDGE('',*,*,#38439,.F.);
#52971=ORIENTED_EDGE('',*,*,#38140,.T.);
#52972=ORIENTED_EDGE('',*,*,#38139,.T.);
#52973=ORIENTED_EDGE('',*,*,#38440,.F.);
#52974=ORIENTED_EDGE('',*,*,#38143,.T.);
#52975=ORIENTED_EDGE('',*,*,#38141,.T.);
#52976=ORIENTED_EDGE('',*,*,#38439,.T.);
#52977=ORIENTED_EDGE('',*,*,#38441,.F.);
#52978=ORIENTED_EDGE('',*,*,#38442,.F.);
#52979=ORIENTED_EDGE('',*,*,#38147,.T.);
#52980=ORIENTED_EDGE('',*,*,#38146,.T.);
#52981=ORIENTED_EDGE('',*,*,#38443,.F.);
#52982=ORIENTED_EDGE('',*,*,#38150,.T.);
#52983=ORIENTED_EDGE('',*,*,#38148,.T.);
#52984=ORIENTED_EDGE('',*,*,#38442,.T.);
#52985=ORIENTED_EDGE('',*,*,#38444,.F.);
#52986=ORIENTED_EDGE('',*,*,#38445,.F.);
#52987=ORIENTED_EDGE('',*,*,#38154,.T.);
#52988=ORIENTED_EDGE('',*,*,#38153,.T.);
#52989=ORIENTED_EDGE('',*,*,#38446,.F.);
#52990=ORIENTED_EDGE('',*,*,#38157,.T.);
#52991=ORIENTED_EDGE('',*,*,#38155,.T.);
#52992=ORIENTED_EDGE('',*,*,#38445,.T.);
#52993=ORIENTED_EDGE('',*,*,#38447,.F.);
#52994=ORIENTED_EDGE('',*,*,#38362,.T.);
#52995=ORIENTED_EDGE('',*,*,#38158,.T.);
#52996=ORIENTED_EDGE('',*,*,#38161,.T.);
#52997=ORIENTED_EDGE('',*,*,#38359,.T.);
#52998=ORIENTED_EDGE('',*,*,#38448,.F.);
#52999=ORIENTED_EDGE('',*,*,#38449,.F.);
#53000=ORIENTED_EDGE('',*,*,#38164,.T.);
#53001=ORIENTED_EDGE('',*,*,#38170,.T.);
#53002=ORIENTED_EDGE('',*,*,#38165,.T.);
#53003=ORIENTED_EDGE('',*,*,#38450,.F.);
#53004=ORIENTED_EDGE('',*,*,#38451,.F.);
#53005=ORIENTED_EDGE('',*,*,#38171,.T.);
#53006=ORIENTED_EDGE('',*,*,#38451,.T.);
#53007=ORIENTED_EDGE('',*,*,#38452,.F.);
#53008=ORIENTED_EDGE('',*,*,#38169,.T.);
#53009=ORIENTED_EDGE('',*,*,#38177,.T.);
#53010=ORIENTED_EDGE('',*,*,#38172,.T.);
#53011=ORIENTED_EDGE('',*,*,#38453,.F.);
#53012=ORIENTED_EDGE('',*,*,#38454,.F.);
#53013=ORIENTED_EDGE('',*,*,#38178,.T.);
#53014=ORIENTED_EDGE('',*,*,#38454,.T.);
#53015=ORIENTED_EDGE('',*,*,#38455,.F.);
#53016=ORIENTED_EDGE('',*,*,#38176,.T.);
#53017=ORIENTED_EDGE('',*,*,#38184,.T.);
#53018=ORIENTED_EDGE('',*,*,#38179,.T.);
#53019=ORIENTED_EDGE('',*,*,#38456,.F.);
#53020=ORIENTED_EDGE('',*,*,#38457,.F.);
#53021=ORIENTED_EDGE('',*,*,#38185,.T.);
#53022=ORIENTED_EDGE('',*,*,#38457,.T.);
#53023=ORIENTED_EDGE('',*,*,#38458,.F.);
#53024=ORIENTED_EDGE('',*,*,#38183,.T.);
#53025=ORIENTED_EDGE('',*,*,#38191,.T.);
#53026=ORIENTED_EDGE('',*,*,#38186,.T.);
#53027=ORIENTED_EDGE('',*,*,#38459,.F.);
#53028=ORIENTED_EDGE('',*,*,#38460,.F.);
#53029=ORIENTED_EDGE('',*,*,#38192,.T.);
#53030=ORIENTED_EDGE('',*,*,#38460,.T.);
#53031=ORIENTED_EDGE('',*,*,#38461,.F.);
#53032=ORIENTED_EDGE('',*,*,#38190,.T.);
#53033=ORIENTED_EDGE('',*,*,#38198,.T.);
#53034=ORIENTED_EDGE('',*,*,#38193,.T.);
#53035=ORIENTED_EDGE('',*,*,#38462,.F.);
#53036=ORIENTED_EDGE('',*,*,#38463,.F.);
#53037=ORIENTED_EDGE('',*,*,#38199,.T.);
#53038=ORIENTED_EDGE('',*,*,#38463,.T.);
#53039=ORIENTED_EDGE('',*,*,#38464,.F.);
#53040=ORIENTED_EDGE('',*,*,#38197,.T.);
#53041=ORIENTED_EDGE('',*,*,#38205,.T.);
#53042=ORIENTED_EDGE('',*,*,#38200,.T.);
#53043=ORIENTED_EDGE('',*,*,#38465,.F.);
#53044=ORIENTED_EDGE('',*,*,#38466,.F.);
#53045=ORIENTED_EDGE('',*,*,#38206,.T.);
#53046=ORIENTED_EDGE('',*,*,#38466,.T.);
#53047=ORIENTED_EDGE('',*,*,#38467,.F.);
#53048=ORIENTED_EDGE('',*,*,#38204,.T.);
#53049=ORIENTED_EDGE('',*,*,#38212,.T.);
#53050=ORIENTED_EDGE('',*,*,#38207,.T.);
#53051=ORIENTED_EDGE('',*,*,#38468,.F.);
#53052=ORIENTED_EDGE('',*,*,#38469,.F.);
#53053=ORIENTED_EDGE('',*,*,#38213,.T.);
#53054=ORIENTED_EDGE('',*,*,#38469,.T.);
#53055=ORIENTED_EDGE('',*,*,#38470,.F.);
#53056=ORIENTED_EDGE('',*,*,#38211,.T.);
#53057=ORIENTED_EDGE('',*,*,#38219,.T.);
#53058=ORIENTED_EDGE('',*,*,#38214,.T.);
#53059=ORIENTED_EDGE('',*,*,#38471,.F.);
#53060=ORIENTED_EDGE('',*,*,#38472,.F.);
#53061=ORIENTED_EDGE('',*,*,#38220,.T.);
#53062=ORIENTED_EDGE('',*,*,#38472,.T.);
#53063=ORIENTED_EDGE('',*,*,#38473,.F.);
#53064=ORIENTED_EDGE('',*,*,#38218,.T.);
#53065=ORIENTED_EDGE('',*,*,#38226,.T.);
#53066=ORIENTED_EDGE('',*,*,#38221,.T.);
#53067=ORIENTED_EDGE('',*,*,#38474,.F.);
#53068=ORIENTED_EDGE('',*,*,#38475,.F.);
#53069=ORIENTED_EDGE('',*,*,#38227,.T.);
#53070=ORIENTED_EDGE('',*,*,#38475,.T.);
#53071=ORIENTED_EDGE('',*,*,#38476,.F.);
#53072=ORIENTED_EDGE('',*,*,#38225,.T.);
#53073=ORIENTED_EDGE('',*,*,#38233,.T.);
#53074=ORIENTED_EDGE('',*,*,#38228,.T.);
#53075=ORIENTED_EDGE('',*,*,#38477,.F.);
#53076=ORIENTED_EDGE('',*,*,#38478,.F.);
#53077=ORIENTED_EDGE('',*,*,#38234,.T.);
#53078=ORIENTED_EDGE('',*,*,#38478,.T.);
#53079=ORIENTED_EDGE('',*,*,#38479,.F.);
#53080=ORIENTED_EDGE('',*,*,#38232,.T.);
#53081=ORIENTED_EDGE('',*,*,#38240,.T.);
#53082=ORIENTED_EDGE('',*,*,#38235,.T.);
#53083=ORIENTED_EDGE('',*,*,#38480,.F.);
#53084=ORIENTED_EDGE('',*,*,#38481,.F.);
#53085=ORIENTED_EDGE('',*,*,#38241,.T.);
#53086=ORIENTED_EDGE('',*,*,#38481,.T.);
#53087=ORIENTED_EDGE('',*,*,#38482,.F.);
#53088=ORIENTED_EDGE('',*,*,#38239,.T.);
#53089=ORIENTED_EDGE('',*,*,#38247,.T.);
#53090=ORIENTED_EDGE('',*,*,#38242,.T.);
#53091=ORIENTED_EDGE('',*,*,#38483,.F.);
#53092=ORIENTED_EDGE('',*,*,#38484,.F.);
#53093=ORIENTED_EDGE('',*,*,#38248,.T.);
#53094=ORIENTED_EDGE('',*,*,#38484,.T.);
#53095=ORIENTED_EDGE('',*,*,#38485,.F.);
#53096=ORIENTED_EDGE('',*,*,#38246,.T.);
#53097=ORIENTED_EDGE('',*,*,#38254,.T.);
#53098=ORIENTED_EDGE('',*,*,#38249,.T.);
#53099=ORIENTED_EDGE('',*,*,#38486,.F.);
#53100=ORIENTED_EDGE('',*,*,#38487,.F.);
#53101=ORIENTED_EDGE('',*,*,#38255,.T.);
#53102=ORIENTED_EDGE('',*,*,#38487,.T.);
#53103=ORIENTED_EDGE('',*,*,#38488,.F.);
#53104=ORIENTED_EDGE('',*,*,#38253,.T.);
#53105=ORIENTED_EDGE('',*,*,#34420,.T.);
#53106=ORIENTED_EDGE('',*,*,#38256,.T.);
#53107=ORIENTED_EDGE('',*,*,#38489,.F.);
#53108=ORIENTED_EDGE('',*,*,#38490,.F.);
#53109=ORIENTED_EDGE('',*,*,#34417,.T.);
#53110=ORIENTED_EDGE('',*,*,#38490,.T.);
#53111=ORIENTED_EDGE('',*,*,#38491,.F.);
#53112=ORIENTED_EDGE('',*,*,#38258,.T.);
#53113=ORIENTED_EDGE('',*,*,#38264,.T.);
#53114=ORIENTED_EDGE('',*,*,#38259,.T.);
#53115=ORIENTED_EDGE('',*,*,#38492,.F.);
#53116=ORIENTED_EDGE('',*,*,#38493,.F.);
#53117=ORIENTED_EDGE('',*,*,#38265,.T.);
#53118=ORIENTED_EDGE('',*,*,#38493,.T.);
#53119=ORIENTED_EDGE('',*,*,#38494,.F.);
#53120=ORIENTED_EDGE('',*,*,#38263,.T.);
#53121=ORIENTED_EDGE('',*,*,#38271,.T.);
#53122=ORIENTED_EDGE('',*,*,#38266,.T.);
#53123=ORIENTED_EDGE('',*,*,#38495,.F.);
#53124=ORIENTED_EDGE('',*,*,#38496,.F.);
#53125=ORIENTED_EDGE('',*,*,#38272,.T.);
#53126=ORIENTED_EDGE('',*,*,#38496,.T.);
#53127=ORIENTED_EDGE('',*,*,#38497,.F.);
#53128=ORIENTED_EDGE('',*,*,#38270,.T.);
#53129=ORIENTED_EDGE('',*,*,#38278,.T.);
#53130=ORIENTED_EDGE('',*,*,#38273,.T.);
#53131=ORIENTED_EDGE('',*,*,#38498,.F.);
#53132=ORIENTED_EDGE('',*,*,#38499,.F.);
#53133=ORIENTED_EDGE('',*,*,#38279,.T.);
#53134=ORIENTED_EDGE('',*,*,#38499,.T.);
#53135=ORIENTED_EDGE('',*,*,#38500,.F.);
#53136=ORIENTED_EDGE('',*,*,#38277,.T.);
#53137=ORIENTED_EDGE('',*,*,#38285,.T.);
#53138=ORIENTED_EDGE('',*,*,#38280,.T.);
#53139=ORIENTED_EDGE('',*,*,#38501,.F.);
#53140=ORIENTED_EDGE('',*,*,#38502,.F.);
#53141=ORIENTED_EDGE('',*,*,#38286,.T.);
#53142=ORIENTED_EDGE('',*,*,#38502,.T.);
#53143=ORIENTED_EDGE('',*,*,#38503,.F.);
#53144=ORIENTED_EDGE('',*,*,#38284,.T.);
#53145=ORIENTED_EDGE('',*,*,#38292,.T.);
#53146=ORIENTED_EDGE('',*,*,#38287,.T.);
#53147=ORIENTED_EDGE('',*,*,#38504,.F.);
#53148=ORIENTED_EDGE('',*,*,#38505,.F.);
#53149=ORIENTED_EDGE('',*,*,#38293,.T.);
#53150=ORIENTED_EDGE('',*,*,#38505,.T.);
#53151=ORIENTED_EDGE('',*,*,#38506,.F.);
#53152=ORIENTED_EDGE('',*,*,#38291,.T.);
#53153=ORIENTED_EDGE('',*,*,#38299,.T.);
#53154=ORIENTED_EDGE('',*,*,#38294,.T.);
#53155=ORIENTED_EDGE('',*,*,#38507,.F.);
#53156=ORIENTED_EDGE('',*,*,#38508,.F.);
#53157=ORIENTED_EDGE('',*,*,#38300,.T.);
#53158=ORIENTED_EDGE('',*,*,#38508,.T.);
#53159=ORIENTED_EDGE('',*,*,#38509,.F.);
#53160=ORIENTED_EDGE('',*,*,#38298,.T.);
#53161=ORIENTED_EDGE('',*,*,#38306,.T.);
#53162=ORIENTED_EDGE('',*,*,#38301,.T.);
#53163=ORIENTED_EDGE('',*,*,#38510,.F.);
#53164=ORIENTED_EDGE('',*,*,#38511,.F.);
#53165=ORIENTED_EDGE('',*,*,#38307,.T.);
#53166=ORIENTED_EDGE('',*,*,#38511,.T.);
#53167=ORIENTED_EDGE('',*,*,#38512,.F.);
#53168=ORIENTED_EDGE('',*,*,#38305,.T.);
#53169=ORIENTED_EDGE('',*,*,#38313,.T.);
#53170=ORIENTED_EDGE('',*,*,#38308,.T.);
#53171=ORIENTED_EDGE('',*,*,#38513,.F.);
#53172=ORIENTED_EDGE('',*,*,#38514,.F.);
#53173=ORIENTED_EDGE('',*,*,#38314,.T.);
#53174=ORIENTED_EDGE('',*,*,#38514,.T.);
#53175=ORIENTED_EDGE('',*,*,#38515,.F.);
#53176=ORIENTED_EDGE('',*,*,#38312,.T.);
#53177=ORIENTED_EDGE('',*,*,#38320,.T.);
#53178=ORIENTED_EDGE('',*,*,#38315,.T.);
#53179=ORIENTED_EDGE('',*,*,#38516,.F.);
#53180=ORIENTED_EDGE('',*,*,#38517,.F.);
#53181=ORIENTED_EDGE('',*,*,#38321,.T.);
#53182=ORIENTED_EDGE('',*,*,#38517,.T.);
#53183=ORIENTED_EDGE('',*,*,#38518,.F.);
#53184=ORIENTED_EDGE('',*,*,#38319,.T.);
#53185=ORIENTED_EDGE('',*,*,#38327,.T.);
#53186=ORIENTED_EDGE('',*,*,#38322,.T.);
#53187=ORIENTED_EDGE('',*,*,#38519,.F.);
#53188=ORIENTED_EDGE('',*,*,#38520,.F.);
#53189=ORIENTED_EDGE('',*,*,#38328,.T.);
#53190=ORIENTED_EDGE('',*,*,#38520,.T.);
#53191=ORIENTED_EDGE('',*,*,#38521,.F.);
#53192=ORIENTED_EDGE('',*,*,#38326,.T.);
#53193=ORIENTED_EDGE('',*,*,#38334,.T.);
#53194=ORIENTED_EDGE('',*,*,#38329,.T.);
#53195=ORIENTED_EDGE('',*,*,#38522,.F.);
#53196=ORIENTED_EDGE('',*,*,#38523,.F.);
#53197=ORIENTED_EDGE('',*,*,#38335,.T.);
#53198=ORIENTED_EDGE('',*,*,#38523,.T.);
#53199=ORIENTED_EDGE('',*,*,#38524,.F.);
#53200=ORIENTED_EDGE('',*,*,#38333,.T.);
#53201=ORIENTED_EDGE('',*,*,#38341,.T.);
#53202=ORIENTED_EDGE('',*,*,#38336,.T.);
#53203=ORIENTED_EDGE('',*,*,#38525,.F.);
#53204=ORIENTED_EDGE('',*,*,#38526,.F.);
#53205=ORIENTED_EDGE('',*,*,#38342,.T.);
#53206=ORIENTED_EDGE('',*,*,#38526,.T.);
#53207=ORIENTED_EDGE('',*,*,#38527,.F.);
#53208=ORIENTED_EDGE('',*,*,#38340,.T.);
#53209=ORIENTED_EDGE('',*,*,#38348,.T.);
#53210=ORIENTED_EDGE('',*,*,#38343,.T.);
#53211=ORIENTED_EDGE('',*,*,#38528,.F.);
#53212=ORIENTED_EDGE('',*,*,#38529,.F.);
#53213=ORIENTED_EDGE('',*,*,#38349,.T.);
#53214=ORIENTED_EDGE('',*,*,#38529,.T.);
#53215=ORIENTED_EDGE('',*,*,#38530,.F.);
#53216=ORIENTED_EDGE('',*,*,#38347,.T.);
#53217=ORIENTED_EDGE('',*,*,#38531,.F.);
#53218=ORIENTED_EDGE('',*,*,#38532,.F.);
#53219=ORIENTED_EDGE('',*,*,#38355,.T.);
#53220=ORIENTED_EDGE('',*,*,#38350,.T.);
#53221=ORIENTED_EDGE('',*,*,#38356,.T.);
#53222=ORIENTED_EDGE('',*,*,#38532,.T.);
#53223=ORIENTED_EDGE('',*,*,#38533,.F.);
#53224=ORIENTED_EDGE('',*,*,#38354,.T.);
#53225=ORIENTED_EDGE('',*,*,#38358,.T.);
#53226=ORIENTED_EDGE('',*,*,#38360,.T.);
#53227=ORIENTED_EDGE('',*,*,#38534,.F.);
#53228=ORIENTED_EDGE('',*,*,#38448,.T.);
#53229=ORIENTED_EDGE('',*,*,#38535,.T.);
#53230=ORIENTED_EDGE('',*,*,#38536,.F.);
#53231=ORIENTED_EDGE('',*,*,#38361,.T.);
#53232=ORIENTED_EDGE('',*,*,#38537,.F.);
#53233=ORIENTED_EDGE('',*,*,#38538,.F.);
#53234=ORIENTED_EDGE('',*,*,#38539,.F.);
#53235=ORIENTED_EDGE('',*,*,#38540,.F.);
#53236=ORIENTED_EDGE('',*,*,#38535,.F.);
#53237=ORIENTED_EDGE('',*,*,#38540,.T.);
#53238=ORIENTED_EDGE('',*,*,#38541,.F.);
#53239=ORIENTED_EDGE('',*,*,#38363,.T.);
#53240=ORIENTED_EDGE('',*,*,#38536,.T.);
#53241=ORIENTED_EDGE('',*,*,#38542,.T.);
#53242=ORIENTED_EDGE('',*,*,#38543,.F.);
#53243=ORIENTED_EDGE('',*,*,#38365,.T.);
#53244=ORIENTED_EDGE('',*,*,#38544,.F.);
#53245=ORIENTED_EDGE('',*,*,#38545,.F.);
#53246=ORIENTED_EDGE('',*,*,#38546,.F.);
#53247=ORIENTED_EDGE('',*,*,#38547,.F.);
#53248=ORIENTED_EDGE('',*,*,#38542,.F.);
#53249=ORIENTED_EDGE('',*,*,#38547,.T.);
#53250=ORIENTED_EDGE('',*,*,#38548,.F.);
#53251=ORIENTED_EDGE('',*,*,#38366,.T.);
#53252=ORIENTED_EDGE('',*,*,#38543,.T.);
#53253=ORIENTED_EDGE('',*,*,#38549,.T.);
#53254=ORIENTED_EDGE('',*,*,#38550,.F.);
#53255=ORIENTED_EDGE('',*,*,#38368,.T.);
#53256=ORIENTED_EDGE('',*,*,#38551,.F.);
#53257=ORIENTED_EDGE('',*,*,#38552,.F.);
#53258=ORIENTED_EDGE('',*,*,#38553,.F.);
#53259=ORIENTED_EDGE('',*,*,#38554,.F.);
#53260=ORIENTED_EDGE('',*,*,#38549,.F.);
#53261=ORIENTED_EDGE('',*,*,#38554,.T.);
#53262=ORIENTED_EDGE('',*,*,#38555,.F.);
#53263=ORIENTED_EDGE('',*,*,#38369,.T.);
#53264=ORIENTED_EDGE('',*,*,#38550,.T.);
#53265=ORIENTED_EDGE('',*,*,#38556,.T.);
#53266=ORIENTED_EDGE('',*,*,#38557,.F.);
#53267=ORIENTED_EDGE('',*,*,#38371,.T.);
#53268=ORIENTED_EDGE('',*,*,#38558,.F.);
#53269=ORIENTED_EDGE('',*,*,#38559,.F.);
#53270=ORIENTED_EDGE('',*,*,#38560,.F.);
#53271=ORIENTED_EDGE('',*,*,#38561,.F.);
#53272=ORIENTED_EDGE('',*,*,#38556,.F.);
#53273=ORIENTED_EDGE('',*,*,#38561,.T.);
#53274=ORIENTED_EDGE('',*,*,#38562,.F.);
#53275=ORIENTED_EDGE('',*,*,#38372,.T.);
#53276=ORIENTED_EDGE('',*,*,#38557,.T.);
#53277=ORIENTED_EDGE('',*,*,#38563,.T.);
#53278=ORIENTED_EDGE('',*,*,#38564,.F.);
#53279=ORIENTED_EDGE('',*,*,#38374,.T.);
#53280=ORIENTED_EDGE('',*,*,#38565,.F.);
#53281=ORIENTED_EDGE('',*,*,#38566,.F.);
#53282=ORIENTED_EDGE('',*,*,#38567,.F.);
#53283=ORIENTED_EDGE('',*,*,#38568,.F.);
#53284=ORIENTED_EDGE('',*,*,#38563,.F.);
#53285=ORIENTED_EDGE('',*,*,#38568,.T.);
#53286=ORIENTED_EDGE('',*,*,#38569,.F.);
#53287=ORIENTED_EDGE('',*,*,#38375,.T.);
#53288=ORIENTED_EDGE('',*,*,#38564,.T.);
#53289=ORIENTED_EDGE('',*,*,#38570,.T.);
#53290=ORIENTED_EDGE('',*,*,#38571,.F.);
#53291=ORIENTED_EDGE('',*,*,#38377,.T.);
#53292=ORIENTED_EDGE('',*,*,#38572,.F.);
#53293=ORIENTED_EDGE('',*,*,#38573,.F.);
#53294=ORIENTED_EDGE('',*,*,#38574,.F.);
#53295=ORIENTED_EDGE('',*,*,#38575,.F.);
#53296=ORIENTED_EDGE('',*,*,#38570,.F.);
#53297=ORIENTED_EDGE('',*,*,#38575,.T.);
#53298=ORIENTED_EDGE('',*,*,#38576,.F.);
#53299=ORIENTED_EDGE('',*,*,#38378,.T.);
#53300=ORIENTED_EDGE('',*,*,#38571,.T.);
#53301=ORIENTED_EDGE('',*,*,#38577,.T.);
#53302=ORIENTED_EDGE('',*,*,#38578,.F.);
#53303=ORIENTED_EDGE('',*,*,#38380,.T.);
#53304=ORIENTED_EDGE('',*,*,#38579,.F.);
#53305=ORIENTED_EDGE('',*,*,#38580,.F.);
#53306=ORIENTED_EDGE('',*,*,#38581,.F.);
#53307=ORIENTED_EDGE('',*,*,#38582,.F.);
#53308=ORIENTED_EDGE('',*,*,#38577,.F.);
#53309=ORIENTED_EDGE('',*,*,#38582,.T.);
#53310=ORIENTED_EDGE('',*,*,#38583,.F.);
#53311=ORIENTED_EDGE('',*,*,#38381,.T.);
#53312=ORIENTED_EDGE('',*,*,#38578,.T.);
#53313=ORIENTED_EDGE('',*,*,#38584,.T.);
#53314=ORIENTED_EDGE('',*,*,#38585,.F.);
#53315=ORIENTED_EDGE('',*,*,#38383,.T.);
#53316=ORIENTED_EDGE('',*,*,#38586,.F.);
#53317=ORIENTED_EDGE('',*,*,#38587,.F.);
#53318=ORIENTED_EDGE('',*,*,#38588,.F.);
#53319=ORIENTED_EDGE('',*,*,#38589,.F.);
#53320=ORIENTED_EDGE('',*,*,#38584,.F.);
#53321=ORIENTED_EDGE('',*,*,#38589,.T.);
#53322=ORIENTED_EDGE('',*,*,#38590,.F.);
#53323=ORIENTED_EDGE('',*,*,#38384,.T.);
#53324=ORIENTED_EDGE('',*,*,#38585,.T.);
#53325=ORIENTED_EDGE('',*,*,#38591,.T.);
#53326=ORIENTED_EDGE('',*,*,#38592,.F.);
#53327=ORIENTED_EDGE('',*,*,#38386,.T.);
#53328=ORIENTED_EDGE('',*,*,#38593,.F.);
#53329=ORIENTED_EDGE('',*,*,#38594,.F.);
#53330=ORIENTED_EDGE('',*,*,#38595,.F.);
#53331=ORIENTED_EDGE('',*,*,#38596,.F.);
#53332=ORIENTED_EDGE('',*,*,#38591,.F.);
#53333=ORIENTED_EDGE('',*,*,#38596,.T.);
#53334=ORIENTED_EDGE('',*,*,#38597,.F.);
#53335=ORIENTED_EDGE('',*,*,#38387,.T.);
#53336=ORIENTED_EDGE('',*,*,#38592,.T.);
#53337=ORIENTED_EDGE('',*,*,#38598,.T.);
#53338=ORIENTED_EDGE('',*,*,#38599,.F.);
#53339=ORIENTED_EDGE('',*,*,#38389,.T.);
#53340=ORIENTED_EDGE('',*,*,#38600,.F.);
#53341=ORIENTED_EDGE('',*,*,#38601,.F.);
#53342=ORIENTED_EDGE('',*,*,#38602,.F.);
#53343=ORIENTED_EDGE('',*,*,#38603,.F.);
#53344=ORIENTED_EDGE('',*,*,#38598,.F.);
#53345=ORIENTED_EDGE('',*,*,#38603,.T.);
#53346=ORIENTED_EDGE('',*,*,#38604,.F.);
#53347=ORIENTED_EDGE('',*,*,#38390,.T.);
#53348=ORIENTED_EDGE('',*,*,#38599,.T.);
#53349=ORIENTED_EDGE('',*,*,#38605,.T.);
#53350=ORIENTED_EDGE('',*,*,#38606,.F.);
#53351=ORIENTED_EDGE('',*,*,#38392,.T.);
#53352=ORIENTED_EDGE('',*,*,#38607,.F.);
#53353=ORIENTED_EDGE('',*,*,#38608,.F.);
#53354=ORIENTED_EDGE('',*,*,#38609,.F.);
#53355=ORIENTED_EDGE('',*,*,#38610,.F.);
#53356=ORIENTED_EDGE('',*,*,#38605,.F.);
#53357=ORIENTED_EDGE('',*,*,#38610,.T.);
#53358=ORIENTED_EDGE('',*,*,#38611,.F.);
#53359=ORIENTED_EDGE('',*,*,#38393,.T.);
#53360=ORIENTED_EDGE('',*,*,#38606,.T.);
#53361=ORIENTED_EDGE('',*,*,#38612,.T.);
#53362=ORIENTED_EDGE('',*,*,#38613,.F.);
#53363=ORIENTED_EDGE('',*,*,#38395,.T.);
#53364=ORIENTED_EDGE('',*,*,#38614,.F.);
#53365=ORIENTED_EDGE('',*,*,#38615,.F.);
#53366=ORIENTED_EDGE('',*,*,#38616,.F.);
#53367=ORIENTED_EDGE('',*,*,#38617,.F.);
#53368=ORIENTED_EDGE('',*,*,#38612,.F.);
#53369=ORIENTED_EDGE('',*,*,#38617,.T.);
#53370=ORIENTED_EDGE('',*,*,#38618,.F.);
#53371=ORIENTED_EDGE('',*,*,#38396,.T.);
#53372=ORIENTED_EDGE('',*,*,#38613,.T.);
#53373=ORIENTED_EDGE('',*,*,#38619,.T.);
#53374=ORIENTED_EDGE('',*,*,#38620,.F.);
#53375=ORIENTED_EDGE('',*,*,#38398,.T.);
#53376=ORIENTED_EDGE('',*,*,#38621,.F.);
#53377=ORIENTED_EDGE('',*,*,#38622,.F.);
#53378=ORIENTED_EDGE('',*,*,#38623,.F.);
#53379=ORIENTED_EDGE('',*,*,#38624,.F.);
#53380=ORIENTED_EDGE('',*,*,#38619,.F.);
#53381=ORIENTED_EDGE('',*,*,#38624,.T.);
#53382=ORIENTED_EDGE('',*,*,#38625,.F.);
#53383=ORIENTED_EDGE('',*,*,#38399,.T.);
#53384=ORIENTED_EDGE('',*,*,#38620,.T.);
#53385=ORIENTED_EDGE('',*,*,#38626,.T.);
#53386=ORIENTED_EDGE('',*,*,#38627,.F.);
#53387=ORIENTED_EDGE('',*,*,#38401,.T.);
#53388=ORIENTED_EDGE('',*,*,#38628,.F.);
#53389=ORIENTED_EDGE('',*,*,#38629,.F.);
#53390=ORIENTED_EDGE('',*,*,#38630,.F.);
#53391=ORIENTED_EDGE('',*,*,#38631,.F.);
#53392=ORIENTED_EDGE('',*,*,#38626,.F.);
#53393=ORIENTED_EDGE('',*,*,#38631,.T.);
#53394=ORIENTED_EDGE('',*,*,#38632,.F.);
#53395=ORIENTED_EDGE('',*,*,#38402,.T.);
#53396=ORIENTED_EDGE('',*,*,#38627,.T.);
#53397=ORIENTED_EDGE('',*,*,#34413,.T.);
#53398=ORIENTED_EDGE('',*,*,#38633,.F.);
#53399=ORIENTED_EDGE('',*,*,#38404,.T.);
#53400=ORIENTED_EDGE('',*,*,#38634,.F.);
#53401=ORIENTED_EDGE('',*,*,#34416,.T.);
#53402=ORIENTED_EDGE('',*,*,#38635,.F.);
#53403=ORIENTED_EDGE('',*,*,#38405,.T.);
#53404=ORIENTED_EDGE('',*,*,#38633,.T.);
#53405=ORIENTED_EDGE('',*,*,#38636,.T.);
#53406=ORIENTED_EDGE('',*,*,#38637,.F.);
#53407=ORIENTED_EDGE('',*,*,#38407,.T.);
#53408=ORIENTED_EDGE('',*,*,#38638,.F.);
#53409=ORIENTED_EDGE('',*,*,#38639,.F.);
#53410=ORIENTED_EDGE('',*,*,#38640,.F.);
#53411=ORIENTED_EDGE('',*,*,#38641,.F.);
#53412=ORIENTED_EDGE('',*,*,#38636,.F.);
#53413=ORIENTED_EDGE('',*,*,#38641,.T.);
#53414=ORIENTED_EDGE('',*,*,#38642,.F.);
#53415=ORIENTED_EDGE('',*,*,#38408,.T.);
#53416=ORIENTED_EDGE('',*,*,#38637,.T.);
#53417=ORIENTED_EDGE('',*,*,#38643,.T.);
#53418=ORIENTED_EDGE('',*,*,#38644,.F.);
#53419=ORIENTED_EDGE('',*,*,#38410,.T.);
#53420=ORIENTED_EDGE('',*,*,#38645,.F.);
#53421=ORIENTED_EDGE('',*,*,#38646,.F.);
#53422=ORIENTED_EDGE('',*,*,#38647,.F.);
#53423=ORIENTED_EDGE('',*,*,#38648,.F.);
#53424=ORIENTED_EDGE('',*,*,#38643,.F.);
#53425=ORIENTED_EDGE('',*,*,#38648,.T.);
#53426=ORIENTED_EDGE('',*,*,#38649,.F.);
#53427=ORIENTED_EDGE('',*,*,#38411,.T.);
#53428=ORIENTED_EDGE('',*,*,#38644,.T.);
#53429=ORIENTED_EDGE('',*,*,#38650,.T.);
#53430=ORIENTED_EDGE('',*,*,#38651,.F.);
#53431=ORIENTED_EDGE('',*,*,#38413,.T.);
#53432=ORIENTED_EDGE('',*,*,#38652,.F.);
#53433=ORIENTED_EDGE('',*,*,#38653,.F.);
#53434=ORIENTED_EDGE('',*,*,#38654,.F.);
#53435=ORIENTED_EDGE('',*,*,#38655,.F.);
#53436=ORIENTED_EDGE('',*,*,#38650,.F.);
#53437=ORIENTED_EDGE('',*,*,#38655,.T.);
#53438=ORIENTED_EDGE('',*,*,#38656,.F.);
#53439=ORIENTED_EDGE('',*,*,#38414,.T.);
#53440=ORIENTED_EDGE('',*,*,#38651,.T.);
#53441=ORIENTED_EDGE('',*,*,#38657,.T.);
#53442=ORIENTED_EDGE('',*,*,#38658,.F.);
#53443=ORIENTED_EDGE('',*,*,#38416,.T.);
#53444=ORIENTED_EDGE('',*,*,#38659,.F.);
#53445=ORIENTED_EDGE('',*,*,#38660,.F.);
#53446=ORIENTED_EDGE('',*,*,#38661,.F.);
#53447=ORIENTED_EDGE('',*,*,#38662,.F.);
#53448=ORIENTED_EDGE('',*,*,#38657,.F.);
#53449=ORIENTED_EDGE('',*,*,#38662,.T.);
#53450=ORIENTED_EDGE('',*,*,#38663,.F.);
#53451=ORIENTED_EDGE('',*,*,#38417,.T.);
#53452=ORIENTED_EDGE('',*,*,#38658,.T.);
#53453=ORIENTED_EDGE('',*,*,#38664,.T.);
#53454=ORIENTED_EDGE('',*,*,#38665,.F.);
#53455=ORIENTED_EDGE('',*,*,#38419,.T.);
#53456=ORIENTED_EDGE('',*,*,#38666,.F.);
#53457=ORIENTED_EDGE('',*,*,#38667,.F.);
#53458=ORIENTED_EDGE('',*,*,#38668,.F.);
#53459=ORIENTED_EDGE('',*,*,#38669,.F.);
#53460=ORIENTED_EDGE('',*,*,#38664,.F.);
#53461=ORIENTED_EDGE('',*,*,#38669,.T.);
#53462=ORIENTED_EDGE('',*,*,#38670,.F.);
#53463=ORIENTED_EDGE('',*,*,#38420,.T.);
#53464=ORIENTED_EDGE('',*,*,#38665,.T.);
#53465=ORIENTED_EDGE('',*,*,#38671,.T.);
#53466=ORIENTED_EDGE('',*,*,#38672,.F.);
#53467=ORIENTED_EDGE('',*,*,#38422,.T.);
#53468=ORIENTED_EDGE('',*,*,#38673,.F.);
#53469=ORIENTED_EDGE('',*,*,#38674,.F.);
#53470=ORIENTED_EDGE('',*,*,#38675,.F.);
#53471=ORIENTED_EDGE('',*,*,#38676,.F.);
#53472=ORIENTED_EDGE('',*,*,#38671,.F.);
#53473=ORIENTED_EDGE('',*,*,#38676,.T.);
#53474=ORIENTED_EDGE('',*,*,#38677,.F.);
#53475=ORIENTED_EDGE('',*,*,#38423,.T.);
#53476=ORIENTED_EDGE('',*,*,#38672,.T.);
#53477=ORIENTED_EDGE('',*,*,#38678,.T.);
#53478=ORIENTED_EDGE('',*,*,#38679,.F.);
#53479=ORIENTED_EDGE('',*,*,#38425,.T.);
#53480=ORIENTED_EDGE('',*,*,#38680,.F.);
#53481=ORIENTED_EDGE('',*,*,#38681,.T.);
#53482=ORIENTED_EDGE('',*,*,#38682,.F.);
#53483=ORIENTED_EDGE('',*,*,#38426,.T.);
#53484=ORIENTED_EDGE('',*,*,#38679,.T.);
#53485=ORIENTED_EDGE('',*,*,#38683,.F.);
#53486=ORIENTED_EDGE('',*,*,#38684,.F.);
#53487=ORIENTED_EDGE('',*,*,#38681,.F.);
#53488=ORIENTED_EDGE('',*,*,#38678,.F.);
#53489=ORIENTED_EDGE('',*,*,#38428,.T.);
#53490=ORIENTED_EDGE('',*,*,#38685,.F.);
#53491=ORIENTED_EDGE('',*,*,#38686,.T.);
#53492=ORIENTED_EDGE('',*,*,#38687,.F.);
#53493=ORIENTED_EDGE('',*,*,#38688,.F.);
#53494=ORIENTED_EDGE('',*,*,#38686,.F.);
#53495=ORIENTED_EDGE('',*,*,#38689,.F.);
#53496=ORIENTED_EDGE('',*,*,#38690,.F.);
#53497=ORIENTED_EDGE('',*,*,#38429,.T.);
#53498=ORIENTED_EDGE('',*,*,#38687,.T.);
#53499=ORIENTED_EDGE('',*,*,#38688,.T.);
#53500=ORIENTED_EDGE('',*,*,#38691,.F.);
#53501=ORIENTED_EDGE('',*,*,#38692,.T.);
#53502=ORIENTED_EDGE('',*,*,#38693,.F.);
#53503=ORIENTED_EDGE('',*,*,#38431,.T.);
#53504=ORIENTED_EDGE('',*,*,#38694,.F.);
#53505=ORIENTED_EDGE('',*,*,#38695,.F.);
#53506=ORIENTED_EDGE('',*,*,#38696,.F.);
#53507=ORIENTED_EDGE('',*,*,#38697,.F.);
#53508=ORIENTED_EDGE('',*,*,#38692,.F.);
#53509=ORIENTED_EDGE('',*,*,#38697,.T.);
#53510=ORIENTED_EDGE('',*,*,#38698,.F.);
#53511=ORIENTED_EDGE('',*,*,#38432,.T.);
#53512=ORIENTED_EDGE('',*,*,#38693,.T.);
#53513=ORIENTED_EDGE('',*,*,#38699,.T.);
#53514=ORIENTED_EDGE('',*,*,#38700,.F.);
#53515=ORIENTED_EDGE('',*,*,#38434,.T.);
#53516=ORIENTED_EDGE('',*,*,#38701,.F.);
#53517=ORIENTED_EDGE('',*,*,#38702,.F.);
#53518=ORIENTED_EDGE('',*,*,#38703,.F.);
#53519=ORIENTED_EDGE('',*,*,#38704,.F.);
#53520=ORIENTED_EDGE('',*,*,#38699,.F.);
#53521=ORIENTED_EDGE('',*,*,#38704,.T.);
#53522=ORIENTED_EDGE('',*,*,#38705,.F.);
#53523=ORIENTED_EDGE('',*,*,#38435,.T.);
#53524=ORIENTED_EDGE('',*,*,#38700,.T.);
#53525=ORIENTED_EDGE('',*,*,#38706,.T.);
#53526=ORIENTED_EDGE('',*,*,#38707,.F.);
#53527=ORIENTED_EDGE('',*,*,#38437,.T.);
#53528=ORIENTED_EDGE('',*,*,#38708,.F.);
#53529=ORIENTED_EDGE('',*,*,#38709,.F.);
#53530=ORIENTED_EDGE('',*,*,#38710,.F.);
#53531=ORIENTED_EDGE('',*,*,#38711,.F.);
#53532=ORIENTED_EDGE('',*,*,#38706,.F.);
#53533=ORIENTED_EDGE('',*,*,#38711,.T.);
#53534=ORIENTED_EDGE('',*,*,#38712,.F.);
#53535=ORIENTED_EDGE('',*,*,#38438,.T.);
#53536=ORIENTED_EDGE('',*,*,#38707,.T.);
#53537=ORIENTED_EDGE('',*,*,#38713,.T.);
#53538=ORIENTED_EDGE('',*,*,#38714,.F.);
#53539=ORIENTED_EDGE('',*,*,#38440,.T.);
#53540=ORIENTED_EDGE('',*,*,#38715,.F.);
#53541=ORIENTED_EDGE('',*,*,#38716,.F.);
#53542=ORIENTED_EDGE('',*,*,#38717,.F.);
#53543=ORIENTED_EDGE('',*,*,#38718,.F.);
#53544=ORIENTED_EDGE('',*,*,#38713,.F.);
#53545=ORIENTED_EDGE('',*,*,#38718,.T.);
#53546=ORIENTED_EDGE('',*,*,#38719,.F.);
#53547=ORIENTED_EDGE('',*,*,#38441,.T.);
#53548=ORIENTED_EDGE('',*,*,#38714,.T.);
#53549=ORIENTED_EDGE('',*,*,#38720,.T.);
#53550=ORIENTED_EDGE('',*,*,#38721,.F.);
#53551=ORIENTED_EDGE('',*,*,#38443,.T.);
#53552=ORIENTED_EDGE('',*,*,#38722,.F.);
#53553=ORIENTED_EDGE('',*,*,#38723,.F.);
#53554=ORIENTED_EDGE('',*,*,#38724,.F.);
#53555=ORIENTED_EDGE('',*,*,#38725,.F.);
#53556=ORIENTED_EDGE('',*,*,#38720,.F.);
#53557=ORIENTED_EDGE('',*,*,#38725,.T.);
#53558=ORIENTED_EDGE('',*,*,#38726,.F.);
#53559=ORIENTED_EDGE('',*,*,#38444,.T.);
#53560=ORIENTED_EDGE('',*,*,#38721,.T.);
#53561=ORIENTED_EDGE('',*,*,#38727,.T.);
#53562=ORIENTED_EDGE('',*,*,#38728,.F.);
#53563=ORIENTED_EDGE('',*,*,#38446,.T.);
#53564=ORIENTED_EDGE('',*,*,#38729,.F.);
#53565=ORIENTED_EDGE('',*,*,#38730,.F.);
#53566=ORIENTED_EDGE('',*,*,#38731,.F.);
#53567=ORIENTED_EDGE('',*,*,#38732,.F.);
#53568=ORIENTED_EDGE('',*,*,#38727,.F.);
#53569=ORIENTED_EDGE('',*,*,#38732,.T.);
#53570=ORIENTED_EDGE('',*,*,#38733,.F.);
#53571=ORIENTED_EDGE('',*,*,#38447,.T.);
#53572=ORIENTED_EDGE('',*,*,#38728,.T.);
#53573=ORIENTED_EDGE('',*,*,#38449,.T.);
#53574=ORIENTED_EDGE('',*,*,#38734,.F.);
#53575=ORIENTED_EDGE('',*,*,#38735,.T.);
#53576=ORIENTED_EDGE('',*,*,#38736,.F.);
#53577=ORIENTED_EDGE('',*,*,#38450,.T.);
#53578=ORIENTED_EDGE('',*,*,#38736,.T.);
#53579=ORIENTED_EDGE('',*,*,#38737,.T.);
#53580=ORIENTED_EDGE('',*,*,#38738,.F.);
#53581=ORIENTED_EDGE('',*,*,#38737,.F.);
#53582=ORIENTED_EDGE('',*,*,#38735,.F.);
#53583=ORIENTED_EDGE('',*,*,#38739,.F.);
#53584=ORIENTED_EDGE('',*,*,#38740,.F.);
#53585=ORIENTED_EDGE('',*,*,#38452,.T.);
#53586=ORIENTED_EDGE('',*,*,#38741,.F.);
#53587=ORIENTED_EDGE('',*,*,#38742,.T.);
#53588=ORIENTED_EDGE('',*,*,#38743,.F.);
#53589=ORIENTED_EDGE('',*,*,#38453,.T.);
#53590=ORIENTED_EDGE('',*,*,#38743,.T.);
#53591=ORIENTED_EDGE('',*,*,#38744,.T.);
#53592=ORIENTED_EDGE('',*,*,#38745,.F.);
#53593=ORIENTED_EDGE('',*,*,#38744,.F.);
#53594=ORIENTED_EDGE('',*,*,#38742,.F.);
#53595=ORIENTED_EDGE('',*,*,#38746,.F.);
#53596=ORIENTED_EDGE('',*,*,#38747,.F.);
#53597=ORIENTED_EDGE('',*,*,#38455,.T.);
#53598=ORIENTED_EDGE('',*,*,#38748,.F.);
#53599=ORIENTED_EDGE('',*,*,#38749,.T.);
#53600=ORIENTED_EDGE('',*,*,#38750,.F.);
#53601=ORIENTED_EDGE('',*,*,#38456,.T.);
#53602=ORIENTED_EDGE('',*,*,#38750,.T.);
#53603=ORIENTED_EDGE('',*,*,#38751,.T.);
#53604=ORIENTED_EDGE('',*,*,#38752,.F.);
#53605=ORIENTED_EDGE('',*,*,#38751,.F.);
#53606=ORIENTED_EDGE('',*,*,#38749,.F.);
#53607=ORIENTED_EDGE('',*,*,#38753,.F.);
#53608=ORIENTED_EDGE('',*,*,#38754,.F.);
#53609=ORIENTED_EDGE('',*,*,#38458,.T.);
#53610=ORIENTED_EDGE('',*,*,#38755,.F.);
#53611=ORIENTED_EDGE('',*,*,#38756,.T.);
#53612=ORIENTED_EDGE('',*,*,#38757,.F.);
#53613=ORIENTED_EDGE('',*,*,#38459,.T.);
#53614=ORIENTED_EDGE('',*,*,#38757,.T.);
#53615=ORIENTED_EDGE('',*,*,#38758,.T.);
#53616=ORIENTED_EDGE('',*,*,#38759,.F.);
#53617=ORIENTED_EDGE('',*,*,#38758,.F.);
#53618=ORIENTED_EDGE('',*,*,#38756,.F.);
#53619=ORIENTED_EDGE('',*,*,#38760,.F.);
#53620=ORIENTED_EDGE('',*,*,#38761,.F.);
#53621=ORIENTED_EDGE('',*,*,#38461,.T.);
#53622=ORIENTED_EDGE('',*,*,#38762,.F.);
#53623=ORIENTED_EDGE('',*,*,#38763,.T.);
#53624=ORIENTED_EDGE('',*,*,#38764,.F.);
#53625=ORIENTED_EDGE('',*,*,#38462,.T.);
#53626=ORIENTED_EDGE('',*,*,#38764,.T.);
#53627=ORIENTED_EDGE('',*,*,#38765,.T.);
#53628=ORIENTED_EDGE('',*,*,#38766,.F.);
#53629=ORIENTED_EDGE('',*,*,#38765,.F.);
#53630=ORIENTED_EDGE('',*,*,#38763,.F.);
#53631=ORIENTED_EDGE('',*,*,#38767,.F.);
#53632=ORIENTED_EDGE('',*,*,#38768,.F.);
#53633=ORIENTED_EDGE('',*,*,#38464,.T.);
#53634=ORIENTED_EDGE('',*,*,#38769,.F.);
#53635=ORIENTED_EDGE('',*,*,#38770,.T.);
#53636=ORIENTED_EDGE('',*,*,#38771,.F.);
#53637=ORIENTED_EDGE('',*,*,#38465,.T.);
#53638=ORIENTED_EDGE('',*,*,#38771,.T.);
#53639=ORIENTED_EDGE('',*,*,#38772,.T.);
#53640=ORIENTED_EDGE('',*,*,#38773,.F.);
#53641=ORIENTED_EDGE('',*,*,#38772,.F.);
#53642=ORIENTED_EDGE('',*,*,#38770,.F.);
#53643=ORIENTED_EDGE('',*,*,#38774,.F.);
#53644=ORIENTED_EDGE('',*,*,#38775,.F.);
#53645=ORIENTED_EDGE('',*,*,#38467,.T.);
#53646=ORIENTED_EDGE('',*,*,#38776,.F.);
#53647=ORIENTED_EDGE('',*,*,#38777,.T.);
#53648=ORIENTED_EDGE('',*,*,#38778,.F.);
#53649=ORIENTED_EDGE('',*,*,#38468,.T.);
#53650=ORIENTED_EDGE('',*,*,#38778,.T.);
#53651=ORIENTED_EDGE('',*,*,#38779,.T.);
#53652=ORIENTED_EDGE('',*,*,#38780,.F.);
#53653=ORIENTED_EDGE('',*,*,#38779,.F.);
#53654=ORIENTED_EDGE('',*,*,#38777,.F.);
#53655=ORIENTED_EDGE('',*,*,#38781,.F.);
#53656=ORIENTED_EDGE('',*,*,#38782,.F.);
#53657=ORIENTED_EDGE('',*,*,#38470,.T.);
#53658=ORIENTED_EDGE('',*,*,#38783,.F.);
#53659=ORIENTED_EDGE('',*,*,#38784,.T.);
#53660=ORIENTED_EDGE('',*,*,#38785,.F.);
#53661=ORIENTED_EDGE('',*,*,#38471,.T.);
#53662=ORIENTED_EDGE('',*,*,#38785,.T.);
#53663=ORIENTED_EDGE('',*,*,#38786,.T.);
#53664=ORIENTED_EDGE('',*,*,#38787,.F.);
#53665=ORIENTED_EDGE('',*,*,#38786,.F.);
#53666=ORIENTED_EDGE('',*,*,#38784,.F.);
#53667=ORIENTED_EDGE('',*,*,#38788,.F.);
#53668=ORIENTED_EDGE('',*,*,#38789,.F.);
#53669=ORIENTED_EDGE('',*,*,#38473,.T.);
#53670=ORIENTED_EDGE('',*,*,#38790,.F.);
#53671=ORIENTED_EDGE('',*,*,#38791,.T.);
#53672=ORIENTED_EDGE('',*,*,#38792,.F.);
#53673=ORIENTED_EDGE('',*,*,#38474,.T.);
#53674=ORIENTED_EDGE('',*,*,#38792,.T.);
#53675=ORIENTED_EDGE('',*,*,#38793,.T.);
#53676=ORIENTED_EDGE('',*,*,#38794,.F.);
#53677=ORIENTED_EDGE('',*,*,#38793,.F.);
#53678=ORIENTED_EDGE('',*,*,#38791,.F.);
#53679=ORIENTED_EDGE('',*,*,#38795,.F.);
#53680=ORIENTED_EDGE('',*,*,#38796,.F.);
#53681=ORIENTED_EDGE('',*,*,#38476,.T.);
#53682=ORIENTED_EDGE('',*,*,#38797,.F.);
#53683=ORIENTED_EDGE('',*,*,#38798,.T.);
#53684=ORIENTED_EDGE('',*,*,#38799,.F.);
#53685=ORIENTED_EDGE('',*,*,#38477,.T.);
#53686=ORIENTED_EDGE('',*,*,#38799,.T.);
#53687=ORIENTED_EDGE('',*,*,#38800,.T.);
#53688=ORIENTED_EDGE('',*,*,#38801,.F.);
#53689=ORIENTED_EDGE('',*,*,#38800,.F.);
#53690=ORIENTED_EDGE('',*,*,#38798,.F.);
#53691=ORIENTED_EDGE('',*,*,#38802,.F.);
#53692=ORIENTED_EDGE('',*,*,#38803,.F.);
#53693=ORIENTED_EDGE('',*,*,#38479,.T.);
#53694=ORIENTED_EDGE('',*,*,#38804,.F.);
#53695=ORIENTED_EDGE('',*,*,#38805,.T.);
#53696=ORIENTED_EDGE('',*,*,#38806,.F.);
#53697=ORIENTED_EDGE('',*,*,#38480,.T.);
#53698=ORIENTED_EDGE('',*,*,#38806,.T.);
#53699=ORIENTED_EDGE('',*,*,#38807,.T.);
#53700=ORIENTED_EDGE('',*,*,#38808,.F.);
#53701=ORIENTED_EDGE('',*,*,#38807,.F.);
#53702=ORIENTED_EDGE('',*,*,#38805,.F.);
#53703=ORIENTED_EDGE('',*,*,#38809,.F.);
#53704=ORIENTED_EDGE('',*,*,#38810,.F.);
#53705=ORIENTED_EDGE('',*,*,#38482,.T.);
#53706=ORIENTED_EDGE('',*,*,#38811,.F.);
#53707=ORIENTED_EDGE('',*,*,#38812,.T.);
#53708=ORIENTED_EDGE('',*,*,#38813,.F.);
#53709=ORIENTED_EDGE('',*,*,#38483,.T.);
#53710=ORIENTED_EDGE('',*,*,#38813,.T.);
#53711=ORIENTED_EDGE('',*,*,#38814,.T.);
#53712=ORIENTED_EDGE('',*,*,#38815,.F.);
#53713=ORIENTED_EDGE('',*,*,#38814,.F.);
#53714=ORIENTED_EDGE('',*,*,#38812,.F.);
#53715=ORIENTED_EDGE('',*,*,#38816,.F.);
#53716=ORIENTED_EDGE('',*,*,#38817,.F.);
#53717=ORIENTED_EDGE('',*,*,#38485,.T.);
#53718=ORIENTED_EDGE('',*,*,#38818,.F.);
#53719=ORIENTED_EDGE('',*,*,#38819,.T.);
#53720=ORIENTED_EDGE('',*,*,#38820,.F.);
#53721=ORIENTED_EDGE('',*,*,#38486,.T.);
#53722=ORIENTED_EDGE('',*,*,#38820,.T.);
#53723=ORIENTED_EDGE('',*,*,#38821,.T.);
#53724=ORIENTED_EDGE('',*,*,#38822,.F.);
#53725=ORIENTED_EDGE('',*,*,#38821,.F.);
#53726=ORIENTED_EDGE('',*,*,#38819,.F.);
#53727=ORIENTED_EDGE('',*,*,#38823,.F.);
#53728=ORIENTED_EDGE('',*,*,#38824,.F.);
#53729=ORIENTED_EDGE('',*,*,#38488,.T.);
#53730=ORIENTED_EDGE('',*,*,#38825,.F.);
#53731=ORIENTED_EDGE('',*,*,#38826,.T.);
#53732=ORIENTED_EDGE('',*,*,#38827,.F.);
#53733=ORIENTED_EDGE('',*,*,#38489,.T.);
#53734=ORIENTED_EDGE('',*,*,#38827,.T.);
#53735=ORIENTED_EDGE('',*,*,#38828,.T.);
#53736=ORIENTED_EDGE('',*,*,#38829,.F.);
#53737=ORIENTED_EDGE('',*,*,#38828,.F.);
#53738=ORIENTED_EDGE('',*,*,#38826,.F.);
#53739=ORIENTED_EDGE('',*,*,#38830,.F.);
#53740=ORIENTED_EDGE('',*,*,#38831,.F.);
#53741=ORIENTED_EDGE('',*,*,#38491,.T.);
#53742=ORIENTED_EDGE('',*,*,#38832,.F.);
#53743=ORIENTED_EDGE('',*,*,#38833,.T.);
#53744=ORIENTED_EDGE('',*,*,#38834,.F.);
#53745=ORIENTED_EDGE('',*,*,#38492,.T.);
#53746=ORIENTED_EDGE('',*,*,#38834,.T.);
#53747=ORIENTED_EDGE('',*,*,#38835,.T.);
#53748=ORIENTED_EDGE('',*,*,#38836,.F.);
#53749=ORIENTED_EDGE('',*,*,#38835,.F.);
#53750=ORIENTED_EDGE('',*,*,#38833,.F.);
#53751=ORIENTED_EDGE('',*,*,#38837,.F.);
#53752=ORIENTED_EDGE('',*,*,#38838,.F.);
#53753=ORIENTED_EDGE('',*,*,#38494,.T.);
#53754=ORIENTED_EDGE('',*,*,#38839,.F.);
#53755=ORIENTED_EDGE('',*,*,#38840,.T.);
#53756=ORIENTED_EDGE('',*,*,#38841,.F.);
#53757=ORIENTED_EDGE('',*,*,#38495,.T.);
#53758=ORIENTED_EDGE('',*,*,#38841,.T.);
#53759=ORIENTED_EDGE('',*,*,#38842,.T.);
#53760=ORIENTED_EDGE('',*,*,#38843,.F.);
#53761=ORIENTED_EDGE('',*,*,#38842,.F.);
#53762=ORIENTED_EDGE('',*,*,#38840,.F.);
#53763=ORIENTED_EDGE('',*,*,#38844,.F.);
#53764=ORIENTED_EDGE('',*,*,#38845,.F.);
#53765=ORIENTED_EDGE('',*,*,#38497,.T.);
#53766=ORIENTED_EDGE('',*,*,#38846,.F.);
#53767=ORIENTED_EDGE('',*,*,#38847,.T.);
#53768=ORIENTED_EDGE('',*,*,#38848,.F.);
#53769=ORIENTED_EDGE('',*,*,#38498,.T.);
#53770=ORIENTED_EDGE('',*,*,#38848,.T.);
#53771=ORIENTED_EDGE('',*,*,#38849,.T.);
#53772=ORIENTED_EDGE('',*,*,#38850,.F.);
#53773=ORIENTED_EDGE('',*,*,#38849,.F.);
#53774=ORIENTED_EDGE('',*,*,#38847,.F.);
#53775=ORIENTED_EDGE('',*,*,#38851,.F.);
#53776=ORIENTED_EDGE('',*,*,#38852,.F.);
#53777=ORIENTED_EDGE('',*,*,#38500,.T.);
#53778=ORIENTED_EDGE('',*,*,#38853,.F.);
#53779=ORIENTED_EDGE('',*,*,#38854,.T.);
#53780=ORIENTED_EDGE('',*,*,#38855,.F.);
#53781=ORIENTED_EDGE('',*,*,#38501,.T.);
#53782=ORIENTED_EDGE('',*,*,#38855,.T.);
#53783=ORIENTED_EDGE('',*,*,#38856,.T.);
#53784=ORIENTED_EDGE('',*,*,#38857,.F.);
#53785=ORIENTED_EDGE('',*,*,#38856,.F.);
#53786=ORIENTED_EDGE('',*,*,#38854,.F.);
#53787=ORIENTED_EDGE('',*,*,#38858,.F.);
#53788=ORIENTED_EDGE('',*,*,#38859,.F.);
#53789=ORIENTED_EDGE('',*,*,#38503,.T.);
#53790=ORIENTED_EDGE('',*,*,#38860,.F.);
#53791=ORIENTED_EDGE('',*,*,#38861,.T.);
#53792=ORIENTED_EDGE('',*,*,#38862,.F.);
#53793=ORIENTED_EDGE('',*,*,#38504,.T.);
#53794=ORIENTED_EDGE('',*,*,#38862,.T.);
#53795=ORIENTED_EDGE('',*,*,#38863,.T.);
#53796=ORIENTED_EDGE('',*,*,#38864,.F.);
#53797=ORIENTED_EDGE('',*,*,#38863,.F.);
#53798=ORIENTED_EDGE('',*,*,#38861,.F.);
#53799=ORIENTED_EDGE('',*,*,#38865,.F.);
#53800=ORIENTED_EDGE('',*,*,#38866,.F.);
#53801=ORIENTED_EDGE('',*,*,#38506,.T.);
#53802=ORIENTED_EDGE('',*,*,#38867,.F.);
#53803=ORIENTED_EDGE('',*,*,#38868,.T.);
#53804=ORIENTED_EDGE('',*,*,#38869,.F.);
#53805=ORIENTED_EDGE('',*,*,#38507,.T.);
#53806=ORIENTED_EDGE('',*,*,#38869,.T.);
#53807=ORIENTED_EDGE('',*,*,#38870,.T.);
#53808=ORIENTED_EDGE('',*,*,#38871,.F.);
#53809=ORIENTED_EDGE('',*,*,#38870,.F.);
#53810=ORIENTED_EDGE('',*,*,#38868,.F.);
#53811=ORIENTED_EDGE('',*,*,#38872,.F.);
#53812=ORIENTED_EDGE('',*,*,#38873,.F.);
#53813=ORIENTED_EDGE('',*,*,#38509,.T.);
#53814=ORIENTED_EDGE('',*,*,#38874,.F.);
#53815=ORIENTED_EDGE('',*,*,#38875,.T.);
#53816=ORIENTED_EDGE('',*,*,#38876,.F.);
#53817=ORIENTED_EDGE('',*,*,#38510,.T.);
#53818=ORIENTED_EDGE('',*,*,#38876,.T.);
#53819=ORIENTED_EDGE('',*,*,#38877,.T.);
#53820=ORIENTED_EDGE('',*,*,#38878,.F.);
#53821=ORIENTED_EDGE('',*,*,#38877,.F.);
#53822=ORIENTED_EDGE('',*,*,#38875,.F.);
#53823=ORIENTED_EDGE('',*,*,#38879,.F.);
#53824=ORIENTED_EDGE('',*,*,#38880,.F.);
#53825=ORIENTED_EDGE('',*,*,#38512,.T.);
#53826=ORIENTED_EDGE('',*,*,#38881,.F.);
#53827=ORIENTED_EDGE('',*,*,#34412,.T.);
#53828=ORIENTED_EDGE('',*,*,#38882,.F.);
#53829=ORIENTED_EDGE('',*,*,#38513,.T.);
#53830=ORIENTED_EDGE('',*,*,#38882,.T.);
#53831=ORIENTED_EDGE('',*,*,#34411,.T.);
#53832=ORIENTED_EDGE('',*,*,#38883,.F.);
#53833=ORIENTED_EDGE('',*,*,#38515,.T.);
#53834=ORIENTED_EDGE('',*,*,#38884,.F.);
#53835=ORIENTED_EDGE('',*,*,#38885,.T.);
#53836=ORIENTED_EDGE('',*,*,#38886,.F.);
#53837=ORIENTED_EDGE('',*,*,#38516,.T.);
#53838=ORIENTED_EDGE('',*,*,#38886,.T.);
#53839=ORIENTED_EDGE('',*,*,#38887,.T.);
#53840=ORIENTED_EDGE('',*,*,#38888,.F.);
#53841=ORIENTED_EDGE('',*,*,#38887,.F.);
#53842=ORIENTED_EDGE('',*,*,#38885,.F.);
#53843=ORIENTED_EDGE('',*,*,#38889,.F.);
#53844=ORIENTED_EDGE('',*,*,#38890,.F.);
#53845=ORIENTED_EDGE('',*,*,#38518,.T.);
#53846=ORIENTED_EDGE('',*,*,#38891,.F.);
#53847=ORIENTED_EDGE('',*,*,#38892,.T.);
#53848=ORIENTED_EDGE('',*,*,#38893,.F.);
#53849=ORIENTED_EDGE('',*,*,#38519,.T.);
#53850=ORIENTED_EDGE('',*,*,#38893,.T.);
#53851=ORIENTED_EDGE('',*,*,#38894,.T.);
#53852=ORIENTED_EDGE('',*,*,#38895,.F.);
#53853=ORIENTED_EDGE('',*,*,#38894,.F.);
#53854=ORIENTED_EDGE('',*,*,#38892,.F.);
#53855=ORIENTED_EDGE('',*,*,#38896,.F.);
#53856=ORIENTED_EDGE('',*,*,#38897,.F.);
#53857=ORIENTED_EDGE('',*,*,#38521,.T.);
#53858=ORIENTED_EDGE('',*,*,#38898,.F.);
#53859=ORIENTED_EDGE('',*,*,#38899,.T.);
#53860=ORIENTED_EDGE('',*,*,#38900,.F.);
#53861=ORIENTED_EDGE('',*,*,#38522,.T.);
#53862=ORIENTED_EDGE('',*,*,#38900,.T.);
#53863=ORIENTED_EDGE('',*,*,#38901,.T.);
#53864=ORIENTED_EDGE('',*,*,#38902,.F.);
#53865=ORIENTED_EDGE('',*,*,#38901,.F.);
#53866=ORIENTED_EDGE('',*,*,#38899,.F.);
#53867=ORIENTED_EDGE('',*,*,#38903,.F.);
#53868=ORIENTED_EDGE('',*,*,#38904,.F.);
#53869=ORIENTED_EDGE('',*,*,#38524,.T.);
#53870=ORIENTED_EDGE('',*,*,#38905,.F.);
#53871=ORIENTED_EDGE('',*,*,#38906,.T.);
#53872=ORIENTED_EDGE('',*,*,#38907,.F.);
#53873=ORIENTED_EDGE('',*,*,#38525,.T.);
#53874=ORIENTED_EDGE('',*,*,#38907,.T.);
#53875=ORIENTED_EDGE('',*,*,#38908,.T.);
#53876=ORIENTED_EDGE('',*,*,#38909,.F.);
#53877=ORIENTED_EDGE('',*,*,#38908,.F.);
#53878=ORIENTED_EDGE('',*,*,#38906,.F.);
#53879=ORIENTED_EDGE('',*,*,#38910,.F.);
#53880=ORIENTED_EDGE('',*,*,#38911,.F.);
#53881=ORIENTED_EDGE('',*,*,#38527,.T.);
#53882=ORIENTED_EDGE('',*,*,#38912,.F.);
#53883=ORIENTED_EDGE('',*,*,#38913,.T.);
#53884=ORIENTED_EDGE('',*,*,#38914,.F.);
#53885=ORIENTED_EDGE('',*,*,#38528,.T.);
#53886=ORIENTED_EDGE('',*,*,#38914,.T.);
#53887=ORIENTED_EDGE('',*,*,#38915,.T.);
#53888=ORIENTED_EDGE('',*,*,#38916,.F.);
#53889=ORIENTED_EDGE('',*,*,#38915,.F.);
#53890=ORIENTED_EDGE('',*,*,#38913,.F.);
#53891=ORIENTED_EDGE('',*,*,#38917,.F.);
#53892=ORIENTED_EDGE('',*,*,#38918,.F.);
#53893=ORIENTED_EDGE('',*,*,#38530,.T.);
#53894=ORIENTED_EDGE('',*,*,#38919,.F.);
#53895=ORIENTED_EDGE('',*,*,#38920,.T.);
#53896=ORIENTED_EDGE('',*,*,#38921,.F.);
#53897=ORIENTED_EDGE('',*,*,#38922,.T.);
#53898=ORIENTED_EDGE('',*,*,#38923,.F.);
#53899=ORIENTED_EDGE('',*,*,#38531,.T.);
#53900=ORIENTED_EDGE('',*,*,#38921,.T.);
#53901=ORIENTED_EDGE('',*,*,#38924,.F.);
#53902=ORIENTED_EDGE('',*,*,#38925,.F.);
#53903=ORIENTED_EDGE('',*,*,#38922,.F.);
#53904=ORIENTED_EDGE('',*,*,#38920,.F.);
#53905=ORIENTED_EDGE('',*,*,#38533,.T.);
#53906=ORIENTED_EDGE('',*,*,#38926,.F.);
#53907=ORIENTED_EDGE('',*,*,#38927,.T.);
#53908=ORIENTED_EDGE('',*,*,#38928,.F.);
#53909=ORIENTED_EDGE('',*,*,#38534,.T.);
#53910=ORIENTED_EDGE('',*,*,#38928,.T.);
#53911=ORIENTED_EDGE('',*,*,#38929,.T.);
#53912=ORIENTED_EDGE('',*,*,#38930,.F.);
#53913=ORIENTED_EDGE('',*,*,#38929,.F.);
#53914=ORIENTED_EDGE('',*,*,#38927,.F.);
#53915=ORIENTED_EDGE('',*,*,#38931,.F.);
#53916=ORIENTED_EDGE('',*,*,#38932,.F.);
#53917=ORIENTED_EDGE('',*,*,#38933,.F.);
#53918=ORIENTED_EDGE('',*,*,#38934,.F.);
#53919=ORIENTED_EDGE('',*,*,#38538,.T.);
#53920=ORIENTED_EDGE('',*,*,#38537,.T.);
#53921=ORIENTED_EDGE('',*,*,#38935,.F.);
#53922=ORIENTED_EDGE('',*,*,#38541,.T.);
#53923=ORIENTED_EDGE('',*,*,#38539,.T.);
#53924=ORIENTED_EDGE('',*,*,#38934,.T.);
#53925=ORIENTED_EDGE('',*,*,#38936,.F.);
#53926=ORIENTED_EDGE('',*,*,#38937,.F.);
#53927=ORIENTED_EDGE('',*,*,#38545,.T.);
#53928=ORIENTED_EDGE('',*,*,#38544,.T.);
#53929=ORIENTED_EDGE('',*,*,#38938,.F.);
#53930=ORIENTED_EDGE('',*,*,#38548,.T.);
#53931=ORIENTED_EDGE('',*,*,#38546,.T.);
#53932=ORIENTED_EDGE('',*,*,#38937,.T.);
#53933=ORIENTED_EDGE('',*,*,#38939,.F.);
#53934=ORIENTED_EDGE('',*,*,#38940,.F.);
#53935=ORIENTED_EDGE('',*,*,#38552,.T.);
#53936=ORIENTED_EDGE('',*,*,#38551,.T.);
#53937=ORIENTED_EDGE('',*,*,#38941,.F.);
#53938=ORIENTED_EDGE('',*,*,#38555,.T.);
#53939=ORIENTED_EDGE('',*,*,#38553,.T.);
#53940=ORIENTED_EDGE('',*,*,#38940,.T.);
#53941=ORIENTED_EDGE('',*,*,#38942,.F.);
#53942=ORIENTED_EDGE('',*,*,#38943,.F.);
#53943=ORIENTED_EDGE('',*,*,#38559,.T.);
#53944=ORIENTED_EDGE('',*,*,#38558,.T.);
#53945=ORIENTED_EDGE('',*,*,#38944,.F.);
#53946=ORIENTED_EDGE('',*,*,#38562,.T.);
#53947=ORIENTED_EDGE('',*,*,#38560,.T.);
#53948=ORIENTED_EDGE('',*,*,#38943,.T.);
#53949=ORIENTED_EDGE('',*,*,#38945,.F.);
#53950=ORIENTED_EDGE('',*,*,#38946,.F.);
#53951=ORIENTED_EDGE('',*,*,#38566,.T.);
#53952=ORIENTED_EDGE('',*,*,#38565,.T.);
#53953=ORIENTED_EDGE('',*,*,#38947,.F.);
#53954=ORIENTED_EDGE('',*,*,#38569,.T.);
#53955=ORIENTED_EDGE('',*,*,#38567,.T.);
#53956=ORIENTED_EDGE('',*,*,#38946,.T.);
#53957=ORIENTED_EDGE('',*,*,#38948,.F.);
#53958=ORIENTED_EDGE('',*,*,#38949,.F.);
#53959=ORIENTED_EDGE('',*,*,#38573,.T.);
#53960=ORIENTED_EDGE('',*,*,#38572,.T.);
#53961=ORIENTED_EDGE('',*,*,#38950,.F.);
#53962=ORIENTED_EDGE('',*,*,#38576,.T.);
#53963=ORIENTED_EDGE('',*,*,#38574,.T.);
#53964=ORIENTED_EDGE('',*,*,#38949,.T.);
#53965=ORIENTED_EDGE('',*,*,#38951,.F.);
#53966=ORIENTED_EDGE('',*,*,#38952,.F.);
#53967=ORIENTED_EDGE('',*,*,#38580,.T.);
#53968=ORIENTED_EDGE('',*,*,#38579,.T.);
#53969=ORIENTED_EDGE('',*,*,#38953,.F.);
#53970=ORIENTED_EDGE('',*,*,#38583,.T.);
#53971=ORIENTED_EDGE('',*,*,#38581,.T.);
#53972=ORIENTED_EDGE('',*,*,#38952,.T.);
#53973=ORIENTED_EDGE('',*,*,#38954,.F.);
#53974=ORIENTED_EDGE('',*,*,#38955,.F.);
#53975=ORIENTED_EDGE('',*,*,#38587,.T.);
#53976=ORIENTED_EDGE('',*,*,#38586,.T.);
#53977=ORIENTED_EDGE('',*,*,#38956,.F.);
#53978=ORIENTED_EDGE('',*,*,#38590,.T.);
#53979=ORIENTED_EDGE('',*,*,#38588,.T.);
#53980=ORIENTED_EDGE('',*,*,#38955,.T.);
#53981=ORIENTED_EDGE('',*,*,#38957,.F.);
#53982=ORIENTED_EDGE('',*,*,#38958,.F.);
#53983=ORIENTED_EDGE('',*,*,#38594,.T.);
#53984=ORIENTED_EDGE('',*,*,#38593,.T.);
#53985=ORIENTED_EDGE('',*,*,#38959,.F.);
#53986=ORIENTED_EDGE('',*,*,#38597,.T.);
#53987=ORIENTED_EDGE('',*,*,#38595,.T.);
#53988=ORIENTED_EDGE('',*,*,#38958,.T.);
#53989=ORIENTED_EDGE('',*,*,#38960,.F.);
#53990=ORIENTED_EDGE('',*,*,#38961,.F.);
#53991=ORIENTED_EDGE('',*,*,#38601,.T.);
#53992=ORIENTED_EDGE('',*,*,#38600,.T.);
#53993=ORIENTED_EDGE('',*,*,#38962,.F.);
#53994=ORIENTED_EDGE('',*,*,#38604,.T.);
#53995=ORIENTED_EDGE('',*,*,#38602,.T.);
#53996=ORIENTED_EDGE('',*,*,#38961,.T.);
#53997=ORIENTED_EDGE('',*,*,#38963,.F.);
#53998=ORIENTED_EDGE('',*,*,#38964,.F.);
#53999=ORIENTED_EDGE('',*,*,#38608,.T.);
#54000=ORIENTED_EDGE('',*,*,#38607,.T.);
#54001=ORIENTED_EDGE('',*,*,#38965,.F.);
#54002=ORIENTED_EDGE('',*,*,#38611,.T.);
#54003=ORIENTED_EDGE('',*,*,#38609,.T.);
#54004=ORIENTED_EDGE('',*,*,#38964,.T.);
#54005=ORIENTED_EDGE('',*,*,#38966,.F.);
#54006=ORIENTED_EDGE('',*,*,#38967,.F.);
#54007=ORIENTED_EDGE('',*,*,#38615,.T.);
#54008=ORIENTED_EDGE('',*,*,#38614,.T.);
#54009=ORIENTED_EDGE('',*,*,#38968,.F.);
#54010=ORIENTED_EDGE('',*,*,#38618,.T.);
#54011=ORIENTED_EDGE('',*,*,#38616,.T.);
#54012=ORIENTED_EDGE('',*,*,#38967,.T.);
#54013=ORIENTED_EDGE('',*,*,#38969,.F.);
#54014=ORIENTED_EDGE('',*,*,#38970,.F.);
#54015=ORIENTED_EDGE('',*,*,#38622,.T.);
#54016=ORIENTED_EDGE('',*,*,#38621,.T.);
#54017=ORIENTED_EDGE('',*,*,#38971,.F.);
#54018=ORIENTED_EDGE('',*,*,#38625,.T.);
#54019=ORIENTED_EDGE('',*,*,#38623,.T.);
#54020=ORIENTED_EDGE('',*,*,#38970,.T.);
#54021=ORIENTED_EDGE('',*,*,#38972,.F.);
#54022=ORIENTED_EDGE('',*,*,#38973,.F.);
#54023=ORIENTED_EDGE('',*,*,#38629,.T.);
#54024=ORIENTED_EDGE('',*,*,#38628,.T.);
#54025=ORIENTED_EDGE('',*,*,#38974,.F.);
#54026=ORIENTED_EDGE('',*,*,#38632,.T.);
#54027=ORIENTED_EDGE('',*,*,#38630,.T.);
#54028=ORIENTED_EDGE('',*,*,#38973,.T.);
#54029=ORIENTED_EDGE('',*,*,#38975,.F.);
#54030=ORIENTED_EDGE('',*,*,#38976,.F.);
#54031=ORIENTED_EDGE('',*,*,#34414,.T.);
#54032=ORIENTED_EDGE('',*,*,#38634,.T.);
#54033=ORIENTED_EDGE('',*,*,#38977,.F.);
#54034=ORIENTED_EDGE('',*,*,#38635,.T.);
#54035=ORIENTED_EDGE('',*,*,#34415,.T.);
#54036=ORIENTED_EDGE('',*,*,#38976,.T.);
#54037=ORIENTED_EDGE('',*,*,#38978,.F.);
#54038=ORIENTED_EDGE('',*,*,#38979,.F.);
#54039=ORIENTED_EDGE('',*,*,#38639,.T.);
#54040=ORIENTED_EDGE('',*,*,#38638,.T.);
#54041=ORIENTED_EDGE('',*,*,#38980,.F.);
#54042=ORIENTED_EDGE('',*,*,#38642,.T.);
#54043=ORIENTED_EDGE('',*,*,#38640,.T.);
#54044=ORIENTED_EDGE('',*,*,#38979,.T.);
#54045=ORIENTED_EDGE('',*,*,#38981,.F.);
#54046=ORIENTED_EDGE('',*,*,#38982,.F.);
#54047=ORIENTED_EDGE('',*,*,#38646,.T.);
#54048=ORIENTED_EDGE('',*,*,#38645,.T.);
#54049=ORIENTED_EDGE('',*,*,#38983,.F.);
#54050=ORIENTED_EDGE('',*,*,#38649,.T.);
#54051=ORIENTED_EDGE('',*,*,#38647,.T.);
#54052=ORIENTED_EDGE('',*,*,#38982,.T.);
#54053=ORIENTED_EDGE('',*,*,#38984,.F.);
#54054=ORIENTED_EDGE('',*,*,#38985,.F.);
#54055=ORIENTED_EDGE('',*,*,#38653,.T.);
#54056=ORIENTED_EDGE('',*,*,#38652,.T.);
#54057=ORIENTED_EDGE('',*,*,#38986,.F.);
#54058=ORIENTED_EDGE('',*,*,#38656,.T.);
#54059=ORIENTED_EDGE('',*,*,#38654,.T.);
#54060=ORIENTED_EDGE('',*,*,#38985,.T.);
#54061=ORIENTED_EDGE('',*,*,#38987,.F.);
#54062=ORIENTED_EDGE('',*,*,#38988,.F.);
#54063=ORIENTED_EDGE('',*,*,#38660,.T.);
#54064=ORIENTED_EDGE('',*,*,#38659,.T.);
#54065=ORIENTED_EDGE('',*,*,#38989,.F.);
#54066=ORIENTED_EDGE('',*,*,#38663,.T.);
#54067=ORIENTED_EDGE('',*,*,#38661,.T.);
#54068=ORIENTED_EDGE('',*,*,#38988,.T.);
#54069=ORIENTED_EDGE('',*,*,#38990,.F.);
#54070=ORIENTED_EDGE('',*,*,#38991,.F.);
#54071=ORIENTED_EDGE('',*,*,#38667,.T.);
#54072=ORIENTED_EDGE('',*,*,#38666,.T.);
#54073=ORIENTED_EDGE('',*,*,#38992,.F.);
#54074=ORIENTED_EDGE('',*,*,#38670,.T.);
#54075=ORIENTED_EDGE('',*,*,#38668,.T.);
#54076=ORIENTED_EDGE('',*,*,#38991,.T.);
#54077=ORIENTED_EDGE('',*,*,#38993,.F.);
#54078=ORIENTED_EDGE('',*,*,#38994,.F.);
#54079=ORIENTED_EDGE('',*,*,#38674,.T.);
#54080=ORIENTED_EDGE('',*,*,#38673,.T.);
#54081=ORIENTED_EDGE('',*,*,#38995,.F.);
#54082=ORIENTED_EDGE('',*,*,#38677,.T.);
#54083=ORIENTED_EDGE('',*,*,#38675,.T.);
#54084=ORIENTED_EDGE('',*,*,#38994,.T.);
#54085=ORIENTED_EDGE('',*,*,#38996,.F.);
#54086=ORIENTED_EDGE('',*,*,#38997,.F.);
#54087=ORIENTED_EDGE('',*,*,#38683,.T.);
#54088=ORIENTED_EDGE('',*,*,#38680,.T.);
#54089=ORIENTED_EDGE('',*,*,#38684,.T.);
#54090=ORIENTED_EDGE('',*,*,#38997,.T.);
#54091=ORIENTED_EDGE('',*,*,#38998,.F.);
#54092=ORIENTED_EDGE('',*,*,#38682,.T.);
#54093=ORIENTED_EDGE('',*,*,#38689,.T.);
#54094=ORIENTED_EDGE('',*,*,#38685,.T.);
#54095=ORIENTED_EDGE('',*,*,#38999,.F.);
#54096=ORIENTED_EDGE('',*,*,#39000,.F.);
#54097=ORIENTED_EDGE('',*,*,#39001,.F.);
#54098=ORIENTED_EDGE('',*,*,#38691,.T.);
#54099=ORIENTED_EDGE('',*,*,#38690,.T.);
#54100=ORIENTED_EDGE('',*,*,#39000,.T.);
#54101=ORIENTED_EDGE('',*,*,#39002,.F.);
#54102=ORIENTED_EDGE('',*,*,#39003,.F.);
#54103=ORIENTED_EDGE('',*,*,#38695,.T.);
#54104=ORIENTED_EDGE('',*,*,#38694,.T.);
#54105=ORIENTED_EDGE('',*,*,#39004,.F.);
#54106=ORIENTED_EDGE('',*,*,#38698,.T.);
#54107=ORIENTED_EDGE('',*,*,#38696,.T.);
#54108=ORIENTED_EDGE('',*,*,#39003,.T.);
#54109=ORIENTED_EDGE('',*,*,#39005,.F.);
#54110=ORIENTED_EDGE('',*,*,#39006,.F.);
#54111=ORIENTED_EDGE('',*,*,#38702,.T.);
#54112=ORIENTED_EDGE('',*,*,#38701,.T.);
#54113=ORIENTED_EDGE('',*,*,#39007,.F.);
#54114=ORIENTED_EDGE('',*,*,#38705,.T.);
#54115=ORIENTED_EDGE('',*,*,#38703,.T.);
#54116=ORIENTED_EDGE('',*,*,#39006,.T.);
#54117=ORIENTED_EDGE('',*,*,#39008,.F.);
#54118=ORIENTED_EDGE('',*,*,#39009,.F.);
#54119=ORIENTED_EDGE('',*,*,#38709,.T.);
#54120=ORIENTED_EDGE('',*,*,#38708,.T.);
#54121=ORIENTED_EDGE('',*,*,#39010,.F.);
#54122=ORIENTED_EDGE('',*,*,#38712,.T.);
#54123=ORIENTED_EDGE('',*,*,#38710,.T.);
#54124=ORIENTED_EDGE('',*,*,#39009,.T.);
#54125=ORIENTED_EDGE('',*,*,#39011,.F.);
#54126=ORIENTED_EDGE('',*,*,#39012,.F.);
#54127=ORIENTED_EDGE('',*,*,#38716,.T.);
#54128=ORIENTED_EDGE('',*,*,#38715,.T.);
#54129=ORIENTED_EDGE('',*,*,#39013,.F.);
#54130=ORIENTED_EDGE('',*,*,#38719,.T.);
#54131=ORIENTED_EDGE('',*,*,#38717,.T.);
#54132=ORIENTED_EDGE('',*,*,#39012,.T.);
#54133=ORIENTED_EDGE('',*,*,#39014,.F.);
#54134=ORIENTED_EDGE('',*,*,#39015,.F.);
#54135=ORIENTED_EDGE('',*,*,#38723,.T.);
#54136=ORIENTED_EDGE('',*,*,#38722,.T.);
#54137=ORIENTED_EDGE('',*,*,#39016,.F.);
#54138=ORIENTED_EDGE('',*,*,#38726,.T.);
#54139=ORIENTED_EDGE('',*,*,#38724,.T.);
#54140=ORIENTED_EDGE('',*,*,#39015,.T.);
#54141=ORIENTED_EDGE('',*,*,#39017,.F.);
#54142=ORIENTED_EDGE('',*,*,#39018,.F.);
#54143=ORIENTED_EDGE('',*,*,#38730,.T.);
#54144=ORIENTED_EDGE('',*,*,#38729,.T.);
#54145=ORIENTED_EDGE('',*,*,#39019,.F.);
#54146=ORIENTED_EDGE('',*,*,#38733,.T.);
#54147=ORIENTED_EDGE('',*,*,#38731,.T.);
#54148=ORIENTED_EDGE('',*,*,#39018,.T.);
#54149=ORIENTED_EDGE('',*,*,#38739,.T.);
#54150=ORIENTED_EDGE('',*,*,#38734,.T.);
#54151=ORIENTED_EDGE('',*,*,#39020,.F.);
#54152=ORIENTED_EDGE('',*,*,#39021,.F.);
#54153=ORIENTED_EDGE('',*,*,#38740,.T.);
#54154=ORIENTED_EDGE('',*,*,#39021,.T.);
#54155=ORIENTED_EDGE('',*,*,#39022,.F.);
#54156=ORIENTED_EDGE('',*,*,#38738,.T.);
#54157=ORIENTED_EDGE('',*,*,#38746,.T.);
#54158=ORIENTED_EDGE('',*,*,#38741,.T.);
#54159=ORIENTED_EDGE('',*,*,#39023,.F.);
#54160=ORIENTED_EDGE('',*,*,#39024,.F.);
#54161=ORIENTED_EDGE('',*,*,#38747,.T.);
#54162=ORIENTED_EDGE('',*,*,#39024,.T.);
#54163=ORIENTED_EDGE('',*,*,#39025,.F.);
#54164=ORIENTED_EDGE('',*,*,#38745,.T.);
#54165=ORIENTED_EDGE('',*,*,#38753,.T.);
#54166=ORIENTED_EDGE('',*,*,#38748,.T.);
#54167=ORIENTED_EDGE('',*,*,#39026,.F.);
#54168=ORIENTED_EDGE('',*,*,#39027,.F.);
#54169=ORIENTED_EDGE('',*,*,#38754,.T.);
#54170=ORIENTED_EDGE('',*,*,#39027,.T.);
#54171=ORIENTED_EDGE('',*,*,#39028,.F.);
#54172=ORIENTED_EDGE('',*,*,#38752,.T.);
#54173=ORIENTED_EDGE('',*,*,#38760,.T.);
#54174=ORIENTED_EDGE('',*,*,#38755,.T.);
#54175=ORIENTED_EDGE('',*,*,#39029,.F.);
#54176=ORIENTED_EDGE('',*,*,#39030,.F.);
#54177=ORIENTED_EDGE('',*,*,#38761,.T.);
#54178=ORIENTED_EDGE('',*,*,#39030,.T.);
#54179=ORIENTED_EDGE('',*,*,#39031,.F.);
#54180=ORIENTED_EDGE('',*,*,#38759,.T.);
#54181=ORIENTED_EDGE('',*,*,#38767,.T.);
#54182=ORIENTED_EDGE('',*,*,#38762,.T.);
#54183=ORIENTED_EDGE('',*,*,#39032,.F.);
#54184=ORIENTED_EDGE('',*,*,#39033,.F.);
#54185=ORIENTED_EDGE('',*,*,#38768,.T.);
#54186=ORIENTED_EDGE('',*,*,#39033,.T.);
#54187=ORIENTED_EDGE('',*,*,#39034,.F.);
#54188=ORIENTED_EDGE('',*,*,#38766,.T.);
#54189=ORIENTED_EDGE('',*,*,#38774,.T.);
#54190=ORIENTED_EDGE('',*,*,#38769,.T.);
#54191=ORIENTED_EDGE('',*,*,#39035,.F.);
#54192=ORIENTED_EDGE('',*,*,#39036,.F.);
#54193=ORIENTED_EDGE('',*,*,#38775,.T.);
#54194=ORIENTED_EDGE('',*,*,#39036,.T.);
#54195=ORIENTED_EDGE('',*,*,#39037,.F.);
#54196=ORIENTED_EDGE('',*,*,#38773,.T.);
#54197=ORIENTED_EDGE('',*,*,#38781,.T.);
#54198=ORIENTED_EDGE('',*,*,#38776,.T.);
#54199=ORIENTED_EDGE('',*,*,#39038,.F.);
#54200=ORIENTED_EDGE('',*,*,#39039,.F.);
#54201=ORIENTED_EDGE('',*,*,#38782,.T.);
#54202=ORIENTED_EDGE('',*,*,#39039,.T.);
#54203=ORIENTED_EDGE('',*,*,#39040,.F.);
#54204=ORIENTED_EDGE('',*,*,#38780,.T.);
#54205=ORIENTED_EDGE('',*,*,#38788,.T.);
#54206=ORIENTED_EDGE('',*,*,#38783,.T.);
#54207=ORIENTED_EDGE('',*,*,#39041,.F.);
#54208=ORIENTED_EDGE('',*,*,#39042,.F.);
#54209=ORIENTED_EDGE('',*,*,#38789,.T.);
#54210=ORIENTED_EDGE('',*,*,#39042,.T.);
#54211=ORIENTED_EDGE('',*,*,#39043,.F.);
#54212=ORIENTED_EDGE('',*,*,#38787,.T.);
#54213=ORIENTED_EDGE('',*,*,#38795,.T.);
#54214=ORIENTED_EDGE('',*,*,#38790,.T.);
#54215=ORIENTED_EDGE('',*,*,#39044,.F.);
#54216=ORIENTED_EDGE('',*,*,#39045,.F.);
#54217=ORIENTED_EDGE('',*,*,#38796,.T.);
#54218=ORIENTED_EDGE('',*,*,#39045,.T.);
#54219=ORIENTED_EDGE('',*,*,#39046,.F.);
#54220=ORIENTED_EDGE('',*,*,#38794,.T.);
#54221=ORIENTED_EDGE('',*,*,#38802,.T.);
#54222=ORIENTED_EDGE('',*,*,#38797,.T.);
#54223=ORIENTED_EDGE('',*,*,#39047,.F.);
#54224=ORIENTED_EDGE('',*,*,#39048,.F.);
#54225=ORIENTED_EDGE('',*,*,#38803,.T.);
#54226=ORIENTED_EDGE('',*,*,#39048,.T.);
#54227=ORIENTED_EDGE('',*,*,#39049,.F.);
#54228=ORIENTED_EDGE('',*,*,#38801,.T.);
#54229=ORIENTED_EDGE('',*,*,#38809,.T.);
#54230=ORIENTED_EDGE('',*,*,#38804,.T.);
#54231=ORIENTED_EDGE('',*,*,#39050,.F.);
#54232=ORIENTED_EDGE('',*,*,#39051,.F.);
#54233=ORIENTED_EDGE('',*,*,#38810,.T.);
#54234=ORIENTED_EDGE('',*,*,#39051,.T.);
#54235=ORIENTED_EDGE('',*,*,#39052,.F.);
#54236=ORIENTED_EDGE('',*,*,#38808,.T.);
#54237=ORIENTED_EDGE('',*,*,#38816,.T.);
#54238=ORIENTED_EDGE('',*,*,#38811,.T.);
#54239=ORIENTED_EDGE('',*,*,#39053,.F.);
#54240=ORIENTED_EDGE('',*,*,#39054,.F.);
#54241=ORIENTED_EDGE('',*,*,#38817,.T.);
#54242=ORIENTED_EDGE('',*,*,#39054,.T.);
#54243=ORIENTED_EDGE('',*,*,#39055,.F.);
#54244=ORIENTED_EDGE('',*,*,#38815,.T.);
#54245=ORIENTED_EDGE('',*,*,#38823,.T.);
#54246=ORIENTED_EDGE('',*,*,#38818,.T.);
#54247=ORIENTED_EDGE('',*,*,#39056,.F.);
#54248=ORIENTED_EDGE('',*,*,#39057,.F.);
#54249=ORIENTED_EDGE('',*,*,#38824,.T.);
#54250=ORIENTED_EDGE('',*,*,#39057,.T.);
#54251=ORIENTED_EDGE('',*,*,#39058,.F.);
#54252=ORIENTED_EDGE('',*,*,#38822,.T.);
#54253=ORIENTED_EDGE('',*,*,#38830,.T.);
#54254=ORIENTED_EDGE('',*,*,#38825,.T.);
#54255=ORIENTED_EDGE('',*,*,#39059,.F.);
#54256=ORIENTED_EDGE('',*,*,#39060,.F.);
#54257=ORIENTED_EDGE('',*,*,#38831,.T.);
#54258=ORIENTED_EDGE('',*,*,#39060,.T.);
#54259=ORIENTED_EDGE('',*,*,#39061,.F.);
#54260=ORIENTED_EDGE('',*,*,#38829,.T.);
#54261=ORIENTED_EDGE('',*,*,#38837,.T.);
#54262=ORIENTED_EDGE('',*,*,#38832,.T.);
#54263=ORIENTED_EDGE('',*,*,#39062,.F.);
#54264=ORIENTED_EDGE('',*,*,#39063,.F.);
#54265=ORIENTED_EDGE('',*,*,#38838,.T.);
#54266=ORIENTED_EDGE('',*,*,#39063,.T.);
#54267=ORIENTED_EDGE('',*,*,#39064,.F.);
#54268=ORIENTED_EDGE('',*,*,#38836,.T.);
#54269=ORIENTED_EDGE('',*,*,#38844,.T.);
#54270=ORIENTED_EDGE('',*,*,#38839,.T.);
#54271=ORIENTED_EDGE('',*,*,#39065,.F.);
#54272=ORIENTED_EDGE('',*,*,#39066,.F.);
#54273=ORIENTED_EDGE('',*,*,#38845,.T.);
#54274=ORIENTED_EDGE('',*,*,#39066,.T.);
#54275=ORIENTED_EDGE('',*,*,#39067,.F.);
#54276=ORIENTED_EDGE('',*,*,#38843,.T.);
#54277=ORIENTED_EDGE('',*,*,#38851,.T.);
#54278=ORIENTED_EDGE('',*,*,#38846,.T.);
#54279=ORIENTED_EDGE('',*,*,#39068,.F.);
#54280=ORIENTED_EDGE('',*,*,#39069,.F.);
#54281=ORIENTED_EDGE('',*,*,#38852,.T.);
#54282=ORIENTED_EDGE('',*,*,#39069,.T.);
#54283=ORIENTED_EDGE('',*,*,#39070,.F.);
#54284=ORIENTED_EDGE('',*,*,#38850,.T.);
#54285=ORIENTED_EDGE('',*,*,#38858,.T.);
#54286=ORIENTED_EDGE('',*,*,#38853,.T.);
#54287=ORIENTED_EDGE('',*,*,#39071,.F.);
#54288=ORIENTED_EDGE('',*,*,#39072,.F.);
#54289=ORIENTED_EDGE('',*,*,#38859,.T.);
#54290=ORIENTED_EDGE('',*,*,#39072,.T.);
#54291=ORIENTED_EDGE('',*,*,#39073,.F.);
#54292=ORIENTED_EDGE('',*,*,#38857,.T.);
#54293=ORIENTED_EDGE('',*,*,#38865,.T.);
#54294=ORIENTED_EDGE('',*,*,#38860,.T.);
#54295=ORIENTED_EDGE('',*,*,#39074,.F.);
#54296=ORIENTED_EDGE('',*,*,#39075,.F.);
#54297=ORIENTED_EDGE('',*,*,#38866,.T.);
#54298=ORIENTED_EDGE('',*,*,#39075,.T.);
#54299=ORIENTED_EDGE('',*,*,#39076,.F.);
#54300=ORIENTED_EDGE('',*,*,#38864,.T.);
#54301=ORIENTED_EDGE('',*,*,#38872,.T.);
#54302=ORIENTED_EDGE('',*,*,#38867,.T.);
#54303=ORIENTED_EDGE('',*,*,#39077,.F.);
#54304=ORIENTED_EDGE('',*,*,#39078,.F.);
#54305=ORIENTED_EDGE('',*,*,#38873,.T.);
#54306=ORIENTED_EDGE('',*,*,#39078,.T.);
#54307=ORIENTED_EDGE('',*,*,#39079,.F.);
#54308=ORIENTED_EDGE('',*,*,#38871,.T.);
#54309=ORIENTED_EDGE('',*,*,#38879,.T.);
#54310=ORIENTED_EDGE('',*,*,#38874,.T.);
#54311=ORIENTED_EDGE('',*,*,#39080,.F.);
#54312=ORIENTED_EDGE('',*,*,#39081,.F.);
#54313=ORIENTED_EDGE('',*,*,#38880,.T.);
#54314=ORIENTED_EDGE('',*,*,#39081,.T.);
#54315=ORIENTED_EDGE('',*,*,#39082,.F.);
#54316=ORIENTED_EDGE('',*,*,#38878,.T.);
#54317=ORIENTED_EDGE('',*,*,#34409,.T.);
#54318=ORIENTED_EDGE('',*,*,#38881,.T.);
#54319=ORIENTED_EDGE('',*,*,#39083,.F.);
#54320=ORIENTED_EDGE('',*,*,#39084,.F.);
#54321=ORIENTED_EDGE('',*,*,#34410,.T.);
#54322=ORIENTED_EDGE('',*,*,#39084,.T.);
#54323=ORIENTED_EDGE('',*,*,#39085,.F.);
#54324=ORIENTED_EDGE('',*,*,#38883,.T.);
#54325=ORIENTED_EDGE('',*,*,#38889,.T.);
#54326=ORIENTED_EDGE('',*,*,#38884,.T.);
#54327=ORIENTED_EDGE('',*,*,#39086,.F.);
#54328=ORIENTED_EDGE('',*,*,#39087,.F.);
#54329=ORIENTED_EDGE('',*,*,#38890,.T.);
#54330=ORIENTED_EDGE('',*,*,#39087,.T.);
#54331=ORIENTED_EDGE('',*,*,#39088,.F.);
#54332=ORIENTED_EDGE('',*,*,#38888,.T.);
#54333=ORIENTED_EDGE('',*,*,#38896,.T.);
#54334=ORIENTED_EDGE('',*,*,#38891,.T.);
#54335=ORIENTED_EDGE('',*,*,#39089,.F.);
#54336=ORIENTED_EDGE('',*,*,#39090,.F.);
#54337=ORIENTED_EDGE('',*,*,#38897,.T.);
#54338=ORIENTED_EDGE('',*,*,#39090,.T.);
#54339=ORIENTED_EDGE('',*,*,#39091,.F.);
#54340=ORIENTED_EDGE('',*,*,#38895,.T.);
#54341=ORIENTED_EDGE('',*,*,#38903,.T.);
#54342=ORIENTED_EDGE('',*,*,#38898,.T.);
#54343=ORIENTED_EDGE('',*,*,#39092,.F.);
#54344=ORIENTED_EDGE('',*,*,#39093,.F.);
#54345=ORIENTED_EDGE('',*,*,#38904,.T.);
#54346=ORIENTED_EDGE('',*,*,#39093,.T.);
#54347=ORIENTED_EDGE('',*,*,#39094,.F.);
#54348=ORIENTED_EDGE('',*,*,#38902,.T.);
#54349=ORIENTED_EDGE('',*,*,#38910,.T.);
#54350=ORIENTED_EDGE('',*,*,#38905,.T.);
#54351=ORIENTED_EDGE('',*,*,#39095,.F.);
#54352=ORIENTED_EDGE('',*,*,#39096,.F.);
#54353=ORIENTED_EDGE('',*,*,#38911,.T.);
#54354=ORIENTED_EDGE('',*,*,#39096,.T.);
#54355=ORIENTED_EDGE('',*,*,#39097,.F.);
#54356=ORIENTED_EDGE('',*,*,#38909,.T.);
#54357=ORIENTED_EDGE('',*,*,#38917,.T.);
#54358=ORIENTED_EDGE('',*,*,#38912,.T.);
#54359=ORIENTED_EDGE('',*,*,#39098,.F.);
#54360=ORIENTED_EDGE('',*,*,#39099,.F.);
#54361=ORIENTED_EDGE('',*,*,#38918,.T.);
#54362=ORIENTED_EDGE('',*,*,#39099,.T.);
#54363=ORIENTED_EDGE('',*,*,#39100,.F.);
#54364=ORIENTED_EDGE('',*,*,#38916,.T.);
#54365=ORIENTED_EDGE('',*,*,#39101,.F.);
#54366=ORIENTED_EDGE('',*,*,#39102,.F.);
#54367=ORIENTED_EDGE('',*,*,#38924,.T.);
#54368=ORIENTED_EDGE('',*,*,#38919,.T.);
#54369=ORIENTED_EDGE('',*,*,#38925,.T.);
#54370=ORIENTED_EDGE('',*,*,#39102,.T.);
#54371=ORIENTED_EDGE('',*,*,#39103,.F.);
#54372=ORIENTED_EDGE('',*,*,#38923,.T.);
#54373=ORIENTED_EDGE('',*,*,#38931,.T.);
#54374=ORIENTED_EDGE('',*,*,#38926,.T.);
#54375=ORIENTED_EDGE('',*,*,#39104,.F.);
#54376=ORIENTED_EDGE('',*,*,#39105,.F.);
#54377=ORIENTED_EDGE('',*,*,#38932,.T.);
#54378=ORIENTED_EDGE('',*,*,#39105,.T.);
#54379=ORIENTED_EDGE('',*,*,#39106,.F.);
#54380=ORIENTED_EDGE('',*,*,#38930,.T.);
#54381=ORIENTED_EDGE('',*,*,#39107,.T.);
#54382=ORIENTED_EDGE('',*,*,#39108,.F.);
#54383=ORIENTED_EDGE('',*,*,#38933,.T.);
#54384=ORIENTED_EDGE('',*,*,#39109,.F.);
#54385=ORIENTED_EDGE('',*,*,#39110,.T.);
#54386=ORIENTED_EDGE('',*,*,#39111,.F.);
#54387=ORIENTED_EDGE('',*,*,#38935,.T.);
#54388=ORIENTED_EDGE('',*,*,#39112,.F.);
#54389=ORIENTED_EDGE('',*,*,#39113,.F.);
#54390=ORIENTED_EDGE('',*,*,#39114,.F.);
#54391=ORIENTED_EDGE('',*,*,#39115,.F.);
#54392=ORIENTED_EDGE('',*,*,#39110,.F.);
#54393=ORIENTED_EDGE('',*,*,#39115,.T.);
#54394=ORIENTED_EDGE('',*,*,#39116,.F.);
#54395=ORIENTED_EDGE('',*,*,#38936,.T.);
#54396=ORIENTED_EDGE('',*,*,#39111,.T.);
#54397=ORIENTED_EDGE('',*,*,#39117,.T.);
#54398=ORIENTED_EDGE('',*,*,#39118,.F.);
#54399=ORIENTED_EDGE('',*,*,#38938,.T.);
#54400=ORIENTED_EDGE('',*,*,#39119,.F.);
#54401=ORIENTED_EDGE('',*,*,#39120,.F.);
#54402=ORIENTED_EDGE('',*,*,#39121,.F.);
#54403=ORIENTED_EDGE('',*,*,#39122,.F.);
#54404=ORIENTED_EDGE('',*,*,#39117,.F.);
#54405=ORIENTED_EDGE('',*,*,#39122,.T.);
#54406=ORIENTED_EDGE('',*,*,#39123,.F.);
#54407=ORIENTED_EDGE('',*,*,#38939,.T.);
#54408=ORIENTED_EDGE('',*,*,#39118,.T.);
#54409=ORIENTED_EDGE('',*,*,#39124,.T.);
#54410=ORIENTED_EDGE('',*,*,#39125,.F.);
#54411=ORIENTED_EDGE('',*,*,#38941,.T.);
#54412=ORIENTED_EDGE('',*,*,#39126,.F.);
#54413=ORIENTED_EDGE('',*,*,#39127,.F.);
#54414=ORIENTED_EDGE('',*,*,#39128,.F.);
#54415=ORIENTED_EDGE('',*,*,#39129,.F.);
#54416=ORIENTED_EDGE('',*,*,#39124,.F.);
#54417=ORIENTED_EDGE('',*,*,#39129,.T.);
#54418=ORIENTED_EDGE('',*,*,#39130,.F.);
#54419=ORIENTED_EDGE('',*,*,#38942,.T.);
#54420=ORIENTED_EDGE('',*,*,#39125,.T.);
#54421=ORIENTED_EDGE('',*,*,#39131,.T.);
#54422=ORIENTED_EDGE('',*,*,#39132,.F.);
#54423=ORIENTED_EDGE('',*,*,#38944,.T.);
#54424=ORIENTED_EDGE('',*,*,#39133,.F.);
#54425=ORIENTED_EDGE('',*,*,#39134,.F.);
#54426=ORIENTED_EDGE('',*,*,#39135,.F.);
#54427=ORIENTED_EDGE('',*,*,#39136,.F.);
#54428=ORIENTED_EDGE('',*,*,#39131,.F.);
#54429=ORIENTED_EDGE('',*,*,#39136,.T.);
#54430=ORIENTED_EDGE('',*,*,#39137,.F.);
#54431=ORIENTED_EDGE('',*,*,#38945,.T.);
#54432=ORIENTED_EDGE('',*,*,#39132,.T.);
#54433=ORIENTED_EDGE('',*,*,#39138,.T.);
#54434=ORIENTED_EDGE('',*,*,#39139,.F.);
#54435=ORIENTED_EDGE('',*,*,#38947,.T.);
#54436=ORIENTED_EDGE('',*,*,#39140,.F.);
#54437=ORIENTED_EDGE('',*,*,#39141,.F.);
#54438=ORIENTED_EDGE('',*,*,#39142,.F.);
#54439=ORIENTED_EDGE('',*,*,#39143,.F.);
#54440=ORIENTED_EDGE('',*,*,#39138,.F.);
#54441=ORIENTED_EDGE('',*,*,#39143,.T.);
#54442=ORIENTED_EDGE('',*,*,#39144,.F.);
#54443=ORIENTED_EDGE('',*,*,#38948,.T.);
#54444=ORIENTED_EDGE('',*,*,#39139,.T.);
#54445=ORIENTED_EDGE('',*,*,#39145,.T.);
#54446=ORIENTED_EDGE('',*,*,#39146,.F.);
#54447=ORIENTED_EDGE('',*,*,#38950,.T.);
#54448=ORIENTED_EDGE('',*,*,#39147,.F.);
#54449=ORIENTED_EDGE('',*,*,#39148,.F.);
#54450=ORIENTED_EDGE('',*,*,#39149,.F.);
#54451=ORIENTED_EDGE('',*,*,#39150,.F.);
#54452=ORIENTED_EDGE('',*,*,#39145,.F.);
#54453=ORIENTED_EDGE('',*,*,#39150,.T.);
#54454=ORIENTED_EDGE('',*,*,#39151,.F.);
#54455=ORIENTED_EDGE('',*,*,#38951,.T.);
#54456=ORIENTED_EDGE('',*,*,#39146,.T.);
#54457=ORIENTED_EDGE('',*,*,#34406,.T.);
#54458=ORIENTED_EDGE('',*,*,#39152,.F.);
#54459=ORIENTED_EDGE('',*,*,#38953,.T.);
#54460=ORIENTED_EDGE('',*,*,#39153,.F.);
#54461=ORIENTED_EDGE('',*,*,#34405,.T.);
#54462=ORIENTED_EDGE('',*,*,#39154,.F.);
#54463=ORIENTED_EDGE('',*,*,#38954,.T.);
#54464=ORIENTED_EDGE('',*,*,#39152,.T.);
#54465=ORIENTED_EDGE('',*,*,#39155,.T.);
#54466=ORIENTED_EDGE('',*,*,#39156,.F.);
#54467=ORIENTED_EDGE('',*,*,#38956,.T.);
#54468=ORIENTED_EDGE('',*,*,#39157,.F.);
#54469=ORIENTED_EDGE('',*,*,#39158,.F.);
#54470=ORIENTED_EDGE('',*,*,#39159,.F.);
#54471=ORIENTED_EDGE('',*,*,#39160,.F.);
#54472=ORIENTED_EDGE('',*,*,#39155,.F.);
#54473=ORIENTED_EDGE('',*,*,#39160,.T.);
#54474=ORIENTED_EDGE('',*,*,#39161,.F.);
#54475=ORIENTED_EDGE('',*,*,#38957,.T.);
#54476=ORIENTED_EDGE('',*,*,#39156,.T.);
#54477=ORIENTED_EDGE('',*,*,#39162,.T.);
#54478=ORIENTED_EDGE('',*,*,#39163,.F.);
#54479=ORIENTED_EDGE('',*,*,#38959,.T.);
#54480=ORIENTED_EDGE('',*,*,#39164,.F.);
#54481=ORIENTED_EDGE('',*,*,#39165,.F.);
#54482=ORIENTED_EDGE('',*,*,#39166,.F.);
#54483=ORIENTED_EDGE('',*,*,#39167,.F.);
#54484=ORIENTED_EDGE('',*,*,#39162,.F.);
#54485=ORIENTED_EDGE('',*,*,#39167,.T.);
#54486=ORIENTED_EDGE('',*,*,#39168,.F.);
#54487=ORIENTED_EDGE('',*,*,#38960,.T.);
#54488=ORIENTED_EDGE('',*,*,#39163,.T.);
#54489=ORIENTED_EDGE('',*,*,#39169,.T.);
#54490=ORIENTED_EDGE('',*,*,#39170,.F.);
#54491=ORIENTED_EDGE('',*,*,#38962,.T.);
#54492=ORIENTED_EDGE('',*,*,#39171,.F.);
#54493=ORIENTED_EDGE('',*,*,#39172,.F.);
#54494=ORIENTED_EDGE('',*,*,#39173,.F.);
#54495=ORIENTED_EDGE('',*,*,#39174,.F.);
#54496=ORIENTED_EDGE('',*,*,#39169,.F.);
#54497=ORIENTED_EDGE('',*,*,#39174,.T.);
#54498=ORIENTED_EDGE('',*,*,#39175,.F.);
#54499=ORIENTED_EDGE('',*,*,#38963,.T.);
#54500=ORIENTED_EDGE('',*,*,#39170,.T.);
#54501=ORIENTED_EDGE('',*,*,#39176,.T.);
#54502=ORIENTED_EDGE('',*,*,#39177,.F.);
#54503=ORIENTED_EDGE('',*,*,#38965,.T.);
#54504=ORIENTED_EDGE('',*,*,#39178,.F.);
#54505=ORIENTED_EDGE('',*,*,#39179,.F.);
#54506=ORIENTED_EDGE('',*,*,#39180,.F.);
#54507=ORIENTED_EDGE('',*,*,#39181,.F.);
#54508=ORIENTED_EDGE('',*,*,#39176,.F.);
#54509=ORIENTED_EDGE('',*,*,#39181,.T.);
#54510=ORIENTED_EDGE('',*,*,#39182,.F.);
#54511=ORIENTED_EDGE('',*,*,#38966,.T.);
#54512=ORIENTED_EDGE('',*,*,#39177,.T.);
#54513=ORIENTED_EDGE('',*,*,#39183,.T.);
#54514=ORIENTED_EDGE('',*,*,#39184,.F.);
#54515=ORIENTED_EDGE('',*,*,#38968,.T.);
#54516=ORIENTED_EDGE('',*,*,#39185,.F.);
#54517=ORIENTED_EDGE('',*,*,#39186,.F.);
#54518=ORIENTED_EDGE('',*,*,#39187,.F.);
#54519=ORIENTED_EDGE('',*,*,#39188,.F.);
#54520=ORIENTED_EDGE('',*,*,#39183,.F.);
#54521=ORIENTED_EDGE('',*,*,#39188,.T.);
#54522=ORIENTED_EDGE('',*,*,#39189,.F.);
#54523=ORIENTED_EDGE('',*,*,#38969,.T.);
#54524=ORIENTED_EDGE('',*,*,#39184,.T.);
#54525=ORIENTED_EDGE('',*,*,#39190,.T.);
#54526=ORIENTED_EDGE('',*,*,#39191,.F.);
#54527=ORIENTED_EDGE('',*,*,#38971,.T.);
#54528=ORIENTED_EDGE('',*,*,#39192,.F.);
#54529=ORIENTED_EDGE('',*,*,#39193,.F.);
#54530=ORIENTED_EDGE('',*,*,#39194,.F.);
#54531=ORIENTED_EDGE('',*,*,#39195,.F.);
#54532=ORIENTED_EDGE('',*,*,#39190,.F.);
#54533=ORIENTED_EDGE('',*,*,#39195,.T.);
#54534=ORIENTED_EDGE('',*,*,#39196,.F.);
#54535=ORIENTED_EDGE('',*,*,#38972,.T.);
#54536=ORIENTED_EDGE('',*,*,#39191,.T.);
#54537=ORIENTED_EDGE('',*,*,#39197,.T.);
#54538=ORIENTED_EDGE('',*,*,#39198,.F.);
#54539=ORIENTED_EDGE('',*,*,#38974,.T.);
#54540=ORIENTED_EDGE('',*,*,#39199,.F.);
#54541=ORIENTED_EDGE('',*,*,#39200,.F.);
#54542=ORIENTED_EDGE('',*,*,#39201,.F.);
#54543=ORIENTED_EDGE('',*,*,#39202,.F.);
#54544=ORIENTED_EDGE('',*,*,#39197,.F.);
#54545=ORIENTED_EDGE('',*,*,#39202,.T.);
#54546=ORIENTED_EDGE('',*,*,#39203,.F.);
#54547=ORIENTED_EDGE('',*,*,#38975,.T.);
#54548=ORIENTED_EDGE('',*,*,#39198,.T.);
#54549=ORIENTED_EDGE('',*,*,#39204,.T.);
#54550=ORIENTED_EDGE('',*,*,#39205,.F.);
#54551=ORIENTED_EDGE('',*,*,#38977,.T.);
#54552=ORIENTED_EDGE('',*,*,#39206,.F.);
#54553=ORIENTED_EDGE('',*,*,#39207,.F.);
#54554=ORIENTED_EDGE('',*,*,#39208,.F.);
#54555=ORIENTED_EDGE('',*,*,#39209,.F.);
#54556=ORIENTED_EDGE('',*,*,#39204,.F.);
#54557=ORIENTED_EDGE('',*,*,#39209,.T.);
#54558=ORIENTED_EDGE('',*,*,#39210,.F.);
#54559=ORIENTED_EDGE('',*,*,#38978,.T.);
#54560=ORIENTED_EDGE('',*,*,#39205,.T.);
#54561=ORIENTED_EDGE('',*,*,#39211,.T.);
#54562=ORIENTED_EDGE('',*,*,#39212,.F.);
#54563=ORIENTED_EDGE('',*,*,#38980,.T.);
#54564=ORIENTED_EDGE('',*,*,#39213,.F.);
#54565=ORIENTED_EDGE('',*,*,#39214,.F.);
#54566=ORIENTED_EDGE('',*,*,#39215,.F.);
#54567=ORIENTED_EDGE('',*,*,#39216,.F.);
#54568=ORIENTED_EDGE('',*,*,#39211,.F.);
#54569=ORIENTED_EDGE('',*,*,#39216,.T.);
#54570=ORIENTED_EDGE('',*,*,#39217,.F.);
#54571=ORIENTED_EDGE('',*,*,#38981,.T.);
#54572=ORIENTED_EDGE('',*,*,#39212,.T.);
#54573=ORIENTED_EDGE('',*,*,#39218,.T.);
#54574=ORIENTED_EDGE('',*,*,#39219,.F.);
#54575=ORIENTED_EDGE('',*,*,#38983,.T.);
#54576=ORIENTED_EDGE('',*,*,#39220,.F.);
#54577=ORIENTED_EDGE('',*,*,#39221,.F.);
#54578=ORIENTED_EDGE('',*,*,#39222,.F.);
#54579=ORIENTED_EDGE('',*,*,#39223,.F.);
#54580=ORIENTED_EDGE('',*,*,#39218,.F.);
#54581=ORIENTED_EDGE('',*,*,#39223,.T.);
#54582=ORIENTED_EDGE('',*,*,#39224,.F.);
#54583=ORIENTED_EDGE('',*,*,#38984,.T.);
#54584=ORIENTED_EDGE('',*,*,#39219,.T.);
#54585=ORIENTED_EDGE('',*,*,#39225,.T.);
#54586=ORIENTED_EDGE('',*,*,#39226,.F.);
#54587=ORIENTED_EDGE('',*,*,#38986,.T.);
#54588=ORIENTED_EDGE('',*,*,#39227,.F.);
#54589=ORIENTED_EDGE('',*,*,#39228,.F.);
#54590=ORIENTED_EDGE('',*,*,#39229,.F.);
#54591=ORIENTED_EDGE('',*,*,#39230,.F.);
#54592=ORIENTED_EDGE('',*,*,#39225,.F.);
#54593=ORIENTED_EDGE('',*,*,#39230,.T.);
#54594=ORIENTED_EDGE('',*,*,#39231,.F.);
#54595=ORIENTED_EDGE('',*,*,#38987,.T.);
#54596=ORIENTED_EDGE('',*,*,#39226,.T.);
#54597=ORIENTED_EDGE('',*,*,#39232,.T.);
#54598=ORIENTED_EDGE('',*,*,#39233,.F.);
#54599=ORIENTED_EDGE('',*,*,#38989,.T.);
#54600=ORIENTED_EDGE('',*,*,#39234,.F.);
#54601=ORIENTED_EDGE('',*,*,#39235,.F.);
#54602=ORIENTED_EDGE('',*,*,#39236,.F.);
#54603=ORIENTED_EDGE('',*,*,#39237,.F.);
#54604=ORIENTED_EDGE('',*,*,#39232,.F.);
#54605=ORIENTED_EDGE('',*,*,#39237,.T.);
#54606=ORIENTED_EDGE('',*,*,#39238,.F.);
#54607=ORIENTED_EDGE('',*,*,#38990,.T.);
#54608=ORIENTED_EDGE('',*,*,#39233,.T.);
#54609=ORIENTED_EDGE('',*,*,#39239,.T.);
#54610=ORIENTED_EDGE('',*,*,#39240,.F.);
#54611=ORIENTED_EDGE('',*,*,#38992,.T.);
#54612=ORIENTED_EDGE('',*,*,#39241,.F.);
#54613=ORIENTED_EDGE('',*,*,#39242,.F.);
#54614=ORIENTED_EDGE('',*,*,#39243,.F.);
#54615=ORIENTED_EDGE('',*,*,#39244,.F.);
#54616=ORIENTED_EDGE('',*,*,#39239,.F.);
#54617=ORIENTED_EDGE('',*,*,#39244,.T.);
#54618=ORIENTED_EDGE('',*,*,#39245,.F.);
#54619=ORIENTED_EDGE('',*,*,#38993,.T.);
#54620=ORIENTED_EDGE('',*,*,#39240,.T.);
#54621=ORIENTED_EDGE('',*,*,#39246,.T.);
#54622=ORIENTED_EDGE('',*,*,#39247,.F.);
#54623=ORIENTED_EDGE('',*,*,#38995,.T.);
#54624=ORIENTED_EDGE('',*,*,#39248,.F.);
#54625=ORIENTED_EDGE('',*,*,#39249,.T.);
#54626=ORIENTED_EDGE('',*,*,#39250,.F.);
#54627=ORIENTED_EDGE('',*,*,#38996,.T.);
#54628=ORIENTED_EDGE('',*,*,#39247,.T.);
#54629=ORIENTED_EDGE('',*,*,#39251,.F.);
#54630=ORIENTED_EDGE('',*,*,#39252,.F.);
#54631=ORIENTED_EDGE('',*,*,#39249,.F.);
#54632=ORIENTED_EDGE('',*,*,#39246,.F.);
#54633=ORIENTED_EDGE('',*,*,#38998,.T.);
#54634=ORIENTED_EDGE('',*,*,#39253,.F.);
#54635=ORIENTED_EDGE('',*,*,#39254,.T.);
#54636=ORIENTED_EDGE('',*,*,#39255,.F.);
#54637=ORIENTED_EDGE('',*,*,#39256,.F.);
#54638=ORIENTED_EDGE('',*,*,#39254,.F.);
#54639=ORIENTED_EDGE('',*,*,#39257,.F.);
#54640=ORIENTED_EDGE('',*,*,#39258,.F.);
#54641=ORIENTED_EDGE('',*,*,#38999,.T.);
#54642=ORIENTED_EDGE('',*,*,#39255,.T.);
#54643=ORIENTED_EDGE('',*,*,#39256,.T.);
#54644=ORIENTED_EDGE('',*,*,#39259,.F.);
#54645=ORIENTED_EDGE('',*,*,#39260,.T.);
#54646=ORIENTED_EDGE('',*,*,#39261,.F.);
#54647=ORIENTED_EDGE('',*,*,#39001,.T.);
#54648=ORIENTED_EDGE('',*,*,#39262,.F.);
#54649=ORIENTED_EDGE('',*,*,#39263,.F.);
#54650=ORIENTED_EDGE('',*,*,#39264,.F.);
#54651=ORIENTED_EDGE('',*,*,#39265,.F.);
#54652=ORIENTED_EDGE('',*,*,#39260,.F.);
#54653=ORIENTED_EDGE('',*,*,#39265,.T.);
#54654=ORIENTED_EDGE('',*,*,#39266,.F.);
#54655=ORIENTED_EDGE('',*,*,#39002,.T.);
#54656=ORIENTED_EDGE('',*,*,#39261,.T.);
#54657=ORIENTED_EDGE('',*,*,#39267,.T.);
#54658=ORIENTED_EDGE('',*,*,#39268,.F.);
#54659=ORIENTED_EDGE('',*,*,#39004,.T.);
#54660=ORIENTED_EDGE('',*,*,#39269,.F.);
#54661=ORIENTED_EDGE('',*,*,#39270,.F.);
#54662=ORIENTED_EDGE('',*,*,#39271,.F.);
#54663=ORIENTED_EDGE('',*,*,#39272,.F.);
#54664=ORIENTED_EDGE('',*,*,#39267,.F.);
#54665=ORIENTED_EDGE('',*,*,#39272,.T.);
#54666=ORIENTED_EDGE('',*,*,#39273,.F.);
#54667=ORIENTED_EDGE('',*,*,#39005,.T.);
#54668=ORIENTED_EDGE('',*,*,#39268,.T.);
#54669=ORIENTED_EDGE('',*,*,#39274,.T.);
#54670=ORIENTED_EDGE('',*,*,#39275,.F.);
#54671=ORIENTED_EDGE('',*,*,#39007,.T.);
#54672=ORIENTED_EDGE('',*,*,#39276,.F.);
#54673=ORIENTED_EDGE('',*,*,#39277,.F.);
#54674=ORIENTED_EDGE('',*,*,#39278,.F.);
#54675=ORIENTED_EDGE('',*,*,#39279,.F.);
#54676=ORIENTED_EDGE('',*,*,#39274,.F.);
#54677=ORIENTED_EDGE('',*,*,#39279,.T.);
#54678=ORIENTED_EDGE('',*,*,#39280,.F.);
#54679=ORIENTED_EDGE('',*,*,#39008,.T.);
#54680=ORIENTED_EDGE('',*,*,#39275,.T.);
#54681=ORIENTED_EDGE('',*,*,#39281,.T.);
#54682=ORIENTED_EDGE('',*,*,#39282,.F.);
#54683=ORIENTED_EDGE('',*,*,#39010,.T.);
#54684=ORIENTED_EDGE('',*,*,#39283,.F.);
#54685=ORIENTED_EDGE('',*,*,#39284,.F.);
#54686=ORIENTED_EDGE('',*,*,#39285,.F.);
#54687=ORIENTED_EDGE('',*,*,#39286,.F.);
#54688=ORIENTED_EDGE('',*,*,#39281,.F.);
#54689=ORIENTED_EDGE('',*,*,#39286,.T.);
#54690=ORIENTED_EDGE('',*,*,#39287,.F.);
#54691=ORIENTED_EDGE('',*,*,#39011,.T.);
#54692=ORIENTED_EDGE('',*,*,#39282,.T.);
#54693=ORIENTED_EDGE('',*,*,#39288,.T.);
#54694=ORIENTED_EDGE('',*,*,#39289,.F.);
#54695=ORIENTED_EDGE('',*,*,#39013,.T.);
#54696=ORIENTED_EDGE('',*,*,#39290,.F.);
#54697=ORIENTED_EDGE('',*,*,#39291,.F.);
#54698=ORIENTED_EDGE('',*,*,#39292,.F.);
#54699=ORIENTED_EDGE('',*,*,#39293,.F.);
#54700=ORIENTED_EDGE('',*,*,#39288,.F.);
#54701=ORIENTED_EDGE('',*,*,#39293,.T.);
#54702=ORIENTED_EDGE('',*,*,#39294,.F.);
#54703=ORIENTED_EDGE('',*,*,#39014,.T.);
#54704=ORIENTED_EDGE('',*,*,#39289,.T.);
#54705=ORIENTED_EDGE('',*,*,#39295,.T.);
#54706=ORIENTED_EDGE('',*,*,#39296,.F.);
#54707=ORIENTED_EDGE('',*,*,#39016,.T.);
#54708=ORIENTED_EDGE('',*,*,#39297,.F.);
#54709=ORIENTED_EDGE('',*,*,#39298,.F.);
#54710=ORIENTED_EDGE('',*,*,#39299,.F.);
#54711=ORIENTED_EDGE('',*,*,#39300,.F.);
#54712=ORIENTED_EDGE('',*,*,#39295,.F.);
#54713=ORIENTED_EDGE('',*,*,#39300,.T.);
#54714=ORIENTED_EDGE('',*,*,#39301,.F.);
#54715=ORIENTED_EDGE('',*,*,#39017,.T.);
#54716=ORIENTED_EDGE('',*,*,#39296,.T.);
#54717=ORIENTED_EDGE('',*,*,#39302,.F.);
#54718=ORIENTED_EDGE('',*,*,#39303,.F.);
#54719=ORIENTED_EDGE('',*,*,#39107,.F.);
#54720=ORIENTED_EDGE('',*,*,#39304,.F.);
#54721=ORIENTED_EDGE('',*,*,#39304,.T.);
#54722=ORIENTED_EDGE('',*,*,#39109,.T.);
#54723=ORIENTED_EDGE('',*,*,#39019,.T.);
#54724=ORIENTED_EDGE('',*,*,#39305,.F.);
#54725=ORIENTED_EDGE('',*,*,#39020,.T.);
#54726=ORIENTED_EDGE('',*,*,#39306,.F.);
#54727=ORIENTED_EDGE('',*,*,#39307,.T.);
#54728=ORIENTED_EDGE('',*,*,#39308,.F.);
#54729=ORIENTED_EDGE('',*,*,#39022,.T.);
#54730=ORIENTED_EDGE('',*,*,#39309,.F.);
#54731=ORIENTED_EDGE('',*,*,#39310,.T.);
#54732=ORIENTED_EDGE('',*,*,#39311,.F.);
#54733=ORIENTED_EDGE('',*,*,#39023,.T.);
#54734=ORIENTED_EDGE('',*,*,#39311,.T.);
#54735=ORIENTED_EDGE('',*,*,#39312,.T.);
#54736=ORIENTED_EDGE('',*,*,#39313,.F.);
#54737=ORIENTED_EDGE('',*,*,#39312,.F.);
#54738=ORIENTED_EDGE('',*,*,#39310,.F.);
#54739=ORIENTED_EDGE('',*,*,#39314,.F.);
#54740=ORIENTED_EDGE('',*,*,#39315,.F.);
#54741=ORIENTED_EDGE('',*,*,#39025,.T.);
#54742=ORIENTED_EDGE('',*,*,#39316,.F.);
#54743=ORIENTED_EDGE('',*,*,#39317,.T.);
#54744=ORIENTED_EDGE('',*,*,#39318,.F.);
#54745=ORIENTED_EDGE('',*,*,#39026,.T.);
#54746=ORIENTED_EDGE('',*,*,#39318,.T.);
#54747=ORIENTED_EDGE('',*,*,#39319,.T.);
#54748=ORIENTED_EDGE('',*,*,#39320,.F.);
#54749=ORIENTED_EDGE('',*,*,#39319,.F.);
#54750=ORIENTED_EDGE('',*,*,#39317,.F.);
#54751=ORIENTED_EDGE('',*,*,#39321,.F.);
#54752=ORIENTED_EDGE('',*,*,#39322,.F.);
#54753=ORIENTED_EDGE('',*,*,#39028,.T.);
#54754=ORIENTED_EDGE('',*,*,#39323,.F.);
#54755=ORIENTED_EDGE('',*,*,#39324,.T.);
#54756=ORIENTED_EDGE('',*,*,#39325,.F.);
#54757=ORIENTED_EDGE('',*,*,#39029,.T.);
#54758=ORIENTED_EDGE('',*,*,#39325,.T.);
#54759=ORIENTED_EDGE('',*,*,#39326,.T.);
#54760=ORIENTED_EDGE('',*,*,#39327,.F.);
#54761=ORIENTED_EDGE('',*,*,#39326,.F.);
#54762=ORIENTED_EDGE('',*,*,#39324,.F.);
#54763=ORIENTED_EDGE('',*,*,#39328,.F.);
#54764=ORIENTED_EDGE('',*,*,#39329,.F.);
#54765=ORIENTED_EDGE('',*,*,#39031,.T.);
#54766=ORIENTED_EDGE('',*,*,#39330,.F.);
#54767=ORIENTED_EDGE('',*,*,#39331,.T.);
#54768=ORIENTED_EDGE('',*,*,#39332,.F.);
#54769=ORIENTED_EDGE('',*,*,#39032,.T.);
#54770=ORIENTED_EDGE('',*,*,#39332,.T.);
#54771=ORIENTED_EDGE('',*,*,#39333,.T.);
#54772=ORIENTED_EDGE('',*,*,#39334,.F.);
#54773=ORIENTED_EDGE('',*,*,#39333,.F.);
#54774=ORIENTED_EDGE('',*,*,#39331,.F.);
#54775=ORIENTED_EDGE('',*,*,#39335,.F.);
#54776=ORIENTED_EDGE('',*,*,#39336,.F.);
#54777=ORIENTED_EDGE('',*,*,#39034,.T.);
#54778=ORIENTED_EDGE('',*,*,#39337,.F.);
#54779=ORIENTED_EDGE('',*,*,#39338,.T.);
#54780=ORIENTED_EDGE('',*,*,#39339,.F.);
#54781=ORIENTED_EDGE('',*,*,#39035,.T.);
#54782=ORIENTED_EDGE('',*,*,#39339,.T.);
#54783=ORIENTED_EDGE('',*,*,#39340,.T.);
#54784=ORIENTED_EDGE('',*,*,#39341,.F.);
#54785=ORIENTED_EDGE('',*,*,#39340,.F.);
#54786=ORIENTED_EDGE('',*,*,#39338,.F.);
#54787=ORIENTED_EDGE('',*,*,#39342,.F.);
#54788=ORIENTED_EDGE('',*,*,#39343,.F.);
#54789=ORIENTED_EDGE('',*,*,#39037,.T.);
#54790=ORIENTED_EDGE('',*,*,#39344,.F.);
#54791=ORIENTED_EDGE('',*,*,#39345,.T.);
#54792=ORIENTED_EDGE('',*,*,#39346,.F.);
#54793=ORIENTED_EDGE('',*,*,#39038,.T.);
#54794=ORIENTED_EDGE('',*,*,#39346,.T.);
#54795=ORIENTED_EDGE('',*,*,#39347,.T.);
#54796=ORIENTED_EDGE('',*,*,#39348,.F.);
#54797=ORIENTED_EDGE('',*,*,#39347,.F.);
#54798=ORIENTED_EDGE('',*,*,#39345,.F.);
#54799=ORIENTED_EDGE('',*,*,#39349,.F.);
#54800=ORIENTED_EDGE('',*,*,#39350,.F.);
#54801=ORIENTED_EDGE('',*,*,#39040,.T.);
#54802=ORIENTED_EDGE('',*,*,#39351,.F.);
#54803=ORIENTED_EDGE('',*,*,#39352,.T.);
#54804=ORIENTED_EDGE('',*,*,#39353,.F.);
#54805=ORIENTED_EDGE('',*,*,#39041,.T.);
#54806=ORIENTED_EDGE('',*,*,#39353,.T.);
#54807=ORIENTED_EDGE('',*,*,#39354,.T.);
#54808=ORIENTED_EDGE('',*,*,#39355,.F.);
#54809=ORIENTED_EDGE('',*,*,#39354,.F.);
#54810=ORIENTED_EDGE('',*,*,#39352,.F.);
#54811=ORIENTED_EDGE('',*,*,#39356,.F.);
#54812=ORIENTED_EDGE('',*,*,#39357,.F.);
#54813=ORIENTED_EDGE('',*,*,#39043,.T.);
#54814=ORIENTED_EDGE('',*,*,#39358,.F.);
#54815=ORIENTED_EDGE('',*,*,#39359,.T.);
#54816=ORIENTED_EDGE('',*,*,#39360,.F.);
#54817=ORIENTED_EDGE('',*,*,#39044,.T.);
#54818=ORIENTED_EDGE('',*,*,#39360,.T.);
#54819=ORIENTED_EDGE('',*,*,#39361,.T.);
#54820=ORIENTED_EDGE('',*,*,#39362,.F.);
#54821=ORIENTED_EDGE('',*,*,#39361,.F.);
#54822=ORIENTED_EDGE('',*,*,#39359,.F.);
#54823=ORIENTED_EDGE('',*,*,#39363,.F.);
#54824=ORIENTED_EDGE('',*,*,#39364,.F.);
#54825=ORIENTED_EDGE('',*,*,#39046,.T.);
#54826=ORIENTED_EDGE('',*,*,#39365,.F.);
#54827=ORIENTED_EDGE('',*,*,#39366,.T.);
#54828=ORIENTED_EDGE('',*,*,#39367,.F.);
#54829=ORIENTED_EDGE('',*,*,#39047,.T.);
#54830=ORIENTED_EDGE('',*,*,#39367,.T.);
#54831=ORIENTED_EDGE('',*,*,#39368,.T.);
#54832=ORIENTED_EDGE('',*,*,#39369,.F.);
#54833=ORIENTED_EDGE('',*,*,#39368,.F.);
#54834=ORIENTED_EDGE('',*,*,#39366,.F.);
#54835=ORIENTED_EDGE('',*,*,#39370,.F.);
#54836=ORIENTED_EDGE('',*,*,#39371,.F.);
#54837=ORIENTED_EDGE('',*,*,#39049,.T.);
#54838=ORIENTED_EDGE('',*,*,#39372,.F.);
#54839=ORIENTED_EDGE('',*,*,#39373,.T.);
#54840=ORIENTED_EDGE('',*,*,#39374,.F.);
#54841=ORIENTED_EDGE('',*,*,#39050,.T.);
#54842=ORIENTED_EDGE('',*,*,#39374,.T.);
#54843=ORIENTED_EDGE('',*,*,#39375,.T.);
#54844=ORIENTED_EDGE('',*,*,#39376,.F.);
#54845=ORIENTED_EDGE('',*,*,#39375,.F.);
#54846=ORIENTED_EDGE('',*,*,#39373,.F.);
#54847=ORIENTED_EDGE('',*,*,#39377,.F.);
#54848=ORIENTED_EDGE('',*,*,#39378,.F.);
#54849=ORIENTED_EDGE('',*,*,#39052,.T.);
#54850=ORIENTED_EDGE('',*,*,#39379,.F.);
#54851=ORIENTED_EDGE('',*,*,#39380,.T.);
#54852=ORIENTED_EDGE('',*,*,#39381,.F.);
#54853=ORIENTED_EDGE('',*,*,#39053,.T.);
#54854=ORIENTED_EDGE('',*,*,#39381,.T.);
#54855=ORIENTED_EDGE('',*,*,#39382,.T.);
#54856=ORIENTED_EDGE('',*,*,#39383,.F.);
#54857=ORIENTED_EDGE('',*,*,#39382,.F.);
#54858=ORIENTED_EDGE('',*,*,#39380,.F.);
#54859=ORIENTED_EDGE('',*,*,#39384,.F.);
#54860=ORIENTED_EDGE('',*,*,#39385,.F.);
#54861=ORIENTED_EDGE('',*,*,#39055,.T.);
#54862=ORIENTED_EDGE('',*,*,#39386,.F.);
#54863=ORIENTED_EDGE('',*,*,#39387,.T.);
#54864=ORIENTED_EDGE('',*,*,#39388,.F.);
#54865=ORIENTED_EDGE('',*,*,#39056,.T.);
#54866=ORIENTED_EDGE('',*,*,#39388,.T.);
#54867=ORIENTED_EDGE('',*,*,#39389,.T.);
#54868=ORIENTED_EDGE('',*,*,#39390,.F.);
#54869=ORIENTED_EDGE('',*,*,#39389,.F.);
#54870=ORIENTED_EDGE('',*,*,#39387,.F.);
#54871=ORIENTED_EDGE('',*,*,#39391,.F.);
#54872=ORIENTED_EDGE('',*,*,#39392,.F.);
#54873=ORIENTED_EDGE('',*,*,#39058,.T.);
#54874=ORIENTED_EDGE('',*,*,#39393,.F.);
#54875=ORIENTED_EDGE('',*,*,#39394,.T.);
#54876=ORIENTED_EDGE('',*,*,#39395,.F.);
#54877=ORIENTED_EDGE('',*,*,#39059,.T.);
#54878=ORIENTED_EDGE('',*,*,#39395,.T.);
#54879=ORIENTED_EDGE('',*,*,#39396,.T.);
#54880=ORIENTED_EDGE('',*,*,#39397,.F.);
#54881=ORIENTED_EDGE('',*,*,#39396,.F.);
#54882=ORIENTED_EDGE('',*,*,#39394,.F.);
#54883=ORIENTED_EDGE('',*,*,#39398,.F.);
#54884=ORIENTED_EDGE('',*,*,#39399,.F.);
#54885=ORIENTED_EDGE('',*,*,#39061,.T.);
#54886=ORIENTED_EDGE('',*,*,#39400,.F.);
#54887=ORIENTED_EDGE('',*,*,#34403,.T.);
#54888=ORIENTED_EDGE('',*,*,#39401,.F.);
#54889=ORIENTED_EDGE('',*,*,#39062,.T.);
#54890=ORIENTED_EDGE('',*,*,#39401,.T.);
#54891=ORIENTED_EDGE('',*,*,#34402,.T.);
#54892=ORIENTED_EDGE('',*,*,#39402,.F.);
#54893=ORIENTED_EDGE('',*,*,#39064,.T.);
#54894=ORIENTED_EDGE('',*,*,#39403,.F.);
#54895=ORIENTED_EDGE('',*,*,#39404,.T.);
#54896=ORIENTED_EDGE('',*,*,#39405,.F.);
#54897=ORIENTED_EDGE('',*,*,#39065,.T.);
#54898=ORIENTED_EDGE('',*,*,#39405,.T.);
#54899=ORIENTED_EDGE('',*,*,#39406,.T.);
#54900=ORIENTED_EDGE('',*,*,#39407,.F.);
#54901=ORIENTED_EDGE('',*,*,#39406,.F.);
#54902=ORIENTED_EDGE('',*,*,#39404,.F.);
#54903=ORIENTED_EDGE('',*,*,#39408,.F.);
#54904=ORIENTED_EDGE('',*,*,#39409,.F.);
#54905=ORIENTED_EDGE('',*,*,#39067,.T.);
#54906=ORIENTED_EDGE('',*,*,#39410,.F.);
#54907=ORIENTED_EDGE('',*,*,#39411,.T.);
#54908=ORIENTED_EDGE('',*,*,#39412,.F.);
#54909=ORIENTED_EDGE('',*,*,#39068,.T.);
#54910=ORIENTED_EDGE('',*,*,#39412,.T.);
#54911=ORIENTED_EDGE('',*,*,#39413,.T.);
#54912=ORIENTED_EDGE('',*,*,#39414,.F.);
#54913=ORIENTED_EDGE('',*,*,#39413,.F.);
#54914=ORIENTED_EDGE('',*,*,#39411,.F.);
#54915=ORIENTED_EDGE('',*,*,#39415,.F.);
#54916=ORIENTED_EDGE('',*,*,#39416,.F.);
#54917=ORIENTED_EDGE('',*,*,#39070,.T.);
#54918=ORIENTED_EDGE('',*,*,#39417,.F.);
#54919=ORIENTED_EDGE('',*,*,#39418,.T.);
#54920=ORIENTED_EDGE('',*,*,#39419,.F.);
#54921=ORIENTED_EDGE('',*,*,#39071,.T.);
#54922=ORIENTED_EDGE('',*,*,#39419,.T.);
#54923=ORIENTED_EDGE('',*,*,#39420,.T.);
#54924=ORIENTED_EDGE('',*,*,#39421,.F.);
#54925=ORIENTED_EDGE('',*,*,#39420,.F.);
#54926=ORIENTED_EDGE('',*,*,#39418,.F.);
#54927=ORIENTED_EDGE('',*,*,#39422,.F.);
#54928=ORIENTED_EDGE('',*,*,#39423,.F.);
#54929=ORIENTED_EDGE('',*,*,#39073,.T.);
#54930=ORIENTED_EDGE('',*,*,#39424,.F.);
#54931=ORIENTED_EDGE('',*,*,#39425,.T.);
#54932=ORIENTED_EDGE('',*,*,#39426,.F.);
#54933=ORIENTED_EDGE('',*,*,#39074,.T.);
#54934=ORIENTED_EDGE('',*,*,#39426,.T.);
#54935=ORIENTED_EDGE('',*,*,#39427,.T.);
#54936=ORIENTED_EDGE('',*,*,#39428,.F.);
#54937=ORIENTED_EDGE('',*,*,#39427,.F.);
#54938=ORIENTED_EDGE('',*,*,#39425,.F.);
#54939=ORIENTED_EDGE('',*,*,#39429,.F.);
#54940=ORIENTED_EDGE('',*,*,#39430,.F.);
#54941=ORIENTED_EDGE('',*,*,#39076,.T.);
#54942=ORIENTED_EDGE('',*,*,#39431,.F.);
#54943=ORIENTED_EDGE('',*,*,#39432,.T.);
#54944=ORIENTED_EDGE('',*,*,#39433,.F.);
#54945=ORIENTED_EDGE('',*,*,#39077,.T.);
#54946=ORIENTED_EDGE('',*,*,#39433,.T.);
#54947=ORIENTED_EDGE('',*,*,#39434,.T.);
#54948=ORIENTED_EDGE('',*,*,#39435,.F.);
#54949=ORIENTED_EDGE('',*,*,#39434,.F.);
#54950=ORIENTED_EDGE('',*,*,#39432,.F.);
#54951=ORIENTED_EDGE('',*,*,#39436,.F.);
#54952=ORIENTED_EDGE('',*,*,#39437,.F.);
#54953=ORIENTED_EDGE('',*,*,#39079,.T.);
#54954=ORIENTED_EDGE('',*,*,#39438,.F.);
#54955=ORIENTED_EDGE('',*,*,#39439,.T.);
#54956=ORIENTED_EDGE('',*,*,#39440,.F.);
#54957=ORIENTED_EDGE('',*,*,#39080,.T.);
#54958=ORIENTED_EDGE('',*,*,#39440,.T.);
#54959=ORIENTED_EDGE('',*,*,#39441,.T.);
#54960=ORIENTED_EDGE('',*,*,#39442,.F.);
#54961=ORIENTED_EDGE('',*,*,#39441,.F.);
#54962=ORIENTED_EDGE('',*,*,#39439,.F.);
#54963=ORIENTED_EDGE('',*,*,#39443,.F.);
#54964=ORIENTED_EDGE('',*,*,#39444,.F.);
#54965=ORIENTED_EDGE('',*,*,#39082,.T.);
#54966=ORIENTED_EDGE('',*,*,#39445,.F.);
#54967=ORIENTED_EDGE('',*,*,#39446,.T.);
#54968=ORIENTED_EDGE('',*,*,#39447,.F.);
#54969=ORIENTED_EDGE('',*,*,#39083,.T.);
#54970=ORIENTED_EDGE('',*,*,#39447,.T.);
#54971=ORIENTED_EDGE('',*,*,#39448,.T.);
#54972=ORIENTED_EDGE('',*,*,#39449,.F.);
#54973=ORIENTED_EDGE('',*,*,#39448,.F.);
#54974=ORIENTED_EDGE('',*,*,#39446,.F.);
#54975=ORIENTED_EDGE('',*,*,#39450,.F.);
#54976=ORIENTED_EDGE('',*,*,#39451,.F.);
#54977=ORIENTED_EDGE('',*,*,#39085,.T.);
#54978=ORIENTED_EDGE('',*,*,#39452,.F.);
#54979=ORIENTED_EDGE('',*,*,#39453,.T.);
#54980=ORIENTED_EDGE('',*,*,#39454,.F.);
#54981=ORIENTED_EDGE('',*,*,#39086,.T.);
#54982=ORIENTED_EDGE('',*,*,#39454,.T.);
#54983=ORIENTED_EDGE('',*,*,#39455,.T.);
#54984=ORIENTED_EDGE('',*,*,#39456,.F.);
#54985=ORIENTED_EDGE('',*,*,#39455,.F.);
#54986=ORIENTED_EDGE('',*,*,#39453,.F.);
#54987=ORIENTED_EDGE('',*,*,#39457,.F.);
#54988=ORIENTED_EDGE('',*,*,#39458,.F.);
#54989=ORIENTED_EDGE('',*,*,#39088,.T.);
#54990=ORIENTED_EDGE('',*,*,#39459,.F.);
#54991=ORIENTED_EDGE('',*,*,#39460,.T.);
#54992=ORIENTED_EDGE('',*,*,#39461,.F.);
#54993=ORIENTED_EDGE('',*,*,#39089,.T.);
#54994=ORIENTED_EDGE('',*,*,#39461,.T.);
#54995=ORIENTED_EDGE('',*,*,#39462,.T.);
#54996=ORIENTED_EDGE('',*,*,#39463,.F.);
#54997=ORIENTED_EDGE('',*,*,#39462,.F.);
#54998=ORIENTED_EDGE('',*,*,#39460,.F.);
#54999=ORIENTED_EDGE('',*,*,#39464,.F.);
#55000=ORIENTED_EDGE('',*,*,#39465,.F.);
#55001=ORIENTED_EDGE('',*,*,#39091,.T.);
#55002=ORIENTED_EDGE('',*,*,#39466,.F.);
#55003=ORIENTED_EDGE('',*,*,#39467,.T.);
#55004=ORIENTED_EDGE('',*,*,#39468,.F.);
#55005=ORIENTED_EDGE('',*,*,#39092,.T.);
#55006=ORIENTED_EDGE('',*,*,#39468,.T.);
#55007=ORIENTED_EDGE('',*,*,#39469,.T.);
#55008=ORIENTED_EDGE('',*,*,#39470,.F.);
#55009=ORIENTED_EDGE('',*,*,#39469,.F.);
#55010=ORIENTED_EDGE('',*,*,#39467,.F.);
#55011=ORIENTED_EDGE('',*,*,#39471,.F.);
#55012=ORIENTED_EDGE('',*,*,#39472,.F.);
#55013=ORIENTED_EDGE('',*,*,#39094,.T.);
#55014=ORIENTED_EDGE('',*,*,#39473,.F.);
#55015=ORIENTED_EDGE('',*,*,#39474,.T.);
#55016=ORIENTED_EDGE('',*,*,#39475,.F.);
#55017=ORIENTED_EDGE('',*,*,#39095,.T.);
#55018=ORIENTED_EDGE('',*,*,#39475,.T.);
#55019=ORIENTED_EDGE('',*,*,#39476,.T.);
#55020=ORIENTED_EDGE('',*,*,#39477,.F.);
#55021=ORIENTED_EDGE('',*,*,#39476,.F.);
#55022=ORIENTED_EDGE('',*,*,#39474,.F.);
#55023=ORIENTED_EDGE('',*,*,#39478,.F.);
#55024=ORIENTED_EDGE('',*,*,#39479,.F.);
#55025=ORIENTED_EDGE('',*,*,#39097,.T.);
#55026=ORIENTED_EDGE('',*,*,#39480,.F.);
#55027=ORIENTED_EDGE('',*,*,#39481,.T.);
#55028=ORIENTED_EDGE('',*,*,#39482,.F.);
#55029=ORIENTED_EDGE('',*,*,#39098,.T.);
#55030=ORIENTED_EDGE('',*,*,#39482,.T.);
#55031=ORIENTED_EDGE('',*,*,#39483,.T.);
#55032=ORIENTED_EDGE('',*,*,#39484,.F.);
#55033=ORIENTED_EDGE('',*,*,#39483,.F.);
#55034=ORIENTED_EDGE('',*,*,#39481,.F.);
#55035=ORIENTED_EDGE('',*,*,#39485,.F.);
#55036=ORIENTED_EDGE('',*,*,#39486,.F.);
#55037=ORIENTED_EDGE('',*,*,#39100,.T.);
#55038=ORIENTED_EDGE('',*,*,#39487,.F.);
#55039=ORIENTED_EDGE('',*,*,#39488,.T.);
#55040=ORIENTED_EDGE('',*,*,#39489,.F.);
#55041=ORIENTED_EDGE('',*,*,#39490,.T.);
#55042=ORIENTED_EDGE('',*,*,#39491,.F.);
#55043=ORIENTED_EDGE('',*,*,#39101,.T.);
#55044=ORIENTED_EDGE('',*,*,#39489,.T.);
#55045=ORIENTED_EDGE('',*,*,#39492,.F.);
#55046=ORIENTED_EDGE('',*,*,#39493,.F.);
#55047=ORIENTED_EDGE('',*,*,#39490,.F.);
#55048=ORIENTED_EDGE('',*,*,#39488,.F.);
#55049=ORIENTED_EDGE('',*,*,#39103,.T.);
#55050=ORIENTED_EDGE('',*,*,#39494,.F.);
#55051=ORIENTED_EDGE('',*,*,#39495,.T.);
#55052=ORIENTED_EDGE('',*,*,#39496,.F.);
#55053=ORIENTED_EDGE('',*,*,#39104,.T.);
#55054=ORIENTED_EDGE('',*,*,#39496,.T.);
#55055=ORIENTED_EDGE('',*,*,#39497,.T.);
#55056=ORIENTED_EDGE('',*,*,#39498,.F.);
#55057=ORIENTED_EDGE('',*,*,#39497,.F.);
#55058=ORIENTED_EDGE('',*,*,#39495,.F.);
#55059=ORIENTED_EDGE('',*,*,#39499,.F.);
#55060=ORIENTED_EDGE('',*,*,#39500,.F.);
#55061=ORIENTED_EDGE('',*,*,#39307,.F.);
#55062=ORIENTED_EDGE('',*,*,#39501,.F.);
#55063=ORIENTED_EDGE('',*,*,#39502,.F.);
#55064=ORIENTED_EDGE('',*,*,#39503,.F.);
#55065=ORIENTED_EDGE('',*,*,#39106,.T.);
#55066=ORIENTED_EDGE('',*,*,#39504,.F.);
#55067=ORIENTED_EDGE('',*,*,#39501,.T.);
#55068=ORIENTED_EDGE('',*,*,#39306,.T.);
#55069=ORIENTED_EDGE('',*,*,#39505,.F.);
#55070=ORIENTED_EDGE('',*,*,#39108,.T.);
#55071=ORIENTED_EDGE('',*,*,#39303,.T.);
#55072=ORIENTED_EDGE('',*,*,#39506,.F.);
#55073=ORIENTED_EDGE('',*,*,#39507,.F.);
#55074=ORIENTED_EDGE('',*,*,#39508,.F.);
#55075=ORIENTED_EDGE('',*,*,#39113,.T.);
#55076=ORIENTED_EDGE('',*,*,#39112,.T.);
#55077=ORIENTED_EDGE('',*,*,#39509,.F.);
#55078=ORIENTED_EDGE('',*,*,#39116,.T.);
#55079=ORIENTED_EDGE('',*,*,#39114,.T.);
#55080=ORIENTED_EDGE('',*,*,#39508,.T.);
#55081=ORIENTED_EDGE('',*,*,#39510,.F.);
#55082=ORIENTED_EDGE('',*,*,#39511,.F.);
#55083=ORIENTED_EDGE('',*,*,#39120,.T.);
#55084=ORIENTED_EDGE('',*,*,#39119,.T.);
#55085=ORIENTED_EDGE('',*,*,#39512,.F.);
#55086=ORIENTED_EDGE('',*,*,#39123,.T.);
#55087=ORIENTED_EDGE('',*,*,#39121,.T.);
#55088=ORIENTED_EDGE('',*,*,#39511,.T.);
#55089=ORIENTED_EDGE('',*,*,#39513,.F.);
#55090=ORIENTED_EDGE('',*,*,#39514,.F.);
#55091=ORIENTED_EDGE('',*,*,#39127,.T.);
#55092=ORIENTED_EDGE('',*,*,#39126,.T.);
#55093=ORIENTED_EDGE('',*,*,#39515,.F.);
#55094=ORIENTED_EDGE('',*,*,#39130,.T.);
#55095=ORIENTED_EDGE('',*,*,#39128,.T.);
#55096=ORIENTED_EDGE('',*,*,#39514,.T.);
#55097=ORIENTED_EDGE('',*,*,#39516,.F.);
#55098=ORIENTED_EDGE('',*,*,#39517,.F.);
#55099=ORIENTED_EDGE('',*,*,#39134,.T.);
#55100=ORIENTED_EDGE('',*,*,#39133,.T.);
#55101=ORIENTED_EDGE('',*,*,#39518,.F.);
#55102=ORIENTED_EDGE('',*,*,#39137,.T.);
#55103=ORIENTED_EDGE('',*,*,#39135,.T.);
#55104=ORIENTED_EDGE('',*,*,#39517,.T.);
#55105=ORIENTED_EDGE('',*,*,#39519,.F.);
#55106=ORIENTED_EDGE('',*,*,#39520,.F.);
#55107=ORIENTED_EDGE('',*,*,#39141,.T.);
#55108=ORIENTED_EDGE('',*,*,#39140,.T.);
#55109=ORIENTED_EDGE('',*,*,#39521,.F.);
#55110=ORIENTED_EDGE('',*,*,#39144,.T.);
#55111=ORIENTED_EDGE('',*,*,#39142,.T.);
#55112=ORIENTED_EDGE('',*,*,#39520,.T.);
#55113=ORIENTED_EDGE('',*,*,#39522,.F.);
#55114=ORIENTED_EDGE('',*,*,#39523,.F.);
#55115=ORIENTED_EDGE('',*,*,#39148,.T.);
#55116=ORIENTED_EDGE('',*,*,#39147,.T.);
#55117=ORIENTED_EDGE('',*,*,#39524,.F.);
#55118=ORIENTED_EDGE('',*,*,#39151,.T.);
#55119=ORIENTED_EDGE('',*,*,#39149,.T.);
#55120=ORIENTED_EDGE('',*,*,#39523,.T.);
#55121=ORIENTED_EDGE('',*,*,#39525,.F.);
#55122=ORIENTED_EDGE('',*,*,#39526,.F.);
#55123=ORIENTED_EDGE('',*,*,#34407,.T.);
#55124=ORIENTED_EDGE('',*,*,#39153,.T.);
#55125=ORIENTED_EDGE('',*,*,#39527,.F.);
#55126=ORIENTED_EDGE('',*,*,#39154,.T.);
#55127=ORIENTED_EDGE('',*,*,#34408,.T.);
#55128=ORIENTED_EDGE('',*,*,#39526,.T.);
#55129=ORIENTED_EDGE('',*,*,#39528,.F.);
#55130=ORIENTED_EDGE('',*,*,#39529,.F.);
#55131=ORIENTED_EDGE('',*,*,#39158,.T.);
#55132=ORIENTED_EDGE('',*,*,#39157,.T.);
#55133=ORIENTED_EDGE('',*,*,#39530,.F.);
#55134=ORIENTED_EDGE('',*,*,#39161,.T.);
#55135=ORIENTED_EDGE('',*,*,#39159,.T.);
#55136=ORIENTED_EDGE('',*,*,#39529,.T.);
#55137=ORIENTED_EDGE('',*,*,#39531,.F.);
#55138=ORIENTED_EDGE('',*,*,#39532,.F.);
#55139=ORIENTED_EDGE('',*,*,#39165,.T.);
#55140=ORIENTED_EDGE('',*,*,#39164,.T.);
#55141=ORIENTED_EDGE('',*,*,#39533,.F.);
#55142=ORIENTED_EDGE('',*,*,#39168,.T.);
#55143=ORIENTED_EDGE('',*,*,#39166,.T.);
#55144=ORIENTED_EDGE('',*,*,#39532,.T.);
#55145=ORIENTED_EDGE('',*,*,#39534,.F.);
#55146=ORIENTED_EDGE('',*,*,#39535,.F.);
#55147=ORIENTED_EDGE('',*,*,#39172,.T.);
#55148=ORIENTED_EDGE('',*,*,#39171,.T.);
#55149=ORIENTED_EDGE('',*,*,#39536,.F.);
#55150=ORIENTED_EDGE('',*,*,#39175,.T.);
#55151=ORIENTED_EDGE('',*,*,#39173,.T.);
#55152=ORIENTED_EDGE('',*,*,#39535,.T.);
#55153=ORIENTED_EDGE('',*,*,#39537,.F.);
#55154=ORIENTED_EDGE('',*,*,#39538,.F.);
#55155=ORIENTED_EDGE('',*,*,#39179,.T.);
#55156=ORIENTED_EDGE('',*,*,#39178,.T.);
#55157=ORIENTED_EDGE('',*,*,#39539,.F.);
#55158=ORIENTED_EDGE('',*,*,#39182,.T.);
#55159=ORIENTED_EDGE('',*,*,#39180,.T.);
#55160=ORIENTED_EDGE('',*,*,#39538,.T.);
#55161=ORIENTED_EDGE('',*,*,#39540,.F.);
#55162=ORIENTED_EDGE('',*,*,#39541,.F.);
#55163=ORIENTED_EDGE('',*,*,#39186,.T.);
#55164=ORIENTED_EDGE('',*,*,#39185,.T.);
#55165=ORIENTED_EDGE('',*,*,#39542,.F.);
#55166=ORIENTED_EDGE('',*,*,#39189,.T.);
#55167=ORIENTED_EDGE('',*,*,#39187,.T.);
#55168=ORIENTED_EDGE('',*,*,#39541,.T.);
#55169=ORIENTED_EDGE('',*,*,#39543,.F.);
#55170=ORIENTED_EDGE('',*,*,#39544,.F.);
#55171=ORIENTED_EDGE('',*,*,#39193,.T.);
#55172=ORIENTED_EDGE('',*,*,#39192,.T.);
#55173=ORIENTED_EDGE('',*,*,#39545,.F.);
#55174=ORIENTED_EDGE('',*,*,#39196,.T.);
#55175=ORIENTED_EDGE('',*,*,#39194,.T.);
#55176=ORIENTED_EDGE('',*,*,#39544,.T.);
#55177=ORIENTED_EDGE('',*,*,#39546,.F.);
#55178=ORIENTED_EDGE('',*,*,#39547,.F.);
#55179=ORIENTED_EDGE('',*,*,#39200,.T.);
#55180=ORIENTED_EDGE('',*,*,#39199,.T.);
#55181=ORIENTED_EDGE('',*,*,#39548,.F.);
#55182=ORIENTED_EDGE('',*,*,#39203,.T.);
#55183=ORIENTED_EDGE('',*,*,#39201,.T.);
#55184=ORIENTED_EDGE('',*,*,#39547,.T.);
#55185=ORIENTED_EDGE('',*,*,#39549,.F.);
#55186=ORIENTED_EDGE('',*,*,#39550,.F.);
#55187=ORIENTED_EDGE('',*,*,#39207,.T.);
#55188=ORIENTED_EDGE('',*,*,#39206,.T.);
#55189=ORIENTED_EDGE('',*,*,#39551,.F.);
#55190=ORIENTED_EDGE('',*,*,#39210,.T.);
#55191=ORIENTED_EDGE('',*,*,#39208,.T.);
#55192=ORIENTED_EDGE('',*,*,#39550,.T.);
#55193=ORIENTED_EDGE('',*,*,#39552,.F.);
#55194=ORIENTED_EDGE('',*,*,#39553,.F.);
#55195=ORIENTED_EDGE('',*,*,#39214,.T.);
#55196=ORIENTED_EDGE('',*,*,#39213,.T.);
#55197=ORIENTED_EDGE('',*,*,#39554,.F.);
#55198=ORIENTED_EDGE('',*,*,#39217,.T.);
#55199=ORIENTED_EDGE('',*,*,#39215,.T.);
#55200=ORIENTED_EDGE('',*,*,#39553,.T.);
#55201=ORIENTED_EDGE('',*,*,#39555,.F.);
#55202=ORIENTED_EDGE('',*,*,#39556,.F.);
#55203=ORIENTED_EDGE('',*,*,#39221,.T.);
#55204=ORIENTED_EDGE('',*,*,#39220,.T.);
#55205=ORIENTED_EDGE('',*,*,#39557,.F.);
#55206=ORIENTED_EDGE('',*,*,#39224,.T.);
#55207=ORIENTED_EDGE('',*,*,#39222,.T.);
#55208=ORIENTED_EDGE('',*,*,#39556,.T.);
#55209=ORIENTED_EDGE('',*,*,#39558,.F.);
#55210=ORIENTED_EDGE('',*,*,#39559,.F.);
#55211=ORIENTED_EDGE('',*,*,#39228,.T.);
#55212=ORIENTED_EDGE('',*,*,#39227,.T.);
#55213=ORIENTED_EDGE('',*,*,#39560,.F.);
#55214=ORIENTED_EDGE('',*,*,#39231,.T.);
#55215=ORIENTED_EDGE('',*,*,#39229,.T.);
#55216=ORIENTED_EDGE('',*,*,#39559,.T.);
#55217=ORIENTED_EDGE('',*,*,#39561,.F.);
#55218=ORIENTED_EDGE('',*,*,#39562,.F.);
#55219=ORIENTED_EDGE('',*,*,#39235,.T.);
#55220=ORIENTED_EDGE('',*,*,#39234,.T.);
#55221=ORIENTED_EDGE('',*,*,#39563,.F.);
#55222=ORIENTED_EDGE('',*,*,#39238,.T.);
#55223=ORIENTED_EDGE('',*,*,#39236,.T.);
#55224=ORIENTED_EDGE('',*,*,#39562,.T.);
#55225=ORIENTED_EDGE('',*,*,#39564,.F.);
#55226=ORIENTED_EDGE('',*,*,#39565,.F.);
#55227=ORIENTED_EDGE('',*,*,#39242,.T.);
#55228=ORIENTED_EDGE('',*,*,#39241,.T.);
#55229=ORIENTED_EDGE('',*,*,#39566,.F.);
#55230=ORIENTED_EDGE('',*,*,#39245,.T.);
#55231=ORIENTED_EDGE('',*,*,#39243,.T.);
#55232=ORIENTED_EDGE('',*,*,#39565,.T.);
#55233=ORIENTED_EDGE('',*,*,#39567,.F.);
#55234=ORIENTED_EDGE('',*,*,#39568,.F.);
#55235=ORIENTED_EDGE('',*,*,#39251,.T.);
#55236=ORIENTED_EDGE('',*,*,#39248,.T.);
#55237=ORIENTED_EDGE('',*,*,#39252,.T.);
#55238=ORIENTED_EDGE('',*,*,#39568,.T.);
#55239=ORIENTED_EDGE('',*,*,#39569,.F.);
#55240=ORIENTED_EDGE('',*,*,#39250,.T.);
#55241=ORIENTED_EDGE('',*,*,#39257,.T.);
#55242=ORIENTED_EDGE('',*,*,#39253,.T.);
#55243=ORIENTED_EDGE('',*,*,#39570,.F.);
#55244=ORIENTED_EDGE('',*,*,#39571,.F.);
#55245=ORIENTED_EDGE('',*,*,#39572,.F.);
#55246=ORIENTED_EDGE('',*,*,#39259,.T.);
#55247=ORIENTED_EDGE('',*,*,#39258,.T.);
#55248=ORIENTED_EDGE('',*,*,#39571,.T.);
#55249=ORIENTED_EDGE('',*,*,#39573,.F.);
#55250=ORIENTED_EDGE('',*,*,#39574,.F.);
#55251=ORIENTED_EDGE('',*,*,#39263,.T.);
#55252=ORIENTED_EDGE('',*,*,#39262,.T.);
#55253=ORIENTED_EDGE('',*,*,#39575,.F.);
#55254=ORIENTED_EDGE('',*,*,#39266,.T.);
#55255=ORIENTED_EDGE('',*,*,#39264,.T.);
#55256=ORIENTED_EDGE('',*,*,#39574,.T.);
#55257=ORIENTED_EDGE('',*,*,#39576,.F.);
#55258=ORIENTED_EDGE('',*,*,#39577,.F.);
#55259=ORIENTED_EDGE('',*,*,#39270,.T.);
#55260=ORIENTED_EDGE('',*,*,#39269,.T.);
#55261=ORIENTED_EDGE('',*,*,#39578,.F.);
#55262=ORIENTED_EDGE('',*,*,#39273,.T.);
#55263=ORIENTED_EDGE('',*,*,#39271,.T.);
#55264=ORIENTED_EDGE('',*,*,#39577,.T.);
#55265=ORIENTED_EDGE('',*,*,#39579,.F.);
#55266=ORIENTED_EDGE('',*,*,#39580,.F.);
#55267=ORIENTED_EDGE('',*,*,#39277,.T.);
#55268=ORIENTED_EDGE('',*,*,#39276,.T.);
#55269=ORIENTED_EDGE('',*,*,#39581,.F.);
#55270=ORIENTED_EDGE('',*,*,#39280,.T.);
#55271=ORIENTED_EDGE('',*,*,#39278,.T.);
#55272=ORIENTED_EDGE('',*,*,#39580,.T.);
#55273=ORIENTED_EDGE('',*,*,#39582,.F.);
#55274=ORIENTED_EDGE('',*,*,#39583,.F.);
#55275=ORIENTED_EDGE('',*,*,#39284,.T.);
#55276=ORIENTED_EDGE('',*,*,#39283,.T.);
#55277=ORIENTED_EDGE('',*,*,#39584,.F.);
#55278=ORIENTED_EDGE('',*,*,#39287,.T.);
#55279=ORIENTED_EDGE('',*,*,#39285,.T.);
#55280=ORIENTED_EDGE('',*,*,#39583,.T.);
#55281=ORIENTED_EDGE('',*,*,#39585,.F.);
#55282=ORIENTED_EDGE('',*,*,#39586,.F.);
#55283=ORIENTED_EDGE('',*,*,#39291,.T.);
#55284=ORIENTED_EDGE('',*,*,#39290,.T.);
#55285=ORIENTED_EDGE('',*,*,#39587,.F.);
#55286=ORIENTED_EDGE('',*,*,#39294,.T.);
#55287=ORIENTED_EDGE('',*,*,#39292,.T.);
#55288=ORIENTED_EDGE('',*,*,#39586,.T.);
#55289=ORIENTED_EDGE('',*,*,#39588,.F.);
#55290=ORIENTED_EDGE('',*,*,#39589,.F.);
#55291=ORIENTED_EDGE('',*,*,#39298,.T.);
#55292=ORIENTED_EDGE('',*,*,#39297,.T.);
#55293=ORIENTED_EDGE('',*,*,#39590,.F.);
#55294=ORIENTED_EDGE('',*,*,#39301,.T.);
#55295=ORIENTED_EDGE('',*,*,#39299,.T.);
#55296=ORIENTED_EDGE('',*,*,#39589,.T.);
#55297=ORIENTED_EDGE('',*,*,#39591,.F.);
#55298=ORIENTED_EDGE('',*,*,#39506,.T.);
#55299=ORIENTED_EDGE('',*,*,#39302,.T.);
#55300=ORIENTED_EDGE('',*,*,#39305,.T.);
#55301=ORIENTED_EDGE('',*,*,#39503,.T.);
#55302=ORIENTED_EDGE('',*,*,#39592,.F.);
#55303=ORIENTED_EDGE('',*,*,#39593,.F.);
#55304=ORIENTED_EDGE('',*,*,#39308,.T.);
#55305=ORIENTED_EDGE('',*,*,#39314,.T.);
#55306=ORIENTED_EDGE('',*,*,#39309,.T.);
#55307=ORIENTED_EDGE('',*,*,#39594,.F.);
#55308=ORIENTED_EDGE('',*,*,#39595,.F.);
#55309=ORIENTED_EDGE('',*,*,#39315,.T.);
#55310=ORIENTED_EDGE('',*,*,#39595,.T.);
#55311=ORIENTED_EDGE('',*,*,#39596,.F.);
#55312=ORIENTED_EDGE('',*,*,#39313,.T.);
#55313=ORIENTED_EDGE('',*,*,#39321,.T.);
#55314=ORIENTED_EDGE('',*,*,#39316,.T.);
#55315=ORIENTED_EDGE('',*,*,#39597,.F.);
#55316=ORIENTED_EDGE('',*,*,#39598,.F.);
#55317=ORIENTED_EDGE('',*,*,#39322,.T.);
#55318=ORIENTED_EDGE('',*,*,#39598,.T.);
#55319=ORIENTED_EDGE('',*,*,#39599,.F.);
#55320=ORIENTED_EDGE('',*,*,#39320,.T.);
#55321=ORIENTED_EDGE('',*,*,#39328,.T.);
#55322=ORIENTED_EDGE('',*,*,#39323,.T.);
#55323=ORIENTED_EDGE('',*,*,#39600,.F.);
#55324=ORIENTED_EDGE('',*,*,#39601,.F.);
#55325=ORIENTED_EDGE('',*,*,#39329,.T.);
#55326=ORIENTED_EDGE('',*,*,#39601,.T.);
#55327=ORIENTED_EDGE('',*,*,#39602,.F.);
#55328=ORIENTED_EDGE('',*,*,#39327,.T.);
#55329=ORIENTED_EDGE('',*,*,#39335,.T.);
#55330=ORIENTED_EDGE('',*,*,#39330,.T.);
#55331=ORIENTED_EDGE('',*,*,#39603,.F.);
#55332=ORIENTED_EDGE('',*,*,#39604,.F.);
#55333=ORIENTED_EDGE('',*,*,#39336,.T.);
#55334=ORIENTED_EDGE('',*,*,#39604,.T.);
#55335=ORIENTED_EDGE('',*,*,#39605,.F.);
#55336=ORIENTED_EDGE('',*,*,#39334,.T.);
#55337=ORIENTED_EDGE('',*,*,#39342,.T.);
#55338=ORIENTED_EDGE('',*,*,#39337,.T.);
#55339=ORIENTED_EDGE('',*,*,#39606,.F.);
#55340=ORIENTED_EDGE('',*,*,#39607,.F.);
#55341=ORIENTED_EDGE('',*,*,#39343,.T.);
#55342=ORIENTED_EDGE('',*,*,#39607,.T.);
#55343=ORIENTED_EDGE('',*,*,#39608,.F.);
#55344=ORIENTED_EDGE('',*,*,#39341,.T.);
#55345=ORIENTED_EDGE('',*,*,#39349,.T.);
#55346=ORIENTED_EDGE('',*,*,#39344,.T.);
#55347=ORIENTED_EDGE('',*,*,#39609,.F.);
#55348=ORIENTED_EDGE('',*,*,#39610,.F.);
#55349=ORIENTED_EDGE('',*,*,#39350,.T.);
#55350=ORIENTED_EDGE('',*,*,#39610,.T.);
#55351=ORIENTED_EDGE('',*,*,#39611,.F.);
#55352=ORIENTED_EDGE('',*,*,#39348,.T.);
#55353=ORIENTED_EDGE('',*,*,#39356,.T.);
#55354=ORIENTED_EDGE('',*,*,#39351,.T.);
#55355=ORIENTED_EDGE('',*,*,#39612,.F.);
#55356=ORIENTED_EDGE('',*,*,#39613,.F.);
#55357=ORIENTED_EDGE('',*,*,#39357,.T.);
#55358=ORIENTED_EDGE('',*,*,#39613,.T.);
#55359=ORIENTED_EDGE('',*,*,#39614,.F.);
#55360=ORIENTED_EDGE('',*,*,#39355,.T.);
#55361=ORIENTED_EDGE('',*,*,#39363,.T.);
#55362=ORIENTED_EDGE('',*,*,#39358,.T.);
#55363=ORIENTED_EDGE('',*,*,#39615,.F.);
#55364=ORIENTED_EDGE('',*,*,#39616,.F.);
#55365=ORIENTED_EDGE('',*,*,#39364,.T.);
#55366=ORIENTED_EDGE('',*,*,#39616,.T.);
#55367=ORIENTED_EDGE('',*,*,#39617,.F.);
#55368=ORIENTED_EDGE('',*,*,#39362,.T.);
#55369=ORIENTED_EDGE('',*,*,#39370,.T.);
#55370=ORIENTED_EDGE('',*,*,#39365,.T.);
#55371=ORIENTED_EDGE('',*,*,#39618,.F.);
#55372=ORIENTED_EDGE('',*,*,#39619,.F.);
#55373=ORIENTED_EDGE('',*,*,#39371,.T.);
#55374=ORIENTED_EDGE('',*,*,#39619,.T.);
#55375=ORIENTED_EDGE('',*,*,#39620,.F.);
#55376=ORIENTED_EDGE('',*,*,#39369,.T.);
#55377=ORIENTED_EDGE('',*,*,#39377,.T.);
#55378=ORIENTED_EDGE('',*,*,#39372,.T.);
#55379=ORIENTED_EDGE('',*,*,#39621,.F.);
#55380=ORIENTED_EDGE('',*,*,#39622,.F.);
#55381=ORIENTED_EDGE('',*,*,#39378,.T.);
#55382=ORIENTED_EDGE('',*,*,#39622,.T.);
#55383=ORIENTED_EDGE('',*,*,#39623,.F.);
#55384=ORIENTED_EDGE('',*,*,#39376,.T.);
#55385=ORIENTED_EDGE('',*,*,#39384,.T.);
#55386=ORIENTED_EDGE('',*,*,#39379,.T.);
#55387=ORIENTED_EDGE('',*,*,#39624,.F.);
#55388=ORIENTED_EDGE('',*,*,#39625,.F.);
#55389=ORIENTED_EDGE('',*,*,#39385,.T.);
#55390=ORIENTED_EDGE('',*,*,#39625,.T.);
#55391=ORIENTED_EDGE('',*,*,#39626,.F.);
#55392=ORIENTED_EDGE('',*,*,#39383,.T.);
#55393=ORIENTED_EDGE('',*,*,#39391,.T.);
#55394=ORIENTED_EDGE('',*,*,#39386,.T.);
#55395=ORIENTED_EDGE('',*,*,#39627,.F.);
#55396=ORIENTED_EDGE('',*,*,#39628,.F.);
#55397=ORIENTED_EDGE('',*,*,#39392,.T.);
#55398=ORIENTED_EDGE('',*,*,#39628,.T.);
#55399=ORIENTED_EDGE('',*,*,#39629,.F.);
#55400=ORIENTED_EDGE('',*,*,#39390,.T.);
#55401=ORIENTED_EDGE('',*,*,#39398,.T.);
#55402=ORIENTED_EDGE('',*,*,#39393,.T.);
#55403=ORIENTED_EDGE('',*,*,#39630,.F.);
#55404=ORIENTED_EDGE('',*,*,#39631,.F.);
#55405=ORIENTED_EDGE('',*,*,#39399,.T.);
#55406=ORIENTED_EDGE('',*,*,#39631,.T.);
#55407=ORIENTED_EDGE('',*,*,#39632,.F.);
#55408=ORIENTED_EDGE('',*,*,#39397,.T.);
#55409=ORIENTED_EDGE('',*,*,#34404,.T.);
#55410=ORIENTED_EDGE('',*,*,#39400,.T.);
#55411=ORIENTED_EDGE('',*,*,#39633,.F.);
#55412=ORIENTED_EDGE('',*,*,#39634,.F.);
#55413=ORIENTED_EDGE('',*,*,#34401,.T.);
#55414=ORIENTED_EDGE('',*,*,#39634,.T.);
#55415=ORIENTED_EDGE('',*,*,#39635,.F.);
#55416=ORIENTED_EDGE('',*,*,#39402,.T.);
#55417=ORIENTED_EDGE('',*,*,#39408,.T.);
#55418=ORIENTED_EDGE('',*,*,#39403,.T.);
#55419=ORIENTED_EDGE('',*,*,#39636,.F.);
#55420=ORIENTED_EDGE('',*,*,#39637,.F.);
#55421=ORIENTED_EDGE('',*,*,#39409,.T.);
#55422=ORIENTED_EDGE('',*,*,#39637,.T.);
#55423=ORIENTED_EDGE('',*,*,#39638,.F.);
#55424=ORIENTED_EDGE('',*,*,#39407,.T.);
#55425=ORIENTED_EDGE('',*,*,#39415,.T.);
#55426=ORIENTED_EDGE('',*,*,#39410,.T.);
#55427=ORIENTED_EDGE('',*,*,#39639,.F.);
#55428=ORIENTED_EDGE('',*,*,#39640,.F.);
#55429=ORIENTED_EDGE('',*,*,#39416,.T.);
#55430=ORIENTED_EDGE('',*,*,#39640,.T.);
#55431=ORIENTED_EDGE('',*,*,#39641,.F.);
#55432=ORIENTED_EDGE('',*,*,#39414,.T.);
#55433=ORIENTED_EDGE('',*,*,#39422,.T.);
#55434=ORIENTED_EDGE('',*,*,#39417,.T.);
#55435=ORIENTED_EDGE('',*,*,#39642,.F.);
#55436=ORIENTED_EDGE('',*,*,#39643,.F.);
#55437=ORIENTED_EDGE('',*,*,#39423,.T.);
#55438=ORIENTED_EDGE('',*,*,#39643,.T.);
#55439=ORIENTED_EDGE('',*,*,#39644,.F.);
#55440=ORIENTED_EDGE('',*,*,#39421,.T.);
#55441=ORIENTED_EDGE('',*,*,#39429,.T.);
#55442=ORIENTED_EDGE('',*,*,#39424,.T.);
#55443=ORIENTED_EDGE('',*,*,#39645,.F.);
#55444=ORIENTED_EDGE('',*,*,#39646,.F.);
#55445=ORIENTED_EDGE('',*,*,#39430,.T.);
#55446=ORIENTED_EDGE('',*,*,#39646,.T.);
#55447=ORIENTED_EDGE('',*,*,#39647,.F.);
#55448=ORIENTED_EDGE('',*,*,#39428,.T.);
#55449=ORIENTED_EDGE('',*,*,#39436,.T.);
#55450=ORIENTED_EDGE('',*,*,#39431,.T.);
#55451=ORIENTED_EDGE('',*,*,#39648,.F.);
#55452=ORIENTED_EDGE('',*,*,#39649,.F.);
#55453=ORIENTED_EDGE('',*,*,#39437,.T.);
#55454=ORIENTED_EDGE('',*,*,#39649,.T.);
#55455=ORIENTED_EDGE('',*,*,#39650,.F.);
#55456=ORIENTED_EDGE('',*,*,#39435,.T.);
#55457=ORIENTED_EDGE('',*,*,#39443,.T.);
#55458=ORIENTED_EDGE('',*,*,#39438,.T.);
#55459=ORIENTED_EDGE('',*,*,#39651,.F.);
#55460=ORIENTED_EDGE('',*,*,#39652,.F.);
#55461=ORIENTED_EDGE('',*,*,#39444,.T.);
#55462=ORIENTED_EDGE('',*,*,#39652,.T.);
#55463=ORIENTED_EDGE('',*,*,#39653,.F.);
#55464=ORIENTED_EDGE('',*,*,#39442,.T.);
#55465=ORIENTED_EDGE('',*,*,#39450,.T.);
#55466=ORIENTED_EDGE('',*,*,#39445,.T.);
#55467=ORIENTED_EDGE('',*,*,#39654,.F.);
#55468=ORIENTED_EDGE('',*,*,#39655,.F.);
#55469=ORIENTED_EDGE('',*,*,#39451,.T.);
#55470=ORIENTED_EDGE('',*,*,#39655,.T.);
#55471=ORIENTED_EDGE('',*,*,#39656,.F.);
#55472=ORIENTED_EDGE('',*,*,#39449,.T.);
#55473=ORIENTED_EDGE('',*,*,#39457,.T.);
#55474=ORIENTED_EDGE('',*,*,#39452,.T.);
#55475=ORIENTED_EDGE('',*,*,#39657,.F.);
#55476=ORIENTED_EDGE('',*,*,#39658,.F.);
#55477=ORIENTED_EDGE('',*,*,#39458,.T.);
#55478=ORIENTED_EDGE('',*,*,#39658,.T.);
#55479=ORIENTED_EDGE('',*,*,#39659,.F.);
#55480=ORIENTED_EDGE('',*,*,#39456,.T.);
#55481=ORIENTED_EDGE('',*,*,#39464,.T.);
#55482=ORIENTED_EDGE('',*,*,#39459,.T.);
#55483=ORIENTED_EDGE('',*,*,#39660,.F.);
#55484=ORIENTED_EDGE('',*,*,#39661,.F.);
#55485=ORIENTED_EDGE('',*,*,#39465,.T.);
#55486=ORIENTED_EDGE('',*,*,#39661,.T.);
#55487=ORIENTED_EDGE('',*,*,#39662,.F.);
#55488=ORIENTED_EDGE('',*,*,#39463,.T.);
#55489=ORIENTED_EDGE('',*,*,#39471,.T.);
#55490=ORIENTED_EDGE('',*,*,#39466,.T.);
#55491=ORIENTED_EDGE('',*,*,#39663,.F.);
#55492=ORIENTED_EDGE('',*,*,#39664,.F.);
#55493=ORIENTED_EDGE('',*,*,#39472,.T.);
#55494=ORIENTED_EDGE('',*,*,#39664,.T.);
#55495=ORIENTED_EDGE('',*,*,#39665,.F.);
#55496=ORIENTED_EDGE('',*,*,#39470,.T.);
#55497=ORIENTED_EDGE('',*,*,#39478,.T.);
#55498=ORIENTED_EDGE('',*,*,#39473,.T.);
#55499=ORIENTED_EDGE('',*,*,#39666,.F.);
#55500=ORIENTED_EDGE('',*,*,#39667,.F.);
#55501=ORIENTED_EDGE('',*,*,#39479,.T.);
#55502=ORIENTED_EDGE('',*,*,#39667,.T.);
#55503=ORIENTED_EDGE('',*,*,#39668,.F.);
#55504=ORIENTED_EDGE('',*,*,#39477,.T.);
#55505=ORIENTED_EDGE('',*,*,#39485,.T.);
#55506=ORIENTED_EDGE('',*,*,#39480,.T.);
#55507=ORIENTED_EDGE('',*,*,#39669,.F.);
#55508=ORIENTED_EDGE('',*,*,#39670,.F.);
#55509=ORIENTED_EDGE('',*,*,#39486,.T.);
#55510=ORIENTED_EDGE('',*,*,#39670,.T.);
#55511=ORIENTED_EDGE('',*,*,#39671,.F.);
#55512=ORIENTED_EDGE('',*,*,#39484,.T.);
#55513=ORIENTED_EDGE('',*,*,#39672,.F.);
#55514=ORIENTED_EDGE('',*,*,#39673,.F.);
#55515=ORIENTED_EDGE('',*,*,#39492,.T.);
#55516=ORIENTED_EDGE('',*,*,#39487,.T.);
#55517=ORIENTED_EDGE('',*,*,#39493,.T.);
#55518=ORIENTED_EDGE('',*,*,#39673,.T.);
#55519=ORIENTED_EDGE('',*,*,#39674,.F.);
#55520=ORIENTED_EDGE('',*,*,#39491,.T.);
#55521=ORIENTED_EDGE('',*,*,#39499,.T.);
#55522=ORIENTED_EDGE('',*,*,#39494,.T.);
#55523=ORIENTED_EDGE('',*,*,#39675,.F.);
#55524=ORIENTED_EDGE('',*,*,#39676,.F.);
#55525=ORIENTED_EDGE('',*,*,#39500,.T.);
#55526=ORIENTED_EDGE('',*,*,#39676,.T.);
#55527=ORIENTED_EDGE('',*,*,#39677,.F.);
#55528=ORIENTED_EDGE('',*,*,#39498,.T.);
#55529=ORIENTED_EDGE('',*,*,#39502,.T.);
#55530=ORIENTED_EDGE('',*,*,#39504,.T.);
#55531=ORIENTED_EDGE('',*,*,#39678,.F.);
#55532=ORIENTED_EDGE('',*,*,#39592,.T.);
#55533=ORIENTED_EDGE('',*,*,#39679,.T.);
#55534=ORIENTED_EDGE('',*,*,#39680,.F.);
#55535=ORIENTED_EDGE('',*,*,#39505,.T.);
#55536=ORIENTED_EDGE('',*,*,#39681,.F.);
#55537=ORIENTED_EDGE('',*,*,#39682,.F.);
#55538=ORIENTED_EDGE('',*,*,#39683,.F.);
#55539=ORIENTED_EDGE('',*,*,#39684,.F.);
#55540=ORIENTED_EDGE('',*,*,#39679,.F.);
#55541=ORIENTED_EDGE('',*,*,#39684,.T.);
#55542=ORIENTED_EDGE('',*,*,#39685,.F.);
#55543=ORIENTED_EDGE('',*,*,#39507,.T.);
#55544=ORIENTED_EDGE('',*,*,#39680,.T.);
#55545=ORIENTED_EDGE('',*,*,#39686,.T.);
#55546=ORIENTED_EDGE('',*,*,#39687,.F.);
#55547=ORIENTED_EDGE('',*,*,#39509,.T.);
#55548=ORIENTED_EDGE('',*,*,#39688,.F.);
#55549=ORIENTED_EDGE('',*,*,#39689,.F.);
#55550=ORIENTED_EDGE('',*,*,#39690,.F.);
#55551=ORIENTED_EDGE('',*,*,#39691,.F.);
#55552=ORIENTED_EDGE('',*,*,#39686,.F.);
#55553=ORIENTED_EDGE('',*,*,#39691,.T.);
#55554=ORIENTED_EDGE('',*,*,#39692,.F.);
#55555=ORIENTED_EDGE('',*,*,#39510,.T.);
#55556=ORIENTED_EDGE('',*,*,#39687,.T.);
#55557=ORIENTED_EDGE('',*,*,#39693,.T.);
#55558=ORIENTED_EDGE('',*,*,#39694,.F.);
#55559=ORIENTED_EDGE('',*,*,#39512,.T.);
#55560=ORIENTED_EDGE('',*,*,#39695,.F.);
#55561=ORIENTED_EDGE('',*,*,#39696,.F.);
#55562=ORIENTED_EDGE('',*,*,#39697,.F.);
#55563=ORIENTED_EDGE('',*,*,#39698,.F.);
#55564=ORIENTED_EDGE('',*,*,#39693,.F.);
#55565=ORIENTED_EDGE('',*,*,#39698,.T.);
#55566=ORIENTED_EDGE('',*,*,#39699,.F.);
#55567=ORIENTED_EDGE('',*,*,#39513,.T.);
#55568=ORIENTED_EDGE('',*,*,#39694,.T.);
#55569=ORIENTED_EDGE('',*,*,#39700,.T.);
#55570=ORIENTED_EDGE('',*,*,#39701,.F.);
#55571=ORIENTED_EDGE('',*,*,#39515,.T.);
#55572=ORIENTED_EDGE('',*,*,#39702,.F.);
#55573=ORIENTED_EDGE('',*,*,#39703,.F.);
#55574=ORIENTED_EDGE('',*,*,#39704,.F.);
#55575=ORIENTED_EDGE('',*,*,#39705,.F.);
#55576=ORIENTED_EDGE('',*,*,#39700,.F.);
#55577=ORIENTED_EDGE('',*,*,#39705,.T.);
#55578=ORIENTED_EDGE('',*,*,#39706,.F.);
#55579=ORIENTED_EDGE('',*,*,#39516,.T.);
#55580=ORIENTED_EDGE('',*,*,#39701,.T.);
#55581=ORIENTED_EDGE('',*,*,#39707,.T.);
#55582=ORIENTED_EDGE('',*,*,#39708,.F.);
#55583=ORIENTED_EDGE('',*,*,#39518,.T.);
#55584=ORIENTED_EDGE('',*,*,#39709,.F.);
#55585=ORIENTED_EDGE('',*,*,#39710,.F.);
#55586=ORIENTED_EDGE('',*,*,#39711,.F.);
#55587=ORIENTED_EDGE('',*,*,#39712,.F.);
#55588=ORIENTED_EDGE('',*,*,#39707,.F.);
#55589=ORIENTED_EDGE('',*,*,#39712,.T.);
#55590=ORIENTED_EDGE('',*,*,#39713,.F.);
#55591=ORIENTED_EDGE('',*,*,#39519,.T.);
#55592=ORIENTED_EDGE('',*,*,#39708,.T.);
#55593=ORIENTED_EDGE('',*,*,#39714,.T.);
#55594=ORIENTED_EDGE('',*,*,#39715,.F.);
#55595=ORIENTED_EDGE('',*,*,#39521,.T.);
#55596=ORIENTED_EDGE('',*,*,#39716,.F.);
#55597=ORIENTED_EDGE('',*,*,#39717,.F.);
#55598=ORIENTED_EDGE('',*,*,#39718,.F.);
#55599=ORIENTED_EDGE('',*,*,#39719,.F.);
#55600=ORIENTED_EDGE('',*,*,#39714,.F.);
#55601=ORIENTED_EDGE('',*,*,#39719,.T.);
#55602=ORIENTED_EDGE('',*,*,#39720,.F.);
#55603=ORIENTED_EDGE('',*,*,#39522,.T.);
#55604=ORIENTED_EDGE('',*,*,#39715,.T.);
#55605=ORIENTED_EDGE('',*,*,#39721,.T.);
#55606=ORIENTED_EDGE('',*,*,#39722,.F.);
#55607=ORIENTED_EDGE('',*,*,#39524,.T.);
#55608=ORIENTED_EDGE('',*,*,#39723,.F.);
#55609=ORIENTED_EDGE('',*,*,#39724,.F.);
#55610=ORIENTED_EDGE('',*,*,#39725,.F.);
#55611=ORIENTED_EDGE('',*,*,#39726,.F.);
#55612=ORIENTED_EDGE('',*,*,#39721,.F.);
#55613=ORIENTED_EDGE('',*,*,#39726,.T.);
#55614=ORIENTED_EDGE('',*,*,#39727,.F.);
#55615=ORIENTED_EDGE('',*,*,#39525,.T.);
#55616=ORIENTED_EDGE('',*,*,#39722,.T.);
#55617=ORIENTED_EDGE('',*,*,#39728,.T.);
#55618=ORIENTED_EDGE('',*,*,#39729,.F.);
#55619=ORIENTED_EDGE('',*,*,#39527,.T.);
#55620=ORIENTED_EDGE('',*,*,#39730,.F.);
#55621=ORIENTED_EDGE('',*,*,#39731,.F.);
#55622=ORIENTED_EDGE('',*,*,#39732,.F.);
#55623=ORIENTED_EDGE('',*,*,#39733,.F.);
#55624=ORIENTED_EDGE('',*,*,#39728,.F.);
#55625=ORIENTED_EDGE('',*,*,#39733,.T.);
#55626=ORIENTED_EDGE('',*,*,#39734,.F.);
#55627=ORIENTED_EDGE('',*,*,#39528,.T.);
#55628=ORIENTED_EDGE('',*,*,#39729,.T.);
#55629=ORIENTED_EDGE('',*,*,#39735,.T.);
#55630=ORIENTED_EDGE('',*,*,#39736,.F.);
#55631=ORIENTED_EDGE('',*,*,#39530,.T.);
#55632=ORIENTED_EDGE('',*,*,#39737,.F.);
#55633=ORIENTED_EDGE('',*,*,#39738,.F.);
#55634=ORIENTED_EDGE('',*,*,#39739,.F.);
#55635=ORIENTED_EDGE('',*,*,#39740,.F.);
#55636=ORIENTED_EDGE('',*,*,#39735,.F.);
#55637=ORIENTED_EDGE('',*,*,#39740,.T.);
#55638=ORIENTED_EDGE('',*,*,#39741,.F.);
#55639=ORIENTED_EDGE('',*,*,#39531,.T.);
#55640=ORIENTED_EDGE('',*,*,#39736,.T.);
#55641=ORIENTED_EDGE('',*,*,#39742,.T.);
#55642=ORIENTED_EDGE('',*,*,#39743,.F.);
#55643=ORIENTED_EDGE('',*,*,#39533,.T.);
#55644=ORIENTED_EDGE('',*,*,#39744,.F.);
#55645=ORIENTED_EDGE('',*,*,#39745,.F.);
#55646=ORIENTED_EDGE('',*,*,#39746,.F.);
#55647=ORIENTED_EDGE('',*,*,#39747,.F.);
#55648=ORIENTED_EDGE('',*,*,#39742,.F.);
#55649=ORIENTED_EDGE('',*,*,#39747,.T.);
#55650=ORIENTED_EDGE('',*,*,#39748,.F.);
#55651=ORIENTED_EDGE('',*,*,#39534,.T.);
#55652=ORIENTED_EDGE('',*,*,#39743,.T.);
#55653=ORIENTED_EDGE('',*,*,#39749,.T.);
#55654=ORIENTED_EDGE('',*,*,#39750,.F.);
#55655=ORIENTED_EDGE('',*,*,#39536,.T.);
#55656=ORIENTED_EDGE('',*,*,#39751,.F.);
#55657=ORIENTED_EDGE('',*,*,#39752,.F.);
#55658=ORIENTED_EDGE('',*,*,#39753,.F.);
#55659=ORIENTED_EDGE('',*,*,#39754,.F.);
#55660=ORIENTED_EDGE('',*,*,#39749,.F.);
#55661=ORIENTED_EDGE('',*,*,#39754,.T.);
#55662=ORIENTED_EDGE('',*,*,#39755,.F.);
#55663=ORIENTED_EDGE('',*,*,#39537,.T.);
#55664=ORIENTED_EDGE('',*,*,#39750,.T.);
#55665=ORIENTED_EDGE('',*,*,#39756,.T.);
#55666=ORIENTED_EDGE('',*,*,#39757,.F.);
#55667=ORIENTED_EDGE('',*,*,#39539,.T.);
#55668=ORIENTED_EDGE('',*,*,#39758,.F.);
#55669=ORIENTED_EDGE('',*,*,#39759,.F.);
#55670=ORIENTED_EDGE('',*,*,#39760,.F.);
#55671=ORIENTED_EDGE('',*,*,#39761,.F.);
#55672=ORIENTED_EDGE('',*,*,#39756,.F.);
#55673=ORIENTED_EDGE('',*,*,#39761,.T.);
#55674=ORIENTED_EDGE('',*,*,#39762,.F.);
#55675=ORIENTED_EDGE('',*,*,#39540,.T.);
#55676=ORIENTED_EDGE('',*,*,#39757,.T.);
#55677=ORIENTED_EDGE('',*,*,#39763,.T.);
#55678=ORIENTED_EDGE('',*,*,#39764,.F.);
#55679=ORIENTED_EDGE('',*,*,#39542,.T.);
#55680=ORIENTED_EDGE('',*,*,#39765,.F.);
#55681=ORIENTED_EDGE('',*,*,#39766,.F.);
#55682=ORIENTED_EDGE('',*,*,#39767,.F.);
#55683=ORIENTED_EDGE('',*,*,#39768,.F.);
#55684=ORIENTED_EDGE('',*,*,#39763,.F.);
#55685=ORIENTED_EDGE('',*,*,#39768,.T.);
#55686=ORIENTED_EDGE('',*,*,#39769,.F.);
#55687=ORIENTED_EDGE('',*,*,#39543,.T.);
#55688=ORIENTED_EDGE('',*,*,#39764,.T.);
#55689=ORIENTED_EDGE('',*,*,#39770,.T.);
#55690=ORIENTED_EDGE('',*,*,#39771,.F.);
#55691=ORIENTED_EDGE('',*,*,#39545,.T.);
#55692=ORIENTED_EDGE('',*,*,#39772,.F.);
#55693=ORIENTED_EDGE('',*,*,#39773,.F.);
#55694=ORIENTED_EDGE('',*,*,#39774,.F.);
#55695=ORIENTED_EDGE('',*,*,#39775,.F.);
#55696=ORIENTED_EDGE('',*,*,#39770,.F.);
#55697=ORIENTED_EDGE('',*,*,#39775,.T.);
#55698=ORIENTED_EDGE('',*,*,#39776,.F.);
#55699=ORIENTED_EDGE('',*,*,#39546,.T.);
#55700=ORIENTED_EDGE('',*,*,#39771,.T.);
#55701=ORIENTED_EDGE('',*,*,#34397,.T.);
#55702=ORIENTED_EDGE('',*,*,#39777,.F.);
#55703=ORIENTED_EDGE('',*,*,#39548,.T.);
#55704=ORIENTED_EDGE('',*,*,#39778,.F.);
#55705=ORIENTED_EDGE('',*,*,#34400,.T.);
#55706=ORIENTED_EDGE('',*,*,#39779,.F.);
#55707=ORIENTED_EDGE('',*,*,#39549,.T.);
#55708=ORIENTED_EDGE('',*,*,#39777,.T.);
#55709=ORIENTED_EDGE('',*,*,#39780,.T.);
#55710=ORIENTED_EDGE('',*,*,#39781,.F.);
#55711=ORIENTED_EDGE('',*,*,#39551,.T.);
#55712=ORIENTED_EDGE('',*,*,#39782,.F.);
#55713=ORIENTED_EDGE('',*,*,#39783,.F.);
#55714=ORIENTED_EDGE('',*,*,#39784,.F.);
#55715=ORIENTED_EDGE('',*,*,#39785,.F.);
#55716=ORIENTED_EDGE('',*,*,#39780,.F.);
#55717=ORIENTED_EDGE('',*,*,#39785,.T.);
#55718=ORIENTED_EDGE('',*,*,#39786,.F.);
#55719=ORIENTED_EDGE('',*,*,#39552,.T.);
#55720=ORIENTED_EDGE('',*,*,#39781,.T.);
#55721=ORIENTED_EDGE('',*,*,#39787,.T.);
#55722=ORIENTED_EDGE('',*,*,#39788,.F.);
#55723=ORIENTED_EDGE('',*,*,#39554,.T.);
#55724=ORIENTED_EDGE('',*,*,#39789,.F.);
#55725=ORIENTED_EDGE('',*,*,#39790,.F.);
#55726=ORIENTED_EDGE('',*,*,#39791,.F.);
#55727=ORIENTED_EDGE('',*,*,#39792,.F.);
#55728=ORIENTED_EDGE('',*,*,#39787,.F.);
#55729=ORIENTED_EDGE('',*,*,#39792,.T.);
#55730=ORIENTED_EDGE('',*,*,#39793,.F.);
#55731=ORIENTED_EDGE('',*,*,#39555,.T.);
#55732=ORIENTED_EDGE('',*,*,#39788,.T.);
#55733=ORIENTED_EDGE('',*,*,#39794,.T.);
#55734=ORIENTED_EDGE('',*,*,#39795,.F.);
#55735=ORIENTED_EDGE('',*,*,#39557,.T.);
#55736=ORIENTED_EDGE('',*,*,#39796,.F.);
#55737=ORIENTED_EDGE('',*,*,#39797,.F.);
#55738=ORIENTED_EDGE('',*,*,#39798,.F.);
#55739=ORIENTED_EDGE('',*,*,#39799,.F.);
#55740=ORIENTED_EDGE('',*,*,#39794,.F.);
#55741=ORIENTED_EDGE('',*,*,#39799,.T.);
#55742=ORIENTED_EDGE('',*,*,#39800,.F.);
#55743=ORIENTED_EDGE('',*,*,#39558,.T.);
#55744=ORIENTED_EDGE('',*,*,#39795,.T.);
#55745=ORIENTED_EDGE('',*,*,#39801,.T.);
#55746=ORIENTED_EDGE('',*,*,#39802,.F.);
#55747=ORIENTED_EDGE('',*,*,#39560,.T.);
#55748=ORIENTED_EDGE('',*,*,#39803,.F.);
#55749=ORIENTED_EDGE('',*,*,#39804,.F.);
#55750=ORIENTED_EDGE('',*,*,#39805,.F.);
#55751=ORIENTED_EDGE('',*,*,#39806,.F.);
#55752=ORIENTED_EDGE('',*,*,#39801,.F.);
#55753=ORIENTED_EDGE('',*,*,#39806,.T.);
#55754=ORIENTED_EDGE('',*,*,#39807,.F.);
#55755=ORIENTED_EDGE('',*,*,#39561,.T.);
#55756=ORIENTED_EDGE('',*,*,#39802,.T.);
#55757=ORIENTED_EDGE('',*,*,#39808,.T.);
#55758=ORIENTED_EDGE('',*,*,#39809,.F.);
#55759=ORIENTED_EDGE('',*,*,#39563,.T.);
#55760=ORIENTED_EDGE('',*,*,#39810,.F.);
#55761=ORIENTED_EDGE('',*,*,#39811,.F.);
#55762=ORIENTED_EDGE('',*,*,#39812,.F.);
#55763=ORIENTED_EDGE('',*,*,#39813,.F.);
#55764=ORIENTED_EDGE('',*,*,#39808,.F.);
#55765=ORIENTED_EDGE('',*,*,#39813,.T.);
#55766=ORIENTED_EDGE('',*,*,#39814,.F.);
#55767=ORIENTED_EDGE('',*,*,#39564,.T.);
#55768=ORIENTED_EDGE('',*,*,#39809,.T.);
#55769=ORIENTED_EDGE('',*,*,#39815,.T.);
#55770=ORIENTED_EDGE('',*,*,#39816,.F.);
#55771=ORIENTED_EDGE('',*,*,#39566,.T.);
#55772=ORIENTED_EDGE('',*,*,#39817,.F.);
#55773=ORIENTED_EDGE('',*,*,#39818,.T.);
#55774=ORIENTED_EDGE('',*,*,#39819,.F.);
#55775=ORIENTED_EDGE('',*,*,#39567,.T.);
#55776=ORIENTED_EDGE('',*,*,#39816,.T.);
#55777=ORIENTED_EDGE('',*,*,#39820,.F.);
#55778=ORIENTED_EDGE('',*,*,#39821,.F.);
#55779=ORIENTED_EDGE('',*,*,#39818,.F.);
#55780=ORIENTED_EDGE('',*,*,#39815,.F.);
#55781=ORIENTED_EDGE('',*,*,#39569,.T.);
#55782=ORIENTED_EDGE('',*,*,#39822,.F.);
#55783=ORIENTED_EDGE('',*,*,#39823,.T.);
#55784=ORIENTED_EDGE('',*,*,#39824,.F.);
#55785=ORIENTED_EDGE('',*,*,#39825,.F.);
#55786=ORIENTED_EDGE('',*,*,#39823,.F.);
#55787=ORIENTED_EDGE('',*,*,#39826,.F.);
#55788=ORIENTED_EDGE('',*,*,#39827,.F.);
#55789=ORIENTED_EDGE('',*,*,#39570,.T.);
#55790=ORIENTED_EDGE('',*,*,#39824,.T.);
#55791=ORIENTED_EDGE('',*,*,#39825,.T.);
#55792=ORIENTED_EDGE('',*,*,#39828,.F.);
#55793=ORIENTED_EDGE('',*,*,#39829,.T.);
#55794=ORIENTED_EDGE('',*,*,#39830,.F.);
#55795=ORIENTED_EDGE('',*,*,#39572,.T.);
#55796=ORIENTED_EDGE('',*,*,#39831,.F.);
#55797=ORIENTED_EDGE('',*,*,#39832,.F.);
#55798=ORIENTED_EDGE('',*,*,#39833,.F.);
#55799=ORIENTED_EDGE('',*,*,#39834,.F.);
#55800=ORIENTED_EDGE('',*,*,#39829,.F.);
#55801=ORIENTED_EDGE('',*,*,#39834,.T.);
#55802=ORIENTED_EDGE('',*,*,#39835,.F.);
#55803=ORIENTED_EDGE('',*,*,#39573,.T.);
#55804=ORIENTED_EDGE('',*,*,#39830,.T.);
#55805=ORIENTED_EDGE('',*,*,#39836,.T.);
#55806=ORIENTED_EDGE('',*,*,#39837,.F.);
#55807=ORIENTED_EDGE('',*,*,#39575,.T.);
#55808=ORIENTED_EDGE('',*,*,#39838,.F.);
#55809=ORIENTED_EDGE('',*,*,#39839,.F.);
#55810=ORIENTED_EDGE('',*,*,#39840,.F.);
#55811=ORIENTED_EDGE('',*,*,#39841,.F.);
#55812=ORIENTED_EDGE('',*,*,#39836,.F.);
#55813=ORIENTED_EDGE('',*,*,#39841,.T.);
#55814=ORIENTED_EDGE('',*,*,#39842,.F.);
#55815=ORIENTED_EDGE('',*,*,#39576,.T.);
#55816=ORIENTED_EDGE('',*,*,#39837,.T.);
#55817=ORIENTED_EDGE('',*,*,#39843,.T.);
#55818=ORIENTED_EDGE('',*,*,#39844,.F.);
#55819=ORIENTED_EDGE('',*,*,#39578,.T.);
#55820=ORIENTED_EDGE('',*,*,#39845,.F.);
#55821=ORIENTED_EDGE('',*,*,#39846,.F.);
#55822=ORIENTED_EDGE('',*,*,#39847,.F.);
#55823=ORIENTED_EDGE('',*,*,#39848,.F.);
#55824=ORIENTED_EDGE('',*,*,#39843,.F.);
#55825=ORIENTED_EDGE('',*,*,#39848,.T.);
#55826=ORIENTED_EDGE('',*,*,#39849,.F.);
#55827=ORIENTED_EDGE('',*,*,#39579,.T.);
#55828=ORIENTED_EDGE('',*,*,#39844,.T.);
#55829=ORIENTED_EDGE('',*,*,#39850,.T.);
#55830=ORIENTED_EDGE('',*,*,#39851,.F.);
#55831=ORIENTED_EDGE('',*,*,#39581,.T.);
#55832=ORIENTED_EDGE('',*,*,#39852,.F.);
#55833=ORIENTED_EDGE('',*,*,#39853,.F.);
#55834=ORIENTED_EDGE('',*,*,#39854,.F.);
#55835=ORIENTED_EDGE('',*,*,#39855,.F.);
#55836=ORIENTED_EDGE('',*,*,#39850,.F.);
#55837=ORIENTED_EDGE('',*,*,#39855,.T.);
#55838=ORIENTED_EDGE('',*,*,#39856,.F.);
#55839=ORIENTED_EDGE('',*,*,#39582,.T.);
#55840=ORIENTED_EDGE('',*,*,#39851,.T.);
#55841=ORIENTED_EDGE('',*,*,#39857,.T.);
#55842=ORIENTED_EDGE('',*,*,#39858,.F.);
#55843=ORIENTED_EDGE('',*,*,#39584,.T.);
#55844=ORIENTED_EDGE('',*,*,#39859,.F.);
#55845=ORIENTED_EDGE('',*,*,#39860,.F.);
#55846=ORIENTED_EDGE('',*,*,#39861,.F.);
#55847=ORIENTED_EDGE('',*,*,#39862,.F.);
#55848=ORIENTED_EDGE('',*,*,#39857,.F.);
#55849=ORIENTED_EDGE('',*,*,#39862,.T.);
#55850=ORIENTED_EDGE('',*,*,#39863,.F.);
#55851=ORIENTED_EDGE('',*,*,#39585,.T.);
#55852=ORIENTED_EDGE('',*,*,#39858,.T.);
#55853=ORIENTED_EDGE('',*,*,#39864,.T.);
#55854=ORIENTED_EDGE('',*,*,#39865,.F.);
#55855=ORIENTED_EDGE('',*,*,#39587,.T.);
#55856=ORIENTED_EDGE('',*,*,#39866,.F.);
#55857=ORIENTED_EDGE('',*,*,#39867,.F.);
#55858=ORIENTED_EDGE('',*,*,#39868,.F.);
#55859=ORIENTED_EDGE('',*,*,#39869,.F.);
#55860=ORIENTED_EDGE('',*,*,#39864,.F.);
#55861=ORIENTED_EDGE('',*,*,#39869,.T.);
#55862=ORIENTED_EDGE('',*,*,#39870,.F.);
#55863=ORIENTED_EDGE('',*,*,#39588,.T.);
#55864=ORIENTED_EDGE('',*,*,#39865,.T.);
#55865=ORIENTED_EDGE('',*,*,#39871,.T.);
#55866=ORIENTED_EDGE('',*,*,#39872,.F.);
#55867=ORIENTED_EDGE('',*,*,#39590,.T.);
#55868=ORIENTED_EDGE('',*,*,#39873,.F.);
#55869=ORIENTED_EDGE('',*,*,#39874,.F.);
#55870=ORIENTED_EDGE('',*,*,#39875,.F.);
#55871=ORIENTED_EDGE('',*,*,#39876,.F.);
#55872=ORIENTED_EDGE('',*,*,#39871,.F.);
#55873=ORIENTED_EDGE('',*,*,#39876,.T.);
#55874=ORIENTED_EDGE('',*,*,#39877,.F.);
#55875=ORIENTED_EDGE('',*,*,#39591,.T.);
#55876=ORIENTED_EDGE('',*,*,#39872,.T.);
#55877=ORIENTED_EDGE('',*,*,#39593,.T.);
#55878=ORIENTED_EDGE('',*,*,#39878,.F.);
#55879=ORIENTED_EDGE('',*,*,#39879,.T.);
#55880=ORIENTED_EDGE('',*,*,#39880,.F.);
#55881=ORIENTED_EDGE('',*,*,#39594,.T.);
#55882=ORIENTED_EDGE('',*,*,#39880,.T.);
#55883=ORIENTED_EDGE('',*,*,#39881,.T.);
#55884=ORIENTED_EDGE('',*,*,#39882,.F.);
#55885=ORIENTED_EDGE('',*,*,#39881,.F.);
#55886=ORIENTED_EDGE('',*,*,#39879,.F.);
#55887=ORIENTED_EDGE('',*,*,#39883,.F.);
#55888=ORIENTED_EDGE('',*,*,#39884,.F.);
#55889=ORIENTED_EDGE('',*,*,#39596,.T.);
#55890=ORIENTED_EDGE('',*,*,#39885,.F.);
#55891=ORIENTED_EDGE('',*,*,#39886,.T.);
#55892=ORIENTED_EDGE('',*,*,#39887,.F.);
#55893=ORIENTED_EDGE('',*,*,#39597,.T.);
#55894=ORIENTED_EDGE('',*,*,#39887,.T.);
#55895=ORIENTED_EDGE('',*,*,#39888,.T.);
#55896=ORIENTED_EDGE('',*,*,#39889,.F.);
#55897=ORIENTED_EDGE('',*,*,#39888,.F.);
#55898=ORIENTED_EDGE('',*,*,#39886,.F.);
#55899=ORIENTED_EDGE('',*,*,#39890,.F.);
#55900=ORIENTED_EDGE('',*,*,#39891,.F.);
#55901=ORIENTED_EDGE('',*,*,#39599,.T.);
#55902=ORIENTED_EDGE('',*,*,#39892,.F.);
#55903=ORIENTED_EDGE('',*,*,#39893,.T.);
#55904=ORIENTED_EDGE('',*,*,#39894,.F.);
#55905=ORIENTED_EDGE('',*,*,#39600,.T.);
#55906=ORIENTED_EDGE('',*,*,#39894,.T.);
#55907=ORIENTED_EDGE('',*,*,#39895,.T.);
#55908=ORIENTED_EDGE('',*,*,#39896,.F.);
#55909=ORIENTED_EDGE('',*,*,#39895,.F.);
#55910=ORIENTED_EDGE('',*,*,#39893,.F.);
#55911=ORIENTED_EDGE('',*,*,#39897,.F.);
#55912=ORIENTED_EDGE('',*,*,#39898,.F.);
#55913=ORIENTED_EDGE('',*,*,#39602,.T.);
#55914=ORIENTED_EDGE('',*,*,#39899,.F.);
#55915=ORIENTED_EDGE('',*,*,#39900,.T.);
#55916=ORIENTED_EDGE('',*,*,#39901,.F.);
#55917=ORIENTED_EDGE('',*,*,#39603,.T.);
#55918=ORIENTED_EDGE('',*,*,#39901,.T.);
#55919=ORIENTED_EDGE('',*,*,#39902,.T.);
#55920=ORIENTED_EDGE('',*,*,#39903,.F.);
#55921=ORIENTED_EDGE('',*,*,#39902,.F.);
#55922=ORIENTED_EDGE('',*,*,#39900,.F.);
#55923=ORIENTED_EDGE('',*,*,#39904,.F.);
#55924=ORIENTED_EDGE('',*,*,#39905,.F.);
#55925=ORIENTED_EDGE('',*,*,#39605,.T.);
#55926=ORIENTED_EDGE('',*,*,#39906,.F.);
#55927=ORIENTED_EDGE('',*,*,#39907,.T.);
#55928=ORIENTED_EDGE('',*,*,#39908,.F.);
#55929=ORIENTED_EDGE('',*,*,#39606,.T.);
#55930=ORIENTED_EDGE('',*,*,#39908,.T.);
#55931=ORIENTED_EDGE('',*,*,#39909,.T.);
#55932=ORIENTED_EDGE('',*,*,#39910,.F.);
#55933=ORIENTED_EDGE('',*,*,#39909,.F.);
#55934=ORIENTED_EDGE('',*,*,#39907,.F.);
#55935=ORIENTED_EDGE('',*,*,#39911,.F.);
#55936=ORIENTED_EDGE('',*,*,#39912,.F.);
#55937=ORIENTED_EDGE('',*,*,#39608,.T.);
#55938=ORIENTED_EDGE('',*,*,#39913,.F.);
#55939=ORIENTED_EDGE('',*,*,#39914,.T.);
#55940=ORIENTED_EDGE('',*,*,#39915,.F.);
#55941=ORIENTED_EDGE('',*,*,#39609,.T.);
#55942=ORIENTED_EDGE('',*,*,#39915,.T.);
#55943=ORIENTED_EDGE('',*,*,#39916,.T.);
#55944=ORIENTED_EDGE('',*,*,#39917,.F.);
#55945=ORIENTED_EDGE('',*,*,#39916,.F.);
#55946=ORIENTED_EDGE('',*,*,#39914,.F.);
#55947=ORIENTED_EDGE('',*,*,#39918,.F.);
#55948=ORIENTED_EDGE('',*,*,#39919,.F.);
#55949=ORIENTED_EDGE('',*,*,#39611,.T.);
#55950=ORIENTED_EDGE('',*,*,#39920,.F.);
#55951=ORIENTED_EDGE('',*,*,#39921,.T.);
#55952=ORIENTED_EDGE('',*,*,#39922,.F.);
#55953=ORIENTED_EDGE('',*,*,#39612,.T.);
#55954=ORIENTED_EDGE('',*,*,#39922,.T.);
#55955=ORIENTED_EDGE('',*,*,#39923,.T.);
#55956=ORIENTED_EDGE('',*,*,#39924,.F.);
#55957=ORIENTED_EDGE('',*,*,#39923,.F.);
#55958=ORIENTED_EDGE('',*,*,#39921,.F.);
#55959=ORIENTED_EDGE('',*,*,#39925,.F.);
#55960=ORIENTED_EDGE('',*,*,#39926,.F.);
#55961=ORIENTED_EDGE('',*,*,#39614,.T.);
#55962=ORIENTED_EDGE('',*,*,#39927,.F.);
#55963=ORIENTED_EDGE('',*,*,#39928,.T.);
#55964=ORIENTED_EDGE('',*,*,#39929,.F.);
#55965=ORIENTED_EDGE('',*,*,#39615,.T.);
#55966=ORIENTED_EDGE('',*,*,#39929,.T.);
#55967=ORIENTED_EDGE('',*,*,#39930,.T.);
#55968=ORIENTED_EDGE('',*,*,#39931,.F.);
#55969=ORIENTED_EDGE('',*,*,#39930,.F.);
#55970=ORIENTED_EDGE('',*,*,#39928,.F.);
#55971=ORIENTED_EDGE('',*,*,#39932,.F.);
#55972=ORIENTED_EDGE('',*,*,#39933,.F.);
#55973=ORIENTED_EDGE('',*,*,#39617,.T.);
#55974=ORIENTED_EDGE('',*,*,#39934,.F.);
#55975=ORIENTED_EDGE('',*,*,#39935,.T.);
#55976=ORIENTED_EDGE('',*,*,#39936,.F.);
#55977=ORIENTED_EDGE('',*,*,#39618,.T.);
#55978=ORIENTED_EDGE('',*,*,#39936,.T.);
#55979=ORIENTED_EDGE('',*,*,#39937,.T.);
#55980=ORIENTED_EDGE('',*,*,#39938,.F.);
#55981=ORIENTED_EDGE('',*,*,#39937,.F.);
#55982=ORIENTED_EDGE('',*,*,#39935,.F.);
#55983=ORIENTED_EDGE('',*,*,#39939,.F.);
#55984=ORIENTED_EDGE('',*,*,#39940,.F.);
#55985=ORIENTED_EDGE('',*,*,#39620,.T.);
#55986=ORIENTED_EDGE('',*,*,#39941,.F.);
#55987=ORIENTED_EDGE('',*,*,#39942,.T.);
#55988=ORIENTED_EDGE('',*,*,#39943,.F.);
#55989=ORIENTED_EDGE('',*,*,#39621,.T.);
#55990=ORIENTED_EDGE('',*,*,#39943,.T.);
#55991=ORIENTED_EDGE('',*,*,#39944,.T.);
#55992=ORIENTED_EDGE('',*,*,#39945,.F.);
#55993=ORIENTED_EDGE('',*,*,#39944,.F.);
#55994=ORIENTED_EDGE('',*,*,#39942,.F.);
#55995=ORIENTED_EDGE('',*,*,#39946,.F.);
#55996=ORIENTED_EDGE('',*,*,#39947,.F.);
#55997=ORIENTED_EDGE('',*,*,#39623,.T.);
#55998=ORIENTED_EDGE('',*,*,#39948,.F.);
#55999=ORIENTED_EDGE('',*,*,#39949,.T.);
#56000=ORIENTED_EDGE('',*,*,#39950,.F.);
#56001=ORIENTED_EDGE('',*,*,#39624,.T.);
#56002=ORIENTED_EDGE('',*,*,#39950,.T.);
#56003=ORIENTED_EDGE('',*,*,#39951,.T.);
#56004=ORIENTED_EDGE('',*,*,#39952,.F.);
#56005=ORIENTED_EDGE('',*,*,#39951,.F.);
#56006=ORIENTED_EDGE('',*,*,#39949,.F.);
#56007=ORIENTED_EDGE('',*,*,#39953,.F.);
#56008=ORIENTED_EDGE('',*,*,#39954,.F.);
#56009=ORIENTED_EDGE('',*,*,#39626,.T.);
#56010=ORIENTED_EDGE('',*,*,#39955,.F.);
#56011=ORIENTED_EDGE('',*,*,#39956,.T.);
#56012=ORIENTED_EDGE('',*,*,#39957,.F.);
#56013=ORIENTED_EDGE('',*,*,#39627,.T.);
#56014=ORIENTED_EDGE('',*,*,#39957,.T.);
#56015=ORIENTED_EDGE('',*,*,#39958,.T.);
#56016=ORIENTED_EDGE('',*,*,#39959,.F.);
#56017=ORIENTED_EDGE('',*,*,#39958,.F.);
#56018=ORIENTED_EDGE('',*,*,#39956,.F.);
#56019=ORIENTED_EDGE('',*,*,#39960,.F.);
#56020=ORIENTED_EDGE('',*,*,#39961,.F.);
#56021=ORIENTED_EDGE('',*,*,#39629,.T.);
#56022=ORIENTED_EDGE('',*,*,#39962,.F.);
#56023=ORIENTED_EDGE('',*,*,#39963,.T.);
#56024=ORIENTED_EDGE('',*,*,#39964,.F.);
#56025=ORIENTED_EDGE('',*,*,#39630,.T.);
#56026=ORIENTED_EDGE('',*,*,#39964,.T.);
#56027=ORIENTED_EDGE('',*,*,#39965,.T.);
#56028=ORIENTED_EDGE('',*,*,#39966,.F.);
#56029=ORIENTED_EDGE('',*,*,#39965,.F.);
#56030=ORIENTED_EDGE('',*,*,#39963,.F.);
#56031=ORIENTED_EDGE('',*,*,#39967,.F.);
#56032=ORIENTED_EDGE('',*,*,#39968,.F.);
#56033=ORIENTED_EDGE('',*,*,#39632,.T.);
#56034=ORIENTED_EDGE('',*,*,#39969,.F.);
#56035=ORIENTED_EDGE('',*,*,#39970,.T.);
#56036=ORIENTED_EDGE('',*,*,#39971,.F.);
#56037=ORIENTED_EDGE('',*,*,#39633,.T.);
#56038=ORIENTED_EDGE('',*,*,#39971,.T.);
#56039=ORIENTED_EDGE('',*,*,#39972,.T.);
#56040=ORIENTED_EDGE('',*,*,#39973,.F.);
#56041=ORIENTED_EDGE('',*,*,#39972,.F.);
#56042=ORIENTED_EDGE('',*,*,#39970,.F.);
#56043=ORIENTED_EDGE('',*,*,#39974,.F.);
#56044=ORIENTED_EDGE('',*,*,#39975,.F.);
#56045=ORIENTED_EDGE('',*,*,#39635,.T.);
#56046=ORIENTED_EDGE('',*,*,#39976,.F.);
#56047=ORIENTED_EDGE('',*,*,#39977,.T.);
#56048=ORIENTED_EDGE('',*,*,#39978,.F.);
#56049=ORIENTED_EDGE('',*,*,#39636,.T.);
#56050=ORIENTED_EDGE('',*,*,#39978,.T.);
#56051=ORIENTED_EDGE('',*,*,#39979,.T.);
#56052=ORIENTED_EDGE('',*,*,#39980,.F.);
#56053=ORIENTED_EDGE('',*,*,#39979,.F.);
#56054=ORIENTED_EDGE('',*,*,#39977,.F.);
#56055=ORIENTED_EDGE('',*,*,#39981,.F.);
#56056=ORIENTED_EDGE('',*,*,#39982,.F.);
#56057=ORIENTED_EDGE('',*,*,#39638,.T.);
#56058=ORIENTED_EDGE('',*,*,#39983,.F.);
#56059=ORIENTED_EDGE('',*,*,#39984,.T.);
#56060=ORIENTED_EDGE('',*,*,#39985,.F.);
#56061=ORIENTED_EDGE('',*,*,#39639,.T.);
#56062=ORIENTED_EDGE('',*,*,#39985,.T.);
#56063=ORIENTED_EDGE('',*,*,#39986,.T.);
#56064=ORIENTED_EDGE('',*,*,#39987,.F.);
#56065=ORIENTED_EDGE('',*,*,#39986,.F.);
#56066=ORIENTED_EDGE('',*,*,#39984,.F.);
#56067=ORIENTED_EDGE('',*,*,#39988,.F.);
#56068=ORIENTED_EDGE('',*,*,#39989,.F.);
#56069=ORIENTED_EDGE('',*,*,#39641,.T.);
#56070=ORIENTED_EDGE('',*,*,#39990,.F.);
#56071=ORIENTED_EDGE('',*,*,#39991,.T.);
#56072=ORIENTED_EDGE('',*,*,#39992,.F.);
#56073=ORIENTED_EDGE('',*,*,#39642,.T.);
#56074=ORIENTED_EDGE('',*,*,#39992,.T.);
#56075=ORIENTED_EDGE('',*,*,#39993,.T.);
#56076=ORIENTED_EDGE('',*,*,#39994,.F.);
#56077=ORIENTED_EDGE('',*,*,#39993,.F.);
#56078=ORIENTED_EDGE('',*,*,#39991,.F.);
#56079=ORIENTED_EDGE('',*,*,#39995,.F.);
#56080=ORIENTED_EDGE('',*,*,#39996,.F.);
#56081=ORIENTED_EDGE('',*,*,#39644,.T.);
#56082=ORIENTED_EDGE('',*,*,#39997,.F.);
#56083=ORIENTED_EDGE('',*,*,#39998,.T.);
#56084=ORIENTED_EDGE('',*,*,#39999,.F.);
#56085=ORIENTED_EDGE('',*,*,#39645,.T.);
#56086=ORIENTED_EDGE('',*,*,#39999,.T.);
#56087=ORIENTED_EDGE('',*,*,#40000,.T.);
#56088=ORIENTED_EDGE('',*,*,#40001,.F.);
#56089=ORIENTED_EDGE('',*,*,#40000,.F.);
#56090=ORIENTED_EDGE('',*,*,#39998,.F.);
#56091=ORIENTED_EDGE('',*,*,#40002,.F.);
#56092=ORIENTED_EDGE('',*,*,#40003,.F.);
#56093=ORIENTED_EDGE('',*,*,#39647,.T.);
#56094=ORIENTED_EDGE('',*,*,#40004,.F.);
#56095=ORIENTED_EDGE('',*,*,#40005,.T.);
#56096=ORIENTED_EDGE('',*,*,#40006,.F.);
#56097=ORIENTED_EDGE('',*,*,#39648,.T.);
#56098=ORIENTED_EDGE('',*,*,#40006,.T.);
#56099=ORIENTED_EDGE('',*,*,#40007,.T.);
#56100=ORIENTED_EDGE('',*,*,#40008,.F.);
#56101=ORIENTED_EDGE('',*,*,#40007,.F.);
#56102=ORIENTED_EDGE('',*,*,#40005,.F.);
#56103=ORIENTED_EDGE('',*,*,#40009,.F.);
#56104=ORIENTED_EDGE('',*,*,#40010,.F.);
#56105=ORIENTED_EDGE('',*,*,#39650,.T.);
#56106=ORIENTED_EDGE('',*,*,#40011,.F.);
#56107=ORIENTED_EDGE('',*,*,#40012,.T.);
#56108=ORIENTED_EDGE('',*,*,#40013,.F.);
#56109=ORIENTED_EDGE('',*,*,#39651,.T.);
#56110=ORIENTED_EDGE('',*,*,#40013,.T.);
#56111=ORIENTED_EDGE('',*,*,#40014,.T.);
#56112=ORIENTED_EDGE('',*,*,#40015,.F.);
#56113=ORIENTED_EDGE('',*,*,#40014,.F.);
#56114=ORIENTED_EDGE('',*,*,#40012,.F.);
#56115=ORIENTED_EDGE('',*,*,#40016,.F.);
#56116=ORIENTED_EDGE('',*,*,#40017,.F.);
#56117=ORIENTED_EDGE('',*,*,#39653,.T.);
#56118=ORIENTED_EDGE('',*,*,#40018,.F.);
#56119=ORIENTED_EDGE('',*,*,#40019,.T.);
#56120=ORIENTED_EDGE('',*,*,#40020,.F.);
#56121=ORIENTED_EDGE('',*,*,#39654,.T.);
#56122=ORIENTED_EDGE('',*,*,#40020,.T.);
#56123=ORIENTED_EDGE('',*,*,#40021,.T.);
#56124=ORIENTED_EDGE('',*,*,#40022,.F.);
#56125=ORIENTED_EDGE('',*,*,#40021,.F.);
#56126=ORIENTED_EDGE('',*,*,#40019,.F.);
#56127=ORIENTED_EDGE('',*,*,#40023,.F.);
#56128=ORIENTED_EDGE('',*,*,#40024,.F.);
#56129=ORIENTED_EDGE('',*,*,#39656,.T.);
#56130=ORIENTED_EDGE('',*,*,#40025,.F.);
#56131=ORIENTED_EDGE('',*,*,#40026,.T.);
#56132=ORIENTED_EDGE('',*,*,#40027,.F.);
#56133=ORIENTED_EDGE('',*,*,#39657,.T.);
#56134=ORIENTED_EDGE('',*,*,#40027,.T.);
#56135=ORIENTED_EDGE('',*,*,#40028,.T.);
#56136=ORIENTED_EDGE('',*,*,#40029,.F.);
#56137=ORIENTED_EDGE('',*,*,#40028,.F.);
#56138=ORIENTED_EDGE('',*,*,#40026,.F.);
#56139=ORIENTED_EDGE('',*,*,#40030,.F.);
#56140=ORIENTED_EDGE('',*,*,#40031,.F.);
#56141=ORIENTED_EDGE('',*,*,#39659,.T.);
#56142=ORIENTED_EDGE('',*,*,#40032,.F.);
#56143=ORIENTED_EDGE('',*,*,#40033,.T.);
#56144=ORIENTED_EDGE('',*,*,#40034,.F.);
#56145=ORIENTED_EDGE('',*,*,#39660,.T.);
#56146=ORIENTED_EDGE('',*,*,#40034,.T.);
#56147=ORIENTED_EDGE('',*,*,#40035,.T.);
#56148=ORIENTED_EDGE('',*,*,#40036,.F.);
#56149=ORIENTED_EDGE('',*,*,#40035,.F.);
#56150=ORIENTED_EDGE('',*,*,#40033,.F.);
#56151=ORIENTED_EDGE('',*,*,#40037,.F.);
#56152=ORIENTED_EDGE('',*,*,#40038,.F.);
#56153=ORIENTED_EDGE('',*,*,#39662,.T.);
#56154=ORIENTED_EDGE('',*,*,#40039,.F.);
#56155=ORIENTED_EDGE('',*,*,#40040,.T.);
#56156=ORIENTED_EDGE('',*,*,#40041,.F.);
#56157=ORIENTED_EDGE('',*,*,#39663,.T.);
#56158=ORIENTED_EDGE('',*,*,#40041,.T.);
#56159=ORIENTED_EDGE('',*,*,#40042,.T.);
#56160=ORIENTED_EDGE('',*,*,#40043,.F.);
#56161=ORIENTED_EDGE('',*,*,#40042,.F.);
#56162=ORIENTED_EDGE('',*,*,#40040,.F.);
#56163=ORIENTED_EDGE('',*,*,#40044,.F.);
#56164=ORIENTED_EDGE('',*,*,#40045,.F.);
#56165=ORIENTED_EDGE('',*,*,#39665,.T.);
#56166=ORIENTED_EDGE('',*,*,#40046,.F.);
#56167=ORIENTED_EDGE('',*,*,#40047,.T.);
#56168=ORIENTED_EDGE('',*,*,#40048,.F.);
#56169=ORIENTED_EDGE('',*,*,#39666,.T.);
#56170=ORIENTED_EDGE('',*,*,#40048,.T.);
#56171=ORIENTED_EDGE('',*,*,#40049,.T.);
#56172=ORIENTED_EDGE('',*,*,#40050,.F.);
#56173=ORIENTED_EDGE('',*,*,#40049,.F.);
#56174=ORIENTED_EDGE('',*,*,#40047,.F.);
#56175=ORIENTED_EDGE('',*,*,#40051,.F.);
#56176=ORIENTED_EDGE('',*,*,#40052,.F.);
#56177=ORIENTED_EDGE('',*,*,#39668,.T.);
#56178=ORIENTED_EDGE('',*,*,#40053,.F.);
#56179=ORIENTED_EDGE('',*,*,#40054,.T.);
#56180=ORIENTED_EDGE('',*,*,#40055,.F.);
#56181=ORIENTED_EDGE('',*,*,#39669,.T.);
#56182=ORIENTED_EDGE('',*,*,#40055,.T.);
#56183=ORIENTED_EDGE('',*,*,#40056,.T.);
#56184=ORIENTED_EDGE('',*,*,#40057,.F.);
#56185=ORIENTED_EDGE('',*,*,#40056,.F.);
#56186=ORIENTED_EDGE('',*,*,#40054,.F.);
#56187=ORIENTED_EDGE('',*,*,#40058,.F.);
#56188=ORIENTED_EDGE('',*,*,#40059,.F.);
#56189=ORIENTED_EDGE('',*,*,#39671,.T.);
#56190=ORIENTED_EDGE('',*,*,#40060,.F.);
#56191=ORIENTED_EDGE('',*,*,#40061,.T.);
#56192=ORIENTED_EDGE('',*,*,#40062,.F.);
#56193=ORIENTED_EDGE('',*,*,#40063,.T.);
#56194=ORIENTED_EDGE('',*,*,#40064,.F.);
#56195=ORIENTED_EDGE('',*,*,#39672,.T.);
#56196=ORIENTED_EDGE('',*,*,#40062,.T.);
#56197=ORIENTED_EDGE('',*,*,#40065,.F.);
#56198=ORIENTED_EDGE('',*,*,#40066,.F.);
#56199=ORIENTED_EDGE('',*,*,#40063,.F.);
#56200=ORIENTED_EDGE('',*,*,#40061,.F.);
#56201=ORIENTED_EDGE('',*,*,#39674,.T.);
#56202=ORIENTED_EDGE('',*,*,#40067,.F.);
#56203=ORIENTED_EDGE('',*,*,#40068,.T.);
#56204=ORIENTED_EDGE('',*,*,#40069,.F.);
#56205=ORIENTED_EDGE('',*,*,#39675,.T.);
#56206=ORIENTED_EDGE('',*,*,#40069,.T.);
#56207=ORIENTED_EDGE('',*,*,#40070,.T.);
#56208=ORIENTED_EDGE('',*,*,#40071,.F.);
#56209=ORIENTED_EDGE('',*,*,#40070,.F.);
#56210=ORIENTED_EDGE('',*,*,#40068,.F.);
#56211=ORIENTED_EDGE('',*,*,#40072,.F.);
#56212=ORIENTED_EDGE('',*,*,#40073,.F.);
#56213=ORIENTED_EDGE('',*,*,#39677,.T.);
#56214=ORIENTED_EDGE('',*,*,#40074,.F.);
#56215=ORIENTED_EDGE('',*,*,#40075,.T.);
#56216=ORIENTED_EDGE('',*,*,#40076,.F.);
#56217=ORIENTED_EDGE('',*,*,#39678,.T.);
#56218=ORIENTED_EDGE('',*,*,#40076,.T.);
#56219=ORIENTED_EDGE('',*,*,#40077,.T.);
#56220=ORIENTED_EDGE('',*,*,#40078,.F.);
#56221=ORIENTED_EDGE('',*,*,#40077,.F.);
#56222=ORIENTED_EDGE('',*,*,#40075,.F.);
#56223=ORIENTED_EDGE('',*,*,#40079,.F.);
#56224=ORIENTED_EDGE('',*,*,#40080,.F.);
#56225=ORIENTED_EDGE('',*,*,#40081,.F.);
#56226=ORIENTED_EDGE('',*,*,#40082,.F.);
#56227=ORIENTED_EDGE('',*,*,#39682,.T.);
#56228=ORIENTED_EDGE('',*,*,#39681,.T.);
#56229=ORIENTED_EDGE('',*,*,#40083,.F.);
#56230=ORIENTED_EDGE('',*,*,#39685,.T.);
#56231=ORIENTED_EDGE('',*,*,#39683,.T.);
#56232=ORIENTED_EDGE('',*,*,#40082,.T.);
#56233=ORIENTED_EDGE('',*,*,#40084,.F.);
#56234=ORIENTED_EDGE('',*,*,#40085,.F.);
#56235=ORIENTED_EDGE('',*,*,#39689,.T.);
#56236=ORIENTED_EDGE('',*,*,#39688,.T.);
#56237=ORIENTED_EDGE('',*,*,#40086,.F.);
#56238=ORIENTED_EDGE('',*,*,#39692,.T.);
#56239=ORIENTED_EDGE('',*,*,#39690,.T.);
#56240=ORIENTED_EDGE('',*,*,#40085,.T.);
#56241=ORIENTED_EDGE('',*,*,#40087,.F.);
#56242=ORIENTED_EDGE('',*,*,#40088,.F.);
#56243=ORIENTED_EDGE('',*,*,#39696,.T.);
#56244=ORIENTED_EDGE('',*,*,#39695,.T.);
#56245=ORIENTED_EDGE('',*,*,#40089,.F.);
#56246=ORIENTED_EDGE('',*,*,#39699,.T.);
#56247=ORIENTED_EDGE('',*,*,#39697,.T.);
#56248=ORIENTED_EDGE('',*,*,#40088,.T.);
#56249=ORIENTED_EDGE('',*,*,#40090,.F.);
#56250=ORIENTED_EDGE('',*,*,#40091,.F.);
#56251=ORIENTED_EDGE('',*,*,#39703,.T.);
#56252=ORIENTED_EDGE('',*,*,#39702,.T.);
#56253=ORIENTED_EDGE('',*,*,#40092,.F.);
#56254=ORIENTED_EDGE('',*,*,#39706,.T.);
#56255=ORIENTED_EDGE('',*,*,#39704,.T.);
#56256=ORIENTED_EDGE('',*,*,#40091,.T.);
#56257=ORIENTED_EDGE('',*,*,#40093,.F.);
#56258=ORIENTED_EDGE('',*,*,#40094,.F.);
#56259=ORIENTED_EDGE('',*,*,#39710,.T.);
#56260=ORIENTED_EDGE('',*,*,#39709,.T.);
#56261=ORIENTED_EDGE('',*,*,#40095,.F.);
#56262=ORIENTED_EDGE('',*,*,#39713,.T.);
#56263=ORIENTED_EDGE('',*,*,#39711,.T.);
#56264=ORIENTED_EDGE('',*,*,#40094,.T.);
#56265=ORIENTED_EDGE('',*,*,#40096,.F.);
#56266=ORIENTED_EDGE('',*,*,#40097,.F.);
#56267=ORIENTED_EDGE('',*,*,#39717,.T.);
#56268=ORIENTED_EDGE('',*,*,#39716,.T.);
#56269=ORIENTED_EDGE('',*,*,#40098,.F.);
#56270=ORIENTED_EDGE('',*,*,#39720,.T.);
#56271=ORIENTED_EDGE('',*,*,#39718,.T.);
#56272=ORIENTED_EDGE('',*,*,#40097,.T.);
#56273=ORIENTED_EDGE('',*,*,#40099,.F.);
#56274=ORIENTED_EDGE('',*,*,#40100,.F.);
#56275=ORIENTED_EDGE('',*,*,#39724,.T.);
#56276=ORIENTED_EDGE('',*,*,#39723,.T.);
#56277=ORIENTED_EDGE('',*,*,#40101,.F.);
#56278=ORIENTED_EDGE('',*,*,#39727,.T.);
#56279=ORIENTED_EDGE('',*,*,#39725,.T.);
#56280=ORIENTED_EDGE('',*,*,#40100,.T.);
#56281=ORIENTED_EDGE('',*,*,#40102,.F.);
#56282=ORIENTED_EDGE('',*,*,#40103,.F.);
#56283=ORIENTED_EDGE('',*,*,#39731,.T.);
#56284=ORIENTED_EDGE('',*,*,#39730,.T.);
#56285=ORIENTED_EDGE('',*,*,#40104,.F.);
#56286=ORIENTED_EDGE('',*,*,#39734,.T.);
#56287=ORIENTED_EDGE('',*,*,#39732,.T.);
#56288=ORIENTED_EDGE('',*,*,#40103,.T.);
#56289=ORIENTED_EDGE('',*,*,#40105,.F.);
#56290=ORIENTED_EDGE('',*,*,#40106,.F.);
#56291=ORIENTED_EDGE('',*,*,#39738,.T.);
#56292=ORIENTED_EDGE('',*,*,#39737,.T.);
#56293=ORIENTED_EDGE('',*,*,#40107,.F.);
#56294=ORIENTED_EDGE('',*,*,#39741,.T.);
#56295=ORIENTED_EDGE('',*,*,#39739,.T.);
#56296=ORIENTED_EDGE('',*,*,#40106,.T.);
#56297=ORIENTED_EDGE('',*,*,#40108,.F.);
#56298=ORIENTED_EDGE('',*,*,#40109,.F.);
#56299=ORIENTED_EDGE('',*,*,#39745,.T.);
#56300=ORIENTED_EDGE('',*,*,#39744,.T.);
#56301=ORIENTED_EDGE('',*,*,#40110,.F.);
#56302=ORIENTED_EDGE('',*,*,#39748,.T.);
#56303=ORIENTED_EDGE('',*,*,#39746,.T.);
#56304=ORIENTED_EDGE('',*,*,#40109,.T.);
#56305=ORIENTED_EDGE('',*,*,#40111,.F.);
#56306=ORIENTED_EDGE('',*,*,#40112,.F.);
#56307=ORIENTED_EDGE('',*,*,#39752,.T.);
#56308=ORIENTED_EDGE('',*,*,#39751,.T.);
#56309=ORIENTED_EDGE('',*,*,#40113,.F.);
#56310=ORIENTED_EDGE('',*,*,#39755,.T.);
#56311=ORIENTED_EDGE('',*,*,#39753,.T.);
#56312=ORIENTED_EDGE('',*,*,#40112,.T.);
#56313=ORIENTED_EDGE('',*,*,#40114,.F.);
#56314=ORIENTED_EDGE('',*,*,#40115,.F.);
#56315=ORIENTED_EDGE('',*,*,#39759,.T.);
#56316=ORIENTED_EDGE('',*,*,#39758,.T.);
#56317=ORIENTED_EDGE('',*,*,#40116,.F.);
#56318=ORIENTED_EDGE('',*,*,#39762,.T.);
#56319=ORIENTED_EDGE('',*,*,#39760,.T.);
#56320=ORIENTED_EDGE('',*,*,#40115,.T.);
#56321=ORIENTED_EDGE('',*,*,#40117,.F.);
#56322=ORIENTED_EDGE('',*,*,#40118,.F.);
#56323=ORIENTED_EDGE('',*,*,#39766,.T.);
#56324=ORIENTED_EDGE('',*,*,#39765,.T.);
#56325=ORIENTED_EDGE('',*,*,#40119,.F.);
#56326=ORIENTED_EDGE('',*,*,#39769,.T.);
#56327=ORIENTED_EDGE('',*,*,#39767,.T.);
#56328=ORIENTED_EDGE('',*,*,#40118,.T.);
#56329=ORIENTED_EDGE('',*,*,#40120,.F.);
#56330=ORIENTED_EDGE('',*,*,#40121,.F.);
#56331=ORIENTED_EDGE('',*,*,#39773,.T.);
#56332=ORIENTED_EDGE('',*,*,#39772,.T.);
#56333=ORIENTED_EDGE('',*,*,#40122,.F.);
#56334=ORIENTED_EDGE('',*,*,#39776,.T.);
#56335=ORIENTED_EDGE('',*,*,#39774,.T.);
#56336=ORIENTED_EDGE('',*,*,#40121,.T.);
#56337=ORIENTED_EDGE('',*,*,#40123,.F.);
#56338=ORIENTED_EDGE('',*,*,#40124,.F.);
#56339=ORIENTED_EDGE('',*,*,#34398,.T.);
#56340=ORIENTED_EDGE('',*,*,#39778,.T.);
#56341=ORIENTED_EDGE('',*,*,#40125,.F.);
#56342=ORIENTED_EDGE('',*,*,#39779,.T.);
#56343=ORIENTED_EDGE('',*,*,#34399,.T.);
#56344=ORIENTED_EDGE('',*,*,#40124,.T.);
#56345=ORIENTED_EDGE('',*,*,#40126,.F.);
#56346=ORIENTED_EDGE('',*,*,#40127,.F.);
#56347=ORIENTED_EDGE('',*,*,#39783,.T.);
#56348=ORIENTED_EDGE('',*,*,#39782,.T.);
#56349=ORIENTED_EDGE('',*,*,#40128,.F.);
#56350=ORIENTED_EDGE('',*,*,#39786,.T.);
#56351=ORIENTED_EDGE('',*,*,#39784,.T.);
#56352=ORIENTED_EDGE('',*,*,#40127,.T.);
#56353=ORIENTED_EDGE('',*,*,#40129,.F.);
#56354=ORIENTED_EDGE('',*,*,#40130,.F.);
#56355=ORIENTED_EDGE('',*,*,#39790,.T.);
#56356=ORIENTED_EDGE('',*,*,#39789,.T.);
#56357=ORIENTED_EDGE('',*,*,#40131,.F.);
#56358=ORIENTED_EDGE('',*,*,#39793,.T.);
#56359=ORIENTED_EDGE('',*,*,#39791,.T.);
#56360=ORIENTED_EDGE('',*,*,#40130,.T.);
#56361=ORIENTED_EDGE('',*,*,#40132,.F.);
#56362=ORIENTED_EDGE('',*,*,#40133,.F.);
#56363=ORIENTED_EDGE('',*,*,#39797,.T.);
#56364=ORIENTED_EDGE('',*,*,#39796,.T.);
#56365=ORIENTED_EDGE('',*,*,#40134,.F.);
#56366=ORIENTED_EDGE('',*,*,#39800,.T.);
#56367=ORIENTED_EDGE('',*,*,#39798,.T.);
#56368=ORIENTED_EDGE('',*,*,#40133,.T.);
#56369=ORIENTED_EDGE('',*,*,#40135,.F.);
#56370=ORIENTED_EDGE('',*,*,#40136,.F.);
#56371=ORIENTED_EDGE('',*,*,#39804,.T.);
#56372=ORIENTED_EDGE('',*,*,#39803,.T.);
#56373=ORIENTED_EDGE('',*,*,#40137,.F.);
#56374=ORIENTED_EDGE('',*,*,#39807,.T.);
#56375=ORIENTED_EDGE('',*,*,#39805,.T.);
#56376=ORIENTED_EDGE('',*,*,#40136,.T.);
#56377=ORIENTED_EDGE('',*,*,#40138,.F.);
#56378=ORIENTED_EDGE('',*,*,#40139,.F.);
#56379=ORIENTED_EDGE('',*,*,#39811,.T.);
#56380=ORIENTED_EDGE('',*,*,#39810,.T.);
#56381=ORIENTED_EDGE('',*,*,#40140,.F.);
#56382=ORIENTED_EDGE('',*,*,#39814,.T.);
#56383=ORIENTED_EDGE('',*,*,#39812,.T.);
#56384=ORIENTED_EDGE('',*,*,#40139,.T.);
#56385=ORIENTED_EDGE('',*,*,#40141,.F.);
#56386=ORIENTED_EDGE('',*,*,#40142,.F.);
#56387=ORIENTED_EDGE('',*,*,#39820,.T.);
#56388=ORIENTED_EDGE('',*,*,#39817,.T.);
#56389=ORIENTED_EDGE('',*,*,#39821,.T.);
#56390=ORIENTED_EDGE('',*,*,#40142,.T.);
#56391=ORIENTED_EDGE('',*,*,#40143,.F.);
#56392=ORIENTED_EDGE('',*,*,#39819,.T.);
#56393=ORIENTED_EDGE('',*,*,#39826,.T.);
#56394=ORIENTED_EDGE('',*,*,#39822,.T.);
#56395=ORIENTED_EDGE('',*,*,#40144,.F.);
#56396=ORIENTED_EDGE('',*,*,#40145,.F.);
#56397=ORIENTED_EDGE('',*,*,#40146,.F.);
#56398=ORIENTED_EDGE('',*,*,#39828,.T.);
#56399=ORIENTED_EDGE('',*,*,#39827,.T.);
#56400=ORIENTED_EDGE('',*,*,#40145,.T.);
#56401=ORIENTED_EDGE('',*,*,#40147,.F.);
#56402=ORIENTED_EDGE('',*,*,#40148,.F.);
#56403=ORIENTED_EDGE('',*,*,#39832,.T.);
#56404=ORIENTED_EDGE('',*,*,#39831,.T.);
#56405=ORIENTED_EDGE('',*,*,#40149,.F.);
#56406=ORIENTED_EDGE('',*,*,#39835,.T.);
#56407=ORIENTED_EDGE('',*,*,#39833,.T.);
#56408=ORIENTED_EDGE('',*,*,#40148,.T.);
#56409=ORIENTED_EDGE('',*,*,#40150,.F.);
#56410=ORIENTED_EDGE('',*,*,#40151,.F.);
#56411=ORIENTED_EDGE('',*,*,#39839,.T.);
#56412=ORIENTED_EDGE('',*,*,#39838,.T.);
#56413=ORIENTED_EDGE('',*,*,#40152,.F.);
#56414=ORIENTED_EDGE('',*,*,#39842,.T.);
#56415=ORIENTED_EDGE('',*,*,#39840,.T.);
#56416=ORIENTED_EDGE('',*,*,#40151,.T.);
#56417=ORIENTED_EDGE('',*,*,#40153,.F.);
#56418=ORIENTED_EDGE('',*,*,#40154,.F.);
#56419=ORIENTED_EDGE('',*,*,#39846,.T.);
#56420=ORIENTED_EDGE('',*,*,#39845,.T.);
#56421=ORIENTED_EDGE('',*,*,#40155,.F.);
#56422=ORIENTED_EDGE('',*,*,#39849,.T.);
#56423=ORIENTED_EDGE('',*,*,#39847,.T.);
#56424=ORIENTED_EDGE('',*,*,#40154,.T.);
#56425=ORIENTED_EDGE('',*,*,#40156,.F.);
#56426=ORIENTED_EDGE('',*,*,#40157,.F.);
#56427=ORIENTED_EDGE('',*,*,#39853,.T.);
#56428=ORIENTED_EDGE('',*,*,#39852,.T.);
#56429=ORIENTED_EDGE('',*,*,#40158,.F.);
#56430=ORIENTED_EDGE('',*,*,#39856,.T.);
#56431=ORIENTED_EDGE('',*,*,#39854,.T.);
#56432=ORIENTED_EDGE('',*,*,#40157,.T.);
#56433=ORIENTED_EDGE('',*,*,#40159,.F.);
#56434=ORIENTED_EDGE('',*,*,#40160,.F.);
#56435=ORIENTED_EDGE('',*,*,#39860,.T.);
#56436=ORIENTED_EDGE('',*,*,#39859,.T.);
#56437=ORIENTED_EDGE('',*,*,#40161,.F.);
#56438=ORIENTED_EDGE('',*,*,#39863,.T.);
#56439=ORIENTED_EDGE('',*,*,#39861,.T.);
#56440=ORIENTED_EDGE('',*,*,#40160,.T.);
#56441=ORIENTED_EDGE('',*,*,#40162,.F.);
#56442=ORIENTED_EDGE('',*,*,#40163,.F.);
#56443=ORIENTED_EDGE('',*,*,#39867,.T.);
#56444=ORIENTED_EDGE('',*,*,#39866,.T.);
#56445=ORIENTED_EDGE('',*,*,#40164,.F.);
#56446=ORIENTED_EDGE('',*,*,#39870,.T.);
#56447=ORIENTED_EDGE('',*,*,#39868,.T.);
#56448=ORIENTED_EDGE('',*,*,#40163,.T.);
#56449=ORIENTED_EDGE('',*,*,#40165,.F.);
#56450=ORIENTED_EDGE('',*,*,#40166,.F.);
#56451=ORIENTED_EDGE('',*,*,#39874,.T.);
#56452=ORIENTED_EDGE('',*,*,#39873,.T.);
#56453=ORIENTED_EDGE('',*,*,#40167,.F.);
#56454=ORIENTED_EDGE('',*,*,#39877,.T.);
#56455=ORIENTED_EDGE('',*,*,#39875,.T.);
#56456=ORIENTED_EDGE('',*,*,#40166,.T.);
#56457=ORIENTED_EDGE('',*,*,#39883,.T.);
#56458=ORIENTED_EDGE('',*,*,#39878,.T.);
#56459=ORIENTED_EDGE('',*,*,#40168,.F.);
#56460=ORIENTED_EDGE('',*,*,#40169,.F.);
#56461=ORIENTED_EDGE('',*,*,#39884,.T.);
#56462=ORIENTED_EDGE('',*,*,#40169,.T.);
#56463=ORIENTED_EDGE('',*,*,#40170,.F.);
#56464=ORIENTED_EDGE('',*,*,#39882,.T.);
#56465=ORIENTED_EDGE('',*,*,#39890,.T.);
#56466=ORIENTED_EDGE('',*,*,#39885,.T.);
#56467=ORIENTED_EDGE('',*,*,#40171,.F.);
#56468=ORIENTED_EDGE('',*,*,#40172,.F.);
#56469=ORIENTED_EDGE('',*,*,#39891,.T.);
#56470=ORIENTED_EDGE('',*,*,#40172,.T.);
#56471=ORIENTED_EDGE('',*,*,#40173,.F.);
#56472=ORIENTED_EDGE('',*,*,#39889,.T.);
#56473=ORIENTED_EDGE('',*,*,#39897,.T.);
#56474=ORIENTED_EDGE('',*,*,#39892,.T.);
#56475=ORIENTED_EDGE('',*,*,#40174,.F.);
#56476=ORIENTED_EDGE('',*,*,#40175,.F.);
#56477=ORIENTED_EDGE('',*,*,#39898,.T.);
#56478=ORIENTED_EDGE('',*,*,#40175,.T.);
#56479=ORIENTED_EDGE('',*,*,#40176,.F.);
#56480=ORIENTED_EDGE('',*,*,#39896,.T.);
#56481=ORIENTED_EDGE('',*,*,#39904,.T.);
#56482=ORIENTED_EDGE('',*,*,#39899,.T.);
#56483=ORIENTED_EDGE('',*,*,#40177,.F.);
#56484=ORIENTED_EDGE('',*,*,#40178,.F.);
#56485=ORIENTED_EDGE('',*,*,#39905,.T.);
#56486=ORIENTED_EDGE('',*,*,#40178,.T.);
#56487=ORIENTED_EDGE('',*,*,#40179,.F.);
#56488=ORIENTED_EDGE('',*,*,#39903,.T.);
#56489=ORIENTED_EDGE('',*,*,#39911,.T.);
#56490=ORIENTED_EDGE('',*,*,#39906,.T.);
#56491=ORIENTED_EDGE('',*,*,#40180,.F.);
#56492=ORIENTED_EDGE('',*,*,#40181,.F.);
#56493=ORIENTED_EDGE('',*,*,#39912,.T.);
#56494=ORIENTED_EDGE('',*,*,#40181,.T.);
#56495=ORIENTED_EDGE('',*,*,#40182,.F.);
#56496=ORIENTED_EDGE('',*,*,#39910,.T.);
#56497=ORIENTED_EDGE('',*,*,#39918,.T.);
#56498=ORIENTED_EDGE('',*,*,#39913,.T.);
#56499=ORIENTED_EDGE('',*,*,#40183,.F.);
#56500=ORIENTED_EDGE('',*,*,#40184,.F.);
#56501=ORIENTED_EDGE('',*,*,#39919,.T.);
#56502=ORIENTED_EDGE('',*,*,#40184,.T.);
#56503=ORIENTED_EDGE('',*,*,#40185,.F.);
#56504=ORIENTED_EDGE('',*,*,#39917,.T.);
#56505=ORIENTED_EDGE('',*,*,#39925,.T.);
#56506=ORIENTED_EDGE('',*,*,#39920,.T.);
#56507=ORIENTED_EDGE('',*,*,#40186,.F.);
#56508=ORIENTED_EDGE('',*,*,#40187,.F.);
#56509=ORIENTED_EDGE('',*,*,#39926,.T.);
#56510=ORIENTED_EDGE('',*,*,#40187,.T.);
#56511=ORIENTED_EDGE('',*,*,#40188,.F.);
#56512=ORIENTED_EDGE('',*,*,#39924,.T.);
#56513=ORIENTED_EDGE('',*,*,#39932,.T.);
#56514=ORIENTED_EDGE('',*,*,#39927,.T.);
#56515=ORIENTED_EDGE('',*,*,#40189,.F.);
#56516=ORIENTED_EDGE('',*,*,#40190,.F.);
#56517=ORIENTED_EDGE('',*,*,#39933,.T.);
#56518=ORIENTED_EDGE('',*,*,#40190,.T.);
#56519=ORIENTED_EDGE('',*,*,#40191,.F.);
#56520=ORIENTED_EDGE('',*,*,#39931,.T.);
#56521=ORIENTED_EDGE('',*,*,#39939,.T.);
#56522=ORIENTED_EDGE('',*,*,#39934,.T.);
#56523=ORIENTED_EDGE('',*,*,#40192,.F.);
#56524=ORIENTED_EDGE('',*,*,#40193,.F.);
#56525=ORIENTED_EDGE('',*,*,#39940,.T.);
#56526=ORIENTED_EDGE('',*,*,#40193,.T.);
#56527=ORIENTED_EDGE('',*,*,#40194,.F.);
#56528=ORIENTED_EDGE('',*,*,#39938,.T.);
#56529=ORIENTED_EDGE('',*,*,#39946,.T.);
#56530=ORIENTED_EDGE('',*,*,#39941,.T.);
#56531=ORIENTED_EDGE('',*,*,#40195,.F.);
#56532=ORIENTED_EDGE('',*,*,#40196,.F.);
#56533=ORIENTED_EDGE('',*,*,#39947,.T.);
#56534=ORIENTED_EDGE('',*,*,#40196,.T.);
#56535=ORIENTED_EDGE('',*,*,#40197,.F.);
#56536=ORIENTED_EDGE('',*,*,#39945,.T.);
#56537=ORIENTED_EDGE('',*,*,#39953,.T.);
#56538=ORIENTED_EDGE('',*,*,#39948,.T.);
#56539=ORIENTED_EDGE('',*,*,#40198,.F.);
#56540=ORIENTED_EDGE('',*,*,#40199,.F.);
#56541=ORIENTED_EDGE('',*,*,#39954,.T.);
#56542=ORIENTED_EDGE('',*,*,#40199,.T.);
#56543=ORIENTED_EDGE('',*,*,#40200,.F.);
#56544=ORIENTED_EDGE('',*,*,#39952,.T.);
#56545=ORIENTED_EDGE('',*,*,#39960,.T.);
#56546=ORIENTED_EDGE('',*,*,#39955,.T.);
#56547=ORIENTED_EDGE('',*,*,#40201,.F.);
#56548=ORIENTED_EDGE('',*,*,#40202,.F.);
#56549=ORIENTED_EDGE('',*,*,#39961,.T.);
#56550=ORIENTED_EDGE('',*,*,#40202,.T.);
#56551=ORIENTED_EDGE('',*,*,#40203,.F.);
#56552=ORIENTED_EDGE('',*,*,#39959,.T.);
#56553=ORIENTED_EDGE('',*,*,#39967,.T.);
#56554=ORIENTED_EDGE('',*,*,#39962,.T.);
#56555=ORIENTED_EDGE('',*,*,#40204,.F.);
#56556=ORIENTED_EDGE('',*,*,#40205,.F.);
#56557=ORIENTED_EDGE('',*,*,#39968,.T.);
#56558=ORIENTED_EDGE('',*,*,#40205,.T.);
#56559=ORIENTED_EDGE('',*,*,#40206,.F.);
#56560=ORIENTED_EDGE('',*,*,#39966,.T.);
#56561=ORIENTED_EDGE('',*,*,#39974,.T.);
#56562=ORIENTED_EDGE('',*,*,#39969,.T.);
#56563=ORIENTED_EDGE('',*,*,#40207,.F.);
#56564=ORIENTED_EDGE('',*,*,#40208,.F.);
#56565=ORIENTED_EDGE('',*,*,#39975,.T.);
#56566=ORIENTED_EDGE('',*,*,#40208,.T.);
#56567=ORIENTED_EDGE('',*,*,#40209,.F.);
#56568=ORIENTED_EDGE('',*,*,#39973,.T.);
#56569=ORIENTED_EDGE('',*,*,#39981,.T.);
#56570=ORIENTED_EDGE('',*,*,#39976,.T.);
#56571=ORIENTED_EDGE('',*,*,#40210,.F.);
#56572=ORIENTED_EDGE('',*,*,#40211,.F.);
#56573=ORIENTED_EDGE('',*,*,#39982,.T.);
#56574=ORIENTED_EDGE('',*,*,#40211,.T.);
#56575=ORIENTED_EDGE('',*,*,#40212,.F.);
#56576=ORIENTED_EDGE('',*,*,#39980,.T.);
#56577=ORIENTED_EDGE('',*,*,#39988,.T.);
#56578=ORIENTED_EDGE('',*,*,#39983,.T.);
#56579=ORIENTED_EDGE('',*,*,#40213,.F.);
#56580=ORIENTED_EDGE('',*,*,#40214,.F.);
#56581=ORIENTED_EDGE('',*,*,#39989,.T.);
#56582=ORIENTED_EDGE('',*,*,#40214,.T.);
#56583=ORIENTED_EDGE('',*,*,#40215,.F.);
#56584=ORIENTED_EDGE('',*,*,#39987,.T.);
#56585=ORIENTED_EDGE('',*,*,#39995,.T.);
#56586=ORIENTED_EDGE('',*,*,#39990,.T.);
#56587=ORIENTED_EDGE('',*,*,#40216,.F.);
#56588=ORIENTED_EDGE('',*,*,#40217,.F.);
#56589=ORIENTED_EDGE('',*,*,#39996,.T.);
#56590=ORIENTED_EDGE('',*,*,#40217,.T.);
#56591=ORIENTED_EDGE('',*,*,#40218,.F.);
#56592=ORIENTED_EDGE('',*,*,#39994,.T.);
#56593=ORIENTED_EDGE('',*,*,#40002,.T.);
#56594=ORIENTED_EDGE('',*,*,#39997,.T.);
#56595=ORIENTED_EDGE('',*,*,#40219,.F.);
#56596=ORIENTED_EDGE('',*,*,#40220,.F.);
#56597=ORIENTED_EDGE('',*,*,#40003,.T.);
#56598=ORIENTED_EDGE('',*,*,#40220,.T.);
#56599=ORIENTED_EDGE('',*,*,#40221,.F.);
#56600=ORIENTED_EDGE('',*,*,#40001,.T.);
#56601=ORIENTED_EDGE('',*,*,#40009,.T.);
#56602=ORIENTED_EDGE('',*,*,#40004,.T.);
#56603=ORIENTED_EDGE('',*,*,#40222,.F.);
#56604=ORIENTED_EDGE('',*,*,#40223,.F.);
#56605=ORIENTED_EDGE('',*,*,#40010,.T.);
#56606=ORIENTED_EDGE('',*,*,#40223,.T.);
#56607=ORIENTED_EDGE('',*,*,#40224,.F.);
#56608=ORIENTED_EDGE('',*,*,#40008,.T.);
#56609=ORIENTED_EDGE('',*,*,#40016,.T.);
#56610=ORIENTED_EDGE('',*,*,#40011,.T.);
#56611=ORIENTED_EDGE('',*,*,#40225,.F.);
#56612=ORIENTED_EDGE('',*,*,#40226,.F.);
#56613=ORIENTED_EDGE('',*,*,#40017,.T.);
#56614=ORIENTED_EDGE('',*,*,#40226,.T.);
#56615=ORIENTED_EDGE('',*,*,#40227,.F.);
#56616=ORIENTED_EDGE('',*,*,#40015,.T.);
#56617=ORIENTED_EDGE('',*,*,#40023,.T.);
#56618=ORIENTED_EDGE('',*,*,#40018,.T.);
#56619=ORIENTED_EDGE('',*,*,#40228,.F.);
#56620=ORIENTED_EDGE('',*,*,#40229,.F.);
#56621=ORIENTED_EDGE('',*,*,#40024,.T.);
#56622=ORIENTED_EDGE('',*,*,#40229,.T.);
#56623=ORIENTED_EDGE('',*,*,#40230,.F.);
#56624=ORIENTED_EDGE('',*,*,#40022,.T.);
#56625=ORIENTED_EDGE('',*,*,#40030,.T.);
#56626=ORIENTED_EDGE('',*,*,#40025,.T.);
#56627=ORIENTED_EDGE('',*,*,#40231,.F.);
#56628=ORIENTED_EDGE('',*,*,#40232,.F.);
#56629=ORIENTED_EDGE('',*,*,#40031,.T.);
#56630=ORIENTED_EDGE('',*,*,#40232,.T.);
#56631=ORIENTED_EDGE('',*,*,#40233,.F.);
#56632=ORIENTED_EDGE('',*,*,#40029,.T.);
#56633=ORIENTED_EDGE('',*,*,#40037,.T.);
#56634=ORIENTED_EDGE('',*,*,#40032,.T.);
#56635=ORIENTED_EDGE('',*,*,#40234,.F.);
#56636=ORIENTED_EDGE('',*,*,#40235,.F.);
#56637=ORIENTED_EDGE('',*,*,#40038,.T.);
#56638=ORIENTED_EDGE('',*,*,#40235,.T.);
#56639=ORIENTED_EDGE('',*,*,#40236,.F.);
#56640=ORIENTED_EDGE('',*,*,#40036,.T.);
#56641=ORIENTED_EDGE('',*,*,#40044,.T.);
#56642=ORIENTED_EDGE('',*,*,#40039,.T.);
#56643=ORIENTED_EDGE('',*,*,#40237,.F.);
#56644=ORIENTED_EDGE('',*,*,#40238,.F.);
#56645=ORIENTED_EDGE('',*,*,#40045,.T.);
#56646=ORIENTED_EDGE('',*,*,#40238,.T.);
#56647=ORIENTED_EDGE('',*,*,#40239,.F.);
#56648=ORIENTED_EDGE('',*,*,#40043,.T.);
#56649=ORIENTED_EDGE('',*,*,#40051,.T.);
#56650=ORIENTED_EDGE('',*,*,#40046,.T.);
#56651=ORIENTED_EDGE('',*,*,#40240,.F.);
#56652=ORIENTED_EDGE('',*,*,#40241,.F.);
#56653=ORIENTED_EDGE('',*,*,#40052,.T.);
#56654=ORIENTED_EDGE('',*,*,#40241,.T.);
#56655=ORIENTED_EDGE('',*,*,#40242,.F.);
#56656=ORIENTED_EDGE('',*,*,#40050,.T.);
#56657=ORIENTED_EDGE('',*,*,#40058,.T.);
#56658=ORIENTED_EDGE('',*,*,#40053,.T.);
#56659=ORIENTED_EDGE('',*,*,#40243,.F.);
#56660=ORIENTED_EDGE('',*,*,#40244,.F.);
#56661=ORIENTED_EDGE('',*,*,#40059,.T.);
#56662=ORIENTED_EDGE('',*,*,#40244,.T.);
#56663=ORIENTED_EDGE('',*,*,#40245,.F.);
#56664=ORIENTED_EDGE('',*,*,#40057,.T.);
#56665=ORIENTED_EDGE('',*,*,#40246,.F.);
#56666=ORIENTED_EDGE('',*,*,#40247,.F.);
#56667=ORIENTED_EDGE('',*,*,#40065,.T.);
#56668=ORIENTED_EDGE('',*,*,#40060,.T.);
#56669=ORIENTED_EDGE('',*,*,#40066,.T.);
#56670=ORIENTED_EDGE('',*,*,#40247,.T.);
#56671=ORIENTED_EDGE('',*,*,#40248,.F.);
#56672=ORIENTED_EDGE('',*,*,#40064,.T.);
#56673=ORIENTED_EDGE('',*,*,#40072,.T.);
#56674=ORIENTED_EDGE('',*,*,#40067,.T.);
#56675=ORIENTED_EDGE('',*,*,#40249,.F.);
#56676=ORIENTED_EDGE('',*,*,#40250,.F.);
#56677=ORIENTED_EDGE('',*,*,#40073,.T.);
#56678=ORIENTED_EDGE('',*,*,#40250,.T.);
#56679=ORIENTED_EDGE('',*,*,#40251,.F.);
#56680=ORIENTED_EDGE('',*,*,#40071,.T.);
#56681=ORIENTED_EDGE('',*,*,#40079,.T.);
#56682=ORIENTED_EDGE('',*,*,#40074,.T.);
#56683=ORIENTED_EDGE('',*,*,#40252,.F.);
#56684=ORIENTED_EDGE('',*,*,#40253,.F.);
#56685=ORIENTED_EDGE('',*,*,#40080,.T.);
#56686=ORIENTED_EDGE('',*,*,#40253,.T.);
#56687=ORIENTED_EDGE('',*,*,#40254,.F.);
#56688=ORIENTED_EDGE('',*,*,#40078,.T.);
#56689=ORIENTED_EDGE('',*,*,#40255,.T.);
#56690=ORIENTED_EDGE('',*,*,#40256,.F.);
#56691=ORIENTED_EDGE('',*,*,#40081,.T.);
#56692=ORIENTED_EDGE('',*,*,#40257,.F.);
#56693=ORIENTED_EDGE('',*,*,#40258,.T.);
#56694=ORIENTED_EDGE('',*,*,#40259,.F.);
#56695=ORIENTED_EDGE('',*,*,#40083,.T.);
#56696=ORIENTED_EDGE('',*,*,#40260,.F.);
#56697=ORIENTED_EDGE('',*,*,#40261,.F.);
#56698=ORIENTED_EDGE('',*,*,#40262,.F.);
#56699=ORIENTED_EDGE('',*,*,#40263,.F.);
#56700=ORIENTED_EDGE('',*,*,#40258,.F.);
#56701=ORIENTED_EDGE('',*,*,#40263,.T.);
#56702=ORIENTED_EDGE('',*,*,#40264,.F.);
#56703=ORIENTED_EDGE('',*,*,#40084,.T.);
#56704=ORIENTED_EDGE('',*,*,#40259,.T.);
#56705=ORIENTED_EDGE('',*,*,#40265,.T.);
#56706=ORIENTED_EDGE('',*,*,#40266,.F.);
#56707=ORIENTED_EDGE('',*,*,#40086,.T.);
#56708=ORIENTED_EDGE('',*,*,#40267,.F.);
#56709=ORIENTED_EDGE('',*,*,#40268,.F.);
#56710=ORIENTED_EDGE('',*,*,#40269,.F.);
#56711=ORIENTED_EDGE('',*,*,#40270,.F.);
#56712=ORIENTED_EDGE('',*,*,#40265,.F.);
#56713=ORIENTED_EDGE('',*,*,#40270,.T.);
#56714=ORIENTED_EDGE('',*,*,#40271,.F.);
#56715=ORIENTED_EDGE('',*,*,#40087,.T.);
#56716=ORIENTED_EDGE('',*,*,#40266,.T.);
#56717=ORIENTED_EDGE('',*,*,#40272,.T.);
#56718=ORIENTED_EDGE('',*,*,#40273,.F.);
#56719=ORIENTED_EDGE('',*,*,#40089,.T.);
#56720=ORIENTED_EDGE('',*,*,#40274,.F.);
#56721=ORIENTED_EDGE('',*,*,#40275,.F.);
#56722=ORIENTED_EDGE('',*,*,#40276,.F.);
#56723=ORIENTED_EDGE('',*,*,#40277,.F.);
#56724=ORIENTED_EDGE('',*,*,#40272,.F.);
#56725=ORIENTED_EDGE('',*,*,#40277,.T.);
#56726=ORIENTED_EDGE('',*,*,#40278,.F.);
#56727=ORIENTED_EDGE('',*,*,#40090,.T.);
#56728=ORIENTED_EDGE('',*,*,#40273,.T.);
#56729=ORIENTED_EDGE('',*,*,#40279,.T.);
#56730=ORIENTED_EDGE('',*,*,#40280,.F.);
#56731=ORIENTED_EDGE('',*,*,#40092,.T.);
#56732=ORIENTED_EDGE('',*,*,#40281,.F.);
#56733=ORIENTED_EDGE('',*,*,#40282,.F.);
#56734=ORIENTED_EDGE('',*,*,#40283,.F.);
#56735=ORIENTED_EDGE('',*,*,#40284,.F.);
#56736=ORIENTED_EDGE('',*,*,#40279,.F.);
#56737=ORIENTED_EDGE('',*,*,#40284,.T.);
#56738=ORIENTED_EDGE('',*,*,#40285,.F.);
#56739=ORIENTED_EDGE('',*,*,#40093,.T.);
#56740=ORIENTED_EDGE('',*,*,#40280,.T.);
#56741=ORIENTED_EDGE('',*,*,#40286,.T.);
#56742=ORIENTED_EDGE('',*,*,#40287,.F.);
#56743=ORIENTED_EDGE('',*,*,#40095,.T.);
#56744=ORIENTED_EDGE('',*,*,#40288,.F.);
#56745=ORIENTED_EDGE('',*,*,#40289,.F.);
#56746=ORIENTED_EDGE('',*,*,#40290,.F.);
#56747=ORIENTED_EDGE('',*,*,#40291,.F.);
#56748=ORIENTED_EDGE('',*,*,#40286,.F.);
#56749=ORIENTED_EDGE('',*,*,#40291,.T.);
#56750=ORIENTED_EDGE('',*,*,#40292,.F.);
#56751=ORIENTED_EDGE('',*,*,#40096,.T.);
#56752=ORIENTED_EDGE('',*,*,#40287,.T.);
#56753=ORIENTED_EDGE('',*,*,#40293,.T.);
#56754=ORIENTED_EDGE('',*,*,#40294,.F.);
#56755=ORIENTED_EDGE('',*,*,#40098,.T.);
#56756=ORIENTED_EDGE('',*,*,#40295,.F.);
#56757=ORIENTED_EDGE('',*,*,#40296,.F.);
#56758=ORIENTED_EDGE('',*,*,#40297,.F.);
#56759=ORIENTED_EDGE('',*,*,#40298,.F.);
#56760=ORIENTED_EDGE('',*,*,#40293,.F.);
#56761=ORIENTED_EDGE('',*,*,#40298,.T.);
#56762=ORIENTED_EDGE('',*,*,#40299,.F.);
#56763=ORIENTED_EDGE('',*,*,#40099,.T.);
#56764=ORIENTED_EDGE('',*,*,#40294,.T.);
#56765=ORIENTED_EDGE('',*,*,#34394,.T.);
#56766=ORIENTED_EDGE('',*,*,#40300,.F.);
#56767=ORIENTED_EDGE('',*,*,#40101,.T.);
#56768=ORIENTED_EDGE('',*,*,#40301,.F.);
#56769=ORIENTED_EDGE('',*,*,#34393,.T.);
#56770=ORIENTED_EDGE('',*,*,#40302,.F.);
#56771=ORIENTED_EDGE('',*,*,#40102,.T.);
#56772=ORIENTED_EDGE('',*,*,#40300,.T.);
#56773=ORIENTED_EDGE('',*,*,#40303,.T.);
#56774=ORIENTED_EDGE('',*,*,#40304,.F.);
#56775=ORIENTED_EDGE('',*,*,#40104,.T.);
#56776=ORIENTED_EDGE('',*,*,#40305,.F.);
#56777=ORIENTED_EDGE('',*,*,#40306,.F.);
#56778=ORIENTED_EDGE('',*,*,#40307,.F.);
#56779=ORIENTED_EDGE('',*,*,#40308,.F.);
#56780=ORIENTED_EDGE('',*,*,#40303,.F.);
#56781=ORIENTED_EDGE('',*,*,#40308,.T.);
#56782=ORIENTED_EDGE('',*,*,#40309,.F.);
#56783=ORIENTED_EDGE('',*,*,#40105,.T.);
#56784=ORIENTED_EDGE('',*,*,#40304,.T.);
#56785=ORIENTED_EDGE('',*,*,#40310,.T.);
#56786=ORIENTED_EDGE('',*,*,#40311,.F.);
#56787=ORIENTED_EDGE('',*,*,#40107,.T.);
#56788=ORIENTED_EDGE('',*,*,#40312,.F.);
#56789=ORIENTED_EDGE('',*,*,#40313,.F.);
#56790=ORIENTED_EDGE('',*,*,#40314,.F.);
#56791=ORIENTED_EDGE('',*,*,#40315,.F.);
#56792=ORIENTED_EDGE('',*,*,#40310,.F.);
#56793=ORIENTED_EDGE('',*,*,#40315,.T.);
#56794=ORIENTED_EDGE('',*,*,#40316,.F.);
#56795=ORIENTED_EDGE('',*,*,#40108,.T.);
#56796=ORIENTED_EDGE('',*,*,#40311,.T.);
#56797=ORIENTED_EDGE('',*,*,#40317,.T.);
#56798=ORIENTED_EDGE('',*,*,#40318,.F.);
#56799=ORIENTED_EDGE('',*,*,#40110,.T.);
#56800=ORIENTED_EDGE('',*,*,#40319,.F.);
#56801=ORIENTED_EDGE('',*,*,#40320,.F.);
#56802=ORIENTED_EDGE('',*,*,#40321,.F.);
#56803=ORIENTED_EDGE('',*,*,#40322,.F.);
#56804=ORIENTED_EDGE('',*,*,#40317,.F.);
#56805=ORIENTED_EDGE('',*,*,#40322,.T.);
#56806=ORIENTED_EDGE('',*,*,#40323,.F.);
#56807=ORIENTED_EDGE('',*,*,#40111,.T.);
#56808=ORIENTED_EDGE('',*,*,#40318,.T.);
#56809=ORIENTED_EDGE('',*,*,#40324,.T.);
#56810=ORIENTED_EDGE('',*,*,#40325,.F.);
#56811=ORIENTED_EDGE('',*,*,#40113,.T.);
#56812=ORIENTED_EDGE('',*,*,#40326,.F.);
#56813=ORIENTED_EDGE('',*,*,#40327,.F.);
#56814=ORIENTED_EDGE('',*,*,#40328,.F.);
#56815=ORIENTED_EDGE('',*,*,#40329,.F.);
#56816=ORIENTED_EDGE('',*,*,#40324,.F.);
#56817=ORIENTED_EDGE('',*,*,#40329,.T.);
#56818=ORIENTED_EDGE('',*,*,#40330,.F.);
#56819=ORIENTED_EDGE('',*,*,#40114,.T.);
#56820=ORIENTED_EDGE('',*,*,#40325,.T.);
#56821=ORIENTED_EDGE('',*,*,#40331,.T.);
#56822=ORIENTED_EDGE('',*,*,#40332,.F.);
#56823=ORIENTED_EDGE('',*,*,#40116,.T.);
#56824=ORIENTED_EDGE('',*,*,#40333,.F.);
#56825=ORIENTED_EDGE('',*,*,#40334,.F.);
#56826=ORIENTED_EDGE('',*,*,#40335,.F.);
#56827=ORIENTED_EDGE('',*,*,#40336,.F.);
#56828=ORIENTED_EDGE('',*,*,#40331,.F.);
#56829=ORIENTED_EDGE('',*,*,#40336,.T.);
#56830=ORIENTED_EDGE('',*,*,#40337,.F.);
#56831=ORIENTED_EDGE('',*,*,#40117,.T.);
#56832=ORIENTED_EDGE('',*,*,#40332,.T.);
#56833=ORIENTED_EDGE('',*,*,#40338,.T.);
#56834=ORIENTED_EDGE('',*,*,#40339,.F.);
#56835=ORIENTED_EDGE('',*,*,#40119,.T.);
#56836=ORIENTED_EDGE('',*,*,#40340,.F.);
#56837=ORIENTED_EDGE('',*,*,#40341,.F.);
#56838=ORIENTED_EDGE('',*,*,#40342,.F.);
#56839=ORIENTED_EDGE('',*,*,#40343,.F.);
#56840=ORIENTED_EDGE('',*,*,#40338,.F.);
#56841=ORIENTED_EDGE('',*,*,#40343,.T.);
#56842=ORIENTED_EDGE('',*,*,#40344,.F.);
#56843=ORIENTED_EDGE('',*,*,#40120,.T.);
#56844=ORIENTED_EDGE('',*,*,#40339,.T.);
#56845=ORIENTED_EDGE('',*,*,#40345,.T.);
#56846=ORIENTED_EDGE('',*,*,#40346,.F.);
#56847=ORIENTED_EDGE('',*,*,#40122,.T.);
#56848=ORIENTED_EDGE('',*,*,#40347,.F.);
#56849=ORIENTED_EDGE('',*,*,#40348,.F.);
#56850=ORIENTED_EDGE('',*,*,#40349,.F.);
#56851=ORIENTED_EDGE('',*,*,#40350,.F.);
#56852=ORIENTED_EDGE('',*,*,#40345,.F.);
#56853=ORIENTED_EDGE('',*,*,#40350,.T.);
#56854=ORIENTED_EDGE('',*,*,#40351,.F.);
#56855=ORIENTED_EDGE('',*,*,#40123,.T.);
#56856=ORIENTED_EDGE('',*,*,#40346,.T.);
#56857=ORIENTED_EDGE('',*,*,#40352,.T.);
#56858=ORIENTED_EDGE('',*,*,#40353,.F.);
#56859=ORIENTED_EDGE('',*,*,#40125,.T.);
#56860=ORIENTED_EDGE('',*,*,#40354,.F.);
#56861=ORIENTED_EDGE('',*,*,#40355,.F.);
#56862=ORIENTED_EDGE('',*,*,#40356,.F.);
#56863=ORIENTED_EDGE('',*,*,#40357,.F.);
#56864=ORIENTED_EDGE('',*,*,#40352,.F.);
#56865=ORIENTED_EDGE('',*,*,#40357,.T.);
#56866=ORIENTED_EDGE('',*,*,#40358,.F.);
#56867=ORIENTED_EDGE('',*,*,#40126,.T.);
#56868=ORIENTED_EDGE('',*,*,#40353,.T.);
#56869=ORIENTED_EDGE('',*,*,#40359,.T.);
#56870=ORIENTED_EDGE('',*,*,#40360,.F.);
#56871=ORIENTED_EDGE('',*,*,#40128,.T.);
#56872=ORIENTED_EDGE('',*,*,#40361,.F.);
#56873=ORIENTED_EDGE('',*,*,#40362,.F.);
#56874=ORIENTED_EDGE('',*,*,#40363,.F.);
#56875=ORIENTED_EDGE('',*,*,#40364,.F.);
#56876=ORIENTED_EDGE('',*,*,#40359,.F.);
#56877=ORIENTED_EDGE('',*,*,#40364,.T.);
#56878=ORIENTED_EDGE('',*,*,#40365,.F.);
#56879=ORIENTED_EDGE('',*,*,#40129,.T.);
#56880=ORIENTED_EDGE('',*,*,#40360,.T.);
#56881=ORIENTED_EDGE('',*,*,#40366,.T.);
#56882=ORIENTED_EDGE('',*,*,#40367,.F.);
#56883=ORIENTED_EDGE('',*,*,#40131,.T.);
#56884=ORIENTED_EDGE('',*,*,#40368,.F.);
#56885=ORIENTED_EDGE('',*,*,#40369,.F.);
#56886=ORIENTED_EDGE('',*,*,#40370,.F.);
#56887=ORIENTED_EDGE('',*,*,#40371,.F.);
#56888=ORIENTED_EDGE('',*,*,#40366,.F.);
#56889=ORIENTED_EDGE('',*,*,#40371,.T.);
#56890=ORIENTED_EDGE('',*,*,#40372,.F.);
#56891=ORIENTED_EDGE('',*,*,#40132,.T.);
#56892=ORIENTED_EDGE('',*,*,#40367,.T.);
#56893=ORIENTED_EDGE('',*,*,#40373,.T.);
#56894=ORIENTED_EDGE('',*,*,#40374,.F.);
#56895=ORIENTED_EDGE('',*,*,#40134,.T.);
#56896=ORIENTED_EDGE('',*,*,#40375,.F.);
#56897=ORIENTED_EDGE('',*,*,#40376,.F.);
#56898=ORIENTED_EDGE('',*,*,#40377,.F.);
#56899=ORIENTED_EDGE('',*,*,#40378,.F.);
#56900=ORIENTED_EDGE('',*,*,#40373,.F.);
#56901=ORIENTED_EDGE('',*,*,#40378,.T.);
#56902=ORIENTED_EDGE('',*,*,#40379,.F.);
#56903=ORIENTED_EDGE('',*,*,#40135,.T.);
#56904=ORIENTED_EDGE('',*,*,#40374,.T.);
#56905=ORIENTED_EDGE('',*,*,#40380,.T.);
#56906=ORIENTED_EDGE('',*,*,#40381,.F.);
#56907=ORIENTED_EDGE('',*,*,#40137,.T.);
#56908=ORIENTED_EDGE('',*,*,#40382,.F.);
#56909=ORIENTED_EDGE('',*,*,#40383,.F.);
#56910=ORIENTED_EDGE('',*,*,#40384,.F.);
#56911=ORIENTED_EDGE('',*,*,#40385,.F.);
#56912=ORIENTED_EDGE('',*,*,#40380,.F.);
#56913=ORIENTED_EDGE('',*,*,#40385,.T.);
#56914=ORIENTED_EDGE('',*,*,#40386,.F.);
#56915=ORIENTED_EDGE('',*,*,#40138,.T.);
#56916=ORIENTED_EDGE('',*,*,#40381,.T.);
#56917=ORIENTED_EDGE('',*,*,#40387,.T.);
#56918=ORIENTED_EDGE('',*,*,#40388,.F.);
#56919=ORIENTED_EDGE('',*,*,#40140,.T.);
#56920=ORIENTED_EDGE('',*,*,#40389,.F.);
#56921=ORIENTED_EDGE('',*,*,#40390,.T.);
#56922=ORIENTED_EDGE('',*,*,#40391,.F.);
#56923=ORIENTED_EDGE('',*,*,#40141,.T.);
#56924=ORIENTED_EDGE('',*,*,#40388,.T.);
#56925=ORIENTED_EDGE('',*,*,#40392,.F.);
#56926=ORIENTED_EDGE('',*,*,#40393,.F.);
#56927=ORIENTED_EDGE('',*,*,#40390,.F.);
#56928=ORIENTED_EDGE('',*,*,#40387,.F.);
#56929=ORIENTED_EDGE('',*,*,#40143,.T.);
#56930=ORIENTED_EDGE('',*,*,#40394,.F.);
#56931=ORIENTED_EDGE('',*,*,#40395,.T.);
#56932=ORIENTED_EDGE('',*,*,#40396,.F.);
#56933=ORIENTED_EDGE('',*,*,#40397,.F.);
#56934=ORIENTED_EDGE('',*,*,#40395,.F.);
#56935=ORIENTED_EDGE('',*,*,#40398,.F.);
#56936=ORIENTED_EDGE('',*,*,#40399,.F.);
#56937=ORIENTED_EDGE('',*,*,#40144,.T.);
#56938=ORIENTED_EDGE('',*,*,#40396,.T.);
#56939=ORIENTED_EDGE('',*,*,#40397,.T.);
#56940=ORIENTED_EDGE('',*,*,#40400,.F.);
#56941=ORIENTED_EDGE('',*,*,#40401,.T.);
#56942=ORIENTED_EDGE('',*,*,#40402,.F.);
#56943=ORIENTED_EDGE('',*,*,#40146,.T.);
#56944=ORIENTED_EDGE('',*,*,#40403,.F.);
#56945=ORIENTED_EDGE('',*,*,#40404,.F.);
#56946=ORIENTED_EDGE('',*,*,#40405,.F.);
#56947=ORIENTED_EDGE('',*,*,#40406,.F.);
#56948=ORIENTED_EDGE('',*,*,#40401,.F.);
#56949=ORIENTED_EDGE('',*,*,#40406,.T.);
#56950=ORIENTED_EDGE('',*,*,#40407,.F.);
#56951=ORIENTED_EDGE('',*,*,#40147,.T.);
#56952=ORIENTED_EDGE('',*,*,#40402,.T.);
#56953=ORIENTED_EDGE('',*,*,#40408,.T.);
#56954=ORIENTED_EDGE('',*,*,#40409,.F.);
#56955=ORIENTED_EDGE('',*,*,#40149,.T.);
#56956=ORIENTED_EDGE('',*,*,#40410,.F.);
#56957=ORIENTED_EDGE('',*,*,#40411,.F.);
#56958=ORIENTED_EDGE('',*,*,#40412,.F.);
#56959=ORIENTED_EDGE('',*,*,#40413,.F.);
#56960=ORIENTED_EDGE('',*,*,#40408,.F.);
#56961=ORIENTED_EDGE('',*,*,#40413,.T.);
#56962=ORIENTED_EDGE('',*,*,#40414,.F.);
#56963=ORIENTED_EDGE('',*,*,#40150,.T.);
#56964=ORIENTED_EDGE('',*,*,#40409,.T.);
#56965=ORIENTED_EDGE('',*,*,#40415,.T.);
#56966=ORIENTED_EDGE('',*,*,#40416,.F.);
#56967=ORIENTED_EDGE('',*,*,#40152,.T.);
#56968=ORIENTED_EDGE('',*,*,#40417,.F.);
#56969=ORIENTED_EDGE('',*,*,#40418,.F.);
#56970=ORIENTED_EDGE('',*,*,#40419,.F.);
#56971=ORIENTED_EDGE('',*,*,#40420,.F.);
#56972=ORIENTED_EDGE('',*,*,#40415,.F.);
#56973=ORIENTED_EDGE('',*,*,#40420,.T.);
#56974=ORIENTED_EDGE('',*,*,#40421,.F.);
#56975=ORIENTED_EDGE('',*,*,#40153,.T.);
#56976=ORIENTED_EDGE('',*,*,#40416,.T.);
#56977=ORIENTED_EDGE('',*,*,#40422,.T.);
#56978=ORIENTED_EDGE('',*,*,#40423,.F.);
#56979=ORIENTED_EDGE('',*,*,#40155,.T.);
#56980=ORIENTED_EDGE('',*,*,#40424,.F.);
#56981=ORIENTED_EDGE('',*,*,#40425,.F.);
#56982=ORIENTED_EDGE('',*,*,#40426,.F.);
#56983=ORIENTED_EDGE('',*,*,#40427,.F.);
#56984=ORIENTED_EDGE('',*,*,#40422,.F.);
#56985=ORIENTED_EDGE('',*,*,#40427,.T.);
#56986=ORIENTED_EDGE('',*,*,#40428,.F.);
#56987=ORIENTED_EDGE('',*,*,#40156,.T.);
#56988=ORIENTED_EDGE('',*,*,#40423,.T.);
#56989=ORIENTED_EDGE('',*,*,#40429,.T.);
#56990=ORIENTED_EDGE('',*,*,#40430,.F.);
#56991=ORIENTED_EDGE('',*,*,#40158,.T.);
#56992=ORIENTED_EDGE('',*,*,#40431,.F.);
#56993=ORIENTED_EDGE('',*,*,#40432,.F.);
#56994=ORIENTED_EDGE('',*,*,#40433,.F.);
#56995=ORIENTED_EDGE('',*,*,#40434,.F.);
#56996=ORIENTED_EDGE('',*,*,#40429,.F.);
#56997=ORIENTED_EDGE('',*,*,#40434,.T.);
#56998=ORIENTED_EDGE('',*,*,#40435,.F.);
#56999=ORIENTED_EDGE('',*,*,#40159,.T.);
#57000=ORIENTED_EDGE('',*,*,#40430,.T.);
#57001=ORIENTED_EDGE('',*,*,#40436,.T.);
#57002=ORIENTED_EDGE('',*,*,#40437,.F.);
#57003=ORIENTED_EDGE('',*,*,#40161,.T.);
#57004=ORIENTED_EDGE('',*,*,#40438,.F.);
#57005=ORIENTED_EDGE('',*,*,#40439,.F.);
#57006=ORIENTED_EDGE('',*,*,#40440,.F.);
#57007=ORIENTED_EDGE('',*,*,#40441,.F.);
#57008=ORIENTED_EDGE('',*,*,#40436,.F.);
#57009=ORIENTED_EDGE('',*,*,#40441,.T.);
#57010=ORIENTED_EDGE('',*,*,#40442,.F.);
#57011=ORIENTED_EDGE('',*,*,#40162,.T.);
#57012=ORIENTED_EDGE('',*,*,#40437,.T.);
#57013=ORIENTED_EDGE('',*,*,#40443,.T.);
#57014=ORIENTED_EDGE('',*,*,#40444,.F.);
#57015=ORIENTED_EDGE('',*,*,#40164,.T.);
#57016=ORIENTED_EDGE('',*,*,#40445,.F.);
#57017=ORIENTED_EDGE('',*,*,#40446,.F.);
#57018=ORIENTED_EDGE('',*,*,#40447,.F.);
#57019=ORIENTED_EDGE('',*,*,#40448,.F.);
#57020=ORIENTED_EDGE('',*,*,#40443,.F.);
#57021=ORIENTED_EDGE('',*,*,#40448,.T.);
#57022=ORIENTED_EDGE('',*,*,#40449,.F.);
#57023=ORIENTED_EDGE('',*,*,#40165,.T.);
#57024=ORIENTED_EDGE('',*,*,#40444,.T.);
#57025=ORIENTED_EDGE('',*,*,#40450,.F.);
#57026=ORIENTED_EDGE('',*,*,#40451,.F.);
#57027=ORIENTED_EDGE('',*,*,#40255,.F.);
#57028=ORIENTED_EDGE('',*,*,#40452,.F.);
#57029=ORIENTED_EDGE('',*,*,#40452,.T.);
#57030=ORIENTED_EDGE('',*,*,#40257,.T.);
#57031=ORIENTED_EDGE('',*,*,#40167,.T.);
#57032=ORIENTED_EDGE('',*,*,#40453,.F.);
#57033=ORIENTED_EDGE('',*,*,#40168,.T.);
#57034=ORIENTED_EDGE('',*,*,#40454,.F.);
#57035=ORIENTED_EDGE('',*,*,#40455,.T.);
#57036=ORIENTED_EDGE('',*,*,#40456,.F.);
#57037=ORIENTED_EDGE('',*,*,#40170,.T.);
#57038=ORIENTED_EDGE('',*,*,#40457,.F.);
#57039=ORIENTED_EDGE('',*,*,#40458,.T.);
#57040=ORIENTED_EDGE('',*,*,#40459,.F.);
#57041=ORIENTED_EDGE('',*,*,#40171,.T.);
#57042=ORIENTED_EDGE('',*,*,#40459,.T.);
#57043=ORIENTED_EDGE('',*,*,#40460,.T.);
#57044=ORIENTED_EDGE('',*,*,#40461,.F.);
#57045=ORIENTED_EDGE('',*,*,#40460,.F.);
#57046=ORIENTED_EDGE('',*,*,#40458,.F.);
#57047=ORIENTED_EDGE('',*,*,#40462,.F.);
#57048=ORIENTED_EDGE('',*,*,#40463,.F.);
#57049=ORIENTED_EDGE('',*,*,#40173,.T.);
#57050=ORIENTED_EDGE('',*,*,#40464,.F.);
#57051=ORIENTED_EDGE('',*,*,#40465,.T.);
#57052=ORIENTED_EDGE('',*,*,#40466,.F.);
#57053=ORIENTED_EDGE('',*,*,#40174,.T.);
#57054=ORIENTED_EDGE('',*,*,#40466,.T.);
#57055=ORIENTED_EDGE('',*,*,#40467,.T.);
#57056=ORIENTED_EDGE('',*,*,#40468,.F.);
#57057=ORIENTED_EDGE('',*,*,#40467,.F.);
#57058=ORIENTED_EDGE('',*,*,#40465,.F.);
#57059=ORIENTED_EDGE('',*,*,#40469,.F.);
#57060=ORIENTED_EDGE('',*,*,#40470,.F.);
#57061=ORIENTED_EDGE('',*,*,#40176,.T.);
#57062=ORIENTED_EDGE('',*,*,#40471,.F.);
#57063=ORIENTED_EDGE('',*,*,#40472,.T.);
#57064=ORIENTED_EDGE('',*,*,#40473,.F.);
#57065=ORIENTED_EDGE('',*,*,#40177,.T.);
#57066=ORIENTED_EDGE('',*,*,#40473,.T.);
#57067=ORIENTED_EDGE('',*,*,#40474,.T.);
#57068=ORIENTED_EDGE('',*,*,#40475,.F.);
#57069=ORIENTED_EDGE('',*,*,#40474,.F.);
#57070=ORIENTED_EDGE('',*,*,#40472,.F.);
#57071=ORIENTED_EDGE('',*,*,#40476,.F.);
#57072=ORIENTED_EDGE('',*,*,#40477,.F.);
#57073=ORIENTED_EDGE('',*,*,#40179,.T.);
#57074=ORIENTED_EDGE('',*,*,#40478,.F.);
#57075=ORIENTED_EDGE('',*,*,#40479,.T.);
#57076=ORIENTED_EDGE('',*,*,#40480,.F.);
#57077=ORIENTED_EDGE('',*,*,#40180,.T.);
#57078=ORIENTED_EDGE('',*,*,#40480,.T.);
#57079=ORIENTED_EDGE('',*,*,#40481,.T.);
#57080=ORIENTED_EDGE('',*,*,#40482,.F.);
#57081=ORIENTED_EDGE('',*,*,#40481,.F.);
#57082=ORIENTED_EDGE('',*,*,#40479,.F.);
#57083=ORIENTED_EDGE('',*,*,#40483,.F.);
#57084=ORIENTED_EDGE('',*,*,#40484,.F.);
#57085=ORIENTED_EDGE('',*,*,#40182,.T.);
#57086=ORIENTED_EDGE('',*,*,#40485,.F.);
#57087=ORIENTED_EDGE('',*,*,#40486,.T.);
#57088=ORIENTED_EDGE('',*,*,#40487,.F.);
#57089=ORIENTED_EDGE('',*,*,#40183,.T.);
#57090=ORIENTED_EDGE('',*,*,#40487,.T.);
#57091=ORIENTED_EDGE('',*,*,#40488,.T.);
#57092=ORIENTED_EDGE('',*,*,#40489,.F.);
#57093=ORIENTED_EDGE('',*,*,#40488,.F.);
#57094=ORIENTED_EDGE('',*,*,#40486,.F.);
#57095=ORIENTED_EDGE('',*,*,#40490,.F.);
#57096=ORIENTED_EDGE('',*,*,#40491,.F.);
#57097=ORIENTED_EDGE('',*,*,#40185,.T.);
#57098=ORIENTED_EDGE('',*,*,#40492,.F.);
#57099=ORIENTED_EDGE('',*,*,#40493,.T.);
#57100=ORIENTED_EDGE('',*,*,#40494,.F.);
#57101=ORIENTED_EDGE('',*,*,#40186,.T.);
#57102=ORIENTED_EDGE('',*,*,#40494,.T.);
#57103=ORIENTED_EDGE('',*,*,#40495,.T.);
#57104=ORIENTED_EDGE('',*,*,#40496,.F.);
#57105=ORIENTED_EDGE('',*,*,#40495,.F.);
#57106=ORIENTED_EDGE('',*,*,#40493,.F.);
#57107=ORIENTED_EDGE('',*,*,#40497,.F.);
#57108=ORIENTED_EDGE('',*,*,#40498,.F.);
#57109=ORIENTED_EDGE('',*,*,#40188,.T.);
#57110=ORIENTED_EDGE('',*,*,#40499,.F.);
#57111=ORIENTED_EDGE('',*,*,#40500,.T.);
#57112=ORIENTED_EDGE('',*,*,#40501,.F.);
#57113=ORIENTED_EDGE('',*,*,#40189,.T.);
#57114=ORIENTED_EDGE('',*,*,#40501,.T.);
#57115=ORIENTED_EDGE('',*,*,#40502,.T.);
#57116=ORIENTED_EDGE('',*,*,#40503,.F.);
#57117=ORIENTED_EDGE('',*,*,#40502,.F.);
#57118=ORIENTED_EDGE('',*,*,#40500,.F.);
#57119=ORIENTED_EDGE('',*,*,#40504,.F.);
#57120=ORIENTED_EDGE('',*,*,#40505,.F.);
#57121=ORIENTED_EDGE('',*,*,#40191,.T.);
#57122=ORIENTED_EDGE('',*,*,#40506,.F.);
#57123=ORIENTED_EDGE('',*,*,#40507,.T.);
#57124=ORIENTED_EDGE('',*,*,#40508,.F.);
#57125=ORIENTED_EDGE('',*,*,#40192,.T.);
#57126=ORIENTED_EDGE('',*,*,#40508,.T.);
#57127=ORIENTED_EDGE('',*,*,#40509,.T.);
#57128=ORIENTED_EDGE('',*,*,#40510,.F.);
#57129=ORIENTED_EDGE('',*,*,#40509,.F.);
#57130=ORIENTED_EDGE('',*,*,#40507,.F.);
#57131=ORIENTED_EDGE('',*,*,#40511,.F.);
#57132=ORIENTED_EDGE('',*,*,#40512,.F.);
#57133=ORIENTED_EDGE('',*,*,#40194,.T.);
#57134=ORIENTED_EDGE('',*,*,#40513,.F.);
#57135=ORIENTED_EDGE('',*,*,#40514,.T.);
#57136=ORIENTED_EDGE('',*,*,#40515,.F.);
#57137=ORIENTED_EDGE('',*,*,#40195,.T.);
#57138=ORIENTED_EDGE('',*,*,#40515,.T.);
#57139=ORIENTED_EDGE('',*,*,#40516,.T.);
#57140=ORIENTED_EDGE('',*,*,#40517,.F.);
#57141=ORIENTED_EDGE('',*,*,#40516,.F.);
#57142=ORIENTED_EDGE('',*,*,#40514,.F.);
#57143=ORIENTED_EDGE('',*,*,#40518,.F.);
#57144=ORIENTED_EDGE('',*,*,#40519,.F.);
#57145=ORIENTED_EDGE('',*,*,#40197,.T.);
#57146=ORIENTED_EDGE('',*,*,#40520,.F.);
#57147=ORIENTED_EDGE('',*,*,#40521,.T.);
#57148=ORIENTED_EDGE('',*,*,#40522,.F.);
#57149=ORIENTED_EDGE('',*,*,#40198,.T.);
#57150=ORIENTED_EDGE('',*,*,#40522,.T.);
#57151=ORIENTED_EDGE('',*,*,#40523,.T.);
#57152=ORIENTED_EDGE('',*,*,#40524,.F.);
#57153=ORIENTED_EDGE('',*,*,#40523,.F.);
#57154=ORIENTED_EDGE('',*,*,#40521,.F.);
#57155=ORIENTED_EDGE('',*,*,#40525,.F.);
#57156=ORIENTED_EDGE('',*,*,#40526,.F.);
#57157=ORIENTED_EDGE('',*,*,#40200,.T.);
#57158=ORIENTED_EDGE('',*,*,#40527,.F.);
#57159=ORIENTED_EDGE('',*,*,#40528,.T.);
#57160=ORIENTED_EDGE('',*,*,#40529,.F.);
#57161=ORIENTED_EDGE('',*,*,#40201,.T.);
#57162=ORIENTED_EDGE('',*,*,#40529,.T.);
#57163=ORIENTED_EDGE('',*,*,#40530,.T.);
#57164=ORIENTED_EDGE('',*,*,#40531,.F.);
#57165=ORIENTED_EDGE('',*,*,#40530,.F.);
#57166=ORIENTED_EDGE('',*,*,#40528,.F.);
#57167=ORIENTED_EDGE('',*,*,#40532,.F.);
#57168=ORIENTED_EDGE('',*,*,#40533,.F.);
#57169=ORIENTED_EDGE('',*,*,#40203,.T.);
#57170=ORIENTED_EDGE('',*,*,#40534,.F.);
#57171=ORIENTED_EDGE('',*,*,#40535,.T.);
#57172=ORIENTED_EDGE('',*,*,#40536,.F.);
#57173=ORIENTED_EDGE('',*,*,#40204,.T.);
#57174=ORIENTED_EDGE('',*,*,#40536,.T.);
#57175=ORIENTED_EDGE('',*,*,#40537,.T.);
#57176=ORIENTED_EDGE('',*,*,#40538,.F.);
#57177=ORIENTED_EDGE('',*,*,#40537,.F.);
#57178=ORIENTED_EDGE('',*,*,#40535,.F.);
#57179=ORIENTED_EDGE('',*,*,#40539,.F.);
#57180=ORIENTED_EDGE('',*,*,#40540,.F.);
#57181=ORIENTED_EDGE('',*,*,#40206,.T.);
#57182=ORIENTED_EDGE('',*,*,#40541,.F.);
#57183=ORIENTED_EDGE('',*,*,#40542,.T.);
#57184=ORIENTED_EDGE('',*,*,#40543,.F.);
#57185=ORIENTED_EDGE('',*,*,#40207,.T.);
#57186=ORIENTED_EDGE('',*,*,#40543,.T.);
#57187=ORIENTED_EDGE('',*,*,#40544,.T.);
#57188=ORIENTED_EDGE('',*,*,#40545,.F.);
#57189=ORIENTED_EDGE('',*,*,#40544,.F.);
#57190=ORIENTED_EDGE('',*,*,#40542,.F.);
#57191=ORIENTED_EDGE('',*,*,#40546,.F.);
#57192=ORIENTED_EDGE('',*,*,#40547,.F.);
#57193=ORIENTED_EDGE('',*,*,#40209,.T.);
#57194=ORIENTED_EDGE('',*,*,#40548,.F.);
#57195=ORIENTED_EDGE('',*,*,#34391,.T.);
#57196=ORIENTED_EDGE('',*,*,#40549,.F.);
#57197=ORIENTED_EDGE('',*,*,#40210,.T.);
#57198=ORIENTED_EDGE('',*,*,#40549,.T.);
#57199=ORIENTED_EDGE('',*,*,#34390,.T.);
#57200=ORIENTED_EDGE('',*,*,#40550,.F.);
#57201=ORIENTED_EDGE('',*,*,#40212,.T.);
#57202=ORIENTED_EDGE('',*,*,#40551,.F.);
#57203=ORIENTED_EDGE('',*,*,#40552,.T.);
#57204=ORIENTED_EDGE('',*,*,#40553,.F.);
#57205=ORIENTED_EDGE('',*,*,#40213,.T.);
#57206=ORIENTED_EDGE('',*,*,#40553,.T.);
#57207=ORIENTED_EDGE('',*,*,#40554,.T.);
#57208=ORIENTED_EDGE('',*,*,#40555,.F.);
#57209=ORIENTED_EDGE('',*,*,#40554,.F.);
#57210=ORIENTED_EDGE('',*,*,#40552,.F.);
#57211=ORIENTED_EDGE('',*,*,#40556,.F.);
#57212=ORIENTED_EDGE('',*,*,#40557,.F.);
#57213=ORIENTED_EDGE('',*,*,#40215,.T.);
#57214=ORIENTED_EDGE('',*,*,#40558,.F.);
#57215=ORIENTED_EDGE('',*,*,#40559,.T.);
#57216=ORIENTED_EDGE('',*,*,#40560,.F.);
#57217=ORIENTED_EDGE('',*,*,#40216,.T.);
#57218=ORIENTED_EDGE('',*,*,#40560,.T.);
#57219=ORIENTED_EDGE('',*,*,#40561,.T.);
#57220=ORIENTED_EDGE('',*,*,#40562,.F.);
#57221=ORIENTED_EDGE('',*,*,#40561,.F.);
#57222=ORIENTED_EDGE('',*,*,#40559,.F.);
#57223=ORIENTED_EDGE('',*,*,#40563,.F.);
#57224=ORIENTED_EDGE('',*,*,#40564,.F.);
#57225=ORIENTED_EDGE('',*,*,#40218,.T.);
#57226=ORIENTED_EDGE('',*,*,#40565,.F.);
#57227=ORIENTED_EDGE('',*,*,#40566,.T.);
#57228=ORIENTED_EDGE('',*,*,#40567,.F.);
#57229=ORIENTED_EDGE('',*,*,#40219,.T.);
#57230=ORIENTED_EDGE('',*,*,#40567,.T.);
#57231=ORIENTED_EDGE('',*,*,#40568,.T.);
#57232=ORIENTED_EDGE('',*,*,#40569,.F.);
#57233=ORIENTED_EDGE('',*,*,#40568,.F.);
#57234=ORIENTED_EDGE('',*,*,#40566,.F.);
#57235=ORIENTED_EDGE('',*,*,#40570,.F.);
#57236=ORIENTED_EDGE('',*,*,#40571,.F.);
#57237=ORIENTED_EDGE('',*,*,#40221,.T.);
#57238=ORIENTED_EDGE('',*,*,#40572,.F.);
#57239=ORIENTED_EDGE('',*,*,#40573,.T.);
#57240=ORIENTED_EDGE('',*,*,#40574,.F.);
#57241=ORIENTED_EDGE('',*,*,#40222,.T.);
#57242=ORIENTED_EDGE('',*,*,#40574,.T.);
#57243=ORIENTED_EDGE('',*,*,#40575,.T.);
#57244=ORIENTED_EDGE('',*,*,#40576,.F.);
#57245=ORIENTED_EDGE('',*,*,#40575,.F.);
#57246=ORIENTED_EDGE('',*,*,#40573,.F.);
#57247=ORIENTED_EDGE('',*,*,#40577,.F.);
#57248=ORIENTED_EDGE('',*,*,#40578,.F.);
#57249=ORIENTED_EDGE('',*,*,#40224,.T.);
#57250=ORIENTED_EDGE('',*,*,#40579,.F.);
#57251=ORIENTED_EDGE('',*,*,#40580,.T.);
#57252=ORIENTED_EDGE('',*,*,#40581,.F.);
#57253=ORIENTED_EDGE('',*,*,#40225,.T.);
#57254=ORIENTED_EDGE('',*,*,#40581,.T.);
#57255=ORIENTED_EDGE('',*,*,#40582,.T.);
#57256=ORIENTED_EDGE('',*,*,#40583,.F.);
#57257=ORIENTED_EDGE('',*,*,#40582,.F.);
#57258=ORIENTED_EDGE('',*,*,#40580,.F.);
#57259=ORIENTED_EDGE('',*,*,#40584,.F.);
#57260=ORIENTED_EDGE('',*,*,#40585,.F.);
#57261=ORIENTED_EDGE('',*,*,#40227,.T.);
#57262=ORIENTED_EDGE('',*,*,#40586,.F.);
#57263=ORIENTED_EDGE('',*,*,#40587,.T.);
#57264=ORIENTED_EDGE('',*,*,#40588,.F.);
#57265=ORIENTED_EDGE('',*,*,#40228,.T.);
#57266=ORIENTED_EDGE('',*,*,#40588,.T.);
#57267=ORIENTED_EDGE('',*,*,#40589,.T.);
#57268=ORIENTED_EDGE('',*,*,#40590,.F.);
#57269=ORIENTED_EDGE('',*,*,#40589,.F.);
#57270=ORIENTED_EDGE('',*,*,#40587,.F.);
#57271=ORIENTED_EDGE('',*,*,#40591,.F.);
#57272=ORIENTED_EDGE('',*,*,#40592,.F.);
#57273=ORIENTED_EDGE('',*,*,#40230,.T.);
#57274=ORIENTED_EDGE('',*,*,#40593,.F.);
#57275=ORIENTED_EDGE('',*,*,#40594,.T.);
#57276=ORIENTED_EDGE('',*,*,#40595,.F.);
#57277=ORIENTED_EDGE('',*,*,#40231,.T.);
#57278=ORIENTED_EDGE('',*,*,#40595,.T.);
#57279=ORIENTED_EDGE('',*,*,#40596,.T.);
#57280=ORIENTED_EDGE('',*,*,#40597,.F.);
#57281=ORIENTED_EDGE('',*,*,#40596,.F.);
#57282=ORIENTED_EDGE('',*,*,#40594,.F.);
#57283=ORIENTED_EDGE('',*,*,#40598,.F.);
#57284=ORIENTED_EDGE('',*,*,#40599,.F.);
#57285=ORIENTED_EDGE('',*,*,#40233,.T.);
#57286=ORIENTED_EDGE('',*,*,#40600,.F.);
#57287=ORIENTED_EDGE('',*,*,#40601,.T.);
#57288=ORIENTED_EDGE('',*,*,#40602,.F.);
#57289=ORIENTED_EDGE('',*,*,#40234,.T.);
#57290=ORIENTED_EDGE('',*,*,#40602,.T.);
#57291=ORIENTED_EDGE('',*,*,#40603,.T.);
#57292=ORIENTED_EDGE('',*,*,#40604,.F.);
#57293=ORIENTED_EDGE('',*,*,#40603,.F.);
#57294=ORIENTED_EDGE('',*,*,#40601,.F.);
#57295=ORIENTED_EDGE('',*,*,#40605,.F.);
#57296=ORIENTED_EDGE('',*,*,#40606,.F.);
#57297=ORIENTED_EDGE('',*,*,#40236,.T.);
#57298=ORIENTED_EDGE('',*,*,#40607,.F.);
#57299=ORIENTED_EDGE('',*,*,#40608,.T.);
#57300=ORIENTED_EDGE('',*,*,#40609,.F.);
#57301=ORIENTED_EDGE('',*,*,#40237,.T.);
#57302=ORIENTED_EDGE('',*,*,#40609,.T.);
#57303=ORIENTED_EDGE('',*,*,#40610,.T.);
#57304=ORIENTED_EDGE('',*,*,#40611,.F.);
#57305=ORIENTED_EDGE('',*,*,#40610,.F.);
#57306=ORIENTED_EDGE('',*,*,#40608,.F.);
#57307=ORIENTED_EDGE('',*,*,#40612,.F.);
#57308=ORIENTED_EDGE('',*,*,#40613,.F.);
#57309=ORIENTED_EDGE('',*,*,#40239,.T.);
#57310=ORIENTED_EDGE('',*,*,#40614,.F.);
#57311=ORIENTED_EDGE('',*,*,#40615,.T.);
#57312=ORIENTED_EDGE('',*,*,#40616,.F.);
#57313=ORIENTED_EDGE('',*,*,#40240,.T.);
#57314=ORIENTED_EDGE('',*,*,#40616,.T.);
#57315=ORIENTED_EDGE('',*,*,#40617,.T.);
#57316=ORIENTED_EDGE('',*,*,#40618,.F.);
#57317=ORIENTED_EDGE('',*,*,#40617,.F.);
#57318=ORIENTED_EDGE('',*,*,#40615,.F.);
#57319=ORIENTED_EDGE('',*,*,#40619,.F.);
#57320=ORIENTED_EDGE('',*,*,#40620,.F.);
#57321=ORIENTED_EDGE('',*,*,#40242,.T.);
#57322=ORIENTED_EDGE('',*,*,#40621,.F.);
#57323=ORIENTED_EDGE('',*,*,#40622,.T.);
#57324=ORIENTED_EDGE('',*,*,#40623,.F.);
#57325=ORIENTED_EDGE('',*,*,#40243,.T.);
#57326=ORIENTED_EDGE('',*,*,#40623,.T.);
#57327=ORIENTED_EDGE('',*,*,#40624,.T.);
#57328=ORIENTED_EDGE('',*,*,#40625,.F.);
#57329=ORIENTED_EDGE('',*,*,#40624,.F.);
#57330=ORIENTED_EDGE('',*,*,#40622,.F.);
#57331=ORIENTED_EDGE('',*,*,#40626,.F.);
#57332=ORIENTED_EDGE('',*,*,#40627,.F.);
#57333=ORIENTED_EDGE('',*,*,#40245,.T.);
#57334=ORIENTED_EDGE('',*,*,#40628,.F.);
#57335=ORIENTED_EDGE('',*,*,#40629,.T.);
#57336=ORIENTED_EDGE('',*,*,#40630,.F.);
#57337=ORIENTED_EDGE('',*,*,#40631,.T.);
#57338=ORIENTED_EDGE('',*,*,#40632,.F.);
#57339=ORIENTED_EDGE('',*,*,#40246,.T.);
#57340=ORIENTED_EDGE('',*,*,#40630,.T.);
#57341=ORIENTED_EDGE('',*,*,#40633,.F.);
#57342=ORIENTED_EDGE('',*,*,#40634,.F.);
#57343=ORIENTED_EDGE('',*,*,#40631,.F.);
#57344=ORIENTED_EDGE('',*,*,#40629,.F.);
#57345=ORIENTED_EDGE('',*,*,#40248,.T.);
#57346=ORIENTED_EDGE('',*,*,#40635,.F.);
#57347=ORIENTED_EDGE('',*,*,#40636,.T.);
#57348=ORIENTED_EDGE('',*,*,#40637,.F.);
#57349=ORIENTED_EDGE('',*,*,#40249,.T.);
#57350=ORIENTED_EDGE('',*,*,#40637,.T.);
#57351=ORIENTED_EDGE('',*,*,#40638,.T.);
#57352=ORIENTED_EDGE('',*,*,#40639,.F.);
#57353=ORIENTED_EDGE('',*,*,#40638,.F.);
#57354=ORIENTED_EDGE('',*,*,#40636,.F.);
#57355=ORIENTED_EDGE('',*,*,#40640,.F.);
#57356=ORIENTED_EDGE('',*,*,#40641,.F.);
#57357=ORIENTED_EDGE('',*,*,#40251,.T.);
#57358=ORIENTED_EDGE('',*,*,#40642,.F.);
#57359=ORIENTED_EDGE('',*,*,#40643,.T.);
#57360=ORIENTED_EDGE('',*,*,#40644,.F.);
#57361=ORIENTED_EDGE('',*,*,#40252,.T.);
#57362=ORIENTED_EDGE('',*,*,#40644,.T.);
#57363=ORIENTED_EDGE('',*,*,#40645,.T.);
#57364=ORIENTED_EDGE('',*,*,#40646,.F.);
#57365=ORIENTED_EDGE('',*,*,#40645,.F.);
#57366=ORIENTED_EDGE('',*,*,#40643,.F.);
#57367=ORIENTED_EDGE('',*,*,#40647,.F.);
#57368=ORIENTED_EDGE('',*,*,#40648,.F.);
#57369=ORIENTED_EDGE('',*,*,#40455,.F.);
#57370=ORIENTED_EDGE('',*,*,#40649,.F.);
#57371=ORIENTED_EDGE('',*,*,#40650,.F.);
#57372=ORIENTED_EDGE('',*,*,#40651,.F.);
#57373=ORIENTED_EDGE('',*,*,#40254,.T.);
#57374=ORIENTED_EDGE('',*,*,#40652,.F.);
#57375=ORIENTED_EDGE('',*,*,#40649,.T.);
#57376=ORIENTED_EDGE('',*,*,#40454,.T.);
#57377=ORIENTED_EDGE('',*,*,#40653,.F.);
#57378=ORIENTED_EDGE('',*,*,#40256,.T.);
#57379=ORIENTED_EDGE('',*,*,#40451,.T.);
#57380=ORIENTED_EDGE('',*,*,#40654,.F.);
#57381=ORIENTED_EDGE('',*,*,#40655,.F.);
#57382=ORIENTED_EDGE('',*,*,#40656,.F.);
#57383=ORIENTED_EDGE('',*,*,#40261,.T.);
#57384=ORIENTED_EDGE('',*,*,#40260,.T.);
#57385=ORIENTED_EDGE('',*,*,#40657,.F.);
#57386=ORIENTED_EDGE('',*,*,#40264,.T.);
#57387=ORIENTED_EDGE('',*,*,#40262,.T.);
#57388=ORIENTED_EDGE('',*,*,#40656,.T.);
#57389=ORIENTED_EDGE('',*,*,#40658,.F.);
#57390=ORIENTED_EDGE('',*,*,#40659,.F.);
#57391=ORIENTED_EDGE('',*,*,#40268,.T.);
#57392=ORIENTED_EDGE('',*,*,#40267,.T.);
#57393=ORIENTED_EDGE('',*,*,#40660,.F.);
#57394=ORIENTED_EDGE('',*,*,#40271,.T.);
#57395=ORIENTED_EDGE('',*,*,#40269,.T.);
#57396=ORIENTED_EDGE('',*,*,#40659,.T.);
#57397=ORIENTED_EDGE('',*,*,#40661,.F.);
#57398=ORIENTED_EDGE('',*,*,#40662,.F.);
#57399=ORIENTED_EDGE('',*,*,#40275,.T.);
#57400=ORIENTED_EDGE('',*,*,#40274,.T.);
#57401=ORIENTED_EDGE('',*,*,#40663,.F.);
#57402=ORIENTED_EDGE('',*,*,#40278,.T.);
#57403=ORIENTED_EDGE('',*,*,#40276,.T.);
#57404=ORIENTED_EDGE('',*,*,#40662,.T.);
#57405=ORIENTED_EDGE('',*,*,#40664,.F.);
#57406=ORIENTED_EDGE('',*,*,#40665,.F.);
#57407=ORIENTED_EDGE('',*,*,#40282,.T.);
#57408=ORIENTED_EDGE('',*,*,#40281,.T.);
#57409=ORIENTED_EDGE('',*,*,#40666,.F.);
#57410=ORIENTED_EDGE('',*,*,#40285,.T.);
#57411=ORIENTED_EDGE('',*,*,#40283,.T.);
#57412=ORIENTED_EDGE('',*,*,#40665,.T.);
#57413=ORIENTED_EDGE('',*,*,#40667,.F.);
#57414=ORIENTED_EDGE('',*,*,#40668,.F.);
#57415=ORIENTED_EDGE('',*,*,#40289,.T.);
#57416=ORIENTED_EDGE('',*,*,#40288,.T.);
#57417=ORIENTED_EDGE('',*,*,#40669,.F.);
#57418=ORIENTED_EDGE('',*,*,#40292,.T.);
#57419=ORIENTED_EDGE('',*,*,#40290,.T.);
#57420=ORIENTED_EDGE('',*,*,#40668,.T.);
#57421=ORIENTED_EDGE('',*,*,#40670,.F.);
#57422=ORIENTED_EDGE('',*,*,#40671,.F.);
#57423=ORIENTED_EDGE('',*,*,#40296,.T.);
#57424=ORIENTED_EDGE('',*,*,#40295,.T.);
#57425=ORIENTED_EDGE('',*,*,#40672,.F.);
#57426=ORIENTED_EDGE('',*,*,#40299,.T.);
#57427=ORIENTED_EDGE('',*,*,#40297,.T.);
#57428=ORIENTED_EDGE('',*,*,#40671,.T.);
#57429=ORIENTED_EDGE('',*,*,#40673,.F.);
#57430=ORIENTED_EDGE('',*,*,#40674,.F.);
#57431=ORIENTED_EDGE('',*,*,#34395,.T.);
#57432=ORIENTED_EDGE('',*,*,#40301,.T.);
#57433=ORIENTED_EDGE('',*,*,#40675,.F.);
#57434=ORIENTED_EDGE('',*,*,#40302,.T.);
#57435=ORIENTED_EDGE('',*,*,#34396,.T.);
#57436=ORIENTED_EDGE('',*,*,#40674,.T.);
#57437=ORIENTED_EDGE('',*,*,#40676,.F.);
#57438=ORIENTED_EDGE('',*,*,#40677,.F.);
#57439=ORIENTED_EDGE('',*,*,#40306,.T.);
#57440=ORIENTED_EDGE('',*,*,#40305,.T.);
#57441=ORIENTED_EDGE('',*,*,#40678,.F.);
#57442=ORIENTED_EDGE('',*,*,#40309,.T.);
#57443=ORIENTED_EDGE('',*,*,#40307,.T.);
#57444=ORIENTED_EDGE('',*,*,#40677,.T.);
#57445=ORIENTED_EDGE('',*,*,#40679,.F.);
#57446=ORIENTED_EDGE('',*,*,#40680,.F.);
#57447=ORIENTED_EDGE('',*,*,#40313,.T.);
#57448=ORIENTED_EDGE('',*,*,#40312,.T.);
#57449=ORIENTED_EDGE('',*,*,#40681,.F.);
#57450=ORIENTED_EDGE('',*,*,#40316,.T.);
#57451=ORIENTED_EDGE('',*,*,#40314,.T.);
#57452=ORIENTED_EDGE('',*,*,#40680,.T.);
#57453=ORIENTED_EDGE('',*,*,#40682,.F.);
#57454=ORIENTED_EDGE('',*,*,#40683,.F.);
#57455=ORIENTED_EDGE('',*,*,#40320,.T.);
#57456=ORIENTED_EDGE('',*,*,#40319,.T.);
#57457=ORIENTED_EDGE('',*,*,#40684,.F.);
#57458=ORIENTED_EDGE('',*,*,#40323,.T.);
#57459=ORIENTED_EDGE('',*,*,#40321,.T.);
#57460=ORIENTED_EDGE('',*,*,#40683,.T.);
#57461=ORIENTED_EDGE('',*,*,#40685,.F.);
#57462=ORIENTED_EDGE('',*,*,#40686,.F.);
#57463=ORIENTED_EDGE('',*,*,#40327,.T.);
#57464=ORIENTED_EDGE('',*,*,#40326,.T.);
#57465=ORIENTED_EDGE('',*,*,#40687,.F.);
#57466=ORIENTED_EDGE('',*,*,#40330,.T.);
#57467=ORIENTED_EDGE('',*,*,#40328,.T.);
#57468=ORIENTED_EDGE('',*,*,#40686,.T.);
#57469=ORIENTED_EDGE('',*,*,#40688,.F.);
#57470=ORIENTED_EDGE('',*,*,#40689,.F.);
#57471=ORIENTED_EDGE('',*,*,#40334,.T.);
#57472=ORIENTED_EDGE('',*,*,#40333,.T.);
#57473=ORIENTED_EDGE('',*,*,#40690,.F.);
#57474=ORIENTED_EDGE('',*,*,#40337,.T.);
#57475=ORIENTED_EDGE('',*,*,#40335,.T.);
#57476=ORIENTED_EDGE('',*,*,#40689,.T.);
#57477=ORIENTED_EDGE('',*,*,#40691,.F.);
#57478=ORIENTED_EDGE('',*,*,#40692,.F.);
#57479=ORIENTED_EDGE('',*,*,#40341,.T.);
#57480=ORIENTED_EDGE('',*,*,#40340,.T.);
#57481=ORIENTED_EDGE('',*,*,#40693,.F.);
#57482=ORIENTED_EDGE('',*,*,#40344,.T.);
#57483=ORIENTED_EDGE('',*,*,#40342,.T.);
#57484=ORIENTED_EDGE('',*,*,#40692,.T.);
#57485=ORIENTED_EDGE('',*,*,#40694,.F.);
#57486=ORIENTED_EDGE('',*,*,#40695,.F.);
#57487=ORIENTED_EDGE('',*,*,#40348,.T.);
#57488=ORIENTED_EDGE('',*,*,#40347,.T.);
#57489=ORIENTED_EDGE('',*,*,#40696,.F.);
#57490=ORIENTED_EDGE('',*,*,#40351,.T.);
#57491=ORIENTED_EDGE('',*,*,#40349,.T.);
#57492=ORIENTED_EDGE('',*,*,#40695,.T.);
#57493=ORIENTED_EDGE('',*,*,#40697,.F.);
#57494=ORIENTED_EDGE('',*,*,#40698,.F.);
#57495=ORIENTED_EDGE('',*,*,#40355,.T.);
#57496=ORIENTED_EDGE('',*,*,#40354,.T.);
#57497=ORIENTED_EDGE('',*,*,#40699,.F.);
#57498=ORIENTED_EDGE('',*,*,#40358,.T.);
#57499=ORIENTED_EDGE('',*,*,#40356,.T.);
#57500=ORIENTED_EDGE('',*,*,#40698,.T.);
#57501=ORIENTED_EDGE('',*,*,#40700,.F.);
#57502=ORIENTED_EDGE('',*,*,#40701,.F.);
#57503=ORIENTED_EDGE('',*,*,#40362,.T.);
#57504=ORIENTED_EDGE('',*,*,#40361,.T.);
#57505=ORIENTED_EDGE('',*,*,#40702,.F.);
#57506=ORIENTED_EDGE('',*,*,#40365,.T.);
#57507=ORIENTED_EDGE('',*,*,#40363,.T.);
#57508=ORIENTED_EDGE('',*,*,#40701,.T.);
#57509=ORIENTED_EDGE('',*,*,#40703,.F.);
#57510=ORIENTED_EDGE('',*,*,#40704,.F.);
#57511=ORIENTED_EDGE('',*,*,#40369,.T.);
#57512=ORIENTED_EDGE('',*,*,#40368,.T.);
#57513=ORIENTED_EDGE('',*,*,#40705,.F.);
#57514=ORIENTED_EDGE('',*,*,#40372,.T.);
#57515=ORIENTED_EDGE('',*,*,#40370,.T.);
#57516=ORIENTED_EDGE('',*,*,#40704,.T.);
#57517=ORIENTED_EDGE('',*,*,#40706,.F.);
#57518=ORIENTED_EDGE('',*,*,#40707,.F.);
#57519=ORIENTED_EDGE('',*,*,#40376,.T.);
#57520=ORIENTED_EDGE('',*,*,#40375,.T.);
#57521=ORIENTED_EDGE('',*,*,#40708,.F.);
#57522=ORIENTED_EDGE('',*,*,#40379,.T.);
#57523=ORIENTED_EDGE('',*,*,#40377,.T.);
#57524=ORIENTED_EDGE('',*,*,#40707,.T.);
#57525=ORIENTED_EDGE('',*,*,#40709,.F.);
#57526=ORIENTED_EDGE('',*,*,#40710,.F.);
#57527=ORIENTED_EDGE('',*,*,#40383,.T.);
#57528=ORIENTED_EDGE('',*,*,#40382,.T.);
#57529=ORIENTED_EDGE('',*,*,#40711,.F.);
#57530=ORIENTED_EDGE('',*,*,#40386,.T.);
#57531=ORIENTED_EDGE('',*,*,#40384,.T.);
#57532=ORIENTED_EDGE('',*,*,#40710,.T.);
#57533=ORIENTED_EDGE('',*,*,#40712,.F.);
#57534=ORIENTED_EDGE('',*,*,#40713,.F.);
#57535=ORIENTED_EDGE('',*,*,#40392,.T.);
#57536=ORIENTED_EDGE('',*,*,#40389,.T.);
#57537=ORIENTED_EDGE('',*,*,#40393,.T.);
#57538=ORIENTED_EDGE('',*,*,#40713,.T.);
#57539=ORIENTED_EDGE('',*,*,#40714,.F.);
#57540=ORIENTED_EDGE('',*,*,#40391,.T.);
#57541=ORIENTED_EDGE('',*,*,#40398,.T.);
#57542=ORIENTED_EDGE('',*,*,#40394,.T.);
#57543=ORIENTED_EDGE('',*,*,#40715,.F.);
#57544=ORIENTED_EDGE('',*,*,#40716,.F.);
#57545=ORIENTED_EDGE('',*,*,#40717,.F.);
#57546=ORIENTED_EDGE('',*,*,#40400,.T.);
#57547=ORIENTED_EDGE('',*,*,#40399,.T.);
#57548=ORIENTED_EDGE('',*,*,#40716,.T.);
#57549=ORIENTED_EDGE('',*,*,#40718,.F.);
#57550=ORIENTED_EDGE('',*,*,#40719,.F.);
#57551=ORIENTED_EDGE('',*,*,#40404,.T.);
#57552=ORIENTED_EDGE('',*,*,#40403,.T.);
#57553=ORIENTED_EDGE('',*,*,#40720,.F.);
#57554=ORIENTED_EDGE('',*,*,#40407,.T.);
#57555=ORIENTED_EDGE('',*,*,#40405,.T.);
#57556=ORIENTED_EDGE('',*,*,#40719,.T.);
#57557=ORIENTED_EDGE('',*,*,#40721,.F.);
#57558=ORIENTED_EDGE('',*,*,#40722,.F.);
#57559=ORIENTED_EDGE('',*,*,#40411,.T.);
#57560=ORIENTED_EDGE('',*,*,#40410,.T.);
#57561=ORIENTED_EDGE('',*,*,#40723,.F.);
#57562=ORIENTED_EDGE('',*,*,#40414,.T.);
#57563=ORIENTED_EDGE('',*,*,#40412,.T.);
#57564=ORIENTED_EDGE('',*,*,#40722,.T.);
#57565=ORIENTED_EDGE('',*,*,#40724,.F.);
#57566=ORIENTED_EDGE('',*,*,#40725,.F.);
#57567=ORIENTED_EDGE('',*,*,#40418,.T.);
#57568=ORIENTED_EDGE('',*,*,#40417,.T.);
#57569=ORIENTED_EDGE('',*,*,#40726,.F.);
#57570=ORIENTED_EDGE('',*,*,#40421,.T.);
#57571=ORIENTED_EDGE('',*,*,#40419,.T.);
#57572=ORIENTED_EDGE('',*,*,#40725,.T.);
#57573=ORIENTED_EDGE('',*,*,#40727,.F.);
#57574=ORIENTED_EDGE('',*,*,#40728,.F.);
#57575=ORIENTED_EDGE('',*,*,#40425,.T.);
#57576=ORIENTED_EDGE('',*,*,#40424,.T.);
#57577=ORIENTED_EDGE('',*,*,#40729,.F.);
#57578=ORIENTED_EDGE('',*,*,#40428,.T.);
#57579=ORIENTED_EDGE('',*,*,#40426,.T.);
#57580=ORIENTED_EDGE('',*,*,#40728,.T.);
#57581=ORIENTED_EDGE('',*,*,#40730,.F.);
#57582=ORIENTED_EDGE('',*,*,#40731,.F.);
#57583=ORIENTED_EDGE('',*,*,#40432,.T.);
#57584=ORIENTED_EDGE('',*,*,#40431,.T.);
#57585=ORIENTED_EDGE('',*,*,#40732,.F.);
#57586=ORIENTED_EDGE('',*,*,#40435,.T.);
#57587=ORIENTED_EDGE('',*,*,#40433,.T.);
#57588=ORIENTED_EDGE('',*,*,#40731,.T.);
#57589=ORIENTED_EDGE('',*,*,#40733,.F.);
#57590=ORIENTED_EDGE('',*,*,#40734,.F.);
#57591=ORIENTED_EDGE('',*,*,#40439,.T.);
#57592=ORIENTED_EDGE('',*,*,#40438,.T.);
#57593=ORIENTED_EDGE('',*,*,#40735,.F.);
#57594=ORIENTED_EDGE('',*,*,#40442,.T.);
#57595=ORIENTED_EDGE('',*,*,#40440,.T.);
#57596=ORIENTED_EDGE('',*,*,#40734,.T.);
#57597=ORIENTED_EDGE('',*,*,#40736,.F.);
#57598=ORIENTED_EDGE('',*,*,#40737,.F.);
#57599=ORIENTED_EDGE('',*,*,#40446,.T.);
#57600=ORIENTED_EDGE('',*,*,#40445,.T.);
#57601=ORIENTED_EDGE('',*,*,#40738,.F.);
#57602=ORIENTED_EDGE('',*,*,#40449,.T.);
#57603=ORIENTED_EDGE('',*,*,#40447,.T.);
#57604=ORIENTED_EDGE('',*,*,#40737,.T.);
#57605=ORIENTED_EDGE('',*,*,#40739,.F.);
#57606=ORIENTED_EDGE('',*,*,#40654,.T.);
#57607=ORIENTED_EDGE('',*,*,#40450,.T.);
#57608=ORIENTED_EDGE('',*,*,#40453,.T.);
#57609=ORIENTED_EDGE('',*,*,#40651,.T.);
#57610=ORIENTED_EDGE('',*,*,#40740,.F.);
#57611=ORIENTED_EDGE('',*,*,#40741,.F.);
#57612=ORIENTED_EDGE('',*,*,#40456,.T.);
#57613=ORIENTED_EDGE('',*,*,#40462,.T.);
#57614=ORIENTED_EDGE('',*,*,#40457,.T.);
#57615=ORIENTED_EDGE('',*,*,#40742,.F.);
#57616=ORIENTED_EDGE('',*,*,#40743,.F.);
#57617=ORIENTED_EDGE('',*,*,#40463,.T.);
#57618=ORIENTED_EDGE('',*,*,#40743,.T.);
#57619=ORIENTED_EDGE('',*,*,#40744,.F.);
#57620=ORIENTED_EDGE('',*,*,#40461,.T.);
#57621=ORIENTED_EDGE('',*,*,#40469,.T.);
#57622=ORIENTED_EDGE('',*,*,#40464,.T.);
#57623=ORIENTED_EDGE('',*,*,#40745,.F.);
#57624=ORIENTED_EDGE('',*,*,#40746,.F.);
#57625=ORIENTED_EDGE('',*,*,#40470,.T.);
#57626=ORIENTED_EDGE('',*,*,#40746,.T.);
#57627=ORIENTED_EDGE('',*,*,#40747,.F.);
#57628=ORIENTED_EDGE('',*,*,#40468,.T.);
#57629=ORIENTED_EDGE('',*,*,#40476,.T.);
#57630=ORIENTED_EDGE('',*,*,#40471,.T.);
#57631=ORIENTED_EDGE('',*,*,#40748,.F.);
#57632=ORIENTED_EDGE('',*,*,#40749,.F.);
#57633=ORIENTED_EDGE('',*,*,#40477,.T.);
#57634=ORIENTED_EDGE('',*,*,#40749,.T.);
#57635=ORIENTED_EDGE('',*,*,#40750,.F.);
#57636=ORIENTED_EDGE('',*,*,#40475,.T.);
#57637=ORIENTED_EDGE('',*,*,#40483,.T.);
#57638=ORIENTED_EDGE('',*,*,#40478,.T.);
#57639=ORIENTED_EDGE('',*,*,#40751,.F.);
#57640=ORIENTED_EDGE('',*,*,#40752,.F.);
#57641=ORIENTED_EDGE('',*,*,#40484,.T.);
#57642=ORIENTED_EDGE('',*,*,#40752,.T.);
#57643=ORIENTED_EDGE('',*,*,#40753,.F.);
#57644=ORIENTED_EDGE('',*,*,#40482,.T.);
#57645=ORIENTED_EDGE('',*,*,#40490,.T.);
#57646=ORIENTED_EDGE('',*,*,#40485,.T.);
#57647=ORIENTED_EDGE('',*,*,#40754,.F.);
#57648=ORIENTED_EDGE('',*,*,#40755,.F.);
#57649=ORIENTED_EDGE('',*,*,#40491,.T.);
#57650=ORIENTED_EDGE('',*,*,#40755,.T.);
#57651=ORIENTED_EDGE('',*,*,#40756,.F.);
#57652=ORIENTED_EDGE('',*,*,#40489,.T.);
#57653=ORIENTED_EDGE('',*,*,#40497,.T.);
#57654=ORIENTED_EDGE('',*,*,#40492,.T.);
#57655=ORIENTED_EDGE('',*,*,#40757,.F.);
#57656=ORIENTED_EDGE('',*,*,#40758,.F.);
#57657=ORIENTED_EDGE('',*,*,#40498,.T.);
#57658=ORIENTED_EDGE('',*,*,#40758,.T.);
#57659=ORIENTED_EDGE('',*,*,#40759,.F.);
#57660=ORIENTED_EDGE('',*,*,#40496,.T.);
#57661=ORIENTED_EDGE('',*,*,#40504,.T.);
#57662=ORIENTED_EDGE('',*,*,#40499,.T.);
#57663=ORIENTED_EDGE('',*,*,#40760,.F.);
#57664=ORIENTED_EDGE('',*,*,#40761,.F.);
#57665=ORIENTED_EDGE('',*,*,#40505,.T.);
#57666=ORIENTED_EDGE('',*,*,#40761,.T.);
#57667=ORIENTED_EDGE('',*,*,#40762,.F.);
#57668=ORIENTED_EDGE('',*,*,#40503,.T.);
#57669=ORIENTED_EDGE('',*,*,#40511,.T.);
#57670=ORIENTED_EDGE('',*,*,#40506,.T.);
#57671=ORIENTED_EDGE('',*,*,#40763,.F.);
#57672=ORIENTED_EDGE('',*,*,#40764,.F.);
#57673=ORIENTED_EDGE('',*,*,#40512,.T.);
#57674=ORIENTED_EDGE('',*,*,#40764,.T.);
#57675=ORIENTED_EDGE('',*,*,#40765,.F.);
#57676=ORIENTED_EDGE('',*,*,#40510,.T.);
#57677=ORIENTED_EDGE('',*,*,#40518,.T.);
#57678=ORIENTED_EDGE('',*,*,#40513,.T.);
#57679=ORIENTED_EDGE('',*,*,#40766,.F.);
#57680=ORIENTED_EDGE('',*,*,#40767,.F.);
#57681=ORIENTED_EDGE('',*,*,#40519,.T.);
#57682=ORIENTED_EDGE('',*,*,#40767,.T.);
#57683=ORIENTED_EDGE('',*,*,#40768,.F.);
#57684=ORIENTED_EDGE('',*,*,#40517,.T.);
#57685=ORIENTED_EDGE('',*,*,#40525,.T.);
#57686=ORIENTED_EDGE('',*,*,#40520,.T.);
#57687=ORIENTED_EDGE('',*,*,#40769,.F.);
#57688=ORIENTED_EDGE('',*,*,#40770,.F.);
#57689=ORIENTED_EDGE('',*,*,#40526,.T.);
#57690=ORIENTED_EDGE('',*,*,#40770,.T.);
#57691=ORIENTED_EDGE('',*,*,#40771,.F.);
#57692=ORIENTED_EDGE('',*,*,#40524,.T.);
#57693=ORIENTED_EDGE('',*,*,#40532,.T.);
#57694=ORIENTED_EDGE('',*,*,#40527,.T.);
#57695=ORIENTED_EDGE('',*,*,#40772,.F.);
#57696=ORIENTED_EDGE('',*,*,#40773,.F.);
#57697=ORIENTED_EDGE('',*,*,#40533,.T.);
#57698=ORIENTED_EDGE('',*,*,#40773,.T.);
#57699=ORIENTED_EDGE('',*,*,#40774,.F.);
#57700=ORIENTED_EDGE('',*,*,#40531,.T.);
#57701=ORIENTED_EDGE('',*,*,#40539,.T.);
#57702=ORIENTED_EDGE('',*,*,#40534,.T.);
#57703=ORIENTED_EDGE('',*,*,#40775,.F.);
#57704=ORIENTED_EDGE('',*,*,#40776,.F.);
#57705=ORIENTED_EDGE('',*,*,#40540,.T.);
#57706=ORIENTED_EDGE('',*,*,#40776,.T.);
#57707=ORIENTED_EDGE('',*,*,#40777,.F.);
#57708=ORIENTED_EDGE('',*,*,#40538,.T.);
#57709=ORIENTED_EDGE('',*,*,#40546,.T.);
#57710=ORIENTED_EDGE('',*,*,#40541,.T.);
#57711=ORIENTED_EDGE('',*,*,#40778,.F.);
#57712=ORIENTED_EDGE('',*,*,#40779,.F.);
#57713=ORIENTED_EDGE('',*,*,#40547,.T.);
#57714=ORIENTED_EDGE('',*,*,#40779,.T.);
#57715=ORIENTED_EDGE('',*,*,#40780,.F.);
#57716=ORIENTED_EDGE('',*,*,#40545,.T.);
#57717=ORIENTED_EDGE('',*,*,#34392,.T.);
#57718=ORIENTED_EDGE('',*,*,#40548,.T.);
#57719=ORIENTED_EDGE('',*,*,#40781,.F.);
#57720=ORIENTED_EDGE('',*,*,#40782,.F.);
#57721=ORIENTED_EDGE('',*,*,#34389,.T.);
#57722=ORIENTED_EDGE('',*,*,#40782,.T.);
#57723=ORIENTED_EDGE('',*,*,#40783,.F.);
#57724=ORIENTED_EDGE('',*,*,#40550,.T.);
#57725=ORIENTED_EDGE('',*,*,#40556,.T.);
#57726=ORIENTED_EDGE('',*,*,#40551,.T.);
#57727=ORIENTED_EDGE('',*,*,#40784,.F.);
#57728=ORIENTED_EDGE('',*,*,#40785,.F.);
#57729=ORIENTED_EDGE('',*,*,#40557,.T.);
#57730=ORIENTED_EDGE('',*,*,#40785,.T.);
#57731=ORIENTED_EDGE('',*,*,#40786,.F.);
#57732=ORIENTED_EDGE('',*,*,#40555,.T.);
#57733=ORIENTED_EDGE('',*,*,#40563,.T.);
#57734=ORIENTED_EDGE('',*,*,#40558,.T.);
#57735=ORIENTED_EDGE('',*,*,#40787,.F.);
#57736=ORIENTED_EDGE('',*,*,#40788,.F.);
#57737=ORIENTED_EDGE('',*,*,#40564,.T.);
#57738=ORIENTED_EDGE('',*,*,#40788,.T.);
#57739=ORIENTED_EDGE('',*,*,#40789,.F.);
#57740=ORIENTED_EDGE('',*,*,#40562,.T.);
#57741=ORIENTED_EDGE('',*,*,#40570,.T.);
#57742=ORIENTED_EDGE('',*,*,#40565,.T.);
#57743=ORIENTED_EDGE('',*,*,#40790,.F.);
#57744=ORIENTED_EDGE('',*,*,#40791,.F.);
#57745=ORIENTED_EDGE('',*,*,#40571,.T.);
#57746=ORIENTED_EDGE('',*,*,#40791,.T.);
#57747=ORIENTED_EDGE('',*,*,#40792,.F.);
#57748=ORIENTED_EDGE('',*,*,#40569,.T.);
#57749=ORIENTED_EDGE('',*,*,#40577,.T.);
#57750=ORIENTED_EDGE('',*,*,#40572,.T.);
#57751=ORIENTED_EDGE('',*,*,#40793,.F.);
#57752=ORIENTED_EDGE('',*,*,#40794,.F.);
#57753=ORIENTED_EDGE('',*,*,#40578,.T.);
#57754=ORIENTED_EDGE('',*,*,#40794,.T.);
#57755=ORIENTED_EDGE('',*,*,#40795,.F.);
#57756=ORIENTED_EDGE('',*,*,#40576,.T.);
#57757=ORIENTED_EDGE('',*,*,#40584,.T.);
#57758=ORIENTED_EDGE('',*,*,#40579,.T.);
#57759=ORIENTED_EDGE('',*,*,#40796,.F.);
#57760=ORIENTED_EDGE('',*,*,#40797,.F.);
#57761=ORIENTED_EDGE('',*,*,#40585,.T.);
#57762=ORIENTED_EDGE('',*,*,#40797,.T.);
#57763=ORIENTED_EDGE('',*,*,#40798,.F.);
#57764=ORIENTED_EDGE('',*,*,#40583,.T.);
#57765=ORIENTED_EDGE('',*,*,#40591,.T.);
#57766=ORIENTED_EDGE('',*,*,#40586,.T.);
#57767=ORIENTED_EDGE('',*,*,#40799,.F.);
#57768=ORIENTED_EDGE('',*,*,#40800,.F.);
#57769=ORIENTED_EDGE('',*,*,#40592,.T.);
#57770=ORIENTED_EDGE('',*,*,#40800,.T.);
#57771=ORIENTED_EDGE('',*,*,#40801,.F.);
#57772=ORIENTED_EDGE('',*,*,#40590,.T.);
#57773=ORIENTED_EDGE('',*,*,#40598,.T.);
#57774=ORIENTED_EDGE('',*,*,#40593,.T.);
#57775=ORIENTED_EDGE('',*,*,#40802,.F.);
#57776=ORIENTED_EDGE('',*,*,#40803,.F.);
#57777=ORIENTED_EDGE('',*,*,#40599,.T.);
#57778=ORIENTED_EDGE('',*,*,#40803,.T.);
#57779=ORIENTED_EDGE('',*,*,#40804,.F.);
#57780=ORIENTED_EDGE('',*,*,#40597,.T.);
#57781=ORIENTED_EDGE('',*,*,#40605,.T.);
#57782=ORIENTED_EDGE('',*,*,#40600,.T.);
#57783=ORIENTED_EDGE('',*,*,#40805,.F.);
#57784=ORIENTED_EDGE('',*,*,#40806,.F.);
#57785=ORIENTED_EDGE('',*,*,#40606,.T.);
#57786=ORIENTED_EDGE('',*,*,#40806,.T.);
#57787=ORIENTED_EDGE('',*,*,#40807,.F.);
#57788=ORIENTED_EDGE('',*,*,#40604,.T.);
#57789=ORIENTED_EDGE('',*,*,#40612,.T.);
#57790=ORIENTED_EDGE('',*,*,#40607,.T.);
#57791=ORIENTED_EDGE('',*,*,#40808,.F.);
#57792=ORIENTED_EDGE('',*,*,#40809,.F.);
#57793=ORIENTED_EDGE('',*,*,#40613,.T.);
#57794=ORIENTED_EDGE('',*,*,#40809,.T.);
#57795=ORIENTED_EDGE('',*,*,#40810,.F.);
#57796=ORIENTED_EDGE('',*,*,#40611,.T.);
#57797=ORIENTED_EDGE('',*,*,#40619,.T.);
#57798=ORIENTED_EDGE('',*,*,#40614,.T.);
#57799=ORIENTED_EDGE('',*,*,#40811,.F.);
#57800=ORIENTED_EDGE('',*,*,#40812,.F.);
#57801=ORIENTED_EDGE('',*,*,#40620,.T.);
#57802=ORIENTED_EDGE('',*,*,#40812,.T.);
#57803=ORIENTED_EDGE('',*,*,#40813,.F.);
#57804=ORIENTED_EDGE('',*,*,#40618,.T.);
#57805=ORIENTED_EDGE('',*,*,#40626,.T.);
#57806=ORIENTED_EDGE('',*,*,#40621,.T.);
#57807=ORIENTED_EDGE('',*,*,#40814,.F.);
#57808=ORIENTED_EDGE('',*,*,#40815,.F.);
#57809=ORIENTED_EDGE('',*,*,#40627,.T.);
#57810=ORIENTED_EDGE('',*,*,#40815,.T.);
#57811=ORIENTED_EDGE('',*,*,#40816,.F.);
#57812=ORIENTED_EDGE('',*,*,#40625,.T.);
#57813=ORIENTED_EDGE('',*,*,#40817,.F.);
#57814=ORIENTED_EDGE('',*,*,#40818,.F.);
#57815=ORIENTED_EDGE('',*,*,#40633,.T.);
#57816=ORIENTED_EDGE('',*,*,#40628,.T.);
#57817=ORIENTED_EDGE('',*,*,#40634,.T.);
#57818=ORIENTED_EDGE('',*,*,#40818,.T.);
#57819=ORIENTED_EDGE('',*,*,#40819,.F.);
#57820=ORIENTED_EDGE('',*,*,#40632,.T.);
#57821=ORIENTED_EDGE('',*,*,#40640,.T.);
#57822=ORIENTED_EDGE('',*,*,#40635,.T.);
#57823=ORIENTED_EDGE('',*,*,#40820,.F.);
#57824=ORIENTED_EDGE('',*,*,#40821,.F.);
#57825=ORIENTED_EDGE('',*,*,#40641,.T.);
#57826=ORIENTED_EDGE('',*,*,#40821,.T.);
#57827=ORIENTED_EDGE('',*,*,#40822,.F.);
#57828=ORIENTED_EDGE('',*,*,#40639,.T.);
#57829=ORIENTED_EDGE('',*,*,#40647,.T.);
#57830=ORIENTED_EDGE('',*,*,#40642,.T.);
#57831=ORIENTED_EDGE('',*,*,#40823,.F.);
#57832=ORIENTED_EDGE('',*,*,#40824,.F.);
#57833=ORIENTED_EDGE('',*,*,#40648,.T.);
#57834=ORIENTED_EDGE('',*,*,#40824,.T.);
#57835=ORIENTED_EDGE('',*,*,#40825,.F.);
#57836=ORIENTED_EDGE('',*,*,#40646,.T.);
#57837=ORIENTED_EDGE('',*,*,#40650,.T.);
#57838=ORIENTED_EDGE('',*,*,#40652,.T.);
#57839=ORIENTED_EDGE('',*,*,#40826,.F.);
#57840=ORIENTED_EDGE('',*,*,#40740,.T.);
#57841=ORIENTED_EDGE('',*,*,#40827,.T.);
#57842=ORIENTED_EDGE('',*,*,#40828,.F.);
#57843=ORIENTED_EDGE('',*,*,#40653,.T.);
#57844=ORIENTED_EDGE('',*,*,#40829,.F.);
#57845=ORIENTED_EDGE('',*,*,#40830,.F.);
#57846=ORIENTED_EDGE('',*,*,#40831,.F.);
#57847=ORIENTED_EDGE('',*,*,#40832,.F.);
#57848=ORIENTED_EDGE('',*,*,#40827,.F.);
#57849=ORIENTED_EDGE('',*,*,#40832,.T.);
#57850=ORIENTED_EDGE('',*,*,#40833,.F.);
#57851=ORIENTED_EDGE('',*,*,#40655,.T.);
#57852=ORIENTED_EDGE('',*,*,#40828,.T.);
#57853=ORIENTED_EDGE('',*,*,#40834,.T.);
#57854=ORIENTED_EDGE('',*,*,#40835,.F.);
#57855=ORIENTED_EDGE('',*,*,#40657,.T.);
#57856=ORIENTED_EDGE('',*,*,#40836,.F.);
#57857=ORIENTED_EDGE('',*,*,#40837,.F.);
#57858=ORIENTED_EDGE('',*,*,#40838,.F.);
#57859=ORIENTED_EDGE('',*,*,#40839,.F.);
#57860=ORIENTED_EDGE('',*,*,#40834,.F.);
#57861=ORIENTED_EDGE('',*,*,#40839,.T.);
#57862=ORIENTED_EDGE('',*,*,#40840,.F.);
#57863=ORIENTED_EDGE('',*,*,#40658,.T.);
#57864=ORIENTED_EDGE('',*,*,#40835,.T.);
#57865=ORIENTED_EDGE('',*,*,#40841,.T.);
#57866=ORIENTED_EDGE('',*,*,#40842,.F.);
#57867=ORIENTED_EDGE('',*,*,#40660,.T.);
#57868=ORIENTED_EDGE('',*,*,#40843,.F.);
#57869=ORIENTED_EDGE('',*,*,#40844,.F.);
#57870=ORIENTED_EDGE('',*,*,#40845,.F.);
#57871=ORIENTED_EDGE('',*,*,#40846,.F.);
#57872=ORIENTED_EDGE('',*,*,#40841,.F.);
#57873=ORIENTED_EDGE('',*,*,#40846,.T.);
#57874=ORIENTED_EDGE('',*,*,#40847,.F.);
#57875=ORIENTED_EDGE('',*,*,#40661,.T.);
#57876=ORIENTED_EDGE('',*,*,#40842,.T.);
#57877=ORIENTED_EDGE('',*,*,#40848,.T.);
#57878=ORIENTED_EDGE('',*,*,#40849,.F.);
#57879=ORIENTED_EDGE('',*,*,#40663,.T.);
#57880=ORIENTED_EDGE('',*,*,#40850,.F.);
#57881=ORIENTED_EDGE('',*,*,#40851,.F.);
#57882=ORIENTED_EDGE('',*,*,#40852,.F.);
#57883=ORIENTED_EDGE('',*,*,#40853,.F.);
#57884=ORIENTED_EDGE('',*,*,#40848,.F.);
#57885=ORIENTED_EDGE('',*,*,#40853,.T.);
#57886=ORIENTED_EDGE('',*,*,#40854,.F.);
#57887=ORIENTED_EDGE('',*,*,#40664,.T.);
#57888=ORIENTED_EDGE('',*,*,#40849,.T.);
#57889=ORIENTED_EDGE('',*,*,#40855,.T.);
#57890=ORIENTED_EDGE('',*,*,#40856,.F.);
#57891=ORIENTED_EDGE('',*,*,#40666,.T.);
#57892=ORIENTED_EDGE('',*,*,#40857,.F.);
#57893=ORIENTED_EDGE('',*,*,#40858,.F.);
#57894=ORIENTED_EDGE('',*,*,#40859,.F.);
#57895=ORIENTED_EDGE('',*,*,#40860,.F.);
#57896=ORIENTED_EDGE('',*,*,#40855,.F.);
#57897=ORIENTED_EDGE('',*,*,#40860,.T.);
#57898=ORIENTED_EDGE('',*,*,#40861,.F.);
#57899=ORIENTED_EDGE('',*,*,#40667,.T.);
#57900=ORIENTED_EDGE('',*,*,#40856,.T.);
#57901=ORIENTED_EDGE('',*,*,#40862,.T.);
#57902=ORIENTED_EDGE('',*,*,#40863,.F.);
#57903=ORIENTED_EDGE('',*,*,#40669,.T.);
#57904=ORIENTED_EDGE('',*,*,#40864,.F.);
#57905=ORIENTED_EDGE('',*,*,#40865,.F.);
#57906=ORIENTED_EDGE('',*,*,#40866,.F.);
#57907=ORIENTED_EDGE('',*,*,#40867,.F.);
#57908=ORIENTED_EDGE('',*,*,#40862,.F.);
#57909=ORIENTED_EDGE('',*,*,#40867,.T.);
#57910=ORIENTED_EDGE('',*,*,#40868,.F.);
#57911=ORIENTED_EDGE('',*,*,#40670,.T.);
#57912=ORIENTED_EDGE('',*,*,#40863,.T.);
#57913=ORIENTED_EDGE('',*,*,#40869,.T.);
#57914=ORIENTED_EDGE('',*,*,#40870,.F.);
#57915=ORIENTED_EDGE('',*,*,#40672,.T.);
#57916=ORIENTED_EDGE('',*,*,#40871,.F.);
#57917=ORIENTED_EDGE('',*,*,#40872,.F.);
#57918=ORIENTED_EDGE('',*,*,#40873,.F.);
#57919=ORIENTED_EDGE('',*,*,#40874,.F.);
#57920=ORIENTED_EDGE('',*,*,#40869,.F.);
#57921=ORIENTED_EDGE('',*,*,#40874,.T.);
#57922=ORIENTED_EDGE('',*,*,#40875,.F.);
#57923=ORIENTED_EDGE('',*,*,#40673,.T.);
#57924=ORIENTED_EDGE('',*,*,#40870,.T.);
#57925=ORIENTED_EDGE('',*,*,#40876,.T.);
#57926=ORIENTED_EDGE('',*,*,#40877,.F.);
#57927=ORIENTED_EDGE('',*,*,#40675,.T.);
#57928=ORIENTED_EDGE('',*,*,#40878,.F.);
#57929=ORIENTED_EDGE('',*,*,#40879,.F.);
#57930=ORIENTED_EDGE('',*,*,#40880,.F.);
#57931=ORIENTED_EDGE('',*,*,#40881,.F.);
#57932=ORIENTED_EDGE('',*,*,#40876,.F.);
#57933=ORIENTED_EDGE('',*,*,#40881,.T.);
#57934=ORIENTED_EDGE('',*,*,#40882,.F.);
#57935=ORIENTED_EDGE('',*,*,#40676,.T.);
#57936=ORIENTED_EDGE('',*,*,#40877,.T.);
#57937=ORIENTED_EDGE('',*,*,#40883,.T.);
#57938=ORIENTED_EDGE('',*,*,#40884,.F.);
#57939=ORIENTED_EDGE('',*,*,#40678,.T.);
#57940=ORIENTED_EDGE('',*,*,#40885,.F.);
#57941=ORIENTED_EDGE('',*,*,#40886,.F.);
#57942=ORIENTED_EDGE('',*,*,#40887,.F.);
#57943=ORIENTED_EDGE('',*,*,#40888,.F.);
#57944=ORIENTED_EDGE('',*,*,#40883,.F.);
#57945=ORIENTED_EDGE('',*,*,#40888,.T.);
#57946=ORIENTED_EDGE('',*,*,#40889,.F.);
#57947=ORIENTED_EDGE('',*,*,#40679,.T.);
#57948=ORIENTED_EDGE('',*,*,#40884,.T.);
#57949=ORIENTED_EDGE('',*,*,#40890,.T.);
#57950=ORIENTED_EDGE('',*,*,#40891,.F.);
#57951=ORIENTED_EDGE('',*,*,#40681,.T.);
#57952=ORIENTED_EDGE('',*,*,#40892,.F.);
#57953=ORIENTED_EDGE('',*,*,#40893,.F.);
#57954=ORIENTED_EDGE('',*,*,#40894,.F.);
#57955=ORIENTED_EDGE('',*,*,#40895,.F.);
#57956=ORIENTED_EDGE('',*,*,#40890,.F.);
#57957=ORIENTED_EDGE('',*,*,#40895,.T.);
#57958=ORIENTED_EDGE('',*,*,#40896,.F.);
#57959=ORIENTED_EDGE('',*,*,#40682,.T.);
#57960=ORIENTED_EDGE('',*,*,#40891,.T.);
#57961=ORIENTED_EDGE('',*,*,#40897,.T.);
#57962=ORIENTED_EDGE('',*,*,#40898,.F.);
#57963=ORIENTED_EDGE('',*,*,#40684,.T.);
#57964=ORIENTED_EDGE('',*,*,#40899,.F.);
#57965=ORIENTED_EDGE('',*,*,#40900,.F.);
#57966=ORIENTED_EDGE('',*,*,#40901,.F.);
#57967=ORIENTED_EDGE('',*,*,#40902,.F.);
#57968=ORIENTED_EDGE('',*,*,#40897,.F.);
#57969=ORIENTED_EDGE('',*,*,#40902,.T.);
#57970=ORIENTED_EDGE('',*,*,#40903,.F.);
#57971=ORIENTED_EDGE('',*,*,#40685,.T.);
#57972=ORIENTED_EDGE('',*,*,#40898,.T.);
#57973=ORIENTED_EDGE('',*,*,#40904,.T.);
#57974=ORIENTED_EDGE('',*,*,#40905,.F.);
#57975=ORIENTED_EDGE('',*,*,#40687,.T.);
#57976=ORIENTED_EDGE('',*,*,#40906,.F.);
#57977=ORIENTED_EDGE('',*,*,#40907,.F.);
#57978=ORIENTED_EDGE('',*,*,#40908,.F.);
#57979=ORIENTED_EDGE('',*,*,#40909,.F.);
#57980=ORIENTED_EDGE('',*,*,#40904,.F.);
#57981=ORIENTED_EDGE('',*,*,#40909,.T.);
#57982=ORIENTED_EDGE('',*,*,#40910,.F.);
#57983=ORIENTED_EDGE('',*,*,#40688,.T.);
#57984=ORIENTED_EDGE('',*,*,#40905,.T.);
#57985=ORIENTED_EDGE('',*,*,#40911,.T.);
#57986=ORIENTED_EDGE('',*,*,#40912,.F.);
#57987=ORIENTED_EDGE('',*,*,#40690,.T.);
#57988=ORIENTED_EDGE('',*,*,#40913,.F.);
#57989=ORIENTED_EDGE('',*,*,#40914,.F.);
#57990=ORIENTED_EDGE('',*,*,#40915,.F.);
#57991=ORIENTED_EDGE('',*,*,#40916,.F.);
#57992=ORIENTED_EDGE('',*,*,#40911,.F.);
#57993=ORIENTED_EDGE('',*,*,#40916,.T.);
#57994=ORIENTED_EDGE('',*,*,#40917,.F.);
#57995=ORIENTED_EDGE('',*,*,#40691,.T.);
#57996=ORIENTED_EDGE('',*,*,#40912,.T.);
#57997=ORIENTED_EDGE('',*,*,#40918,.T.);
#57998=ORIENTED_EDGE('',*,*,#40919,.F.);
#57999=ORIENTED_EDGE('',*,*,#40693,.T.);
#58000=ORIENTED_EDGE('',*,*,#40920,.F.);
#58001=ORIENTED_EDGE('',*,*,#40921,.F.);
#58002=ORIENTED_EDGE('',*,*,#40922,.F.);
#58003=ORIENTED_EDGE('',*,*,#40923,.F.);
#58004=ORIENTED_EDGE('',*,*,#40918,.F.);
#58005=ORIENTED_EDGE('',*,*,#40923,.T.);
#58006=ORIENTED_EDGE('',*,*,#40924,.F.);
#58007=ORIENTED_EDGE('',*,*,#40694,.T.);
#58008=ORIENTED_EDGE('',*,*,#40919,.T.);
#58009=ORIENTED_EDGE('',*,*,#34385,.T.);
#58010=ORIENTED_EDGE('',*,*,#40925,.F.);
#58011=ORIENTED_EDGE('',*,*,#40696,.T.);
#58012=ORIENTED_EDGE('',*,*,#40926,.F.);
#58013=ORIENTED_EDGE('',*,*,#34388,.T.);
#58014=ORIENTED_EDGE('',*,*,#40927,.F.);
#58015=ORIENTED_EDGE('',*,*,#40697,.T.);
#58016=ORIENTED_EDGE('',*,*,#40925,.T.);
#58017=ORIENTED_EDGE('',*,*,#40928,.T.);
#58018=ORIENTED_EDGE('',*,*,#40929,.F.);
#58019=ORIENTED_EDGE('',*,*,#40699,.T.);
#58020=ORIENTED_EDGE('',*,*,#40930,.F.);
#58021=ORIENTED_EDGE('',*,*,#40931,.F.);
#58022=ORIENTED_EDGE('',*,*,#40932,.F.);
#58023=ORIENTED_EDGE('',*,*,#40933,.F.);
#58024=ORIENTED_EDGE('',*,*,#40928,.F.);
#58025=ORIENTED_EDGE('',*,*,#40933,.T.);
#58026=ORIENTED_EDGE('',*,*,#40934,.F.);
#58027=ORIENTED_EDGE('',*,*,#40700,.T.);
#58028=ORIENTED_EDGE('',*,*,#40929,.T.);
#58029=ORIENTED_EDGE('',*,*,#40935,.T.);
#58030=ORIENTED_EDGE('',*,*,#40936,.F.);
#58031=ORIENTED_EDGE('',*,*,#40702,.T.);
#58032=ORIENTED_EDGE('',*,*,#40937,.F.);
#58033=ORIENTED_EDGE('',*,*,#40938,.F.);
#58034=ORIENTED_EDGE('',*,*,#40939,.F.);
#58035=ORIENTED_EDGE('',*,*,#40940,.F.);
#58036=ORIENTED_EDGE('',*,*,#40935,.F.);
#58037=ORIENTED_EDGE('',*,*,#40940,.T.);
#58038=ORIENTED_EDGE('',*,*,#40941,.F.);
#58039=ORIENTED_EDGE('',*,*,#40703,.T.);
#58040=ORIENTED_EDGE('',*,*,#40936,.T.);
#58041=ORIENTED_EDGE('',*,*,#40942,.T.);
#58042=ORIENTED_EDGE('',*,*,#40943,.F.);
#58043=ORIENTED_EDGE('',*,*,#40705,.T.);
#58044=ORIENTED_EDGE('',*,*,#40944,.F.);
#58045=ORIENTED_EDGE('',*,*,#40945,.F.);
#58046=ORIENTED_EDGE('',*,*,#40946,.F.);
#58047=ORIENTED_EDGE('',*,*,#40947,.F.);
#58048=ORIENTED_EDGE('',*,*,#40942,.F.);
#58049=ORIENTED_EDGE('',*,*,#40947,.T.);
#58050=ORIENTED_EDGE('',*,*,#40948,.F.);
#58051=ORIENTED_EDGE('',*,*,#40706,.T.);
#58052=ORIENTED_EDGE('',*,*,#40943,.T.);
#58053=ORIENTED_EDGE('',*,*,#40949,.T.);
#58054=ORIENTED_EDGE('',*,*,#40950,.F.);
#58055=ORIENTED_EDGE('',*,*,#40708,.T.);
#58056=ORIENTED_EDGE('',*,*,#40951,.F.);
#58057=ORIENTED_EDGE('',*,*,#40952,.F.);
#58058=ORIENTED_EDGE('',*,*,#40953,.F.);
#58059=ORIENTED_EDGE('',*,*,#40954,.F.);
#58060=ORIENTED_EDGE('',*,*,#40949,.F.);
#58061=ORIENTED_EDGE('',*,*,#40954,.T.);
#58062=ORIENTED_EDGE('',*,*,#40955,.F.);
#58063=ORIENTED_EDGE('',*,*,#40709,.T.);
#58064=ORIENTED_EDGE('',*,*,#40950,.T.);
#58065=ORIENTED_EDGE('',*,*,#40956,.T.);
#58066=ORIENTED_EDGE('',*,*,#40957,.F.);
#58067=ORIENTED_EDGE('',*,*,#40711,.T.);
#58068=ORIENTED_EDGE('',*,*,#40958,.F.);
#58069=ORIENTED_EDGE('',*,*,#40959,.T.);
#58070=ORIENTED_EDGE('',*,*,#40960,.F.);
#58071=ORIENTED_EDGE('',*,*,#40712,.T.);
#58072=ORIENTED_EDGE('',*,*,#40957,.T.);
#58073=ORIENTED_EDGE('',*,*,#40961,.F.);
#58074=ORIENTED_EDGE('',*,*,#40962,.F.);
#58075=ORIENTED_EDGE('',*,*,#40959,.F.);
#58076=ORIENTED_EDGE('',*,*,#40956,.F.);
#58077=ORIENTED_EDGE('',*,*,#40714,.T.);
#58078=ORIENTED_EDGE('',*,*,#40963,.F.);
#58079=ORIENTED_EDGE('',*,*,#40964,.T.);
#58080=ORIENTED_EDGE('',*,*,#40965,.F.);
#58081=ORIENTED_EDGE('',*,*,#40966,.F.);
#58082=ORIENTED_EDGE('',*,*,#40964,.F.);
#58083=ORIENTED_EDGE('',*,*,#40967,.F.);
#58084=ORIENTED_EDGE('',*,*,#40968,.F.);
#58085=ORIENTED_EDGE('',*,*,#40715,.T.);
#58086=ORIENTED_EDGE('',*,*,#40965,.T.);
#58087=ORIENTED_EDGE('',*,*,#40966,.T.);
#58088=ORIENTED_EDGE('',*,*,#40969,.F.);
#58089=ORIENTED_EDGE('',*,*,#40970,.T.);
#58090=ORIENTED_EDGE('',*,*,#40971,.F.);
#58091=ORIENTED_EDGE('',*,*,#40717,.T.);
#58092=ORIENTED_EDGE('',*,*,#40972,.F.);
#58093=ORIENTED_EDGE('',*,*,#40973,.F.);
#58094=ORIENTED_EDGE('',*,*,#40974,.F.);
#58095=ORIENTED_EDGE('',*,*,#40975,.F.);
#58096=ORIENTED_EDGE('',*,*,#40970,.F.);
#58097=ORIENTED_EDGE('',*,*,#40975,.T.);
#58098=ORIENTED_EDGE('',*,*,#40976,.F.);
#58099=ORIENTED_EDGE('',*,*,#40718,.T.);
#58100=ORIENTED_EDGE('',*,*,#40971,.T.);
#58101=ORIENTED_EDGE('',*,*,#40977,.T.);
#58102=ORIENTED_EDGE('',*,*,#40978,.F.);
#58103=ORIENTED_EDGE('',*,*,#40720,.T.);
#58104=ORIENTED_EDGE('',*,*,#40979,.F.);
#58105=ORIENTED_EDGE('',*,*,#40980,.F.);
#58106=ORIENTED_EDGE('',*,*,#40981,.F.);
#58107=ORIENTED_EDGE('',*,*,#40982,.F.);
#58108=ORIENTED_EDGE('',*,*,#40977,.F.);
#58109=ORIENTED_EDGE('',*,*,#40982,.T.);
#58110=ORIENTED_EDGE('',*,*,#40983,.F.);
#58111=ORIENTED_EDGE('',*,*,#40721,.T.);
#58112=ORIENTED_EDGE('',*,*,#40978,.T.);
#58113=ORIENTED_EDGE('',*,*,#40984,.T.);
#58114=ORIENTED_EDGE('',*,*,#40985,.F.);
#58115=ORIENTED_EDGE('',*,*,#40723,.T.);
#58116=ORIENTED_EDGE('',*,*,#40986,.F.);
#58117=ORIENTED_EDGE('',*,*,#40987,.F.);
#58118=ORIENTED_EDGE('',*,*,#40988,.F.);
#58119=ORIENTED_EDGE('',*,*,#40989,.F.);
#58120=ORIENTED_EDGE('',*,*,#40984,.F.);
#58121=ORIENTED_EDGE('',*,*,#40989,.T.);
#58122=ORIENTED_EDGE('',*,*,#40990,.F.);
#58123=ORIENTED_EDGE('',*,*,#40724,.T.);
#58124=ORIENTED_EDGE('',*,*,#40985,.T.);
#58125=ORIENTED_EDGE('',*,*,#40991,.T.);
#58126=ORIENTED_EDGE('',*,*,#40992,.F.);
#58127=ORIENTED_EDGE('',*,*,#40726,.T.);
#58128=ORIENTED_EDGE('',*,*,#40993,.F.);
#58129=ORIENTED_EDGE('',*,*,#40994,.F.);
#58130=ORIENTED_EDGE('',*,*,#40995,.F.);
#58131=ORIENTED_EDGE('',*,*,#40996,.F.);
#58132=ORIENTED_EDGE('',*,*,#40991,.F.);
#58133=ORIENTED_EDGE('',*,*,#40996,.T.);
#58134=ORIENTED_EDGE('',*,*,#40997,.F.);
#58135=ORIENTED_EDGE('',*,*,#40727,.T.);
#58136=ORIENTED_EDGE('',*,*,#40992,.T.);
#58137=ORIENTED_EDGE('',*,*,#40998,.T.);
#58138=ORIENTED_EDGE('',*,*,#40999,.F.);
#58139=ORIENTED_EDGE('',*,*,#40729,.T.);
#58140=ORIENTED_EDGE('',*,*,#41000,.F.);
#58141=ORIENTED_EDGE('',*,*,#41001,.F.);
#58142=ORIENTED_EDGE('',*,*,#41002,.F.);
#58143=ORIENTED_EDGE('',*,*,#41003,.F.);
#58144=ORIENTED_EDGE('',*,*,#40998,.F.);
#58145=ORIENTED_EDGE('',*,*,#41003,.T.);
#58146=ORIENTED_EDGE('',*,*,#41004,.F.);
#58147=ORIENTED_EDGE('',*,*,#40730,.T.);
#58148=ORIENTED_EDGE('',*,*,#40999,.T.);
#58149=ORIENTED_EDGE('',*,*,#41005,.T.);
#58150=ORIENTED_EDGE('',*,*,#41006,.F.);
#58151=ORIENTED_EDGE('',*,*,#40732,.T.);
#58152=ORIENTED_EDGE('',*,*,#41007,.F.);
#58153=ORIENTED_EDGE('',*,*,#41008,.F.);
#58154=ORIENTED_EDGE('',*,*,#41009,.F.);
#58155=ORIENTED_EDGE('',*,*,#41010,.F.);
#58156=ORIENTED_EDGE('',*,*,#41005,.F.);
#58157=ORIENTED_EDGE('',*,*,#41010,.T.);
#58158=ORIENTED_EDGE('',*,*,#41011,.F.);
#58159=ORIENTED_EDGE('',*,*,#40733,.T.);
#58160=ORIENTED_EDGE('',*,*,#41006,.T.);
#58161=ORIENTED_EDGE('',*,*,#41012,.T.);
#58162=ORIENTED_EDGE('',*,*,#41013,.F.);
#58163=ORIENTED_EDGE('',*,*,#40735,.T.);
#58164=ORIENTED_EDGE('',*,*,#41014,.F.);
#58165=ORIENTED_EDGE('',*,*,#41015,.F.);
#58166=ORIENTED_EDGE('',*,*,#41016,.F.);
#58167=ORIENTED_EDGE('',*,*,#41017,.F.);
#58168=ORIENTED_EDGE('',*,*,#41012,.F.);
#58169=ORIENTED_EDGE('',*,*,#41017,.T.);
#58170=ORIENTED_EDGE('',*,*,#41018,.F.);
#58171=ORIENTED_EDGE('',*,*,#40736,.T.);
#58172=ORIENTED_EDGE('',*,*,#41013,.T.);
#58173=ORIENTED_EDGE('',*,*,#41019,.T.);
#58174=ORIENTED_EDGE('',*,*,#41020,.F.);
#58175=ORIENTED_EDGE('',*,*,#40738,.T.);
#58176=ORIENTED_EDGE('',*,*,#41021,.F.);
#58177=ORIENTED_EDGE('',*,*,#41022,.F.);
#58178=ORIENTED_EDGE('',*,*,#41023,.F.);
#58179=ORIENTED_EDGE('',*,*,#41024,.F.);
#58180=ORIENTED_EDGE('',*,*,#41019,.F.);
#58181=ORIENTED_EDGE('',*,*,#41024,.T.);
#58182=ORIENTED_EDGE('',*,*,#41025,.F.);
#58183=ORIENTED_EDGE('',*,*,#40739,.T.);
#58184=ORIENTED_EDGE('',*,*,#41020,.T.);
#58185=ORIENTED_EDGE('',*,*,#40741,.T.);
#58186=ORIENTED_EDGE('',*,*,#41026,.F.);
#58187=ORIENTED_EDGE('',*,*,#41027,.T.);
#58188=ORIENTED_EDGE('',*,*,#41028,.F.);
#58189=ORIENTED_EDGE('',*,*,#40742,.T.);
#58190=ORIENTED_EDGE('',*,*,#41028,.T.);
#58191=ORIENTED_EDGE('',*,*,#41029,.T.);
#58192=ORIENTED_EDGE('',*,*,#41030,.F.);
#58193=ORIENTED_EDGE('',*,*,#41029,.F.);
#58194=ORIENTED_EDGE('',*,*,#41027,.F.);
#58195=ORIENTED_EDGE('',*,*,#41031,.F.);
#58196=ORIENTED_EDGE('',*,*,#41032,.F.);
#58197=ORIENTED_EDGE('',*,*,#40744,.T.);
#58198=ORIENTED_EDGE('',*,*,#41033,.F.);
#58199=ORIENTED_EDGE('',*,*,#41034,.T.);
#58200=ORIENTED_EDGE('',*,*,#41035,.F.);
#58201=ORIENTED_EDGE('',*,*,#40745,.T.);
#58202=ORIENTED_EDGE('',*,*,#41035,.T.);
#58203=ORIENTED_EDGE('',*,*,#41036,.T.);
#58204=ORIENTED_EDGE('',*,*,#41037,.F.);
#58205=ORIENTED_EDGE('',*,*,#41036,.F.);
#58206=ORIENTED_EDGE('',*,*,#41034,.F.);
#58207=ORIENTED_EDGE('',*,*,#41038,.F.);
#58208=ORIENTED_EDGE('',*,*,#41039,.F.);
#58209=ORIENTED_EDGE('',*,*,#40747,.T.);
#58210=ORIENTED_EDGE('',*,*,#41040,.F.);
#58211=ORIENTED_EDGE('',*,*,#41041,.T.);
#58212=ORIENTED_EDGE('',*,*,#41042,.F.);
#58213=ORIENTED_EDGE('',*,*,#40748,.T.);
#58214=ORIENTED_EDGE('',*,*,#41042,.T.);
#58215=ORIENTED_EDGE('',*,*,#41043,.T.);
#58216=ORIENTED_EDGE('',*,*,#41044,.F.);
#58217=ORIENTED_EDGE('',*,*,#41043,.F.);
#58218=ORIENTED_EDGE('',*,*,#41041,.F.);
#58219=ORIENTED_EDGE('',*,*,#41045,.F.);
#58220=ORIENTED_EDGE('',*,*,#41046,.F.);
#58221=ORIENTED_EDGE('',*,*,#40750,.T.);
#58222=ORIENTED_EDGE('',*,*,#41047,.F.);
#58223=ORIENTED_EDGE('',*,*,#41048,.T.);
#58224=ORIENTED_EDGE('',*,*,#41049,.F.);
#58225=ORIENTED_EDGE('',*,*,#40751,.T.);
#58226=ORIENTED_EDGE('',*,*,#41049,.T.);
#58227=ORIENTED_EDGE('',*,*,#41050,.T.);
#58228=ORIENTED_EDGE('',*,*,#41051,.F.);
#58229=ORIENTED_EDGE('',*,*,#41050,.F.);
#58230=ORIENTED_EDGE('',*,*,#41048,.F.);
#58231=ORIENTED_EDGE('',*,*,#41052,.F.);
#58232=ORIENTED_EDGE('',*,*,#41053,.F.);
#58233=ORIENTED_EDGE('',*,*,#40753,.T.);
#58234=ORIENTED_EDGE('',*,*,#41054,.F.);
#58235=ORIENTED_EDGE('',*,*,#41055,.T.);
#58236=ORIENTED_EDGE('',*,*,#41056,.F.);
#58237=ORIENTED_EDGE('',*,*,#40754,.T.);
#58238=ORIENTED_EDGE('',*,*,#41056,.T.);
#58239=ORIENTED_EDGE('',*,*,#41057,.T.);
#58240=ORIENTED_EDGE('',*,*,#41058,.F.);
#58241=ORIENTED_EDGE('',*,*,#41057,.F.);
#58242=ORIENTED_EDGE('',*,*,#41055,.F.);
#58243=ORIENTED_EDGE('',*,*,#41059,.F.);
#58244=ORIENTED_EDGE('',*,*,#41060,.F.);
#58245=ORIENTED_EDGE('',*,*,#40756,.T.);
#58246=ORIENTED_EDGE('',*,*,#41061,.F.);
#58247=ORIENTED_EDGE('',*,*,#41062,.T.);
#58248=ORIENTED_EDGE('',*,*,#41063,.F.);
#58249=ORIENTED_EDGE('',*,*,#40757,.T.);
#58250=ORIENTED_EDGE('',*,*,#41063,.T.);
#58251=ORIENTED_EDGE('',*,*,#41064,.T.);
#58252=ORIENTED_EDGE('',*,*,#41065,.F.);
#58253=ORIENTED_EDGE('',*,*,#41064,.F.);
#58254=ORIENTED_EDGE('',*,*,#41062,.F.);
#58255=ORIENTED_EDGE('',*,*,#41066,.F.);
#58256=ORIENTED_EDGE('',*,*,#41067,.F.);
#58257=ORIENTED_EDGE('',*,*,#40759,.T.);
#58258=ORIENTED_EDGE('',*,*,#41068,.F.);
#58259=ORIENTED_EDGE('',*,*,#41069,.T.);
#58260=ORIENTED_EDGE('',*,*,#41070,.F.);
#58261=ORIENTED_EDGE('',*,*,#40760,.T.);
#58262=ORIENTED_EDGE('',*,*,#41070,.T.);
#58263=ORIENTED_EDGE('',*,*,#41071,.T.);
#58264=ORIENTED_EDGE('',*,*,#41072,.F.);
#58265=ORIENTED_EDGE('',*,*,#41071,.F.);
#58266=ORIENTED_EDGE('',*,*,#41069,.F.);
#58267=ORIENTED_EDGE('',*,*,#41073,.F.);
#58268=ORIENTED_EDGE('',*,*,#41074,.F.);
#58269=ORIENTED_EDGE('',*,*,#40762,.T.);
#58270=ORIENTED_EDGE('',*,*,#41075,.F.);
#58271=ORIENTED_EDGE('',*,*,#41076,.T.);
#58272=ORIENTED_EDGE('',*,*,#41077,.F.);
#58273=ORIENTED_EDGE('',*,*,#40763,.T.);
#58274=ORIENTED_EDGE('',*,*,#41077,.T.);
#58275=ORIENTED_EDGE('',*,*,#41078,.T.);
#58276=ORIENTED_EDGE('',*,*,#41079,.F.);
#58277=ORIENTED_EDGE('',*,*,#41078,.F.);
#58278=ORIENTED_EDGE('',*,*,#41076,.F.);
#58279=ORIENTED_EDGE('',*,*,#41080,.F.);
#58280=ORIENTED_EDGE('',*,*,#41081,.F.);
#58281=ORIENTED_EDGE('',*,*,#40765,.T.);
#58282=ORIENTED_EDGE('',*,*,#41082,.F.);
#58283=ORIENTED_EDGE('',*,*,#41083,.T.);
#58284=ORIENTED_EDGE('',*,*,#41084,.F.);
#58285=ORIENTED_EDGE('',*,*,#40766,.T.);
#58286=ORIENTED_EDGE('',*,*,#41084,.T.);
#58287=ORIENTED_EDGE('',*,*,#41085,.T.);
#58288=ORIENTED_EDGE('',*,*,#41086,.F.);
#58289=ORIENTED_EDGE('',*,*,#41085,.F.);
#58290=ORIENTED_EDGE('',*,*,#41083,.F.);
#58291=ORIENTED_EDGE('',*,*,#41087,.F.);
#58292=ORIENTED_EDGE('',*,*,#41088,.F.);
#58293=ORIENTED_EDGE('',*,*,#40768,.T.);
#58294=ORIENTED_EDGE('',*,*,#41089,.F.);
#58295=ORIENTED_EDGE('',*,*,#41090,.T.);
#58296=ORIENTED_EDGE('',*,*,#41091,.F.);
#58297=ORIENTED_EDGE('',*,*,#40769,.T.);
#58298=ORIENTED_EDGE('',*,*,#41091,.T.);
#58299=ORIENTED_EDGE('',*,*,#41092,.T.);
#58300=ORIENTED_EDGE('',*,*,#41093,.F.);
#58301=ORIENTED_EDGE('',*,*,#41092,.F.);
#58302=ORIENTED_EDGE('',*,*,#41090,.F.);
#58303=ORIENTED_EDGE('',*,*,#41094,.F.);
#58304=ORIENTED_EDGE('',*,*,#41095,.F.);
#58305=ORIENTED_EDGE('',*,*,#40771,.T.);
#58306=ORIENTED_EDGE('',*,*,#41096,.F.);
#58307=ORIENTED_EDGE('',*,*,#41097,.T.);
#58308=ORIENTED_EDGE('',*,*,#41098,.F.);
#58309=ORIENTED_EDGE('',*,*,#40772,.T.);
#58310=ORIENTED_EDGE('',*,*,#41098,.T.);
#58311=ORIENTED_EDGE('',*,*,#41099,.T.);
#58312=ORIENTED_EDGE('',*,*,#41100,.F.);
#58313=ORIENTED_EDGE('',*,*,#41099,.F.);
#58314=ORIENTED_EDGE('',*,*,#41097,.F.);
#58315=ORIENTED_EDGE('',*,*,#41101,.F.);
#58316=ORIENTED_EDGE('',*,*,#41102,.F.);
#58317=ORIENTED_EDGE('',*,*,#40774,.T.);
#58318=ORIENTED_EDGE('',*,*,#41103,.F.);
#58319=ORIENTED_EDGE('',*,*,#41104,.T.);
#58320=ORIENTED_EDGE('',*,*,#41105,.F.);
#58321=ORIENTED_EDGE('',*,*,#40775,.T.);
#58322=ORIENTED_EDGE('',*,*,#41105,.T.);
#58323=ORIENTED_EDGE('',*,*,#41106,.T.);
#58324=ORIENTED_EDGE('',*,*,#41107,.F.);
#58325=ORIENTED_EDGE('',*,*,#41106,.F.);
#58326=ORIENTED_EDGE('',*,*,#41104,.F.);
#58327=ORIENTED_EDGE('',*,*,#41108,.F.);
#58328=ORIENTED_EDGE('',*,*,#41109,.F.);
#58329=ORIENTED_EDGE('',*,*,#40777,.T.);
#58330=ORIENTED_EDGE('',*,*,#41110,.F.);
#58331=ORIENTED_EDGE('',*,*,#41111,.T.);
#58332=ORIENTED_EDGE('',*,*,#41112,.F.);
#58333=ORIENTED_EDGE('',*,*,#40778,.T.);
#58334=ORIENTED_EDGE('',*,*,#41112,.T.);
#58335=ORIENTED_EDGE('',*,*,#41113,.T.);
#58336=ORIENTED_EDGE('',*,*,#41114,.F.);
#58337=ORIENTED_EDGE('',*,*,#41113,.F.);
#58338=ORIENTED_EDGE('',*,*,#41111,.F.);
#58339=ORIENTED_EDGE('',*,*,#41115,.F.);
#58340=ORIENTED_EDGE('',*,*,#41116,.F.);
#58341=ORIENTED_EDGE('',*,*,#40780,.T.);
#58342=ORIENTED_EDGE('',*,*,#41117,.F.);
#58343=ORIENTED_EDGE('',*,*,#41118,.T.);
#58344=ORIENTED_EDGE('',*,*,#41119,.F.);
#58345=ORIENTED_EDGE('',*,*,#40781,.T.);
#58346=ORIENTED_EDGE('',*,*,#41119,.T.);
#58347=ORIENTED_EDGE('',*,*,#41120,.T.);
#58348=ORIENTED_EDGE('',*,*,#41121,.F.);
#58349=ORIENTED_EDGE('',*,*,#41120,.F.);
#58350=ORIENTED_EDGE('',*,*,#41118,.F.);
#58351=ORIENTED_EDGE('',*,*,#41122,.F.);
#58352=ORIENTED_EDGE('',*,*,#41123,.F.);
#58353=ORIENTED_EDGE('',*,*,#40783,.T.);
#58354=ORIENTED_EDGE('',*,*,#41124,.F.);
#58355=ORIENTED_EDGE('',*,*,#41125,.T.);
#58356=ORIENTED_EDGE('',*,*,#41126,.F.);
#58357=ORIENTED_EDGE('',*,*,#40784,.T.);
#58358=ORIENTED_EDGE('',*,*,#41126,.T.);
#58359=ORIENTED_EDGE('',*,*,#41127,.T.);
#58360=ORIENTED_EDGE('',*,*,#41128,.F.);
#58361=ORIENTED_EDGE('',*,*,#41127,.F.);
#58362=ORIENTED_EDGE('',*,*,#41125,.F.);
#58363=ORIENTED_EDGE('',*,*,#41129,.F.);
#58364=ORIENTED_EDGE('',*,*,#41130,.F.);
#58365=ORIENTED_EDGE('',*,*,#40786,.T.);
#58366=ORIENTED_EDGE('',*,*,#41131,.F.);
#58367=ORIENTED_EDGE('',*,*,#41132,.T.);
#58368=ORIENTED_EDGE('',*,*,#41133,.F.);
#58369=ORIENTED_EDGE('',*,*,#40787,.T.);
#58370=ORIENTED_EDGE('',*,*,#41133,.T.);
#58371=ORIENTED_EDGE('',*,*,#41134,.T.);
#58372=ORIENTED_EDGE('',*,*,#41135,.F.);
#58373=ORIENTED_EDGE('',*,*,#41134,.F.);
#58374=ORIENTED_EDGE('',*,*,#41132,.F.);
#58375=ORIENTED_EDGE('',*,*,#41136,.F.);
#58376=ORIENTED_EDGE('',*,*,#41137,.F.);
#58377=ORIENTED_EDGE('',*,*,#40789,.T.);
#58378=ORIENTED_EDGE('',*,*,#41138,.F.);
#58379=ORIENTED_EDGE('',*,*,#41139,.T.);
#58380=ORIENTED_EDGE('',*,*,#41140,.F.);
#58381=ORIENTED_EDGE('',*,*,#40790,.T.);
#58382=ORIENTED_EDGE('',*,*,#41140,.T.);
#58383=ORIENTED_EDGE('',*,*,#41141,.T.);
#58384=ORIENTED_EDGE('',*,*,#41142,.F.);
#58385=ORIENTED_EDGE('',*,*,#41141,.F.);
#58386=ORIENTED_EDGE('',*,*,#41139,.F.);
#58387=ORIENTED_EDGE('',*,*,#41143,.F.);
#58388=ORIENTED_EDGE('',*,*,#41144,.F.);
#58389=ORIENTED_EDGE('',*,*,#40792,.T.);
#58390=ORIENTED_EDGE('',*,*,#41145,.F.);
#58391=ORIENTED_EDGE('',*,*,#41146,.T.);
#58392=ORIENTED_EDGE('',*,*,#41147,.F.);
#58393=ORIENTED_EDGE('',*,*,#40793,.T.);
#58394=ORIENTED_EDGE('',*,*,#41147,.T.);
#58395=ORIENTED_EDGE('',*,*,#41148,.T.);
#58396=ORIENTED_EDGE('',*,*,#41149,.F.);
#58397=ORIENTED_EDGE('',*,*,#41148,.F.);
#58398=ORIENTED_EDGE('',*,*,#41146,.F.);
#58399=ORIENTED_EDGE('',*,*,#41150,.F.);
#58400=ORIENTED_EDGE('',*,*,#41151,.F.);
#58401=ORIENTED_EDGE('',*,*,#40795,.T.);
#58402=ORIENTED_EDGE('',*,*,#41152,.F.);
#58403=ORIENTED_EDGE('',*,*,#41153,.T.);
#58404=ORIENTED_EDGE('',*,*,#41154,.F.);
#58405=ORIENTED_EDGE('',*,*,#40796,.T.);
#58406=ORIENTED_EDGE('',*,*,#41154,.T.);
#58407=ORIENTED_EDGE('',*,*,#41155,.T.);
#58408=ORIENTED_EDGE('',*,*,#41156,.F.);
#58409=ORIENTED_EDGE('',*,*,#41155,.F.);
#58410=ORIENTED_EDGE('',*,*,#41153,.F.);
#58411=ORIENTED_EDGE('',*,*,#41157,.F.);
#58412=ORIENTED_EDGE('',*,*,#41158,.F.);
#58413=ORIENTED_EDGE('',*,*,#40798,.T.);
#58414=ORIENTED_EDGE('',*,*,#41159,.F.);
#58415=ORIENTED_EDGE('',*,*,#41160,.T.);
#58416=ORIENTED_EDGE('',*,*,#41161,.F.);
#58417=ORIENTED_EDGE('',*,*,#40799,.T.);
#58418=ORIENTED_EDGE('',*,*,#41161,.T.);
#58419=ORIENTED_EDGE('',*,*,#41162,.T.);
#58420=ORIENTED_EDGE('',*,*,#41163,.F.);
#58421=ORIENTED_EDGE('',*,*,#41162,.F.);
#58422=ORIENTED_EDGE('',*,*,#41160,.F.);
#58423=ORIENTED_EDGE('',*,*,#41164,.F.);
#58424=ORIENTED_EDGE('',*,*,#41165,.F.);
#58425=ORIENTED_EDGE('',*,*,#40801,.T.);
#58426=ORIENTED_EDGE('',*,*,#41166,.F.);
#58427=ORIENTED_EDGE('',*,*,#41167,.T.);
#58428=ORIENTED_EDGE('',*,*,#41168,.F.);
#58429=ORIENTED_EDGE('',*,*,#40802,.T.);
#58430=ORIENTED_EDGE('',*,*,#41168,.T.);
#58431=ORIENTED_EDGE('',*,*,#41169,.T.);
#58432=ORIENTED_EDGE('',*,*,#41170,.F.);
#58433=ORIENTED_EDGE('',*,*,#41169,.F.);
#58434=ORIENTED_EDGE('',*,*,#41167,.F.);
#58435=ORIENTED_EDGE('',*,*,#41171,.F.);
#58436=ORIENTED_EDGE('',*,*,#41172,.F.);
#58437=ORIENTED_EDGE('',*,*,#40804,.T.);
#58438=ORIENTED_EDGE('',*,*,#41173,.F.);
#58439=ORIENTED_EDGE('',*,*,#34384,.T.);
#58440=ORIENTED_EDGE('',*,*,#41174,.F.);
#58441=ORIENTED_EDGE('',*,*,#40805,.T.);
#58442=ORIENTED_EDGE('',*,*,#41174,.T.);
#58443=ORIENTED_EDGE('',*,*,#34383,.T.);
#58444=ORIENTED_EDGE('',*,*,#41175,.F.);
#58445=ORIENTED_EDGE('',*,*,#40807,.T.);
#58446=ORIENTED_EDGE('',*,*,#41176,.F.);
#58447=ORIENTED_EDGE('',*,*,#41177,.T.);
#58448=ORIENTED_EDGE('',*,*,#41178,.F.);
#58449=ORIENTED_EDGE('',*,*,#40808,.T.);
#58450=ORIENTED_EDGE('',*,*,#41178,.T.);
#58451=ORIENTED_EDGE('',*,*,#41179,.T.);
#58452=ORIENTED_EDGE('',*,*,#41180,.F.);
#58453=ORIENTED_EDGE('',*,*,#41179,.F.);
#58454=ORIENTED_EDGE('',*,*,#41177,.F.);
#58455=ORIENTED_EDGE('',*,*,#41181,.F.);
#58456=ORIENTED_EDGE('',*,*,#41182,.F.);
#58457=ORIENTED_EDGE('',*,*,#40810,.T.);
#58458=ORIENTED_EDGE('',*,*,#41183,.F.);
#58459=ORIENTED_EDGE('',*,*,#41184,.T.);
#58460=ORIENTED_EDGE('',*,*,#41185,.F.);
#58461=ORIENTED_EDGE('',*,*,#40811,.T.);
#58462=ORIENTED_EDGE('',*,*,#41185,.T.);
#58463=ORIENTED_EDGE('',*,*,#41186,.T.);
#58464=ORIENTED_EDGE('',*,*,#41187,.F.);
#58465=ORIENTED_EDGE('',*,*,#41186,.F.);
#58466=ORIENTED_EDGE('',*,*,#41184,.F.);
#58467=ORIENTED_EDGE('',*,*,#41188,.F.);
#58468=ORIENTED_EDGE('',*,*,#41189,.F.);
#58469=ORIENTED_EDGE('',*,*,#40813,.T.);
#58470=ORIENTED_EDGE('',*,*,#41190,.F.);
#58471=ORIENTED_EDGE('',*,*,#41191,.T.);
#58472=ORIENTED_EDGE('',*,*,#41192,.F.);
#58473=ORIENTED_EDGE('',*,*,#40814,.T.);
#58474=ORIENTED_EDGE('',*,*,#41192,.T.);
#58475=ORIENTED_EDGE('',*,*,#41193,.T.);
#58476=ORIENTED_EDGE('',*,*,#41194,.F.);
#58477=ORIENTED_EDGE('',*,*,#41193,.F.);
#58478=ORIENTED_EDGE('',*,*,#41191,.F.);
#58479=ORIENTED_EDGE('',*,*,#41195,.F.);
#58480=ORIENTED_EDGE('',*,*,#41196,.F.);
#58481=ORIENTED_EDGE('',*,*,#40816,.T.);
#58482=ORIENTED_EDGE('',*,*,#41197,.F.);
#58483=ORIENTED_EDGE('',*,*,#41198,.T.);
#58484=ORIENTED_EDGE('',*,*,#41199,.F.);
#58485=ORIENTED_EDGE('',*,*,#41200,.T.);
#58486=ORIENTED_EDGE('',*,*,#41201,.F.);
#58487=ORIENTED_EDGE('',*,*,#40817,.T.);
#58488=ORIENTED_EDGE('',*,*,#41199,.T.);
#58489=ORIENTED_EDGE('',*,*,#41202,.F.);
#58490=ORIENTED_EDGE('',*,*,#41203,.F.);
#58491=ORIENTED_EDGE('',*,*,#41200,.F.);
#58492=ORIENTED_EDGE('',*,*,#41198,.F.);
#58493=ORIENTED_EDGE('',*,*,#40819,.T.);
#58494=ORIENTED_EDGE('',*,*,#41204,.F.);
#58495=ORIENTED_EDGE('',*,*,#41205,.T.);
#58496=ORIENTED_EDGE('',*,*,#41206,.F.);
#58497=ORIENTED_EDGE('',*,*,#40820,.T.);
#58498=ORIENTED_EDGE('',*,*,#41206,.T.);
#58499=ORIENTED_EDGE('',*,*,#41207,.T.);
#58500=ORIENTED_EDGE('',*,*,#41208,.F.);
#58501=ORIENTED_EDGE('',*,*,#41207,.F.);
#58502=ORIENTED_EDGE('',*,*,#41205,.F.);
#58503=ORIENTED_EDGE('',*,*,#41209,.F.);
#58504=ORIENTED_EDGE('',*,*,#41210,.F.);
#58505=ORIENTED_EDGE('',*,*,#40822,.T.);
#58506=ORIENTED_EDGE('',*,*,#41211,.F.);
#58507=ORIENTED_EDGE('',*,*,#41212,.T.);
#58508=ORIENTED_EDGE('',*,*,#41213,.F.);
#58509=ORIENTED_EDGE('',*,*,#40823,.T.);
#58510=ORIENTED_EDGE('',*,*,#41213,.T.);
#58511=ORIENTED_EDGE('',*,*,#41214,.T.);
#58512=ORIENTED_EDGE('',*,*,#41215,.F.);
#58513=ORIENTED_EDGE('',*,*,#41214,.F.);
#58514=ORIENTED_EDGE('',*,*,#41212,.F.);
#58515=ORIENTED_EDGE('',*,*,#41216,.F.);
#58516=ORIENTED_EDGE('',*,*,#41217,.F.);
#58517=ORIENTED_EDGE('',*,*,#40825,.T.);
#58518=ORIENTED_EDGE('',*,*,#41218,.F.);
#58519=ORIENTED_EDGE('',*,*,#41219,.T.);
#58520=ORIENTED_EDGE('',*,*,#41220,.F.);
#58521=ORIENTED_EDGE('',*,*,#40826,.T.);
#58522=ORIENTED_EDGE('',*,*,#41220,.T.);
#58523=ORIENTED_EDGE('',*,*,#41221,.T.);
#58524=ORIENTED_EDGE('',*,*,#41222,.F.);
#58525=ORIENTED_EDGE('',*,*,#41221,.F.);
#58526=ORIENTED_EDGE('',*,*,#41219,.F.);
#58527=ORIENTED_EDGE('',*,*,#41223,.F.);
#58528=ORIENTED_EDGE('',*,*,#41224,.F.);
#58529=ORIENTED_EDGE('',*,*,#41225,.F.);
#58530=ORIENTED_EDGE('',*,*,#41226,.F.);
#58531=ORIENTED_EDGE('',*,*,#40830,.T.);
#58532=ORIENTED_EDGE('',*,*,#40829,.T.);
#58533=ORIENTED_EDGE('',*,*,#41227,.F.);
#58534=ORIENTED_EDGE('',*,*,#40833,.T.);
#58535=ORIENTED_EDGE('',*,*,#40831,.T.);
#58536=ORIENTED_EDGE('',*,*,#41226,.T.);
#58537=ORIENTED_EDGE('',*,*,#41228,.F.);
#58538=ORIENTED_EDGE('',*,*,#41229,.F.);
#58539=ORIENTED_EDGE('',*,*,#40837,.T.);
#58540=ORIENTED_EDGE('',*,*,#40836,.T.);
#58541=ORIENTED_EDGE('',*,*,#41230,.F.);
#58542=ORIENTED_EDGE('',*,*,#40840,.T.);
#58543=ORIENTED_EDGE('',*,*,#40838,.T.);
#58544=ORIENTED_EDGE('',*,*,#41229,.T.);
#58545=ORIENTED_EDGE('',*,*,#41231,.F.);
#58546=ORIENTED_EDGE('',*,*,#41232,.F.);
#58547=ORIENTED_EDGE('',*,*,#40844,.T.);
#58548=ORIENTED_EDGE('',*,*,#40843,.T.);
#58549=ORIENTED_EDGE('',*,*,#41233,.F.);
#58550=ORIENTED_EDGE('',*,*,#40847,.T.);
#58551=ORIENTED_EDGE('',*,*,#40845,.T.);
#58552=ORIENTED_EDGE('',*,*,#41232,.T.);
#58553=ORIENTED_EDGE('',*,*,#41234,.F.);
#58554=ORIENTED_EDGE('',*,*,#41235,.F.);
#58555=ORIENTED_EDGE('',*,*,#40851,.T.);
#58556=ORIENTED_EDGE('',*,*,#40850,.T.);
#58557=ORIENTED_EDGE('',*,*,#41236,.F.);
#58558=ORIENTED_EDGE('',*,*,#40854,.T.);
#58559=ORIENTED_EDGE('',*,*,#40852,.T.);
#58560=ORIENTED_EDGE('',*,*,#41235,.T.);
#58561=ORIENTED_EDGE('',*,*,#41237,.F.);
#58562=ORIENTED_EDGE('',*,*,#41238,.F.);
#58563=ORIENTED_EDGE('',*,*,#40858,.T.);
#58564=ORIENTED_EDGE('',*,*,#40857,.T.);
#58565=ORIENTED_EDGE('',*,*,#41239,.F.);
#58566=ORIENTED_EDGE('',*,*,#40861,.T.);
#58567=ORIENTED_EDGE('',*,*,#40859,.T.);
#58568=ORIENTED_EDGE('',*,*,#41238,.T.);
#58569=ORIENTED_EDGE('',*,*,#41240,.F.);
#58570=ORIENTED_EDGE('',*,*,#41241,.F.);
#58571=ORIENTED_EDGE('',*,*,#40865,.T.);
#58572=ORIENTED_EDGE('',*,*,#40864,.T.);
#58573=ORIENTED_EDGE('',*,*,#41242,.F.);
#58574=ORIENTED_EDGE('',*,*,#40868,.T.);
#58575=ORIENTED_EDGE('',*,*,#40866,.T.);
#58576=ORIENTED_EDGE('',*,*,#41241,.T.);
#58577=ORIENTED_EDGE('',*,*,#41243,.F.);
#58578=ORIENTED_EDGE('',*,*,#41244,.F.);
#58579=ORIENTED_EDGE('',*,*,#40872,.T.);
#58580=ORIENTED_EDGE('',*,*,#40871,.T.);
#58581=ORIENTED_EDGE('',*,*,#41245,.F.);
#58582=ORIENTED_EDGE('',*,*,#40875,.T.);
#58583=ORIENTED_EDGE('',*,*,#40873,.T.);
#58584=ORIENTED_EDGE('',*,*,#41244,.T.);
#58585=ORIENTED_EDGE('',*,*,#41246,.F.);
#58586=ORIENTED_EDGE('',*,*,#41247,.F.);
#58587=ORIENTED_EDGE('',*,*,#40879,.T.);
#58588=ORIENTED_EDGE('',*,*,#40878,.T.);
#58589=ORIENTED_EDGE('',*,*,#41248,.F.);
#58590=ORIENTED_EDGE('',*,*,#40882,.T.);
#58591=ORIENTED_EDGE('',*,*,#40880,.T.);
#58592=ORIENTED_EDGE('',*,*,#41247,.T.);
#58593=ORIENTED_EDGE('',*,*,#41249,.F.);
#58594=ORIENTED_EDGE('',*,*,#41250,.F.);
#58595=ORIENTED_EDGE('',*,*,#40886,.T.);
#58596=ORIENTED_EDGE('',*,*,#40885,.T.);
#58597=ORIENTED_EDGE('',*,*,#41251,.F.);
#58598=ORIENTED_EDGE('',*,*,#40889,.T.);
#58599=ORIENTED_EDGE('',*,*,#40887,.T.);
#58600=ORIENTED_EDGE('',*,*,#41250,.T.);
#58601=ORIENTED_EDGE('',*,*,#41252,.F.);
#58602=ORIENTED_EDGE('',*,*,#41253,.F.);
#58603=ORIENTED_EDGE('',*,*,#40893,.T.);
#58604=ORIENTED_EDGE('',*,*,#40892,.T.);
#58605=ORIENTED_EDGE('',*,*,#41254,.F.);
#58606=ORIENTED_EDGE('',*,*,#40896,.T.);
#58607=ORIENTED_EDGE('',*,*,#40894,.T.);
#58608=ORIENTED_EDGE('',*,*,#41253,.T.);
#58609=ORIENTED_EDGE('',*,*,#41255,.F.);
#58610=ORIENTED_EDGE('',*,*,#41256,.F.);
#58611=ORIENTED_EDGE('',*,*,#40900,.T.);
#58612=ORIENTED_EDGE('',*,*,#40899,.T.);
#58613=ORIENTED_EDGE('',*,*,#41257,.F.);
#58614=ORIENTED_EDGE('',*,*,#40903,.T.);
#58615=ORIENTED_EDGE('',*,*,#40901,.T.);
#58616=ORIENTED_EDGE('',*,*,#41256,.T.);
#58617=ORIENTED_EDGE('',*,*,#41258,.F.);
#58618=ORIENTED_EDGE('',*,*,#41259,.F.);
#58619=ORIENTED_EDGE('',*,*,#40907,.T.);
#58620=ORIENTED_EDGE('',*,*,#40906,.T.);
#58621=ORIENTED_EDGE('',*,*,#41260,.F.);
#58622=ORIENTED_EDGE('',*,*,#40910,.T.);
#58623=ORIENTED_EDGE('',*,*,#40908,.T.);
#58624=ORIENTED_EDGE('',*,*,#41259,.T.);
#58625=ORIENTED_EDGE('',*,*,#41261,.F.);
#58626=ORIENTED_EDGE('',*,*,#41262,.F.);
#58627=ORIENTED_EDGE('',*,*,#40914,.T.);
#58628=ORIENTED_EDGE('',*,*,#40913,.T.);
#58629=ORIENTED_EDGE('',*,*,#41263,.F.);
#58630=ORIENTED_EDGE('',*,*,#40917,.T.);
#58631=ORIENTED_EDGE('',*,*,#40915,.T.);
#58632=ORIENTED_EDGE('',*,*,#41262,.T.);
#58633=ORIENTED_EDGE('',*,*,#41264,.F.);
#58634=ORIENTED_EDGE('',*,*,#41265,.F.);
#58635=ORIENTED_EDGE('',*,*,#40921,.T.);
#58636=ORIENTED_EDGE('',*,*,#40920,.T.);
#58637=ORIENTED_EDGE('',*,*,#41266,.F.);
#58638=ORIENTED_EDGE('',*,*,#40924,.T.);
#58639=ORIENTED_EDGE('',*,*,#40922,.T.);
#58640=ORIENTED_EDGE('',*,*,#41265,.T.);
#58641=ORIENTED_EDGE('',*,*,#41267,.F.);
#58642=ORIENTED_EDGE('',*,*,#41268,.F.);
#58643=ORIENTED_EDGE('',*,*,#34386,.T.);
#58644=ORIENTED_EDGE('',*,*,#40926,.T.);
#58645=ORIENTED_EDGE('',*,*,#41269,.F.);
#58646=ORIENTED_EDGE('',*,*,#40927,.T.);
#58647=ORIENTED_EDGE('',*,*,#34387,.T.);
#58648=ORIENTED_EDGE('',*,*,#41268,.T.);
#58649=ORIENTED_EDGE('',*,*,#41270,.F.);
#58650=ORIENTED_EDGE('',*,*,#41271,.F.);
#58651=ORIENTED_EDGE('',*,*,#40931,.T.);
#58652=ORIENTED_EDGE('',*,*,#40930,.T.);
#58653=ORIENTED_EDGE('',*,*,#41272,.F.);
#58654=ORIENTED_EDGE('',*,*,#40934,.T.);
#58655=ORIENTED_EDGE('',*,*,#40932,.T.);
#58656=ORIENTED_EDGE('',*,*,#41271,.T.);
#58657=ORIENTED_EDGE('',*,*,#41273,.F.);
#58658=ORIENTED_EDGE('',*,*,#41274,.F.);
#58659=ORIENTED_EDGE('',*,*,#40938,.T.);
#58660=ORIENTED_EDGE('',*,*,#40937,.T.);
#58661=ORIENTED_EDGE('',*,*,#41275,.F.);
#58662=ORIENTED_EDGE('',*,*,#40941,.T.);
#58663=ORIENTED_EDGE('',*,*,#40939,.T.);
#58664=ORIENTED_EDGE('',*,*,#41274,.T.);
#58665=ORIENTED_EDGE('',*,*,#41276,.F.);
#58666=ORIENTED_EDGE('',*,*,#41277,.F.);
#58667=ORIENTED_EDGE('',*,*,#40945,.T.);
#58668=ORIENTED_EDGE('',*,*,#40944,.T.);
#58669=ORIENTED_EDGE('',*,*,#41278,.F.);
#58670=ORIENTED_EDGE('',*,*,#40948,.T.);
#58671=ORIENTED_EDGE('',*,*,#40946,.T.);
#58672=ORIENTED_EDGE('',*,*,#41277,.T.);
#58673=ORIENTED_EDGE('',*,*,#41279,.F.);
#58674=ORIENTED_EDGE('',*,*,#41280,.F.);
#58675=ORIENTED_EDGE('',*,*,#40952,.T.);
#58676=ORIENTED_EDGE('',*,*,#40951,.T.);
#58677=ORIENTED_EDGE('',*,*,#41281,.F.);
#58678=ORIENTED_EDGE('',*,*,#40955,.T.);
#58679=ORIENTED_EDGE('',*,*,#40953,.T.);
#58680=ORIENTED_EDGE('',*,*,#41280,.T.);
#58681=ORIENTED_EDGE('',*,*,#41282,.F.);
#58682=ORIENTED_EDGE('',*,*,#41283,.F.);
#58683=ORIENTED_EDGE('',*,*,#40961,.T.);
#58684=ORIENTED_EDGE('',*,*,#40958,.T.);
#58685=ORIENTED_EDGE('',*,*,#40962,.T.);
#58686=ORIENTED_EDGE('',*,*,#41283,.T.);
#58687=ORIENTED_EDGE('',*,*,#41284,.F.);
#58688=ORIENTED_EDGE('',*,*,#40960,.T.);
#58689=ORIENTED_EDGE('',*,*,#40967,.T.);
#58690=ORIENTED_EDGE('',*,*,#40963,.T.);
#58691=ORIENTED_EDGE('',*,*,#41285,.F.);
#58692=ORIENTED_EDGE('',*,*,#41286,.F.);
#58693=ORIENTED_EDGE('',*,*,#41287,.F.);
#58694=ORIENTED_EDGE('',*,*,#40969,.T.);
#58695=ORIENTED_EDGE('',*,*,#40968,.T.);
#58696=ORIENTED_EDGE('',*,*,#41286,.T.);
#58697=ORIENTED_EDGE('',*,*,#41288,.F.);
#58698=ORIENTED_EDGE('',*,*,#41289,.F.);
#58699=ORIENTED_EDGE('',*,*,#40973,.T.);
#58700=ORIENTED_EDGE('',*,*,#40972,.T.);
#58701=ORIENTED_EDGE('',*,*,#41290,.F.);
#58702=ORIENTED_EDGE('',*,*,#40976,.T.);
#58703=ORIENTED_EDGE('',*,*,#40974,.T.);
#58704=ORIENTED_EDGE('',*,*,#41289,.T.);
#58705=ORIENTED_EDGE('',*,*,#41291,.F.);
#58706=ORIENTED_EDGE('',*,*,#41292,.F.);
#58707=ORIENTED_EDGE('',*,*,#40980,.T.);
#58708=ORIENTED_EDGE('',*,*,#40979,.T.);
#58709=ORIENTED_EDGE('',*,*,#41293,.F.);
#58710=ORIENTED_EDGE('',*,*,#40983,.T.);
#58711=ORIENTED_EDGE('',*,*,#40981,.T.);
#58712=ORIENTED_EDGE('',*,*,#41292,.T.);
#58713=ORIENTED_EDGE('',*,*,#41294,.F.);
#58714=ORIENTED_EDGE('',*,*,#41295,.F.);
#58715=ORIENTED_EDGE('',*,*,#40987,.T.);
#58716=ORIENTED_EDGE('',*,*,#40986,.T.);
#58717=ORIENTED_EDGE('',*,*,#41296,.F.);
#58718=ORIENTED_EDGE('',*,*,#40990,.T.);
#58719=ORIENTED_EDGE('',*,*,#40988,.T.);
#58720=ORIENTED_EDGE('',*,*,#41295,.T.);
#58721=ORIENTED_EDGE('',*,*,#41297,.F.);
#58722=ORIENTED_EDGE('',*,*,#41298,.F.);
#58723=ORIENTED_EDGE('',*,*,#40994,.T.);
#58724=ORIENTED_EDGE('',*,*,#40993,.T.);
#58725=ORIENTED_EDGE('',*,*,#41299,.F.);
#58726=ORIENTED_EDGE('',*,*,#40997,.T.);
#58727=ORIENTED_EDGE('',*,*,#40995,.T.);
#58728=ORIENTED_EDGE('',*,*,#41298,.T.);
#58729=ORIENTED_EDGE('',*,*,#41300,.F.);
#58730=ORIENTED_EDGE('',*,*,#41301,.F.);
#58731=ORIENTED_EDGE('',*,*,#41001,.T.);
#58732=ORIENTED_EDGE('',*,*,#41000,.T.);
#58733=ORIENTED_EDGE('',*,*,#41302,.F.);
#58734=ORIENTED_EDGE('',*,*,#41004,.T.);
#58735=ORIENTED_EDGE('',*,*,#41002,.T.);
#58736=ORIENTED_EDGE('',*,*,#41301,.T.);
#58737=ORIENTED_EDGE('',*,*,#41303,.F.);
#58738=ORIENTED_EDGE('',*,*,#41304,.F.);
#58739=ORIENTED_EDGE('',*,*,#41008,.T.);
#58740=ORIENTED_EDGE('',*,*,#41007,.T.);
#58741=ORIENTED_EDGE('',*,*,#41305,.F.);
#58742=ORIENTED_EDGE('',*,*,#41011,.T.);
#58743=ORIENTED_EDGE('',*,*,#41009,.T.);
#58744=ORIENTED_EDGE('',*,*,#41304,.T.);
#58745=ORIENTED_EDGE('',*,*,#41306,.F.);
#58746=ORIENTED_EDGE('',*,*,#41307,.F.);
#58747=ORIENTED_EDGE('',*,*,#41015,.T.);
#58748=ORIENTED_EDGE('',*,*,#41014,.T.);
#58749=ORIENTED_EDGE('',*,*,#41308,.F.);
#58750=ORIENTED_EDGE('',*,*,#41018,.T.);
#58751=ORIENTED_EDGE('',*,*,#41016,.T.);
#58752=ORIENTED_EDGE('',*,*,#41307,.T.);
#58753=ORIENTED_EDGE('',*,*,#41309,.F.);
#58754=ORIENTED_EDGE('',*,*,#41310,.F.);
#58755=ORIENTED_EDGE('',*,*,#41022,.T.);
#58756=ORIENTED_EDGE('',*,*,#41021,.T.);
#58757=ORIENTED_EDGE('',*,*,#41311,.F.);
#58758=ORIENTED_EDGE('',*,*,#41025,.T.);
#58759=ORIENTED_EDGE('',*,*,#41023,.T.);
#58760=ORIENTED_EDGE('',*,*,#41310,.T.);
#58761=ORIENTED_EDGE('',*,*,#41031,.T.);
#58762=ORIENTED_EDGE('',*,*,#41026,.T.);
#58763=ORIENTED_EDGE('',*,*,#41312,.F.);
#58764=ORIENTED_EDGE('',*,*,#41313,.F.);
#58765=ORIENTED_EDGE('',*,*,#41032,.T.);
#58766=ORIENTED_EDGE('',*,*,#41313,.T.);
#58767=ORIENTED_EDGE('',*,*,#41314,.F.);
#58768=ORIENTED_EDGE('',*,*,#41030,.T.);
#58769=ORIENTED_EDGE('',*,*,#41038,.T.);
#58770=ORIENTED_EDGE('',*,*,#41033,.T.);
#58771=ORIENTED_EDGE('',*,*,#41315,.F.);
#58772=ORIENTED_EDGE('',*,*,#41316,.F.);
#58773=ORIENTED_EDGE('',*,*,#41039,.T.);
#58774=ORIENTED_EDGE('',*,*,#41316,.T.);
#58775=ORIENTED_EDGE('',*,*,#41317,.F.);
#58776=ORIENTED_EDGE('',*,*,#41037,.T.);
#58777=ORIENTED_EDGE('',*,*,#41045,.T.);
#58778=ORIENTED_EDGE('',*,*,#41040,.T.);
#58779=ORIENTED_EDGE('',*,*,#41318,.F.);
#58780=ORIENTED_EDGE('',*,*,#41319,.F.);
#58781=ORIENTED_EDGE('',*,*,#41046,.T.);
#58782=ORIENTED_EDGE('',*,*,#41319,.T.);
#58783=ORIENTED_EDGE('',*,*,#41320,.F.);
#58784=ORIENTED_EDGE('',*,*,#41044,.T.);
#58785=ORIENTED_EDGE('',*,*,#41052,.T.);
#58786=ORIENTED_EDGE('',*,*,#41047,.T.);
#58787=ORIENTED_EDGE('',*,*,#41321,.F.);
#58788=ORIENTED_EDGE('',*,*,#41322,.F.);
#58789=ORIENTED_EDGE('',*,*,#41053,.T.);
#58790=ORIENTED_EDGE('',*,*,#41322,.T.);
#58791=ORIENTED_EDGE('',*,*,#41323,.F.);
#58792=ORIENTED_EDGE('',*,*,#41051,.T.);
#58793=ORIENTED_EDGE('',*,*,#41059,.T.);
#58794=ORIENTED_EDGE('',*,*,#41054,.T.);
#58795=ORIENTED_EDGE('',*,*,#41324,.F.);
#58796=ORIENTED_EDGE('',*,*,#41325,.F.);
#58797=ORIENTED_EDGE('',*,*,#41060,.T.);
#58798=ORIENTED_EDGE('',*,*,#41325,.T.);
#58799=ORIENTED_EDGE('',*,*,#41326,.F.);
#58800=ORIENTED_EDGE('',*,*,#41058,.T.);
#58801=ORIENTED_EDGE('',*,*,#41066,.T.);
#58802=ORIENTED_EDGE('',*,*,#41061,.T.);
#58803=ORIENTED_EDGE('',*,*,#41327,.F.);
#58804=ORIENTED_EDGE('',*,*,#41328,.F.);
#58805=ORIENTED_EDGE('',*,*,#41067,.T.);
#58806=ORIENTED_EDGE('',*,*,#41328,.T.);
#58807=ORIENTED_EDGE('',*,*,#41329,.F.);
#58808=ORIENTED_EDGE('',*,*,#41065,.T.);
#58809=ORIENTED_EDGE('',*,*,#41073,.T.);
#58810=ORIENTED_EDGE('',*,*,#41068,.T.);
#58811=ORIENTED_EDGE('',*,*,#41330,.F.);
#58812=ORIENTED_EDGE('',*,*,#41331,.F.);
#58813=ORIENTED_EDGE('',*,*,#41074,.T.);
#58814=ORIENTED_EDGE('',*,*,#41331,.T.);
#58815=ORIENTED_EDGE('',*,*,#41332,.F.);
#58816=ORIENTED_EDGE('',*,*,#41072,.T.);
#58817=ORIENTED_EDGE('',*,*,#41080,.T.);
#58818=ORIENTED_EDGE('',*,*,#41075,.T.);
#58819=ORIENTED_EDGE('',*,*,#41333,.F.);
#58820=ORIENTED_EDGE('',*,*,#41334,.F.);
#58821=ORIENTED_EDGE('',*,*,#41081,.T.);
#58822=ORIENTED_EDGE('',*,*,#41334,.T.);
#58823=ORIENTED_EDGE('',*,*,#41335,.F.);
#58824=ORIENTED_EDGE('',*,*,#41079,.T.);
#58825=ORIENTED_EDGE('',*,*,#41087,.T.);
#58826=ORIENTED_EDGE('',*,*,#41082,.T.);
#58827=ORIENTED_EDGE('',*,*,#41336,.F.);
#58828=ORIENTED_EDGE('',*,*,#41337,.F.);
#58829=ORIENTED_EDGE('',*,*,#41088,.T.);
#58830=ORIENTED_EDGE('',*,*,#41337,.T.);
#58831=ORIENTED_EDGE('',*,*,#41338,.F.);
#58832=ORIENTED_EDGE('',*,*,#41086,.T.);
#58833=ORIENTED_EDGE('',*,*,#41094,.T.);
#58834=ORIENTED_EDGE('',*,*,#41089,.T.);
#58835=ORIENTED_EDGE('',*,*,#41339,.F.);
#58836=ORIENTED_EDGE('',*,*,#41340,.F.);
#58837=ORIENTED_EDGE('',*,*,#41095,.T.);
#58838=ORIENTED_EDGE('',*,*,#41340,.T.);
#58839=ORIENTED_EDGE('',*,*,#41341,.F.);
#58840=ORIENTED_EDGE('',*,*,#41093,.T.);
#58841=ORIENTED_EDGE('',*,*,#41101,.T.);
#58842=ORIENTED_EDGE('',*,*,#41096,.T.);
#58843=ORIENTED_EDGE('',*,*,#41342,.F.);
#58844=ORIENTED_EDGE('',*,*,#41343,.F.);
#58845=ORIENTED_EDGE('',*,*,#41102,.T.);
#58846=ORIENTED_EDGE('',*,*,#41343,.T.);
#58847=ORIENTED_EDGE('',*,*,#41344,.F.);
#58848=ORIENTED_EDGE('',*,*,#41100,.T.);
#58849=ORIENTED_EDGE('',*,*,#41108,.T.);
#58850=ORIENTED_EDGE('',*,*,#41103,.T.);
#58851=ORIENTED_EDGE('',*,*,#41345,.F.);
#58852=ORIENTED_EDGE('',*,*,#41346,.F.);
#58853=ORIENTED_EDGE('',*,*,#41109,.T.);
#58854=ORIENTED_EDGE('',*,*,#41346,.T.);
#58855=ORIENTED_EDGE('',*,*,#41347,.F.);
#58856=ORIENTED_EDGE('',*,*,#41107,.T.);
#58857=ORIENTED_EDGE('',*,*,#41115,.T.);
#58858=ORIENTED_EDGE('',*,*,#41110,.T.);
#58859=ORIENTED_EDGE('',*,*,#41348,.F.);
#58860=ORIENTED_EDGE('',*,*,#41349,.F.);
#58861=ORIENTED_EDGE('',*,*,#41116,.T.);
#58862=ORIENTED_EDGE('',*,*,#41349,.T.);
#58863=ORIENTED_EDGE('',*,*,#41350,.F.);
#58864=ORIENTED_EDGE('',*,*,#41114,.T.);
#58865=ORIENTED_EDGE('',*,*,#41122,.T.);
#58866=ORIENTED_EDGE('',*,*,#41117,.T.);
#58867=ORIENTED_EDGE('',*,*,#41351,.F.);
#58868=ORIENTED_EDGE('',*,*,#41352,.F.);
#58869=ORIENTED_EDGE('',*,*,#41123,.T.);
#58870=ORIENTED_EDGE('',*,*,#41352,.T.);
#58871=ORIENTED_EDGE('',*,*,#41353,.F.);
#58872=ORIENTED_EDGE('',*,*,#41121,.T.);
#58873=ORIENTED_EDGE('',*,*,#41129,.T.);
#58874=ORIENTED_EDGE('',*,*,#41124,.T.);
#58875=ORIENTED_EDGE('',*,*,#41354,.F.);
#58876=ORIENTED_EDGE('',*,*,#41355,.F.);
#58877=ORIENTED_EDGE('',*,*,#41130,.T.);
#58878=ORIENTED_EDGE('',*,*,#41355,.T.);
#58879=ORIENTED_EDGE('',*,*,#41356,.F.);
#58880=ORIENTED_EDGE('',*,*,#41128,.T.);
#58881=ORIENTED_EDGE('',*,*,#41136,.T.);
#58882=ORIENTED_EDGE('',*,*,#41131,.T.);
#58883=ORIENTED_EDGE('',*,*,#41357,.F.);
#58884=ORIENTED_EDGE('',*,*,#41358,.F.);
#58885=ORIENTED_EDGE('',*,*,#41137,.T.);
#58886=ORIENTED_EDGE('',*,*,#41358,.T.);
#58887=ORIENTED_EDGE('',*,*,#41359,.F.);
#58888=ORIENTED_EDGE('',*,*,#41135,.T.);
#58889=ORIENTED_EDGE('',*,*,#41143,.T.);
#58890=ORIENTED_EDGE('',*,*,#41138,.T.);
#58891=ORIENTED_EDGE('',*,*,#41360,.F.);
#58892=ORIENTED_EDGE('',*,*,#41361,.F.);
#58893=ORIENTED_EDGE('',*,*,#41144,.T.);
#58894=ORIENTED_EDGE('',*,*,#41361,.T.);
#58895=ORIENTED_EDGE('',*,*,#41362,.F.);
#58896=ORIENTED_EDGE('',*,*,#41142,.T.);
#58897=ORIENTED_EDGE('',*,*,#41150,.T.);
#58898=ORIENTED_EDGE('',*,*,#41145,.T.);
#58899=ORIENTED_EDGE('',*,*,#41363,.F.);
#58900=ORIENTED_EDGE('',*,*,#41364,.F.);
#58901=ORIENTED_EDGE('',*,*,#41151,.T.);
#58902=ORIENTED_EDGE('',*,*,#41364,.T.);
#58903=ORIENTED_EDGE('',*,*,#41365,.F.);
#58904=ORIENTED_EDGE('',*,*,#41149,.T.);
#58905=ORIENTED_EDGE('',*,*,#41157,.T.);
#58906=ORIENTED_EDGE('',*,*,#41152,.T.);
#58907=ORIENTED_EDGE('',*,*,#41366,.F.);
#58908=ORIENTED_EDGE('',*,*,#41367,.F.);
#58909=ORIENTED_EDGE('',*,*,#41158,.T.);
#58910=ORIENTED_EDGE('',*,*,#41367,.T.);
#58911=ORIENTED_EDGE('',*,*,#41368,.F.);
#58912=ORIENTED_EDGE('',*,*,#41156,.T.);
#58913=ORIENTED_EDGE('',*,*,#41164,.T.);
#58914=ORIENTED_EDGE('',*,*,#41159,.T.);
#58915=ORIENTED_EDGE('',*,*,#41369,.F.);
#58916=ORIENTED_EDGE('',*,*,#41370,.F.);
#58917=ORIENTED_EDGE('',*,*,#41165,.T.);
#58918=ORIENTED_EDGE('',*,*,#41370,.T.);
#58919=ORIENTED_EDGE('',*,*,#41371,.F.);
#58920=ORIENTED_EDGE('',*,*,#41163,.T.);
#58921=ORIENTED_EDGE('',*,*,#41171,.T.);
#58922=ORIENTED_EDGE('',*,*,#41166,.T.);
#58923=ORIENTED_EDGE('',*,*,#41372,.F.);
#58924=ORIENTED_EDGE('',*,*,#41373,.F.);
#58925=ORIENTED_EDGE('',*,*,#41172,.T.);
#58926=ORIENTED_EDGE('',*,*,#41373,.T.);
#58927=ORIENTED_EDGE('',*,*,#41374,.F.);
#58928=ORIENTED_EDGE('',*,*,#41170,.T.);
#58929=ORIENTED_EDGE('',*,*,#34381,.T.);
#58930=ORIENTED_EDGE('',*,*,#41173,.T.);
#58931=ORIENTED_EDGE('',*,*,#41375,.F.);
#58932=ORIENTED_EDGE('',*,*,#41376,.F.);
#58933=ORIENTED_EDGE('',*,*,#34382,.T.);
#58934=ORIENTED_EDGE('',*,*,#41376,.T.);
#58935=ORIENTED_EDGE('',*,*,#41377,.F.);
#58936=ORIENTED_EDGE('',*,*,#41175,.T.);
#58937=ORIENTED_EDGE('',*,*,#41181,.T.);
#58938=ORIENTED_EDGE('',*,*,#41176,.T.);
#58939=ORIENTED_EDGE('',*,*,#41378,.F.);
#58940=ORIENTED_EDGE('',*,*,#41379,.F.);
#58941=ORIENTED_EDGE('',*,*,#41182,.T.);
#58942=ORIENTED_EDGE('',*,*,#41379,.T.);
#58943=ORIENTED_EDGE('',*,*,#41380,.F.);
#58944=ORIENTED_EDGE('',*,*,#41180,.T.);
#58945=ORIENTED_EDGE('',*,*,#41188,.T.);
#58946=ORIENTED_EDGE('',*,*,#41183,.T.);
#58947=ORIENTED_EDGE('',*,*,#41381,.F.);
#58948=ORIENTED_EDGE('',*,*,#41382,.F.);
#58949=ORIENTED_EDGE('',*,*,#41189,.T.);
#58950=ORIENTED_EDGE('',*,*,#41382,.T.);
#58951=ORIENTED_EDGE('',*,*,#41383,.F.);
#58952=ORIENTED_EDGE('',*,*,#41187,.T.);
#58953=ORIENTED_EDGE('',*,*,#41195,.T.);
#58954=ORIENTED_EDGE('',*,*,#41190,.T.);
#58955=ORIENTED_EDGE('',*,*,#41384,.F.);
#58956=ORIENTED_EDGE('',*,*,#41385,.F.);
#58957=ORIENTED_EDGE('',*,*,#41196,.T.);
#58958=ORIENTED_EDGE('',*,*,#41385,.T.);
#58959=ORIENTED_EDGE('',*,*,#41386,.F.);
#58960=ORIENTED_EDGE('',*,*,#41194,.T.);
#58961=ORIENTED_EDGE('',*,*,#41387,.F.);
#58962=ORIENTED_EDGE('',*,*,#41388,.F.);
#58963=ORIENTED_EDGE('',*,*,#41202,.T.);
#58964=ORIENTED_EDGE('',*,*,#41197,.T.);
#58965=ORIENTED_EDGE('',*,*,#41203,.T.);
#58966=ORIENTED_EDGE('',*,*,#41388,.T.);
#58967=ORIENTED_EDGE('',*,*,#41389,.F.);
#58968=ORIENTED_EDGE('',*,*,#41201,.T.);
#58969=ORIENTED_EDGE('',*,*,#41209,.T.);
#58970=ORIENTED_EDGE('',*,*,#41204,.T.);
#58971=ORIENTED_EDGE('',*,*,#41390,.F.);
#58972=ORIENTED_EDGE('',*,*,#41391,.F.);
#58973=ORIENTED_EDGE('',*,*,#41210,.T.);
#58974=ORIENTED_EDGE('',*,*,#41391,.T.);
#58975=ORIENTED_EDGE('',*,*,#41392,.F.);
#58976=ORIENTED_EDGE('',*,*,#41208,.T.);
#58977=ORIENTED_EDGE('',*,*,#41216,.T.);
#58978=ORIENTED_EDGE('',*,*,#41211,.T.);
#58979=ORIENTED_EDGE('',*,*,#41393,.F.);
#58980=ORIENTED_EDGE('',*,*,#41394,.F.);
#58981=ORIENTED_EDGE('',*,*,#41217,.T.);
#58982=ORIENTED_EDGE('',*,*,#41394,.T.);
#58983=ORIENTED_EDGE('',*,*,#41395,.F.);
#58984=ORIENTED_EDGE('',*,*,#41215,.T.);
#58985=ORIENTED_EDGE('',*,*,#41223,.T.);
#58986=ORIENTED_EDGE('',*,*,#41218,.T.);
#58987=ORIENTED_EDGE('',*,*,#41396,.F.);
#58988=ORIENTED_EDGE('',*,*,#41397,.F.);
#58989=ORIENTED_EDGE('',*,*,#41224,.T.);
#58990=ORIENTED_EDGE('',*,*,#41397,.T.);
#58991=ORIENTED_EDGE('',*,*,#41398,.F.);
#58992=ORIENTED_EDGE('',*,*,#41222,.T.);
#58993=ORIENTED_EDGE('',*,*,#41399,.T.);
#58994=ORIENTED_EDGE('',*,*,#41400,.F.);
#58995=ORIENTED_EDGE('',*,*,#41225,.T.);
#58996=ORIENTED_EDGE('',*,*,#41401,.F.);
#58997=ORIENTED_EDGE('',*,*,#41402,.T.);
#58998=ORIENTED_EDGE('',*,*,#41403,.F.);
#58999=ORIENTED_EDGE('',*,*,#41227,.T.);
#59000=ORIENTED_EDGE('',*,*,#41404,.F.);
#59001=ORIENTED_EDGE('',*,*,#41405,.F.);
#59002=ORIENTED_EDGE('',*,*,#41406,.F.);
#59003=ORIENTED_EDGE('',*,*,#41407,.F.);
#59004=ORIENTED_EDGE('',*,*,#41402,.F.);
#59005=ORIENTED_EDGE('',*,*,#41407,.T.);
#59006=ORIENTED_EDGE('',*,*,#41408,.F.);
#59007=ORIENTED_EDGE('',*,*,#41228,.T.);
#59008=ORIENTED_EDGE('',*,*,#41403,.T.);
#59009=ORIENTED_EDGE('',*,*,#41409,.T.);
#59010=ORIENTED_EDGE('',*,*,#41410,.F.);
#59011=ORIENTED_EDGE('',*,*,#41230,.T.);
#59012=ORIENTED_EDGE('',*,*,#41411,.F.);
#59013=ORIENTED_EDGE('',*,*,#41412,.F.);
#59014=ORIENTED_EDGE('',*,*,#41413,.F.);
#59015=ORIENTED_EDGE('',*,*,#41414,.F.);
#59016=ORIENTED_EDGE('',*,*,#41409,.F.);
#59017=ORIENTED_EDGE('',*,*,#41414,.T.);
#59018=ORIENTED_EDGE('',*,*,#41415,.F.);
#59019=ORIENTED_EDGE('',*,*,#41231,.T.);
#59020=ORIENTED_EDGE('',*,*,#41410,.T.);
#59021=ORIENTED_EDGE('',*,*,#41416,.T.);
#59022=ORIENTED_EDGE('',*,*,#41417,.F.);
#59023=ORIENTED_EDGE('',*,*,#41233,.T.);
#59024=ORIENTED_EDGE('',*,*,#41418,.F.);
#59025=ORIENTED_EDGE('',*,*,#41419,.F.);
#59026=ORIENTED_EDGE('',*,*,#41420,.F.);
#59027=ORIENTED_EDGE('',*,*,#41421,.F.);
#59028=ORIENTED_EDGE('',*,*,#41416,.F.);
#59029=ORIENTED_EDGE('',*,*,#41421,.T.);
#59030=ORIENTED_EDGE('',*,*,#41422,.F.);
#59031=ORIENTED_EDGE('',*,*,#41234,.T.);
#59032=ORIENTED_EDGE('',*,*,#41417,.T.);
#59033=ORIENTED_EDGE('',*,*,#41423,.T.);
#59034=ORIENTED_EDGE('',*,*,#41424,.F.);
#59035=ORIENTED_EDGE('',*,*,#41236,.T.);
#59036=ORIENTED_EDGE('',*,*,#41425,.F.);
#59037=ORIENTED_EDGE('',*,*,#41426,.F.);
#59038=ORIENTED_EDGE('',*,*,#41427,.F.);
#59039=ORIENTED_EDGE('',*,*,#41428,.F.);
#59040=ORIENTED_EDGE('',*,*,#41423,.F.);
#59041=ORIENTED_EDGE('',*,*,#41428,.T.);
#59042=ORIENTED_EDGE('',*,*,#41429,.F.);
#59043=ORIENTED_EDGE('',*,*,#41237,.T.);
#59044=ORIENTED_EDGE('',*,*,#41424,.T.);
#59045=ORIENTED_EDGE('',*,*,#41430,.T.);
#59046=ORIENTED_EDGE('',*,*,#41431,.F.);
#59047=ORIENTED_EDGE('',*,*,#41239,.T.);
#59048=ORIENTED_EDGE('',*,*,#41432,.F.);
#59049=ORIENTED_EDGE('',*,*,#41433,.F.);
#59050=ORIENTED_EDGE('',*,*,#41434,.F.);
#59051=ORIENTED_EDGE('',*,*,#41435,.F.);
#59052=ORIENTED_EDGE('',*,*,#41430,.F.);
#59053=ORIENTED_EDGE('',*,*,#41435,.T.);
#59054=ORIENTED_EDGE('',*,*,#41436,.F.);
#59055=ORIENTED_EDGE('',*,*,#41240,.T.);
#59056=ORIENTED_EDGE('',*,*,#41431,.T.);
#59057=ORIENTED_EDGE('',*,*,#41437,.T.);
#59058=ORIENTED_EDGE('',*,*,#41438,.F.);
#59059=ORIENTED_EDGE('',*,*,#41242,.T.);
#59060=ORIENTED_EDGE('',*,*,#41439,.F.);
#59061=ORIENTED_EDGE('',*,*,#41440,.F.);
#59062=ORIENTED_EDGE('',*,*,#41441,.F.);
#59063=ORIENTED_EDGE('',*,*,#41442,.F.);
#59064=ORIENTED_EDGE('',*,*,#41437,.F.);
#59065=ORIENTED_EDGE('',*,*,#41442,.T.);
#59066=ORIENTED_EDGE('',*,*,#41443,.F.);
#59067=ORIENTED_EDGE('',*,*,#41243,.T.);
#59068=ORIENTED_EDGE('',*,*,#41438,.T.);
#59069=ORIENTED_EDGE('',*,*,#34378,.T.);
#59070=ORIENTED_EDGE('',*,*,#41444,.F.);
#59071=ORIENTED_EDGE('',*,*,#41245,.T.);
#59072=ORIENTED_EDGE('',*,*,#41445,.F.);
#59073=ORIENTED_EDGE('',*,*,#34377,.T.);
#59074=ORIENTED_EDGE('',*,*,#41446,.F.);
#59075=ORIENTED_EDGE('',*,*,#41246,.T.);
#59076=ORIENTED_EDGE('',*,*,#41444,.T.);
#59077=ORIENTED_EDGE('',*,*,#41447,.T.);
#59078=ORIENTED_EDGE('',*,*,#41448,.F.);
#59079=ORIENTED_EDGE('',*,*,#41248,.T.);
#59080=ORIENTED_EDGE('',*,*,#41449,.F.);
#59081=ORIENTED_EDGE('',*,*,#41450,.F.);
#59082=ORIENTED_EDGE('',*,*,#41451,.F.);
#59083=ORIENTED_EDGE('',*,*,#41452,.F.);
#59084=ORIENTED_EDGE('',*,*,#41447,.F.);
#59085=ORIENTED_EDGE('',*,*,#41452,.T.);
#59086=ORIENTED_EDGE('',*,*,#41453,.F.);
#59087=ORIENTED_EDGE('',*,*,#41249,.T.);
#59088=ORIENTED_EDGE('',*,*,#41448,.T.);
#59089=ORIENTED_EDGE('',*,*,#41454,.T.);
#59090=ORIENTED_EDGE('',*,*,#41455,.F.);
#59091=ORIENTED_EDGE('',*,*,#41251,.T.);
#59092=ORIENTED_EDGE('',*,*,#41456,.F.);
#59093=ORIENTED_EDGE('',*,*,#41457,.F.);
#59094=ORIENTED_EDGE('',*,*,#41458,.F.);
#59095=ORIENTED_EDGE('',*,*,#41459,.F.);
#59096=ORIENTED_EDGE('',*,*,#41454,.F.);
#59097=ORIENTED_EDGE('',*,*,#41459,.T.);
#59098=ORIENTED_EDGE('',*,*,#41460,.F.);
#59099=ORIENTED_EDGE('',*,*,#41252,.T.);
#59100=ORIENTED_EDGE('',*,*,#41455,.T.);
#59101=ORIENTED_EDGE('',*,*,#41461,.T.);
#59102=ORIENTED_EDGE('',*,*,#41462,.F.);
#59103=ORIENTED_EDGE('',*,*,#41254,.T.);
#59104=ORIENTED_EDGE('',*,*,#41463,.F.);
#59105=ORIENTED_EDGE('',*,*,#41464,.F.);
#59106=ORIENTED_EDGE('',*,*,#41465,.F.);
#59107=ORIENTED_EDGE('',*,*,#41466,.F.);
#59108=ORIENTED_EDGE('',*,*,#41461,.F.);
#59109=ORIENTED_EDGE('',*,*,#41466,.T.);
#59110=ORIENTED_EDGE('',*,*,#41467,.F.);
#59111=ORIENTED_EDGE('',*,*,#41255,.T.);
#59112=ORIENTED_EDGE('',*,*,#41462,.T.);
#59113=ORIENTED_EDGE('',*,*,#41468,.T.);
#59114=ORIENTED_EDGE('',*,*,#41469,.F.);
#59115=ORIENTED_EDGE('',*,*,#41257,.T.);
#59116=ORIENTED_EDGE('',*,*,#41470,.F.);
#59117=ORIENTED_EDGE('',*,*,#41471,.F.);
#59118=ORIENTED_EDGE('',*,*,#41472,.F.);
#59119=ORIENTED_EDGE('',*,*,#41473,.F.);
#59120=ORIENTED_EDGE('',*,*,#41468,.F.);
#59121=ORIENTED_EDGE('',*,*,#41473,.T.);
#59122=ORIENTED_EDGE('',*,*,#41474,.F.);
#59123=ORIENTED_EDGE('',*,*,#41258,.T.);
#59124=ORIENTED_EDGE('',*,*,#41469,.T.);
#59125=ORIENTED_EDGE('',*,*,#41475,.T.);
#59126=ORIENTED_EDGE('',*,*,#41476,.F.);
#59127=ORIENTED_EDGE('',*,*,#41260,.T.);
#59128=ORIENTED_EDGE('',*,*,#41477,.F.);
#59129=ORIENTED_EDGE('',*,*,#41478,.F.);
#59130=ORIENTED_EDGE('',*,*,#41479,.F.);
#59131=ORIENTED_EDGE('',*,*,#41480,.F.);
#59132=ORIENTED_EDGE('',*,*,#41475,.F.);
#59133=ORIENTED_EDGE('',*,*,#41480,.T.);
#59134=ORIENTED_EDGE('',*,*,#41481,.F.);
#59135=ORIENTED_EDGE('',*,*,#41261,.T.);
#59136=ORIENTED_EDGE('',*,*,#41476,.T.);
#59137=ORIENTED_EDGE('',*,*,#41482,.T.);
#59138=ORIENTED_EDGE('',*,*,#41483,.F.);
#59139=ORIENTED_EDGE('',*,*,#41263,.T.);
#59140=ORIENTED_EDGE('',*,*,#41484,.F.);
#59141=ORIENTED_EDGE('',*,*,#41485,.F.);
#59142=ORIENTED_EDGE('',*,*,#41486,.F.);
#59143=ORIENTED_EDGE('',*,*,#41487,.F.);
#59144=ORIENTED_EDGE('',*,*,#41482,.F.);
#59145=ORIENTED_EDGE('',*,*,#41487,.T.);
#59146=ORIENTED_EDGE('',*,*,#41488,.F.);
#59147=ORIENTED_EDGE('',*,*,#41264,.T.);
#59148=ORIENTED_EDGE('',*,*,#41483,.T.);
#59149=ORIENTED_EDGE('',*,*,#41489,.T.);
#59150=ORIENTED_EDGE('',*,*,#41490,.F.);
#59151=ORIENTED_EDGE('',*,*,#41266,.T.);
#59152=ORIENTED_EDGE('',*,*,#41491,.F.);
#59153=ORIENTED_EDGE('',*,*,#41492,.F.);
#59154=ORIENTED_EDGE('',*,*,#41493,.F.);
#59155=ORIENTED_EDGE('',*,*,#41494,.F.);
#59156=ORIENTED_EDGE('',*,*,#41489,.F.);
#59157=ORIENTED_EDGE('',*,*,#41494,.T.);
#59158=ORIENTED_EDGE('',*,*,#41495,.F.);
#59159=ORIENTED_EDGE('',*,*,#41267,.T.);
#59160=ORIENTED_EDGE('',*,*,#41490,.T.);
#59161=ORIENTED_EDGE('',*,*,#41496,.T.);
#59162=ORIENTED_EDGE('',*,*,#41497,.F.);
#59163=ORIENTED_EDGE('',*,*,#41269,.T.);
#59164=ORIENTED_EDGE('',*,*,#41498,.F.);
#59165=ORIENTED_EDGE('',*,*,#41499,.F.);
#59166=ORIENTED_EDGE('',*,*,#41500,.F.);
#59167=ORIENTED_EDGE('',*,*,#41501,.F.);
#59168=ORIENTED_EDGE('',*,*,#41496,.F.);
#59169=ORIENTED_EDGE('',*,*,#41501,.T.);
#59170=ORIENTED_EDGE('',*,*,#41502,.F.);
#59171=ORIENTED_EDGE('',*,*,#41270,.T.);
#59172=ORIENTED_EDGE('',*,*,#41497,.T.);
#59173=ORIENTED_EDGE('',*,*,#41503,.T.);
#59174=ORIENTED_EDGE('',*,*,#41504,.F.);
#59175=ORIENTED_EDGE('',*,*,#41272,.T.);
#59176=ORIENTED_EDGE('',*,*,#41505,.F.);
#59177=ORIENTED_EDGE('',*,*,#41506,.F.);
#59178=ORIENTED_EDGE('',*,*,#41507,.F.);
#59179=ORIENTED_EDGE('',*,*,#41508,.F.);
#59180=ORIENTED_EDGE('',*,*,#41503,.F.);
#59181=ORIENTED_EDGE('',*,*,#41508,.T.);
#59182=ORIENTED_EDGE('',*,*,#41509,.F.);
#59183=ORIENTED_EDGE('',*,*,#41273,.T.);
#59184=ORIENTED_EDGE('',*,*,#41504,.T.);
#59185=ORIENTED_EDGE('',*,*,#41510,.T.);
#59186=ORIENTED_EDGE('',*,*,#41511,.F.);
#59187=ORIENTED_EDGE('',*,*,#41275,.T.);
#59188=ORIENTED_EDGE('',*,*,#41512,.F.);
#59189=ORIENTED_EDGE('',*,*,#41513,.F.);
#59190=ORIENTED_EDGE('',*,*,#41514,.F.);
#59191=ORIENTED_EDGE('',*,*,#41515,.F.);
#59192=ORIENTED_EDGE('',*,*,#41510,.F.);
#59193=ORIENTED_EDGE('',*,*,#41515,.T.);
#59194=ORIENTED_EDGE('',*,*,#41516,.F.);
#59195=ORIENTED_EDGE('',*,*,#41276,.T.);
#59196=ORIENTED_EDGE('',*,*,#41511,.T.);
#59197=ORIENTED_EDGE('',*,*,#41517,.T.);
#59198=ORIENTED_EDGE('',*,*,#41518,.F.);
#59199=ORIENTED_EDGE('',*,*,#41278,.T.);
#59200=ORIENTED_EDGE('',*,*,#41519,.F.);
#59201=ORIENTED_EDGE('',*,*,#41520,.F.);
#59202=ORIENTED_EDGE('',*,*,#41521,.F.);
#59203=ORIENTED_EDGE('',*,*,#41522,.F.);
#59204=ORIENTED_EDGE('',*,*,#41517,.F.);
#59205=ORIENTED_EDGE('',*,*,#41522,.T.);
#59206=ORIENTED_EDGE('',*,*,#41523,.F.);
#59207=ORIENTED_EDGE('',*,*,#41279,.T.);
#59208=ORIENTED_EDGE('',*,*,#41518,.T.);
#59209=ORIENTED_EDGE('',*,*,#41524,.T.);
#59210=ORIENTED_EDGE('',*,*,#41525,.F.);
#59211=ORIENTED_EDGE('',*,*,#41281,.T.);
#59212=ORIENTED_EDGE('',*,*,#41526,.F.);
#59213=ORIENTED_EDGE('',*,*,#41527,.T.);
#59214=ORIENTED_EDGE('',*,*,#41528,.F.);
#59215=ORIENTED_EDGE('',*,*,#41282,.T.);
#59216=ORIENTED_EDGE('',*,*,#41525,.T.);
#59217=ORIENTED_EDGE('',*,*,#41529,.F.);
#59218=ORIENTED_EDGE('',*,*,#41530,.F.);
#59219=ORIENTED_EDGE('',*,*,#41527,.F.);
#59220=ORIENTED_EDGE('',*,*,#41524,.F.);
#59221=ORIENTED_EDGE('',*,*,#41284,.T.);
#59222=ORIENTED_EDGE('',*,*,#41531,.F.);
#59223=ORIENTED_EDGE('',*,*,#41532,.T.);
#59224=ORIENTED_EDGE('',*,*,#41533,.F.);
#59225=ORIENTED_EDGE('',*,*,#41534,.F.);
#59226=ORIENTED_EDGE('',*,*,#41532,.F.);
#59227=ORIENTED_EDGE('',*,*,#41535,.F.);
#59228=ORIENTED_EDGE('',*,*,#41536,.F.);
#59229=ORIENTED_EDGE('',*,*,#41285,.T.);
#59230=ORIENTED_EDGE('',*,*,#41533,.T.);
#59231=ORIENTED_EDGE('',*,*,#41534,.T.);
#59232=ORIENTED_EDGE('',*,*,#41537,.F.);
#59233=ORIENTED_EDGE('',*,*,#41538,.T.);
#59234=ORIENTED_EDGE('',*,*,#41539,.F.);
#59235=ORIENTED_EDGE('',*,*,#41287,.T.);
#59236=ORIENTED_EDGE('',*,*,#41540,.F.);
#59237=ORIENTED_EDGE('',*,*,#41541,.F.);
#59238=ORIENTED_EDGE('',*,*,#41542,.F.);
#59239=ORIENTED_EDGE('',*,*,#41543,.F.);
#59240=ORIENTED_EDGE('',*,*,#41538,.F.);
#59241=ORIENTED_EDGE('',*,*,#41543,.T.);
#59242=ORIENTED_EDGE('',*,*,#41544,.F.);
#59243=ORIENTED_EDGE('',*,*,#41288,.T.);
#59244=ORIENTED_EDGE('',*,*,#41539,.T.);
#59245=ORIENTED_EDGE('',*,*,#41545,.T.);
#59246=ORIENTED_EDGE('',*,*,#41546,.F.);
#59247=ORIENTED_EDGE('',*,*,#41290,.T.);
#59248=ORIENTED_EDGE('',*,*,#41547,.F.);
#59249=ORIENTED_EDGE('',*,*,#41548,.F.);
#59250=ORIENTED_EDGE('',*,*,#41549,.F.);
#59251=ORIENTED_EDGE('',*,*,#41550,.F.);
#59252=ORIENTED_EDGE('',*,*,#41545,.F.);
#59253=ORIENTED_EDGE('',*,*,#41550,.T.);
#59254=ORIENTED_EDGE('',*,*,#41551,.F.);
#59255=ORIENTED_EDGE('',*,*,#41291,.T.);
#59256=ORIENTED_EDGE('',*,*,#41546,.T.);
#59257=ORIENTED_EDGE('',*,*,#41552,.T.);
#59258=ORIENTED_EDGE('',*,*,#41553,.F.);
#59259=ORIENTED_EDGE('',*,*,#41293,.T.);
#59260=ORIENTED_EDGE('',*,*,#41554,.F.);
#59261=ORIENTED_EDGE('',*,*,#41555,.F.);
#59262=ORIENTED_EDGE('',*,*,#41556,.F.);
#59263=ORIENTED_EDGE('',*,*,#41557,.F.);
#59264=ORIENTED_EDGE('',*,*,#41552,.F.);
#59265=ORIENTED_EDGE('',*,*,#41557,.T.);
#59266=ORIENTED_EDGE('',*,*,#41558,.F.);
#59267=ORIENTED_EDGE('',*,*,#41294,.T.);
#59268=ORIENTED_EDGE('',*,*,#41553,.T.);
#59269=ORIENTED_EDGE('',*,*,#41559,.T.);
#59270=ORIENTED_EDGE('',*,*,#41560,.F.);
#59271=ORIENTED_EDGE('',*,*,#41296,.T.);
#59272=ORIENTED_EDGE('',*,*,#41561,.F.);
#59273=ORIENTED_EDGE('',*,*,#41562,.F.);
#59274=ORIENTED_EDGE('',*,*,#41563,.F.);
#59275=ORIENTED_EDGE('',*,*,#41564,.F.);
#59276=ORIENTED_EDGE('',*,*,#41559,.F.);
#59277=ORIENTED_EDGE('',*,*,#41564,.T.);
#59278=ORIENTED_EDGE('',*,*,#41565,.F.);
#59279=ORIENTED_EDGE('',*,*,#41297,.T.);
#59280=ORIENTED_EDGE('',*,*,#41560,.T.);
#59281=ORIENTED_EDGE('',*,*,#41566,.T.);
#59282=ORIENTED_EDGE('',*,*,#41567,.F.);
#59283=ORIENTED_EDGE('',*,*,#41299,.T.);
#59284=ORIENTED_EDGE('',*,*,#41568,.F.);
#59285=ORIENTED_EDGE('',*,*,#41569,.F.);
#59286=ORIENTED_EDGE('',*,*,#41570,.F.);
#59287=ORIENTED_EDGE('',*,*,#41571,.F.);
#59288=ORIENTED_EDGE('',*,*,#41566,.F.);
#59289=ORIENTED_EDGE('',*,*,#41571,.T.);
#59290=ORIENTED_EDGE('',*,*,#41572,.F.);
#59291=ORIENTED_EDGE('',*,*,#41300,.T.);
#59292=ORIENTED_EDGE('',*,*,#41567,.T.);
#59293=ORIENTED_EDGE('',*,*,#41573,.T.);
#59294=ORIENTED_EDGE('',*,*,#41574,.F.);
#59295=ORIENTED_EDGE('',*,*,#41302,.T.);
#59296=ORIENTED_EDGE('',*,*,#41575,.F.);
#59297=ORIENTED_EDGE('',*,*,#41576,.F.);
#59298=ORIENTED_EDGE('',*,*,#41577,.F.);
#59299=ORIENTED_EDGE('',*,*,#41578,.F.);
#59300=ORIENTED_EDGE('',*,*,#41573,.F.);
#59301=ORIENTED_EDGE('',*,*,#41578,.T.);
#59302=ORIENTED_EDGE('',*,*,#41579,.F.);
#59303=ORIENTED_EDGE('',*,*,#41303,.T.);
#59304=ORIENTED_EDGE('',*,*,#41574,.T.);
#59305=ORIENTED_EDGE('',*,*,#41580,.T.);
#59306=ORIENTED_EDGE('',*,*,#41581,.F.);
#59307=ORIENTED_EDGE('',*,*,#41305,.T.);
#59308=ORIENTED_EDGE('',*,*,#41582,.F.);
#59309=ORIENTED_EDGE('',*,*,#41583,.F.);
#59310=ORIENTED_EDGE('',*,*,#41584,.F.);
#59311=ORIENTED_EDGE('',*,*,#41585,.F.);
#59312=ORIENTED_EDGE('',*,*,#41580,.F.);
#59313=ORIENTED_EDGE('',*,*,#41585,.T.);
#59314=ORIENTED_EDGE('',*,*,#41586,.F.);
#59315=ORIENTED_EDGE('',*,*,#41306,.T.);
#59316=ORIENTED_EDGE('',*,*,#41581,.T.);
#59317=ORIENTED_EDGE('',*,*,#41587,.T.);
#59318=ORIENTED_EDGE('',*,*,#41588,.F.);
#59319=ORIENTED_EDGE('',*,*,#41308,.T.);
#59320=ORIENTED_EDGE('',*,*,#41589,.F.);
#59321=ORIENTED_EDGE('',*,*,#41590,.F.);
#59322=ORIENTED_EDGE('',*,*,#41591,.F.);
#59323=ORIENTED_EDGE('',*,*,#41592,.F.);
#59324=ORIENTED_EDGE('',*,*,#41587,.F.);
#59325=ORIENTED_EDGE('',*,*,#41592,.T.);
#59326=ORIENTED_EDGE('',*,*,#41593,.F.);
#59327=ORIENTED_EDGE('',*,*,#41309,.T.);
#59328=ORIENTED_EDGE('',*,*,#41588,.T.);
#59329=ORIENTED_EDGE('',*,*,#41594,.F.);
#59330=ORIENTED_EDGE('',*,*,#41595,.F.);
#59331=ORIENTED_EDGE('',*,*,#41399,.F.);
#59332=ORIENTED_EDGE('',*,*,#41596,.F.);
#59333=ORIENTED_EDGE('',*,*,#41596,.T.);
#59334=ORIENTED_EDGE('',*,*,#41401,.T.);
#59335=ORIENTED_EDGE('',*,*,#41311,.T.);
#59336=ORIENTED_EDGE('',*,*,#41597,.F.);
#59337=ORIENTED_EDGE('',*,*,#41312,.T.);
#59338=ORIENTED_EDGE('',*,*,#41598,.F.);
#59339=ORIENTED_EDGE('',*,*,#41599,.T.);
#59340=ORIENTED_EDGE('',*,*,#41600,.F.);
#59341=ORIENTED_EDGE('',*,*,#41314,.T.);
#59342=ORIENTED_EDGE('',*,*,#41601,.F.);
#59343=ORIENTED_EDGE('',*,*,#41602,.T.);
#59344=ORIENTED_EDGE('',*,*,#41603,.F.);
#59345=ORIENTED_EDGE('',*,*,#41315,.T.);
#59346=ORIENTED_EDGE('',*,*,#41603,.T.);
#59347=ORIENTED_EDGE('',*,*,#41604,.T.);
#59348=ORIENTED_EDGE('',*,*,#41605,.F.);
#59349=ORIENTED_EDGE('',*,*,#41604,.F.);
#59350=ORIENTED_EDGE('',*,*,#41602,.F.);
#59351=ORIENTED_EDGE('',*,*,#41606,.F.);
#59352=ORIENTED_EDGE('',*,*,#41607,.F.);
#59353=ORIENTED_EDGE('',*,*,#41317,.T.);
#59354=ORIENTED_EDGE('',*,*,#41608,.F.);
#59355=ORIENTED_EDGE('',*,*,#41609,.T.);
#59356=ORIENTED_EDGE('',*,*,#41610,.F.);
#59357=ORIENTED_EDGE('',*,*,#41318,.T.);
#59358=ORIENTED_EDGE('',*,*,#41610,.T.);
#59359=ORIENTED_EDGE('',*,*,#41611,.T.);
#59360=ORIENTED_EDGE('',*,*,#41612,.F.);
#59361=ORIENTED_EDGE('',*,*,#41611,.F.);
#59362=ORIENTED_EDGE('',*,*,#41609,.F.);
#59363=ORIENTED_EDGE('',*,*,#41613,.F.);
#59364=ORIENTED_EDGE('',*,*,#41614,.F.);
#59365=ORIENTED_EDGE('',*,*,#41320,.T.);
#59366=ORIENTED_EDGE('',*,*,#41615,.F.);
#59367=ORIENTED_EDGE('',*,*,#41616,.T.);
#59368=ORIENTED_EDGE('',*,*,#41617,.F.);
#59369=ORIENTED_EDGE('',*,*,#41321,.T.);
#59370=ORIENTED_EDGE('',*,*,#41617,.T.);
#59371=ORIENTED_EDGE('',*,*,#41618,.T.);
#59372=ORIENTED_EDGE('',*,*,#41619,.F.);
#59373=ORIENTED_EDGE('',*,*,#41618,.F.);
#59374=ORIENTED_EDGE('',*,*,#41616,.F.);
#59375=ORIENTED_EDGE('',*,*,#41620,.F.);
#59376=ORIENTED_EDGE('',*,*,#41621,.F.);
#59377=ORIENTED_EDGE('',*,*,#41323,.T.);
#59378=ORIENTED_EDGE('',*,*,#41622,.F.);
#59379=ORIENTED_EDGE('',*,*,#41623,.T.);
#59380=ORIENTED_EDGE('',*,*,#41624,.F.);
#59381=ORIENTED_EDGE('',*,*,#41324,.T.);
#59382=ORIENTED_EDGE('',*,*,#41624,.T.);
#59383=ORIENTED_EDGE('',*,*,#41625,.T.);
#59384=ORIENTED_EDGE('',*,*,#41626,.F.);
#59385=ORIENTED_EDGE('',*,*,#41625,.F.);
#59386=ORIENTED_EDGE('',*,*,#41623,.F.);
#59387=ORIENTED_EDGE('',*,*,#41627,.F.);
#59388=ORIENTED_EDGE('',*,*,#41628,.F.);
#59389=ORIENTED_EDGE('',*,*,#41326,.T.);
#59390=ORIENTED_EDGE('',*,*,#41629,.F.);
#59391=ORIENTED_EDGE('',*,*,#41630,.T.);
#59392=ORIENTED_EDGE('',*,*,#41631,.F.);
#59393=ORIENTED_EDGE('',*,*,#41327,.T.);
#59394=ORIENTED_EDGE('',*,*,#41631,.T.);
#59395=ORIENTED_EDGE('',*,*,#41632,.T.);
#59396=ORIENTED_EDGE('',*,*,#41633,.F.);
#59397=ORIENTED_EDGE('',*,*,#41632,.F.);
#59398=ORIENTED_EDGE('',*,*,#41630,.F.);
#59399=ORIENTED_EDGE('',*,*,#41634,.F.);
#59400=ORIENTED_EDGE('',*,*,#41635,.F.);
#59401=ORIENTED_EDGE('',*,*,#41329,.T.);
#59402=ORIENTED_EDGE('',*,*,#41636,.F.);
#59403=ORIENTED_EDGE('',*,*,#41637,.T.);
#59404=ORIENTED_EDGE('',*,*,#41638,.F.);
#59405=ORIENTED_EDGE('',*,*,#41330,.T.);
#59406=ORIENTED_EDGE('',*,*,#41638,.T.);
#59407=ORIENTED_EDGE('',*,*,#41639,.T.);
#59408=ORIENTED_EDGE('',*,*,#41640,.F.);
#59409=ORIENTED_EDGE('',*,*,#41639,.F.);
#59410=ORIENTED_EDGE('',*,*,#41637,.F.);
#59411=ORIENTED_EDGE('',*,*,#41641,.F.);
#59412=ORIENTED_EDGE('',*,*,#41642,.F.);
#59413=ORIENTED_EDGE('',*,*,#41332,.T.);
#59414=ORIENTED_EDGE('',*,*,#41643,.F.);
#59415=ORIENTED_EDGE('',*,*,#41644,.T.);
#59416=ORIENTED_EDGE('',*,*,#41645,.F.);
#59417=ORIENTED_EDGE('',*,*,#41333,.T.);
#59418=ORIENTED_EDGE('',*,*,#41645,.T.);
#59419=ORIENTED_EDGE('',*,*,#41646,.T.);
#59420=ORIENTED_EDGE('',*,*,#41647,.F.);
#59421=ORIENTED_EDGE('',*,*,#41646,.F.);
#59422=ORIENTED_EDGE('',*,*,#41644,.F.);
#59423=ORIENTED_EDGE('',*,*,#41648,.F.);
#59424=ORIENTED_EDGE('',*,*,#41649,.F.);
#59425=ORIENTED_EDGE('',*,*,#41335,.T.);
#59426=ORIENTED_EDGE('',*,*,#41650,.F.);
#59427=ORIENTED_EDGE('',*,*,#41651,.T.);
#59428=ORIENTED_EDGE('',*,*,#41652,.F.);
#59429=ORIENTED_EDGE('',*,*,#41336,.T.);
#59430=ORIENTED_EDGE('',*,*,#41652,.T.);
#59431=ORIENTED_EDGE('',*,*,#41653,.T.);
#59432=ORIENTED_EDGE('',*,*,#41654,.F.);
#59433=ORIENTED_EDGE('',*,*,#41653,.F.);
#59434=ORIENTED_EDGE('',*,*,#41651,.F.);
#59435=ORIENTED_EDGE('',*,*,#41655,.F.);
#59436=ORIENTED_EDGE('',*,*,#41656,.F.);
#59437=ORIENTED_EDGE('',*,*,#41338,.T.);
#59438=ORIENTED_EDGE('',*,*,#41657,.F.);
#59439=ORIENTED_EDGE('',*,*,#41658,.T.);
#59440=ORIENTED_EDGE('',*,*,#41659,.F.);
#59441=ORIENTED_EDGE('',*,*,#41339,.T.);
#59442=ORIENTED_EDGE('',*,*,#41659,.T.);
#59443=ORIENTED_EDGE('',*,*,#41660,.T.);
#59444=ORIENTED_EDGE('',*,*,#41661,.F.);
#59445=ORIENTED_EDGE('',*,*,#41660,.F.);
#59446=ORIENTED_EDGE('',*,*,#41658,.F.);
#59447=ORIENTED_EDGE('',*,*,#41662,.F.);
#59448=ORIENTED_EDGE('',*,*,#41663,.F.);
#59449=ORIENTED_EDGE('',*,*,#41341,.T.);
#59450=ORIENTED_EDGE('',*,*,#41664,.F.);
#59451=ORIENTED_EDGE('',*,*,#41665,.T.);
#59452=ORIENTED_EDGE('',*,*,#41666,.F.);
#59453=ORIENTED_EDGE('',*,*,#41342,.T.);
#59454=ORIENTED_EDGE('',*,*,#41666,.T.);
#59455=ORIENTED_EDGE('',*,*,#41667,.T.);
#59456=ORIENTED_EDGE('',*,*,#41668,.F.);
#59457=ORIENTED_EDGE('',*,*,#41667,.F.);
#59458=ORIENTED_EDGE('',*,*,#41665,.F.);
#59459=ORIENTED_EDGE('',*,*,#41669,.F.);
#59460=ORIENTED_EDGE('',*,*,#41670,.F.);
#59461=ORIENTED_EDGE('',*,*,#41344,.T.);
#59462=ORIENTED_EDGE('',*,*,#41671,.F.);
#59463=ORIENTED_EDGE('',*,*,#41672,.T.);
#59464=ORIENTED_EDGE('',*,*,#41673,.F.);
#59465=ORIENTED_EDGE('',*,*,#41345,.T.);
#59466=ORIENTED_EDGE('',*,*,#41673,.T.);
#59467=ORIENTED_EDGE('',*,*,#41674,.T.);
#59468=ORIENTED_EDGE('',*,*,#41675,.F.);
#59469=ORIENTED_EDGE('',*,*,#41674,.F.);
#59470=ORIENTED_EDGE('',*,*,#41672,.F.);
#59471=ORIENTED_EDGE('',*,*,#41676,.F.);
#59472=ORIENTED_EDGE('',*,*,#41677,.F.);
#59473=ORIENTED_EDGE('',*,*,#41347,.T.);
#59474=ORIENTED_EDGE('',*,*,#41678,.F.);
#59475=ORIENTED_EDGE('',*,*,#41679,.T.);
#59476=ORIENTED_EDGE('',*,*,#41680,.F.);
#59477=ORIENTED_EDGE('',*,*,#41348,.T.);
#59478=ORIENTED_EDGE('',*,*,#41680,.T.);
#59479=ORIENTED_EDGE('',*,*,#41681,.T.);
#59480=ORIENTED_EDGE('',*,*,#41682,.F.);
#59481=ORIENTED_EDGE('',*,*,#41681,.F.);
#59482=ORIENTED_EDGE('',*,*,#41679,.F.);
#59483=ORIENTED_EDGE('',*,*,#41683,.F.);
#59484=ORIENTED_EDGE('',*,*,#41684,.F.);
#59485=ORIENTED_EDGE('',*,*,#41350,.T.);
#59486=ORIENTED_EDGE('',*,*,#41685,.F.);
#59487=ORIENTED_EDGE('',*,*,#41686,.T.);
#59488=ORIENTED_EDGE('',*,*,#41687,.F.);
#59489=ORIENTED_EDGE('',*,*,#41351,.T.);
#59490=ORIENTED_EDGE('',*,*,#41687,.T.);
#59491=ORIENTED_EDGE('',*,*,#41688,.T.);
#59492=ORIENTED_EDGE('',*,*,#41689,.F.);
#59493=ORIENTED_EDGE('',*,*,#41688,.F.);
#59494=ORIENTED_EDGE('',*,*,#41686,.F.);
#59495=ORIENTED_EDGE('',*,*,#41690,.F.);
#59496=ORIENTED_EDGE('',*,*,#41691,.F.);
#59497=ORIENTED_EDGE('',*,*,#41353,.T.);
#59498=ORIENTED_EDGE('',*,*,#41692,.F.);
#59499=ORIENTED_EDGE('',*,*,#34375,.T.);
#59500=ORIENTED_EDGE('',*,*,#41693,.F.);
#59501=ORIENTED_EDGE('',*,*,#41354,.T.);
#59502=ORIENTED_EDGE('',*,*,#41693,.T.);
#59503=ORIENTED_EDGE('',*,*,#34374,.T.);
#59504=ORIENTED_EDGE('',*,*,#41694,.F.);
#59505=ORIENTED_EDGE('',*,*,#41356,.T.);
#59506=ORIENTED_EDGE('',*,*,#41695,.F.);
#59507=ORIENTED_EDGE('',*,*,#41696,.T.);
#59508=ORIENTED_EDGE('',*,*,#41697,.F.);
#59509=ORIENTED_EDGE('',*,*,#41357,.T.);
#59510=ORIENTED_EDGE('',*,*,#41697,.T.);
#59511=ORIENTED_EDGE('',*,*,#41698,.T.);
#59512=ORIENTED_EDGE('',*,*,#41699,.F.);
#59513=ORIENTED_EDGE('',*,*,#41698,.F.);
#59514=ORIENTED_EDGE('',*,*,#41696,.F.);
#59515=ORIENTED_EDGE('',*,*,#41700,.F.);
#59516=ORIENTED_EDGE('',*,*,#41701,.F.);
#59517=ORIENTED_EDGE('',*,*,#41359,.T.);
#59518=ORIENTED_EDGE('',*,*,#41702,.F.);
#59519=ORIENTED_EDGE('',*,*,#41703,.T.);
#59520=ORIENTED_EDGE('',*,*,#41704,.F.);
#59521=ORIENTED_EDGE('',*,*,#41360,.T.);
#59522=ORIENTED_EDGE('',*,*,#41704,.T.);
#59523=ORIENTED_EDGE('',*,*,#41705,.T.);
#59524=ORIENTED_EDGE('',*,*,#41706,.F.);
#59525=ORIENTED_EDGE('',*,*,#41705,.F.);
#59526=ORIENTED_EDGE('',*,*,#41703,.F.);
#59527=ORIENTED_EDGE('',*,*,#41707,.F.);
#59528=ORIENTED_EDGE('',*,*,#41708,.F.);
#59529=ORIENTED_EDGE('',*,*,#41362,.T.);
#59530=ORIENTED_EDGE('',*,*,#41709,.F.);
#59531=ORIENTED_EDGE('',*,*,#41710,.T.);
#59532=ORIENTED_EDGE('',*,*,#41711,.F.);
#59533=ORIENTED_EDGE('',*,*,#41363,.T.);
#59534=ORIENTED_EDGE('',*,*,#41711,.T.);
#59535=ORIENTED_EDGE('',*,*,#41712,.T.);
#59536=ORIENTED_EDGE('',*,*,#41713,.F.);
#59537=ORIENTED_EDGE('',*,*,#41712,.F.);
#59538=ORIENTED_EDGE('',*,*,#41710,.F.);
#59539=ORIENTED_EDGE('',*,*,#41714,.F.);
#59540=ORIENTED_EDGE('',*,*,#41715,.F.);
#59541=ORIENTED_EDGE('',*,*,#41365,.T.);
#59542=ORIENTED_EDGE('',*,*,#41716,.F.);
#59543=ORIENTED_EDGE('',*,*,#41717,.T.);
#59544=ORIENTED_EDGE('',*,*,#41718,.F.);
#59545=ORIENTED_EDGE('',*,*,#41366,.T.);
#59546=ORIENTED_EDGE('',*,*,#41718,.T.);
#59547=ORIENTED_EDGE('',*,*,#41719,.T.);
#59548=ORIENTED_EDGE('',*,*,#41720,.F.);
#59549=ORIENTED_EDGE('',*,*,#41719,.F.);
#59550=ORIENTED_EDGE('',*,*,#41717,.F.);
#59551=ORIENTED_EDGE('',*,*,#41721,.F.);
#59552=ORIENTED_EDGE('',*,*,#41722,.F.);
#59553=ORIENTED_EDGE('',*,*,#41368,.T.);
#59554=ORIENTED_EDGE('',*,*,#41723,.F.);
#59555=ORIENTED_EDGE('',*,*,#41724,.T.);
#59556=ORIENTED_EDGE('',*,*,#41725,.F.);
#59557=ORIENTED_EDGE('',*,*,#41369,.T.);
#59558=ORIENTED_EDGE('',*,*,#41725,.T.);
#59559=ORIENTED_EDGE('',*,*,#41726,.T.);
#59560=ORIENTED_EDGE('',*,*,#41727,.F.);
#59561=ORIENTED_EDGE('',*,*,#41726,.F.);
#59562=ORIENTED_EDGE('',*,*,#41724,.F.);
#59563=ORIENTED_EDGE('',*,*,#41728,.F.);
#59564=ORIENTED_EDGE('',*,*,#41729,.F.);
#59565=ORIENTED_EDGE('',*,*,#41371,.T.);
#59566=ORIENTED_EDGE('',*,*,#41730,.F.);
#59567=ORIENTED_EDGE('',*,*,#41731,.T.);
#59568=ORIENTED_EDGE('',*,*,#41732,.F.);
#59569=ORIENTED_EDGE('',*,*,#41372,.T.);
#59570=ORIENTED_EDGE('',*,*,#41732,.T.);
#59571=ORIENTED_EDGE('',*,*,#41733,.T.);
#59572=ORIENTED_EDGE('',*,*,#41734,.F.);
#59573=ORIENTED_EDGE('',*,*,#41733,.F.);
#59574=ORIENTED_EDGE('',*,*,#41731,.F.);
#59575=ORIENTED_EDGE('',*,*,#41735,.F.);
#59576=ORIENTED_EDGE('',*,*,#41736,.F.);
#59577=ORIENTED_EDGE('',*,*,#41374,.T.);
#59578=ORIENTED_EDGE('',*,*,#41737,.F.);
#59579=ORIENTED_EDGE('',*,*,#41738,.T.);
#59580=ORIENTED_EDGE('',*,*,#41739,.F.);
#59581=ORIENTED_EDGE('',*,*,#41375,.T.);
#59582=ORIENTED_EDGE('',*,*,#41739,.T.);
#59583=ORIENTED_EDGE('',*,*,#41740,.T.);
#59584=ORIENTED_EDGE('',*,*,#41741,.F.);
#59585=ORIENTED_EDGE('',*,*,#41740,.F.);
#59586=ORIENTED_EDGE('',*,*,#41738,.F.);
#59587=ORIENTED_EDGE('',*,*,#41742,.F.);
#59588=ORIENTED_EDGE('',*,*,#41743,.F.);
#59589=ORIENTED_EDGE('',*,*,#41377,.T.);
#59590=ORIENTED_EDGE('',*,*,#41744,.F.);
#59591=ORIENTED_EDGE('',*,*,#41745,.T.);
#59592=ORIENTED_EDGE('',*,*,#41746,.F.);
#59593=ORIENTED_EDGE('',*,*,#41378,.T.);
#59594=ORIENTED_EDGE('',*,*,#41746,.T.);
#59595=ORIENTED_EDGE('',*,*,#41747,.T.);
#59596=ORIENTED_EDGE('',*,*,#41748,.F.);
#59597=ORIENTED_EDGE('',*,*,#41747,.F.);
#59598=ORIENTED_EDGE('',*,*,#41745,.F.);
#59599=ORIENTED_EDGE('',*,*,#41749,.F.);
#59600=ORIENTED_EDGE('',*,*,#41750,.F.);
#59601=ORIENTED_EDGE('',*,*,#41380,.T.);
#59602=ORIENTED_EDGE('',*,*,#41751,.F.);
#59603=ORIENTED_EDGE('',*,*,#41752,.T.);
#59604=ORIENTED_EDGE('',*,*,#41753,.F.);
#59605=ORIENTED_EDGE('',*,*,#41381,.T.);
#59606=ORIENTED_EDGE('',*,*,#41753,.T.);
#59607=ORIENTED_EDGE('',*,*,#41754,.T.);
#59608=ORIENTED_EDGE('',*,*,#41755,.F.);
#59609=ORIENTED_EDGE('',*,*,#41754,.F.);
#59610=ORIENTED_EDGE('',*,*,#41752,.F.);
#59611=ORIENTED_EDGE('',*,*,#41756,.F.);
#59612=ORIENTED_EDGE('',*,*,#41757,.F.);
#59613=ORIENTED_EDGE('',*,*,#41383,.T.);
#59614=ORIENTED_EDGE('',*,*,#41758,.F.);
#59615=ORIENTED_EDGE('',*,*,#41759,.T.);
#59616=ORIENTED_EDGE('',*,*,#41760,.F.);
#59617=ORIENTED_EDGE('',*,*,#41384,.T.);
#59618=ORIENTED_EDGE('',*,*,#41760,.T.);
#59619=ORIENTED_EDGE('',*,*,#41761,.T.);
#59620=ORIENTED_EDGE('',*,*,#41762,.F.);
#59621=ORIENTED_EDGE('',*,*,#41761,.F.);
#59622=ORIENTED_EDGE('',*,*,#41759,.F.);
#59623=ORIENTED_EDGE('',*,*,#41763,.F.);
#59624=ORIENTED_EDGE('',*,*,#41764,.F.);
#59625=ORIENTED_EDGE('',*,*,#41386,.T.);
#59626=ORIENTED_EDGE('',*,*,#41765,.F.);
#59627=ORIENTED_EDGE('',*,*,#41766,.T.);
#59628=ORIENTED_EDGE('',*,*,#41767,.F.);
#59629=ORIENTED_EDGE('',*,*,#41768,.T.);
#59630=ORIENTED_EDGE('',*,*,#41769,.F.);
#59631=ORIENTED_EDGE('',*,*,#41387,.T.);
#59632=ORIENTED_EDGE('',*,*,#41767,.T.);
#59633=ORIENTED_EDGE('',*,*,#41770,.F.);
#59634=ORIENTED_EDGE('',*,*,#41771,.F.);
#59635=ORIENTED_EDGE('',*,*,#41768,.F.);
#59636=ORIENTED_EDGE('',*,*,#41766,.F.);
#59637=ORIENTED_EDGE('',*,*,#41389,.T.);
#59638=ORIENTED_EDGE('',*,*,#41772,.F.);
#59639=ORIENTED_EDGE('',*,*,#41773,.T.);
#59640=ORIENTED_EDGE('',*,*,#41774,.F.);
#59641=ORIENTED_EDGE('',*,*,#41390,.T.);
#59642=ORIENTED_EDGE('',*,*,#41774,.T.);
#59643=ORIENTED_EDGE('',*,*,#41775,.T.);
#59644=ORIENTED_EDGE('',*,*,#41776,.F.);
#59645=ORIENTED_EDGE('',*,*,#41775,.F.);
#59646=ORIENTED_EDGE('',*,*,#41773,.F.);
#59647=ORIENTED_EDGE('',*,*,#41777,.F.);
#59648=ORIENTED_EDGE('',*,*,#41778,.F.);
#59649=ORIENTED_EDGE('',*,*,#41392,.T.);
#59650=ORIENTED_EDGE('',*,*,#41779,.F.);
#59651=ORIENTED_EDGE('',*,*,#41780,.T.);
#59652=ORIENTED_EDGE('',*,*,#41781,.F.);
#59653=ORIENTED_EDGE('',*,*,#41393,.T.);
#59654=ORIENTED_EDGE('',*,*,#41781,.T.);
#59655=ORIENTED_EDGE('',*,*,#41782,.T.);
#59656=ORIENTED_EDGE('',*,*,#41783,.F.);
#59657=ORIENTED_EDGE('',*,*,#41782,.F.);
#59658=ORIENTED_EDGE('',*,*,#41780,.F.);
#59659=ORIENTED_EDGE('',*,*,#41784,.F.);
#59660=ORIENTED_EDGE('',*,*,#41785,.F.);
#59661=ORIENTED_EDGE('',*,*,#41395,.T.);
#59662=ORIENTED_EDGE('',*,*,#41786,.F.);
#59663=ORIENTED_EDGE('',*,*,#41787,.T.);
#59664=ORIENTED_EDGE('',*,*,#41788,.F.);
#59665=ORIENTED_EDGE('',*,*,#41396,.T.);
#59666=ORIENTED_EDGE('',*,*,#41788,.T.);
#59667=ORIENTED_EDGE('',*,*,#41789,.T.);
#59668=ORIENTED_EDGE('',*,*,#41790,.F.);
#59669=ORIENTED_EDGE('',*,*,#41789,.F.);
#59670=ORIENTED_EDGE('',*,*,#41787,.F.);
#59671=ORIENTED_EDGE('',*,*,#41791,.F.);
#59672=ORIENTED_EDGE('',*,*,#41792,.F.);
#59673=ORIENTED_EDGE('',*,*,#41599,.F.);
#59674=ORIENTED_EDGE('',*,*,#41793,.F.);
#59675=ORIENTED_EDGE('',*,*,#41794,.F.);
#59676=ORIENTED_EDGE('',*,*,#41795,.F.);
#59677=ORIENTED_EDGE('',*,*,#41398,.T.);
#59678=ORIENTED_EDGE('',*,*,#41796,.F.);
#59679=ORIENTED_EDGE('',*,*,#41793,.T.);
#59680=ORIENTED_EDGE('',*,*,#41598,.T.);
#59681=ORIENTED_EDGE('',*,*,#41797,.F.);
#59682=ORIENTED_EDGE('',*,*,#41400,.T.);
#59683=ORIENTED_EDGE('',*,*,#41595,.T.);
#59684=ORIENTED_EDGE('',*,*,#41798,.F.);
#59685=ORIENTED_EDGE('',*,*,#41799,.F.);
#59686=ORIENTED_EDGE('',*,*,#41800,.F.);
#59687=ORIENTED_EDGE('',*,*,#41405,.T.);
#59688=ORIENTED_EDGE('',*,*,#41404,.T.);
#59689=ORIENTED_EDGE('',*,*,#41801,.F.);
#59690=ORIENTED_EDGE('',*,*,#41408,.T.);
#59691=ORIENTED_EDGE('',*,*,#41406,.T.);
#59692=ORIENTED_EDGE('',*,*,#41800,.T.);
#59693=ORIENTED_EDGE('',*,*,#41802,.F.);
#59694=ORIENTED_EDGE('',*,*,#41803,.F.);
#59695=ORIENTED_EDGE('',*,*,#41412,.T.);
#59696=ORIENTED_EDGE('',*,*,#41411,.T.);
#59697=ORIENTED_EDGE('',*,*,#41804,.F.);
#59698=ORIENTED_EDGE('',*,*,#41415,.T.);
#59699=ORIENTED_EDGE('',*,*,#41413,.T.);
#59700=ORIENTED_EDGE('',*,*,#41803,.T.);
#59701=ORIENTED_EDGE('',*,*,#41805,.F.);
#59702=ORIENTED_EDGE('',*,*,#41806,.F.);
#59703=ORIENTED_EDGE('',*,*,#41419,.T.);
#59704=ORIENTED_EDGE('',*,*,#41418,.T.);
#59705=ORIENTED_EDGE('',*,*,#41807,.F.);
#59706=ORIENTED_EDGE('',*,*,#41422,.T.);
#59707=ORIENTED_EDGE('',*,*,#41420,.T.);
#59708=ORIENTED_EDGE('',*,*,#41806,.T.);
#59709=ORIENTED_EDGE('',*,*,#41808,.F.);
#59710=ORIENTED_EDGE('',*,*,#41809,.F.);
#59711=ORIENTED_EDGE('',*,*,#41426,.T.);
#59712=ORIENTED_EDGE('',*,*,#41425,.T.);
#59713=ORIENTED_EDGE('',*,*,#41810,.F.);
#59714=ORIENTED_EDGE('',*,*,#41429,.T.);
#59715=ORIENTED_EDGE('',*,*,#41427,.T.);
#59716=ORIENTED_EDGE('',*,*,#41809,.T.);
#59717=ORIENTED_EDGE('',*,*,#41811,.F.);
#59718=ORIENTED_EDGE('',*,*,#41812,.F.);
#59719=ORIENTED_EDGE('',*,*,#41433,.T.);
#59720=ORIENTED_EDGE('',*,*,#41432,.T.);
#59721=ORIENTED_EDGE('',*,*,#41813,.F.);
#59722=ORIENTED_EDGE('',*,*,#41436,.T.);
#59723=ORIENTED_EDGE('',*,*,#41434,.T.);
#59724=ORIENTED_EDGE('',*,*,#41812,.T.);
#59725=ORIENTED_EDGE('',*,*,#41814,.F.);
#59726=ORIENTED_EDGE('',*,*,#41815,.F.);
#59727=ORIENTED_EDGE('',*,*,#41440,.T.);
#59728=ORIENTED_EDGE('',*,*,#41439,.T.);
#59729=ORIENTED_EDGE('',*,*,#41816,.F.);
#59730=ORIENTED_EDGE('',*,*,#41443,.T.);
#59731=ORIENTED_EDGE('',*,*,#41441,.T.);
#59732=ORIENTED_EDGE('',*,*,#41815,.T.);
#59733=ORIENTED_EDGE('',*,*,#41817,.F.);
#59734=ORIENTED_EDGE('',*,*,#41818,.F.);
#59735=ORIENTED_EDGE('',*,*,#34379,.T.);
#59736=ORIENTED_EDGE('',*,*,#41445,.T.);
#59737=ORIENTED_EDGE('',*,*,#41819,.F.);
#59738=ORIENTED_EDGE('',*,*,#41446,.T.);
#59739=ORIENTED_EDGE('',*,*,#34380,.T.);
#59740=ORIENTED_EDGE('',*,*,#41818,.T.);
#59741=ORIENTED_EDGE('',*,*,#41820,.F.);
#59742=ORIENTED_EDGE('',*,*,#41821,.F.);
#59743=ORIENTED_EDGE('',*,*,#41450,.T.);
#59744=ORIENTED_EDGE('',*,*,#41449,.T.);
#59745=ORIENTED_EDGE('',*,*,#41822,.F.);
#59746=ORIENTED_EDGE('',*,*,#41453,.T.);
#59747=ORIENTED_EDGE('',*,*,#41451,.T.);
#59748=ORIENTED_EDGE('',*,*,#41821,.T.);
#59749=ORIENTED_EDGE('',*,*,#41823,.F.);
#59750=ORIENTED_EDGE('',*,*,#41824,.F.);
#59751=ORIENTED_EDGE('',*,*,#41457,.T.);
#59752=ORIENTED_EDGE('',*,*,#41456,.T.);
#59753=ORIENTED_EDGE('',*,*,#41825,.F.);
#59754=ORIENTED_EDGE('',*,*,#41460,.T.);
#59755=ORIENTED_EDGE('',*,*,#41458,.T.);
#59756=ORIENTED_EDGE('',*,*,#41824,.T.);
#59757=ORIENTED_EDGE('',*,*,#41826,.F.);
#59758=ORIENTED_EDGE('',*,*,#41827,.F.);
#59759=ORIENTED_EDGE('',*,*,#41464,.T.);
#59760=ORIENTED_EDGE('',*,*,#41463,.T.);
#59761=ORIENTED_EDGE('',*,*,#41828,.F.);
#59762=ORIENTED_EDGE('',*,*,#41467,.T.);
#59763=ORIENTED_EDGE('',*,*,#41465,.T.);
#59764=ORIENTED_EDGE('',*,*,#41827,.T.);
#59765=ORIENTED_EDGE('',*,*,#41829,.F.);
#59766=ORIENTED_EDGE('',*,*,#41830,.F.);
#59767=ORIENTED_EDGE('',*,*,#41471,.T.);
#59768=ORIENTED_EDGE('',*,*,#41470,.T.);
#59769=ORIENTED_EDGE('',*,*,#41831,.F.);
#59770=ORIENTED_EDGE('',*,*,#41474,.T.);
#59771=ORIENTED_EDGE('',*,*,#41472,.T.);
#59772=ORIENTED_EDGE('',*,*,#41830,.T.);
#59773=ORIENTED_EDGE('',*,*,#41832,.F.);
#59774=ORIENTED_EDGE('',*,*,#41833,.F.);
#59775=ORIENTED_EDGE('',*,*,#41478,.T.);
#59776=ORIENTED_EDGE('',*,*,#41477,.T.);
#59777=ORIENTED_EDGE('',*,*,#41834,.F.);
#59778=ORIENTED_EDGE('',*,*,#41481,.T.);
#59779=ORIENTED_EDGE('',*,*,#41479,.T.);
#59780=ORIENTED_EDGE('',*,*,#41833,.T.);
#59781=ORIENTED_EDGE('',*,*,#41835,.F.);
#59782=ORIENTED_EDGE('',*,*,#41836,.F.);
#59783=ORIENTED_EDGE('',*,*,#41485,.T.);
#59784=ORIENTED_EDGE('',*,*,#41484,.T.);
#59785=ORIENTED_EDGE('',*,*,#41837,.F.);
#59786=ORIENTED_EDGE('',*,*,#41488,.T.);
#59787=ORIENTED_EDGE('',*,*,#41486,.T.);
#59788=ORIENTED_EDGE('',*,*,#41836,.T.);
#59789=ORIENTED_EDGE('',*,*,#41838,.F.);
#59790=ORIENTED_EDGE('',*,*,#41839,.F.);
#59791=ORIENTED_EDGE('',*,*,#41492,.T.);
#59792=ORIENTED_EDGE('',*,*,#41491,.T.);
#59793=ORIENTED_EDGE('',*,*,#41840,.F.);
#59794=ORIENTED_EDGE('',*,*,#41495,.T.);
#59795=ORIENTED_EDGE('',*,*,#41493,.T.);
#59796=ORIENTED_EDGE('',*,*,#41839,.T.);
#59797=ORIENTED_EDGE('',*,*,#41841,.F.);
#59798=ORIENTED_EDGE('',*,*,#41842,.F.);
#59799=ORIENTED_EDGE('',*,*,#41499,.T.);
#59800=ORIENTED_EDGE('',*,*,#41498,.T.);
#59801=ORIENTED_EDGE('',*,*,#41843,.F.);
#59802=ORIENTED_EDGE('',*,*,#41502,.T.);
#59803=ORIENTED_EDGE('',*,*,#41500,.T.);
#59804=ORIENTED_EDGE('',*,*,#41842,.T.);
#59805=ORIENTED_EDGE('',*,*,#41844,.F.);
#59806=ORIENTED_EDGE('',*,*,#41845,.F.);
#59807=ORIENTED_EDGE('',*,*,#41506,.T.);
#59808=ORIENTED_EDGE('',*,*,#41505,.T.);
#59809=ORIENTED_EDGE('',*,*,#41846,.F.);
#59810=ORIENTED_EDGE('',*,*,#41509,.T.);
#59811=ORIENTED_EDGE('',*,*,#41507,.T.);
#59812=ORIENTED_EDGE('',*,*,#41845,.T.);
#59813=ORIENTED_EDGE('',*,*,#41847,.F.);
#59814=ORIENTED_EDGE('',*,*,#41848,.F.);
#59815=ORIENTED_EDGE('',*,*,#41513,.T.);
#59816=ORIENTED_EDGE('',*,*,#41512,.T.);
#59817=ORIENTED_EDGE('',*,*,#41849,.F.);
#59818=ORIENTED_EDGE('',*,*,#41516,.T.);
#59819=ORIENTED_EDGE('',*,*,#41514,.T.);
#59820=ORIENTED_EDGE('',*,*,#41848,.T.);
#59821=ORIENTED_EDGE('',*,*,#41850,.F.);
#59822=ORIENTED_EDGE('',*,*,#41851,.F.);
#59823=ORIENTED_EDGE('',*,*,#41520,.T.);
#59824=ORIENTED_EDGE('',*,*,#41519,.T.);
#59825=ORIENTED_EDGE('',*,*,#41852,.F.);
#59826=ORIENTED_EDGE('',*,*,#41523,.T.);
#59827=ORIENTED_EDGE('',*,*,#41521,.T.);
#59828=ORIENTED_EDGE('',*,*,#41851,.T.);
#59829=ORIENTED_EDGE('',*,*,#41853,.F.);
#59830=ORIENTED_EDGE('',*,*,#41854,.F.);
#59831=ORIENTED_EDGE('',*,*,#41529,.T.);
#59832=ORIENTED_EDGE('',*,*,#41526,.T.);
#59833=ORIENTED_EDGE('',*,*,#41530,.T.);
#59834=ORIENTED_EDGE('',*,*,#41854,.T.);
#59835=ORIENTED_EDGE('',*,*,#41855,.F.);
#59836=ORIENTED_EDGE('',*,*,#41528,.T.);
#59837=ORIENTED_EDGE('',*,*,#41535,.T.);
#59838=ORIENTED_EDGE('',*,*,#41531,.T.);
#59839=ORIENTED_EDGE('',*,*,#41856,.F.);
#59840=ORIENTED_EDGE('',*,*,#41857,.F.);
#59841=ORIENTED_EDGE('',*,*,#41858,.F.);
#59842=ORIENTED_EDGE('',*,*,#41537,.T.);
#59843=ORIENTED_EDGE('',*,*,#41536,.T.);
#59844=ORIENTED_EDGE('',*,*,#41857,.T.);
#59845=ORIENTED_EDGE('',*,*,#41859,.F.);
#59846=ORIENTED_EDGE('',*,*,#41860,.F.);
#59847=ORIENTED_EDGE('',*,*,#41541,.T.);
#59848=ORIENTED_EDGE('',*,*,#41540,.T.);
#59849=ORIENTED_EDGE('',*,*,#41861,.F.);
#59850=ORIENTED_EDGE('',*,*,#41544,.T.);
#59851=ORIENTED_EDGE('',*,*,#41542,.T.);
#59852=ORIENTED_EDGE('',*,*,#41860,.T.);
#59853=ORIENTED_EDGE('',*,*,#41862,.F.);
#59854=ORIENTED_EDGE('',*,*,#41863,.F.);
#59855=ORIENTED_EDGE('',*,*,#41548,.T.);
#59856=ORIENTED_EDGE('',*,*,#41547,.T.);
#59857=ORIENTED_EDGE('',*,*,#41864,.F.);
#59858=ORIENTED_EDGE('',*,*,#41551,.T.);
#59859=ORIENTED_EDGE('',*,*,#41549,.T.);
#59860=ORIENTED_EDGE('',*,*,#41863,.T.);
#59861=ORIENTED_EDGE('',*,*,#41865,.F.);
#59862=ORIENTED_EDGE('',*,*,#41866,.F.);
#59863=ORIENTED_EDGE('',*,*,#41555,.T.);
#59864=ORIENTED_EDGE('',*,*,#41554,.T.);
#59865=ORIENTED_EDGE('',*,*,#41867,.F.);
#59866=ORIENTED_EDGE('',*,*,#41558,.T.);
#59867=ORIENTED_EDGE('',*,*,#41556,.T.);
#59868=ORIENTED_EDGE('',*,*,#41866,.T.);
#59869=ORIENTED_EDGE('',*,*,#41868,.F.);
#59870=ORIENTED_EDGE('',*,*,#41869,.F.);
#59871=ORIENTED_EDGE('',*,*,#41562,.T.);
#59872=ORIENTED_EDGE('',*,*,#41561,.T.);
#59873=ORIENTED_EDGE('',*,*,#41870,.F.);
#59874=ORIENTED_EDGE('',*,*,#41565,.T.);
#59875=ORIENTED_EDGE('',*,*,#41563,.T.);
#59876=ORIENTED_EDGE('',*,*,#41869,.T.);
#59877=ORIENTED_EDGE('',*,*,#41871,.F.);
#59878=ORIENTED_EDGE('',*,*,#41872,.F.);
#59879=ORIENTED_EDGE('',*,*,#41569,.T.);
#59880=ORIENTED_EDGE('',*,*,#41568,.T.);
#59881=ORIENTED_EDGE('',*,*,#41873,.F.);
#59882=ORIENTED_EDGE('',*,*,#41572,.T.);
#59883=ORIENTED_EDGE('',*,*,#41570,.T.);
#59884=ORIENTED_EDGE('',*,*,#41872,.T.);
#59885=ORIENTED_EDGE('',*,*,#41874,.F.);
#59886=ORIENTED_EDGE('',*,*,#41875,.F.);
#59887=ORIENTED_EDGE('',*,*,#41576,.T.);
#59888=ORIENTED_EDGE('',*,*,#41575,.T.);
#59889=ORIENTED_EDGE('',*,*,#41876,.F.);
#59890=ORIENTED_EDGE('',*,*,#41579,.T.);
#59891=ORIENTED_EDGE('',*,*,#41577,.T.);
#59892=ORIENTED_EDGE('',*,*,#41875,.T.);
#59893=ORIENTED_EDGE('',*,*,#41877,.F.);
#59894=ORIENTED_EDGE('',*,*,#41878,.F.);
#59895=ORIENTED_EDGE('',*,*,#41583,.T.);
#59896=ORIENTED_EDGE('',*,*,#41582,.T.);
#59897=ORIENTED_EDGE('',*,*,#41879,.F.);
#59898=ORIENTED_EDGE('',*,*,#41586,.T.);
#59899=ORIENTED_EDGE('',*,*,#41584,.T.);
#59900=ORIENTED_EDGE('',*,*,#41878,.T.);
#59901=ORIENTED_EDGE('',*,*,#41880,.F.);
#59902=ORIENTED_EDGE('',*,*,#41881,.F.);
#59903=ORIENTED_EDGE('',*,*,#41590,.T.);
#59904=ORIENTED_EDGE('',*,*,#41589,.T.);
#59905=ORIENTED_EDGE('',*,*,#41882,.F.);
#59906=ORIENTED_EDGE('',*,*,#41593,.T.);
#59907=ORIENTED_EDGE('',*,*,#41591,.T.);
#59908=ORIENTED_EDGE('',*,*,#41881,.T.);
#59909=ORIENTED_EDGE('',*,*,#41883,.F.);
#59910=ORIENTED_EDGE('',*,*,#41798,.T.);
#59911=ORIENTED_EDGE('',*,*,#41594,.T.);
#59912=ORIENTED_EDGE('',*,*,#41597,.T.);
#59913=ORIENTED_EDGE('',*,*,#41795,.T.);
#59914=ORIENTED_EDGE('',*,*,#41884,.F.);
#59915=ORIENTED_EDGE('',*,*,#41885,.F.);
#59916=ORIENTED_EDGE('',*,*,#41600,.T.);
#59917=ORIENTED_EDGE('',*,*,#41606,.T.);
#59918=ORIENTED_EDGE('',*,*,#41601,.T.);
#59919=ORIENTED_EDGE('',*,*,#41886,.F.);
#59920=ORIENTED_EDGE('',*,*,#41887,.F.);
#59921=ORIENTED_EDGE('',*,*,#41607,.T.);
#59922=ORIENTED_EDGE('',*,*,#41887,.T.);
#59923=ORIENTED_EDGE('',*,*,#41888,.F.);
#59924=ORIENTED_EDGE('',*,*,#41605,.T.);
#59925=ORIENTED_EDGE('',*,*,#41613,.T.);
#59926=ORIENTED_EDGE('',*,*,#41608,.T.);
#59927=ORIENTED_EDGE('',*,*,#41889,.F.);
#59928=ORIENTED_EDGE('',*,*,#41890,.F.);
#59929=ORIENTED_EDGE('',*,*,#41614,.T.);
#59930=ORIENTED_EDGE('',*,*,#41890,.T.);
#59931=ORIENTED_EDGE('',*,*,#41891,.F.);
#59932=ORIENTED_EDGE('',*,*,#41612,.T.);
#59933=ORIENTED_EDGE('',*,*,#41620,.T.);
#59934=ORIENTED_EDGE('',*,*,#41615,.T.);
#59935=ORIENTED_EDGE('',*,*,#41892,.F.);
#59936=ORIENTED_EDGE('',*,*,#41893,.F.);
#59937=ORIENTED_EDGE('',*,*,#41621,.T.);
#59938=ORIENTED_EDGE('',*,*,#41893,.T.);
#59939=ORIENTED_EDGE('',*,*,#41894,.F.);
#59940=ORIENTED_EDGE('',*,*,#41619,.T.);
#59941=ORIENTED_EDGE('',*,*,#41627,.T.);
#59942=ORIENTED_EDGE('',*,*,#41622,.T.);
#59943=ORIENTED_EDGE('',*,*,#41895,.F.);
#59944=ORIENTED_EDGE('',*,*,#41896,.F.);
#59945=ORIENTED_EDGE('',*,*,#41628,.T.);
#59946=ORIENTED_EDGE('',*,*,#41896,.T.);
#59947=ORIENTED_EDGE('',*,*,#41897,.F.);
#59948=ORIENTED_EDGE('',*,*,#41626,.T.);
#59949=ORIENTED_EDGE('',*,*,#41634,.T.);
#59950=ORIENTED_EDGE('',*,*,#41629,.T.);
#59951=ORIENTED_EDGE('',*,*,#41898,.F.);
#59952=ORIENTED_EDGE('',*,*,#41899,.F.);
#59953=ORIENTED_EDGE('',*,*,#41635,.T.);
#59954=ORIENTED_EDGE('',*,*,#41899,.T.);
#59955=ORIENTED_EDGE('',*,*,#41900,.F.);
#59956=ORIENTED_EDGE('',*,*,#41633,.T.);
#59957=ORIENTED_EDGE('',*,*,#41641,.T.);
#59958=ORIENTED_EDGE('',*,*,#41636,.T.);
#59959=ORIENTED_EDGE('',*,*,#41901,.F.);
#59960=ORIENTED_EDGE('',*,*,#41902,.F.);
#59961=ORIENTED_EDGE('',*,*,#41642,.T.);
#59962=ORIENTED_EDGE('',*,*,#41902,.T.);
#59963=ORIENTED_EDGE('',*,*,#41903,.F.);
#59964=ORIENTED_EDGE('',*,*,#41640,.T.);
#59965=ORIENTED_EDGE('',*,*,#41648,.T.);
#59966=ORIENTED_EDGE('',*,*,#41643,.T.);
#59967=ORIENTED_EDGE('',*,*,#41904,.F.);
#59968=ORIENTED_EDGE('',*,*,#41905,.F.);
#59969=ORIENTED_EDGE('',*,*,#41649,.T.);
#59970=ORIENTED_EDGE('',*,*,#41905,.T.);
#59971=ORIENTED_EDGE('',*,*,#41906,.F.);
#59972=ORIENTED_EDGE('',*,*,#41647,.T.);
#59973=ORIENTED_EDGE('',*,*,#41655,.T.);
#59974=ORIENTED_EDGE('',*,*,#41650,.T.);
#59975=ORIENTED_EDGE('',*,*,#41907,.F.);
#59976=ORIENTED_EDGE('',*,*,#41908,.F.);
#59977=ORIENTED_EDGE('',*,*,#41656,.T.);
#59978=ORIENTED_EDGE('',*,*,#41908,.T.);
#59979=ORIENTED_EDGE('',*,*,#41909,.F.);
#59980=ORIENTED_EDGE('',*,*,#41654,.T.);
#59981=ORIENTED_EDGE('',*,*,#41662,.T.);
#59982=ORIENTED_EDGE('',*,*,#41657,.T.);
#59983=ORIENTED_EDGE('',*,*,#41910,.F.);
#59984=ORIENTED_EDGE('',*,*,#41911,.F.);
#59985=ORIENTED_EDGE('',*,*,#41663,.T.);
#59986=ORIENTED_EDGE('',*,*,#41911,.T.);
#59987=ORIENTED_EDGE('',*,*,#41912,.F.);
#59988=ORIENTED_EDGE('',*,*,#41661,.T.);
#59989=ORIENTED_EDGE('',*,*,#41669,.T.);
#59990=ORIENTED_EDGE('',*,*,#41664,.T.);
#59991=ORIENTED_EDGE('',*,*,#41913,.F.);
#59992=ORIENTED_EDGE('',*,*,#41914,.F.);
#59993=ORIENTED_EDGE('',*,*,#41670,.T.);
#59994=ORIENTED_EDGE('',*,*,#41914,.T.);
#59995=ORIENTED_EDGE('',*,*,#41915,.F.);
#59996=ORIENTED_EDGE('',*,*,#41668,.T.);
#59997=ORIENTED_EDGE('',*,*,#41676,.T.);
#59998=ORIENTED_EDGE('',*,*,#41671,.T.);
#59999=ORIENTED_EDGE('',*,*,#41916,.F.);
#60000=ORIENTED_EDGE('',*,*,#41917,.F.);
#60001=ORIENTED_EDGE('',*,*,#41677,.T.);
#60002=ORIENTED_EDGE('',*,*,#41917,.T.);
#60003=ORIENTED_EDGE('',*,*,#41918,.F.);
#60004=ORIENTED_EDGE('',*,*,#41675,.T.);
#60005=ORIENTED_EDGE('',*,*,#41683,.T.);
#60006=ORIENTED_EDGE('',*,*,#41678,.T.);
#60007=ORIENTED_EDGE('',*,*,#41919,.F.);
#60008=ORIENTED_EDGE('',*,*,#41920,.F.);
#60009=ORIENTED_EDGE('',*,*,#41684,.T.);
#60010=ORIENTED_EDGE('',*,*,#41920,.T.);
#60011=ORIENTED_EDGE('',*,*,#41921,.F.);
#60012=ORIENTED_EDGE('',*,*,#41682,.T.);
#60013=ORIENTED_EDGE('',*,*,#41690,.T.);
#60014=ORIENTED_EDGE('',*,*,#41685,.T.);
#60015=ORIENTED_EDGE('',*,*,#41922,.F.);
#60016=ORIENTED_EDGE('',*,*,#41923,.F.);
#60017=ORIENTED_EDGE('',*,*,#41691,.T.);
#60018=ORIENTED_EDGE('',*,*,#41923,.T.);
#60019=ORIENTED_EDGE('',*,*,#41924,.F.);
#60020=ORIENTED_EDGE('',*,*,#41689,.T.);
#60021=ORIENTED_EDGE('',*,*,#34376,.T.);
#60022=ORIENTED_EDGE('',*,*,#41692,.T.);
#60023=ORIENTED_EDGE('',*,*,#41925,.F.);
#60024=ORIENTED_EDGE('',*,*,#41926,.F.);
#60025=ORIENTED_EDGE('',*,*,#34373,.T.);
#60026=ORIENTED_EDGE('',*,*,#41926,.T.);
#60027=ORIENTED_EDGE('',*,*,#41927,.F.);
#60028=ORIENTED_EDGE('',*,*,#41694,.T.);
#60029=ORIENTED_EDGE('',*,*,#41700,.T.);
#60030=ORIENTED_EDGE('',*,*,#41695,.T.);
#60031=ORIENTED_EDGE('',*,*,#41928,.F.);
#60032=ORIENTED_EDGE('',*,*,#41929,.F.);
#60033=ORIENTED_EDGE('',*,*,#41701,.T.);
#60034=ORIENTED_EDGE('',*,*,#41929,.T.);
#60035=ORIENTED_EDGE('',*,*,#41930,.F.);
#60036=ORIENTED_EDGE('',*,*,#41699,.T.);
#60037=ORIENTED_EDGE('',*,*,#41707,.T.);
#60038=ORIENTED_EDGE('',*,*,#41702,.T.);
#60039=ORIENTED_EDGE('',*,*,#41931,.F.);
#60040=ORIENTED_EDGE('',*,*,#41932,.F.);
#60041=ORIENTED_EDGE('',*,*,#41708,.T.);
#60042=ORIENTED_EDGE('',*,*,#41932,.T.);
#60043=ORIENTED_EDGE('',*,*,#41933,.F.);
#60044=ORIENTED_EDGE('',*,*,#41706,.T.);
#60045=ORIENTED_EDGE('',*,*,#41714,.T.);
#60046=ORIENTED_EDGE('',*,*,#41709,.T.);
#60047=ORIENTED_EDGE('',*,*,#41934,.F.);
#60048=ORIENTED_EDGE('',*,*,#41935,.F.);
#60049=ORIENTED_EDGE('',*,*,#41715,.T.);
#60050=ORIENTED_EDGE('',*,*,#41935,.T.);
#60051=ORIENTED_EDGE('',*,*,#41936,.F.);
#60052=ORIENTED_EDGE('',*,*,#41713,.T.);
#60053=ORIENTED_EDGE('',*,*,#41721,.T.);
#60054=ORIENTED_EDGE('',*,*,#41716,.T.);
#60055=ORIENTED_EDGE('',*,*,#41937,.F.);
#60056=ORIENTED_EDGE('',*,*,#41938,.F.);
#60057=ORIENTED_EDGE('',*,*,#41722,.T.);
#60058=ORIENTED_EDGE('',*,*,#41938,.T.);
#60059=ORIENTED_EDGE('',*,*,#41939,.F.);
#60060=ORIENTED_EDGE('',*,*,#41720,.T.);
#60061=ORIENTED_EDGE('',*,*,#41728,.T.);
#60062=ORIENTED_EDGE('',*,*,#41723,.T.);
#60063=ORIENTED_EDGE('',*,*,#41940,.F.);
#60064=ORIENTED_EDGE('',*,*,#41941,.F.);
#60065=ORIENTED_EDGE('',*,*,#41729,.T.);
#60066=ORIENTED_EDGE('',*,*,#41941,.T.);
#60067=ORIENTED_EDGE('',*,*,#41942,.F.);
#60068=ORIENTED_EDGE('',*,*,#41727,.T.);
#60069=ORIENTED_EDGE('',*,*,#41735,.T.);
#60070=ORIENTED_EDGE('',*,*,#41730,.T.);
#60071=ORIENTED_EDGE('',*,*,#41943,.F.);
#60072=ORIENTED_EDGE('',*,*,#41944,.F.);
#60073=ORIENTED_EDGE('',*,*,#41736,.T.);
#60074=ORIENTED_EDGE('',*,*,#41944,.T.);
#60075=ORIENTED_EDGE('',*,*,#41945,.F.);
#60076=ORIENTED_EDGE('',*,*,#41734,.T.);
#60077=ORIENTED_EDGE('',*,*,#41742,.T.);
#60078=ORIENTED_EDGE('',*,*,#41737,.T.);
#60079=ORIENTED_EDGE('',*,*,#41946,.F.);
#60080=ORIENTED_EDGE('',*,*,#41947,.F.);
#60081=ORIENTED_EDGE('',*,*,#41743,.T.);
#60082=ORIENTED_EDGE('',*,*,#41947,.T.);
#60083=ORIENTED_EDGE('',*,*,#41948,.F.);
#60084=ORIENTED_EDGE('',*,*,#41741,.T.);
#60085=ORIENTED_EDGE('',*,*,#41749,.T.);
#60086=ORIENTED_EDGE('',*,*,#41744,.T.);
#60087=ORIENTED_EDGE('',*,*,#41949,.F.);
#60088=ORIENTED_EDGE('',*,*,#41950,.F.);
#60089=ORIENTED_EDGE('',*,*,#41750,.T.);
#60090=ORIENTED_EDGE('',*,*,#41950,.T.);
#60091=ORIENTED_EDGE('',*,*,#41951,.F.);
#60092=ORIENTED_EDGE('',*,*,#41748,.T.);
#60093=ORIENTED_EDGE('',*,*,#41756,.T.);
#60094=ORIENTED_EDGE('',*,*,#41751,.T.);
#60095=ORIENTED_EDGE('',*,*,#41952,.F.);
#60096=ORIENTED_EDGE('',*,*,#41953,.F.);
#60097=ORIENTED_EDGE('',*,*,#41757,.T.);
#60098=ORIENTED_EDGE('',*,*,#41953,.T.);
#60099=ORIENTED_EDGE('',*,*,#41954,.F.);
#60100=ORIENTED_EDGE('',*,*,#41755,.T.);
#60101=ORIENTED_EDGE('',*,*,#41763,.T.);
#60102=ORIENTED_EDGE('',*,*,#41758,.T.);
#60103=ORIENTED_EDGE('',*,*,#41955,.F.);
#60104=ORIENTED_EDGE('',*,*,#41956,.F.);
#60105=ORIENTED_EDGE('',*,*,#41764,.T.);
#60106=ORIENTED_EDGE('',*,*,#41956,.T.);
#60107=ORIENTED_EDGE('',*,*,#41957,.F.);
#60108=ORIENTED_EDGE('',*,*,#41762,.T.);
#60109=ORIENTED_EDGE('',*,*,#41958,.F.);
#60110=ORIENTED_EDGE('',*,*,#41959,.F.);
#60111=ORIENTED_EDGE('',*,*,#41770,.T.);
#60112=ORIENTED_EDGE('',*,*,#41765,.T.);
#60113=ORIENTED_EDGE('',*,*,#41771,.T.);
#60114=ORIENTED_EDGE('',*,*,#41959,.T.);
#60115=ORIENTED_EDGE('',*,*,#41960,.F.);
#60116=ORIENTED_EDGE('',*,*,#41769,.T.);
#60117=ORIENTED_EDGE('',*,*,#41777,.T.);
#60118=ORIENTED_EDGE('',*,*,#41772,.T.);
#60119=ORIENTED_EDGE('',*,*,#41961,.F.);
#60120=ORIENTED_EDGE('',*,*,#41962,.F.);
#60121=ORIENTED_EDGE('',*,*,#41778,.T.);
#60122=ORIENTED_EDGE('',*,*,#41962,.T.);
#60123=ORIENTED_EDGE('',*,*,#41963,.F.);
#60124=ORIENTED_EDGE('',*,*,#41776,.T.);
#60125=ORIENTED_EDGE('',*,*,#41784,.T.);
#60126=ORIENTED_EDGE('',*,*,#41779,.T.);
#60127=ORIENTED_EDGE('',*,*,#41964,.F.);
#60128=ORIENTED_EDGE('',*,*,#41965,.F.);
#60129=ORIENTED_EDGE('',*,*,#41785,.T.);
#60130=ORIENTED_EDGE('',*,*,#41965,.T.);
#60131=ORIENTED_EDGE('',*,*,#41966,.F.);
#60132=ORIENTED_EDGE('',*,*,#41783,.T.);
#60133=ORIENTED_EDGE('',*,*,#41791,.T.);
#60134=ORIENTED_EDGE('',*,*,#41786,.T.);
#60135=ORIENTED_EDGE('',*,*,#41967,.F.);
#60136=ORIENTED_EDGE('',*,*,#41968,.F.);
#60137=ORIENTED_EDGE('',*,*,#41792,.T.);
#60138=ORIENTED_EDGE('',*,*,#41968,.T.);
#60139=ORIENTED_EDGE('',*,*,#41969,.F.);
#60140=ORIENTED_EDGE('',*,*,#41790,.T.);
#60141=ORIENTED_EDGE('',*,*,#41794,.T.);
#60142=ORIENTED_EDGE('',*,*,#41796,.T.);
#60143=ORIENTED_EDGE('',*,*,#41970,.F.);
#60144=ORIENTED_EDGE('',*,*,#41884,.T.);
#60145=ORIENTED_EDGE('',*,*,#41971,.T.);
#60146=ORIENTED_EDGE('',*,*,#41972,.F.);
#60147=ORIENTED_EDGE('',*,*,#41797,.T.);
#60148=ORIENTED_EDGE('',*,*,#41973,.F.);
#60149=ORIENTED_EDGE('',*,*,#41974,.F.);
#60150=ORIENTED_EDGE('',*,*,#41975,.F.);
#60151=ORIENTED_EDGE('',*,*,#41976,.F.);
#60152=ORIENTED_EDGE('',*,*,#41971,.F.);
#60153=ORIENTED_EDGE('',*,*,#41976,.T.);
#60154=ORIENTED_EDGE('',*,*,#41977,.F.);
#60155=ORIENTED_EDGE('',*,*,#41799,.T.);
#60156=ORIENTED_EDGE('',*,*,#41972,.T.);
#60157=ORIENTED_EDGE('',*,*,#41978,.T.);
#60158=ORIENTED_EDGE('',*,*,#41979,.F.);
#60159=ORIENTED_EDGE('',*,*,#41801,.T.);
#60160=ORIENTED_EDGE('',*,*,#41980,.F.);
#60161=ORIENTED_EDGE('',*,*,#41981,.F.);
#60162=ORIENTED_EDGE('',*,*,#41982,.F.);
#60163=ORIENTED_EDGE('',*,*,#41983,.F.);
#60164=ORIENTED_EDGE('',*,*,#41978,.F.);
#60165=ORIENTED_EDGE('',*,*,#41983,.T.);
#60166=ORIENTED_EDGE('',*,*,#41984,.F.);
#60167=ORIENTED_EDGE('',*,*,#41802,.T.);
#60168=ORIENTED_EDGE('',*,*,#41979,.T.);
#60169=ORIENTED_EDGE('',*,*,#41985,.T.);
#60170=ORIENTED_EDGE('',*,*,#41986,.F.);
#60171=ORIENTED_EDGE('',*,*,#41804,.T.);
#60172=ORIENTED_EDGE('',*,*,#41987,.F.);
#60173=ORIENTED_EDGE('',*,*,#41988,.F.);
#60174=ORIENTED_EDGE('',*,*,#41989,.F.);
#60175=ORIENTED_EDGE('',*,*,#41990,.F.);
#60176=ORIENTED_EDGE('',*,*,#41985,.F.);
#60177=ORIENTED_EDGE('',*,*,#41990,.T.);
#60178=ORIENTED_EDGE('',*,*,#41991,.F.);
#60179=ORIENTED_EDGE('',*,*,#41805,.T.);
#60180=ORIENTED_EDGE('',*,*,#41986,.T.);
#60181=ORIENTED_EDGE('',*,*,#41992,.T.);
#60182=ORIENTED_EDGE('',*,*,#41993,.F.);
#60183=ORIENTED_EDGE('',*,*,#41807,.T.);
#60184=ORIENTED_EDGE('',*,*,#41994,.F.);
#60185=ORIENTED_EDGE('',*,*,#41995,.F.);
#60186=ORIENTED_EDGE('',*,*,#41996,.F.);
#60187=ORIENTED_EDGE('',*,*,#41997,.F.);
#60188=ORIENTED_EDGE('',*,*,#41992,.F.);
#60189=ORIENTED_EDGE('',*,*,#41997,.T.);
#60190=ORIENTED_EDGE('',*,*,#41998,.F.);
#60191=ORIENTED_EDGE('',*,*,#41808,.T.);
#60192=ORIENTED_EDGE('',*,*,#41993,.T.);
#60193=ORIENTED_EDGE('',*,*,#41999,.T.);
#60194=ORIENTED_EDGE('',*,*,#42000,.F.);
#60195=ORIENTED_EDGE('',*,*,#41810,.T.);
#60196=ORIENTED_EDGE('',*,*,#42001,.F.);
#60197=ORIENTED_EDGE('',*,*,#42002,.F.);
#60198=ORIENTED_EDGE('',*,*,#42003,.F.);
#60199=ORIENTED_EDGE('',*,*,#42004,.F.);
#60200=ORIENTED_EDGE('',*,*,#41999,.F.);
#60201=ORIENTED_EDGE('',*,*,#42004,.T.);
#60202=ORIENTED_EDGE('',*,*,#42005,.F.);
#60203=ORIENTED_EDGE('',*,*,#41811,.T.);
#60204=ORIENTED_EDGE('',*,*,#42000,.T.);
#60205=ORIENTED_EDGE('',*,*,#42006,.T.);
#60206=ORIENTED_EDGE('',*,*,#42007,.F.);
#60207=ORIENTED_EDGE('',*,*,#41813,.T.);
#60208=ORIENTED_EDGE('',*,*,#42008,.F.);
#60209=ORIENTED_EDGE('',*,*,#42009,.F.);
#60210=ORIENTED_EDGE('',*,*,#42010,.F.);
#60211=ORIENTED_EDGE('',*,*,#42011,.F.);
#60212=ORIENTED_EDGE('',*,*,#42006,.F.);
#60213=ORIENTED_EDGE('',*,*,#42011,.T.);
#60214=ORIENTED_EDGE('',*,*,#42012,.F.);
#60215=ORIENTED_EDGE('',*,*,#41814,.T.);
#60216=ORIENTED_EDGE('',*,*,#42007,.T.);
#60217=ORIENTED_EDGE('',*,*,#42013,.T.);
#60218=ORIENTED_EDGE('',*,*,#42014,.F.);
#60219=ORIENTED_EDGE('',*,*,#41816,.T.);
#60220=ORIENTED_EDGE('',*,*,#42015,.F.);
#60221=ORIENTED_EDGE('',*,*,#42016,.F.);
#60222=ORIENTED_EDGE('',*,*,#42017,.F.);
#60223=ORIENTED_EDGE('',*,*,#42018,.F.);
#60224=ORIENTED_EDGE('',*,*,#42013,.F.);
#60225=ORIENTED_EDGE('',*,*,#42018,.T.);
#60226=ORIENTED_EDGE('',*,*,#42019,.F.);
#60227=ORIENTED_EDGE('',*,*,#41817,.T.);
#60228=ORIENTED_EDGE('',*,*,#42014,.T.);
#60229=ORIENTED_EDGE('',*,*,#42020,.T.);
#60230=ORIENTED_EDGE('',*,*,#42021,.F.);
#60231=ORIENTED_EDGE('',*,*,#41819,.T.);
#60232=ORIENTED_EDGE('',*,*,#42022,.F.);
#60233=ORIENTED_EDGE('',*,*,#42023,.F.);
#60234=ORIENTED_EDGE('',*,*,#42024,.F.);
#60235=ORIENTED_EDGE('',*,*,#42025,.F.);
#60236=ORIENTED_EDGE('',*,*,#42020,.F.);
#60237=ORIENTED_EDGE('',*,*,#42025,.T.);
#60238=ORIENTED_EDGE('',*,*,#42026,.F.);
#60239=ORIENTED_EDGE('',*,*,#41820,.T.);
#60240=ORIENTED_EDGE('',*,*,#42021,.T.);
#60241=ORIENTED_EDGE('',*,*,#42027,.T.);
#60242=ORIENTED_EDGE('',*,*,#42028,.F.);
#60243=ORIENTED_EDGE('',*,*,#41822,.T.);
#60244=ORIENTED_EDGE('',*,*,#42029,.F.);
#60245=ORIENTED_EDGE('',*,*,#42030,.F.);
#60246=ORIENTED_EDGE('',*,*,#42031,.F.);
#60247=ORIENTED_EDGE('',*,*,#42032,.F.);
#60248=ORIENTED_EDGE('',*,*,#42027,.F.);
#60249=ORIENTED_EDGE('',*,*,#42032,.T.);
#60250=ORIENTED_EDGE('',*,*,#42033,.F.);
#60251=ORIENTED_EDGE('',*,*,#41823,.T.);
#60252=ORIENTED_EDGE('',*,*,#42028,.T.);
#60253=ORIENTED_EDGE('',*,*,#42034,.T.);
#60254=ORIENTED_EDGE('',*,*,#42035,.F.);
#60255=ORIENTED_EDGE('',*,*,#41825,.T.);
#60256=ORIENTED_EDGE('',*,*,#42036,.F.);
#60257=ORIENTED_EDGE('',*,*,#42037,.F.);
#60258=ORIENTED_EDGE('',*,*,#42038,.F.);
#60259=ORIENTED_EDGE('',*,*,#42039,.F.);
#60260=ORIENTED_EDGE('',*,*,#42034,.F.);
#60261=ORIENTED_EDGE('',*,*,#42039,.T.);
#60262=ORIENTED_EDGE('',*,*,#42040,.F.);
#60263=ORIENTED_EDGE('',*,*,#41826,.T.);
#60264=ORIENTED_EDGE('',*,*,#42035,.T.);
#60265=ORIENTED_EDGE('',*,*,#42041,.T.);
#60266=ORIENTED_EDGE('',*,*,#42042,.F.);
#60267=ORIENTED_EDGE('',*,*,#41828,.T.);
#60268=ORIENTED_EDGE('',*,*,#42043,.F.);
#60269=ORIENTED_EDGE('',*,*,#42044,.F.);
#60270=ORIENTED_EDGE('',*,*,#42045,.F.);
#60271=ORIENTED_EDGE('',*,*,#42046,.F.);
#60272=ORIENTED_EDGE('',*,*,#42041,.F.);
#60273=ORIENTED_EDGE('',*,*,#42046,.T.);
#60274=ORIENTED_EDGE('',*,*,#42047,.F.);
#60275=ORIENTED_EDGE('',*,*,#41829,.T.);
#60276=ORIENTED_EDGE('',*,*,#42042,.T.);
#60277=ORIENTED_EDGE('',*,*,#42048,.T.);
#60278=ORIENTED_EDGE('',*,*,#42049,.F.);
#60279=ORIENTED_EDGE('',*,*,#41831,.T.);
#60280=ORIENTED_EDGE('',*,*,#42050,.F.);
#60281=ORIENTED_EDGE('',*,*,#42051,.F.);
#60282=ORIENTED_EDGE('',*,*,#42052,.F.);
#60283=ORIENTED_EDGE('',*,*,#42053,.F.);
#60284=ORIENTED_EDGE('',*,*,#42048,.F.);
#60285=ORIENTED_EDGE('',*,*,#42053,.T.);
#60286=ORIENTED_EDGE('',*,*,#42054,.F.);
#60287=ORIENTED_EDGE('',*,*,#41832,.T.);
#60288=ORIENTED_EDGE('',*,*,#42049,.T.);
#60289=ORIENTED_EDGE('',*,*,#42055,.T.);
#60290=ORIENTED_EDGE('',*,*,#42056,.F.);
#60291=ORIENTED_EDGE('',*,*,#41834,.T.);
#60292=ORIENTED_EDGE('',*,*,#42057,.F.);
#60293=ORIENTED_EDGE('',*,*,#42058,.F.);
#60294=ORIENTED_EDGE('',*,*,#42059,.F.);
#60295=ORIENTED_EDGE('',*,*,#42060,.F.);
#60296=ORIENTED_EDGE('',*,*,#42055,.F.);
#60297=ORIENTED_EDGE('',*,*,#42060,.T.);
#60298=ORIENTED_EDGE('',*,*,#42061,.F.);
#60299=ORIENTED_EDGE('',*,*,#41835,.T.);
#60300=ORIENTED_EDGE('',*,*,#42056,.T.);
#60301=ORIENTED_EDGE('',*,*,#42062,.T.);
#60302=ORIENTED_EDGE('',*,*,#42063,.F.);
#60303=ORIENTED_EDGE('',*,*,#41837,.T.);
#60304=ORIENTED_EDGE('',*,*,#42064,.F.);
#60305=ORIENTED_EDGE('',*,*,#42065,.F.);
#60306=ORIENTED_EDGE('',*,*,#42066,.F.);
#60307=ORIENTED_EDGE('',*,*,#42067,.F.);
#60308=ORIENTED_EDGE('',*,*,#42062,.F.);
#60309=ORIENTED_EDGE('',*,*,#42067,.T.);
#60310=ORIENTED_EDGE('',*,*,#42068,.F.);
#60311=ORIENTED_EDGE('',*,*,#41838,.T.);
#60312=ORIENTED_EDGE('',*,*,#42063,.T.);
#60313=ORIENTED_EDGE('',*,*,#34369,.T.);
#60314=ORIENTED_EDGE('',*,*,#42069,.F.);
#60315=ORIENTED_EDGE('',*,*,#41840,.T.);
#60316=ORIENTED_EDGE('',*,*,#42070,.F.);
#60317=ORIENTED_EDGE('',*,*,#34372,.T.);
#60318=ORIENTED_EDGE('',*,*,#42071,.F.);
#60319=ORIENTED_EDGE('',*,*,#41841,.T.);
#60320=ORIENTED_EDGE('',*,*,#42069,.T.);
#60321=ORIENTED_EDGE('',*,*,#42072,.T.);
#60322=ORIENTED_EDGE('',*,*,#42073,.F.);
#60323=ORIENTED_EDGE('',*,*,#41843,.T.);
#60324=ORIENTED_EDGE('',*,*,#42074,.F.);
#60325=ORIENTED_EDGE('',*,*,#42075,.F.);
#60326=ORIENTED_EDGE('',*,*,#42076,.F.);
#60327=ORIENTED_EDGE('',*,*,#42077,.F.);
#60328=ORIENTED_EDGE('',*,*,#42072,.F.);
#60329=ORIENTED_EDGE('',*,*,#42077,.T.);
#60330=ORIENTED_EDGE('',*,*,#42078,.F.);
#60331=ORIENTED_EDGE('',*,*,#41844,.T.);
#60332=ORIENTED_EDGE('',*,*,#42073,.T.);
#60333=ORIENTED_EDGE('',*,*,#42079,.T.);
#60334=ORIENTED_EDGE('',*,*,#42080,.F.);
#60335=ORIENTED_EDGE('',*,*,#41846,.T.);
#60336=ORIENTED_EDGE('',*,*,#42081,.F.);
#60337=ORIENTED_EDGE('',*,*,#42082,.F.);
#60338=ORIENTED_EDGE('',*,*,#42083,.F.);
#60339=ORIENTED_EDGE('',*,*,#42084,.F.);
#60340=ORIENTED_EDGE('',*,*,#42079,.F.);
#60341=ORIENTED_EDGE('',*,*,#42084,.T.);
#60342=ORIENTED_EDGE('',*,*,#42085,.F.);
#60343=ORIENTED_EDGE('',*,*,#41847,.T.);
#60344=ORIENTED_EDGE('',*,*,#42080,.T.);
#60345=ORIENTED_EDGE('',*,*,#42086,.T.);
#60346=ORIENTED_EDGE('',*,*,#42087,.F.);
#60347=ORIENTED_EDGE('',*,*,#41849,.T.);
#60348=ORIENTED_EDGE('',*,*,#42088,.F.);
#60349=ORIENTED_EDGE('',*,*,#42089,.F.);
#60350=ORIENTED_EDGE('',*,*,#42090,.F.);
#60351=ORIENTED_EDGE('',*,*,#42091,.F.);
#60352=ORIENTED_EDGE('',*,*,#42086,.F.);
#60353=ORIENTED_EDGE('',*,*,#42091,.T.);
#60354=ORIENTED_EDGE('',*,*,#42092,.F.);
#60355=ORIENTED_EDGE('',*,*,#41850,.T.);
#60356=ORIENTED_EDGE('',*,*,#42087,.T.);
#60357=ORIENTED_EDGE('',*,*,#42093,.T.);
#60358=ORIENTED_EDGE('',*,*,#42094,.F.);
#60359=ORIENTED_EDGE('',*,*,#41852,.T.);
#60360=ORIENTED_EDGE('',*,*,#42095,.F.);
#60361=ORIENTED_EDGE('',*,*,#42096,.T.);
#60362=ORIENTED_EDGE('',*,*,#42097,.F.);
#60363=ORIENTED_EDGE('',*,*,#41853,.T.);
#60364=ORIENTED_EDGE('',*,*,#42094,.T.);
#60365=ORIENTED_EDGE('',*,*,#42098,.F.);
#60366=ORIENTED_EDGE('',*,*,#42099,.F.);
#60367=ORIENTED_EDGE('',*,*,#42096,.F.);
#60368=ORIENTED_EDGE('',*,*,#42093,.F.);
#60369=ORIENTED_EDGE('',*,*,#41855,.T.);
#60370=ORIENTED_EDGE('',*,*,#42100,.F.);
#60371=ORIENTED_EDGE('',*,*,#42101,.T.);
#60372=ORIENTED_EDGE('',*,*,#42102,.F.);
#60373=ORIENTED_EDGE('',*,*,#42103,.F.);
#60374=ORIENTED_EDGE('',*,*,#42101,.F.);
#60375=ORIENTED_EDGE('',*,*,#42104,.F.);
#60376=ORIENTED_EDGE('',*,*,#42105,.F.);
#60377=ORIENTED_EDGE('',*,*,#41856,.T.);
#60378=ORIENTED_EDGE('',*,*,#42102,.T.);
#60379=ORIENTED_EDGE('',*,*,#42103,.T.);
#60380=ORIENTED_EDGE('',*,*,#42106,.F.);
#60381=ORIENTED_EDGE('',*,*,#42107,.T.);
#60382=ORIENTED_EDGE('',*,*,#42108,.F.);
#60383=ORIENTED_EDGE('',*,*,#41858,.T.);
#60384=ORIENTED_EDGE('',*,*,#42109,.F.);
#60385=ORIENTED_EDGE('',*,*,#42110,.F.);
#60386=ORIENTED_EDGE('',*,*,#42111,.F.);
#60387=ORIENTED_EDGE('',*,*,#42112,.F.);
#60388=ORIENTED_EDGE('',*,*,#42107,.F.);
#60389=ORIENTED_EDGE('',*,*,#42112,.T.);
#60390=ORIENTED_EDGE('',*,*,#42113,.F.);
#60391=ORIENTED_EDGE('',*,*,#41859,.T.);
#60392=ORIENTED_EDGE('',*,*,#42108,.T.);
#60393=ORIENTED_EDGE('',*,*,#42114,.T.);
#60394=ORIENTED_EDGE('',*,*,#42115,.F.);
#60395=ORIENTED_EDGE('',*,*,#41861,.T.);
#60396=ORIENTED_EDGE('',*,*,#42116,.F.);
#60397=ORIENTED_EDGE('',*,*,#42117,.F.);
#60398=ORIENTED_EDGE('',*,*,#42118,.F.);
#60399=ORIENTED_EDGE('',*,*,#42119,.F.);
#60400=ORIENTED_EDGE('',*,*,#42114,.F.);
#60401=ORIENTED_EDGE('',*,*,#42119,.T.);
#60402=ORIENTED_EDGE('',*,*,#42120,.F.);
#60403=ORIENTED_EDGE('',*,*,#41862,.T.);
#60404=ORIENTED_EDGE('',*,*,#42115,.T.);
#60405=ORIENTED_EDGE('',*,*,#42121,.T.);
#60406=ORIENTED_EDGE('',*,*,#42122,.F.);
#60407=ORIENTED_EDGE('',*,*,#41864,.T.);
#60408=ORIENTED_EDGE('',*,*,#42123,.F.);
#60409=ORIENTED_EDGE('',*,*,#42124,.F.);
#60410=ORIENTED_EDGE('',*,*,#42125,.F.);
#60411=ORIENTED_EDGE('',*,*,#42126,.F.);
#60412=ORIENTED_EDGE('',*,*,#42121,.F.);
#60413=ORIENTED_EDGE('',*,*,#42126,.T.);
#60414=ORIENTED_EDGE('',*,*,#42127,.F.);
#60415=ORIENTED_EDGE('',*,*,#41865,.T.);
#60416=ORIENTED_EDGE('',*,*,#42122,.T.);
#60417=ORIENTED_EDGE('',*,*,#42128,.T.);
#60418=ORIENTED_EDGE('',*,*,#42129,.F.);
#60419=ORIENTED_EDGE('',*,*,#41867,.T.);
#60420=ORIENTED_EDGE('',*,*,#42130,.F.);
#60421=ORIENTED_EDGE('',*,*,#42131,.F.);
#60422=ORIENTED_EDGE('',*,*,#42132,.F.);
#60423=ORIENTED_EDGE('',*,*,#42133,.F.);
#60424=ORIENTED_EDGE('',*,*,#42128,.F.);
#60425=ORIENTED_EDGE('',*,*,#42133,.T.);
#60426=ORIENTED_EDGE('',*,*,#42134,.F.);
#60427=ORIENTED_EDGE('',*,*,#41868,.T.);
#60428=ORIENTED_EDGE('',*,*,#42129,.T.);
#60429=ORIENTED_EDGE('',*,*,#42135,.T.);
#60430=ORIENTED_EDGE('',*,*,#42136,.F.);
#60431=ORIENTED_EDGE('',*,*,#41870,.T.);
#60432=ORIENTED_EDGE('',*,*,#42137,.F.);
#60433=ORIENTED_EDGE('',*,*,#42138,.F.);
#60434=ORIENTED_EDGE('',*,*,#42139,.F.);
#60435=ORIENTED_EDGE('',*,*,#42140,.F.);
#60436=ORIENTED_EDGE('',*,*,#42135,.F.);
#60437=ORIENTED_EDGE('',*,*,#42140,.T.);
#60438=ORIENTED_EDGE('',*,*,#42141,.F.);
#60439=ORIENTED_EDGE('',*,*,#41871,.T.);
#60440=ORIENTED_EDGE('',*,*,#42136,.T.);
#60441=ORIENTED_EDGE('',*,*,#42142,.T.);
#60442=ORIENTED_EDGE('',*,*,#42143,.F.);
#60443=ORIENTED_EDGE('',*,*,#41873,.T.);
#60444=ORIENTED_EDGE('',*,*,#42144,.F.);
#60445=ORIENTED_EDGE('',*,*,#42145,.F.);
#60446=ORIENTED_EDGE('',*,*,#42146,.F.);
#60447=ORIENTED_EDGE('',*,*,#42147,.F.);
#60448=ORIENTED_EDGE('',*,*,#42142,.F.);
#60449=ORIENTED_EDGE('',*,*,#42147,.T.);
#60450=ORIENTED_EDGE('',*,*,#42148,.F.);
#60451=ORIENTED_EDGE('',*,*,#41874,.T.);
#60452=ORIENTED_EDGE('',*,*,#42143,.T.);
#60453=ORIENTED_EDGE('',*,*,#42149,.T.);
#60454=ORIENTED_EDGE('',*,*,#42150,.F.);
#60455=ORIENTED_EDGE('',*,*,#41876,.T.);
#60456=ORIENTED_EDGE('',*,*,#42151,.F.);
#60457=ORIENTED_EDGE('',*,*,#42152,.F.);
#60458=ORIENTED_EDGE('',*,*,#42153,.F.);
#60459=ORIENTED_EDGE('',*,*,#42154,.F.);
#60460=ORIENTED_EDGE('',*,*,#42149,.F.);
#60461=ORIENTED_EDGE('',*,*,#42154,.T.);
#60462=ORIENTED_EDGE('',*,*,#42155,.F.);
#60463=ORIENTED_EDGE('',*,*,#41877,.T.);
#60464=ORIENTED_EDGE('',*,*,#42150,.T.);
#60465=ORIENTED_EDGE('',*,*,#42156,.T.);
#60466=ORIENTED_EDGE('',*,*,#42157,.F.);
#60467=ORIENTED_EDGE('',*,*,#41879,.T.);
#60468=ORIENTED_EDGE('',*,*,#42158,.F.);
#60469=ORIENTED_EDGE('',*,*,#42159,.F.);
#60470=ORIENTED_EDGE('',*,*,#42160,.F.);
#60471=ORIENTED_EDGE('',*,*,#42161,.F.);
#60472=ORIENTED_EDGE('',*,*,#42156,.F.);
#60473=ORIENTED_EDGE('',*,*,#42161,.T.);
#60474=ORIENTED_EDGE('',*,*,#42162,.F.);
#60475=ORIENTED_EDGE('',*,*,#41880,.T.);
#60476=ORIENTED_EDGE('',*,*,#42157,.T.);
#60477=ORIENTED_EDGE('',*,*,#42163,.T.);
#60478=ORIENTED_EDGE('',*,*,#42164,.F.);
#60479=ORIENTED_EDGE('',*,*,#41882,.T.);
#60480=ORIENTED_EDGE('',*,*,#42165,.F.);
#60481=ORIENTED_EDGE('',*,*,#42166,.F.);
#60482=ORIENTED_EDGE('',*,*,#42167,.F.);
#60483=ORIENTED_EDGE('',*,*,#42168,.F.);
#60484=ORIENTED_EDGE('',*,*,#42163,.F.);
#60485=ORIENTED_EDGE('',*,*,#42168,.T.);
#60486=ORIENTED_EDGE('',*,*,#42169,.F.);
#60487=ORIENTED_EDGE('',*,*,#41883,.T.);
#60488=ORIENTED_EDGE('',*,*,#42164,.T.);
#60489=ORIENTED_EDGE('',*,*,#41885,.T.);
#60490=ORIENTED_EDGE('',*,*,#42170,.F.);
#60491=ORIENTED_EDGE('',*,*,#42171,.T.);
#60492=ORIENTED_EDGE('',*,*,#42172,.F.);
#60493=ORIENTED_EDGE('',*,*,#42173,.F.);
#60494=ORIENTED_EDGE('',*,*,#42174,.T.);
#60495=ORIENTED_EDGE('',*,*,#42175,.F.);
#60496=ORIENTED_EDGE('',*,*,#41886,.T.);
#60497=ORIENTED_EDGE('',*,*,#42172,.T.);
#60498=ORIENTED_EDGE('',*,*,#42176,.T.);
#60499=ORIENTED_EDGE('',*,*,#42177,.F.);
#60500=ORIENTED_EDGE('',*,*,#42178,.F.);
#60501=ORIENTED_EDGE('',*,*,#42176,.F.);
#60502=ORIENTED_EDGE('',*,*,#42171,.F.);
#60503=ORIENTED_EDGE('',*,*,#42179,.F.);
#60504=ORIENTED_EDGE('',*,*,#42174,.F.);
#60505=ORIENTED_EDGE('',*,*,#41888,.T.);
#60506=ORIENTED_EDGE('',*,*,#42180,.F.);
#60507=ORIENTED_EDGE('',*,*,#42181,.T.);
#60508=ORIENTED_EDGE('',*,*,#42182,.F.);
#60509=ORIENTED_EDGE('',*,*,#42183,.F.);
#60510=ORIENTED_EDGE('',*,*,#42184,.T.);
#60511=ORIENTED_EDGE('',*,*,#42185,.F.);
#60512=ORIENTED_EDGE('',*,*,#41889,.T.);
#60513=ORIENTED_EDGE('',*,*,#42182,.T.);
#60514=ORIENTED_EDGE('',*,*,#42186,.T.);
#60515=ORIENTED_EDGE('',*,*,#42187,.F.);
#60516=ORIENTED_EDGE('',*,*,#42188,.F.);
#60517=ORIENTED_EDGE('',*,*,#42186,.F.);
#60518=ORIENTED_EDGE('',*,*,#42181,.F.);
#60519=ORIENTED_EDGE('',*,*,#42189,.F.);
#60520=ORIENTED_EDGE('',*,*,#42184,.F.);
#60521=ORIENTED_EDGE('',*,*,#41891,.T.);
#60522=ORIENTED_EDGE('',*,*,#42190,.F.);
#60523=ORIENTED_EDGE('',*,*,#42191,.T.);
#60524=ORIENTED_EDGE('',*,*,#42192,.F.);
#60525=ORIENTED_EDGE('',*,*,#42193,.F.);
#60526=ORIENTED_EDGE('',*,*,#42194,.T.);
#60527=ORIENTED_EDGE('',*,*,#42195,.F.);
#60528=ORIENTED_EDGE('',*,*,#41892,.T.);
#60529=ORIENTED_EDGE('',*,*,#42192,.T.);
#60530=ORIENTED_EDGE('',*,*,#42196,.T.);
#60531=ORIENTED_EDGE('',*,*,#42197,.F.);
#60532=ORIENTED_EDGE('',*,*,#42198,.F.);
#60533=ORIENTED_EDGE('',*,*,#42196,.F.);
#60534=ORIENTED_EDGE('',*,*,#42191,.F.);
#60535=ORIENTED_EDGE('',*,*,#42199,.F.);
#60536=ORIENTED_EDGE('',*,*,#42194,.F.);
#60537=ORIENTED_EDGE('',*,*,#41894,.T.);
#60538=ORIENTED_EDGE('',*,*,#42200,.F.);
#60539=ORIENTED_EDGE('',*,*,#42201,.T.);
#60540=ORIENTED_EDGE('',*,*,#42202,.F.);
#60541=ORIENTED_EDGE('',*,*,#42203,.F.);
#60542=ORIENTED_EDGE('',*,*,#42204,.T.);
#60543=ORIENTED_EDGE('',*,*,#42205,.F.);
#60544=ORIENTED_EDGE('',*,*,#41895,.T.);
#60545=ORIENTED_EDGE('',*,*,#42202,.T.);
#60546=ORIENTED_EDGE('',*,*,#42206,.T.);
#60547=ORIENTED_EDGE('',*,*,#42207,.F.);
#60548=ORIENTED_EDGE('',*,*,#42208,.F.);
#60549=ORIENTED_EDGE('',*,*,#42206,.F.);
#60550=ORIENTED_EDGE('',*,*,#42201,.F.);
#60551=ORIENTED_EDGE('',*,*,#42209,.F.);
#60552=ORIENTED_EDGE('',*,*,#42204,.F.);
#60553=ORIENTED_EDGE('',*,*,#41897,.T.);
#60554=ORIENTED_EDGE('',*,*,#42210,.F.);
#60555=ORIENTED_EDGE('',*,*,#42211,.T.);
#60556=ORIENTED_EDGE('',*,*,#42212,.F.);
#60557=ORIENTED_EDGE('',*,*,#42213,.F.);
#60558=ORIENTED_EDGE('',*,*,#42214,.T.);
#60559=ORIENTED_EDGE('',*,*,#42215,.F.);
#60560=ORIENTED_EDGE('',*,*,#41898,.T.);
#60561=ORIENTED_EDGE('',*,*,#42212,.T.);
#60562=ORIENTED_EDGE('',*,*,#42216,.T.);
#60563=ORIENTED_EDGE('',*,*,#42217,.F.);
#60564=ORIENTED_EDGE('',*,*,#42218,.F.);
#60565=ORIENTED_EDGE('',*,*,#42216,.F.);
#60566=ORIENTED_EDGE('',*,*,#42211,.F.);
#60567=ORIENTED_EDGE('',*,*,#42219,.F.);
#60568=ORIENTED_EDGE('',*,*,#42214,.F.);
#60569=ORIENTED_EDGE('',*,*,#41900,.T.);
#60570=ORIENTED_EDGE('',*,*,#42220,.F.);
#60571=ORIENTED_EDGE('',*,*,#42221,.T.);
#60572=ORIENTED_EDGE('',*,*,#42222,.F.);
#60573=ORIENTED_EDGE('',*,*,#42223,.F.);
#60574=ORIENTED_EDGE('',*,*,#42224,.T.);
#60575=ORIENTED_EDGE('',*,*,#42225,.F.);
#60576=ORIENTED_EDGE('',*,*,#41901,.T.);
#60577=ORIENTED_EDGE('',*,*,#42222,.T.);
#60578=ORIENTED_EDGE('',*,*,#42226,.T.);
#60579=ORIENTED_EDGE('',*,*,#42227,.F.);
#60580=ORIENTED_EDGE('',*,*,#42228,.F.);
#60581=ORIENTED_EDGE('',*,*,#42226,.F.);
#60582=ORIENTED_EDGE('',*,*,#42221,.F.);
#60583=ORIENTED_EDGE('',*,*,#42229,.F.);
#60584=ORIENTED_EDGE('',*,*,#42224,.F.);
#60585=ORIENTED_EDGE('',*,*,#41903,.T.);
#60586=ORIENTED_EDGE('',*,*,#42230,.F.);
#60587=ORIENTED_EDGE('',*,*,#42231,.T.);
#60588=ORIENTED_EDGE('',*,*,#42232,.F.);
#60589=ORIENTED_EDGE('',*,*,#42233,.F.);
#60590=ORIENTED_EDGE('',*,*,#42234,.T.);
#60591=ORIENTED_EDGE('',*,*,#42235,.F.);
#60592=ORIENTED_EDGE('',*,*,#41904,.T.);
#60593=ORIENTED_EDGE('',*,*,#42232,.T.);
#60594=ORIENTED_EDGE('',*,*,#42236,.T.);
#60595=ORIENTED_EDGE('',*,*,#42237,.F.);
#60596=ORIENTED_EDGE('',*,*,#42238,.F.);
#60597=ORIENTED_EDGE('',*,*,#42236,.F.);
#60598=ORIENTED_EDGE('',*,*,#42231,.F.);
#60599=ORIENTED_EDGE('',*,*,#42239,.F.);
#60600=ORIENTED_EDGE('',*,*,#42234,.F.);
#60601=ORIENTED_EDGE('',*,*,#41906,.T.);
#60602=ORIENTED_EDGE('',*,*,#42240,.F.);
#60603=ORIENTED_EDGE('',*,*,#42241,.T.);
#60604=ORIENTED_EDGE('',*,*,#42242,.F.);
#60605=ORIENTED_EDGE('',*,*,#42243,.F.);
#60606=ORIENTED_EDGE('',*,*,#42244,.T.);
#60607=ORIENTED_EDGE('',*,*,#42245,.F.);
#60608=ORIENTED_EDGE('',*,*,#41907,.T.);
#60609=ORIENTED_EDGE('',*,*,#42242,.T.);
#60610=ORIENTED_EDGE('',*,*,#42246,.T.);
#60611=ORIENTED_EDGE('',*,*,#42247,.F.);
#60612=ORIENTED_EDGE('',*,*,#42248,.F.);
#60613=ORIENTED_EDGE('',*,*,#42246,.F.);
#60614=ORIENTED_EDGE('',*,*,#42241,.F.);
#60615=ORIENTED_EDGE('',*,*,#42249,.F.);
#60616=ORIENTED_EDGE('',*,*,#42244,.F.);
#60617=ORIENTED_EDGE('',*,*,#41909,.T.);
#60618=ORIENTED_EDGE('',*,*,#42250,.F.);
#60619=ORIENTED_EDGE('',*,*,#42251,.T.);
#60620=ORIENTED_EDGE('',*,*,#42252,.F.);
#60621=ORIENTED_EDGE('',*,*,#42253,.F.);
#60622=ORIENTED_EDGE('',*,*,#42254,.T.);
#60623=ORIENTED_EDGE('',*,*,#42255,.F.);
#60624=ORIENTED_EDGE('',*,*,#41910,.T.);
#60625=ORIENTED_EDGE('',*,*,#42252,.T.);
#60626=ORIENTED_EDGE('',*,*,#42256,.T.);
#60627=ORIENTED_EDGE('',*,*,#42257,.F.);
#60628=ORIENTED_EDGE('',*,*,#42258,.F.);
#60629=ORIENTED_EDGE('',*,*,#42256,.F.);
#60630=ORIENTED_EDGE('',*,*,#42251,.F.);
#60631=ORIENTED_EDGE('',*,*,#42259,.F.);
#60632=ORIENTED_EDGE('',*,*,#42254,.F.);
#60633=ORIENTED_EDGE('',*,*,#41912,.T.);
#60634=ORIENTED_EDGE('',*,*,#42260,.F.);
#60635=ORIENTED_EDGE('',*,*,#42261,.T.);
#60636=ORIENTED_EDGE('',*,*,#42262,.F.);
#60637=ORIENTED_EDGE('',*,*,#42263,.F.);
#60638=ORIENTED_EDGE('',*,*,#42264,.T.);
#60639=ORIENTED_EDGE('',*,*,#42265,.F.);
#60640=ORIENTED_EDGE('',*,*,#41913,.T.);
#60641=ORIENTED_EDGE('',*,*,#42262,.T.);
#60642=ORIENTED_EDGE('',*,*,#42266,.T.);
#60643=ORIENTED_EDGE('',*,*,#42267,.F.);
#60644=ORIENTED_EDGE('',*,*,#42268,.F.);
#60645=ORIENTED_EDGE('',*,*,#42266,.F.);
#60646=ORIENTED_EDGE('',*,*,#42261,.F.);
#60647=ORIENTED_EDGE('',*,*,#42269,.F.);
#60648=ORIENTED_EDGE('',*,*,#42264,.F.);
#60649=ORIENTED_EDGE('',*,*,#41915,.T.);
#60650=ORIENTED_EDGE('',*,*,#42270,.F.);
#60651=ORIENTED_EDGE('',*,*,#42271,.T.);
#60652=ORIENTED_EDGE('',*,*,#42272,.F.);
#60653=ORIENTED_EDGE('',*,*,#42273,.F.);
#60654=ORIENTED_EDGE('',*,*,#42274,.T.);
#60655=ORIENTED_EDGE('',*,*,#42275,.F.);
#60656=ORIENTED_EDGE('',*,*,#41916,.T.);
#60657=ORIENTED_EDGE('',*,*,#42272,.T.);
#60658=ORIENTED_EDGE('',*,*,#42276,.T.);
#60659=ORIENTED_EDGE('',*,*,#42277,.F.);
#60660=ORIENTED_EDGE('',*,*,#42278,.F.);
#60661=ORIENTED_EDGE('',*,*,#42276,.F.);
#60662=ORIENTED_EDGE('',*,*,#42271,.F.);
#60663=ORIENTED_EDGE('',*,*,#42279,.F.);
#60664=ORIENTED_EDGE('',*,*,#42274,.F.);
#60665=ORIENTED_EDGE('',*,*,#41918,.T.);
#60666=ORIENTED_EDGE('',*,*,#42280,.F.);
#60667=ORIENTED_EDGE('',*,*,#42281,.T.);
#60668=ORIENTED_EDGE('',*,*,#42282,.F.);
#60669=ORIENTED_EDGE('',*,*,#42283,.F.);
#60670=ORIENTED_EDGE('',*,*,#42284,.T.);
#60671=ORIENTED_EDGE('',*,*,#42285,.F.);
#60672=ORIENTED_EDGE('',*,*,#41919,.T.);
#60673=ORIENTED_EDGE('',*,*,#42282,.T.);
#60674=ORIENTED_EDGE('',*,*,#42286,.T.);
#60675=ORIENTED_EDGE('',*,*,#42287,.F.);
#60676=ORIENTED_EDGE('',*,*,#42288,.F.);
#60677=ORIENTED_EDGE('',*,*,#42286,.F.);
#60678=ORIENTED_EDGE('',*,*,#42281,.F.);
#60679=ORIENTED_EDGE('',*,*,#42289,.F.);
#60680=ORIENTED_EDGE('',*,*,#42284,.F.);
#60681=ORIENTED_EDGE('',*,*,#41921,.T.);
#60682=ORIENTED_EDGE('',*,*,#42290,.F.);
#60683=ORIENTED_EDGE('',*,*,#42291,.T.);
#60684=ORIENTED_EDGE('',*,*,#42292,.F.);
#60685=ORIENTED_EDGE('',*,*,#42293,.F.);
#60686=ORIENTED_EDGE('',*,*,#42294,.T.);
#60687=ORIENTED_EDGE('',*,*,#42295,.F.);
#60688=ORIENTED_EDGE('',*,*,#41922,.T.);
#60689=ORIENTED_EDGE('',*,*,#42292,.T.);
#60690=ORIENTED_EDGE('',*,*,#42296,.T.);
#60691=ORIENTED_EDGE('',*,*,#42297,.F.);
#60692=ORIENTED_EDGE('',*,*,#42298,.F.);
#60693=ORIENTED_EDGE('',*,*,#42296,.F.);
#60694=ORIENTED_EDGE('',*,*,#42291,.F.);
#60695=ORIENTED_EDGE('',*,*,#42299,.F.);
#60696=ORIENTED_EDGE('',*,*,#42294,.F.);
#60697=ORIENTED_EDGE('',*,*,#41924,.T.);
#60698=ORIENTED_EDGE('',*,*,#42300,.F.);
#60699=ORIENTED_EDGE('',*,*,#42301,.T.);
#60700=ORIENTED_EDGE('',*,*,#42302,.F.);
#60701=ORIENTED_EDGE('',*,*,#42303,.F.);
#60702=ORIENTED_EDGE('',*,*,#42304,.T.);
#60703=ORIENTED_EDGE('',*,*,#42305,.F.);
#60704=ORIENTED_EDGE('',*,*,#41925,.T.);
#60705=ORIENTED_EDGE('',*,*,#42302,.T.);
#60706=ORIENTED_EDGE('',*,*,#42306,.T.);
#60707=ORIENTED_EDGE('',*,*,#42307,.F.);
#60708=ORIENTED_EDGE('',*,*,#42308,.F.);
#60709=ORIENTED_EDGE('',*,*,#42306,.F.);
#60710=ORIENTED_EDGE('',*,*,#42301,.F.);
#60711=ORIENTED_EDGE('',*,*,#42309,.F.);
#60712=ORIENTED_EDGE('',*,*,#42304,.F.);
#60713=ORIENTED_EDGE('',*,*,#41927,.T.);
#60714=ORIENTED_EDGE('',*,*,#42310,.F.);
#60715=ORIENTED_EDGE('',*,*,#42311,.T.);
#60716=ORIENTED_EDGE('',*,*,#42312,.F.);
#60717=ORIENTED_EDGE('',*,*,#42313,.F.);
#60718=ORIENTED_EDGE('',*,*,#42314,.T.);
#60719=ORIENTED_EDGE('',*,*,#42315,.F.);
#60720=ORIENTED_EDGE('',*,*,#41928,.T.);
#60721=ORIENTED_EDGE('',*,*,#42312,.T.);
#60722=ORIENTED_EDGE('',*,*,#42316,.T.);
#60723=ORIENTED_EDGE('',*,*,#42317,.F.);
#60724=ORIENTED_EDGE('',*,*,#42318,.F.);
#60725=ORIENTED_EDGE('',*,*,#42316,.F.);
#60726=ORIENTED_EDGE('',*,*,#42311,.F.);
#60727=ORIENTED_EDGE('',*,*,#42319,.F.);
#60728=ORIENTED_EDGE('',*,*,#42314,.F.);
#60729=ORIENTED_EDGE('',*,*,#41930,.T.);
#60730=ORIENTED_EDGE('',*,*,#42320,.F.);
#60731=ORIENTED_EDGE('',*,*,#42321,.T.);
#60732=ORIENTED_EDGE('',*,*,#42322,.F.);
#60733=ORIENTED_EDGE('',*,*,#42323,.F.);
#60734=ORIENTED_EDGE('',*,*,#42324,.T.);
#60735=ORIENTED_EDGE('',*,*,#42325,.F.);
#60736=ORIENTED_EDGE('',*,*,#41931,.T.);
#60737=ORIENTED_EDGE('',*,*,#42322,.T.);
#60738=ORIENTED_EDGE('',*,*,#42326,.T.);
#60739=ORIENTED_EDGE('',*,*,#42327,.F.);
#60740=ORIENTED_EDGE('',*,*,#42328,.F.);
#60741=ORIENTED_EDGE('',*,*,#42326,.F.);
#60742=ORIENTED_EDGE('',*,*,#42321,.F.);
#60743=ORIENTED_EDGE('',*,*,#42329,.F.);
#60744=ORIENTED_EDGE('',*,*,#42324,.F.);
#60745=ORIENTED_EDGE('',*,*,#41933,.T.);
#60746=ORIENTED_EDGE('',*,*,#42330,.F.);
#60747=ORIENTED_EDGE('',*,*,#42331,.T.);
#60748=ORIENTED_EDGE('',*,*,#42332,.F.);
#60749=ORIENTED_EDGE('',*,*,#42333,.F.);
#60750=ORIENTED_EDGE('',*,*,#42334,.T.);
#60751=ORIENTED_EDGE('',*,*,#42335,.F.);
#60752=ORIENTED_EDGE('',*,*,#41934,.T.);
#60753=ORIENTED_EDGE('',*,*,#42332,.T.);
#60754=ORIENTED_EDGE('',*,*,#42336,.T.);
#60755=ORIENTED_EDGE('',*,*,#42337,.F.);
#60756=ORIENTED_EDGE('',*,*,#42338,.F.);
#60757=ORIENTED_EDGE('',*,*,#42336,.F.);
#60758=ORIENTED_EDGE('',*,*,#42331,.F.);
#60759=ORIENTED_EDGE('',*,*,#42339,.F.);
#60760=ORIENTED_EDGE('',*,*,#42334,.F.);
#60761=ORIENTED_EDGE('',*,*,#41936,.T.);
#60762=ORIENTED_EDGE('',*,*,#42340,.F.);
#60763=ORIENTED_EDGE('',*,*,#42341,.T.);
#60764=ORIENTED_EDGE('',*,*,#42342,.F.);
#60765=ORIENTED_EDGE('',*,*,#42343,.F.);
#60766=ORIENTED_EDGE('',*,*,#42344,.T.);
#60767=ORIENTED_EDGE('',*,*,#42345,.F.);
#60768=ORIENTED_EDGE('',*,*,#41937,.T.);
#60769=ORIENTED_EDGE('',*,*,#42342,.T.);
#60770=ORIENTED_EDGE('',*,*,#42346,.T.);
#60771=ORIENTED_EDGE('',*,*,#42347,.F.);
#60772=ORIENTED_EDGE('',*,*,#42348,.F.);
#60773=ORIENTED_EDGE('',*,*,#42346,.F.);
#60774=ORIENTED_EDGE('',*,*,#42341,.F.);
#60775=ORIENTED_EDGE('',*,*,#42349,.F.);
#60776=ORIENTED_EDGE('',*,*,#42344,.F.);
#60777=ORIENTED_EDGE('',*,*,#41939,.T.);
#60778=ORIENTED_EDGE('',*,*,#42350,.F.);
#60779=ORIENTED_EDGE('',*,*,#42351,.T.);
#60780=ORIENTED_EDGE('',*,*,#42352,.F.);
#60781=ORIENTED_EDGE('',*,*,#42353,.F.);
#60782=ORIENTED_EDGE('',*,*,#42354,.T.);
#60783=ORIENTED_EDGE('',*,*,#42355,.F.);
#60784=ORIENTED_EDGE('',*,*,#41940,.T.);
#60785=ORIENTED_EDGE('',*,*,#42352,.T.);
#60786=ORIENTED_EDGE('',*,*,#42356,.T.);
#60787=ORIENTED_EDGE('',*,*,#42357,.F.);
#60788=ORIENTED_EDGE('',*,*,#42358,.F.);
#60789=ORIENTED_EDGE('',*,*,#42356,.F.);
#60790=ORIENTED_EDGE('',*,*,#42351,.F.);
#60791=ORIENTED_EDGE('',*,*,#42359,.F.);
#60792=ORIENTED_EDGE('',*,*,#42354,.F.);
#60793=ORIENTED_EDGE('',*,*,#41942,.T.);
#60794=ORIENTED_EDGE('',*,*,#42360,.F.);
#60795=ORIENTED_EDGE('',*,*,#42361,.T.);
#60796=ORIENTED_EDGE('',*,*,#42362,.F.);
#60797=ORIENTED_EDGE('',*,*,#42363,.F.);
#60798=ORIENTED_EDGE('',*,*,#42364,.T.);
#60799=ORIENTED_EDGE('',*,*,#42365,.F.);
#60800=ORIENTED_EDGE('',*,*,#41943,.T.);
#60801=ORIENTED_EDGE('',*,*,#42362,.T.);
#60802=ORIENTED_EDGE('',*,*,#42366,.T.);
#60803=ORIENTED_EDGE('',*,*,#42367,.F.);
#60804=ORIENTED_EDGE('',*,*,#42368,.F.);
#60805=ORIENTED_EDGE('',*,*,#42366,.F.);
#60806=ORIENTED_EDGE('',*,*,#42361,.F.);
#60807=ORIENTED_EDGE('',*,*,#42369,.F.);
#60808=ORIENTED_EDGE('',*,*,#42364,.F.);
#60809=ORIENTED_EDGE('',*,*,#41945,.T.);
#60810=ORIENTED_EDGE('',*,*,#42370,.F.);
#60811=ORIENTED_EDGE('',*,*,#42371,.T.);
#60812=ORIENTED_EDGE('',*,*,#42372,.F.);
#60813=ORIENTED_EDGE('',*,*,#42373,.F.);
#60814=ORIENTED_EDGE('',*,*,#42374,.T.);
#60815=ORIENTED_EDGE('',*,*,#42375,.F.);
#60816=ORIENTED_EDGE('',*,*,#41946,.T.);
#60817=ORIENTED_EDGE('',*,*,#42372,.T.);
#60818=ORIENTED_EDGE('',*,*,#42376,.T.);
#60819=ORIENTED_EDGE('',*,*,#42377,.F.);
#60820=ORIENTED_EDGE('',*,*,#42378,.F.);
#60821=ORIENTED_EDGE('',*,*,#42376,.F.);
#60822=ORIENTED_EDGE('',*,*,#42371,.F.);
#60823=ORIENTED_EDGE('',*,*,#42379,.F.);
#60824=ORIENTED_EDGE('',*,*,#42374,.F.);
#60825=ORIENTED_EDGE('',*,*,#41948,.T.);
#60826=ORIENTED_EDGE('',*,*,#42380,.F.);
#60827=ORIENTED_EDGE('',*,*,#34365,.T.);
#60828=ORIENTED_EDGE('',*,*,#42381,.F.);
#60829=ORIENTED_EDGE('',*,*,#41949,.T.);
#60830=ORIENTED_EDGE('',*,*,#42381,.T.);
#60831=ORIENTED_EDGE('',*,*,#34364,.T.);
#60832=ORIENTED_EDGE('',*,*,#42382,.F.);
#60833=ORIENTED_EDGE('',*,*,#41951,.T.);
#60834=ORIENTED_EDGE('',*,*,#42383,.F.);
#60835=ORIENTED_EDGE('',*,*,#42384,.T.);
#60836=ORIENTED_EDGE('',*,*,#42385,.F.);
#60837=ORIENTED_EDGE('',*,*,#42386,.F.);
#60838=ORIENTED_EDGE('',*,*,#42387,.T.);
#60839=ORIENTED_EDGE('',*,*,#42388,.F.);
#60840=ORIENTED_EDGE('',*,*,#41952,.T.);
#60841=ORIENTED_EDGE('',*,*,#42385,.T.);
#60842=ORIENTED_EDGE('',*,*,#42389,.T.);
#60843=ORIENTED_EDGE('',*,*,#42390,.F.);
#60844=ORIENTED_EDGE('',*,*,#42391,.F.);
#60845=ORIENTED_EDGE('',*,*,#42389,.F.);
#60846=ORIENTED_EDGE('',*,*,#42384,.F.);
#60847=ORIENTED_EDGE('',*,*,#42392,.F.);
#60848=ORIENTED_EDGE('',*,*,#42387,.F.);
#60849=ORIENTED_EDGE('',*,*,#41954,.T.);
#60850=ORIENTED_EDGE('',*,*,#42393,.F.);
#60851=ORIENTED_EDGE('',*,*,#42394,.T.);
#60852=ORIENTED_EDGE('',*,*,#42395,.F.);
#60853=ORIENTED_EDGE('',*,*,#42396,.F.);
#60854=ORIENTED_EDGE('',*,*,#42397,.T.);
#60855=ORIENTED_EDGE('',*,*,#42398,.F.);
#60856=ORIENTED_EDGE('',*,*,#41955,.T.);
#60857=ORIENTED_EDGE('',*,*,#42395,.T.);
#60858=ORIENTED_EDGE('',*,*,#42399,.T.);
#60859=ORIENTED_EDGE('',*,*,#42400,.F.);
#60860=ORIENTED_EDGE('',*,*,#42401,.F.);
#60861=ORIENTED_EDGE('',*,*,#42399,.F.);
#60862=ORIENTED_EDGE('',*,*,#42394,.F.);
#60863=ORIENTED_EDGE('',*,*,#42402,.F.);
#60864=ORIENTED_EDGE('',*,*,#42397,.F.);
#60865=ORIENTED_EDGE('',*,*,#41957,.T.);
#60866=ORIENTED_EDGE('',*,*,#42403,.F.);
#60867=ORIENTED_EDGE('',*,*,#42404,.T.);
#60868=ORIENTED_EDGE('',*,*,#42405,.F.);
#60869=ORIENTED_EDGE('',*,*,#42406,.F.);
#60870=ORIENTED_EDGE('',*,*,#42407,.F.);
#60871=ORIENTED_EDGE('',*,*,#42408,.T.);
#60872=ORIENTED_EDGE('',*,*,#42409,.T.);
#60873=ORIENTED_EDGE('',*,*,#42410,.F.);
#60874=ORIENTED_EDGE('',*,*,#41958,.T.);
#60875=ORIENTED_EDGE('',*,*,#42405,.T.);
#60876=ORIENTED_EDGE('',*,*,#42411,.F.);
#60877=ORIENTED_EDGE('',*,*,#42409,.F.);
#60878=ORIENTED_EDGE('',*,*,#42404,.F.);
#60879=ORIENTED_EDGE('',*,*,#42412,.F.);
#60880=ORIENTED_EDGE('',*,*,#42408,.F.);
#60881=ORIENTED_EDGE('',*,*,#41960,.T.);
#60882=ORIENTED_EDGE('',*,*,#42413,.F.);
#60883=ORIENTED_EDGE('',*,*,#42414,.T.);
#60884=ORIENTED_EDGE('',*,*,#42415,.F.);
#60885=ORIENTED_EDGE('',*,*,#42416,.F.);
#60886=ORIENTED_EDGE('',*,*,#42417,.T.);
#60887=ORIENTED_EDGE('',*,*,#42418,.F.);
#60888=ORIENTED_EDGE('',*,*,#41961,.T.);
#60889=ORIENTED_EDGE('',*,*,#42415,.T.);
#60890=ORIENTED_EDGE('',*,*,#42419,.T.);
#60891=ORIENTED_EDGE('',*,*,#42420,.F.);
#60892=ORIENTED_EDGE('',*,*,#42421,.F.);
#60893=ORIENTED_EDGE('',*,*,#42419,.F.);
#60894=ORIENTED_EDGE('',*,*,#42414,.F.);
#60895=ORIENTED_EDGE('',*,*,#42422,.F.);
#60896=ORIENTED_EDGE('',*,*,#42417,.F.);
#60897=ORIENTED_EDGE('',*,*,#41963,.T.);
#60898=ORIENTED_EDGE('',*,*,#42423,.F.);
#60899=ORIENTED_EDGE('',*,*,#42424,.T.);
#60900=ORIENTED_EDGE('',*,*,#42425,.F.);
#60901=ORIENTED_EDGE('',*,*,#42426,.F.);
#60902=ORIENTED_EDGE('',*,*,#42427,.T.);
#60903=ORIENTED_EDGE('',*,*,#42428,.F.);
#60904=ORIENTED_EDGE('',*,*,#41964,.T.);
#60905=ORIENTED_EDGE('',*,*,#42425,.T.);
#60906=ORIENTED_EDGE('',*,*,#42429,.T.);
#60907=ORIENTED_EDGE('',*,*,#42430,.F.);
#60908=ORIENTED_EDGE('',*,*,#42431,.F.);
#60909=ORIENTED_EDGE('',*,*,#42429,.F.);
#60910=ORIENTED_EDGE('',*,*,#42424,.F.);
#60911=ORIENTED_EDGE('',*,*,#42432,.F.);
#60912=ORIENTED_EDGE('',*,*,#42427,.F.);
#60913=ORIENTED_EDGE('',*,*,#41966,.T.);
#60914=ORIENTED_EDGE('',*,*,#42433,.F.);
#60915=ORIENTED_EDGE('',*,*,#42434,.T.);
#60916=ORIENTED_EDGE('',*,*,#42435,.F.);
#60917=ORIENTED_EDGE('',*,*,#42436,.F.);
#60918=ORIENTED_EDGE('',*,*,#42437,.T.);
#60919=ORIENTED_EDGE('',*,*,#42438,.F.);
#60920=ORIENTED_EDGE('',*,*,#41967,.T.);
#60921=ORIENTED_EDGE('',*,*,#42435,.T.);
#60922=ORIENTED_EDGE('',*,*,#42439,.T.);
#60923=ORIENTED_EDGE('',*,*,#42440,.F.);
#60924=ORIENTED_EDGE('',*,*,#42441,.F.);
#60925=ORIENTED_EDGE('',*,*,#42439,.F.);
#60926=ORIENTED_EDGE('',*,*,#42434,.F.);
#60927=ORIENTED_EDGE('',*,*,#42442,.F.);
#60928=ORIENTED_EDGE('',*,*,#42437,.F.);
#60929=ORIENTED_EDGE('',*,*,#41969,.T.);
#60930=ORIENTED_EDGE('',*,*,#42443,.F.);
#60931=ORIENTED_EDGE('',*,*,#42444,.T.);
#60932=ORIENTED_EDGE('',*,*,#42445,.F.);
#60933=ORIENTED_EDGE('',*,*,#42446,.F.);
#60934=ORIENTED_EDGE('',*,*,#42447,.T.);
#60935=ORIENTED_EDGE('',*,*,#42448,.F.);
#60936=ORIENTED_EDGE('',*,*,#41970,.T.);
#60937=ORIENTED_EDGE('',*,*,#42445,.T.);
#60938=ORIENTED_EDGE('',*,*,#42449,.T.);
#60939=ORIENTED_EDGE('',*,*,#42450,.F.);
#60940=ORIENTED_EDGE('',*,*,#42451,.F.);
#60941=ORIENTED_EDGE('',*,*,#42449,.F.);
#60942=ORIENTED_EDGE('',*,*,#42444,.F.);
#60943=ORIENTED_EDGE('',*,*,#42452,.F.);
#60944=ORIENTED_EDGE('',*,*,#42447,.F.);
#60945=ORIENTED_EDGE('',*,*,#42453,.F.);
#60946=ORIENTED_EDGE('',*,*,#42454,.F.);
#60947=ORIENTED_EDGE('',*,*,#41974,.T.);
#60948=ORIENTED_EDGE('',*,*,#41973,.T.);
#60949=ORIENTED_EDGE('',*,*,#42455,.F.);
#60950=ORIENTED_EDGE('',*,*,#41977,.T.);
#60951=ORIENTED_EDGE('',*,*,#41975,.T.);
#60952=ORIENTED_EDGE('',*,*,#42454,.T.);
#60953=ORIENTED_EDGE('',*,*,#42456,.F.);
#60954=ORIENTED_EDGE('',*,*,#42457,.F.);
#60955=ORIENTED_EDGE('',*,*,#41981,.T.);
#60956=ORIENTED_EDGE('',*,*,#41980,.T.);
#60957=ORIENTED_EDGE('',*,*,#42458,.F.);
#60958=ORIENTED_EDGE('',*,*,#41984,.T.);
#60959=ORIENTED_EDGE('',*,*,#41982,.T.);
#60960=ORIENTED_EDGE('',*,*,#42457,.T.);
#60961=ORIENTED_EDGE('',*,*,#42459,.F.);
#60962=ORIENTED_EDGE('',*,*,#42460,.F.);
#60963=ORIENTED_EDGE('',*,*,#41988,.T.);
#60964=ORIENTED_EDGE('',*,*,#41987,.T.);
#60965=ORIENTED_EDGE('',*,*,#42461,.F.);
#60966=ORIENTED_EDGE('',*,*,#41991,.T.);
#60967=ORIENTED_EDGE('',*,*,#41989,.T.);
#60968=ORIENTED_EDGE('',*,*,#42460,.T.);
#60969=ORIENTED_EDGE('',*,*,#42462,.F.);
#60970=ORIENTED_EDGE('',*,*,#42463,.F.);
#60971=ORIENTED_EDGE('',*,*,#41995,.T.);
#60972=ORIENTED_EDGE('',*,*,#41994,.T.);
#60973=ORIENTED_EDGE('',*,*,#42464,.F.);
#60974=ORIENTED_EDGE('',*,*,#41998,.T.);
#60975=ORIENTED_EDGE('',*,*,#41996,.T.);
#60976=ORIENTED_EDGE('',*,*,#42463,.T.);
#60977=ORIENTED_EDGE('',*,*,#42465,.F.);
#60978=ORIENTED_EDGE('',*,*,#42466,.F.);
#60979=ORIENTED_EDGE('',*,*,#42002,.T.);
#60980=ORIENTED_EDGE('',*,*,#42001,.T.);
#60981=ORIENTED_EDGE('',*,*,#42467,.F.);
#60982=ORIENTED_EDGE('',*,*,#42005,.T.);
#60983=ORIENTED_EDGE('',*,*,#42003,.T.);
#60984=ORIENTED_EDGE('',*,*,#42466,.T.);
#60985=ORIENTED_EDGE('',*,*,#42468,.F.);
#60986=ORIENTED_EDGE('',*,*,#42469,.F.);
#60987=ORIENTED_EDGE('',*,*,#42009,.T.);
#60988=ORIENTED_EDGE('',*,*,#42008,.T.);
#60989=ORIENTED_EDGE('',*,*,#42470,.F.);
#60990=ORIENTED_EDGE('',*,*,#42012,.T.);
#60991=ORIENTED_EDGE('',*,*,#42010,.T.);
#60992=ORIENTED_EDGE('',*,*,#42469,.T.);
#60993=ORIENTED_EDGE('',*,*,#42471,.F.);
#60994=ORIENTED_EDGE('',*,*,#42472,.F.);
#60995=ORIENTED_EDGE('',*,*,#42016,.T.);
#60996=ORIENTED_EDGE('',*,*,#42015,.T.);
#60997=ORIENTED_EDGE('',*,*,#42473,.F.);
#60998=ORIENTED_EDGE('',*,*,#42019,.T.);
#60999=ORIENTED_EDGE('',*,*,#42017,.T.);
#61000=ORIENTED_EDGE('',*,*,#42472,.T.);
#61001=ORIENTED_EDGE('',*,*,#42474,.F.);
#61002=ORIENTED_EDGE('',*,*,#42475,.F.);
#61003=ORIENTED_EDGE('',*,*,#42023,.T.);
#61004=ORIENTED_EDGE('',*,*,#42022,.T.);
#61005=ORIENTED_EDGE('',*,*,#42476,.F.);
#61006=ORIENTED_EDGE('',*,*,#42026,.T.);
#61007=ORIENTED_EDGE('',*,*,#42024,.T.);
#61008=ORIENTED_EDGE('',*,*,#42475,.T.);
#61009=ORIENTED_EDGE('',*,*,#42477,.F.);
#61010=ORIENTED_EDGE('',*,*,#42478,.F.);
#61011=ORIENTED_EDGE('',*,*,#42030,.T.);
#61012=ORIENTED_EDGE('',*,*,#42029,.T.);
#61013=ORIENTED_EDGE('',*,*,#42479,.F.);
#61014=ORIENTED_EDGE('',*,*,#42033,.T.);
#61015=ORIENTED_EDGE('',*,*,#42031,.T.);
#61016=ORIENTED_EDGE('',*,*,#42478,.T.);
#61017=ORIENTED_EDGE('',*,*,#42480,.F.);
#61018=ORIENTED_EDGE('',*,*,#42481,.F.);
#61019=ORIENTED_EDGE('',*,*,#42037,.T.);
#61020=ORIENTED_EDGE('',*,*,#42036,.T.);
#61021=ORIENTED_EDGE('',*,*,#42482,.F.);
#61022=ORIENTED_EDGE('',*,*,#42040,.T.);
#61023=ORIENTED_EDGE('',*,*,#42038,.T.);
#61024=ORIENTED_EDGE('',*,*,#42481,.T.);
#61025=ORIENTED_EDGE('',*,*,#42483,.F.);
#61026=ORIENTED_EDGE('',*,*,#42484,.F.);
#61027=ORIENTED_EDGE('',*,*,#42044,.T.);
#61028=ORIENTED_EDGE('',*,*,#42043,.T.);
#61029=ORIENTED_EDGE('',*,*,#42485,.F.);
#61030=ORIENTED_EDGE('',*,*,#42047,.T.);
#61031=ORIENTED_EDGE('',*,*,#42045,.T.);
#61032=ORIENTED_EDGE('',*,*,#42484,.T.);
#61033=ORIENTED_EDGE('',*,*,#42486,.F.);
#61034=ORIENTED_EDGE('',*,*,#42487,.F.);
#61035=ORIENTED_EDGE('',*,*,#42051,.T.);
#61036=ORIENTED_EDGE('',*,*,#42050,.T.);
#61037=ORIENTED_EDGE('',*,*,#42488,.F.);
#61038=ORIENTED_EDGE('',*,*,#42054,.T.);
#61039=ORIENTED_EDGE('',*,*,#42052,.T.);
#61040=ORIENTED_EDGE('',*,*,#42487,.T.);
#61041=ORIENTED_EDGE('',*,*,#42489,.F.);
#61042=ORIENTED_EDGE('',*,*,#42490,.F.);
#61043=ORIENTED_EDGE('',*,*,#42058,.T.);
#61044=ORIENTED_EDGE('',*,*,#42057,.T.);
#61045=ORIENTED_EDGE('',*,*,#42491,.F.);
#61046=ORIENTED_EDGE('',*,*,#42061,.T.);
#61047=ORIENTED_EDGE('',*,*,#42059,.T.);
#61048=ORIENTED_EDGE('',*,*,#42490,.T.);
#61049=ORIENTED_EDGE('',*,*,#42492,.F.);
#61050=ORIENTED_EDGE('',*,*,#42493,.F.);
#61051=ORIENTED_EDGE('',*,*,#42065,.T.);
#61052=ORIENTED_EDGE('',*,*,#42064,.T.);
#61053=ORIENTED_EDGE('',*,*,#42494,.F.);
#61054=ORIENTED_EDGE('',*,*,#42068,.T.);
#61055=ORIENTED_EDGE('',*,*,#42066,.T.);
#61056=ORIENTED_EDGE('',*,*,#42493,.T.);
#61057=ORIENTED_EDGE('',*,*,#42495,.F.);
#61058=ORIENTED_EDGE('',*,*,#42496,.F.);
#61059=ORIENTED_EDGE('',*,*,#34370,.T.);
#61060=ORIENTED_EDGE('',*,*,#42070,.T.);
#61061=ORIENTED_EDGE('',*,*,#42497,.F.);
#61062=ORIENTED_EDGE('',*,*,#42071,.T.);
#61063=ORIENTED_EDGE('',*,*,#34371,.T.);
#61064=ORIENTED_EDGE('',*,*,#42496,.T.);
#61065=ORIENTED_EDGE('',*,*,#42498,.F.);
#61066=ORIENTED_EDGE('',*,*,#42499,.F.);
#61067=ORIENTED_EDGE('',*,*,#42075,.T.);
#61068=ORIENTED_EDGE('',*,*,#42074,.T.);
#61069=ORIENTED_EDGE('',*,*,#42500,.F.);
#61070=ORIENTED_EDGE('',*,*,#42078,.T.);
#61071=ORIENTED_EDGE('',*,*,#42076,.T.);
#61072=ORIENTED_EDGE('',*,*,#42499,.T.);
#61073=ORIENTED_EDGE('',*,*,#42501,.F.);
#61074=ORIENTED_EDGE('',*,*,#42502,.F.);
#61075=ORIENTED_EDGE('',*,*,#42082,.T.);
#61076=ORIENTED_EDGE('',*,*,#42081,.T.);
#61077=ORIENTED_EDGE('',*,*,#42503,.F.);
#61078=ORIENTED_EDGE('',*,*,#42085,.T.);
#61079=ORIENTED_EDGE('',*,*,#42083,.T.);
#61080=ORIENTED_EDGE('',*,*,#42502,.T.);
#61081=ORIENTED_EDGE('',*,*,#42504,.F.);
#61082=ORIENTED_EDGE('',*,*,#42505,.F.);
#61083=ORIENTED_EDGE('',*,*,#42089,.T.);
#61084=ORIENTED_EDGE('',*,*,#42088,.T.);
#61085=ORIENTED_EDGE('',*,*,#42506,.F.);
#61086=ORIENTED_EDGE('',*,*,#42092,.T.);
#61087=ORIENTED_EDGE('',*,*,#42090,.T.);
#61088=ORIENTED_EDGE('',*,*,#42505,.T.);
#61089=ORIENTED_EDGE('',*,*,#42507,.F.);
#61090=ORIENTED_EDGE('',*,*,#42508,.F.);
#61091=ORIENTED_EDGE('',*,*,#42098,.T.);
#61092=ORIENTED_EDGE('',*,*,#42095,.T.);
#61093=ORIENTED_EDGE('',*,*,#42099,.T.);
#61094=ORIENTED_EDGE('',*,*,#42508,.T.);
#61095=ORIENTED_EDGE('',*,*,#42509,.F.);
#61096=ORIENTED_EDGE('',*,*,#42097,.T.);
#61097=ORIENTED_EDGE('',*,*,#42104,.T.);
#61098=ORIENTED_EDGE('',*,*,#42100,.T.);
#61099=ORIENTED_EDGE('',*,*,#42510,.F.);
#61100=ORIENTED_EDGE('',*,*,#42511,.F.);
#61101=ORIENTED_EDGE('',*,*,#42512,.F.);
#61102=ORIENTED_EDGE('',*,*,#42106,.T.);
#61103=ORIENTED_EDGE('',*,*,#42105,.T.);
#61104=ORIENTED_EDGE('',*,*,#42511,.T.);
#61105=ORIENTED_EDGE('',*,*,#42513,.F.);
#61106=ORIENTED_EDGE('',*,*,#42514,.F.);
#61107=ORIENTED_EDGE('',*,*,#42110,.T.);
#61108=ORIENTED_EDGE('',*,*,#42109,.T.);
#61109=ORIENTED_EDGE('',*,*,#42515,.F.);
#61110=ORIENTED_EDGE('',*,*,#42113,.T.);
#61111=ORIENTED_EDGE('',*,*,#42111,.T.);
#61112=ORIENTED_EDGE('',*,*,#42514,.T.);
#61113=ORIENTED_EDGE('',*,*,#42516,.F.);
#61114=ORIENTED_EDGE('',*,*,#42517,.F.);
#61115=ORIENTED_EDGE('',*,*,#42117,.T.);
#61116=ORIENTED_EDGE('',*,*,#42116,.T.);
#61117=ORIENTED_EDGE('',*,*,#42518,.F.);
#61118=ORIENTED_EDGE('',*,*,#42120,.T.);
#61119=ORIENTED_EDGE('',*,*,#42118,.T.);
#61120=ORIENTED_EDGE('',*,*,#42517,.T.);
#61121=ORIENTED_EDGE('',*,*,#42519,.F.);
#61122=ORIENTED_EDGE('',*,*,#42520,.F.);
#61123=ORIENTED_EDGE('',*,*,#42124,.T.);
#61124=ORIENTED_EDGE('',*,*,#42123,.T.);
#61125=ORIENTED_EDGE('',*,*,#42521,.F.);
#61126=ORIENTED_EDGE('',*,*,#42127,.T.);
#61127=ORIENTED_EDGE('',*,*,#42125,.T.);
#61128=ORIENTED_EDGE('',*,*,#42520,.T.);
#61129=ORIENTED_EDGE('',*,*,#42522,.F.);
#61130=ORIENTED_EDGE('',*,*,#42523,.F.);
#61131=ORIENTED_EDGE('',*,*,#42131,.T.);
#61132=ORIENTED_EDGE('',*,*,#42130,.T.);
#61133=ORIENTED_EDGE('',*,*,#42524,.F.);
#61134=ORIENTED_EDGE('',*,*,#42134,.T.);
#61135=ORIENTED_EDGE('',*,*,#42132,.T.);
#61136=ORIENTED_EDGE('',*,*,#42523,.T.);
#61137=ORIENTED_EDGE('',*,*,#42525,.F.);
#61138=ORIENTED_EDGE('',*,*,#42526,.F.);
#61139=ORIENTED_EDGE('',*,*,#42138,.T.);
#61140=ORIENTED_EDGE('',*,*,#42137,.T.);
#61141=ORIENTED_EDGE('',*,*,#42527,.F.);
#61142=ORIENTED_EDGE('',*,*,#42141,.T.);
#61143=ORIENTED_EDGE('',*,*,#42139,.T.);
#61144=ORIENTED_EDGE('',*,*,#42526,.T.);
#61145=ORIENTED_EDGE('',*,*,#42528,.F.);
#61146=ORIENTED_EDGE('',*,*,#42529,.F.);
#61147=ORIENTED_EDGE('',*,*,#42145,.T.);
#61148=ORIENTED_EDGE('',*,*,#42144,.T.);
#61149=ORIENTED_EDGE('',*,*,#42530,.F.);
#61150=ORIENTED_EDGE('',*,*,#42148,.T.);
#61151=ORIENTED_EDGE('',*,*,#42146,.T.);
#61152=ORIENTED_EDGE('',*,*,#42529,.T.);
#61153=ORIENTED_EDGE('',*,*,#42531,.F.);
#61154=ORIENTED_EDGE('',*,*,#42532,.F.);
#61155=ORIENTED_EDGE('',*,*,#42152,.T.);
#61156=ORIENTED_EDGE('',*,*,#42151,.T.);
#61157=ORIENTED_EDGE('',*,*,#42533,.F.);
#61158=ORIENTED_EDGE('',*,*,#42155,.T.);
#61159=ORIENTED_EDGE('',*,*,#42153,.T.);
#61160=ORIENTED_EDGE('',*,*,#42532,.T.);
#61161=ORIENTED_EDGE('',*,*,#42534,.F.);
#61162=ORIENTED_EDGE('',*,*,#42535,.F.);
#61163=ORIENTED_EDGE('',*,*,#42159,.T.);
#61164=ORIENTED_EDGE('',*,*,#42158,.T.);
#61165=ORIENTED_EDGE('',*,*,#42536,.F.);
#61166=ORIENTED_EDGE('',*,*,#42162,.T.);
#61167=ORIENTED_EDGE('',*,*,#42160,.T.);
#61168=ORIENTED_EDGE('',*,*,#42535,.T.);
#61169=ORIENTED_EDGE('',*,*,#42537,.F.);
#61170=ORIENTED_EDGE('',*,*,#42538,.F.);
#61171=ORIENTED_EDGE('',*,*,#42166,.T.);
#61172=ORIENTED_EDGE('',*,*,#42165,.T.);
#61173=ORIENTED_EDGE('',*,*,#42539,.F.);
#61174=ORIENTED_EDGE('',*,*,#42169,.T.);
#61175=ORIENTED_EDGE('',*,*,#42167,.T.);
#61176=ORIENTED_EDGE('',*,*,#42538,.T.);
#61177=ORIENTED_EDGE('',*,*,#42540,.F.);
#61178=ORIENTED_EDGE('',*,*,#42541,.F.);
#61179=ORIENTED_EDGE('',*,*,#42175,.T.);
#61180=ORIENTED_EDGE('',*,*,#42179,.T.);
#61181=ORIENTED_EDGE('',*,*,#42170,.T.);
#61182=ORIENTED_EDGE('',*,*,#42177,.T.);
#61183=ORIENTED_EDGE('',*,*,#42178,.T.);
#61184=ORIENTED_EDGE('',*,*,#42173,.T.);
#61185=ORIENTED_EDGE('',*,*,#42541,.T.);
#61186=ORIENTED_EDGE('',*,*,#42542,.F.);
#61187=ORIENTED_EDGE('',*,*,#42543,.F.);
#61188=ORIENTED_EDGE('',*,*,#42544,.F.);
#61189=ORIENTED_EDGE('',*,*,#42185,.T.);
#61190=ORIENTED_EDGE('',*,*,#42189,.T.);
#61191=ORIENTED_EDGE('',*,*,#42180,.T.);
#61192=ORIENTED_EDGE('',*,*,#42187,.T.);
#61193=ORIENTED_EDGE('',*,*,#42188,.T.);
#61194=ORIENTED_EDGE('',*,*,#42183,.T.);
#61195=ORIENTED_EDGE('',*,*,#42544,.T.);
#61196=ORIENTED_EDGE('',*,*,#42545,.F.);
#61197=ORIENTED_EDGE('',*,*,#42546,.F.);
#61198=ORIENTED_EDGE('',*,*,#42547,.F.);
#61199=ORIENTED_EDGE('',*,*,#42195,.T.);
#61200=ORIENTED_EDGE('',*,*,#42199,.T.);
#61201=ORIENTED_EDGE('',*,*,#42190,.T.);
#61202=ORIENTED_EDGE('',*,*,#42197,.T.);
#61203=ORIENTED_EDGE('',*,*,#42198,.T.);
#61204=ORIENTED_EDGE('',*,*,#42193,.T.);
#61205=ORIENTED_EDGE('',*,*,#42547,.T.);
#61206=ORIENTED_EDGE('',*,*,#42548,.F.);
#61207=ORIENTED_EDGE('',*,*,#42549,.F.);
#61208=ORIENTED_EDGE('',*,*,#42550,.F.);
#61209=ORIENTED_EDGE('',*,*,#42205,.T.);
#61210=ORIENTED_EDGE('',*,*,#42209,.T.);
#61211=ORIENTED_EDGE('',*,*,#42200,.T.);
#61212=ORIENTED_EDGE('',*,*,#42207,.T.);
#61213=ORIENTED_EDGE('',*,*,#42208,.T.);
#61214=ORIENTED_EDGE('',*,*,#42203,.T.);
#61215=ORIENTED_EDGE('',*,*,#42550,.T.);
#61216=ORIENTED_EDGE('',*,*,#42551,.F.);
#61217=ORIENTED_EDGE('',*,*,#42552,.F.);
#61218=ORIENTED_EDGE('',*,*,#42553,.F.);
#61219=ORIENTED_EDGE('',*,*,#42215,.T.);
#61220=ORIENTED_EDGE('',*,*,#42219,.T.);
#61221=ORIENTED_EDGE('',*,*,#42210,.T.);
#61222=ORIENTED_EDGE('',*,*,#42217,.T.);
#61223=ORIENTED_EDGE('',*,*,#42218,.T.);
#61224=ORIENTED_EDGE('',*,*,#42213,.T.);
#61225=ORIENTED_EDGE('',*,*,#42553,.T.);
#61226=ORIENTED_EDGE('',*,*,#42554,.F.);
#61227=ORIENTED_EDGE('',*,*,#42555,.F.);
#61228=ORIENTED_EDGE('',*,*,#42556,.F.);
#61229=ORIENTED_EDGE('',*,*,#42225,.T.);
#61230=ORIENTED_EDGE('',*,*,#42229,.T.);
#61231=ORIENTED_EDGE('',*,*,#42220,.T.);
#61232=ORIENTED_EDGE('',*,*,#42227,.T.);
#61233=ORIENTED_EDGE('',*,*,#42228,.T.);
#61234=ORIENTED_EDGE('',*,*,#42223,.T.);
#61235=ORIENTED_EDGE('',*,*,#42556,.T.);
#61236=ORIENTED_EDGE('',*,*,#42557,.F.);
#61237=ORIENTED_EDGE('',*,*,#42558,.F.);
#61238=ORIENTED_EDGE('',*,*,#42559,.F.);
#61239=ORIENTED_EDGE('',*,*,#42235,.T.);
#61240=ORIENTED_EDGE('',*,*,#42239,.T.);
#61241=ORIENTED_EDGE('',*,*,#42230,.T.);
#61242=ORIENTED_EDGE('',*,*,#42237,.T.);
#61243=ORIENTED_EDGE('',*,*,#42238,.T.);
#61244=ORIENTED_EDGE('',*,*,#42233,.T.);
#61245=ORIENTED_EDGE('',*,*,#42559,.T.);
#61246=ORIENTED_EDGE('',*,*,#42560,.F.);
#61247=ORIENTED_EDGE('',*,*,#42561,.F.);
#61248=ORIENTED_EDGE('',*,*,#42562,.F.);
#61249=ORIENTED_EDGE('',*,*,#42245,.T.);
#61250=ORIENTED_EDGE('',*,*,#42249,.T.);
#61251=ORIENTED_EDGE('',*,*,#42240,.T.);
#61252=ORIENTED_EDGE('',*,*,#42247,.T.);
#61253=ORIENTED_EDGE('',*,*,#42248,.T.);
#61254=ORIENTED_EDGE('',*,*,#42243,.T.);
#61255=ORIENTED_EDGE('',*,*,#42562,.T.);
#61256=ORIENTED_EDGE('',*,*,#42563,.F.);
#61257=ORIENTED_EDGE('',*,*,#42564,.F.);
#61258=ORIENTED_EDGE('',*,*,#42565,.F.);
#61259=ORIENTED_EDGE('',*,*,#42255,.T.);
#61260=ORIENTED_EDGE('',*,*,#42259,.T.);
#61261=ORIENTED_EDGE('',*,*,#42250,.T.);
#61262=ORIENTED_EDGE('',*,*,#42257,.T.);
#61263=ORIENTED_EDGE('',*,*,#42258,.T.);
#61264=ORIENTED_EDGE('',*,*,#42253,.T.);
#61265=ORIENTED_EDGE('',*,*,#42565,.T.);
#61266=ORIENTED_EDGE('',*,*,#42566,.F.);
#61267=ORIENTED_EDGE('',*,*,#42567,.F.);
#61268=ORIENTED_EDGE('',*,*,#42568,.F.);
#61269=ORIENTED_EDGE('',*,*,#42265,.T.);
#61270=ORIENTED_EDGE('',*,*,#42269,.T.);
#61271=ORIENTED_EDGE('',*,*,#42260,.T.);
#61272=ORIENTED_EDGE('',*,*,#42267,.T.);
#61273=ORIENTED_EDGE('',*,*,#42268,.T.);
#61274=ORIENTED_EDGE('',*,*,#42263,.T.);
#61275=ORIENTED_EDGE('',*,*,#42568,.T.);
#61276=ORIENTED_EDGE('',*,*,#42569,.F.);
#61277=ORIENTED_EDGE('',*,*,#42570,.F.);
#61278=ORIENTED_EDGE('',*,*,#42571,.F.);
#61279=ORIENTED_EDGE('',*,*,#42275,.T.);
#61280=ORIENTED_EDGE('',*,*,#42279,.T.);
#61281=ORIENTED_EDGE('',*,*,#42270,.T.);
#61282=ORIENTED_EDGE('',*,*,#42277,.T.);
#61283=ORIENTED_EDGE('',*,*,#42278,.T.);
#61284=ORIENTED_EDGE('',*,*,#42273,.T.);
#61285=ORIENTED_EDGE('',*,*,#42571,.T.);
#61286=ORIENTED_EDGE('',*,*,#42572,.F.);
#61287=ORIENTED_EDGE('',*,*,#42573,.F.);
#61288=ORIENTED_EDGE('',*,*,#42574,.F.);
#61289=ORIENTED_EDGE('',*,*,#42285,.T.);
#61290=ORIENTED_EDGE('',*,*,#42289,.T.);
#61291=ORIENTED_EDGE('',*,*,#42280,.T.);
#61292=ORIENTED_EDGE('',*,*,#42287,.T.);
#61293=ORIENTED_EDGE('',*,*,#42288,.T.);
#61294=ORIENTED_EDGE('',*,*,#42283,.T.);
#61295=ORIENTED_EDGE('',*,*,#42574,.T.);
#61296=ORIENTED_EDGE('',*,*,#42575,.F.);
#61297=ORIENTED_EDGE('',*,*,#42576,.F.);
#61298=ORIENTED_EDGE('',*,*,#42577,.F.);
#61299=ORIENTED_EDGE('',*,*,#42295,.T.);
#61300=ORIENTED_EDGE('',*,*,#42299,.T.);
#61301=ORIENTED_EDGE('',*,*,#42290,.T.);
#61302=ORIENTED_EDGE('',*,*,#42297,.T.);
#61303=ORIENTED_EDGE('',*,*,#42298,.T.);
#61304=ORIENTED_EDGE('',*,*,#42293,.T.);
#61305=ORIENTED_EDGE('',*,*,#42577,.T.);
#61306=ORIENTED_EDGE('',*,*,#42578,.F.);
#61307=ORIENTED_EDGE('',*,*,#42579,.F.);
#61308=ORIENTED_EDGE('',*,*,#42580,.F.);
#61309=ORIENTED_EDGE('',*,*,#42305,.T.);
#61310=ORIENTED_EDGE('',*,*,#42309,.T.);
#61311=ORIENTED_EDGE('',*,*,#42300,.T.);
#61312=ORIENTED_EDGE('',*,*,#42307,.T.);
#61313=ORIENTED_EDGE('',*,*,#42308,.T.);
#61314=ORIENTED_EDGE('',*,*,#42303,.T.);
#61315=ORIENTED_EDGE('',*,*,#42580,.T.);
#61316=ORIENTED_EDGE('',*,*,#42581,.F.);
#61317=ORIENTED_EDGE('',*,*,#42582,.F.);
#61318=ORIENTED_EDGE('',*,*,#42583,.F.);
#61319=ORIENTED_EDGE('',*,*,#42315,.T.);
#61320=ORIENTED_EDGE('',*,*,#42319,.T.);
#61321=ORIENTED_EDGE('',*,*,#42310,.T.);
#61322=ORIENTED_EDGE('',*,*,#42317,.T.);
#61323=ORIENTED_EDGE('',*,*,#42318,.T.);
#61324=ORIENTED_EDGE('',*,*,#42313,.T.);
#61325=ORIENTED_EDGE('',*,*,#42583,.T.);
#61326=ORIENTED_EDGE('',*,*,#42584,.F.);
#61327=ORIENTED_EDGE('',*,*,#42585,.F.);
#61328=ORIENTED_EDGE('',*,*,#42586,.F.);
#61329=ORIENTED_EDGE('',*,*,#42325,.T.);
#61330=ORIENTED_EDGE('',*,*,#42329,.T.);
#61331=ORIENTED_EDGE('',*,*,#42320,.T.);
#61332=ORIENTED_EDGE('',*,*,#42327,.T.);
#61333=ORIENTED_EDGE('',*,*,#42328,.T.);
#61334=ORIENTED_EDGE('',*,*,#42323,.T.);
#61335=ORIENTED_EDGE('',*,*,#42586,.T.);
#61336=ORIENTED_EDGE('',*,*,#42587,.F.);
#61337=ORIENTED_EDGE('',*,*,#42588,.F.);
#61338=ORIENTED_EDGE('',*,*,#42589,.F.);
#61339=ORIENTED_EDGE('',*,*,#42335,.T.);
#61340=ORIENTED_EDGE('',*,*,#42339,.T.);
#61341=ORIENTED_EDGE('',*,*,#42330,.T.);
#61342=ORIENTED_EDGE('',*,*,#42337,.T.);
#61343=ORIENTED_EDGE('',*,*,#42338,.T.);
#61344=ORIENTED_EDGE('',*,*,#42333,.T.);
#61345=ORIENTED_EDGE('',*,*,#42589,.T.);
#61346=ORIENTED_EDGE('',*,*,#42590,.F.);
#61347=ORIENTED_EDGE('',*,*,#42591,.F.);
#61348=ORIENTED_EDGE('',*,*,#42592,.F.);
#61349=ORIENTED_EDGE('',*,*,#42345,.T.);
#61350=ORIENTED_EDGE('',*,*,#42349,.T.);
#61351=ORIENTED_EDGE('',*,*,#42340,.T.);
#61352=ORIENTED_EDGE('',*,*,#42347,.T.);
#61353=ORIENTED_EDGE('',*,*,#42348,.T.);
#61354=ORIENTED_EDGE('',*,*,#42343,.T.);
#61355=ORIENTED_EDGE('',*,*,#42592,.T.);
#61356=ORIENTED_EDGE('',*,*,#42593,.F.);
#61357=ORIENTED_EDGE('',*,*,#42594,.F.);
#61358=ORIENTED_EDGE('',*,*,#42595,.F.);
#61359=ORIENTED_EDGE('',*,*,#42355,.T.);
#61360=ORIENTED_EDGE('',*,*,#42359,.T.);
#61361=ORIENTED_EDGE('',*,*,#42350,.T.);
#61362=ORIENTED_EDGE('',*,*,#42357,.T.);
#61363=ORIENTED_EDGE('',*,*,#42358,.T.);
#61364=ORIENTED_EDGE('',*,*,#42353,.T.);
#61365=ORIENTED_EDGE('',*,*,#42595,.T.);
#61366=ORIENTED_EDGE('',*,*,#42596,.F.);
#61367=ORIENTED_EDGE('',*,*,#42597,.F.);
#61368=ORIENTED_EDGE('',*,*,#42598,.F.);
#61369=ORIENTED_EDGE('',*,*,#42365,.T.);
#61370=ORIENTED_EDGE('',*,*,#42369,.T.);
#61371=ORIENTED_EDGE('',*,*,#42360,.T.);
#61372=ORIENTED_EDGE('',*,*,#42367,.T.);
#61373=ORIENTED_EDGE('',*,*,#42368,.T.);
#61374=ORIENTED_EDGE('',*,*,#42363,.T.);
#61375=ORIENTED_EDGE('',*,*,#42598,.T.);
#61376=ORIENTED_EDGE('',*,*,#42599,.F.);
#61377=ORIENTED_EDGE('',*,*,#42600,.F.);
#61378=ORIENTED_EDGE('',*,*,#42601,.F.);
#61379=ORIENTED_EDGE('',*,*,#42375,.T.);
#61380=ORIENTED_EDGE('',*,*,#42379,.T.);
#61381=ORIENTED_EDGE('',*,*,#42370,.T.);
#61382=ORIENTED_EDGE('',*,*,#42377,.T.);
#61383=ORIENTED_EDGE('',*,*,#42378,.T.);
#61384=ORIENTED_EDGE('',*,*,#42373,.T.);
#61385=ORIENTED_EDGE('',*,*,#42601,.T.);
#61386=ORIENTED_EDGE('',*,*,#42602,.F.);
#61387=ORIENTED_EDGE('',*,*,#42603,.F.);
#61388=ORIENTED_EDGE('',*,*,#42604,.F.);
#61389=ORIENTED_EDGE('',*,*,#34367,.T.);
#61390=ORIENTED_EDGE('',*,*,#34366,.T.);
#61391=ORIENTED_EDGE('',*,*,#42380,.T.);
#61392=ORIENTED_EDGE('',*,*,#42382,.T.);
#61393=ORIENTED_EDGE('',*,*,#34363,.T.);
#61394=ORIENTED_EDGE('',*,*,#34368,.T.);
#61395=ORIENTED_EDGE('',*,*,#42604,.T.);
#61396=ORIENTED_EDGE('',*,*,#42605,.F.);
#61397=ORIENTED_EDGE('',*,*,#42606,.F.);
#61398=ORIENTED_EDGE('',*,*,#42607,.F.);
#61399=ORIENTED_EDGE('',*,*,#42388,.T.);
#61400=ORIENTED_EDGE('',*,*,#42392,.T.);
#61401=ORIENTED_EDGE('',*,*,#42383,.T.);
#61402=ORIENTED_EDGE('',*,*,#42390,.T.);
#61403=ORIENTED_EDGE('',*,*,#42391,.T.);
#61404=ORIENTED_EDGE('',*,*,#42386,.T.);
#61405=ORIENTED_EDGE('',*,*,#42607,.T.);
#61406=ORIENTED_EDGE('',*,*,#42608,.F.);
#61407=ORIENTED_EDGE('',*,*,#42609,.F.);
#61408=ORIENTED_EDGE('',*,*,#42610,.F.);
#61409=ORIENTED_EDGE('',*,*,#42398,.T.);
#61410=ORIENTED_EDGE('',*,*,#42402,.T.);
#61411=ORIENTED_EDGE('',*,*,#42393,.T.);
#61412=ORIENTED_EDGE('',*,*,#42400,.T.);
#61413=ORIENTED_EDGE('',*,*,#42401,.T.);
#61414=ORIENTED_EDGE('',*,*,#42396,.T.);
#61415=ORIENTED_EDGE('',*,*,#42610,.T.);
#61416=ORIENTED_EDGE('',*,*,#42611,.F.);
#61417=ORIENTED_EDGE('',*,*,#42612,.F.);
#61418=ORIENTED_EDGE('',*,*,#42613,.F.);
#61419=ORIENTED_EDGE('',*,*,#42406,.T.);
#61420=ORIENTED_EDGE('',*,*,#42412,.T.);
#61421=ORIENTED_EDGE('',*,*,#42403,.T.);
#61422=ORIENTED_EDGE('',*,*,#42410,.T.);
#61423=ORIENTED_EDGE('',*,*,#42411,.T.);
#61424=ORIENTED_EDGE('',*,*,#42407,.T.);
#61425=ORIENTED_EDGE('',*,*,#42613,.T.);
#61426=ORIENTED_EDGE('',*,*,#42614,.F.);
#61427=ORIENTED_EDGE('',*,*,#42615,.F.);
#61428=ORIENTED_EDGE('',*,*,#42616,.F.);
#61429=ORIENTED_EDGE('',*,*,#42418,.T.);
#61430=ORIENTED_EDGE('',*,*,#42422,.T.);
#61431=ORIENTED_EDGE('',*,*,#42413,.T.);
#61432=ORIENTED_EDGE('',*,*,#42420,.T.);
#61433=ORIENTED_EDGE('',*,*,#42421,.T.);
#61434=ORIENTED_EDGE('',*,*,#42416,.T.);
#61435=ORIENTED_EDGE('',*,*,#42616,.T.);
#61436=ORIENTED_EDGE('',*,*,#42617,.F.);
#61437=ORIENTED_EDGE('',*,*,#42618,.F.);
#61438=ORIENTED_EDGE('',*,*,#42619,.F.);
#61439=ORIENTED_EDGE('',*,*,#42428,.T.);
#61440=ORIENTED_EDGE('',*,*,#42432,.T.);
#61441=ORIENTED_EDGE('',*,*,#42423,.T.);
#61442=ORIENTED_EDGE('',*,*,#42430,.T.);
#61443=ORIENTED_EDGE('',*,*,#42431,.T.);
#61444=ORIENTED_EDGE('',*,*,#42426,.T.);
#61445=ORIENTED_EDGE('',*,*,#42619,.T.);
#61446=ORIENTED_EDGE('',*,*,#42620,.F.);
#61447=ORIENTED_EDGE('',*,*,#42621,.F.);
#61448=ORIENTED_EDGE('',*,*,#42622,.F.);
#61449=ORIENTED_EDGE('',*,*,#42438,.T.);
#61450=ORIENTED_EDGE('',*,*,#42442,.T.);
#61451=ORIENTED_EDGE('',*,*,#42433,.T.);
#61452=ORIENTED_EDGE('',*,*,#42440,.T.);
#61453=ORIENTED_EDGE('',*,*,#42441,.T.);
#61454=ORIENTED_EDGE('',*,*,#42436,.T.);
#61455=ORIENTED_EDGE('',*,*,#42622,.T.);
#61456=ORIENTED_EDGE('',*,*,#42623,.F.);
#61457=ORIENTED_EDGE('',*,*,#42624,.F.);
#61458=ORIENTED_EDGE('',*,*,#42625,.F.);
#61459=ORIENTED_EDGE('',*,*,#42448,.T.);
#61460=ORIENTED_EDGE('',*,*,#42452,.T.);
#61461=ORIENTED_EDGE('',*,*,#42443,.T.);
#61462=ORIENTED_EDGE('',*,*,#42450,.T.);
#61463=ORIENTED_EDGE('',*,*,#42451,.T.);
#61464=ORIENTED_EDGE('',*,*,#42446,.T.);
#61465=ORIENTED_EDGE('',*,*,#42625,.T.);
#61466=ORIENTED_EDGE('',*,*,#42626,.F.);
#61467=ORIENTED_EDGE('',*,*,#42627,.T.);
#61468=ORIENTED_EDGE('',*,*,#42628,.F.);
#61469=ORIENTED_EDGE('',*,*,#42453,.T.);
#61470=ORIENTED_EDGE('',*,*,#42629,.F.);
#61471=ORIENTED_EDGE('',*,*,#42630,.T.);
#61472=ORIENTED_EDGE('',*,*,#42631,.F.);
#61473=ORIENTED_EDGE('',*,*,#42455,.T.);
#61474=ORIENTED_EDGE('',*,*,#42632,.F.);
#61475=ORIENTED_EDGE('',*,*,#42633,.F.);
#61476=ORIENTED_EDGE('',*,*,#42634,.F.);
#61477=ORIENTED_EDGE('',*,*,#42635,.F.);
#61478=ORIENTED_EDGE('',*,*,#42630,.F.);
#61479=ORIENTED_EDGE('',*,*,#42635,.T.);
#61480=ORIENTED_EDGE('',*,*,#42636,.F.);
#61481=ORIENTED_EDGE('',*,*,#42456,.T.);
#61482=ORIENTED_EDGE('',*,*,#42631,.T.);
#61483=ORIENTED_EDGE('',*,*,#42637,.T.);
#61484=ORIENTED_EDGE('',*,*,#42638,.F.);
#61485=ORIENTED_EDGE('',*,*,#42458,.T.);
#61486=ORIENTED_EDGE('',*,*,#42639,.F.);
#61487=ORIENTED_EDGE('',*,*,#42640,.F.);
#61488=ORIENTED_EDGE('',*,*,#42641,.F.);
#61489=ORIENTED_EDGE('',*,*,#42642,.F.);
#61490=ORIENTED_EDGE('',*,*,#42637,.F.);
#61491=ORIENTED_EDGE('',*,*,#42642,.T.);
#61492=ORIENTED_EDGE('',*,*,#42643,.F.);
#61493=ORIENTED_EDGE('',*,*,#42459,.T.);
#61494=ORIENTED_EDGE('',*,*,#42638,.T.);
#61495=ORIENTED_EDGE('',*,*,#42644,.T.);
#61496=ORIENTED_EDGE('',*,*,#42645,.F.);
#61497=ORIENTED_EDGE('',*,*,#42461,.T.);
#61498=ORIENTED_EDGE('',*,*,#42646,.F.);
#61499=ORIENTED_EDGE('',*,*,#42647,.F.);
#61500=ORIENTED_EDGE('',*,*,#42648,.F.);
#61501=ORIENTED_EDGE('',*,*,#42649,.F.);
#61502=ORIENTED_EDGE('',*,*,#42644,.F.);
#61503=ORIENTED_EDGE('',*,*,#42649,.T.);
#61504=ORIENTED_EDGE('',*,*,#42650,.F.);
#61505=ORIENTED_EDGE('',*,*,#42462,.T.);
#61506=ORIENTED_EDGE('',*,*,#42645,.T.);
#61507=ORIENTED_EDGE('',*,*,#42651,.T.);
#61508=ORIENTED_EDGE('',*,*,#42652,.F.);
#61509=ORIENTED_EDGE('',*,*,#42464,.T.);
#61510=ORIENTED_EDGE('',*,*,#42653,.F.);
#61511=ORIENTED_EDGE('',*,*,#42654,.F.);
#61512=ORIENTED_EDGE('',*,*,#42655,.F.);
#61513=ORIENTED_EDGE('',*,*,#42656,.F.);
#61514=ORIENTED_EDGE('',*,*,#42651,.F.);
#61515=ORIENTED_EDGE('',*,*,#42656,.T.);
#61516=ORIENTED_EDGE('',*,*,#42657,.F.);
#61517=ORIENTED_EDGE('',*,*,#42465,.T.);
#61518=ORIENTED_EDGE('',*,*,#42652,.T.);
#61519=ORIENTED_EDGE('',*,*,#42658,.T.);
#61520=ORIENTED_EDGE('',*,*,#42659,.F.);
#61521=ORIENTED_EDGE('',*,*,#42467,.T.);
#61522=ORIENTED_EDGE('',*,*,#42660,.F.);
#61523=ORIENTED_EDGE('',*,*,#42661,.F.);
#61524=ORIENTED_EDGE('',*,*,#42662,.F.);
#61525=ORIENTED_EDGE('',*,*,#42663,.F.);
#61526=ORIENTED_EDGE('',*,*,#42658,.F.);
#61527=ORIENTED_EDGE('',*,*,#42663,.T.);
#61528=ORIENTED_EDGE('',*,*,#42664,.F.);
#61529=ORIENTED_EDGE('',*,*,#42468,.T.);
#61530=ORIENTED_EDGE('',*,*,#42659,.T.);
#61531=ORIENTED_EDGE('',*,*,#42665,.T.);
#61532=ORIENTED_EDGE('',*,*,#42666,.F.);
#61533=ORIENTED_EDGE('',*,*,#42470,.T.);
#61534=ORIENTED_EDGE('',*,*,#42667,.F.);
#61535=ORIENTED_EDGE('',*,*,#42668,.F.);
#61536=ORIENTED_EDGE('',*,*,#42669,.F.);
#61537=ORIENTED_EDGE('',*,*,#42670,.F.);
#61538=ORIENTED_EDGE('',*,*,#42665,.F.);
#61539=ORIENTED_EDGE('',*,*,#42670,.T.);
#61540=ORIENTED_EDGE('',*,*,#42671,.F.);
#61541=ORIENTED_EDGE('',*,*,#42471,.T.);
#61542=ORIENTED_EDGE('',*,*,#42666,.T.);
#61543=ORIENTED_EDGE('',*,*,#34359,.T.);
#61544=ORIENTED_EDGE('',*,*,#42672,.F.);
#61545=ORIENTED_EDGE('',*,*,#42473,.T.);
#61546=ORIENTED_EDGE('',*,*,#42673,.F.);
#61547=ORIENTED_EDGE('',*,*,#34358,.T.);
#61548=ORIENTED_EDGE('',*,*,#42674,.F.);
#61549=ORIENTED_EDGE('',*,*,#42474,.T.);
#61550=ORIENTED_EDGE('',*,*,#42672,.T.);
#61551=ORIENTED_EDGE('',*,*,#42675,.T.);
#61552=ORIENTED_EDGE('',*,*,#42676,.F.);
#61553=ORIENTED_EDGE('',*,*,#42476,.T.);
#61554=ORIENTED_EDGE('',*,*,#42677,.F.);
#61555=ORIENTED_EDGE('',*,*,#42678,.F.);
#61556=ORIENTED_EDGE('',*,*,#42679,.F.);
#61557=ORIENTED_EDGE('',*,*,#42680,.F.);
#61558=ORIENTED_EDGE('',*,*,#42675,.F.);
#61559=ORIENTED_EDGE('',*,*,#42680,.T.);
#61560=ORIENTED_EDGE('',*,*,#42681,.F.);
#61561=ORIENTED_EDGE('',*,*,#42477,.T.);
#61562=ORIENTED_EDGE('',*,*,#42676,.T.);
#61563=ORIENTED_EDGE('',*,*,#42682,.T.);
#61564=ORIENTED_EDGE('',*,*,#42683,.F.);
#61565=ORIENTED_EDGE('',*,*,#42479,.T.);
#61566=ORIENTED_EDGE('',*,*,#42684,.F.);
#61567=ORIENTED_EDGE('',*,*,#42685,.F.);
#61568=ORIENTED_EDGE('',*,*,#42686,.F.);
#61569=ORIENTED_EDGE('',*,*,#42687,.F.);
#61570=ORIENTED_EDGE('',*,*,#42682,.F.);
#61571=ORIENTED_EDGE('',*,*,#42687,.T.);
#61572=ORIENTED_EDGE('',*,*,#42688,.F.);
#61573=ORIENTED_EDGE('',*,*,#42480,.T.);
#61574=ORIENTED_EDGE('',*,*,#42683,.T.);
#61575=ORIENTED_EDGE('',*,*,#42689,.T.);
#61576=ORIENTED_EDGE('',*,*,#42690,.F.);
#61577=ORIENTED_EDGE('',*,*,#42482,.T.);
#61578=ORIENTED_EDGE('',*,*,#42691,.F.);
#61579=ORIENTED_EDGE('',*,*,#42692,.F.);
#61580=ORIENTED_EDGE('',*,*,#42693,.F.);
#61581=ORIENTED_EDGE('',*,*,#42694,.F.);
#61582=ORIENTED_EDGE('',*,*,#42689,.F.);
#61583=ORIENTED_EDGE('',*,*,#42694,.T.);
#61584=ORIENTED_EDGE('',*,*,#42695,.F.);
#61585=ORIENTED_EDGE('',*,*,#42483,.T.);
#61586=ORIENTED_EDGE('',*,*,#42690,.T.);
#61587=ORIENTED_EDGE('',*,*,#42696,.T.);
#61588=ORIENTED_EDGE('',*,*,#42697,.F.);
#61589=ORIENTED_EDGE('',*,*,#42485,.T.);
#61590=ORIENTED_EDGE('',*,*,#42698,.F.);
#61591=ORIENTED_EDGE('',*,*,#42699,.F.);
#61592=ORIENTED_EDGE('',*,*,#42700,.F.);
#61593=ORIENTED_EDGE('',*,*,#42701,.F.);
#61594=ORIENTED_EDGE('',*,*,#42696,.F.);
#61595=ORIENTED_EDGE('',*,*,#42701,.T.);
#61596=ORIENTED_EDGE('',*,*,#42702,.F.);
#61597=ORIENTED_EDGE('',*,*,#42486,.T.);
#61598=ORIENTED_EDGE('',*,*,#42697,.T.);
#61599=ORIENTED_EDGE('',*,*,#42703,.T.);
#61600=ORIENTED_EDGE('',*,*,#42704,.F.);
#61601=ORIENTED_EDGE('',*,*,#42488,.T.);
#61602=ORIENTED_EDGE('',*,*,#42705,.F.);
#61603=ORIENTED_EDGE('',*,*,#42706,.F.);
#61604=ORIENTED_EDGE('',*,*,#42707,.F.);
#61605=ORIENTED_EDGE('',*,*,#42708,.F.);
#61606=ORIENTED_EDGE('',*,*,#42703,.F.);
#61607=ORIENTED_EDGE('',*,*,#42708,.T.);
#61608=ORIENTED_EDGE('',*,*,#42709,.F.);
#61609=ORIENTED_EDGE('',*,*,#42489,.T.);
#61610=ORIENTED_EDGE('',*,*,#42704,.T.);
#61611=ORIENTED_EDGE('',*,*,#42710,.T.);
#61612=ORIENTED_EDGE('',*,*,#42711,.F.);
#61613=ORIENTED_EDGE('',*,*,#42491,.T.);
#61614=ORIENTED_EDGE('',*,*,#42712,.F.);
#61615=ORIENTED_EDGE('',*,*,#42713,.F.);
#61616=ORIENTED_EDGE('',*,*,#42714,.F.);
#61617=ORIENTED_EDGE('',*,*,#42715,.F.);
#61618=ORIENTED_EDGE('',*,*,#42710,.F.);
#61619=ORIENTED_EDGE('',*,*,#42715,.T.);
#61620=ORIENTED_EDGE('',*,*,#42716,.F.);
#61621=ORIENTED_EDGE('',*,*,#42492,.T.);
#61622=ORIENTED_EDGE('',*,*,#42711,.T.);
#61623=ORIENTED_EDGE('',*,*,#42717,.T.);
#61624=ORIENTED_EDGE('',*,*,#42718,.F.);
#61625=ORIENTED_EDGE('',*,*,#42494,.T.);
#61626=ORIENTED_EDGE('',*,*,#42719,.F.);
#61627=ORIENTED_EDGE('',*,*,#42720,.F.);
#61628=ORIENTED_EDGE('',*,*,#42721,.F.);
#61629=ORIENTED_EDGE('',*,*,#42722,.F.);
#61630=ORIENTED_EDGE('',*,*,#42717,.F.);
#61631=ORIENTED_EDGE('',*,*,#42722,.T.);
#61632=ORIENTED_EDGE('',*,*,#42723,.F.);
#61633=ORIENTED_EDGE('',*,*,#42495,.T.);
#61634=ORIENTED_EDGE('',*,*,#42718,.T.);
#61635=ORIENTED_EDGE('',*,*,#42724,.T.);
#61636=ORIENTED_EDGE('',*,*,#42725,.F.);
#61637=ORIENTED_EDGE('',*,*,#42497,.T.);
#61638=ORIENTED_EDGE('',*,*,#42726,.F.);
#61639=ORIENTED_EDGE('',*,*,#42727,.F.);
#61640=ORIENTED_EDGE('',*,*,#42728,.F.);
#61641=ORIENTED_EDGE('',*,*,#42729,.F.);
#61642=ORIENTED_EDGE('',*,*,#42724,.F.);
#61643=ORIENTED_EDGE('',*,*,#42729,.T.);
#61644=ORIENTED_EDGE('',*,*,#42730,.F.);
#61645=ORIENTED_EDGE('',*,*,#42498,.T.);
#61646=ORIENTED_EDGE('',*,*,#42725,.T.);
#61647=ORIENTED_EDGE('',*,*,#42731,.T.);
#61648=ORIENTED_EDGE('',*,*,#42732,.F.);
#61649=ORIENTED_EDGE('',*,*,#42500,.T.);
#61650=ORIENTED_EDGE('',*,*,#42733,.F.);
#61651=ORIENTED_EDGE('',*,*,#42734,.F.);
#61652=ORIENTED_EDGE('',*,*,#42735,.F.);
#61653=ORIENTED_EDGE('',*,*,#42736,.F.);
#61654=ORIENTED_EDGE('',*,*,#42731,.F.);
#61655=ORIENTED_EDGE('',*,*,#42736,.T.);
#61656=ORIENTED_EDGE('',*,*,#42737,.F.);
#61657=ORIENTED_EDGE('',*,*,#42501,.T.);
#61658=ORIENTED_EDGE('',*,*,#42732,.T.);
#61659=ORIENTED_EDGE('',*,*,#42738,.T.);
#61660=ORIENTED_EDGE('',*,*,#42739,.F.);
#61661=ORIENTED_EDGE('',*,*,#42503,.T.);
#61662=ORIENTED_EDGE('',*,*,#42740,.F.);
#61663=ORIENTED_EDGE('',*,*,#42741,.F.);
#61664=ORIENTED_EDGE('',*,*,#42742,.F.);
#61665=ORIENTED_EDGE('',*,*,#42743,.F.);
#61666=ORIENTED_EDGE('',*,*,#42738,.F.);
#61667=ORIENTED_EDGE('',*,*,#42743,.T.);
#61668=ORIENTED_EDGE('',*,*,#42744,.F.);
#61669=ORIENTED_EDGE('',*,*,#42504,.T.);
#61670=ORIENTED_EDGE('',*,*,#42739,.T.);
#61671=ORIENTED_EDGE('',*,*,#42745,.T.);
#61672=ORIENTED_EDGE('',*,*,#42746,.F.);
#61673=ORIENTED_EDGE('',*,*,#42506,.T.);
#61674=ORIENTED_EDGE('',*,*,#42747,.F.);
#61675=ORIENTED_EDGE('',*,*,#42748,.T.);
#61676=ORIENTED_EDGE('',*,*,#42749,.F.);
#61677=ORIENTED_EDGE('',*,*,#42507,.T.);
#61678=ORIENTED_EDGE('',*,*,#42746,.T.);
#61679=ORIENTED_EDGE('',*,*,#42750,.F.);
#61680=ORIENTED_EDGE('',*,*,#42751,.F.);
#61681=ORIENTED_EDGE('',*,*,#42748,.F.);
#61682=ORIENTED_EDGE('',*,*,#42745,.F.);
#61683=ORIENTED_EDGE('',*,*,#42509,.T.);
#61684=ORIENTED_EDGE('',*,*,#42752,.F.);
#61685=ORIENTED_EDGE('',*,*,#42753,.T.);
#61686=ORIENTED_EDGE('',*,*,#42754,.F.);
#61687=ORIENTED_EDGE('',*,*,#42755,.F.);
#61688=ORIENTED_EDGE('',*,*,#42753,.F.);
#61689=ORIENTED_EDGE('',*,*,#42756,.F.);
#61690=ORIENTED_EDGE('',*,*,#42757,.F.);
#61691=ORIENTED_EDGE('',*,*,#42510,.T.);
#61692=ORIENTED_EDGE('',*,*,#42754,.T.);
#61693=ORIENTED_EDGE('',*,*,#42755,.T.);
#61694=ORIENTED_EDGE('',*,*,#42758,.F.);
#61695=ORIENTED_EDGE('',*,*,#42759,.T.);
#61696=ORIENTED_EDGE('',*,*,#42760,.F.);
#61697=ORIENTED_EDGE('',*,*,#42512,.T.);
#61698=ORIENTED_EDGE('',*,*,#42761,.F.);
#61699=ORIENTED_EDGE('',*,*,#42762,.F.);
#61700=ORIENTED_EDGE('',*,*,#42763,.F.);
#61701=ORIENTED_EDGE('',*,*,#42764,.F.);
#61702=ORIENTED_EDGE('',*,*,#42759,.F.);
#61703=ORIENTED_EDGE('',*,*,#42764,.T.);
#61704=ORIENTED_EDGE('',*,*,#42765,.F.);
#61705=ORIENTED_EDGE('',*,*,#42513,.T.);
#61706=ORIENTED_EDGE('',*,*,#42760,.T.);
#61707=ORIENTED_EDGE('',*,*,#42766,.T.);
#61708=ORIENTED_EDGE('',*,*,#42767,.F.);
#61709=ORIENTED_EDGE('',*,*,#42515,.T.);
#61710=ORIENTED_EDGE('',*,*,#42768,.F.);
#61711=ORIENTED_EDGE('',*,*,#42769,.F.);
#61712=ORIENTED_EDGE('',*,*,#42770,.F.);
#61713=ORIENTED_EDGE('',*,*,#42771,.F.);
#61714=ORIENTED_EDGE('',*,*,#42766,.F.);
#61715=ORIENTED_EDGE('',*,*,#42771,.T.);
#61716=ORIENTED_EDGE('',*,*,#42772,.F.);
#61717=ORIENTED_EDGE('',*,*,#42516,.T.);
#61718=ORIENTED_EDGE('',*,*,#42767,.T.);
#61719=ORIENTED_EDGE('',*,*,#42773,.T.);
#61720=ORIENTED_EDGE('',*,*,#42774,.F.);
#61721=ORIENTED_EDGE('',*,*,#42518,.T.);
#61722=ORIENTED_EDGE('',*,*,#42775,.F.);
#61723=ORIENTED_EDGE('',*,*,#42776,.F.);
#61724=ORIENTED_EDGE('',*,*,#42777,.F.);
#61725=ORIENTED_EDGE('',*,*,#42778,.F.);
#61726=ORIENTED_EDGE('',*,*,#42773,.F.);
#61727=ORIENTED_EDGE('',*,*,#42778,.T.);
#61728=ORIENTED_EDGE('',*,*,#42779,.F.);
#61729=ORIENTED_EDGE('',*,*,#42519,.T.);
#61730=ORIENTED_EDGE('',*,*,#42774,.T.);
#61731=ORIENTED_EDGE('',*,*,#42780,.T.);
#61732=ORIENTED_EDGE('',*,*,#42781,.F.);
#61733=ORIENTED_EDGE('',*,*,#42521,.T.);
#61734=ORIENTED_EDGE('',*,*,#42782,.F.);
#61735=ORIENTED_EDGE('',*,*,#42783,.F.);
#61736=ORIENTED_EDGE('',*,*,#42784,.F.);
#61737=ORIENTED_EDGE('',*,*,#42785,.F.);
#61738=ORIENTED_EDGE('',*,*,#42780,.F.);
#61739=ORIENTED_EDGE('',*,*,#42785,.T.);
#61740=ORIENTED_EDGE('',*,*,#42786,.F.);
#61741=ORIENTED_EDGE('',*,*,#42522,.T.);
#61742=ORIENTED_EDGE('',*,*,#42781,.T.);
#61743=ORIENTED_EDGE('',*,*,#42787,.T.);
#61744=ORIENTED_EDGE('',*,*,#42788,.F.);
#61745=ORIENTED_EDGE('',*,*,#42524,.T.);
#61746=ORIENTED_EDGE('',*,*,#42789,.F.);
#61747=ORIENTED_EDGE('',*,*,#42790,.F.);
#61748=ORIENTED_EDGE('',*,*,#42791,.F.);
#61749=ORIENTED_EDGE('',*,*,#42792,.F.);
#61750=ORIENTED_EDGE('',*,*,#42787,.F.);
#61751=ORIENTED_EDGE('',*,*,#42792,.T.);
#61752=ORIENTED_EDGE('',*,*,#42793,.F.);
#61753=ORIENTED_EDGE('',*,*,#42525,.T.);
#61754=ORIENTED_EDGE('',*,*,#42788,.T.);
#61755=ORIENTED_EDGE('',*,*,#42794,.T.);
#61756=ORIENTED_EDGE('',*,*,#42795,.F.);
#61757=ORIENTED_EDGE('',*,*,#42527,.T.);
#61758=ORIENTED_EDGE('',*,*,#42796,.F.);
#61759=ORIENTED_EDGE('',*,*,#42797,.F.);
#61760=ORIENTED_EDGE('',*,*,#42798,.F.);
#61761=ORIENTED_EDGE('',*,*,#42799,.F.);
#61762=ORIENTED_EDGE('',*,*,#42794,.F.);
#61763=ORIENTED_EDGE('',*,*,#42799,.T.);
#61764=ORIENTED_EDGE('',*,*,#42800,.F.);
#61765=ORIENTED_EDGE('',*,*,#42528,.T.);
#61766=ORIENTED_EDGE('',*,*,#42795,.T.);
#61767=ORIENTED_EDGE('',*,*,#42801,.T.);
#61768=ORIENTED_EDGE('',*,*,#42802,.F.);
#61769=ORIENTED_EDGE('',*,*,#42530,.T.);
#61770=ORIENTED_EDGE('',*,*,#42803,.F.);
#61771=ORIENTED_EDGE('',*,*,#42804,.F.);
#61772=ORIENTED_EDGE('',*,*,#42805,.F.);
#61773=ORIENTED_EDGE('',*,*,#42806,.F.);
#61774=ORIENTED_EDGE('',*,*,#42801,.F.);
#61775=ORIENTED_EDGE('',*,*,#42806,.T.);
#61776=ORIENTED_EDGE('',*,*,#42807,.F.);
#61777=ORIENTED_EDGE('',*,*,#42531,.T.);
#61778=ORIENTED_EDGE('',*,*,#42802,.T.);
#61779=ORIENTED_EDGE('',*,*,#42808,.T.);
#61780=ORIENTED_EDGE('',*,*,#42809,.F.);
#61781=ORIENTED_EDGE('',*,*,#42533,.T.);
#61782=ORIENTED_EDGE('',*,*,#42810,.F.);
#61783=ORIENTED_EDGE('',*,*,#42811,.F.);
#61784=ORIENTED_EDGE('',*,*,#42812,.F.);
#61785=ORIENTED_EDGE('',*,*,#42813,.F.);
#61786=ORIENTED_EDGE('',*,*,#42808,.F.);
#61787=ORIENTED_EDGE('',*,*,#42813,.T.);
#61788=ORIENTED_EDGE('',*,*,#42814,.F.);
#61789=ORIENTED_EDGE('',*,*,#42534,.T.);
#61790=ORIENTED_EDGE('',*,*,#42809,.T.);
#61791=ORIENTED_EDGE('',*,*,#42815,.T.);
#61792=ORIENTED_EDGE('',*,*,#42816,.F.);
#61793=ORIENTED_EDGE('',*,*,#42536,.T.);
#61794=ORIENTED_EDGE('',*,*,#42817,.F.);
#61795=ORIENTED_EDGE('',*,*,#42818,.F.);
#61796=ORIENTED_EDGE('',*,*,#42819,.F.);
#61797=ORIENTED_EDGE('',*,*,#42820,.F.);
#61798=ORIENTED_EDGE('',*,*,#42815,.F.);
#61799=ORIENTED_EDGE('',*,*,#42820,.T.);
#61800=ORIENTED_EDGE('',*,*,#42821,.F.);
#61801=ORIENTED_EDGE('',*,*,#42537,.T.);
#61802=ORIENTED_EDGE('',*,*,#42816,.T.);
#61803=ORIENTED_EDGE('',*,*,#42822,.F.);
#61804=ORIENTED_EDGE('',*,*,#42823,.F.);
#61805=ORIENTED_EDGE('',*,*,#42627,.F.);
#61806=ORIENTED_EDGE('',*,*,#42824,.F.);
#61807=ORIENTED_EDGE('',*,*,#42824,.T.);
#61808=ORIENTED_EDGE('',*,*,#42629,.T.);
#61809=ORIENTED_EDGE('',*,*,#42539,.T.);
#61810=ORIENTED_EDGE('',*,*,#42825,.F.);
#61811=ORIENTED_EDGE('',*,*,#42826,.F.);
#61812=ORIENTED_EDGE('',*,*,#42827,.T.);
#61813=ORIENTED_EDGE('',*,*,#42828,.F.);
#61814=ORIENTED_EDGE('',*,*,#42540,.T.);
#61815=ORIENTED_EDGE('',*,*,#42542,.T.);
#61816=ORIENTED_EDGE('',*,*,#42829,.F.);
#61817=ORIENTED_EDGE('',*,*,#42830,.T.);
#61818=ORIENTED_EDGE('',*,*,#42831,.F.);
#61819=ORIENTED_EDGE('',*,*,#42830,.F.);
#61820=ORIENTED_EDGE('',*,*,#42832,.F.);
#61821=ORIENTED_EDGE('',*,*,#42833,.F.);
#61822=ORIENTED_EDGE('',*,*,#42834,.F.);
#61823=ORIENTED_EDGE('',*,*,#42831,.T.);
#61824=ORIENTED_EDGE('',*,*,#42834,.T.);
#61825=ORIENTED_EDGE('',*,*,#42835,.F.);
#61826=ORIENTED_EDGE('',*,*,#42543,.T.);
#61827=ORIENTED_EDGE('',*,*,#42545,.T.);
#61828=ORIENTED_EDGE('',*,*,#42836,.F.);
#61829=ORIENTED_EDGE('',*,*,#42837,.T.);
#61830=ORIENTED_EDGE('',*,*,#42838,.F.);
#61831=ORIENTED_EDGE('',*,*,#42837,.F.);
#61832=ORIENTED_EDGE('',*,*,#42839,.F.);
#61833=ORIENTED_EDGE('',*,*,#42840,.F.);
#61834=ORIENTED_EDGE('',*,*,#42841,.F.);
#61835=ORIENTED_EDGE('',*,*,#42838,.T.);
#61836=ORIENTED_EDGE('',*,*,#42841,.T.);
#61837=ORIENTED_EDGE('',*,*,#42842,.F.);
#61838=ORIENTED_EDGE('',*,*,#42546,.T.);
#61839=ORIENTED_EDGE('',*,*,#42548,.T.);
#61840=ORIENTED_EDGE('',*,*,#42843,.F.);
#61841=ORIENTED_EDGE('',*,*,#42844,.T.);
#61842=ORIENTED_EDGE('',*,*,#42845,.F.);
#61843=ORIENTED_EDGE('',*,*,#42844,.F.);
#61844=ORIENTED_EDGE('',*,*,#42846,.F.);
#61845=ORIENTED_EDGE('',*,*,#42847,.F.);
#61846=ORIENTED_EDGE('',*,*,#42848,.F.);
#61847=ORIENTED_EDGE('',*,*,#42845,.T.);
#61848=ORIENTED_EDGE('',*,*,#42848,.T.);
#61849=ORIENTED_EDGE('',*,*,#42849,.F.);
#61850=ORIENTED_EDGE('',*,*,#42549,.T.);
#61851=ORIENTED_EDGE('',*,*,#42551,.T.);
#61852=ORIENTED_EDGE('',*,*,#42850,.F.);
#61853=ORIENTED_EDGE('',*,*,#42851,.T.);
#61854=ORIENTED_EDGE('',*,*,#42852,.F.);
#61855=ORIENTED_EDGE('',*,*,#42851,.F.);
#61856=ORIENTED_EDGE('',*,*,#42853,.F.);
#61857=ORIENTED_EDGE('',*,*,#42854,.F.);
#61858=ORIENTED_EDGE('',*,*,#42855,.F.);
#61859=ORIENTED_EDGE('',*,*,#42852,.T.);
#61860=ORIENTED_EDGE('',*,*,#42855,.T.);
#61861=ORIENTED_EDGE('',*,*,#42856,.F.);
#61862=ORIENTED_EDGE('',*,*,#42552,.T.);
#61863=ORIENTED_EDGE('',*,*,#42554,.T.);
#61864=ORIENTED_EDGE('',*,*,#42857,.F.);
#61865=ORIENTED_EDGE('',*,*,#42858,.T.);
#61866=ORIENTED_EDGE('',*,*,#42859,.F.);
#61867=ORIENTED_EDGE('',*,*,#42858,.F.);
#61868=ORIENTED_EDGE('',*,*,#42860,.F.);
#61869=ORIENTED_EDGE('',*,*,#42861,.F.);
#61870=ORIENTED_EDGE('',*,*,#42862,.F.);
#61871=ORIENTED_EDGE('',*,*,#42859,.T.);
#61872=ORIENTED_EDGE('',*,*,#42862,.T.);
#61873=ORIENTED_EDGE('',*,*,#42863,.F.);
#61874=ORIENTED_EDGE('',*,*,#42555,.T.);
#61875=ORIENTED_EDGE('',*,*,#42557,.T.);
#61876=ORIENTED_EDGE('',*,*,#42864,.F.);
#61877=ORIENTED_EDGE('',*,*,#42865,.T.);
#61878=ORIENTED_EDGE('',*,*,#42866,.F.);
#61879=ORIENTED_EDGE('',*,*,#42865,.F.);
#61880=ORIENTED_EDGE('',*,*,#42867,.F.);
#61881=ORIENTED_EDGE('',*,*,#42868,.F.);
#61882=ORIENTED_EDGE('',*,*,#42869,.F.);
#61883=ORIENTED_EDGE('',*,*,#42866,.T.);
#61884=ORIENTED_EDGE('',*,*,#42869,.T.);
#61885=ORIENTED_EDGE('',*,*,#42870,.F.);
#61886=ORIENTED_EDGE('',*,*,#42558,.T.);
#61887=ORIENTED_EDGE('',*,*,#42560,.T.);
#61888=ORIENTED_EDGE('',*,*,#42871,.F.);
#61889=ORIENTED_EDGE('',*,*,#42872,.T.);
#61890=ORIENTED_EDGE('',*,*,#42873,.F.);
#61891=ORIENTED_EDGE('',*,*,#42872,.F.);
#61892=ORIENTED_EDGE('',*,*,#42874,.F.);
#61893=ORIENTED_EDGE('',*,*,#42875,.F.);
#61894=ORIENTED_EDGE('',*,*,#42876,.F.);
#61895=ORIENTED_EDGE('',*,*,#42873,.T.);
#61896=ORIENTED_EDGE('',*,*,#42876,.T.);
#61897=ORIENTED_EDGE('',*,*,#42877,.F.);
#61898=ORIENTED_EDGE('',*,*,#42561,.T.);
#61899=ORIENTED_EDGE('',*,*,#42563,.T.);
#61900=ORIENTED_EDGE('',*,*,#42878,.F.);
#61901=ORIENTED_EDGE('',*,*,#42879,.T.);
#61902=ORIENTED_EDGE('',*,*,#42880,.F.);
#61903=ORIENTED_EDGE('',*,*,#42879,.F.);
#61904=ORIENTED_EDGE('',*,*,#42881,.F.);
#61905=ORIENTED_EDGE('',*,*,#42882,.F.);
#61906=ORIENTED_EDGE('',*,*,#42883,.F.);
#61907=ORIENTED_EDGE('',*,*,#42880,.T.);
#61908=ORIENTED_EDGE('',*,*,#42883,.T.);
#61909=ORIENTED_EDGE('',*,*,#42884,.F.);
#61910=ORIENTED_EDGE('',*,*,#42564,.T.);
#61911=ORIENTED_EDGE('',*,*,#42566,.T.);
#61912=ORIENTED_EDGE('',*,*,#42885,.F.);
#61913=ORIENTED_EDGE('',*,*,#42886,.T.);
#61914=ORIENTED_EDGE('',*,*,#42887,.F.);
#61915=ORIENTED_EDGE('',*,*,#42886,.F.);
#61916=ORIENTED_EDGE('',*,*,#42888,.F.);
#61917=ORIENTED_EDGE('',*,*,#42889,.F.);
#61918=ORIENTED_EDGE('',*,*,#42890,.F.);
#61919=ORIENTED_EDGE('',*,*,#42887,.T.);
#61920=ORIENTED_EDGE('',*,*,#42890,.T.);
#61921=ORIENTED_EDGE('',*,*,#42891,.F.);
#61922=ORIENTED_EDGE('',*,*,#42567,.T.);
#61923=ORIENTED_EDGE('',*,*,#42569,.T.);
#61924=ORIENTED_EDGE('',*,*,#42892,.F.);
#61925=ORIENTED_EDGE('',*,*,#42893,.T.);
#61926=ORIENTED_EDGE('',*,*,#42894,.F.);
#61927=ORIENTED_EDGE('',*,*,#42893,.F.);
#61928=ORIENTED_EDGE('',*,*,#42895,.F.);
#61929=ORIENTED_EDGE('',*,*,#42896,.F.);
#61930=ORIENTED_EDGE('',*,*,#42897,.F.);
#61931=ORIENTED_EDGE('',*,*,#42894,.T.);
#61932=ORIENTED_EDGE('',*,*,#42897,.T.);
#61933=ORIENTED_EDGE('',*,*,#42898,.F.);
#61934=ORIENTED_EDGE('',*,*,#42570,.T.);
#61935=ORIENTED_EDGE('',*,*,#42572,.T.);
#61936=ORIENTED_EDGE('',*,*,#42899,.F.);
#61937=ORIENTED_EDGE('',*,*,#42900,.T.);
#61938=ORIENTED_EDGE('',*,*,#42901,.F.);
#61939=ORIENTED_EDGE('',*,*,#42900,.F.);
#61940=ORIENTED_EDGE('',*,*,#42902,.F.);
#61941=ORIENTED_EDGE('',*,*,#42903,.F.);
#61942=ORIENTED_EDGE('',*,*,#42904,.F.);
#61943=ORIENTED_EDGE('',*,*,#42901,.T.);
#61944=ORIENTED_EDGE('',*,*,#42904,.T.);
#61945=ORIENTED_EDGE('',*,*,#42905,.F.);
#61946=ORIENTED_EDGE('',*,*,#42573,.T.);
#61947=ORIENTED_EDGE('',*,*,#42575,.T.);
#61948=ORIENTED_EDGE('',*,*,#42906,.F.);
#61949=ORIENTED_EDGE('',*,*,#42907,.T.);
#61950=ORIENTED_EDGE('',*,*,#42908,.F.);
#61951=ORIENTED_EDGE('',*,*,#42907,.F.);
#61952=ORIENTED_EDGE('',*,*,#42909,.F.);
#61953=ORIENTED_EDGE('',*,*,#42910,.F.);
#61954=ORIENTED_EDGE('',*,*,#42911,.F.);
#61955=ORIENTED_EDGE('',*,*,#42908,.T.);
#61956=ORIENTED_EDGE('',*,*,#42911,.T.);
#61957=ORIENTED_EDGE('',*,*,#42912,.F.);
#61958=ORIENTED_EDGE('',*,*,#42576,.T.);
#61959=ORIENTED_EDGE('',*,*,#42578,.T.);
#61960=ORIENTED_EDGE('',*,*,#42913,.F.);
#61961=ORIENTED_EDGE('',*,*,#42914,.T.);
#61962=ORIENTED_EDGE('',*,*,#42915,.F.);
#61963=ORIENTED_EDGE('',*,*,#42914,.F.);
#61964=ORIENTED_EDGE('',*,*,#42916,.F.);
#61965=ORIENTED_EDGE('',*,*,#42917,.F.);
#61966=ORIENTED_EDGE('',*,*,#42918,.F.);
#61967=ORIENTED_EDGE('',*,*,#42915,.T.);
#61968=ORIENTED_EDGE('',*,*,#42918,.T.);
#61969=ORIENTED_EDGE('',*,*,#42919,.F.);
#61970=ORIENTED_EDGE('',*,*,#42579,.T.);
#61971=ORIENTED_EDGE('',*,*,#42581,.T.);
#61972=ORIENTED_EDGE('',*,*,#42920,.F.);
#61973=ORIENTED_EDGE('',*,*,#34356,.T.);
#61974=ORIENTED_EDGE('',*,*,#42921,.F.);
#61975=ORIENTED_EDGE('',*,*,#34355,.T.);
#61976=ORIENTED_EDGE('',*,*,#42922,.F.);
#61977=ORIENTED_EDGE('',*,*,#42582,.T.);
#61978=ORIENTED_EDGE('',*,*,#42921,.T.);
#61979=ORIENTED_EDGE('',*,*,#42584,.T.);
#61980=ORIENTED_EDGE('',*,*,#42923,.F.);
#61981=ORIENTED_EDGE('',*,*,#42924,.T.);
#61982=ORIENTED_EDGE('',*,*,#42925,.F.);
#61983=ORIENTED_EDGE('',*,*,#42924,.F.);
#61984=ORIENTED_EDGE('',*,*,#42926,.F.);
#61985=ORIENTED_EDGE('',*,*,#42927,.F.);
#61986=ORIENTED_EDGE('',*,*,#42928,.F.);
#61987=ORIENTED_EDGE('',*,*,#42925,.T.);
#61988=ORIENTED_EDGE('',*,*,#42928,.T.);
#61989=ORIENTED_EDGE('',*,*,#42929,.F.);
#61990=ORIENTED_EDGE('',*,*,#42585,.T.);
#61991=ORIENTED_EDGE('',*,*,#42587,.T.);
#61992=ORIENTED_EDGE('',*,*,#42930,.F.);
#61993=ORIENTED_EDGE('',*,*,#42931,.T.);
#61994=ORIENTED_EDGE('',*,*,#42932,.F.);
#61995=ORIENTED_EDGE('',*,*,#42931,.F.);
#61996=ORIENTED_EDGE('',*,*,#42933,.F.);
#61997=ORIENTED_EDGE('',*,*,#42934,.F.);
#61998=ORIENTED_EDGE('',*,*,#42935,.F.);
#61999=ORIENTED_EDGE('',*,*,#42932,.T.);
#62000=ORIENTED_EDGE('',*,*,#42935,.T.);
#62001=ORIENTED_EDGE('',*,*,#42936,.F.);
#62002=ORIENTED_EDGE('',*,*,#42588,.T.);
#62003=ORIENTED_EDGE('',*,*,#42590,.T.);
#62004=ORIENTED_EDGE('',*,*,#42937,.F.);
#62005=ORIENTED_EDGE('',*,*,#42938,.T.);
#62006=ORIENTED_EDGE('',*,*,#42939,.F.);
#62007=ORIENTED_EDGE('',*,*,#42938,.F.);
#62008=ORIENTED_EDGE('',*,*,#42940,.F.);
#62009=ORIENTED_EDGE('',*,*,#42941,.F.);
#62010=ORIENTED_EDGE('',*,*,#42942,.F.);
#62011=ORIENTED_EDGE('',*,*,#42939,.T.);
#62012=ORIENTED_EDGE('',*,*,#42942,.T.);
#62013=ORIENTED_EDGE('',*,*,#42943,.F.);
#62014=ORIENTED_EDGE('',*,*,#42591,.T.);
#62015=ORIENTED_EDGE('',*,*,#42593,.T.);
#62016=ORIENTED_EDGE('',*,*,#42944,.F.);
#62017=ORIENTED_EDGE('',*,*,#42945,.T.);
#62018=ORIENTED_EDGE('',*,*,#42946,.F.);
#62019=ORIENTED_EDGE('',*,*,#42945,.F.);
#62020=ORIENTED_EDGE('',*,*,#42947,.F.);
#62021=ORIENTED_EDGE('',*,*,#42948,.F.);
#62022=ORIENTED_EDGE('',*,*,#42949,.F.);
#62023=ORIENTED_EDGE('',*,*,#42946,.T.);
#62024=ORIENTED_EDGE('',*,*,#42949,.T.);
#62025=ORIENTED_EDGE('',*,*,#42950,.F.);
#62026=ORIENTED_EDGE('',*,*,#42594,.T.);
#62027=ORIENTED_EDGE('',*,*,#42596,.T.);
#62028=ORIENTED_EDGE('',*,*,#42951,.F.);
#62029=ORIENTED_EDGE('',*,*,#42952,.T.);
#62030=ORIENTED_EDGE('',*,*,#42953,.F.);
#62031=ORIENTED_EDGE('',*,*,#42952,.F.);
#62032=ORIENTED_EDGE('',*,*,#42954,.F.);
#62033=ORIENTED_EDGE('',*,*,#42955,.F.);
#62034=ORIENTED_EDGE('',*,*,#42956,.F.);
#62035=ORIENTED_EDGE('',*,*,#42953,.T.);
#62036=ORIENTED_EDGE('',*,*,#42956,.T.);
#62037=ORIENTED_EDGE('',*,*,#42957,.F.);
#62038=ORIENTED_EDGE('',*,*,#42597,.T.);
#62039=ORIENTED_EDGE('',*,*,#42599,.T.);
#62040=ORIENTED_EDGE('',*,*,#42958,.F.);
#62041=ORIENTED_EDGE('',*,*,#42959,.T.);
#62042=ORIENTED_EDGE('',*,*,#42960,.F.);
#62043=ORIENTED_EDGE('',*,*,#42959,.F.);
#62044=ORIENTED_EDGE('',*,*,#42961,.F.);
#62045=ORIENTED_EDGE('',*,*,#42962,.F.);
#62046=ORIENTED_EDGE('',*,*,#42963,.F.);
#62047=ORIENTED_EDGE('',*,*,#42960,.T.);
#62048=ORIENTED_EDGE('',*,*,#42963,.T.);
#62049=ORIENTED_EDGE('',*,*,#42964,.F.);
#62050=ORIENTED_EDGE('',*,*,#42600,.T.);
#62051=ORIENTED_EDGE('',*,*,#42602,.T.);
#62052=ORIENTED_EDGE('',*,*,#42965,.F.);
#62053=ORIENTED_EDGE('',*,*,#34352,.T.);
#62054=ORIENTED_EDGE('',*,*,#42966,.F.);
#62055=ORIENTED_EDGE('',*,*,#42966,.T.);
#62056=ORIENTED_EDGE('',*,*,#34351,.T.);
#62057=ORIENTED_EDGE('',*,*,#42967,.F.);
#62058=ORIENTED_EDGE('',*,*,#42603,.T.);
#62059=ORIENTED_EDGE('',*,*,#42605,.T.);
#62060=ORIENTED_EDGE('',*,*,#42968,.F.);
#62061=ORIENTED_EDGE('',*,*,#42969,.T.);
#62062=ORIENTED_EDGE('',*,*,#42970,.F.);
#62063=ORIENTED_EDGE('',*,*,#42969,.F.);
#62064=ORIENTED_EDGE('',*,*,#42971,.F.);
#62065=ORIENTED_EDGE('',*,*,#42972,.F.);
#62066=ORIENTED_EDGE('',*,*,#42973,.F.);
#62067=ORIENTED_EDGE('',*,*,#42970,.T.);
#62068=ORIENTED_EDGE('',*,*,#42973,.T.);
#62069=ORIENTED_EDGE('',*,*,#42974,.F.);
#62070=ORIENTED_EDGE('',*,*,#42606,.T.);
#62071=ORIENTED_EDGE('',*,*,#42608,.T.);
#62072=ORIENTED_EDGE('',*,*,#42975,.F.);
#62073=ORIENTED_EDGE('',*,*,#42976,.T.);
#62074=ORIENTED_EDGE('',*,*,#42977,.F.);
#62075=ORIENTED_EDGE('',*,*,#42976,.F.);
#62076=ORIENTED_EDGE('',*,*,#42978,.F.);
#62077=ORIENTED_EDGE('',*,*,#42979,.F.);
#62078=ORIENTED_EDGE('',*,*,#42980,.F.);
#62079=ORIENTED_EDGE('',*,*,#42977,.T.);
#62080=ORIENTED_EDGE('',*,*,#42980,.T.);
#62081=ORIENTED_EDGE('',*,*,#42981,.F.);
#62082=ORIENTED_EDGE('',*,*,#42609,.T.);
#62083=ORIENTED_EDGE('',*,*,#42611,.T.);
#62084=ORIENTED_EDGE('',*,*,#42982,.F.);
#62085=ORIENTED_EDGE('',*,*,#42983,.T.);
#62086=ORIENTED_EDGE('',*,*,#42984,.F.);
#62087=ORIENTED_EDGE('',*,*,#42983,.F.);
#62088=ORIENTED_EDGE('',*,*,#42985,.F.);
#62089=ORIENTED_EDGE('',*,*,#42986,.F.);
#62090=ORIENTED_EDGE('',*,*,#42987,.F.);
#62091=ORIENTED_EDGE('',*,*,#42984,.T.);
#62092=ORIENTED_EDGE('',*,*,#42987,.T.);
#62093=ORIENTED_EDGE('',*,*,#42988,.F.);
#62094=ORIENTED_EDGE('',*,*,#42612,.T.);
#62095=ORIENTED_EDGE('',*,*,#42614,.T.);
#62096=ORIENTED_EDGE('',*,*,#42989,.F.);
#62097=ORIENTED_EDGE('',*,*,#42990,.T.);
#62098=ORIENTED_EDGE('',*,*,#42991,.F.);
#62099=ORIENTED_EDGE('',*,*,#42990,.F.);
#62100=ORIENTED_EDGE('',*,*,#42992,.F.);
#62101=ORIENTED_EDGE('',*,*,#42993,.F.);
#62102=ORIENTED_EDGE('',*,*,#42994,.F.);
#62103=ORIENTED_EDGE('',*,*,#42991,.T.);
#62104=ORIENTED_EDGE('',*,*,#42994,.T.);
#62105=ORIENTED_EDGE('',*,*,#42995,.F.);
#62106=ORIENTED_EDGE('',*,*,#42615,.T.);
#62107=ORIENTED_EDGE('',*,*,#42617,.T.);
#62108=ORIENTED_EDGE('',*,*,#42996,.F.);
#62109=ORIENTED_EDGE('',*,*,#42997,.T.);
#62110=ORIENTED_EDGE('',*,*,#42998,.F.);
#62111=ORIENTED_EDGE('',*,*,#42997,.F.);
#62112=ORIENTED_EDGE('',*,*,#42999,.F.);
#62113=ORIENTED_EDGE('',*,*,#43000,.F.);
#62114=ORIENTED_EDGE('',*,*,#43001,.F.);
#62115=ORIENTED_EDGE('',*,*,#42998,.T.);
#62116=ORIENTED_EDGE('',*,*,#43001,.T.);
#62117=ORIENTED_EDGE('',*,*,#43002,.F.);
#62118=ORIENTED_EDGE('',*,*,#42618,.T.);
#62119=ORIENTED_EDGE('',*,*,#42620,.T.);
#62120=ORIENTED_EDGE('',*,*,#43003,.F.);
#62121=ORIENTED_EDGE('',*,*,#43004,.T.);
#62122=ORIENTED_EDGE('',*,*,#43005,.F.);
#62123=ORIENTED_EDGE('',*,*,#43004,.F.);
#62124=ORIENTED_EDGE('',*,*,#43006,.F.);
#62125=ORIENTED_EDGE('',*,*,#43007,.F.);
#62126=ORIENTED_EDGE('',*,*,#43008,.F.);
#62127=ORIENTED_EDGE('',*,*,#43005,.T.);
#62128=ORIENTED_EDGE('',*,*,#43008,.T.);
#62129=ORIENTED_EDGE('',*,*,#43009,.F.);
#62130=ORIENTED_EDGE('',*,*,#42621,.T.);
#62131=ORIENTED_EDGE('',*,*,#42623,.T.);
#62132=ORIENTED_EDGE('',*,*,#43010,.F.);
#62133=ORIENTED_EDGE('',*,*,#43011,.T.);
#62134=ORIENTED_EDGE('',*,*,#43012,.F.);
#62135=ORIENTED_EDGE('',*,*,#43011,.F.);
#62136=ORIENTED_EDGE('',*,*,#43013,.F.);
#62137=ORIENTED_EDGE('',*,*,#43014,.F.);
#62138=ORIENTED_EDGE('',*,*,#43015,.F.);
#62139=ORIENTED_EDGE('',*,*,#43012,.T.);
#62140=ORIENTED_EDGE('',*,*,#43015,.T.);
#62141=ORIENTED_EDGE('',*,*,#43016,.F.);
#62142=ORIENTED_EDGE('',*,*,#42624,.T.);
#62143=ORIENTED_EDGE('',*,*,#43017,.F.);
#62144=ORIENTED_EDGE('',*,*,#43018,.F.);
#62145=ORIENTED_EDGE('',*,*,#43019,.F.);
#62146=ORIENTED_EDGE('',*,*,#42827,.F.);
#62147=ORIENTED_EDGE('',*,*,#42626,.T.);
#62148=ORIENTED_EDGE('',*,*,#43020,.F.);
#62149=ORIENTED_EDGE('',*,*,#43017,.T.);
#62150=ORIENTED_EDGE('',*,*,#42826,.T.);
#62151=ORIENTED_EDGE('',*,*,#43021,.F.);
#62152=ORIENTED_EDGE('',*,*,#42628,.T.);
#62153=ORIENTED_EDGE('',*,*,#42823,.T.);
#62154=ORIENTED_EDGE('',*,*,#43022,.F.);
#62155=ORIENTED_EDGE('',*,*,#43023,.F.);
#62156=ORIENTED_EDGE('',*,*,#43024,.F.);
#62157=ORIENTED_EDGE('',*,*,#42633,.T.);
#62158=ORIENTED_EDGE('',*,*,#42632,.T.);
#62159=ORIENTED_EDGE('',*,*,#43025,.F.);
#62160=ORIENTED_EDGE('',*,*,#42636,.T.);
#62161=ORIENTED_EDGE('',*,*,#42634,.T.);
#62162=ORIENTED_EDGE('',*,*,#43024,.T.);
#62163=ORIENTED_EDGE('',*,*,#43026,.F.);
#62164=ORIENTED_EDGE('',*,*,#43027,.F.);
#62165=ORIENTED_EDGE('',*,*,#42640,.T.);
#62166=ORIENTED_EDGE('',*,*,#42639,.T.);
#62167=ORIENTED_EDGE('',*,*,#43028,.F.);
#62168=ORIENTED_EDGE('',*,*,#42643,.T.);
#62169=ORIENTED_EDGE('',*,*,#42641,.T.);
#62170=ORIENTED_EDGE('',*,*,#43027,.T.);
#62171=ORIENTED_EDGE('',*,*,#43029,.F.);
#62172=ORIENTED_EDGE('',*,*,#43030,.F.);
#62173=ORIENTED_EDGE('',*,*,#42647,.T.);
#62174=ORIENTED_EDGE('',*,*,#42646,.T.);
#62175=ORIENTED_EDGE('',*,*,#43031,.F.);
#62176=ORIENTED_EDGE('',*,*,#42650,.T.);
#62177=ORIENTED_EDGE('',*,*,#42648,.T.);
#62178=ORIENTED_EDGE('',*,*,#43030,.T.);
#62179=ORIENTED_EDGE('',*,*,#43032,.F.);
#62180=ORIENTED_EDGE('',*,*,#43033,.F.);
#62181=ORIENTED_EDGE('',*,*,#42654,.T.);
#62182=ORIENTED_EDGE('',*,*,#42653,.T.);
#62183=ORIENTED_EDGE('',*,*,#43034,.F.);
#62184=ORIENTED_EDGE('',*,*,#42657,.T.);
#62185=ORIENTED_EDGE('',*,*,#42655,.T.);
#62186=ORIENTED_EDGE('',*,*,#43033,.T.);
#62187=ORIENTED_EDGE('',*,*,#43035,.F.);
#62188=ORIENTED_EDGE('',*,*,#43036,.F.);
#62189=ORIENTED_EDGE('',*,*,#42661,.T.);
#62190=ORIENTED_EDGE('',*,*,#42660,.T.);
#62191=ORIENTED_EDGE('',*,*,#43037,.F.);
#62192=ORIENTED_EDGE('',*,*,#42664,.T.);
#62193=ORIENTED_EDGE('',*,*,#42662,.T.);
#62194=ORIENTED_EDGE('',*,*,#43036,.T.);
#62195=ORIENTED_EDGE('',*,*,#43038,.F.);
#62196=ORIENTED_EDGE('',*,*,#43039,.F.);
#62197=ORIENTED_EDGE('',*,*,#42668,.T.);
#62198=ORIENTED_EDGE('',*,*,#42667,.T.);
#62199=ORIENTED_EDGE('',*,*,#43040,.F.);
#62200=ORIENTED_EDGE('',*,*,#42671,.T.);
#62201=ORIENTED_EDGE('',*,*,#42669,.T.);
#62202=ORIENTED_EDGE('',*,*,#43039,.T.);
#62203=ORIENTED_EDGE('',*,*,#43041,.F.);
#62204=ORIENTED_EDGE('',*,*,#43042,.F.);
#62205=ORIENTED_EDGE('',*,*,#34360,.T.);
#62206=ORIENTED_EDGE('',*,*,#42673,.T.);
#62207=ORIENTED_EDGE('',*,*,#43043,.F.);
#62208=ORIENTED_EDGE('',*,*,#42674,.T.);
#62209=ORIENTED_EDGE('',*,*,#34361,.T.);
#62210=ORIENTED_EDGE('',*,*,#43042,.T.);
#62211=ORIENTED_EDGE('',*,*,#43044,.F.);
#62212=ORIENTED_EDGE('',*,*,#43045,.F.);
#62213=ORIENTED_EDGE('',*,*,#42678,.T.);
#62214=ORIENTED_EDGE('',*,*,#42677,.T.);
#62215=ORIENTED_EDGE('',*,*,#43046,.F.);
#62216=ORIENTED_EDGE('',*,*,#42681,.T.);
#62217=ORIENTED_EDGE('',*,*,#42679,.T.);
#62218=ORIENTED_EDGE('',*,*,#43045,.T.);
#62219=ORIENTED_EDGE('',*,*,#43047,.F.);
#62220=ORIENTED_EDGE('',*,*,#43048,.F.);
#62221=ORIENTED_EDGE('',*,*,#42685,.T.);
#62222=ORIENTED_EDGE('',*,*,#42684,.T.);
#62223=ORIENTED_EDGE('',*,*,#43049,.F.);
#62224=ORIENTED_EDGE('',*,*,#42688,.T.);
#62225=ORIENTED_EDGE('',*,*,#42686,.T.);
#62226=ORIENTED_EDGE('',*,*,#43048,.T.);
#62227=ORIENTED_EDGE('',*,*,#43050,.F.);
#62228=ORIENTED_EDGE('',*,*,#43051,.F.);
#62229=ORIENTED_EDGE('',*,*,#42692,.T.);
#62230=ORIENTED_EDGE('',*,*,#42691,.T.);
#62231=ORIENTED_EDGE('',*,*,#43052,.F.);
#62232=ORIENTED_EDGE('',*,*,#42695,.T.);
#62233=ORIENTED_EDGE('',*,*,#42693,.T.);
#62234=ORIENTED_EDGE('',*,*,#43051,.T.);
#62235=ORIENTED_EDGE('',*,*,#43053,.F.);
#62236=ORIENTED_EDGE('',*,*,#43054,.F.);
#62237=ORIENTED_EDGE('',*,*,#42699,.T.);
#62238=ORIENTED_EDGE('',*,*,#42698,.T.);
#62239=ORIENTED_EDGE('',*,*,#43055,.F.);
#62240=ORIENTED_EDGE('',*,*,#42702,.T.);
#62241=ORIENTED_EDGE('',*,*,#42700,.T.);
#62242=ORIENTED_EDGE('',*,*,#43054,.T.);
#62243=ORIENTED_EDGE('',*,*,#43056,.F.);
#62244=ORIENTED_EDGE('',*,*,#43057,.F.);
#62245=ORIENTED_EDGE('',*,*,#42706,.T.);
#62246=ORIENTED_EDGE('',*,*,#42705,.T.);
#62247=ORIENTED_EDGE('',*,*,#43058,.F.);
#62248=ORIENTED_EDGE('',*,*,#42709,.T.);
#62249=ORIENTED_EDGE('',*,*,#42707,.T.);
#62250=ORIENTED_EDGE('',*,*,#43057,.T.);
#62251=ORIENTED_EDGE('',*,*,#43059,.F.);
#62252=ORIENTED_EDGE('',*,*,#43060,.F.);
#62253=ORIENTED_EDGE('',*,*,#42713,.T.);
#62254=ORIENTED_EDGE('',*,*,#42712,.T.);
#62255=ORIENTED_EDGE('',*,*,#43061,.F.);
#62256=ORIENTED_EDGE('',*,*,#42716,.T.);
#62257=ORIENTED_EDGE('',*,*,#42714,.T.);
#62258=ORIENTED_EDGE('',*,*,#43060,.T.);
#62259=ORIENTED_EDGE('',*,*,#43062,.F.);
#62260=ORIENTED_EDGE('',*,*,#43063,.F.);
#62261=ORIENTED_EDGE('',*,*,#42720,.T.);
#62262=ORIENTED_EDGE('',*,*,#42719,.T.);
#62263=ORIENTED_EDGE('',*,*,#43064,.F.);
#62264=ORIENTED_EDGE('',*,*,#42723,.T.);
#62265=ORIENTED_EDGE('',*,*,#42721,.T.);
#62266=ORIENTED_EDGE('',*,*,#43063,.T.);
#62267=ORIENTED_EDGE('',*,*,#43065,.F.);
#62268=ORIENTED_EDGE('',*,*,#43066,.F.);
#62269=ORIENTED_EDGE('',*,*,#42727,.T.);
#62270=ORIENTED_EDGE('',*,*,#42726,.T.);
#62271=ORIENTED_EDGE('',*,*,#43067,.F.);
#62272=ORIENTED_EDGE('',*,*,#42730,.T.);
#62273=ORIENTED_EDGE('',*,*,#42728,.T.);
#62274=ORIENTED_EDGE('',*,*,#43066,.T.);
#62275=ORIENTED_EDGE('',*,*,#43068,.F.);
#62276=ORIENTED_EDGE('',*,*,#43069,.F.);
#62277=ORIENTED_EDGE('',*,*,#42734,.T.);
#62278=ORIENTED_EDGE('',*,*,#42733,.T.);
#62279=ORIENTED_EDGE('',*,*,#43070,.F.);
#62280=ORIENTED_EDGE('',*,*,#42737,.T.);
#62281=ORIENTED_EDGE('',*,*,#42735,.T.);
#62282=ORIENTED_EDGE('',*,*,#43069,.T.);
#62283=ORIENTED_EDGE('',*,*,#43071,.F.);
#62284=ORIENTED_EDGE('',*,*,#43072,.F.);
#62285=ORIENTED_EDGE('',*,*,#42741,.T.);
#62286=ORIENTED_EDGE('',*,*,#42740,.T.);
#62287=ORIENTED_EDGE('',*,*,#43073,.F.);
#62288=ORIENTED_EDGE('',*,*,#42744,.T.);
#62289=ORIENTED_EDGE('',*,*,#42742,.T.);
#62290=ORIENTED_EDGE('',*,*,#43072,.T.);
#62291=ORIENTED_EDGE('',*,*,#43074,.F.);
#62292=ORIENTED_EDGE('',*,*,#43075,.F.);
#62293=ORIENTED_EDGE('',*,*,#42750,.T.);
#62294=ORIENTED_EDGE('',*,*,#42747,.T.);
#62295=ORIENTED_EDGE('',*,*,#42751,.T.);
#62296=ORIENTED_EDGE('',*,*,#43075,.T.);
#62297=ORIENTED_EDGE('',*,*,#43076,.F.);
#62298=ORIENTED_EDGE('',*,*,#42749,.T.);
#62299=ORIENTED_EDGE('',*,*,#42756,.T.);
#62300=ORIENTED_EDGE('',*,*,#42752,.T.);
#62301=ORIENTED_EDGE('',*,*,#43077,.F.);
#62302=ORIENTED_EDGE('',*,*,#43078,.F.);
#62303=ORIENTED_EDGE('',*,*,#43079,.F.);
#62304=ORIENTED_EDGE('',*,*,#42758,.T.);
#62305=ORIENTED_EDGE('',*,*,#42757,.T.);
#62306=ORIENTED_EDGE('',*,*,#43078,.T.);
#62307=ORIENTED_EDGE('',*,*,#43080,.F.);
#62308=ORIENTED_EDGE('',*,*,#43081,.F.);
#62309=ORIENTED_EDGE('',*,*,#42762,.T.);
#62310=ORIENTED_EDGE('',*,*,#42761,.T.);
#62311=ORIENTED_EDGE('',*,*,#43082,.F.);
#62312=ORIENTED_EDGE('',*,*,#42765,.T.);
#62313=ORIENTED_EDGE('',*,*,#42763,.T.);
#62314=ORIENTED_EDGE('',*,*,#43081,.T.);
#62315=ORIENTED_EDGE('',*,*,#43083,.F.);
#62316=ORIENTED_EDGE('',*,*,#43084,.F.);
#62317=ORIENTED_EDGE('',*,*,#42769,.T.);
#62318=ORIENTED_EDGE('',*,*,#42768,.T.);
#62319=ORIENTED_EDGE('',*,*,#43085,.F.);
#62320=ORIENTED_EDGE('',*,*,#42772,.T.);
#62321=ORIENTED_EDGE('',*,*,#42770,.T.);
#62322=ORIENTED_EDGE('',*,*,#43084,.T.);
#62323=ORIENTED_EDGE('',*,*,#43086,.F.);
#62324=ORIENTED_EDGE('',*,*,#43087,.F.);
#62325=ORIENTED_EDGE('',*,*,#42776,.T.);
#62326=ORIENTED_EDGE('',*,*,#42775,.T.);
#62327=ORIENTED_EDGE('',*,*,#43088,.F.);
#62328=ORIENTED_EDGE('',*,*,#42779,.T.);
#62329=ORIENTED_EDGE('',*,*,#42777,.T.);
#62330=ORIENTED_EDGE('',*,*,#43087,.T.);
#62331=ORIENTED_EDGE('',*,*,#43089,.F.);
#62332=ORIENTED_EDGE('',*,*,#43090,.F.);
#62333=ORIENTED_EDGE('',*,*,#42783,.T.);
#62334=ORIENTED_EDGE('',*,*,#42782,.T.);
#62335=ORIENTED_EDGE('',*,*,#43091,.F.);
#62336=ORIENTED_EDGE('',*,*,#42786,.T.);
#62337=ORIENTED_EDGE('',*,*,#42784,.T.);
#62338=ORIENTED_EDGE('',*,*,#43090,.T.);
#62339=ORIENTED_EDGE('',*,*,#43092,.F.);
#62340=ORIENTED_EDGE('',*,*,#43093,.F.);
#62341=ORIENTED_EDGE('',*,*,#42790,.T.);
#62342=ORIENTED_EDGE('',*,*,#42789,.T.);
#62343=ORIENTED_EDGE('',*,*,#43094,.F.);
#62344=ORIENTED_EDGE('',*,*,#42793,.T.);
#62345=ORIENTED_EDGE('',*,*,#42791,.T.);
#62346=ORIENTED_EDGE('',*,*,#43093,.T.);
#62347=ORIENTED_EDGE('',*,*,#43095,.F.);
#62348=ORIENTED_EDGE('',*,*,#43096,.F.);
#62349=ORIENTED_EDGE('',*,*,#42797,.T.);
#62350=ORIENTED_EDGE('',*,*,#42796,.T.);
#62351=ORIENTED_EDGE('',*,*,#43097,.F.);
#62352=ORIENTED_EDGE('',*,*,#42800,.T.);
#62353=ORIENTED_EDGE('',*,*,#42798,.T.);
#62354=ORIENTED_EDGE('',*,*,#43096,.T.);
#62355=ORIENTED_EDGE('',*,*,#43098,.F.);
#62356=ORIENTED_EDGE('',*,*,#43099,.F.);
#62357=ORIENTED_EDGE('',*,*,#42804,.T.);
#62358=ORIENTED_EDGE('',*,*,#42803,.T.);
#62359=ORIENTED_EDGE('',*,*,#43100,.F.);
#62360=ORIENTED_EDGE('',*,*,#42807,.T.);
#62361=ORIENTED_EDGE('',*,*,#42805,.T.);
#62362=ORIENTED_EDGE('',*,*,#43099,.T.);
#62363=ORIENTED_EDGE('',*,*,#43101,.F.);
#62364=ORIENTED_EDGE('',*,*,#43102,.F.);
#62365=ORIENTED_EDGE('',*,*,#42811,.T.);
#62366=ORIENTED_EDGE('',*,*,#42810,.T.);
#62367=ORIENTED_EDGE('',*,*,#43103,.F.);
#62368=ORIENTED_EDGE('',*,*,#42814,.T.);
#62369=ORIENTED_EDGE('',*,*,#42812,.T.);
#62370=ORIENTED_EDGE('',*,*,#43102,.T.);
#62371=ORIENTED_EDGE('',*,*,#43104,.F.);
#62372=ORIENTED_EDGE('',*,*,#43105,.F.);
#62373=ORIENTED_EDGE('',*,*,#42818,.T.);
#62374=ORIENTED_EDGE('',*,*,#42817,.T.);
#62375=ORIENTED_EDGE('',*,*,#43106,.F.);
#62376=ORIENTED_EDGE('',*,*,#42821,.T.);
#62377=ORIENTED_EDGE('',*,*,#42819,.T.);
#62378=ORIENTED_EDGE('',*,*,#43105,.T.);
#62379=ORIENTED_EDGE('',*,*,#43107,.F.);
#62380=ORIENTED_EDGE('',*,*,#43022,.T.);
#62381=ORIENTED_EDGE('',*,*,#42822,.T.);
#62382=ORIENTED_EDGE('',*,*,#42825,.T.);
#62383=ORIENTED_EDGE('',*,*,#43108,.F.);
#62384=ORIENTED_EDGE('',*,*,#42828,.T.);
#62385=ORIENTED_EDGE('',*,*,#43019,.T.);
#62386=ORIENTED_EDGE('',*,*,#43109,.F.);
#62387=ORIENTED_EDGE('',*,*,#43110,.F.);
#62388=ORIENTED_EDGE('',*,*,#43111,.F.);
#62389=ORIENTED_EDGE('',*,*,#42832,.T.);
#62390=ORIENTED_EDGE('',*,*,#42829,.T.);
#62391=ORIENTED_EDGE('',*,*,#43112,.F.);
#62392=ORIENTED_EDGE('',*,*,#42835,.T.);
#62393=ORIENTED_EDGE('',*,*,#42833,.T.);
#62394=ORIENTED_EDGE('',*,*,#43111,.T.);
#62395=ORIENTED_EDGE('',*,*,#43113,.F.);
#62396=ORIENTED_EDGE('',*,*,#43114,.F.);
#62397=ORIENTED_EDGE('',*,*,#42839,.T.);
#62398=ORIENTED_EDGE('',*,*,#42836,.T.);
#62399=ORIENTED_EDGE('',*,*,#43115,.F.);
#62400=ORIENTED_EDGE('',*,*,#42842,.T.);
#62401=ORIENTED_EDGE('',*,*,#42840,.T.);
#62402=ORIENTED_EDGE('',*,*,#43114,.T.);
#62403=ORIENTED_EDGE('',*,*,#43116,.F.);
#62404=ORIENTED_EDGE('',*,*,#43117,.F.);
#62405=ORIENTED_EDGE('',*,*,#42846,.T.);
#62406=ORIENTED_EDGE('',*,*,#42843,.T.);
#62407=ORIENTED_EDGE('',*,*,#43118,.F.);
#62408=ORIENTED_EDGE('',*,*,#42849,.T.);
#62409=ORIENTED_EDGE('',*,*,#42847,.T.);
#62410=ORIENTED_EDGE('',*,*,#43117,.T.);
#62411=ORIENTED_EDGE('',*,*,#43119,.F.);
#62412=ORIENTED_EDGE('',*,*,#43120,.F.);
#62413=ORIENTED_EDGE('',*,*,#42853,.T.);
#62414=ORIENTED_EDGE('',*,*,#42850,.T.);
#62415=ORIENTED_EDGE('',*,*,#43121,.F.);
#62416=ORIENTED_EDGE('',*,*,#42856,.T.);
#62417=ORIENTED_EDGE('',*,*,#42854,.T.);
#62418=ORIENTED_EDGE('',*,*,#43120,.T.);
#62419=ORIENTED_EDGE('',*,*,#43122,.F.);
#62420=ORIENTED_EDGE('',*,*,#43123,.F.);
#62421=ORIENTED_EDGE('',*,*,#42860,.T.);
#62422=ORIENTED_EDGE('',*,*,#42857,.T.);
#62423=ORIENTED_EDGE('',*,*,#43124,.F.);
#62424=ORIENTED_EDGE('',*,*,#42863,.T.);
#62425=ORIENTED_EDGE('',*,*,#42861,.T.);
#62426=ORIENTED_EDGE('',*,*,#43123,.T.);
#62427=ORIENTED_EDGE('',*,*,#43125,.F.);
#62428=ORIENTED_EDGE('',*,*,#43126,.F.);
#62429=ORIENTED_EDGE('',*,*,#42867,.T.);
#62430=ORIENTED_EDGE('',*,*,#42864,.T.);
#62431=ORIENTED_EDGE('',*,*,#43127,.F.);
#62432=ORIENTED_EDGE('',*,*,#42870,.T.);
#62433=ORIENTED_EDGE('',*,*,#42868,.T.);
#62434=ORIENTED_EDGE('',*,*,#43126,.T.);
#62435=ORIENTED_EDGE('',*,*,#43128,.F.);
#62436=ORIENTED_EDGE('',*,*,#43129,.F.);
#62437=ORIENTED_EDGE('',*,*,#42874,.T.);
#62438=ORIENTED_EDGE('',*,*,#42871,.T.);
#62439=ORIENTED_EDGE('',*,*,#43130,.F.);
#62440=ORIENTED_EDGE('',*,*,#42877,.T.);
#62441=ORIENTED_EDGE('',*,*,#42875,.T.);
#62442=ORIENTED_EDGE('',*,*,#43129,.T.);
#62443=ORIENTED_EDGE('',*,*,#43131,.F.);
#62444=ORIENTED_EDGE('',*,*,#43132,.F.);
#62445=ORIENTED_EDGE('',*,*,#42881,.T.);
#62446=ORIENTED_EDGE('',*,*,#42878,.T.);
#62447=ORIENTED_EDGE('',*,*,#43133,.F.);
#62448=ORIENTED_EDGE('',*,*,#42884,.T.);
#62449=ORIENTED_EDGE('',*,*,#42882,.T.);
#62450=ORIENTED_EDGE('',*,*,#43132,.T.);
#62451=ORIENTED_EDGE('',*,*,#43134,.F.);
#62452=ORIENTED_EDGE('',*,*,#43135,.F.);
#62453=ORIENTED_EDGE('',*,*,#42888,.T.);
#62454=ORIENTED_EDGE('',*,*,#42885,.T.);
#62455=ORIENTED_EDGE('',*,*,#43136,.F.);
#62456=ORIENTED_EDGE('',*,*,#42891,.T.);
#62457=ORIENTED_EDGE('',*,*,#42889,.T.);
#62458=ORIENTED_EDGE('',*,*,#43135,.T.);
#62459=ORIENTED_EDGE('',*,*,#43137,.F.);
#62460=ORIENTED_EDGE('',*,*,#43138,.F.);
#62461=ORIENTED_EDGE('',*,*,#42895,.T.);
#62462=ORIENTED_EDGE('',*,*,#42892,.T.);
#62463=ORIENTED_EDGE('',*,*,#43139,.F.);
#62464=ORIENTED_EDGE('',*,*,#42898,.T.);
#62465=ORIENTED_EDGE('',*,*,#42896,.T.);
#62466=ORIENTED_EDGE('',*,*,#43138,.T.);
#62467=ORIENTED_EDGE('',*,*,#43140,.F.);
#62468=ORIENTED_EDGE('',*,*,#43141,.F.);
#62469=ORIENTED_EDGE('',*,*,#42902,.T.);
#62470=ORIENTED_EDGE('',*,*,#42899,.T.);
#62471=ORIENTED_EDGE('',*,*,#43142,.F.);
#62472=ORIENTED_EDGE('',*,*,#42905,.T.);
#62473=ORIENTED_EDGE('',*,*,#42903,.T.);
#62474=ORIENTED_EDGE('',*,*,#43141,.T.);
#62475=ORIENTED_EDGE('',*,*,#43143,.F.);
#62476=ORIENTED_EDGE('',*,*,#43144,.F.);
#62477=ORIENTED_EDGE('',*,*,#42909,.T.);
#62478=ORIENTED_EDGE('',*,*,#42906,.T.);
#62479=ORIENTED_EDGE('',*,*,#43145,.F.);
#62480=ORIENTED_EDGE('',*,*,#42912,.T.);
#62481=ORIENTED_EDGE('',*,*,#42910,.T.);
#62482=ORIENTED_EDGE('',*,*,#43144,.T.);
#62483=ORIENTED_EDGE('',*,*,#43146,.F.);
#62484=ORIENTED_EDGE('',*,*,#43147,.F.);
#62485=ORIENTED_EDGE('',*,*,#42916,.T.);
#62486=ORIENTED_EDGE('',*,*,#42913,.T.);
#62487=ORIENTED_EDGE('',*,*,#43148,.F.);
#62488=ORIENTED_EDGE('',*,*,#42919,.T.);
#62489=ORIENTED_EDGE('',*,*,#42917,.T.);
#62490=ORIENTED_EDGE('',*,*,#43147,.T.);
#62491=ORIENTED_EDGE('',*,*,#43149,.F.);
#62492=ORIENTED_EDGE('',*,*,#43150,.F.);
#62493=ORIENTED_EDGE('',*,*,#34357,.T.);
#62494=ORIENTED_EDGE('',*,*,#42920,.T.);
#62495=ORIENTED_EDGE('',*,*,#42922,.T.);
#62496=ORIENTED_EDGE('',*,*,#34354,.T.);
#62497=ORIENTED_EDGE('',*,*,#43150,.T.);
#62498=ORIENTED_EDGE('',*,*,#43151,.F.);
#62499=ORIENTED_EDGE('',*,*,#43152,.F.);
#62500=ORIENTED_EDGE('',*,*,#43153,.F.);
#62501=ORIENTED_EDGE('',*,*,#42926,.T.);
#62502=ORIENTED_EDGE('',*,*,#42923,.T.);
#62503=ORIENTED_EDGE('',*,*,#43154,.F.);
#62504=ORIENTED_EDGE('',*,*,#42929,.T.);
#62505=ORIENTED_EDGE('',*,*,#42927,.T.);
#62506=ORIENTED_EDGE('',*,*,#43153,.T.);
#62507=ORIENTED_EDGE('',*,*,#43155,.F.);
#62508=ORIENTED_EDGE('',*,*,#43156,.F.);
#62509=ORIENTED_EDGE('',*,*,#42933,.T.);
#62510=ORIENTED_EDGE('',*,*,#42930,.T.);
#62511=ORIENTED_EDGE('',*,*,#43157,.F.);
#62512=ORIENTED_EDGE('',*,*,#42936,.T.);
#62513=ORIENTED_EDGE('',*,*,#42934,.T.);
#62514=ORIENTED_EDGE('',*,*,#43156,.T.);
#62515=ORIENTED_EDGE('',*,*,#43158,.F.);
#62516=ORIENTED_EDGE('',*,*,#43159,.F.);
#62517=ORIENTED_EDGE('',*,*,#42940,.T.);
#62518=ORIENTED_EDGE('',*,*,#42937,.T.);
#62519=ORIENTED_EDGE('',*,*,#43160,.F.);
#62520=ORIENTED_EDGE('',*,*,#42943,.T.);
#62521=ORIENTED_EDGE('',*,*,#42941,.T.);
#62522=ORIENTED_EDGE('',*,*,#43159,.T.);
#62523=ORIENTED_EDGE('',*,*,#43161,.F.);
#62524=ORIENTED_EDGE('',*,*,#43162,.F.);
#62525=ORIENTED_EDGE('',*,*,#42947,.T.);
#62526=ORIENTED_EDGE('',*,*,#42944,.T.);
#62527=ORIENTED_EDGE('',*,*,#43163,.F.);
#62528=ORIENTED_EDGE('',*,*,#42950,.T.);
#62529=ORIENTED_EDGE('',*,*,#42948,.T.);
#62530=ORIENTED_EDGE('',*,*,#43162,.T.);
#62531=ORIENTED_EDGE('',*,*,#43164,.F.);
#62532=ORIENTED_EDGE('',*,*,#43165,.F.);
#62533=ORIENTED_EDGE('',*,*,#42954,.T.);
#62534=ORIENTED_EDGE('',*,*,#42951,.T.);
#62535=ORIENTED_EDGE('',*,*,#43166,.F.);
#62536=ORIENTED_EDGE('',*,*,#42957,.T.);
#62537=ORIENTED_EDGE('',*,*,#42955,.T.);
#62538=ORIENTED_EDGE('',*,*,#43165,.T.);
#62539=ORIENTED_EDGE('',*,*,#43167,.F.);
#62540=ORIENTED_EDGE('',*,*,#43168,.F.);
#62541=ORIENTED_EDGE('',*,*,#42961,.T.);
#62542=ORIENTED_EDGE('',*,*,#42958,.T.);
#62543=ORIENTED_EDGE('',*,*,#43169,.F.);
#62544=ORIENTED_EDGE('',*,*,#42964,.T.);
#62545=ORIENTED_EDGE('',*,*,#42962,.T.);
#62546=ORIENTED_EDGE('',*,*,#43168,.T.);
#62547=ORIENTED_EDGE('',*,*,#43170,.F.);
#62548=ORIENTED_EDGE('',*,*,#43171,.F.);
#62549=ORIENTED_EDGE('',*,*,#34353,.T.);
#62550=ORIENTED_EDGE('',*,*,#42965,.T.);
#62551=ORIENTED_EDGE('',*,*,#43172,.F.);
#62552=ORIENTED_EDGE('',*,*,#42967,.T.);
#62553=ORIENTED_EDGE('',*,*,#34350,.T.);
#62554=ORIENTED_EDGE('',*,*,#43171,.T.);
#62555=ORIENTED_EDGE('',*,*,#43173,.F.);
#62556=ORIENTED_EDGE('',*,*,#43174,.F.);
#62557=ORIENTED_EDGE('',*,*,#42971,.T.);
#62558=ORIENTED_EDGE('',*,*,#42968,.T.);
#62559=ORIENTED_EDGE('',*,*,#43175,.F.);
#62560=ORIENTED_EDGE('',*,*,#42974,.T.);
#62561=ORIENTED_EDGE('',*,*,#42972,.T.);
#62562=ORIENTED_EDGE('',*,*,#43174,.T.);
#62563=ORIENTED_EDGE('',*,*,#43176,.F.);
#62564=ORIENTED_EDGE('',*,*,#43177,.F.);
#62565=ORIENTED_EDGE('',*,*,#42978,.T.);
#62566=ORIENTED_EDGE('',*,*,#42975,.T.);
#62567=ORIENTED_EDGE('',*,*,#43178,.F.);
#62568=ORIENTED_EDGE('',*,*,#42981,.T.);
#62569=ORIENTED_EDGE('',*,*,#42979,.T.);
#62570=ORIENTED_EDGE('',*,*,#43177,.T.);
#62571=ORIENTED_EDGE('',*,*,#43179,.F.);
#62572=ORIENTED_EDGE('',*,*,#43180,.F.);
#62573=ORIENTED_EDGE('',*,*,#42985,.T.);
#62574=ORIENTED_EDGE('',*,*,#42982,.T.);
#62575=ORIENTED_EDGE('',*,*,#43181,.F.);
#62576=ORIENTED_EDGE('',*,*,#42988,.T.);
#62577=ORIENTED_EDGE('',*,*,#42986,.T.);
#62578=ORIENTED_EDGE('',*,*,#43180,.T.);
#62579=ORIENTED_EDGE('',*,*,#43182,.F.);
#62580=ORIENTED_EDGE('',*,*,#43183,.F.);
#62581=ORIENTED_EDGE('',*,*,#42992,.T.);
#62582=ORIENTED_EDGE('',*,*,#42989,.T.);
#62583=ORIENTED_EDGE('',*,*,#43184,.F.);
#62584=ORIENTED_EDGE('',*,*,#42995,.T.);
#62585=ORIENTED_EDGE('',*,*,#42993,.T.);
#62586=ORIENTED_EDGE('',*,*,#43183,.T.);
#62587=ORIENTED_EDGE('',*,*,#43185,.F.);
#62588=ORIENTED_EDGE('',*,*,#43186,.F.);
#62589=ORIENTED_EDGE('',*,*,#42999,.T.);
#62590=ORIENTED_EDGE('',*,*,#42996,.T.);
#62591=ORIENTED_EDGE('',*,*,#43187,.F.);
#62592=ORIENTED_EDGE('',*,*,#43002,.T.);
#62593=ORIENTED_EDGE('',*,*,#43000,.T.);
#62594=ORIENTED_EDGE('',*,*,#43186,.T.);
#62595=ORIENTED_EDGE('',*,*,#43188,.F.);
#62596=ORIENTED_EDGE('',*,*,#43189,.F.);
#62597=ORIENTED_EDGE('',*,*,#43006,.T.);
#62598=ORIENTED_EDGE('',*,*,#43003,.T.);
#62599=ORIENTED_EDGE('',*,*,#43190,.F.);
#62600=ORIENTED_EDGE('',*,*,#43009,.T.);
#62601=ORIENTED_EDGE('',*,*,#43007,.T.);
#62602=ORIENTED_EDGE('',*,*,#43189,.T.);
#62603=ORIENTED_EDGE('',*,*,#43191,.F.);
#62604=ORIENTED_EDGE('',*,*,#43192,.F.);
#62605=ORIENTED_EDGE('',*,*,#43013,.T.);
#62606=ORIENTED_EDGE('',*,*,#43010,.T.);
#62607=ORIENTED_EDGE('',*,*,#43193,.F.);
#62608=ORIENTED_EDGE('',*,*,#43016,.T.);
#62609=ORIENTED_EDGE('',*,*,#43014,.T.);
#62610=ORIENTED_EDGE('',*,*,#43192,.T.);
#62611=ORIENTED_EDGE('',*,*,#43194,.F.);
#62612=ORIENTED_EDGE('',*,*,#43109,.T.);
#62613=ORIENTED_EDGE('',*,*,#43018,.T.);
#62614=ORIENTED_EDGE('',*,*,#43020,.T.);
#62615=ORIENTED_EDGE('',*,*,#43195,.T.);
#62616=ORIENTED_EDGE('',*,*,#43196,.F.);
#62617=ORIENTED_EDGE('',*,*,#43021,.T.);
#62618=ORIENTED_EDGE('',*,*,#43197,.F.);
#62619=ORIENTED_EDGE('',*,*,#43198,.F.);
#62620=ORIENTED_EDGE('',*,*,#43199,.F.);
#62621=ORIENTED_EDGE('',*,*,#43200,.F.);
#62622=ORIENTED_EDGE('',*,*,#43195,.F.);
#62623=ORIENTED_EDGE('',*,*,#43200,.T.);
#62624=ORIENTED_EDGE('',*,*,#43201,.F.);
#62625=ORIENTED_EDGE('',*,*,#43023,.T.);
#62626=ORIENTED_EDGE('',*,*,#43196,.T.);
#62627=ORIENTED_EDGE('',*,*,#43202,.T.);
#62628=ORIENTED_EDGE('',*,*,#43203,.F.);
#62629=ORIENTED_EDGE('',*,*,#43025,.T.);
#62630=ORIENTED_EDGE('',*,*,#43204,.F.);
#62631=ORIENTED_EDGE('',*,*,#43205,.F.);
#62632=ORIENTED_EDGE('',*,*,#43206,.F.);
#62633=ORIENTED_EDGE('',*,*,#43207,.F.);
#62634=ORIENTED_EDGE('',*,*,#43202,.F.);
#62635=ORIENTED_EDGE('',*,*,#43207,.T.);
#62636=ORIENTED_EDGE('',*,*,#43208,.F.);
#62637=ORIENTED_EDGE('',*,*,#43026,.T.);
#62638=ORIENTED_EDGE('',*,*,#43203,.T.);
#62639=ORIENTED_EDGE('',*,*,#43209,.T.);
#62640=ORIENTED_EDGE('',*,*,#43210,.F.);
#62641=ORIENTED_EDGE('',*,*,#43028,.T.);
#62642=ORIENTED_EDGE('',*,*,#43211,.F.);
#62643=ORIENTED_EDGE('',*,*,#43212,.F.);
#62644=ORIENTED_EDGE('',*,*,#43213,.F.);
#62645=ORIENTED_EDGE('',*,*,#43214,.F.);
#62646=ORIENTED_EDGE('',*,*,#43209,.F.);
#62647=ORIENTED_EDGE('',*,*,#43214,.T.);
#62648=ORIENTED_EDGE('',*,*,#43215,.F.);
#62649=ORIENTED_EDGE('',*,*,#43029,.T.);
#62650=ORIENTED_EDGE('',*,*,#43210,.T.);
#62651=ORIENTED_EDGE('',*,*,#43216,.T.);
#62652=ORIENTED_EDGE('',*,*,#43217,.F.);
#62653=ORIENTED_EDGE('',*,*,#43031,.T.);
#62654=ORIENTED_EDGE('',*,*,#43218,.F.);
#62655=ORIENTED_EDGE('',*,*,#43219,.F.);
#62656=ORIENTED_EDGE('',*,*,#43220,.F.);
#62657=ORIENTED_EDGE('',*,*,#43221,.F.);
#62658=ORIENTED_EDGE('',*,*,#43216,.F.);
#62659=ORIENTED_EDGE('',*,*,#43221,.T.);
#62660=ORIENTED_EDGE('',*,*,#43222,.F.);
#62661=ORIENTED_EDGE('',*,*,#43032,.T.);
#62662=ORIENTED_EDGE('',*,*,#43217,.T.);
#62663=ORIENTED_EDGE('',*,*,#43223,.T.);
#62664=ORIENTED_EDGE('',*,*,#43224,.F.);
#62665=ORIENTED_EDGE('',*,*,#43034,.T.);
#62666=ORIENTED_EDGE('',*,*,#43225,.F.);
#62667=ORIENTED_EDGE('',*,*,#43226,.F.);
#62668=ORIENTED_EDGE('',*,*,#43227,.F.);
#62669=ORIENTED_EDGE('',*,*,#43228,.F.);
#62670=ORIENTED_EDGE('',*,*,#43223,.F.);
#62671=ORIENTED_EDGE('',*,*,#43228,.T.);
#62672=ORIENTED_EDGE('',*,*,#43229,.F.);
#62673=ORIENTED_EDGE('',*,*,#43035,.T.);
#62674=ORIENTED_EDGE('',*,*,#43224,.T.);
#62675=ORIENTED_EDGE('',*,*,#43230,.T.);
#62676=ORIENTED_EDGE('',*,*,#43231,.F.);
#62677=ORIENTED_EDGE('',*,*,#43037,.T.);
#62678=ORIENTED_EDGE('',*,*,#43232,.F.);
#62679=ORIENTED_EDGE('',*,*,#43233,.F.);
#62680=ORIENTED_EDGE('',*,*,#43234,.F.);
#62681=ORIENTED_EDGE('',*,*,#43235,.F.);
#62682=ORIENTED_EDGE('',*,*,#43230,.F.);
#62683=ORIENTED_EDGE('',*,*,#43235,.T.);
#62684=ORIENTED_EDGE('',*,*,#43236,.F.);
#62685=ORIENTED_EDGE('',*,*,#43038,.T.);
#62686=ORIENTED_EDGE('',*,*,#43231,.T.);
#62687=ORIENTED_EDGE('',*,*,#43237,.T.);
#62688=ORIENTED_EDGE('',*,*,#43238,.F.);
#62689=ORIENTED_EDGE('',*,*,#43040,.T.);
#62690=ORIENTED_EDGE('',*,*,#43239,.F.);
#62691=ORIENTED_EDGE('',*,*,#43240,.F.);
#62692=ORIENTED_EDGE('',*,*,#43241,.F.);
#62693=ORIENTED_EDGE('',*,*,#43242,.F.);
#62694=ORIENTED_EDGE('',*,*,#43237,.F.);
#62695=ORIENTED_EDGE('',*,*,#43242,.T.);
#62696=ORIENTED_EDGE('',*,*,#43243,.F.);
#62697=ORIENTED_EDGE('',*,*,#43041,.T.);
#62698=ORIENTED_EDGE('',*,*,#43238,.T.);
#62699=ORIENTED_EDGE('',*,*,#43244,.T.);
#62700=ORIENTED_EDGE('',*,*,#43245,.F.);
#62701=ORIENTED_EDGE('',*,*,#43043,.T.);
#62702=ORIENTED_EDGE('',*,*,#43246,.F.);
#62703=ORIENTED_EDGE('',*,*,#43247,.F.);
#62704=ORIENTED_EDGE('',*,*,#43248,.F.);
#62705=ORIENTED_EDGE('',*,*,#43249,.F.);
#62706=ORIENTED_EDGE('',*,*,#43244,.F.);
#62707=ORIENTED_EDGE('',*,*,#43249,.T.);
#62708=ORIENTED_EDGE('',*,*,#43250,.F.);
#62709=ORIENTED_EDGE('',*,*,#43044,.T.);
#62710=ORIENTED_EDGE('',*,*,#43245,.T.);
#62711=ORIENTED_EDGE('',*,*,#43251,.T.);
#62712=ORIENTED_EDGE('',*,*,#43252,.F.);
#62713=ORIENTED_EDGE('',*,*,#43046,.T.);
#62714=ORIENTED_EDGE('',*,*,#43253,.F.);
#62715=ORIENTED_EDGE('',*,*,#43254,.F.);
#62716=ORIENTED_EDGE('',*,*,#43255,.F.);
#62717=ORIENTED_EDGE('',*,*,#43256,.F.);
#62718=ORIENTED_EDGE('',*,*,#43251,.F.);
#62719=ORIENTED_EDGE('',*,*,#43256,.T.);
#62720=ORIENTED_EDGE('',*,*,#43257,.F.);
#62721=ORIENTED_EDGE('',*,*,#43047,.T.);
#62722=ORIENTED_EDGE('',*,*,#43252,.T.);
#62723=ORIENTED_EDGE('',*,*,#43258,.T.);
#62724=ORIENTED_EDGE('',*,*,#43259,.F.);
#62725=ORIENTED_EDGE('',*,*,#43049,.T.);
#62726=ORIENTED_EDGE('',*,*,#43260,.F.);
#62727=ORIENTED_EDGE('',*,*,#43261,.F.);
#62728=ORIENTED_EDGE('',*,*,#43262,.F.);
#62729=ORIENTED_EDGE('',*,*,#43263,.F.);
#62730=ORIENTED_EDGE('',*,*,#43258,.F.);
#62731=ORIENTED_EDGE('',*,*,#43263,.T.);
#62732=ORIENTED_EDGE('',*,*,#43264,.F.);
#62733=ORIENTED_EDGE('',*,*,#43050,.T.);
#62734=ORIENTED_EDGE('',*,*,#43259,.T.);
#62735=ORIENTED_EDGE('',*,*,#43265,.T.);
#62736=ORIENTED_EDGE('',*,*,#43266,.F.);
#62737=ORIENTED_EDGE('',*,*,#43052,.T.);
#62738=ORIENTED_EDGE('',*,*,#43267,.F.);
#62739=ORIENTED_EDGE('',*,*,#43268,.F.);
#62740=ORIENTED_EDGE('',*,*,#43269,.F.);
#62741=ORIENTED_EDGE('',*,*,#43270,.F.);
#62742=ORIENTED_EDGE('',*,*,#43265,.F.);
#62743=ORIENTED_EDGE('',*,*,#43270,.T.);
#62744=ORIENTED_EDGE('',*,*,#43271,.F.);
#62745=ORIENTED_EDGE('',*,*,#43053,.T.);
#62746=ORIENTED_EDGE('',*,*,#43266,.T.);
#62747=ORIENTED_EDGE('',*,*,#43272,.T.);
#62748=ORIENTED_EDGE('',*,*,#43273,.F.);
#62749=ORIENTED_EDGE('',*,*,#43055,.T.);
#62750=ORIENTED_EDGE('',*,*,#43274,.F.);
#62751=ORIENTED_EDGE('',*,*,#43275,.F.);
#62752=ORIENTED_EDGE('',*,*,#43276,.F.);
#62753=ORIENTED_EDGE('',*,*,#43277,.F.);
#62754=ORIENTED_EDGE('',*,*,#43272,.F.);
#62755=ORIENTED_EDGE('',*,*,#43277,.T.);
#62756=ORIENTED_EDGE('',*,*,#43278,.F.);
#62757=ORIENTED_EDGE('',*,*,#43056,.T.);
#62758=ORIENTED_EDGE('',*,*,#43273,.T.);
#62759=ORIENTED_EDGE('',*,*,#43279,.T.);
#62760=ORIENTED_EDGE('',*,*,#43280,.F.);
#62761=ORIENTED_EDGE('',*,*,#43058,.T.);
#62762=ORIENTED_EDGE('',*,*,#43281,.F.);
#62763=ORIENTED_EDGE('',*,*,#43282,.F.);
#62764=ORIENTED_EDGE('',*,*,#43283,.F.);
#62765=ORIENTED_EDGE('',*,*,#43284,.F.);
#62766=ORIENTED_EDGE('',*,*,#43279,.F.);
#62767=ORIENTED_EDGE('',*,*,#43284,.T.);
#62768=ORIENTED_EDGE('',*,*,#43285,.F.);
#62769=ORIENTED_EDGE('',*,*,#43059,.T.);
#62770=ORIENTED_EDGE('',*,*,#43280,.T.);
#62771=ORIENTED_EDGE('',*,*,#43286,.T.);
#62772=ORIENTED_EDGE('',*,*,#43287,.F.);
#62773=ORIENTED_EDGE('',*,*,#43061,.T.);
#62774=ORIENTED_EDGE('',*,*,#43288,.F.);
#62775=ORIENTED_EDGE('',*,*,#43289,.F.);
#62776=ORIENTED_EDGE('',*,*,#43290,.F.);
#62777=ORIENTED_EDGE('',*,*,#43291,.F.);
#62778=ORIENTED_EDGE('',*,*,#43286,.F.);
#62779=ORIENTED_EDGE('',*,*,#43291,.T.);
#62780=ORIENTED_EDGE('',*,*,#43292,.F.);
#62781=ORIENTED_EDGE('',*,*,#43062,.T.);
#62782=ORIENTED_EDGE('',*,*,#43287,.T.);
#62783=ORIENTED_EDGE('',*,*,#34346,.T.);
#62784=ORIENTED_EDGE('',*,*,#43293,.F.);
#62785=ORIENTED_EDGE('',*,*,#43064,.T.);
#62786=ORIENTED_EDGE('',*,*,#43294,.F.);
#62787=ORIENTED_EDGE('',*,*,#34349,.T.);
#62788=ORIENTED_EDGE('',*,*,#43295,.F.);
#62789=ORIENTED_EDGE('',*,*,#43065,.T.);
#62790=ORIENTED_EDGE('',*,*,#43293,.T.);
#62791=ORIENTED_EDGE('',*,*,#43296,.T.);
#62792=ORIENTED_EDGE('',*,*,#43297,.F.);
#62793=ORIENTED_EDGE('',*,*,#43067,.T.);
#62794=ORIENTED_EDGE('',*,*,#43298,.F.);
#62795=ORIENTED_EDGE('',*,*,#43299,.F.);
#62796=ORIENTED_EDGE('',*,*,#43300,.F.);
#62797=ORIENTED_EDGE('',*,*,#43301,.F.);
#62798=ORIENTED_EDGE('',*,*,#43296,.F.);
#62799=ORIENTED_EDGE('',*,*,#43301,.T.);
#62800=ORIENTED_EDGE('',*,*,#43302,.F.);
#62801=ORIENTED_EDGE('',*,*,#43068,.T.);
#62802=ORIENTED_EDGE('',*,*,#43297,.T.);
#62803=ORIENTED_EDGE('',*,*,#43303,.T.);
#62804=ORIENTED_EDGE('',*,*,#43304,.F.);
#62805=ORIENTED_EDGE('',*,*,#43070,.T.);
#62806=ORIENTED_EDGE('',*,*,#43305,.F.);
#62807=ORIENTED_EDGE('',*,*,#43306,.F.);
#62808=ORIENTED_EDGE('',*,*,#43307,.F.);
#62809=ORIENTED_EDGE('',*,*,#43308,.F.);
#62810=ORIENTED_EDGE('',*,*,#43303,.F.);
#62811=ORIENTED_EDGE('',*,*,#43308,.T.);
#62812=ORIENTED_EDGE('',*,*,#43309,.F.);
#62813=ORIENTED_EDGE('',*,*,#43071,.T.);
#62814=ORIENTED_EDGE('',*,*,#43304,.T.);
#62815=ORIENTED_EDGE('',*,*,#43310,.T.);
#62816=ORIENTED_EDGE('',*,*,#43311,.F.);
#62817=ORIENTED_EDGE('',*,*,#43073,.T.);
#62818=ORIENTED_EDGE('',*,*,#43312,.F.);
#62819=ORIENTED_EDGE('',*,*,#43313,.T.);
#62820=ORIENTED_EDGE('',*,*,#43314,.F.);
#62821=ORIENTED_EDGE('',*,*,#43074,.T.);
#62822=ORIENTED_EDGE('',*,*,#43311,.T.);
#62823=ORIENTED_EDGE('',*,*,#43315,.F.);
#62824=ORIENTED_EDGE('',*,*,#43316,.F.);
#62825=ORIENTED_EDGE('',*,*,#43313,.F.);
#62826=ORIENTED_EDGE('',*,*,#43310,.F.);
#62827=ORIENTED_EDGE('',*,*,#43076,.T.);
#62828=ORIENTED_EDGE('',*,*,#43317,.F.);
#62829=ORIENTED_EDGE('',*,*,#43318,.T.);
#62830=ORIENTED_EDGE('',*,*,#43319,.F.);
#62831=ORIENTED_EDGE('',*,*,#43320,.F.);
#62832=ORIENTED_EDGE('',*,*,#43318,.F.);
#62833=ORIENTED_EDGE('',*,*,#43321,.F.);
#62834=ORIENTED_EDGE('',*,*,#43322,.F.);
#62835=ORIENTED_EDGE('',*,*,#43077,.T.);
#62836=ORIENTED_EDGE('',*,*,#43319,.T.);
#62837=ORIENTED_EDGE('',*,*,#43320,.T.);
#62838=ORIENTED_EDGE('',*,*,#43323,.F.);
#62839=ORIENTED_EDGE('',*,*,#43324,.T.);
#62840=ORIENTED_EDGE('',*,*,#43325,.F.);
#62841=ORIENTED_EDGE('',*,*,#43079,.T.);
#62842=ORIENTED_EDGE('',*,*,#43326,.F.);
#62843=ORIENTED_EDGE('',*,*,#43327,.F.);
#62844=ORIENTED_EDGE('',*,*,#43328,.F.);
#62845=ORIENTED_EDGE('',*,*,#43329,.F.);
#62846=ORIENTED_EDGE('',*,*,#43324,.F.);
#62847=ORIENTED_EDGE('',*,*,#43329,.T.);
#62848=ORIENTED_EDGE('',*,*,#43330,.F.);
#62849=ORIENTED_EDGE('',*,*,#43080,.T.);
#62850=ORIENTED_EDGE('',*,*,#43325,.T.);
#62851=ORIENTED_EDGE('',*,*,#43331,.T.);
#62852=ORIENTED_EDGE('',*,*,#43332,.F.);
#62853=ORIENTED_EDGE('',*,*,#43082,.T.);
#62854=ORIENTED_EDGE('',*,*,#43333,.F.);
#62855=ORIENTED_EDGE('',*,*,#43334,.F.);
#62856=ORIENTED_EDGE('',*,*,#43335,.F.);
#62857=ORIENTED_EDGE('',*,*,#43336,.F.);
#62858=ORIENTED_EDGE('',*,*,#43331,.F.);
#62859=ORIENTED_EDGE('',*,*,#43336,.T.);
#62860=ORIENTED_EDGE('',*,*,#43337,.F.);
#62861=ORIENTED_EDGE('',*,*,#43083,.T.);
#62862=ORIENTED_EDGE('',*,*,#43332,.T.);
#62863=ORIENTED_EDGE('',*,*,#43338,.T.);
#62864=ORIENTED_EDGE('',*,*,#43339,.F.);
#62865=ORIENTED_EDGE('',*,*,#43085,.T.);
#62866=ORIENTED_EDGE('',*,*,#43340,.F.);
#62867=ORIENTED_EDGE('',*,*,#43341,.F.);
#62868=ORIENTED_EDGE('',*,*,#43342,.F.);
#62869=ORIENTED_EDGE('',*,*,#43343,.F.);
#62870=ORIENTED_EDGE('',*,*,#43338,.F.);
#62871=ORIENTED_EDGE('',*,*,#43343,.T.);
#62872=ORIENTED_EDGE('',*,*,#43344,.F.);
#62873=ORIENTED_EDGE('',*,*,#43086,.T.);
#62874=ORIENTED_EDGE('',*,*,#43339,.T.);
#62875=ORIENTED_EDGE('',*,*,#43345,.T.);
#62876=ORIENTED_EDGE('',*,*,#43346,.F.);
#62877=ORIENTED_EDGE('',*,*,#43088,.T.);
#62878=ORIENTED_EDGE('',*,*,#43347,.F.);
#62879=ORIENTED_EDGE('',*,*,#43348,.F.);
#62880=ORIENTED_EDGE('',*,*,#43349,.F.);
#62881=ORIENTED_EDGE('',*,*,#43350,.F.);
#62882=ORIENTED_EDGE('',*,*,#43345,.F.);
#62883=ORIENTED_EDGE('',*,*,#43350,.T.);
#62884=ORIENTED_EDGE('',*,*,#43351,.F.);
#62885=ORIENTED_EDGE('',*,*,#43089,.T.);
#62886=ORIENTED_EDGE('',*,*,#43346,.T.);
#62887=ORIENTED_EDGE('',*,*,#43352,.T.);
#62888=ORIENTED_EDGE('',*,*,#43353,.F.);
#62889=ORIENTED_EDGE('',*,*,#43091,.T.);
#62890=ORIENTED_EDGE('',*,*,#43354,.F.);
#62891=ORIENTED_EDGE('',*,*,#43355,.F.);
#62892=ORIENTED_EDGE('',*,*,#43356,.F.);
#62893=ORIENTED_EDGE('',*,*,#43357,.F.);
#62894=ORIENTED_EDGE('',*,*,#43352,.F.);
#62895=ORIENTED_EDGE('',*,*,#43357,.T.);
#62896=ORIENTED_EDGE('',*,*,#43358,.F.);
#62897=ORIENTED_EDGE('',*,*,#43092,.T.);
#62898=ORIENTED_EDGE('',*,*,#43353,.T.);
#62899=ORIENTED_EDGE('',*,*,#43359,.T.);
#62900=ORIENTED_EDGE('',*,*,#43360,.F.);
#62901=ORIENTED_EDGE('',*,*,#43094,.T.);
#62902=ORIENTED_EDGE('',*,*,#43361,.F.);
#62903=ORIENTED_EDGE('',*,*,#43362,.F.);
#62904=ORIENTED_EDGE('',*,*,#43363,.F.);
#62905=ORIENTED_EDGE('',*,*,#43364,.F.);
#62906=ORIENTED_EDGE('',*,*,#43359,.F.);
#62907=ORIENTED_EDGE('',*,*,#43364,.T.);
#62908=ORIENTED_EDGE('',*,*,#43365,.F.);
#62909=ORIENTED_EDGE('',*,*,#43095,.T.);
#62910=ORIENTED_EDGE('',*,*,#43360,.T.);
#62911=ORIENTED_EDGE('',*,*,#43366,.T.);
#62912=ORIENTED_EDGE('',*,*,#43367,.F.);
#62913=ORIENTED_EDGE('',*,*,#43097,.T.);
#62914=ORIENTED_EDGE('',*,*,#43368,.F.);
#62915=ORIENTED_EDGE('',*,*,#43369,.F.);
#62916=ORIENTED_EDGE('',*,*,#43370,.F.);
#62917=ORIENTED_EDGE('',*,*,#43371,.F.);
#62918=ORIENTED_EDGE('',*,*,#43366,.F.);
#62919=ORIENTED_EDGE('',*,*,#43371,.T.);
#62920=ORIENTED_EDGE('',*,*,#43372,.F.);
#62921=ORIENTED_EDGE('',*,*,#43098,.T.);
#62922=ORIENTED_EDGE('',*,*,#43367,.T.);
#62923=ORIENTED_EDGE('',*,*,#43373,.T.);
#62924=ORIENTED_EDGE('',*,*,#43374,.F.);
#62925=ORIENTED_EDGE('',*,*,#43100,.T.);
#62926=ORIENTED_EDGE('',*,*,#43375,.F.);
#62927=ORIENTED_EDGE('',*,*,#43376,.F.);
#62928=ORIENTED_EDGE('',*,*,#43377,.F.);
#62929=ORIENTED_EDGE('',*,*,#43378,.F.);
#62930=ORIENTED_EDGE('',*,*,#43373,.F.);
#62931=ORIENTED_EDGE('',*,*,#43378,.T.);
#62932=ORIENTED_EDGE('',*,*,#43379,.F.);
#62933=ORIENTED_EDGE('',*,*,#43101,.T.);
#62934=ORIENTED_EDGE('',*,*,#43374,.T.);
#62935=ORIENTED_EDGE('',*,*,#43380,.T.);
#62936=ORIENTED_EDGE('',*,*,#43381,.F.);
#62937=ORIENTED_EDGE('',*,*,#43103,.T.);
#62938=ORIENTED_EDGE('',*,*,#43382,.F.);
#62939=ORIENTED_EDGE('',*,*,#43383,.F.);
#62940=ORIENTED_EDGE('',*,*,#43384,.F.);
#62941=ORIENTED_EDGE('',*,*,#43385,.F.);
#62942=ORIENTED_EDGE('',*,*,#43380,.F.);
#62943=ORIENTED_EDGE('',*,*,#43385,.T.);
#62944=ORIENTED_EDGE('',*,*,#43386,.F.);
#62945=ORIENTED_EDGE('',*,*,#43104,.T.);
#62946=ORIENTED_EDGE('',*,*,#43381,.T.);
#62947=ORIENTED_EDGE('',*,*,#43387,.T.);
#62948=ORIENTED_EDGE('',*,*,#43388,.F.);
#62949=ORIENTED_EDGE('',*,*,#43106,.T.);
#62950=ORIENTED_EDGE('',*,*,#43389,.F.);
#62951=ORIENTED_EDGE('',*,*,#43390,.F.);
#62952=ORIENTED_EDGE('',*,*,#43391,.F.);
#62953=ORIENTED_EDGE('',*,*,#43392,.F.);
#62954=ORIENTED_EDGE('',*,*,#43387,.F.);
#62955=ORIENTED_EDGE('',*,*,#43392,.T.);
#62956=ORIENTED_EDGE('',*,*,#43393,.F.);
#62957=ORIENTED_EDGE('',*,*,#43107,.T.);
#62958=ORIENTED_EDGE('',*,*,#43388,.T.);
#62959=ORIENTED_EDGE('',*,*,#43394,.F.);
#62960=ORIENTED_EDGE('',*,*,#43395,.F.);
#62961=ORIENTED_EDGE('',*,*,#34242,.T.);
#62962=ORIENTED_EDGE('',*,*,#43396,.F.);
#62963=ORIENTED_EDGE('',*,*,#43394,.T.);
#62964=ORIENTED_EDGE('',*,*,#34241,.T.);
#62965=ORIENTED_EDGE('',*,*,#43397,.F.);
#62966=ORIENTED_EDGE('',*,*,#43396,.T.);
#62967=ORIENTED_EDGE('',*,*,#34240,.T.);
#62968=ORIENTED_EDGE('',*,*,#43398,.F.);
#62969=ORIENTED_EDGE('',*,*,#43397,.T.);
#62970=ORIENTED_EDGE('',*,*,#34239,.T.);
#62971=ORIENTED_EDGE('',*,*,#43108,.T.);
#62972=ORIENTED_EDGE('',*,*,#43398,.T.);
#62973=ORIENTED_EDGE('',*,*,#34238,.T.);
#62974=ORIENTED_EDGE('',*,*,#43399,.F.);
#62975=ORIENTED_EDGE('',*,*,#43110,.T.);
#62976=ORIENTED_EDGE('',*,*,#43399,.T.);
#62977=ORIENTED_EDGE('',*,*,#34237,.T.);
#62978=ORIENTED_EDGE('',*,*,#43400,.F.);
#62979=ORIENTED_EDGE('',*,*,#43401,.F.);
#62980=ORIENTED_EDGE('',*,*,#43400,.T.);
#62981=ORIENTED_EDGE('',*,*,#34236,.T.);
#62982=ORIENTED_EDGE('',*,*,#43402,.F.);
#62983=ORIENTED_EDGE('',*,*,#43401,.T.);
#62984=ORIENTED_EDGE('',*,*,#34235,.T.);
#62985=ORIENTED_EDGE('',*,*,#43403,.F.);
#62986=ORIENTED_EDGE('',*,*,#43402,.T.);
#62987=ORIENTED_EDGE('',*,*,#34234,.T.);
#62988=ORIENTED_EDGE('',*,*,#43404,.F.);
#62989=ORIENTED_EDGE('',*,*,#43403,.T.);
#62990=ORIENTED_EDGE('',*,*,#34233,.T.);
#62991=ORIENTED_EDGE('',*,*,#43112,.T.);
#62992=ORIENTED_EDGE('',*,*,#43404,.T.);
#62993=ORIENTED_EDGE('',*,*,#34232,.T.);
#62994=ORIENTED_EDGE('',*,*,#43405,.F.);
#62995=ORIENTED_EDGE('',*,*,#43113,.T.);
#62996=ORIENTED_EDGE('',*,*,#43405,.T.);
#62997=ORIENTED_EDGE('',*,*,#34231,.T.);
#62998=ORIENTED_EDGE('',*,*,#43406,.F.);
#62999=ORIENTED_EDGE('',*,*,#43407,.F.);
#63000=ORIENTED_EDGE('',*,*,#43406,.T.);
#63001=ORIENTED_EDGE('',*,*,#34230,.T.);
#63002=ORIENTED_EDGE('',*,*,#43408,.F.);
#63003=ORIENTED_EDGE('',*,*,#43407,.T.);
#63004=ORIENTED_EDGE('',*,*,#34229,.T.);
#63005=ORIENTED_EDGE('',*,*,#43409,.F.);
#63006=ORIENTED_EDGE('',*,*,#43408,.T.);
#63007=ORIENTED_EDGE('',*,*,#34228,.T.);
#63008=ORIENTED_EDGE('',*,*,#43410,.F.);
#63009=ORIENTED_EDGE('',*,*,#43409,.T.);
#63010=ORIENTED_EDGE('',*,*,#34227,.T.);
#63011=ORIENTED_EDGE('',*,*,#43115,.T.);
#63012=ORIENTED_EDGE('',*,*,#43410,.T.);
#63013=ORIENTED_EDGE('',*,*,#34226,.T.);
#63014=ORIENTED_EDGE('',*,*,#43411,.F.);
#63015=ORIENTED_EDGE('',*,*,#43116,.T.);
#63016=ORIENTED_EDGE('',*,*,#43411,.T.);
#63017=ORIENTED_EDGE('',*,*,#34225,.T.);
#63018=ORIENTED_EDGE('',*,*,#43412,.F.);
#63019=ORIENTED_EDGE('',*,*,#43413,.F.);
#63020=ORIENTED_EDGE('',*,*,#43412,.T.);
#63021=ORIENTED_EDGE('',*,*,#34224,.T.);
#63022=ORIENTED_EDGE('',*,*,#43414,.F.);
#63023=ORIENTED_EDGE('',*,*,#43413,.T.);
#63024=ORIENTED_EDGE('',*,*,#34223,.T.);
#63025=ORIENTED_EDGE('',*,*,#43415,.F.);
#63026=ORIENTED_EDGE('',*,*,#43414,.T.);
#63027=ORIENTED_EDGE('',*,*,#34222,.T.);
#63028=ORIENTED_EDGE('',*,*,#43416,.F.);
#63029=ORIENTED_EDGE('',*,*,#43415,.T.);
#63030=ORIENTED_EDGE('',*,*,#34221,.T.);
#63031=ORIENTED_EDGE('',*,*,#43118,.T.);
#63032=ORIENTED_EDGE('',*,*,#43416,.T.);
#63033=ORIENTED_EDGE('',*,*,#34220,.T.);
#63034=ORIENTED_EDGE('',*,*,#43417,.F.);
#63035=ORIENTED_EDGE('',*,*,#43119,.T.);
#63036=ORIENTED_EDGE('',*,*,#43417,.T.);
#63037=ORIENTED_EDGE('',*,*,#34219,.T.);
#63038=ORIENTED_EDGE('',*,*,#43418,.F.);
#63039=ORIENTED_EDGE('',*,*,#43419,.F.);
#63040=ORIENTED_EDGE('',*,*,#43418,.T.);
#63041=ORIENTED_EDGE('',*,*,#34218,.T.);
#63042=ORIENTED_EDGE('',*,*,#43420,.F.);
#63043=ORIENTED_EDGE('',*,*,#43419,.T.);
#63044=ORIENTED_EDGE('',*,*,#34217,.T.);
#63045=ORIENTED_EDGE('',*,*,#43421,.F.);
#63046=ORIENTED_EDGE('',*,*,#43420,.T.);
#63047=ORIENTED_EDGE('',*,*,#34216,.T.);
#63048=ORIENTED_EDGE('',*,*,#43422,.F.);
#63049=ORIENTED_EDGE('',*,*,#43421,.T.);
#63050=ORIENTED_EDGE('',*,*,#34215,.T.);
#63051=ORIENTED_EDGE('',*,*,#43121,.T.);
#63052=ORIENTED_EDGE('',*,*,#43422,.T.);
#63053=ORIENTED_EDGE('',*,*,#34214,.T.);
#63054=ORIENTED_EDGE('',*,*,#43423,.F.);
#63055=ORIENTED_EDGE('',*,*,#43122,.T.);
#63056=ORIENTED_EDGE('',*,*,#43423,.T.);
#63057=ORIENTED_EDGE('',*,*,#34213,.T.);
#63058=ORIENTED_EDGE('',*,*,#43424,.F.);
#63059=ORIENTED_EDGE('',*,*,#43425,.F.);
#63060=ORIENTED_EDGE('',*,*,#43424,.T.);
#63061=ORIENTED_EDGE('',*,*,#34212,.T.);
#63062=ORIENTED_EDGE('',*,*,#43426,.F.);
#63063=ORIENTED_EDGE('',*,*,#43425,.T.);
#63064=ORIENTED_EDGE('',*,*,#34211,.T.);
#63065=ORIENTED_EDGE('',*,*,#43427,.F.);
#63066=ORIENTED_EDGE('',*,*,#43426,.T.);
#63067=ORIENTED_EDGE('',*,*,#34210,.T.);
#63068=ORIENTED_EDGE('',*,*,#43428,.F.);
#63069=ORIENTED_EDGE('',*,*,#43427,.T.);
#63070=ORIENTED_EDGE('',*,*,#34209,.T.);
#63071=ORIENTED_EDGE('',*,*,#43124,.T.);
#63072=ORIENTED_EDGE('',*,*,#43428,.T.);
#63073=ORIENTED_EDGE('',*,*,#34208,.T.);
#63074=ORIENTED_EDGE('',*,*,#43429,.F.);
#63075=ORIENTED_EDGE('',*,*,#43125,.T.);
#63076=ORIENTED_EDGE('',*,*,#43429,.T.);
#63077=ORIENTED_EDGE('',*,*,#34207,.T.);
#63078=ORIENTED_EDGE('',*,*,#43430,.F.);
#63079=ORIENTED_EDGE('',*,*,#43431,.F.);
#63080=ORIENTED_EDGE('',*,*,#43430,.T.);
#63081=ORIENTED_EDGE('',*,*,#34206,.T.);
#63082=ORIENTED_EDGE('',*,*,#43432,.F.);
#63083=ORIENTED_EDGE('',*,*,#43431,.T.);
#63084=ORIENTED_EDGE('',*,*,#34205,.T.);
#63085=ORIENTED_EDGE('',*,*,#43433,.F.);
#63086=ORIENTED_EDGE('',*,*,#43432,.T.);
#63087=ORIENTED_EDGE('',*,*,#34204,.T.);
#63088=ORIENTED_EDGE('',*,*,#43434,.F.);
#63089=ORIENTED_EDGE('',*,*,#43433,.T.);
#63090=ORIENTED_EDGE('',*,*,#34203,.T.);
#63091=ORIENTED_EDGE('',*,*,#43127,.T.);
#63092=ORIENTED_EDGE('',*,*,#43434,.T.);
#63093=ORIENTED_EDGE('',*,*,#34202,.T.);
#63094=ORIENTED_EDGE('',*,*,#43435,.F.);
#63095=ORIENTED_EDGE('',*,*,#43128,.T.);
#63096=ORIENTED_EDGE('',*,*,#43435,.T.);
#63097=ORIENTED_EDGE('',*,*,#34201,.T.);
#63098=ORIENTED_EDGE('',*,*,#43436,.F.);
#63099=ORIENTED_EDGE('',*,*,#43437,.F.);
#63100=ORIENTED_EDGE('',*,*,#43436,.T.);
#63101=ORIENTED_EDGE('',*,*,#34200,.T.);
#63102=ORIENTED_EDGE('',*,*,#43438,.F.);
#63103=ORIENTED_EDGE('',*,*,#43437,.T.);
#63104=ORIENTED_EDGE('',*,*,#34199,.T.);
#63105=ORIENTED_EDGE('',*,*,#43439,.F.);
#63106=ORIENTED_EDGE('',*,*,#43438,.T.);
#63107=ORIENTED_EDGE('',*,*,#34198,.T.);
#63108=ORIENTED_EDGE('',*,*,#43440,.F.);
#63109=ORIENTED_EDGE('',*,*,#43439,.T.);
#63110=ORIENTED_EDGE('',*,*,#34197,.T.);
#63111=ORIENTED_EDGE('',*,*,#43130,.T.);
#63112=ORIENTED_EDGE('',*,*,#43440,.T.);
#63113=ORIENTED_EDGE('',*,*,#34196,.T.);
#63114=ORIENTED_EDGE('',*,*,#43441,.F.);
#63115=ORIENTED_EDGE('',*,*,#43131,.T.);
#63116=ORIENTED_EDGE('',*,*,#43441,.T.);
#63117=ORIENTED_EDGE('',*,*,#34195,.T.);
#63118=ORIENTED_EDGE('',*,*,#43442,.F.);
#63119=ORIENTED_EDGE('',*,*,#43443,.F.);
#63120=ORIENTED_EDGE('',*,*,#43442,.T.);
#63121=ORIENTED_EDGE('',*,*,#34194,.T.);
#63122=ORIENTED_EDGE('',*,*,#43444,.F.);
#63123=ORIENTED_EDGE('',*,*,#43443,.T.);
#63124=ORIENTED_EDGE('',*,*,#34193,.T.);
#63125=ORIENTED_EDGE('',*,*,#43445,.F.);
#63126=ORIENTED_EDGE('',*,*,#43444,.T.);
#63127=ORIENTED_EDGE('',*,*,#34192,.T.);
#63128=ORIENTED_EDGE('',*,*,#43446,.F.);
#63129=ORIENTED_EDGE('',*,*,#43445,.T.);
#63130=ORIENTED_EDGE('',*,*,#34191,.T.);
#63131=ORIENTED_EDGE('',*,*,#43133,.T.);
#63132=ORIENTED_EDGE('',*,*,#43446,.T.);
#63133=ORIENTED_EDGE('',*,*,#34190,.T.);
#63134=ORIENTED_EDGE('',*,*,#43447,.F.);
#63135=ORIENTED_EDGE('',*,*,#43134,.T.);
#63136=ORIENTED_EDGE('',*,*,#43447,.T.);
#63137=ORIENTED_EDGE('',*,*,#34189,.T.);
#63138=ORIENTED_EDGE('',*,*,#43448,.F.);
#63139=ORIENTED_EDGE('',*,*,#43449,.F.);
#63140=ORIENTED_EDGE('',*,*,#43448,.T.);
#63141=ORIENTED_EDGE('',*,*,#34188,.T.);
#63142=ORIENTED_EDGE('',*,*,#43450,.F.);
#63143=ORIENTED_EDGE('',*,*,#43449,.T.);
#63144=ORIENTED_EDGE('',*,*,#34187,.T.);
#63145=ORIENTED_EDGE('',*,*,#43451,.F.);
#63146=ORIENTED_EDGE('',*,*,#43450,.T.);
#63147=ORIENTED_EDGE('',*,*,#34186,.T.);
#63148=ORIENTED_EDGE('',*,*,#43452,.F.);
#63149=ORIENTED_EDGE('',*,*,#43451,.T.);
#63150=ORIENTED_EDGE('',*,*,#34185,.T.);
#63151=ORIENTED_EDGE('',*,*,#43136,.T.);
#63152=ORIENTED_EDGE('',*,*,#43452,.T.);
#63153=ORIENTED_EDGE('',*,*,#34184,.T.);
#63154=ORIENTED_EDGE('',*,*,#43453,.F.);
#63155=ORIENTED_EDGE('',*,*,#43137,.T.);
#63156=ORIENTED_EDGE('',*,*,#43453,.T.);
#63157=ORIENTED_EDGE('',*,*,#34183,.T.);
#63158=ORIENTED_EDGE('',*,*,#43454,.F.);
#63159=ORIENTED_EDGE('',*,*,#43455,.F.);
#63160=ORIENTED_EDGE('',*,*,#43454,.T.);
#63161=ORIENTED_EDGE('',*,*,#34182,.T.);
#63162=ORIENTED_EDGE('',*,*,#43456,.F.);
#63163=ORIENTED_EDGE('',*,*,#43455,.T.);
#63164=ORIENTED_EDGE('',*,*,#34181,.T.);
#63165=ORIENTED_EDGE('',*,*,#43457,.F.);
#63166=ORIENTED_EDGE('',*,*,#43456,.T.);
#63167=ORIENTED_EDGE('',*,*,#34180,.T.);
#63168=ORIENTED_EDGE('',*,*,#43458,.F.);
#63169=ORIENTED_EDGE('',*,*,#43457,.T.);
#63170=ORIENTED_EDGE('',*,*,#34179,.T.);
#63171=ORIENTED_EDGE('',*,*,#43139,.T.);
#63172=ORIENTED_EDGE('',*,*,#43458,.T.);
#63173=ORIENTED_EDGE('',*,*,#34178,.T.);
#63174=ORIENTED_EDGE('',*,*,#43459,.F.);
#63175=ORIENTED_EDGE('',*,*,#43140,.T.);
#63176=ORIENTED_EDGE('',*,*,#43459,.T.);
#63177=ORIENTED_EDGE('',*,*,#34177,.T.);
#63178=ORIENTED_EDGE('',*,*,#43460,.F.);
#63179=ORIENTED_EDGE('',*,*,#43461,.F.);
#63180=ORIENTED_EDGE('',*,*,#43460,.T.);
#63181=ORIENTED_EDGE('',*,*,#34176,.T.);
#63182=ORIENTED_EDGE('',*,*,#43462,.F.);
#63183=ORIENTED_EDGE('',*,*,#43461,.T.);
#63184=ORIENTED_EDGE('',*,*,#34175,.T.);
#63185=ORIENTED_EDGE('',*,*,#43463,.F.);
#63186=ORIENTED_EDGE('',*,*,#43462,.T.);
#63187=ORIENTED_EDGE('',*,*,#34174,.T.);
#63188=ORIENTED_EDGE('',*,*,#43464,.F.);
#63189=ORIENTED_EDGE('',*,*,#43463,.T.);
#63190=ORIENTED_EDGE('',*,*,#34173,.T.);
#63191=ORIENTED_EDGE('',*,*,#43142,.T.);
#63192=ORIENTED_EDGE('',*,*,#43464,.T.);
#63193=ORIENTED_EDGE('',*,*,#34172,.T.);
#63194=ORIENTED_EDGE('',*,*,#43465,.F.);
#63195=ORIENTED_EDGE('',*,*,#43143,.T.);
#63196=ORIENTED_EDGE('',*,*,#43465,.T.);
#63197=ORIENTED_EDGE('',*,*,#34171,.T.);
#63198=ORIENTED_EDGE('',*,*,#43466,.F.);
#63199=ORIENTED_EDGE('',*,*,#43467,.F.);
#63200=ORIENTED_EDGE('',*,*,#43466,.T.);
#63201=ORIENTED_EDGE('',*,*,#34170,.T.);
#63202=ORIENTED_EDGE('',*,*,#43468,.F.);
#63203=ORIENTED_EDGE('',*,*,#43467,.T.);
#63204=ORIENTED_EDGE('',*,*,#34169,.T.);
#63205=ORIENTED_EDGE('',*,*,#43469,.F.);
#63206=ORIENTED_EDGE('',*,*,#43468,.T.);
#63207=ORIENTED_EDGE('',*,*,#34168,.T.);
#63208=ORIENTED_EDGE('',*,*,#43470,.F.);
#63209=ORIENTED_EDGE('',*,*,#43469,.T.);
#63210=ORIENTED_EDGE('',*,*,#34167,.T.);
#63211=ORIENTED_EDGE('',*,*,#43145,.T.);
#63212=ORIENTED_EDGE('',*,*,#43470,.T.);
#63213=ORIENTED_EDGE('',*,*,#34166,.T.);
#63214=ORIENTED_EDGE('',*,*,#43471,.F.);
#63215=ORIENTED_EDGE('',*,*,#43146,.T.);
#63216=ORIENTED_EDGE('',*,*,#43471,.T.);
#63217=ORIENTED_EDGE('',*,*,#34165,.T.);
#63218=ORIENTED_EDGE('',*,*,#43472,.F.);
#63219=ORIENTED_EDGE('',*,*,#43473,.F.);
#63220=ORIENTED_EDGE('',*,*,#43472,.T.);
#63221=ORIENTED_EDGE('',*,*,#34164,.T.);
#63222=ORIENTED_EDGE('',*,*,#43474,.F.);
#63223=ORIENTED_EDGE('',*,*,#43473,.T.);
#63224=ORIENTED_EDGE('',*,*,#34163,.T.);
#63225=ORIENTED_EDGE('',*,*,#43475,.F.);
#63226=ORIENTED_EDGE('',*,*,#43474,.T.);
#63227=ORIENTED_EDGE('',*,*,#34162,.T.);
#63228=ORIENTED_EDGE('',*,*,#43476,.F.);
#63229=ORIENTED_EDGE('',*,*,#43475,.T.);
#63230=ORIENTED_EDGE('',*,*,#34161,.T.);
#63231=ORIENTED_EDGE('',*,*,#43148,.T.);
#63232=ORIENTED_EDGE('',*,*,#43476,.T.);
#63233=ORIENTED_EDGE('',*,*,#34160,.T.);
#63234=ORIENTED_EDGE('',*,*,#43477,.F.);
#63235=ORIENTED_EDGE('',*,*,#43149,.T.);
#63236=ORIENTED_EDGE('',*,*,#43477,.T.);
#63237=ORIENTED_EDGE('',*,*,#34159,.T.);
#63238=ORIENTED_EDGE('',*,*,#43478,.F.);
#63239=ORIENTED_EDGE('',*,*,#43479,.F.);
#63240=ORIENTED_EDGE('',*,*,#43478,.T.);
#63241=ORIENTED_EDGE('',*,*,#34158,.T.);
#63242=ORIENTED_EDGE('',*,*,#43480,.F.);
#63243=ORIENTED_EDGE('',*,*,#43479,.T.);
#63244=ORIENTED_EDGE('',*,*,#34157,.T.);
#63245=ORIENTED_EDGE('',*,*,#43480,.T.);
#63246=ORIENTED_EDGE('',*,*,#34156,.T.);
#63247=ORIENTED_EDGE('',*,*,#43481,.F.);
#63248=ORIENTED_EDGE('',*,*,#43481,.T.);
#63249=ORIENTED_EDGE('',*,*,#34332,.T.);
#63250=ORIENTED_EDGE('',*,*,#43482,.F.);
#63251=ORIENTED_EDGE('',*,*,#43482,.T.);
#63252=ORIENTED_EDGE('',*,*,#34331,.T.);
#63253=ORIENTED_EDGE('',*,*,#43483,.F.);
#63254=ORIENTED_EDGE('',*,*,#43151,.T.);
#63255=ORIENTED_EDGE('',*,*,#43152,.T.);
#63256=ORIENTED_EDGE('',*,*,#43483,.T.);
#63257=ORIENTED_EDGE('',*,*,#34330,.T.);
#63258=ORIENTED_EDGE('',*,*,#43484,.F.);
#63259=ORIENTED_EDGE('',*,*,#43485,.F.);
#63260=ORIENTED_EDGE('',*,*,#43484,.T.);
#63261=ORIENTED_EDGE('',*,*,#34329,.T.);
#63262=ORIENTED_EDGE('',*,*,#43486,.F.);
#63263=ORIENTED_EDGE('',*,*,#43485,.T.);
#63264=ORIENTED_EDGE('',*,*,#34328,.T.);
#63265=ORIENTED_EDGE('',*,*,#43487,.F.);
#63266=ORIENTED_EDGE('',*,*,#43486,.T.);
#63267=ORIENTED_EDGE('',*,*,#34327,.T.);
#63268=ORIENTED_EDGE('',*,*,#43488,.F.);
#63269=ORIENTED_EDGE('',*,*,#43487,.T.);
#63270=ORIENTED_EDGE('',*,*,#34326,.T.);
#63271=ORIENTED_EDGE('',*,*,#43154,.T.);
#63272=ORIENTED_EDGE('',*,*,#43488,.T.);
#63273=ORIENTED_EDGE('',*,*,#34325,.T.);
#63274=ORIENTED_EDGE('',*,*,#43489,.F.);
#63275=ORIENTED_EDGE('',*,*,#43155,.T.);
#63276=ORIENTED_EDGE('',*,*,#43489,.T.);
#63277=ORIENTED_EDGE('',*,*,#34324,.T.);
#63278=ORIENTED_EDGE('',*,*,#43490,.F.);
#63279=ORIENTED_EDGE('',*,*,#43491,.F.);
#63280=ORIENTED_EDGE('',*,*,#43490,.T.);
#63281=ORIENTED_EDGE('',*,*,#34323,.T.);
#63282=ORIENTED_EDGE('',*,*,#43492,.F.);
#63283=ORIENTED_EDGE('',*,*,#43491,.T.);
#63284=ORIENTED_EDGE('',*,*,#34322,.T.);
#63285=ORIENTED_EDGE('',*,*,#43493,.F.);
#63286=ORIENTED_EDGE('',*,*,#43492,.T.);
#63287=ORIENTED_EDGE('',*,*,#34321,.T.);
#63288=ORIENTED_EDGE('',*,*,#43494,.F.);
#63289=ORIENTED_EDGE('',*,*,#43493,.T.);
#63290=ORIENTED_EDGE('',*,*,#34320,.T.);
#63291=ORIENTED_EDGE('',*,*,#43157,.T.);
#63292=ORIENTED_EDGE('',*,*,#43494,.T.);
#63293=ORIENTED_EDGE('',*,*,#34319,.T.);
#63294=ORIENTED_EDGE('',*,*,#43495,.F.);
#63295=ORIENTED_EDGE('',*,*,#43158,.T.);
#63296=ORIENTED_EDGE('',*,*,#43495,.T.);
#63297=ORIENTED_EDGE('',*,*,#34318,.T.);
#63298=ORIENTED_EDGE('',*,*,#43496,.F.);
#63299=ORIENTED_EDGE('',*,*,#43497,.F.);
#63300=ORIENTED_EDGE('',*,*,#43496,.T.);
#63301=ORIENTED_EDGE('',*,*,#34317,.T.);
#63302=ORIENTED_EDGE('',*,*,#43498,.F.);
#63303=ORIENTED_EDGE('',*,*,#43497,.T.);
#63304=ORIENTED_EDGE('',*,*,#34316,.T.);
#63305=ORIENTED_EDGE('',*,*,#43499,.F.);
#63306=ORIENTED_EDGE('',*,*,#43498,.T.);
#63307=ORIENTED_EDGE('',*,*,#34315,.T.);
#63308=ORIENTED_EDGE('',*,*,#43500,.F.);
#63309=ORIENTED_EDGE('',*,*,#43499,.T.);
#63310=ORIENTED_EDGE('',*,*,#34314,.T.);
#63311=ORIENTED_EDGE('',*,*,#43160,.T.);
#63312=ORIENTED_EDGE('',*,*,#43500,.T.);
#63313=ORIENTED_EDGE('',*,*,#34313,.T.);
#63314=ORIENTED_EDGE('',*,*,#43501,.F.);
#63315=ORIENTED_EDGE('',*,*,#43161,.T.);
#63316=ORIENTED_EDGE('',*,*,#43501,.T.);
#63317=ORIENTED_EDGE('',*,*,#34312,.T.);
#63318=ORIENTED_EDGE('',*,*,#43502,.F.);
#63319=ORIENTED_EDGE('',*,*,#43503,.F.);
#63320=ORIENTED_EDGE('',*,*,#43502,.T.);
#63321=ORIENTED_EDGE('',*,*,#34311,.T.);
#63322=ORIENTED_EDGE('',*,*,#43504,.F.);
#63323=ORIENTED_EDGE('',*,*,#43503,.T.);
#63324=ORIENTED_EDGE('',*,*,#34310,.T.);
#63325=ORIENTED_EDGE('',*,*,#43505,.F.);
#63326=ORIENTED_EDGE('',*,*,#43504,.T.);
#63327=ORIENTED_EDGE('',*,*,#34309,.T.);
#63328=ORIENTED_EDGE('',*,*,#43506,.F.);
#63329=ORIENTED_EDGE('',*,*,#43505,.T.);
#63330=ORIENTED_EDGE('',*,*,#34308,.T.);
#63331=ORIENTED_EDGE('',*,*,#43163,.T.);
#63332=ORIENTED_EDGE('',*,*,#43506,.T.);
#63333=ORIENTED_EDGE('',*,*,#34307,.T.);
#63334=ORIENTED_EDGE('',*,*,#43507,.F.);
#63335=ORIENTED_EDGE('',*,*,#43164,.T.);
#63336=ORIENTED_EDGE('',*,*,#43507,.T.);
#63337=ORIENTED_EDGE('',*,*,#34306,.T.);
#63338=ORIENTED_EDGE('',*,*,#43508,.F.);
#63339=ORIENTED_EDGE('',*,*,#43509,.F.);
#63340=ORIENTED_EDGE('',*,*,#43508,.T.);
#63341=ORIENTED_EDGE('',*,*,#34305,.T.);
#63342=ORIENTED_EDGE('',*,*,#43510,.F.);
#63343=ORIENTED_EDGE('',*,*,#43509,.T.);
#63344=ORIENTED_EDGE('',*,*,#34304,.T.);
#63345=ORIENTED_EDGE('',*,*,#43511,.F.);
#63346=ORIENTED_EDGE('',*,*,#43510,.T.);
#63347=ORIENTED_EDGE('',*,*,#34303,.T.);
#63348=ORIENTED_EDGE('',*,*,#43512,.F.);
#63349=ORIENTED_EDGE('',*,*,#43511,.T.);
#63350=ORIENTED_EDGE('',*,*,#34302,.T.);
#63351=ORIENTED_EDGE('',*,*,#43166,.T.);
#63352=ORIENTED_EDGE('',*,*,#43512,.T.);
#63353=ORIENTED_EDGE('',*,*,#34301,.T.);
#63354=ORIENTED_EDGE('',*,*,#43513,.F.);
#63355=ORIENTED_EDGE('',*,*,#43167,.T.);
#63356=ORIENTED_EDGE('',*,*,#43513,.T.);
#63357=ORIENTED_EDGE('',*,*,#34300,.T.);
#63358=ORIENTED_EDGE('',*,*,#43514,.F.);
#63359=ORIENTED_EDGE('',*,*,#43515,.F.);
#63360=ORIENTED_EDGE('',*,*,#43514,.T.);
#63361=ORIENTED_EDGE('',*,*,#34299,.T.);
#63362=ORIENTED_EDGE('',*,*,#43516,.F.);
#63363=ORIENTED_EDGE('',*,*,#43515,.T.);
#63364=ORIENTED_EDGE('',*,*,#34298,.T.);
#63365=ORIENTED_EDGE('',*,*,#43517,.F.);
#63366=ORIENTED_EDGE('',*,*,#43516,.T.);
#63367=ORIENTED_EDGE('',*,*,#34297,.T.);
#63368=ORIENTED_EDGE('',*,*,#43518,.F.);
#63369=ORIENTED_EDGE('',*,*,#43517,.T.);
#63370=ORIENTED_EDGE('',*,*,#34296,.T.);
#63371=ORIENTED_EDGE('',*,*,#43169,.T.);
#63372=ORIENTED_EDGE('',*,*,#43518,.T.);
#63373=ORIENTED_EDGE('',*,*,#34295,.T.);
#63374=ORIENTED_EDGE('',*,*,#43519,.F.);
#63375=ORIENTED_EDGE('',*,*,#43170,.T.);
#63376=ORIENTED_EDGE('',*,*,#43519,.T.);
#63377=ORIENTED_EDGE('',*,*,#34294,.T.);
#63378=ORIENTED_EDGE('',*,*,#43520,.F.);
#63379=ORIENTED_EDGE('',*,*,#43521,.F.);
#63380=ORIENTED_EDGE('',*,*,#43520,.T.);
#63381=ORIENTED_EDGE('',*,*,#34293,.T.);
#63382=ORIENTED_EDGE('',*,*,#43522,.F.);
#63383=ORIENTED_EDGE('',*,*,#43521,.T.);
#63384=ORIENTED_EDGE('',*,*,#34292,.T.);
#63385=ORIENTED_EDGE('',*,*,#43523,.F.);
#63386=ORIENTED_EDGE('',*,*,#43522,.T.);
#63387=ORIENTED_EDGE('',*,*,#34291,.T.);
#63388=ORIENTED_EDGE('',*,*,#43524,.F.);
#63389=ORIENTED_EDGE('',*,*,#43523,.T.);
#63390=ORIENTED_EDGE('',*,*,#34290,.T.);
#63391=ORIENTED_EDGE('',*,*,#43172,.T.);
#63392=ORIENTED_EDGE('',*,*,#43524,.T.);
#63393=ORIENTED_EDGE('',*,*,#34289,.T.);
#63394=ORIENTED_EDGE('',*,*,#43525,.F.);
#63395=ORIENTED_EDGE('',*,*,#43173,.T.);
#63396=ORIENTED_EDGE('',*,*,#43525,.T.);
#63397=ORIENTED_EDGE('',*,*,#34288,.T.);
#63398=ORIENTED_EDGE('',*,*,#43526,.F.);
#63399=ORIENTED_EDGE('',*,*,#43527,.F.);
#63400=ORIENTED_EDGE('',*,*,#43526,.T.);
#63401=ORIENTED_EDGE('',*,*,#34287,.T.);
#63402=ORIENTED_EDGE('',*,*,#43528,.F.);
#63403=ORIENTED_EDGE('',*,*,#43527,.T.);
#63404=ORIENTED_EDGE('',*,*,#34286,.T.);
#63405=ORIENTED_EDGE('',*,*,#43529,.F.);
#63406=ORIENTED_EDGE('',*,*,#43528,.T.);
#63407=ORIENTED_EDGE('',*,*,#34285,.T.);
#63408=ORIENTED_EDGE('',*,*,#43530,.F.);
#63409=ORIENTED_EDGE('',*,*,#43529,.T.);
#63410=ORIENTED_EDGE('',*,*,#34284,.T.);
#63411=ORIENTED_EDGE('',*,*,#43175,.T.);
#63412=ORIENTED_EDGE('',*,*,#43530,.T.);
#63413=ORIENTED_EDGE('',*,*,#34283,.T.);
#63414=ORIENTED_EDGE('',*,*,#43531,.F.);
#63415=ORIENTED_EDGE('',*,*,#43176,.T.);
#63416=ORIENTED_EDGE('',*,*,#43531,.T.);
#63417=ORIENTED_EDGE('',*,*,#34282,.T.);
#63418=ORIENTED_EDGE('',*,*,#43532,.F.);
#63419=ORIENTED_EDGE('',*,*,#43533,.F.);
#63420=ORIENTED_EDGE('',*,*,#43532,.T.);
#63421=ORIENTED_EDGE('',*,*,#34281,.T.);
#63422=ORIENTED_EDGE('',*,*,#43534,.F.);
#63423=ORIENTED_EDGE('',*,*,#43533,.T.);
#63424=ORIENTED_EDGE('',*,*,#34280,.T.);
#63425=ORIENTED_EDGE('',*,*,#43535,.F.);
#63426=ORIENTED_EDGE('',*,*,#43534,.T.);
#63427=ORIENTED_EDGE('',*,*,#34279,.T.);
#63428=ORIENTED_EDGE('',*,*,#43536,.F.);
#63429=ORIENTED_EDGE('',*,*,#43535,.T.);
#63430=ORIENTED_EDGE('',*,*,#34278,.T.);
#63431=ORIENTED_EDGE('',*,*,#43178,.T.);
#63432=ORIENTED_EDGE('',*,*,#43536,.T.);
#63433=ORIENTED_EDGE('',*,*,#34277,.T.);
#63434=ORIENTED_EDGE('',*,*,#43537,.F.);
#63435=ORIENTED_EDGE('',*,*,#43179,.T.);
#63436=ORIENTED_EDGE('',*,*,#43537,.T.);
#63437=ORIENTED_EDGE('',*,*,#34276,.T.);
#63438=ORIENTED_EDGE('',*,*,#43538,.F.);
#63439=ORIENTED_EDGE('',*,*,#43539,.F.);
#63440=ORIENTED_EDGE('',*,*,#43538,.T.);
#63441=ORIENTED_EDGE('',*,*,#34275,.T.);
#63442=ORIENTED_EDGE('',*,*,#43540,.F.);
#63443=ORIENTED_EDGE('',*,*,#43539,.T.);
#63444=ORIENTED_EDGE('',*,*,#34274,.T.);
#63445=ORIENTED_EDGE('',*,*,#43541,.F.);
#63446=ORIENTED_EDGE('',*,*,#43540,.T.);
#63447=ORIENTED_EDGE('',*,*,#34273,.T.);
#63448=ORIENTED_EDGE('',*,*,#43542,.F.);
#63449=ORIENTED_EDGE('',*,*,#43541,.T.);
#63450=ORIENTED_EDGE('',*,*,#34272,.T.);
#63451=ORIENTED_EDGE('',*,*,#43181,.T.);
#63452=ORIENTED_EDGE('',*,*,#43542,.T.);
#63453=ORIENTED_EDGE('',*,*,#34271,.T.);
#63454=ORIENTED_EDGE('',*,*,#43543,.F.);
#63455=ORIENTED_EDGE('',*,*,#43182,.T.);
#63456=ORIENTED_EDGE('',*,*,#43543,.T.);
#63457=ORIENTED_EDGE('',*,*,#34270,.T.);
#63458=ORIENTED_EDGE('',*,*,#43544,.F.);
#63459=ORIENTED_EDGE('',*,*,#43545,.F.);
#63460=ORIENTED_EDGE('',*,*,#43544,.T.);
#63461=ORIENTED_EDGE('',*,*,#34269,.T.);
#63462=ORIENTED_EDGE('',*,*,#43546,.F.);
#63463=ORIENTED_EDGE('',*,*,#43545,.T.);
#63464=ORIENTED_EDGE('',*,*,#34268,.T.);
#63465=ORIENTED_EDGE('',*,*,#43547,.F.);
#63466=ORIENTED_EDGE('',*,*,#43546,.T.);
#63467=ORIENTED_EDGE('',*,*,#34267,.T.);
#63468=ORIENTED_EDGE('',*,*,#43548,.F.);
#63469=ORIENTED_EDGE('',*,*,#43547,.T.);
#63470=ORIENTED_EDGE('',*,*,#34266,.T.);
#63471=ORIENTED_EDGE('',*,*,#43184,.T.);
#63472=ORIENTED_EDGE('',*,*,#43548,.T.);
#63473=ORIENTED_EDGE('',*,*,#34265,.T.);
#63474=ORIENTED_EDGE('',*,*,#43549,.F.);
#63475=ORIENTED_EDGE('',*,*,#43185,.T.);
#63476=ORIENTED_EDGE('',*,*,#43549,.T.);
#63477=ORIENTED_EDGE('',*,*,#34264,.T.);
#63478=ORIENTED_EDGE('',*,*,#43550,.F.);
#63479=ORIENTED_EDGE('',*,*,#43551,.F.);
#63480=ORIENTED_EDGE('',*,*,#43550,.T.);
#63481=ORIENTED_EDGE('',*,*,#34263,.T.);
#63482=ORIENTED_EDGE('',*,*,#43552,.F.);
#63483=ORIENTED_EDGE('',*,*,#43551,.T.);
#63484=ORIENTED_EDGE('',*,*,#34262,.T.);
#63485=ORIENTED_EDGE('',*,*,#43553,.F.);
#63486=ORIENTED_EDGE('',*,*,#43552,.T.);
#63487=ORIENTED_EDGE('',*,*,#34261,.T.);
#63488=ORIENTED_EDGE('',*,*,#43554,.F.);
#63489=ORIENTED_EDGE('',*,*,#43553,.T.);
#63490=ORIENTED_EDGE('',*,*,#34260,.T.);
#63491=ORIENTED_EDGE('',*,*,#43187,.T.);
#63492=ORIENTED_EDGE('',*,*,#43554,.T.);
#63493=ORIENTED_EDGE('',*,*,#34259,.T.);
#63494=ORIENTED_EDGE('',*,*,#43555,.F.);
#63495=ORIENTED_EDGE('',*,*,#43188,.T.);
#63496=ORIENTED_EDGE('',*,*,#43555,.T.);
#63497=ORIENTED_EDGE('',*,*,#34258,.T.);
#63498=ORIENTED_EDGE('',*,*,#43556,.F.);
#63499=ORIENTED_EDGE('',*,*,#43557,.F.);
#63500=ORIENTED_EDGE('',*,*,#43556,.T.);
#63501=ORIENTED_EDGE('',*,*,#34257,.T.);
#63502=ORIENTED_EDGE('',*,*,#43558,.F.);
#63503=ORIENTED_EDGE('',*,*,#43557,.T.);
#63504=ORIENTED_EDGE('',*,*,#34256,.T.);
#63505=ORIENTED_EDGE('',*,*,#43559,.F.);
#63506=ORIENTED_EDGE('',*,*,#43558,.T.);
#63507=ORIENTED_EDGE('',*,*,#34255,.T.);
#63508=ORIENTED_EDGE('',*,*,#43560,.F.);
#63509=ORIENTED_EDGE('',*,*,#43559,.T.);
#63510=ORIENTED_EDGE('',*,*,#34254,.T.);
#63511=ORIENTED_EDGE('',*,*,#43190,.T.);
#63512=ORIENTED_EDGE('',*,*,#43560,.T.);
#63513=ORIENTED_EDGE('',*,*,#34253,.T.);
#63514=ORIENTED_EDGE('',*,*,#43561,.F.);
#63515=ORIENTED_EDGE('',*,*,#43191,.T.);
#63516=ORIENTED_EDGE('',*,*,#43561,.T.);
#63517=ORIENTED_EDGE('',*,*,#34252,.T.);
#63518=ORIENTED_EDGE('',*,*,#43562,.F.);
#63519=ORIENTED_EDGE('',*,*,#43563,.F.);
#63520=ORIENTED_EDGE('',*,*,#43562,.T.);
#63521=ORIENTED_EDGE('',*,*,#34251,.T.);
#63522=ORIENTED_EDGE('',*,*,#43564,.F.);
#63523=ORIENTED_EDGE('',*,*,#43563,.T.);
#63524=ORIENTED_EDGE('',*,*,#34250,.T.);
#63525=ORIENTED_EDGE('',*,*,#43565,.F.);
#63526=ORIENTED_EDGE('',*,*,#43564,.T.);
#63527=ORIENTED_EDGE('',*,*,#34249,.T.);
#63528=ORIENTED_EDGE('',*,*,#43566,.F.);
#63529=ORIENTED_EDGE('',*,*,#43565,.T.);
#63530=ORIENTED_EDGE('',*,*,#34248,.T.);
#63531=ORIENTED_EDGE('',*,*,#43193,.T.);
#63532=ORIENTED_EDGE('',*,*,#43566,.T.);
#63533=ORIENTED_EDGE('',*,*,#34247,.T.);
#63534=ORIENTED_EDGE('',*,*,#43567,.F.);
#63535=ORIENTED_EDGE('',*,*,#43567,.T.);
#63536=ORIENTED_EDGE('',*,*,#34246,.T.);
#63537=ORIENTED_EDGE('',*,*,#34243,.T.);
#63538=ORIENTED_EDGE('',*,*,#43395,.T.);
#63539=ORIENTED_EDGE('',*,*,#43194,.T.);
#63540=ORIENTED_EDGE('',*,*,#43568,.F.);
#63541=ORIENTED_EDGE('',*,*,#43569,.F.);
#63542=ORIENTED_EDGE('',*,*,#43198,.T.);
#63543=ORIENTED_EDGE('',*,*,#43197,.T.);
#63544=ORIENTED_EDGE('',*,*,#43570,.F.);
#63545=ORIENTED_EDGE('',*,*,#43201,.T.);
#63546=ORIENTED_EDGE('',*,*,#43199,.T.);
#63547=ORIENTED_EDGE('',*,*,#43569,.T.);
#63548=ORIENTED_EDGE('',*,*,#43571,.F.);
#63549=ORIENTED_EDGE('',*,*,#43572,.F.);
#63550=ORIENTED_EDGE('',*,*,#43205,.T.);
#63551=ORIENTED_EDGE('',*,*,#43204,.T.);
#63552=ORIENTED_EDGE('',*,*,#43573,.F.);
#63553=ORIENTED_EDGE('',*,*,#43208,.T.);
#63554=ORIENTED_EDGE('',*,*,#43206,.T.);
#63555=ORIENTED_EDGE('',*,*,#43572,.T.);
#63556=ORIENTED_EDGE('',*,*,#43574,.F.);
#63557=ORIENTED_EDGE('',*,*,#43575,.F.);
#63558=ORIENTED_EDGE('',*,*,#43212,.T.);
#63559=ORIENTED_EDGE('',*,*,#43211,.T.);
#63560=ORIENTED_EDGE('',*,*,#43576,.F.);
#63561=ORIENTED_EDGE('',*,*,#43215,.T.);
#63562=ORIENTED_EDGE('',*,*,#43213,.T.);
#63563=ORIENTED_EDGE('',*,*,#43575,.T.);
#63564=ORIENTED_EDGE('',*,*,#43577,.F.);
#63565=ORIENTED_EDGE('',*,*,#43578,.F.);
#63566=ORIENTED_EDGE('',*,*,#43219,.T.);
#63567=ORIENTED_EDGE('',*,*,#43218,.T.);
#63568=ORIENTED_EDGE('',*,*,#43579,.F.);
#63569=ORIENTED_EDGE('',*,*,#43222,.T.);
#63570=ORIENTED_EDGE('',*,*,#43220,.T.);
#63571=ORIENTED_EDGE('',*,*,#43578,.T.);
#63572=ORIENTED_EDGE('',*,*,#43580,.F.);
#63573=ORIENTED_EDGE('',*,*,#43581,.F.);
#63574=ORIENTED_EDGE('',*,*,#43226,.T.);
#63575=ORIENTED_EDGE('',*,*,#43225,.T.);
#63576=ORIENTED_EDGE('',*,*,#43582,.F.);
#63577=ORIENTED_EDGE('',*,*,#43229,.T.);
#63578=ORIENTED_EDGE('',*,*,#43227,.T.);
#63579=ORIENTED_EDGE('',*,*,#43581,.T.);
#63580=ORIENTED_EDGE('',*,*,#43583,.F.);
#63581=ORIENTED_EDGE('',*,*,#43584,.F.);
#63582=ORIENTED_EDGE('',*,*,#43233,.T.);
#63583=ORIENTED_EDGE('',*,*,#43232,.T.);
#63584=ORIENTED_EDGE('',*,*,#43585,.F.);
#63585=ORIENTED_EDGE('',*,*,#43236,.T.);
#63586=ORIENTED_EDGE('',*,*,#43234,.T.);
#63587=ORIENTED_EDGE('',*,*,#43584,.T.);
#63588=ORIENTED_EDGE('',*,*,#43586,.F.);
#63589=ORIENTED_EDGE('',*,*,#43587,.F.);
#63590=ORIENTED_EDGE('',*,*,#43240,.T.);
#63591=ORIENTED_EDGE('',*,*,#43239,.T.);
#63592=ORIENTED_EDGE('',*,*,#43588,.F.);
#63593=ORIENTED_EDGE('',*,*,#43243,.T.);
#63594=ORIENTED_EDGE('',*,*,#43241,.T.);
#63595=ORIENTED_EDGE('',*,*,#43587,.T.);
#63596=ORIENTED_EDGE('',*,*,#43589,.F.);
#63597=ORIENTED_EDGE('',*,*,#43590,.F.);
#63598=ORIENTED_EDGE('',*,*,#43247,.T.);
#63599=ORIENTED_EDGE('',*,*,#43246,.T.);
#63600=ORIENTED_EDGE('',*,*,#43591,.F.);
#63601=ORIENTED_EDGE('',*,*,#43250,.T.);
#63602=ORIENTED_EDGE('',*,*,#43248,.T.);
#63603=ORIENTED_EDGE('',*,*,#43590,.T.);
#63604=ORIENTED_EDGE('',*,*,#43592,.F.);
#63605=ORIENTED_EDGE('',*,*,#43593,.F.);
#63606=ORIENTED_EDGE('',*,*,#43254,.T.);
#63607=ORIENTED_EDGE('',*,*,#43253,.T.);
#63608=ORIENTED_EDGE('',*,*,#43594,.F.);
#63609=ORIENTED_EDGE('',*,*,#43257,.T.);
#63610=ORIENTED_EDGE('',*,*,#43255,.T.);
#63611=ORIENTED_EDGE('',*,*,#43593,.T.);
#63612=ORIENTED_EDGE('',*,*,#43595,.F.);
#63613=ORIENTED_EDGE('',*,*,#43596,.F.);
#63614=ORIENTED_EDGE('',*,*,#43261,.T.);
#63615=ORIENTED_EDGE('',*,*,#43260,.T.);
#63616=ORIENTED_EDGE('',*,*,#43597,.F.);
#63617=ORIENTED_EDGE('',*,*,#43264,.T.);
#63618=ORIENTED_EDGE('',*,*,#43262,.T.);
#63619=ORIENTED_EDGE('',*,*,#43596,.T.);
#63620=ORIENTED_EDGE('',*,*,#43598,.F.);
#63621=ORIENTED_EDGE('',*,*,#43599,.F.);
#63622=ORIENTED_EDGE('',*,*,#43268,.T.);
#63623=ORIENTED_EDGE('',*,*,#43267,.T.);
#63624=ORIENTED_EDGE('',*,*,#43600,.F.);
#63625=ORIENTED_EDGE('',*,*,#43271,.T.);
#63626=ORIENTED_EDGE('',*,*,#43269,.T.);
#63627=ORIENTED_EDGE('',*,*,#43599,.T.);
#63628=ORIENTED_EDGE('',*,*,#43601,.F.);
#63629=ORIENTED_EDGE('',*,*,#43602,.F.);
#63630=ORIENTED_EDGE('',*,*,#43275,.T.);
#63631=ORIENTED_EDGE('',*,*,#43274,.T.);
#63632=ORIENTED_EDGE('',*,*,#43603,.F.);
#63633=ORIENTED_EDGE('',*,*,#43278,.T.);
#63634=ORIENTED_EDGE('',*,*,#43276,.T.);
#63635=ORIENTED_EDGE('',*,*,#43602,.T.);
#63636=ORIENTED_EDGE('',*,*,#43604,.F.);
#63637=ORIENTED_EDGE('',*,*,#43605,.F.);
#63638=ORIENTED_EDGE('',*,*,#43282,.T.);
#63639=ORIENTED_EDGE('',*,*,#43281,.T.);
#63640=ORIENTED_EDGE('',*,*,#43606,.F.);
#63641=ORIENTED_EDGE('',*,*,#43285,.T.);
#63642=ORIENTED_EDGE('',*,*,#43283,.T.);
#63643=ORIENTED_EDGE('',*,*,#43605,.T.);
#63644=ORIENTED_EDGE('',*,*,#43607,.F.);
#63645=ORIENTED_EDGE('',*,*,#43608,.F.);
#63646=ORIENTED_EDGE('',*,*,#43289,.T.);
#63647=ORIENTED_EDGE('',*,*,#43288,.T.);
#63648=ORIENTED_EDGE('',*,*,#43609,.F.);
#63649=ORIENTED_EDGE('',*,*,#43292,.T.);
#63650=ORIENTED_EDGE('',*,*,#43290,.T.);
#63651=ORIENTED_EDGE('',*,*,#43608,.T.);
#63652=ORIENTED_EDGE('',*,*,#43610,.F.);
#63653=ORIENTED_EDGE('',*,*,#43611,.F.);
#63654=ORIENTED_EDGE('',*,*,#34347,.T.);
#63655=ORIENTED_EDGE('',*,*,#43294,.T.);
#63656=ORIENTED_EDGE('',*,*,#43612,.F.);
#63657=ORIENTED_EDGE('',*,*,#43295,.T.);
#63658=ORIENTED_EDGE('',*,*,#34348,.T.);
#63659=ORIENTED_EDGE('',*,*,#43611,.T.);
#63660=ORIENTED_EDGE('',*,*,#43613,.F.);
#63661=ORIENTED_EDGE('',*,*,#43614,.F.);
#63662=ORIENTED_EDGE('',*,*,#43299,.T.);
#63663=ORIENTED_EDGE('',*,*,#43298,.T.);
#63664=ORIENTED_EDGE('',*,*,#43615,.F.);
#63665=ORIENTED_EDGE('',*,*,#43302,.T.);
#63666=ORIENTED_EDGE('',*,*,#43300,.T.);
#63667=ORIENTED_EDGE('',*,*,#43614,.T.);
#63668=ORIENTED_EDGE('',*,*,#43616,.F.);
#63669=ORIENTED_EDGE('',*,*,#43617,.F.);
#63670=ORIENTED_EDGE('',*,*,#43306,.T.);
#63671=ORIENTED_EDGE('',*,*,#43305,.T.);
#63672=ORIENTED_EDGE('',*,*,#43618,.F.);
#63673=ORIENTED_EDGE('',*,*,#43309,.T.);
#63674=ORIENTED_EDGE('',*,*,#43307,.T.);
#63675=ORIENTED_EDGE('',*,*,#43617,.T.);
#63676=ORIENTED_EDGE('',*,*,#43619,.F.);
#63677=ORIENTED_EDGE('',*,*,#43620,.F.);
#63678=ORIENTED_EDGE('',*,*,#43315,.T.);
#63679=ORIENTED_EDGE('',*,*,#43312,.T.);
#63680=ORIENTED_EDGE('',*,*,#43316,.T.);
#63681=ORIENTED_EDGE('',*,*,#43620,.T.);
#63682=ORIENTED_EDGE('',*,*,#43621,.F.);
#63683=ORIENTED_EDGE('',*,*,#43314,.T.);
#63684=ORIENTED_EDGE('',*,*,#43321,.T.);
#63685=ORIENTED_EDGE('',*,*,#43317,.T.);
#63686=ORIENTED_EDGE('',*,*,#43622,.F.);
#63687=ORIENTED_EDGE('',*,*,#43623,.F.);
#63688=ORIENTED_EDGE('',*,*,#43624,.F.);
#63689=ORIENTED_EDGE('',*,*,#43323,.T.);
#63690=ORIENTED_EDGE('',*,*,#43322,.T.);
#63691=ORIENTED_EDGE('',*,*,#43623,.T.);
#63692=ORIENTED_EDGE('',*,*,#43625,.F.);
#63693=ORIENTED_EDGE('',*,*,#43626,.F.);
#63694=ORIENTED_EDGE('',*,*,#43327,.T.);
#63695=ORIENTED_EDGE('',*,*,#43326,.T.);
#63696=ORIENTED_EDGE('',*,*,#43627,.F.);
#63697=ORIENTED_EDGE('',*,*,#43330,.T.);
#63698=ORIENTED_EDGE('',*,*,#43328,.T.);
#63699=ORIENTED_EDGE('',*,*,#43626,.T.);
#63700=ORIENTED_EDGE('',*,*,#43628,.F.);
#63701=ORIENTED_EDGE('',*,*,#43629,.F.);
#63702=ORIENTED_EDGE('',*,*,#43334,.T.);
#63703=ORIENTED_EDGE('',*,*,#43333,.T.);
#63704=ORIENTED_EDGE('',*,*,#43630,.F.);
#63705=ORIENTED_EDGE('',*,*,#43337,.T.);
#63706=ORIENTED_EDGE('',*,*,#43335,.T.);
#63707=ORIENTED_EDGE('',*,*,#43629,.T.);
#63708=ORIENTED_EDGE('',*,*,#43631,.F.);
#63709=ORIENTED_EDGE('',*,*,#43632,.F.);
#63710=ORIENTED_EDGE('',*,*,#43341,.T.);
#63711=ORIENTED_EDGE('',*,*,#43340,.T.);
#63712=ORIENTED_EDGE('',*,*,#43633,.F.);
#63713=ORIENTED_EDGE('',*,*,#43344,.T.);
#63714=ORIENTED_EDGE('',*,*,#43342,.T.);
#63715=ORIENTED_EDGE('',*,*,#43632,.T.);
#63716=ORIENTED_EDGE('',*,*,#43634,.F.);
#63717=ORIENTED_EDGE('',*,*,#43635,.F.);
#63718=ORIENTED_EDGE('',*,*,#43348,.T.);
#63719=ORIENTED_EDGE('',*,*,#43347,.T.);
#63720=ORIENTED_EDGE('',*,*,#43636,.F.);
#63721=ORIENTED_EDGE('',*,*,#43351,.T.);
#63722=ORIENTED_EDGE('',*,*,#43349,.T.);
#63723=ORIENTED_EDGE('',*,*,#43635,.T.);
#63724=ORIENTED_EDGE('',*,*,#43637,.F.);
#63725=ORIENTED_EDGE('',*,*,#43638,.F.);
#63726=ORIENTED_EDGE('',*,*,#43355,.T.);
#63727=ORIENTED_EDGE('',*,*,#43354,.T.);
#63728=ORIENTED_EDGE('',*,*,#43639,.F.);
#63729=ORIENTED_EDGE('',*,*,#43358,.T.);
#63730=ORIENTED_EDGE('',*,*,#43356,.T.);
#63731=ORIENTED_EDGE('',*,*,#43638,.T.);
#63732=ORIENTED_EDGE('',*,*,#43640,.F.);
#63733=ORIENTED_EDGE('',*,*,#43641,.F.);
#63734=ORIENTED_EDGE('',*,*,#43362,.T.);
#63735=ORIENTED_EDGE('',*,*,#43361,.T.);
#63736=ORIENTED_EDGE('',*,*,#43642,.F.);
#63737=ORIENTED_EDGE('',*,*,#43365,.T.);
#63738=ORIENTED_EDGE('',*,*,#43363,.T.);
#63739=ORIENTED_EDGE('',*,*,#43641,.T.);
#63740=ORIENTED_EDGE('',*,*,#43643,.F.);
#63741=ORIENTED_EDGE('',*,*,#43644,.F.);
#63742=ORIENTED_EDGE('',*,*,#43369,.T.);
#63743=ORIENTED_EDGE('',*,*,#43368,.T.);
#63744=ORIENTED_EDGE('',*,*,#43645,.F.);
#63745=ORIENTED_EDGE('',*,*,#43372,.T.);
#63746=ORIENTED_EDGE('',*,*,#43370,.T.);
#63747=ORIENTED_EDGE('',*,*,#43644,.T.);
#63748=ORIENTED_EDGE('',*,*,#43646,.F.);
#63749=ORIENTED_EDGE('',*,*,#43647,.F.);
#63750=ORIENTED_EDGE('',*,*,#43376,.T.);
#63751=ORIENTED_EDGE('',*,*,#43375,.T.);
#63752=ORIENTED_EDGE('',*,*,#43648,.F.);
#63753=ORIENTED_EDGE('',*,*,#43379,.T.);
#63754=ORIENTED_EDGE('',*,*,#43377,.T.);
#63755=ORIENTED_EDGE('',*,*,#43647,.T.);
#63756=ORIENTED_EDGE('',*,*,#43649,.F.);
#63757=ORIENTED_EDGE('',*,*,#43650,.F.);
#63758=ORIENTED_EDGE('',*,*,#43383,.T.);
#63759=ORIENTED_EDGE('',*,*,#43382,.T.);
#63760=ORIENTED_EDGE('',*,*,#43651,.F.);
#63761=ORIENTED_EDGE('',*,*,#43386,.T.);
#63762=ORIENTED_EDGE('',*,*,#43384,.T.);
#63763=ORIENTED_EDGE('',*,*,#43650,.T.);
#63764=ORIENTED_EDGE('',*,*,#43652,.F.);
#63765=ORIENTED_EDGE('',*,*,#43653,.F.);
#63766=ORIENTED_EDGE('',*,*,#43390,.T.);
#63767=ORIENTED_EDGE('',*,*,#43389,.T.);
#63768=ORIENTED_EDGE('',*,*,#43654,.F.);
#63769=ORIENTED_EDGE('',*,*,#43393,.T.);
#63770=ORIENTED_EDGE('',*,*,#43391,.T.);
#63771=ORIENTED_EDGE('',*,*,#43653,.T.);
#63772=ORIENTED_EDGE('',*,*,#43655,.T.);
#63773=ORIENTED_EDGE('',*,*,#43656,.F.);
#63774=ORIENTED_EDGE('',*,*,#43568,.T.);
#63775=ORIENTED_EDGE('',*,*,#43657,.F.);
#63776=ORIENTED_EDGE('',*,*,#43658,.T.);
#63777=ORIENTED_EDGE('',*,*,#43659,.F.);
#63778=ORIENTED_EDGE('',*,*,#43570,.T.);
#63779=ORIENTED_EDGE('',*,*,#43660,.F.);
#63780=ORIENTED_EDGE('',*,*,#43661,.F.);
#63781=ORIENTED_EDGE('',*,*,#43662,.T.);
#63782=ORIENTED_EDGE('',*,*,#43663,.F.);
#63783=ORIENTED_EDGE('',*,*,#43664,.T.);
#63784=ORIENTED_EDGE('',*,*,#43665,.F.);
#63785=ORIENTED_EDGE('',*,*,#43571,.T.);
#63786=ORIENTED_EDGE('',*,*,#43659,.T.);
#63787=ORIENTED_EDGE('',*,*,#43666,.F.);
#63788=ORIENTED_EDGE('',*,*,#43664,.F.);
#63789=ORIENTED_EDGE('',*,*,#43658,.F.);
#63790=ORIENTED_EDGE('',*,*,#43667,.F.);
#63791=ORIENTED_EDGE('',*,*,#43662,.F.);
#63792=ORIENTED_EDGE('',*,*,#43668,.T.);
#63793=ORIENTED_EDGE('',*,*,#43669,.F.);
#63794=ORIENTED_EDGE('',*,*,#43573,.T.);
#63795=ORIENTED_EDGE('',*,*,#43670,.F.);
#63796=ORIENTED_EDGE('',*,*,#43671,.F.);
#63797=ORIENTED_EDGE('',*,*,#43672,.T.);
#63798=ORIENTED_EDGE('',*,*,#43673,.F.);
#63799=ORIENTED_EDGE('',*,*,#43674,.T.);
#63800=ORIENTED_EDGE('',*,*,#43675,.F.);
#63801=ORIENTED_EDGE('',*,*,#43574,.T.);
#63802=ORIENTED_EDGE('',*,*,#43669,.T.);
#63803=ORIENTED_EDGE('',*,*,#43676,.F.);
#63804=ORIENTED_EDGE('',*,*,#43674,.F.);
#63805=ORIENTED_EDGE('',*,*,#43668,.F.);
#63806=ORIENTED_EDGE('',*,*,#43677,.F.);
#63807=ORIENTED_EDGE('',*,*,#43672,.F.);
#63808=ORIENTED_EDGE('',*,*,#43678,.T.);
#63809=ORIENTED_EDGE('',*,*,#43679,.F.);
#63810=ORIENTED_EDGE('',*,*,#43576,.T.);
#63811=ORIENTED_EDGE('',*,*,#43680,.F.);
#63812=ORIENTED_EDGE('',*,*,#43681,.F.);
#63813=ORIENTED_EDGE('',*,*,#43682,.T.);
#63814=ORIENTED_EDGE('',*,*,#43683,.F.);
#63815=ORIENTED_EDGE('',*,*,#43684,.T.);
#63816=ORIENTED_EDGE('',*,*,#43685,.F.);
#63817=ORIENTED_EDGE('',*,*,#43577,.T.);
#63818=ORIENTED_EDGE('',*,*,#43679,.T.);
#63819=ORIENTED_EDGE('',*,*,#43686,.F.);
#63820=ORIENTED_EDGE('',*,*,#43684,.F.);
#63821=ORIENTED_EDGE('',*,*,#43678,.F.);
#63822=ORIENTED_EDGE('',*,*,#43687,.F.);
#63823=ORIENTED_EDGE('',*,*,#43682,.F.);
#63824=ORIENTED_EDGE('',*,*,#43688,.T.);
#63825=ORIENTED_EDGE('',*,*,#43689,.F.);
#63826=ORIENTED_EDGE('',*,*,#43579,.T.);
#63827=ORIENTED_EDGE('',*,*,#43690,.F.);
#63828=ORIENTED_EDGE('',*,*,#43691,.F.);
#63829=ORIENTED_EDGE('',*,*,#43692,.T.);
#63830=ORIENTED_EDGE('',*,*,#43693,.F.);
#63831=ORIENTED_EDGE('',*,*,#43694,.T.);
#63832=ORIENTED_EDGE('',*,*,#43695,.F.);
#63833=ORIENTED_EDGE('',*,*,#43580,.T.);
#63834=ORIENTED_EDGE('',*,*,#43689,.T.);
#63835=ORIENTED_EDGE('',*,*,#43696,.F.);
#63836=ORIENTED_EDGE('',*,*,#43694,.F.);
#63837=ORIENTED_EDGE('',*,*,#43688,.F.);
#63838=ORIENTED_EDGE('',*,*,#43697,.F.);
#63839=ORIENTED_EDGE('',*,*,#43692,.F.);
#63840=ORIENTED_EDGE('',*,*,#43698,.T.);
#63841=ORIENTED_EDGE('',*,*,#43699,.F.);
#63842=ORIENTED_EDGE('',*,*,#43582,.T.);
#63843=ORIENTED_EDGE('',*,*,#43700,.F.);
#63844=ORIENTED_EDGE('',*,*,#43701,.F.);
#63845=ORIENTED_EDGE('',*,*,#43702,.T.);
#63846=ORIENTED_EDGE('',*,*,#43703,.F.);
#63847=ORIENTED_EDGE('',*,*,#43704,.T.);
#63848=ORIENTED_EDGE('',*,*,#43705,.F.);
#63849=ORIENTED_EDGE('',*,*,#43583,.T.);
#63850=ORIENTED_EDGE('',*,*,#43699,.T.);
#63851=ORIENTED_EDGE('',*,*,#43706,.F.);
#63852=ORIENTED_EDGE('',*,*,#43704,.F.);
#63853=ORIENTED_EDGE('',*,*,#43698,.F.);
#63854=ORIENTED_EDGE('',*,*,#43707,.F.);
#63855=ORIENTED_EDGE('',*,*,#43702,.F.);
#63856=ORIENTED_EDGE('',*,*,#43708,.T.);
#63857=ORIENTED_EDGE('',*,*,#43709,.F.);
#63858=ORIENTED_EDGE('',*,*,#43585,.T.);
#63859=ORIENTED_EDGE('',*,*,#43710,.F.);
#63860=ORIENTED_EDGE('',*,*,#43711,.F.);
#63861=ORIENTED_EDGE('',*,*,#43712,.T.);
#63862=ORIENTED_EDGE('',*,*,#43713,.F.);
#63863=ORIENTED_EDGE('',*,*,#43714,.T.);
#63864=ORIENTED_EDGE('',*,*,#43715,.F.);
#63865=ORIENTED_EDGE('',*,*,#43586,.T.);
#63866=ORIENTED_EDGE('',*,*,#43709,.T.);
#63867=ORIENTED_EDGE('',*,*,#43716,.F.);
#63868=ORIENTED_EDGE('',*,*,#43714,.F.);
#63869=ORIENTED_EDGE('',*,*,#43708,.F.);
#63870=ORIENTED_EDGE('',*,*,#43717,.F.);
#63871=ORIENTED_EDGE('',*,*,#43712,.F.);
#63872=ORIENTED_EDGE('',*,*,#34342,.T.);
#63873=ORIENTED_EDGE('',*,*,#43718,.F.);
#63874=ORIENTED_EDGE('',*,*,#43588,.T.);
#63875=ORIENTED_EDGE('',*,*,#43719,.F.);
#63876=ORIENTED_EDGE('',*,*,#43720,.F.);
#63877=ORIENTED_EDGE('',*,*,#34344,.T.);
#63878=ORIENTED_EDGE('',*,*,#43721,.F.);
#63879=ORIENTED_EDGE('',*,*,#34341,.T.);
#63880=ORIENTED_EDGE('',*,*,#43722,.F.);
#63881=ORIENTED_EDGE('',*,*,#43589,.T.);
#63882=ORIENTED_EDGE('',*,*,#43718,.T.);
#63883=ORIENTED_EDGE('',*,*,#43723,.T.);
#63884=ORIENTED_EDGE('',*,*,#43724,.F.);
#63885=ORIENTED_EDGE('',*,*,#43591,.T.);
#63886=ORIENTED_EDGE('',*,*,#43725,.F.);
#63887=ORIENTED_EDGE('',*,*,#43726,.F.);
#63888=ORIENTED_EDGE('',*,*,#43727,.T.);
#63889=ORIENTED_EDGE('',*,*,#43728,.F.);
#63890=ORIENTED_EDGE('',*,*,#43729,.T.);
#63891=ORIENTED_EDGE('',*,*,#43730,.F.);
#63892=ORIENTED_EDGE('',*,*,#43592,.T.);
#63893=ORIENTED_EDGE('',*,*,#43724,.T.);
#63894=ORIENTED_EDGE('',*,*,#43731,.F.);
#63895=ORIENTED_EDGE('',*,*,#43729,.F.);
#63896=ORIENTED_EDGE('',*,*,#43723,.F.);
#63897=ORIENTED_EDGE('',*,*,#43732,.F.);
#63898=ORIENTED_EDGE('',*,*,#43727,.F.);
#63899=ORIENTED_EDGE('',*,*,#43733,.T.);
#63900=ORIENTED_EDGE('',*,*,#43734,.F.);
#63901=ORIENTED_EDGE('',*,*,#43594,.T.);
#63902=ORIENTED_EDGE('',*,*,#43735,.F.);
#63903=ORIENTED_EDGE('',*,*,#43736,.F.);
#63904=ORIENTED_EDGE('',*,*,#43737,.T.);
#63905=ORIENTED_EDGE('',*,*,#43738,.F.);
#63906=ORIENTED_EDGE('',*,*,#43739,.T.);
#63907=ORIENTED_EDGE('',*,*,#43740,.F.);
#63908=ORIENTED_EDGE('',*,*,#43595,.T.);
#63909=ORIENTED_EDGE('',*,*,#43734,.T.);
#63910=ORIENTED_EDGE('',*,*,#43741,.F.);
#63911=ORIENTED_EDGE('',*,*,#43739,.F.);
#63912=ORIENTED_EDGE('',*,*,#43733,.F.);
#63913=ORIENTED_EDGE('',*,*,#43742,.F.);
#63914=ORIENTED_EDGE('',*,*,#43737,.F.);
#63915=ORIENTED_EDGE('',*,*,#43743,.T.);
#63916=ORIENTED_EDGE('',*,*,#43744,.F.);
#63917=ORIENTED_EDGE('',*,*,#43597,.T.);
#63918=ORIENTED_EDGE('',*,*,#43745,.F.);
#63919=ORIENTED_EDGE('',*,*,#43746,.F.);
#63920=ORIENTED_EDGE('',*,*,#43747,.T.);
#63921=ORIENTED_EDGE('',*,*,#43748,.F.);
#63922=ORIENTED_EDGE('',*,*,#43749,.T.);
#63923=ORIENTED_EDGE('',*,*,#43750,.F.);
#63924=ORIENTED_EDGE('',*,*,#43598,.T.);
#63925=ORIENTED_EDGE('',*,*,#43744,.T.);
#63926=ORIENTED_EDGE('',*,*,#43751,.F.);
#63927=ORIENTED_EDGE('',*,*,#43749,.F.);
#63928=ORIENTED_EDGE('',*,*,#43743,.F.);
#63929=ORIENTED_EDGE('',*,*,#43752,.F.);
#63930=ORIENTED_EDGE('',*,*,#43747,.F.);
#63931=ORIENTED_EDGE('',*,*,#43753,.T.);
#63932=ORIENTED_EDGE('',*,*,#43754,.F.);
#63933=ORIENTED_EDGE('',*,*,#43600,.T.);
#63934=ORIENTED_EDGE('',*,*,#43755,.F.);
#63935=ORIENTED_EDGE('',*,*,#43756,.F.);
#63936=ORIENTED_EDGE('',*,*,#43757,.T.);
#63937=ORIENTED_EDGE('',*,*,#43758,.F.);
#63938=ORIENTED_EDGE('',*,*,#43759,.T.);
#63939=ORIENTED_EDGE('',*,*,#43760,.F.);
#63940=ORIENTED_EDGE('',*,*,#43601,.T.);
#63941=ORIENTED_EDGE('',*,*,#43754,.T.);
#63942=ORIENTED_EDGE('',*,*,#43761,.F.);
#63943=ORIENTED_EDGE('',*,*,#43759,.F.);
#63944=ORIENTED_EDGE('',*,*,#43753,.F.);
#63945=ORIENTED_EDGE('',*,*,#43762,.F.);
#63946=ORIENTED_EDGE('',*,*,#43757,.F.);
#63947=ORIENTED_EDGE('',*,*,#43763,.T.);
#63948=ORIENTED_EDGE('',*,*,#43764,.F.);
#63949=ORIENTED_EDGE('',*,*,#43603,.T.);
#63950=ORIENTED_EDGE('',*,*,#43765,.F.);
#63951=ORIENTED_EDGE('',*,*,#43766,.F.);
#63952=ORIENTED_EDGE('',*,*,#43767,.T.);
#63953=ORIENTED_EDGE('',*,*,#43768,.F.);
#63954=ORIENTED_EDGE('',*,*,#43769,.T.);
#63955=ORIENTED_EDGE('',*,*,#43770,.F.);
#63956=ORIENTED_EDGE('',*,*,#43604,.T.);
#63957=ORIENTED_EDGE('',*,*,#43764,.T.);
#63958=ORIENTED_EDGE('',*,*,#43771,.F.);
#63959=ORIENTED_EDGE('',*,*,#43769,.F.);
#63960=ORIENTED_EDGE('',*,*,#43763,.F.);
#63961=ORIENTED_EDGE('',*,*,#43772,.F.);
#63962=ORIENTED_EDGE('',*,*,#43767,.F.);
#63963=ORIENTED_EDGE('',*,*,#43773,.T.);
#63964=ORIENTED_EDGE('',*,*,#43774,.F.);
#63965=ORIENTED_EDGE('',*,*,#43606,.T.);
#63966=ORIENTED_EDGE('',*,*,#43775,.F.);
#63967=ORIENTED_EDGE('',*,*,#43776,.F.);
#63968=ORIENTED_EDGE('',*,*,#43777,.T.);
#63969=ORIENTED_EDGE('',*,*,#43778,.F.);
#63970=ORIENTED_EDGE('',*,*,#43779,.T.);
#63971=ORIENTED_EDGE('',*,*,#43780,.F.);
#63972=ORIENTED_EDGE('',*,*,#43607,.T.);
#63973=ORIENTED_EDGE('',*,*,#43774,.T.);
#63974=ORIENTED_EDGE('',*,*,#43781,.F.);
#63975=ORIENTED_EDGE('',*,*,#43779,.F.);
#63976=ORIENTED_EDGE('',*,*,#43773,.F.);
#63977=ORIENTED_EDGE('',*,*,#43782,.F.);
#63978=ORIENTED_EDGE('',*,*,#43777,.F.);
#63979=ORIENTED_EDGE('',*,*,#43783,.T.);
#63980=ORIENTED_EDGE('',*,*,#43784,.F.);
#63981=ORIENTED_EDGE('',*,*,#43609,.T.);
#63982=ORIENTED_EDGE('',*,*,#43785,.F.);
#63983=ORIENTED_EDGE('',*,*,#43786,.F.);
#63984=ORIENTED_EDGE('',*,*,#43787,.T.);
#63985=ORIENTED_EDGE('',*,*,#43788,.F.);
#63986=ORIENTED_EDGE('',*,*,#43789,.T.);
#63987=ORIENTED_EDGE('',*,*,#43790,.F.);
#63988=ORIENTED_EDGE('',*,*,#43610,.T.);
#63989=ORIENTED_EDGE('',*,*,#43784,.T.);
#63990=ORIENTED_EDGE('',*,*,#43791,.F.);
#63991=ORIENTED_EDGE('',*,*,#43789,.F.);
#63992=ORIENTED_EDGE('',*,*,#43783,.F.);
#63993=ORIENTED_EDGE('',*,*,#43792,.F.);
#63994=ORIENTED_EDGE('',*,*,#43787,.F.);
#63995=ORIENTED_EDGE('',*,*,#43793,.T.);
#63996=ORIENTED_EDGE('',*,*,#43794,.F.);
#63997=ORIENTED_EDGE('',*,*,#43612,.T.);
#63998=ORIENTED_EDGE('',*,*,#43795,.F.);
#63999=ORIENTED_EDGE('',*,*,#43796,.F.);
#64000=ORIENTED_EDGE('',*,*,#43797,.T.);
#64001=ORIENTED_EDGE('',*,*,#43798,.F.);
#64002=ORIENTED_EDGE('',*,*,#43799,.T.);
#64003=ORIENTED_EDGE('',*,*,#43800,.F.);
#64004=ORIENTED_EDGE('',*,*,#43613,.T.);
#64005=ORIENTED_EDGE('',*,*,#43794,.T.);
#64006=ORIENTED_EDGE('',*,*,#43801,.F.);
#64007=ORIENTED_EDGE('',*,*,#43799,.F.);
#64008=ORIENTED_EDGE('',*,*,#43793,.F.);
#64009=ORIENTED_EDGE('',*,*,#43802,.F.);
#64010=ORIENTED_EDGE('',*,*,#43797,.F.);
#64011=ORIENTED_EDGE('',*,*,#43803,.T.);
#64012=ORIENTED_EDGE('',*,*,#43804,.F.);
#64013=ORIENTED_EDGE('',*,*,#43615,.T.);
#64014=ORIENTED_EDGE('',*,*,#43805,.F.);
#64015=ORIENTED_EDGE('',*,*,#43806,.F.);
#64016=ORIENTED_EDGE('',*,*,#43807,.T.);
#64017=ORIENTED_EDGE('',*,*,#43808,.F.);
#64018=ORIENTED_EDGE('',*,*,#43809,.T.);
#64019=ORIENTED_EDGE('',*,*,#43810,.F.);
#64020=ORIENTED_EDGE('',*,*,#43616,.T.);
#64021=ORIENTED_EDGE('',*,*,#43804,.T.);
#64022=ORIENTED_EDGE('',*,*,#43811,.F.);
#64023=ORIENTED_EDGE('',*,*,#43809,.F.);
#64024=ORIENTED_EDGE('',*,*,#43803,.F.);
#64025=ORIENTED_EDGE('',*,*,#43812,.F.);
#64026=ORIENTED_EDGE('',*,*,#43807,.F.);
#64027=ORIENTED_EDGE('',*,*,#43813,.T.);
#64028=ORIENTED_EDGE('',*,*,#43814,.F.);
#64029=ORIENTED_EDGE('',*,*,#43618,.T.);
#64030=ORIENTED_EDGE('',*,*,#43815,.F.);
#64031=ORIENTED_EDGE('',*,*,#43816,.F.);
#64032=ORIENTED_EDGE('',*,*,#43817,.T.);
#64033=ORIENTED_EDGE('',*,*,#43818,.F.);
#64034=ORIENTED_EDGE('',*,*,#43819,.T.);
#64035=ORIENTED_EDGE('',*,*,#43820,.F.);
#64036=ORIENTED_EDGE('',*,*,#43619,.T.);
#64037=ORIENTED_EDGE('',*,*,#43814,.T.);
#64038=ORIENTED_EDGE('',*,*,#43821,.F.);
#64039=ORIENTED_EDGE('',*,*,#43819,.F.);
#64040=ORIENTED_EDGE('',*,*,#43813,.F.);
#64041=ORIENTED_EDGE('',*,*,#43822,.F.);
#64042=ORIENTED_EDGE('',*,*,#43817,.F.);
#64043=ORIENTED_EDGE('',*,*,#43621,.T.);
#64044=ORIENTED_EDGE('',*,*,#43823,.F.);
#64045=ORIENTED_EDGE('',*,*,#43824,.T.);
#64046=ORIENTED_EDGE('',*,*,#43825,.F.);
#64047=ORIENTED_EDGE('',*,*,#43826,.F.);
#64048=ORIENTED_EDGE('',*,*,#43827,.T.);
#64049=ORIENTED_EDGE('',*,*,#43828,.F.);
#64050=ORIENTED_EDGE('',*,*,#43622,.T.);
#64051=ORIENTED_EDGE('',*,*,#43825,.T.);
#64052=ORIENTED_EDGE('',*,*,#43829,.T.);
#64053=ORIENTED_EDGE('',*,*,#43830,.F.);
#64054=ORIENTED_EDGE('',*,*,#43831,.F.);
#64055=ORIENTED_EDGE('',*,*,#43829,.F.);
#64056=ORIENTED_EDGE('',*,*,#43824,.F.);
#64057=ORIENTED_EDGE('',*,*,#43832,.F.);
#64058=ORIENTED_EDGE('',*,*,#43827,.F.);
#64059=ORIENTED_EDGE('',*,*,#43833,.T.);
#64060=ORIENTED_EDGE('',*,*,#43834,.F.);
#64061=ORIENTED_EDGE('',*,*,#43624,.T.);
#64062=ORIENTED_EDGE('',*,*,#43835,.F.);
#64063=ORIENTED_EDGE('',*,*,#43836,.F.);
#64064=ORIENTED_EDGE('',*,*,#43837,.T.);
#64065=ORIENTED_EDGE('',*,*,#43838,.F.);
#64066=ORIENTED_EDGE('',*,*,#43839,.T.);
#64067=ORIENTED_EDGE('',*,*,#43840,.F.);
#64068=ORIENTED_EDGE('',*,*,#43625,.T.);
#64069=ORIENTED_EDGE('',*,*,#43834,.T.);
#64070=ORIENTED_EDGE('',*,*,#43841,.F.);
#64071=ORIENTED_EDGE('',*,*,#43839,.F.);
#64072=ORIENTED_EDGE('',*,*,#43833,.F.);
#64073=ORIENTED_EDGE('',*,*,#43842,.F.);
#64074=ORIENTED_EDGE('',*,*,#43837,.F.);
#64075=ORIENTED_EDGE('',*,*,#43843,.T.);
#64076=ORIENTED_EDGE('',*,*,#43844,.F.);
#64077=ORIENTED_EDGE('',*,*,#43627,.T.);
#64078=ORIENTED_EDGE('',*,*,#43845,.F.);
#64079=ORIENTED_EDGE('',*,*,#43846,.F.);
#64080=ORIENTED_EDGE('',*,*,#43847,.T.);
#64081=ORIENTED_EDGE('',*,*,#43848,.F.);
#64082=ORIENTED_EDGE('',*,*,#43849,.T.);
#64083=ORIENTED_EDGE('',*,*,#43850,.F.);
#64084=ORIENTED_EDGE('',*,*,#43628,.T.);
#64085=ORIENTED_EDGE('',*,*,#43844,.T.);
#64086=ORIENTED_EDGE('',*,*,#43851,.F.);
#64087=ORIENTED_EDGE('',*,*,#43849,.F.);
#64088=ORIENTED_EDGE('',*,*,#43843,.F.);
#64089=ORIENTED_EDGE('',*,*,#43852,.F.);
#64090=ORIENTED_EDGE('',*,*,#43847,.F.);
#64091=ORIENTED_EDGE('',*,*,#43853,.T.);
#64092=ORIENTED_EDGE('',*,*,#43854,.F.);
#64093=ORIENTED_EDGE('',*,*,#43630,.T.);
#64094=ORIENTED_EDGE('',*,*,#43855,.F.);
#64095=ORIENTED_EDGE('',*,*,#43856,.F.);
#64096=ORIENTED_EDGE('',*,*,#43857,.T.);
#64097=ORIENTED_EDGE('',*,*,#43858,.F.);
#64098=ORIENTED_EDGE('',*,*,#43859,.T.);
#64099=ORIENTED_EDGE('',*,*,#43860,.F.);
#64100=ORIENTED_EDGE('',*,*,#43631,.T.);
#64101=ORIENTED_EDGE('',*,*,#43854,.T.);
#64102=ORIENTED_EDGE('',*,*,#43861,.F.);
#64103=ORIENTED_EDGE('',*,*,#43859,.F.);
#64104=ORIENTED_EDGE('',*,*,#43853,.F.);
#64105=ORIENTED_EDGE('',*,*,#43862,.F.);
#64106=ORIENTED_EDGE('',*,*,#43857,.F.);
#64107=ORIENTED_EDGE('',*,*,#43863,.T.);
#64108=ORIENTED_EDGE('',*,*,#43864,.F.);
#64109=ORIENTED_EDGE('',*,*,#43633,.T.);
#64110=ORIENTED_EDGE('',*,*,#43865,.F.);
#64111=ORIENTED_EDGE('',*,*,#43866,.F.);
#64112=ORIENTED_EDGE('',*,*,#43867,.T.);
#64113=ORIENTED_EDGE('',*,*,#43868,.F.);
#64114=ORIENTED_EDGE('',*,*,#43869,.T.);
#64115=ORIENTED_EDGE('',*,*,#43870,.F.);
#64116=ORIENTED_EDGE('',*,*,#43634,.T.);
#64117=ORIENTED_EDGE('',*,*,#43864,.T.);
#64118=ORIENTED_EDGE('',*,*,#43871,.F.);
#64119=ORIENTED_EDGE('',*,*,#43869,.F.);
#64120=ORIENTED_EDGE('',*,*,#43863,.F.);
#64121=ORIENTED_EDGE('',*,*,#43872,.F.);
#64122=ORIENTED_EDGE('',*,*,#43867,.F.);
#64123=ORIENTED_EDGE('',*,*,#43873,.T.);
#64124=ORIENTED_EDGE('',*,*,#43874,.F.);
#64125=ORIENTED_EDGE('',*,*,#43636,.T.);
#64126=ORIENTED_EDGE('',*,*,#43875,.F.);
#64127=ORIENTED_EDGE('',*,*,#43876,.F.);
#64128=ORIENTED_EDGE('',*,*,#43877,.T.);
#64129=ORIENTED_EDGE('',*,*,#43878,.F.);
#64130=ORIENTED_EDGE('',*,*,#43879,.T.);
#64131=ORIENTED_EDGE('',*,*,#43880,.F.);
#64132=ORIENTED_EDGE('',*,*,#43637,.T.);
#64133=ORIENTED_EDGE('',*,*,#43874,.T.);
#64134=ORIENTED_EDGE('',*,*,#43881,.F.);
#64135=ORIENTED_EDGE('',*,*,#43879,.F.);
#64136=ORIENTED_EDGE('',*,*,#43873,.F.);
#64137=ORIENTED_EDGE('',*,*,#43882,.F.);
#64138=ORIENTED_EDGE('',*,*,#43877,.F.);
#64139=ORIENTED_EDGE('',*,*,#43883,.T.);
#64140=ORIENTED_EDGE('',*,*,#43884,.F.);
#64141=ORIENTED_EDGE('',*,*,#43639,.T.);
#64142=ORIENTED_EDGE('',*,*,#43885,.F.);
#64143=ORIENTED_EDGE('',*,*,#43886,.F.);
#64144=ORIENTED_EDGE('',*,*,#43887,.T.);
#64145=ORIENTED_EDGE('',*,*,#43888,.F.);
#64146=ORIENTED_EDGE('',*,*,#43889,.T.);
#64147=ORIENTED_EDGE('',*,*,#43890,.F.);
#64148=ORIENTED_EDGE('',*,*,#43640,.T.);
#64149=ORIENTED_EDGE('',*,*,#43884,.T.);
#64150=ORIENTED_EDGE('',*,*,#43891,.F.);
#64151=ORIENTED_EDGE('',*,*,#43889,.F.);
#64152=ORIENTED_EDGE('',*,*,#43883,.F.);
#64153=ORIENTED_EDGE('',*,*,#43892,.F.);
#64154=ORIENTED_EDGE('',*,*,#43887,.F.);
#64155=ORIENTED_EDGE('',*,*,#43893,.T.);
#64156=ORIENTED_EDGE('',*,*,#43894,.F.);
#64157=ORIENTED_EDGE('',*,*,#43642,.T.);
#64158=ORIENTED_EDGE('',*,*,#43895,.F.);
#64159=ORIENTED_EDGE('',*,*,#43896,.F.);
#64160=ORIENTED_EDGE('',*,*,#43897,.T.);
#64161=ORIENTED_EDGE('',*,*,#43898,.F.);
#64162=ORIENTED_EDGE('',*,*,#43899,.T.);
#64163=ORIENTED_EDGE('',*,*,#43900,.F.);
#64164=ORIENTED_EDGE('',*,*,#43643,.T.);
#64165=ORIENTED_EDGE('',*,*,#43894,.T.);
#64166=ORIENTED_EDGE('',*,*,#43901,.F.);
#64167=ORIENTED_EDGE('',*,*,#43899,.F.);
#64168=ORIENTED_EDGE('',*,*,#43893,.F.);
#64169=ORIENTED_EDGE('',*,*,#43902,.F.);
#64170=ORIENTED_EDGE('',*,*,#43897,.F.);
#64171=ORIENTED_EDGE('',*,*,#43903,.T.);
#64172=ORIENTED_EDGE('',*,*,#43904,.F.);
#64173=ORIENTED_EDGE('',*,*,#43645,.T.);
#64174=ORIENTED_EDGE('',*,*,#43905,.F.);
#64175=ORIENTED_EDGE('',*,*,#43906,.F.);
#64176=ORIENTED_EDGE('',*,*,#43907,.T.);
#64177=ORIENTED_EDGE('',*,*,#43908,.F.);
#64178=ORIENTED_EDGE('',*,*,#43909,.T.);
#64179=ORIENTED_EDGE('',*,*,#43910,.F.);
#64180=ORIENTED_EDGE('',*,*,#43646,.T.);
#64181=ORIENTED_EDGE('',*,*,#43904,.T.);
#64182=ORIENTED_EDGE('',*,*,#43911,.F.);
#64183=ORIENTED_EDGE('',*,*,#43909,.F.);
#64184=ORIENTED_EDGE('',*,*,#43903,.F.);
#64185=ORIENTED_EDGE('',*,*,#43912,.F.);
#64186=ORIENTED_EDGE('',*,*,#43907,.F.);
#64187=ORIENTED_EDGE('',*,*,#43913,.T.);
#64188=ORIENTED_EDGE('',*,*,#43914,.F.);
#64189=ORIENTED_EDGE('',*,*,#43648,.T.);
#64190=ORIENTED_EDGE('',*,*,#43915,.F.);
#64191=ORIENTED_EDGE('',*,*,#43916,.F.);
#64192=ORIENTED_EDGE('',*,*,#43917,.T.);
#64193=ORIENTED_EDGE('',*,*,#43918,.F.);
#64194=ORIENTED_EDGE('',*,*,#43919,.T.);
#64195=ORIENTED_EDGE('',*,*,#43920,.F.);
#64196=ORIENTED_EDGE('',*,*,#43649,.T.);
#64197=ORIENTED_EDGE('',*,*,#43914,.T.);
#64198=ORIENTED_EDGE('',*,*,#43921,.F.);
#64199=ORIENTED_EDGE('',*,*,#43919,.F.);
#64200=ORIENTED_EDGE('',*,*,#43913,.F.);
#64201=ORIENTED_EDGE('',*,*,#43922,.F.);
#64202=ORIENTED_EDGE('',*,*,#43917,.F.);
#64203=ORIENTED_EDGE('',*,*,#43923,.T.);
#64204=ORIENTED_EDGE('',*,*,#43924,.F.);
#64205=ORIENTED_EDGE('',*,*,#43651,.T.);
#64206=ORIENTED_EDGE('',*,*,#43925,.F.);
#64207=ORIENTED_EDGE('',*,*,#43926,.F.);
#64208=ORIENTED_EDGE('',*,*,#43927,.T.);
#64209=ORIENTED_EDGE('',*,*,#43928,.F.);
#64210=ORIENTED_EDGE('',*,*,#43929,.T.);
#64211=ORIENTED_EDGE('',*,*,#43930,.F.);
#64212=ORIENTED_EDGE('',*,*,#43652,.T.);
#64213=ORIENTED_EDGE('',*,*,#43924,.T.);
#64214=ORIENTED_EDGE('',*,*,#43931,.F.);
#64215=ORIENTED_EDGE('',*,*,#43929,.F.);
#64216=ORIENTED_EDGE('',*,*,#43923,.F.);
#64217=ORIENTED_EDGE('',*,*,#43932,.F.);
#64218=ORIENTED_EDGE('',*,*,#43927,.F.);
#64219=ORIENTED_EDGE('',*,*,#43933,.F.);
#64220=ORIENTED_EDGE('',*,*,#43934,.T.);
#64221=ORIENTED_EDGE('',*,*,#43935,.F.);
#64222=ORIENTED_EDGE('',*,*,#43936,.F.);
#64223=ORIENTED_EDGE('',*,*,#43655,.F.);
#64224=ORIENTED_EDGE('',*,*,#43937,.F.);
#64225=ORIENTED_EDGE('',*,*,#43938,.F.);
#64226=ORIENTED_EDGE('',*,*,#43934,.F.);
#64227=ORIENTED_EDGE('',*,*,#43937,.T.);
#64228=ORIENTED_EDGE('',*,*,#43657,.T.);
#64229=ORIENTED_EDGE('',*,*,#43654,.T.);
#64230=ORIENTED_EDGE('',*,*,#43939,.F.);
#64231=ORIENTED_EDGE('',*,*,#34245,.T.);
#64232=ORIENTED_EDGE('',*,*,#34155,.F.);
#64233=ORIENTED_EDGE('',*,*,#43656,.T.);
#64234=ORIENTED_EDGE('',*,*,#43936,.T.);
#64235=ORIENTED_EDGE('',*,*,#43933,.T.);
#64236=ORIENTED_EDGE('',*,*,#43940,.F.);
#64237=ORIENTED_EDGE('',*,*,#43941,.F.);
#64238=ORIENTED_EDGE('',*,*,#43942,.F.);
#64239=ORIENTED_EDGE('',*,*,#43943,.F.);
#64240=ORIENTED_EDGE('',*,*,#43663,.T.);
#64241=ORIENTED_EDGE('',*,*,#43667,.T.);
#64242=ORIENTED_EDGE('',*,*,#43660,.T.);
#64243=ORIENTED_EDGE('',*,*,#43665,.T.);
#64244=ORIENTED_EDGE('',*,*,#43666,.T.);
#64245=ORIENTED_EDGE('',*,*,#43661,.T.);
#64246=ORIENTED_EDGE('',*,*,#43943,.T.);
#64247=ORIENTED_EDGE('',*,*,#43944,.F.);
#64248=ORIENTED_EDGE('',*,*,#43945,.F.);
#64249=ORIENTED_EDGE('',*,*,#43946,.F.);
#64250=ORIENTED_EDGE('',*,*,#43673,.T.);
#64251=ORIENTED_EDGE('',*,*,#43677,.T.);
#64252=ORIENTED_EDGE('',*,*,#43670,.T.);
#64253=ORIENTED_EDGE('',*,*,#43675,.T.);
#64254=ORIENTED_EDGE('',*,*,#43676,.T.);
#64255=ORIENTED_EDGE('',*,*,#43671,.T.);
#64256=ORIENTED_EDGE('',*,*,#43946,.T.);
#64257=ORIENTED_EDGE('',*,*,#43947,.F.);
#64258=ORIENTED_EDGE('',*,*,#43948,.F.);
#64259=ORIENTED_EDGE('',*,*,#43949,.F.);
#64260=ORIENTED_EDGE('',*,*,#43683,.T.);
#64261=ORIENTED_EDGE('',*,*,#43687,.T.);
#64262=ORIENTED_EDGE('',*,*,#43680,.T.);
#64263=ORIENTED_EDGE('',*,*,#43685,.T.);
#64264=ORIENTED_EDGE('',*,*,#43686,.T.);
#64265=ORIENTED_EDGE('',*,*,#43681,.T.);
#64266=ORIENTED_EDGE('',*,*,#43949,.T.);
#64267=ORIENTED_EDGE('',*,*,#43950,.F.);
#64268=ORIENTED_EDGE('',*,*,#43951,.F.);
#64269=ORIENTED_EDGE('',*,*,#43952,.F.);
#64270=ORIENTED_EDGE('',*,*,#43693,.T.);
#64271=ORIENTED_EDGE('',*,*,#43697,.T.);
#64272=ORIENTED_EDGE('',*,*,#43690,.T.);
#64273=ORIENTED_EDGE('',*,*,#43695,.T.);
#64274=ORIENTED_EDGE('',*,*,#43696,.T.);
#64275=ORIENTED_EDGE('',*,*,#43691,.T.);
#64276=ORIENTED_EDGE('',*,*,#43952,.T.);
#64277=ORIENTED_EDGE('',*,*,#43953,.F.);
#64278=ORIENTED_EDGE('',*,*,#43954,.F.);
#64279=ORIENTED_EDGE('',*,*,#43955,.F.);
#64280=ORIENTED_EDGE('',*,*,#43703,.T.);
#64281=ORIENTED_EDGE('',*,*,#43707,.T.);
#64282=ORIENTED_EDGE('',*,*,#43700,.T.);
#64283=ORIENTED_EDGE('',*,*,#43705,.T.);
#64284=ORIENTED_EDGE('',*,*,#43706,.T.);
#64285=ORIENTED_EDGE('',*,*,#43701,.T.);
#64286=ORIENTED_EDGE('',*,*,#43955,.T.);
#64287=ORIENTED_EDGE('',*,*,#43956,.F.);
#64288=ORIENTED_EDGE('',*,*,#43957,.F.);
#64289=ORIENTED_EDGE('',*,*,#43958,.F.);
#64290=ORIENTED_EDGE('',*,*,#43713,.T.);
#64291=ORIENTED_EDGE('',*,*,#43717,.T.);
#64292=ORIENTED_EDGE('',*,*,#43710,.T.);
#64293=ORIENTED_EDGE('',*,*,#43715,.T.);
#64294=ORIENTED_EDGE('',*,*,#43716,.T.);
#64295=ORIENTED_EDGE('',*,*,#43711,.T.);
#64296=ORIENTED_EDGE('',*,*,#43958,.T.);
#64297=ORIENTED_EDGE('',*,*,#43959,.F.);
#64298=ORIENTED_EDGE('',*,*,#43960,.F.);
#64299=ORIENTED_EDGE('',*,*,#43961,.F.);
#64300=ORIENTED_EDGE('',*,*,#43721,.T.);
#64301=ORIENTED_EDGE('',*,*,#34343,.T.);
#64302=ORIENTED_EDGE('',*,*,#43719,.T.);
#64303=ORIENTED_EDGE('',*,*,#43722,.T.);
#64304=ORIENTED_EDGE('',*,*,#34345,.T.);
#64305=ORIENTED_EDGE('',*,*,#43720,.T.);
#64306=ORIENTED_EDGE('',*,*,#43961,.T.);
#64307=ORIENTED_EDGE('',*,*,#43962,.F.);
#64308=ORIENTED_EDGE('',*,*,#43963,.F.);
#64309=ORIENTED_EDGE('',*,*,#43964,.F.);
#64310=ORIENTED_EDGE('',*,*,#43728,.T.);
#64311=ORIENTED_EDGE('',*,*,#43732,.T.);
#64312=ORIENTED_EDGE('',*,*,#43725,.T.);
#64313=ORIENTED_EDGE('',*,*,#43730,.T.);
#64314=ORIENTED_EDGE('',*,*,#43731,.T.);
#64315=ORIENTED_EDGE('',*,*,#43726,.T.);
#64316=ORIENTED_EDGE('',*,*,#43964,.T.);
#64317=ORIENTED_EDGE('',*,*,#43965,.F.);
#64318=ORIENTED_EDGE('',*,*,#43966,.F.);
#64319=ORIENTED_EDGE('',*,*,#43967,.F.);
#64320=ORIENTED_EDGE('',*,*,#43738,.T.);
#64321=ORIENTED_EDGE('',*,*,#43742,.T.);
#64322=ORIENTED_EDGE('',*,*,#43735,.T.);
#64323=ORIENTED_EDGE('',*,*,#43740,.T.);
#64324=ORIENTED_EDGE('',*,*,#43741,.T.);
#64325=ORIENTED_EDGE('',*,*,#43736,.T.);
#64326=ORIENTED_EDGE('',*,*,#43967,.T.);
#64327=ORIENTED_EDGE('',*,*,#43968,.F.);
#64328=ORIENTED_EDGE('',*,*,#43969,.F.);
#64329=ORIENTED_EDGE('',*,*,#43970,.F.);
#64330=ORIENTED_EDGE('',*,*,#43748,.T.);
#64331=ORIENTED_EDGE('',*,*,#43752,.T.);
#64332=ORIENTED_EDGE('',*,*,#43745,.T.);
#64333=ORIENTED_EDGE('',*,*,#43750,.T.);
#64334=ORIENTED_EDGE('',*,*,#43751,.T.);
#64335=ORIENTED_EDGE('',*,*,#43746,.T.);
#64336=ORIENTED_EDGE('',*,*,#43970,.T.);
#64337=ORIENTED_EDGE('',*,*,#43971,.F.);
#64338=ORIENTED_EDGE('',*,*,#43972,.F.);
#64339=ORIENTED_EDGE('',*,*,#43973,.F.);
#64340=ORIENTED_EDGE('',*,*,#43758,.T.);
#64341=ORIENTED_EDGE('',*,*,#43762,.T.);
#64342=ORIENTED_EDGE('',*,*,#43755,.T.);
#64343=ORIENTED_EDGE('',*,*,#43760,.T.);
#64344=ORIENTED_EDGE('',*,*,#43761,.T.);
#64345=ORIENTED_EDGE('',*,*,#43756,.T.);
#64346=ORIENTED_EDGE('',*,*,#43973,.T.);
#64347=ORIENTED_EDGE('',*,*,#43974,.F.);
#64348=ORIENTED_EDGE('',*,*,#43975,.F.);
#64349=ORIENTED_EDGE('',*,*,#43976,.F.);
#64350=ORIENTED_EDGE('',*,*,#43768,.T.);
#64351=ORIENTED_EDGE('',*,*,#43772,.T.);
#64352=ORIENTED_EDGE('',*,*,#43765,.T.);
#64353=ORIENTED_EDGE('',*,*,#43770,.T.);
#64354=ORIENTED_EDGE('',*,*,#43771,.T.);
#64355=ORIENTED_EDGE('',*,*,#43766,.T.);
#64356=ORIENTED_EDGE('',*,*,#43976,.T.);
#64357=ORIENTED_EDGE('',*,*,#43977,.F.);
#64358=ORIENTED_EDGE('',*,*,#43978,.F.);
#64359=ORIENTED_EDGE('',*,*,#43979,.F.);
#64360=ORIENTED_EDGE('',*,*,#43778,.T.);
#64361=ORIENTED_EDGE('',*,*,#43782,.T.);
#64362=ORIENTED_EDGE('',*,*,#43775,.T.);
#64363=ORIENTED_EDGE('',*,*,#43780,.T.);
#64364=ORIENTED_EDGE('',*,*,#43781,.T.);
#64365=ORIENTED_EDGE('',*,*,#43776,.T.);
#64366=ORIENTED_EDGE('',*,*,#43979,.T.);
#64367=ORIENTED_EDGE('',*,*,#43980,.F.);
#64368=ORIENTED_EDGE('',*,*,#43981,.F.);
#64369=ORIENTED_EDGE('',*,*,#43982,.F.);
#64370=ORIENTED_EDGE('',*,*,#43788,.T.);
#64371=ORIENTED_EDGE('',*,*,#43792,.T.);
#64372=ORIENTED_EDGE('',*,*,#43785,.T.);
#64373=ORIENTED_EDGE('',*,*,#43790,.T.);
#64374=ORIENTED_EDGE('',*,*,#43791,.T.);
#64375=ORIENTED_EDGE('',*,*,#43786,.T.);
#64376=ORIENTED_EDGE('',*,*,#43982,.T.);
#64377=ORIENTED_EDGE('',*,*,#43983,.F.);
#64378=ORIENTED_EDGE('',*,*,#43984,.F.);
#64379=ORIENTED_EDGE('',*,*,#43985,.F.);
#64380=ORIENTED_EDGE('',*,*,#43798,.T.);
#64381=ORIENTED_EDGE('',*,*,#43802,.T.);
#64382=ORIENTED_EDGE('',*,*,#43795,.T.);
#64383=ORIENTED_EDGE('',*,*,#43800,.T.);
#64384=ORIENTED_EDGE('',*,*,#43801,.T.);
#64385=ORIENTED_EDGE('',*,*,#43796,.T.);
#64386=ORIENTED_EDGE('',*,*,#43985,.T.);
#64387=ORIENTED_EDGE('',*,*,#43986,.F.);
#64388=ORIENTED_EDGE('',*,*,#43987,.F.);
#64389=ORIENTED_EDGE('',*,*,#43988,.F.);
#64390=ORIENTED_EDGE('',*,*,#43808,.T.);
#64391=ORIENTED_EDGE('',*,*,#43812,.T.);
#64392=ORIENTED_EDGE('',*,*,#43805,.T.);
#64393=ORIENTED_EDGE('',*,*,#43810,.T.);
#64394=ORIENTED_EDGE('',*,*,#43811,.T.);
#64395=ORIENTED_EDGE('',*,*,#43806,.T.);
#64396=ORIENTED_EDGE('',*,*,#43988,.T.);
#64397=ORIENTED_EDGE('',*,*,#43989,.F.);
#64398=ORIENTED_EDGE('',*,*,#43990,.F.);
#64399=ORIENTED_EDGE('',*,*,#43991,.F.);
#64400=ORIENTED_EDGE('',*,*,#43818,.T.);
#64401=ORIENTED_EDGE('',*,*,#43822,.T.);
#64402=ORIENTED_EDGE('',*,*,#43815,.T.);
#64403=ORIENTED_EDGE('',*,*,#43820,.T.);
#64404=ORIENTED_EDGE('',*,*,#43821,.T.);
#64405=ORIENTED_EDGE('',*,*,#43816,.T.);
#64406=ORIENTED_EDGE('',*,*,#43991,.T.);
#64407=ORIENTED_EDGE('',*,*,#43992,.F.);
#64408=ORIENTED_EDGE('',*,*,#43993,.F.);
#64409=ORIENTED_EDGE('',*,*,#43994,.F.);
#64410=ORIENTED_EDGE('',*,*,#43828,.T.);
#64411=ORIENTED_EDGE('',*,*,#43832,.T.);
#64412=ORIENTED_EDGE('',*,*,#43823,.T.);
#64413=ORIENTED_EDGE('',*,*,#43830,.T.);
#64414=ORIENTED_EDGE('',*,*,#43831,.T.);
#64415=ORIENTED_EDGE('',*,*,#43826,.T.);
#64416=ORIENTED_EDGE('',*,*,#43994,.T.);
#64417=ORIENTED_EDGE('',*,*,#43995,.F.);
#64418=ORIENTED_EDGE('',*,*,#43996,.F.);
#64419=ORIENTED_EDGE('',*,*,#43997,.F.);
#64420=ORIENTED_EDGE('',*,*,#43838,.T.);
#64421=ORIENTED_EDGE('',*,*,#43842,.T.);
#64422=ORIENTED_EDGE('',*,*,#43835,.T.);
#64423=ORIENTED_EDGE('',*,*,#43840,.T.);
#64424=ORIENTED_EDGE('',*,*,#43841,.T.);
#64425=ORIENTED_EDGE('',*,*,#43836,.T.);
#64426=ORIENTED_EDGE('',*,*,#43997,.T.);
#64427=ORIENTED_EDGE('',*,*,#43998,.F.);
#64428=ORIENTED_EDGE('',*,*,#43999,.F.);
#64429=ORIENTED_EDGE('',*,*,#44000,.F.);
#64430=ORIENTED_EDGE('',*,*,#43848,.T.);
#64431=ORIENTED_EDGE('',*,*,#43852,.T.);
#64432=ORIENTED_EDGE('',*,*,#43845,.T.);
#64433=ORIENTED_EDGE('',*,*,#43850,.T.);
#64434=ORIENTED_EDGE('',*,*,#43851,.T.);
#64435=ORIENTED_EDGE('',*,*,#43846,.T.);
#64436=ORIENTED_EDGE('',*,*,#44000,.T.);
#64437=ORIENTED_EDGE('',*,*,#44001,.F.);
#64438=ORIENTED_EDGE('',*,*,#44002,.F.);
#64439=ORIENTED_EDGE('',*,*,#44003,.F.);
#64440=ORIENTED_EDGE('',*,*,#43858,.T.);
#64441=ORIENTED_EDGE('',*,*,#43862,.T.);
#64442=ORIENTED_EDGE('',*,*,#43855,.T.);
#64443=ORIENTED_EDGE('',*,*,#43860,.T.);
#64444=ORIENTED_EDGE('',*,*,#43861,.T.);
#64445=ORIENTED_EDGE('',*,*,#43856,.T.);
#64446=ORIENTED_EDGE('',*,*,#44003,.T.);
#64447=ORIENTED_EDGE('',*,*,#44004,.F.);
#64448=ORIENTED_EDGE('',*,*,#44005,.F.);
#64449=ORIENTED_EDGE('',*,*,#44006,.F.);
#64450=ORIENTED_EDGE('',*,*,#43868,.T.);
#64451=ORIENTED_EDGE('',*,*,#43872,.T.);
#64452=ORIENTED_EDGE('',*,*,#43865,.T.);
#64453=ORIENTED_EDGE('',*,*,#43870,.T.);
#64454=ORIENTED_EDGE('',*,*,#43871,.T.);
#64455=ORIENTED_EDGE('',*,*,#43866,.T.);
#64456=ORIENTED_EDGE('',*,*,#44006,.T.);
#64457=ORIENTED_EDGE('',*,*,#44007,.F.);
#64458=ORIENTED_EDGE('',*,*,#44008,.F.);
#64459=ORIENTED_EDGE('',*,*,#44009,.F.);
#64460=ORIENTED_EDGE('',*,*,#43878,.T.);
#64461=ORIENTED_EDGE('',*,*,#43882,.T.);
#64462=ORIENTED_EDGE('',*,*,#43875,.T.);
#64463=ORIENTED_EDGE('',*,*,#43880,.T.);
#64464=ORIENTED_EDGE('',*,*,#43881,.T.);
#64465=ORIENTED_EDGE('',*,*,#43876,.T.);
#64466=ORIENTED_EDGE('',*,*,#44009,.T.);
#64467=ORIENTED_EDGE('',*,*,#44010,.F.);
#64468=ORIENTED_EDGE('',*,*,#44011,.F.);
#64469=ORIENTED_EDGE('',*,*,#44012,.F.);
#64470=ORIENTED_EDGE('',*,*,#43888,.T.);
#64471=ORIENTED_EDGE('',*,*,#43892,.T.);
#64472=ORIENTED_EDGE('',*,*,#43885,.T.);
#64473=ORIENTED_EDGE('',*,*,#43890,.T.);
#64474=ORIENTED_EDGE('',*,*,#43891,.T.);
#64475=ORIENTED_EDGE('',*,*,#43886,.T.);
#64476=ORIENTED_EDGE('',*,*,#44012,.T.);
#64477=ORIENTED_EDGE('',*,*,#44013,.F.);
#64478=ORIENTED_EDGE('',*,*,#44014,.F.);
#64479=ORIENTED_EDGE('',*,*,#44015,.F.);
#64480=ORIENTED_EDGE('',*,*,#43898,.T.);
#64481=ORIENTED_EDGE('',*,*,#43902,.T.);
#64482=ORIENTED_EDGE('',*,*,#43895,.T.);
#64483=ORIENTED_EDGE('',*,*,#43900,.T.);
#64484=ORIENTED_EDGE('',*,*,#43901,.T.);
#64485=ORIENTED_EDGE('',*,*,#43896,.T.);
#64486=ORIENTED_EDGE('',*,*,#44015,.T.);
#64487=ORIENTED_EDGE('',*,*,#44016,.F.);
#64488=ORIENTED_EDGE('',*,*,#44017,.F.);
#64489=ORIENTED_EDGE('',*,*,#44018,.F.);
#64490=ORIENTED_EDGE('',*,*,#43908,.T.);
#64491=ORIENTED_EDGE('',*,*,#43912,.T.);
#64492=ORIENTED_EDGE('',*,*,#43905,.T.);
#64493=ORIENTED_EDGE('',*,*,#43910,.T.);
#64494=ORIENTED_EDGE('',*,*,#43911,.T.);
#64495=ORIENTED_EDGE('',*,*,#43906,.T.);
#64496=ORIENTED_EDGE('',*,*,#44018,.T.);
#64497=ORIENTED_EDGE('',*,*,#44019,.F.);
#64498=ORIENTED_EDGE('',*,*,#44020,.F.);
#64499=ORIENTED_EDGE('',*,*,#44021,.F.);
#64500=ORIENTED_EDGE('',*,*,#43918,.T.);
#64501=ORIENTED_EDGE('',*,*,#43922,.T.);
#64502=ORIENTED_EDGE('',*,*,#43915,.T.);
#64503=ORIENTED_EDGE('',*,*,#43920,.T.);
#64504=ORIENTED_EDGE('',*,*,#43921,.T.);
#64505=ORIENTED_EDGE('',*,*,#43916,.T.);
#64506=ORIENTED_EDGE('',*,*,#44021,.T.);
#64507=ORIENTED_EDGE('',*,*,#44022,.F.);
#64508=ORIENTED_EDGE('',*,*,#44023,.F.);
#64509=ORIENTED_EDGE('',*,*,#44024,.F.);
#64510=ORIENTED_EDGE('',*,*,#43928,.T.);
#64511=ORIENTED_EDGE('',*,*,#43932,.T.);
#64512=ORIENTED_EDGE('',*,*,#43925,.T.);
#64513=ORIENTED_EDGE('',*,*,#43930,.T.);
#64514=ORIENTED_EDGE('',*,*,#43931,.T.);
#64515=ORIENTED_EDGE('',*,*,#43926,.T.);
#64516=ORIENTED_EDGE('',*,*,#44024,.T.);
#64517=ORIENTED_EDGE('',*,*,#44025,.F.);
#64518=ORIENTED_EDGE('',*,*,#44026,.F.);
#64519=ORIENTED_EDGE('',*,*,#43940,.T.);
#64520=ORIENTED_EDGE('',*,*,#43935,.T.);
#64521=ORIENTED_EDGE('',*,*,#43938,.T.);
#64522=ORIENTED_EDGE('',*,*,#43939,.T.);
#64523=ORIENTED_EDGE('',*,*,#43941,.T.);
#64524=ORIENTED_EDGE('',*,*,#44027,.F.);
#64525=ORIENTED_EDGE('',*,*,#44028,.T.);
#64526=ORIENTED_EDGE('',*,*,#44029,.F.);
#64527=ORIENTED_EDGE('',*,*,#44030,.F.);
#64528=ORIENTED_EDGE('',*,*,#44031,.F.);
#64529=ORIENTED_EDGE('',*,*,#44028,.F.);
#64530=ORIENTED_EDGE('',*,*,#44032,.F.);
#64531=ORIENTED_EDGE('',*,*,#44029,.T.);
#64532=ORIENTED_EDGE('',*,*,#44031,.T.);
#64533=ORIENTED_EDGE('',*,*,#44033,.F.);
#64534=ORIENTED_EDGE('',*,*,#43942,.T.);
#64535=ORIENTED_EDGE('',*,*,#43944,.T.);
#64536=ORIENTED_EDGE('',*,*,#44034,.F.);
#64537=ORIENTED_EDGE('',*,*,#44035,.T.);
#64538=ORIENTED_EDGE('',*,*,#44036,.F.);
#64539=ORIENTED_EDGE('',*,*,#44037,.F.);
#64540=ORIENTED_EDGE('',*,*,#44038,.F.);
#64541=ORIENTED_EDGE('',*,*,#44035,.F.);
#64542=ORIENTED_EDGE('',*,*,#44039,.F.);
#64543=ORIENTED_EDGE('',*,*,#44036,.T.);
#64544=ORIENTED_EDGE('',*,*,#44038,.T.);
#64545=ORIENTED_EDGE('',*,*,#44040,.F.);
#64546=ORIENTED_EDGE('',*,*,#43945,.T.);
#64547=ORIENTED_EDGE('',*,*,#43947,.T.);
#64548=ORIENTED_EDGE('',*,*,#44041,.F.);
#64549=ORIENTED_EDGE('',*,*,#44042,.T.);
#64550=ORIENTED_EDGE('',*,*,#44043,.F.);
#64551=ORIENTED_EDGE('',*,*,#44044,.F.);
#64552=ORIENTED_EDGE('',*,*,#44045,.F.);
#64553=ORIENTED_EDGE('',*,*,#44042,.F.);
#64554=ORIENTED_EDGE('',*,*,#44046,.F.);
#64555=ORIENTED_EDGE('',*,*,#44043,.T.);
#64556=ORIENTED_EDGE('',*,*,#44045,.T.);
#64557=ORIENTED_EDGE('',*,*,#44047,.F.);
#64558=ORIENTED_EDGE('',*,*,#43948,.T.);
#64559=ORIENTED_EDGE('',*,*,#43950,.T.);
#64560=ORIENTED_EDGE('',*,*,#44048,.F.);
#64561=ORIENTED_EDGE('',*,*,#44049,.T.);
#64562=ORIENTED_EDGE('',*,*,#44050,.F.);
#64563=ORIENTED_EDGE('',*,*,#44051,.F.);
#64564=ORIENTED_EDGE('',*,*,#44052,.F.);
#64565=ORIENTED_EDGE('',*,*,#44049,.F.);
#64566=ORIENTED_EDGE('',*,*,#44053,.F.);
#64567=ORIENTED_EDGE('',*,*,#44050,.T.);
#64568=ORIENTED_EDGE('',*,*,#44052,.T.);
#64569=ORIENTED_EDGE('',*,*,#44054,.F.);
#64570=ORIENTED_EDGE('',*,*,#43951,.T.);
#64571=ORIENTED_EDGE('',*,*,#43953,.T.);
#64572=ORIENTED_EDGE('',*,*,#44055,.F.);
#64573=ORIENTED_EDGE('',*,*,#44056,.T.);
#64574=ORIENTED_EDGE('',*,*,#44057,.F.);
#64575=ORIENTED_EDGE('',*,*,#44058,.F.);
#64576=ORIENTED_EDGE('',*,*,#44059,.F.);
#64577=ORIENTED_EDGE('',*,*,#44056,.F.);
#64578=ORIENTED_EDGE('',*,*,#44060,.F.);
#64579=ORIENTED_EDGE('',*,*,#44057,.T.);
#64580=ORIENTED_EDGE('',*,*,#44059,.T.);
#64581=ORIENTED_EDGE('',*,*,#44061,.F.);
#64582=ORIENTED_EDGE('',*,*,#43954,.T.);
#64583=ORIENTED_EDGE('',*,*,#43956,.T.);
#64584=ORIENTED_EDGE('',*,*,#44062,.F.);
#64585=ORIENTED_EDGE('',*,*,#44063,.T.);
#64586=ORIENTED_EDGE('',*,*,#44064,.F.);
#64587=ORIENTED_EDGE('',*,*,#44065,.F.);
#64588=ORIENTED_EDGE('',*,*,#44066,.F.);
#64589=ORIENTED_EDGE('',*,*,#44063,.F.);
#64590=ORIENTED_EDGE('',*,*,#44067,.F.);
#64591=ORIENTED_EDGE('',*,*,#44064,.T.);
#64592=ORIENTED_EDGE('',*,*,#44066,.T.);
#64593=ORIENTED_EDGE('',*,*,#44068,.F.);
#64594=ORIENTED_EDGE('',*,*,#43957,.T.);
#64595=ORIENTED_EDGE('',*,*,#43959,.T.);
#64596=ORIENTED_EDGE('',*,*,#44069,.F.);
#64597=ORIENTED_EDGE('',*,*,#44070,.T.);
#64598=ORIENTED_EDGE('',*,*,#44071,.F.);
#64599=ORIENTED_EDGE('',*,*,#44072,.F.);
#64600=ORIENTED_EDGE('',*,*,#44073,.F.);
#64601=ORIENTED_EDGE('',*,*,#44070,.F.);
#64602=ORIENTED_EDGE('',*,*,#44074,.F.);
#64603=ORIENTED_EDGE('',*,*,#44071,.T.);
#64604=ORIENTED_EDGE('',*,*,#44073,.T.);
#64605=ORIENTED_EDGE('',*,*,#44075,.F.);
#64606=ORIENTED_EDGE('',*,*,#43960,.T.);
#64607=ORIENTED_EDGE('',*,*,#43962,.T.);
#64608=ORIENTED_EDGE('',*,*,#44076,.F.);
#64609=ORIENTED_EDGE('',*,*,#44077,.T.);
#64610=ORIENTED_EDGE('',*,*,#44078,.F.);
#64611=ORIENTED_EDGE('',*,*,#44079,.F.);
#64612=ORIENTED_EDGE('',*,*,#44080,.F.);
#64613=ORIENTED_EDGE('',*,*,#44077,.F.);
#64614=ORIENTED_EDGE('',*,*,#44081,.F.);
#64615=ORIENTED_EDGE('',*,*,#44078,.T.);
#64616=ORIENTED_EDGE('',*,*,#44080,.T.);
#64617=ORIENTED_EDGE('',*,*,#44082,.F.);
#64618=ORIENTED_EDGE('',*,*,#43963,.T.);
#64619=ORIENTED_EDGE('',*,*,#43965,.T.);
#64620=ORIENTED_EDGE('',*,*,#44083,.F.);
#64621=ORIENTED_EDGE('',*,*,#44084,.T.);
#64622=ORIENTED_EDGE('',*,*,#44085,.F.);
#64623=ORIENTED_EDGE('',*,*,#44086,.F.);
#64624=ORIENTED_EDGE('',*,*,#44087,.F.);
#64625=ORIENTED_EDGE('',*,*,#44084,.F.);
#64626=ORIENTED_EDGE('',*,*,#44088,.F.);
#64627=ORIENTED_EDGE('',*,*,#44085,.T.);
#64628=ORIENTED_EDGE('',*,*,#44087,.T.);
#64629=ORIENTED_EDGE('',*,*,#44089,.F.);
#64630=ORIENTED_EDGE('',*,*,#43966,.T.);
#64631=ORIENTED_EDGE('',*,*,#43968,.T.);
#64632=ORIENTED_EDGE('',*,*,#44090,.F.);
#64633=ORIENTED_EDGE('',*,*,#44091,.T.);
#64634=ORIENTED_EDGE('',*,*,#44092,.F.);
#64635=ORIENTED_EDGE('',*,*,#44093,.F.);
#64636=ORIENTED_EDGE('',*,*,#44094,.F.);
#64637=ORIENTED_EDGE('',*,*,#44091,.F.);
#64638=ORIENTED_EDGE('',*,*,#44095,.F.);
#64639=ORIENTED_EDGE('',*,*,#44092,.T.);
#64640=ORIENTED_EDGE('',*,*,#44094,.T.);
#64641=ORIENTED_EDGE('',*,*,#44096,.F.);
#64642=ORIENTED_EDGE('',*,*,#43969,.T.);
#64643=ORIENTED_EDGE('',*,*,#43971,.T.);
#64644=ORIENTED_EDGE('',*,*,#44097,.F.);
#64645=ORIENTED_EDGE('',*,*,#44098,.T.);
#64646=ORIENTED_EDGE('',*,*,#44099,.F.);
#64647=ORIENTED_EDGE('',*,*,#44100,.F.);
#64648=ORIENTED_EDGE('',*,*,#44101,.F.);
#64649=ORIENTED_EDGE('',*,*,#44098,.F.);
#64650=ORIENTED_EDGE('',*,*,#44102,.F.);
#64651=ORIENTED_EDGE('',*,*,#44099,.T.);
#64652=ORIENTED_EDGE('',*,*,#44101,.T.);
#64653=ORIENTED_EDGE('',*,*,#44103,.F.);
#64654=ORIENTED_EDGE('',*,*,#43972,.T.);
#64655=ORIENTED_EDGE('',*,*,#43974,.T.);
#64656=ORIENTED_EDGE('',*,*,#44104,.F.);
#64657=ORIENTED_EDGE('',*,*,#44105,.T.);
#64658=ORIENTED_EDGE('',*,*,#44106,.F.);
#64659=ORIENTED_EDGE('',*,*,#44107,.F.);
#64660=ORIENTED_EDGE('',*,*,#44108,.F.);
#64661=ORIENTED_EDGE('',*,*,#44105,.F.);
#64662=ORIENTED_EDGE('',*,*,#44109,.F.);
#64663=ORIENTED_EDGE('',*,*,#44106,.T.);
#64664=ORIENTED_EDGE('',*,*,#44108,.T.);
#64665=ORIENTED_EDGE('',*,*,#44110,.F.);
#64666=ORIENTED_EDGE('',*,*,#43975,.T.);
#64667=ORIENTED_EDGE('',*,*,#43977,.T.);
#64668=ORIENTED_EDGE('',*,*,#44111,.F.);
#64669=ORIENTED_EDGE('',*,*,#44112,.T.);
#64670=ORIENTED_EDGE('',*,*,#44113,.F.);
#64671=ORIENTED_EDGE('',*,*,#44114,.F.);
#64672=ORIENTED_EDGE('',*,*,#44115,.F.);
#64673=ORIENTED_EDGE('',*,*,#44112,.F.);
#64674=ORIENTED_EDGE('',*,*,#44116,.F.);
#64675=ORIENTED_EDGE('',*,*,#44113,.T.);
#64676=ORIENTED_EDGE('',*,*,#44115,.T.);
#64677=ORIENTED_EDGE('',*,*,#44117,.F.);
#64678=ORIENTED_EDGE('',*,*,#43978,.T.);
#64679=ORIENTED_EDGE('',*,*,#43980,.T.);
#64680=ORIENTED_EDGE('',*,*,#44118,.F.);
#64681=ORIENTED_EDGE('',*,*,#44119,.T.);
#64682=ORIENTED_EDGE('',*,*,#44120,.F.);
#64683=ORIENTED_EDGE('',*,*,#44121,.F.);
#64684=ORIENTED_EDGE('',*,*,#44122,.F.);
#64685=ORIENTED_EDGE('',*,*,#44119,.F.);
#64686=ORIENTED_EDGE('',*,*,#44123,.F.);
#64687=ORIENTED_EDGE('',*,*,#44120,.T.);
#64688=ORIENTED_EDGE('',*,*,#44122,.T.);
#64689=ORIENTED_EDGE('',*,*,#44124,.F.);
#64690=ORIENTED_EDGE('',*,*,#43981,.T.);
#64691=ORIENTED_EDGE('',*,*,#43983,.T.);
#64692=ORIENTED_EDGE('',*,*,#44125,.F.);
#64693=ORIENTED_EDGE('',*,*,#44126,.T.);
#64694=ORIENTED_EDGE('',*,*,#44127,.F.);
#64695=ORIENTED_EDGE('',*,*,#44128,.F.);
#64696=ORIENTED_EDGE('',*,*,#44129,.F.);
#64697=ORIENTED_EDGE('',*,*,#44126,.F.);
#64698=ORIENTED_EDGE('',*,*,#44130,.F.);
#64699=ORIENTED_EDGE('',*,*,#44127,.T.);
#64700=ORIENTED_EDGE('',*,*,#44129,.T.);
#64701=ORIENTED_EDGE('',*,*,#44131,.F.);
#64702=ORIENTED_EDGE('',*,*,#43984,.T.);
#64703=ORIENTED_EDGE('',*,*,#43986,.T.);
#64704=ORIENTED_EDGE('',*,*,#44132,.F.);
#64705=ORIENTED_EDGE('',*,*,#44133,.T.);
#64706=ORIENTED_EDGE('',*,*,#44134,.F.);
#64707=ORIENTED_EDGE('',*,*,#44135,.F.);
#64708=ORIENTED_EDGE('',*,*,#44136,.F.);
#64709=ORIENTED_EDGE('',*,*,#44133,.F.);
#64710=ORIENTED_EDGE('',*,*,#44137,.F.);
#64711=ORIENTED_EDGE('',*,*,#44134,.T.);
#64712=ORIENTED_EDGE('',*,*,#44136,.T.);
#64713=ORIENTED_EDGE('',*,*,#44138,.F.);
#64714=ORIENTED_EDGE('',*,*,#43987,.T.);
#64715=ORIENTED_EDGE('',*,*,#43989,.T.);
#64716=ORIENTED_EDGE('',*,*,#44139,.F.);
#64717=ORIENTED_EDGE('',*,*,#44140,.T.);
#64718=ORIENTED_EDGE('',*,*,#44141,.F.);
#64719=ORIENTED_EDGE('',*,*,#44142,.F.);
#64720=ORIENTED_EDGE('',*,*,#44143,.F.);
#64721=ORIENTED_EDGE('',*,*,#44140,.F.);
#64722=ORIENTED_EDGE('',*,*,#44144,.F.);
#64723=ORIENTED_EDGE('',*,*,#44141,.T.);
#64724=ORIENTED_EDGE('',*,*,#44143,.T.);
#64725=ORIENTED_EDGE('',*,*,#44145,.F.);
#64726=ORIENTED_EDGE('',*,*,#43990,.T.);
#64727=ORIENTED_EDGE('',*,*,#43992,.T.);
#64728=ORIENTED_EDGE('',*,*,#44146,.F.);
#64729=ORIENTED_EDGE('',*,*,#44147,.T.);
#64730=ORIENTED_EDGE('',*,*,#44148,.F.);
#64731=ORIENTED_EDGE('',*,*,#44147,.F.);
#64732=ORIENTED_EDGE('',*,*,#44149,.F.);
#64733=ORIENTED_EDGE('',*,*,#44150,.F.);
#64734=ORIENTED_EDGE('',*,*,#44151,.F.);
#64735=ORIENTED_EDGE('',*,*,#44148,.T.);
#64736=ORIENTED_EDGE('',*,*,#44151,.T.);
#64737=ORIENTED_EDGE('',*,*,#44152,.F.);
#64738=ORIENTED_EDGE('',*,*,#43993,.T.);
#64739=ORIENTED_EDGE('',*,*,#43995,.T.);
#64740=ORIENTED_EDGE('',*,*,#44153,.F.);
#64741=ORIENTED_EDGE('',*,*,#44154,.T.);
#64742=ORIENTED_EDGE('',*,*,#44155,.F.);
#64743=ORIENTED_EDGE('',*,*,#44156,.F.);
#64744=ORIENTED_EDGE('',*,*,#44157,.F.);
#64745=ORIENTED_EDGE('',*,*,#44154,.F.);
#64746=ORIENTED_EDGE('',*,*,#44158,.F.);
#64747=ORIENTED_EDGE('',*,*,#44155,.T.);
#64748=ORIENTED_EDGE('',*,*,#44157,.T.);
#64749=ORIENTED_EDGE('',*,*,#44159,.F.);
#64750=ORIENTED_EDGE('',*,*,#43996,.T.);
#64751=ORIENTED_EDGE('',*,*,#43998,.T.);
#64752=ORIENTED_EDGE('',*,*,#44160,.F.);
#64753=ORIENTED_EDGE('',*,*,#44161,.T.);
#64754=ORIENTED_EDGE('',*,*,#44162,.F.);
#64755=ORIENTED_EDGE('',*,*,#44163,.F.);
#64756=ORIENTED_EDGE('',*,*,#44164,.F.);
#64757=ORIENTED_EDGE('',*,*,#44161,.F.);
#64758=ORIENTED_EDGE('',*,*,#44165,.F.);
#64759=ORIENTED_EDGE('',*,*,#44162,.T.);
#64760=ORIENTED_EDGE('',*,*,#44164,.T.);
#64761=ORIENTED_EDGE('',*,*,#44166,.F.);
#64762=ORIENTED_EDGE('',*,*,#43999,.T.);
#64763=ORIENTED_EDGE('',*,*,#44001,.T.);
#64764=ORIENTED_EDGE('',*,*,#44167,.F.);
#64765=ORIENTED_EDGE('',*,*,#44168,.T.);
#64766=ORIENTED_EDGE('',*,*,#44169,.F.);
#64767=ORIENTED_EDGE('',*,*,#44170,.F.);
#64768=ORIENTED_EDGE('',*,*,#44171,.F.);
#64769=ORIENTED_EDGE('',*,*,#44168,.F.);
#64770=ORIENTED_EDGE('',*,*,#44172,.F.);
#64771=ORIENTED_EDGE('',*,*,#44169,.T.);
#64772=ORIENTED_EDGE('',*,*,#44171,.T.);
#64773=ORIENTED_EDGE('',*,*,#44173,.F.);
#64774=ORIENTED_EDGE('',*,*,#44002,.T.);
#64775=ORIENTED_EDGE('',*,*,#44004,.T.);
#64776=ORIENTED_EDGE('',*,*,#44174,.F.);
#64777=ORIENTED_EDGE('',*,*,#34339,.T.);
#64778=ORIENTED_EDGE('',*,*,#44175,.F.);
#64779=ORIENTED_EDGE('',*,*,#44175,.T.);
#64780=ORIENTED_EDGE('',*,*,#34338,.T.);
#64781=ORIENTED_EDGE('',*,*,#44176,.F.);
#64782=ORIENTED_EDGE('',*,*,#44005,.T.);
#64783=ORIENTED_EDGE('',*,*,#44007,.T.);
#64784=ORIENTED_EDGE('',*,*,#44177,.F.);
#64785=ORIENTED_EDGE('',*,*,#44178,.T.);
#64786=ORIENTED_EDGE('',*,*,#44179,.F.);
#64787=ORIENTED_EDGE('',*,*,#44180,.F.);
#64788=ORIENTED_EDGE('',*,*,#44181,.F.);
#64789=ORIENTED_EDGE('',*,*,#44178,.F.);
#64790=ORIENTED_EDGE('',*,*,#44182,.F.);
#64791=ORIENTED_EDGE('',*,*,#44179,.T.);
#64792=ORIENTED_EDGE('',*,*,#44181,.T.);
#64793=ORIENTED_EDGE('',*,*,#44183,.F.);
#64794=ORIENTED_EDGE('',*,*,#44008,.T.);
#64795=ORIENTED_EDGE('',*,*,#44010,.T.);
#64796=ORIENTED_EDGE('',*,*,#44184,.F.);
#64797=ORIENTED_EDGE('',*,*,#44185,.T.);
#64798=ORIENTED_EDGE('',*,*,#44186,.F.);
#64799=ORIENTED_EDGE('',*,*,#44187,.F.);
#64800=ORIENTED_EDGE('',*,*,#44188,.F.);
#64801=ORIENTED_EDGE('',*,*,#44185,.F.);
#64802=ORIENTED_EDGE('',*,*,#44189,.F.);
#64803=ORIENTED_EDGE('',*,*,#44186,.T.);
#64804=ORIENTED_EDGE('',*,*,#44188,.T.);
#64805=ORIENTED_EDGE('',*,*,#44190,.F.);
#64806=ORIENTED_EDGE('',*,*,#44011,.T.);
#64807=ORIENTED_EDGE('',*,*,#44013,.T.);
#64808=ORIENTED_EDGE('',*,*,#44191,.F.);
#64809=ORIENTED_EDGE('',*,*,#44192,.T.);
#64810=ORIENTED_EDGE('',*,*,#44193,.F.);
#64811=ORIENTED_EDGE('',*,*,#44194,.F.);
#64812=ORIENTED_EDGE('',*,*,#44195,.F.);
#64813=ORIENTED_EDGE('',*,*,#44192,.F.);
#64814=ORIENTED_EDGE('',*,*,#44196,.F.);
#64815=ORIENTED_EDGE('',*,*,#44193,.T.);
#64816=ORIENTED_EDGE('',*,*,#44195,.T.);
#64817=ORIENTED_EDGE('',*,*,#44197,.F.);
#64818=ORIENTED_EDGE('',*,*,#44014,.T.);
#64819=ORIENTED_EDGE('',*,*,#44016,.T.);
#64820=ORIENTED_EDGE('',*,*,#44198,.F.);
#64821=ORIENTED_EDGE('',*,*,#44199,.T.);
#64822=ORIENTED_EDGE('',*,*,#44200,.F.);
#64823=ORIENTED_EDGE('',*,*,#44201,.F.);
#64824=ORIENTED_EDGE('',*,*,#44202,.F.);
#64825=ORIENTED_EDGE('',*,*,#44199,.F.);
#64826=ORIENTED_EDGE('',*,*,#44203,.F.);
#64827=ORIENTED_EDGE('',*,*,#44200,.T.);
#64828=ORIENTED_EDGE('',*,*,#44202,.T.);
#64829=ORIENTED_EDGE('',*,*,#44204,.F.);
#64830=ORIENTED_EDGE('',*,*,#44017,.T.);
#64831=ORIENTED_EDGE('',*,*,#44019,.T.);
#64832=ORIENTED_EDGE('',*,*,#44205,.F.);
#64833=ORIENTED_EDGE('',*,*,#44206,.T.);
#64834=ORIENTED_EDGE('',*,*,#44207,.F.);
#64835=ORIENTED_EDGE('',*,*,#44208,.F.);
#64836=ORIENTED_EDGE('',*,*,#44209,.F.);
#64837=ORIENTED_EDGE('',*,*,#44206,.F.);
#64838=ORIENTED_EDGE('',*,*,#44210,.F.);
#64839=ORIENTED_EDGE('',*,*,#44207,.T.);
#64840=ORIENTED_EDGE('',*,*,#44209,.T.);
#64841=ORIENTED_EDGE('',*,*,#44211,.F.);
#64842=ORIENTED_EDGE('',*,*,#44020,.T.);
#64843=ORIENTED_EDGE('',*,*,#44022,.T.);
#64844=ORIENTED_EDGE('',*,*,#44212,.F.);
#64845=ORIENTED_EDGE('',*,*,#44213,.T.);
#64846=ORIENTED_EDGE('',*,*,#44214,.F.);
#64847=ORIENTED_EDGE('',*,*,#44215,.F.);
#64848=ORIENTED_EDGE('',*,*,#44216,.F.);
#64849=ORIENTED_EDGE('',*,*,#44213,.F.);
#64850=ORIENTED_EDGE('',*,*,#44217,.F.);
#64851=ORIENTED_EDGE('',*,*,#44214,.T.);
#64852=ORIENTED_EDGE('',*,*,#44216,.T.);
#64853=ORIENTED_EDGE('',*,*,#44218,.F.);
#64854=ORIENTED_EDGE('',*,*,#44023,.T.);
#64855=ORIENTED_EDGE('',*,*,#44025,.T.);
#64856=ORIENTED_EDGE('',*,*,#44219,.F.);
#64857=ORIENTED_EDGE('',*,*,#34335,.T.);
#64858=ORIENTED_EDGE('',*,*,#44220,.F.);
#64859=ORIENTED_EDGE('',*,*,#44220,.T.);
#64860=ORIENTED_EDGE('',*,*,#34334,.T.);
#64861=ORIENTED_EDGE('',*,*,#44221,.F.);
#64862=ORIENTED_EDGE('',*,*,#44026,.T.);
#64863=ORIENTED_EDGE('',*,*,#44222,.F.);
#64864=ORIENTED_EDGE('',*,*,#44223,.F.);
#64865=ORIENTED_EDGE('',*,*,#44032,.T.);
#64866=ORIENTED_EDGE('',*,*,#44027,.T.);
#64867=ORIENTED_EDGE('',*,*,#44224,.F.);
#64868=ORIENTED_EDGE('',*,*,#44033,.T.);
#64869=ORIENTED_EDGE('',*,*,#44030,.T.);
#64870=ORIENTED_EDGE('',*,*,#44223,.T.);
#64871=ORIENTED_EDGE('',*,*,#44225,.F.);
#64872=ORIENTED_EDGE('',*,*,#44226,.F.);
#64873=ORIENTED_EDGE('',*,*,#44039,.T.);
#64874=ORIENTED_EDGE('',*,*,#44034,.T.);
#64875=ORIENTED_EDGE('',*,*,#44227,.F.);
#64876=ORIENTED_EDGE('',*,*,#44040,.T.);
#64877=ORIENTED_EDGE('',*,*,#44037,.T.);
#64878=ORIENTED_EDGE('',*,*,#44226,.T.);
#64879=ORIENTED_EDGE('',*,*,#44228,.F.);
#64880=ORIENTED_EDGE('',*,*,#44229,.F.);
#64881=ORIENTED_EDGE('',*,*,#44046,.T.);
#64882=ORIENTED_EDGE('',*,*,#44041,.T.);
#64883=ORIENTED_EDGE('',*,*,#44230,.F.);
#64884=ORIENTED_EDGE('',*,*,#44047,.T.);
#64885=ORIENTED_EDGE('',*,*,#44044,.T.);
#64886=ORIENTED_EDGE('',*,*,#44229,.T.);
#64887=ORIENTED_EDGE('',*,*,#44231,.F.);
#64888=ORIENTED_EDGE('',*,*,#44232,.F.);
#64889=ORIENTED_EDGE('',*,*,#44053,.T.);
#64890=ORIENTED_EDGE('',*,*,#44048,.T.);
#64891=ORIENTED_EDGE('',*,*,#44233,.F.);
#64892=ORIENTED_EDGE('',*,*,#44054,.T.);
#64893=ORIENTED_EDGE('',*,*,#44051,.T.);
#64894=ORIENTED_EDGE('',*,*,#44232,.T.);
#64895=ORIENTED_EDGE('',*,*,#44234,.F.);
#64896=ORIENTED_EDGE('',*,*,#44235,.F.);
#64897=ORIENTED_EDGE('',*,*,#44060,.T.);
#64898=ORIENTED_EDGE('',*,*,#44055,.T.);
#64899=ORIENTED_EDGE('',*,*,#44236,.F.);
#64900=ORIENTED_EDGE('',*,*,#44061,.T.);
#64901=ORIENTED_EDGE('',*,*,#44058,.T.);
#64902=ORIENTED_EDGE('',*,*,#44235,.T.);
#64903=ORIENTED_EDGE('',*,*,#44237,.F.);
#64904=ORIENTED_EDGE('',*,*,#44238,.F.);
#64905=ORIENTED_EDGE('',*,*,#44067,.T.);
#64906=ORIENTED_EDGE('',*,*,#44062,.T.);
#64907=ORIENTED_EDGE('',*,*,#44239,.F.);
#64908=ORIENTED_EDGE('',*,*,#44068,.T.);
#64909=ORIENTED_EDGE('',*,*,#44065,.T.);
#64910=ORIENTED_EDGE('',*,*,#44238,.T.);
#64911=ORIENTED_EDGE('',*,*,#44240,.F.);
#64912=ORIENTED_EDGE('',*,*,#44241,.F.);
#64913=ORIENTED_EDGE('',*,*,#44074,.T.);
#64914=ORIENTED_EDGE('',*,*,#44069,.T.);
#64915=ORIENTED_EDGE('',*,*,#44242,.F.);
#64916=ORIENTED_EDGE('',*,*,#44075,.T.);
#64917=ORIENTED_EDGE('',*,*,#44072,.T.);
#64918=ORIENTED_EDGE('',*,*,#44241,.T.);
#64919=ORIENTED_EDGE('',*,*,#44243,.F.);
#64920=ORIENTED_EDGE('',*,*,#44244,.F.);
#64921=ORIENTED_EDGE('',*,*,#44081,.T.);
#64922=ORIENTED_EDGE('',*,*,#44076,.T.);
#64923=ORIENTED_EDGE('',*,*,#44245,.F.);
#64924=ORIENTED_EDGE('',*,*,#44082,.T.);
#64925=ORIENTED_EDGE('',*,*,#44079,.T.);
#64926=ORIENTED_EDGE('',*,*,#44244,.T.);
#64927=ORIENTED_EDGE('',*,*,#44246,.F.);
#64928=ORIENTED_EDGE('',*,*,#44247,.F.);
#64929=ORIENTED_EDGE('',*,*,#44088,.T.);
#64930=ORIENTED_EDGE('',*,*,#44083,.T.);
#64931=ORIENTED_EDGE('',*,*,#44248,.F.);
#64932=ORIENTED_EDGE('',*,*,#44089,.T.);
#64933=ORIENTED_EDGE('',*,*,#44086,.T.);
#64934=ORIENTED_EDGE('',*,*,#44247,.T.);
#64935=ORIENTED_EDGE('',*,*,#44249,.F.);
#64936=ORIENTED_EDGE('',*,*,#44250,.F.);
#64937=ORIENTED_EDGE('',*,*,#44095,.T.);
#64938=ORIENTED_EDGE('',*,*,#44090,.T.);
#64939=ORIENTED_EDGE('',*,*,#44251,.F.);
#64940=ORIENTED_EDGE('',*,*,#44096,.T.);
#64941=ORIENTED_EDGE('',*,*,#44093,.T.);
#64942=ORIENTED_EDGE('',*,*,#44250,.T.);
#64943=ORIENTED_EDGE('',*,*,#44252,.F.);
#64944=ORIENTED_EDGE('',*,*,#44253,.F.);
#64945=ORIENTED_EDGE('',*,*,#44102,.T.);
#64946=ORIENTED_EDGE('',*,*,#44097,.T.);
#64947=ORIENTED_EDGE('',*,*,#44254,.F.);
#64948=ORIENTED_EDGE('',*,*,#44103,.T.);
#64949=ORIENTED_EDGE('',*,*,#44100,.T.);
#64950=ORIENTED_EDGE('',*,*,#44253,.T.);
#64951=ORIENTED_EDGE('',*,*,#44255,.F.);
#64952=ORIENTED_EDGE('',*,*,#44256,.F.);
#64953=ORIENTED_EDGE('',*,*,#44109,.T.);
#64954=ORIENTED_EDGE('',*,*,#44104,.T.);
#64955=ORIENTED_EDGE('',*,*,#44257,.F.);
#64956=ORIENTED_EDGE('',*,*,#44110,.T.);
#64957=ORIENTED_EDGE('',*,*,#44107,.T.);
#64958=ORIENTED_EDGE('',*,*,#44256,.T.);
#64959=ORIENTED_EDGE('',*,*,#44258,.F.);
#64960=ORIENTED_EDGE('',*,*,#44259,.F.);
#64961=ORIENTED_EDGE('',*,*,#44116,.T.);
#64962=ORIENTED_EDGE('',*,*,#44111,.T.);
#64963=ORIENTED_EDGE('',*,*,#44260,.F.);
#64964=ORIENTED_EDGE('',*,*,#44117,.T.);
#64965=ORIENTED_EDGE('',*,*,#44114,.T.);
#64966=ORIENTED_EDGE('',*,*,#44259,.T.);
#64967=ORIENTED_EDGE('',*,*,#44261,.F.);
#64968=ORIENTED_EDGE('',*,*,#44262,.F.);
#64969=ORIENTED_EDGE('',*,*,#44123,.T.);
#64970=ORIENTED_EDGE('',*,*,#44118,.T.);
#64971=ORIENTED_EDGE('',*,*,#44263,.F.);
#64972=ORIENTED_EDGE('',*,*,#44124,.T.);
#64973=ORIENTED_EDGE('',*,*,#44121,.T.);
#64974=ORIENTED_EDGE('',*,*,#44262,.T.);
#64975=ORIENTED_EDGE('',*,*,#44264,.F.);
#64976=ORIENTED_EDGE('',*,*,#44265,.F.);
#64977=ORIENTED_EDGE('',*,*,#44130,.T.);
#64978=ORIENTED_EDGE('',*,*,#44125,.T.);
#64979=ORIENTED_EDGE('',*,*,#44266,.F.);
#64980=ORIENTED_EDGE('',*,*,#44131,.T.);
#64981=ORIENTED_EDGE('',*,*,#44128,.T.);
#64982=ORIENTED_EDGE('',*,*,#44265,.T.);
#64983=ORIENTED_EDGE('',*,*,#44267,.F.);
#64984=ORIENTED_EDGE('',*,*,#44268,.F.);
#64985=ORIENTED_EDGE('',*,*,#44137,.T.);
#64986=ORIENTED_EDGE('',*,*,#44132,.T.);
#64987=ORIENTED_EDGE('',*,*,#44269,.F.);
#64988=ORIENTED_EDGE('',*,*,#44138,.T.);
#64989=ORIENTED_EDGE('',*,*,#44135,.T.);
#64990=ORIENTED_EDGE('',*,*,#44268,.T.);
#64991=ORIENTED_EDGE('',*,*,#44270,.F.);
#64992=ORIENTED_EDGE('',*,*,#44271,.F.);
#64993=ORIENTED_EDGE('',*,*,#44144,.T.);
#64994=ORIENTED_EDGE('',*,*,#44139,.T.);
#64995=ORIENTED_EDGE('',*,*,#44272,.F.);
#64996=ORIENTED_EDGE('',*,*,#44145,.T.);
#64997=ORIENTED_EDGE('',*,*,#44142,.T.);
#64998=ORIENTED_EDGE('',*,*,#44271,.T.);
#64999=ORIENTED_EDGE('',*,*,#44273,.F.);
#65000=ORIENTED_EDGE('',*,*,#44274,.F.);
#65001=ORIENTED_EDGE('',*,*,#44149,.T.);
#65002=ORIENTED_EDGE('',*,*,#44146,.T.);
#65003=ORIENTED_EDGE('',*,*,#44275,.F.);
#65004=ORIENTED_EDGE('',*,*,#44152,.T.);
#65005=ORIENTED_EDGE('',*,*,#44150,.T.);
#65006=ORIENTED_EDGE('',*,*,#44274,.T.);
#65007=ORIENTED_EDGE('',*,*,#44276,.F.);
#65008=ORIENTED_EDGE('',*,*,#44277,.F.);
#65009=ORIENTED_EDGE('',*,*,#44158,.T.);
#65010=ORIENTED_EDGE('',*,*,#44153,.T.);
#65011=ORIENTED_EDGE('',*,*,#44278,.F.);
#65012=ORIENTED_EDGE('',*,*,#44159,.T.);
#65013=ORIENTED_EDGE('',*,*,#44156,.T.);
#65014=ORIENTED_EDGE('',*,*,#44277,.T.);
#65015=ORIENTED_EDGE('',*,*,#44279,.F.);
#65016=ORIENTED_EDGE('',*,*,#44280,.F.);
#65017=ORIENTED_EDGE('',*,*,#44165,.T.);
#65018=ORIENTED_EDGE('',*,*,#44160,.T.);
#65019=ORIENTED_EDGE('',*,*,#44281,.F.);
#65020=ORIENTED_EDGE('',*,*,#44166,.T.);
#65021=ORIENTED_EDGE('',*,*,#44163,.T.);
#65022=ORIENTED_EDGE('',*,*,#44280,.T.);
#65023=ORIENTED_EDGE('',*,*,#44282,.F.);
#65024=ORIENTED_EDGE('',*,*,#44283,.F.);
#65025=ORIENTED_EDGE('',*,*,#44172,.T.);
#65026=ORIENTED_EDGE('',*,*,#44167,.T.);
#65027=ORIENTED_EDGE('',*,*,#44284,.F.);
#65028=ORIENTED_EDGE('',*,*,#44173,.T.);
#65029=ORIENTED_EDGE('',*,*,#44170,.T.);
#65030=ORIENTED_EDGE('',*,*,#44283,.T.);
#65031=ORIENTED_EDGE('',*,*,#44285,.F.);
#65032=ORIENTED_EDGE('',*,*,#44286,.F.);
#65033=ORIENTED_EDGE('',*,*,#34340,.T.);
#65034=ORIENTED_EDGE('',*,*,#44174,.T.);
#65035=ORIENTED_EDGE('',*,*,#44287,.F.);
#65036=ORIENTED_EDGE('',*,*,#44176,.T.);
#65037=ORIENTED_EDGE('',*,*,#34337,.T.);
#65038=ORIENTED_EDGE('',*,*,#44286,.T.);
#65039=ORIENTED_EDGE('',*,*,#44288,.F.);
#65040=ORIENTED_EDGE('',*,*,#44289,.F.);
#65041=ORIENTED_EDGE('',*,*,#44182,.T.);
#65042=ORIENTED_EDGE('',*,*,#44177,.T.);
#65043=ORIENTED_EDGE('',*,*,#44290,.F.);
#65044=ORIENTED_EDGE('',*,*,#44183,.T.);
#65045=ORIENTED_EDGE('',*,*,#44180,.T.);
#65046=ORIENTED_EDGE('',*,*,#44289,.T.);
#65047=ORIENTED_EDGE('',*,*,#44291,.F.);
#65048=ORIENTED_EDGE('',*,*,#44292,.F.);
#65049=ORIENTED_EDGE('',*,*,#44189,.T.);
#65050=ORIENTED_EDGE('',*,*,#44184,.T.);
#65051=ORIENTED_EDGE('',*,*,#44293,.F.);
#65052=ORIENTED_EDGE('',*,*,#44190,.T.);
#65053=ORIENTED_EDGE('',*,*,#44187,.T.);
#65054=ORIENTED_EDGE('',*,*,#44292,.T.);
#65055=ORIENTED_EDGE('',*,*,#44294,.F.);
#65056=ORIENTED_EDGE('',*,*,#44295,.F.);
#65057=ORIENTED_EDGE('',*,*,#44196,.T.);
#65058=ORIENTED_EDGE('',*,*,#44191,.T.);
#65059=ORIENTED_EDGE('',*,*,#44296,.F.);
#65060=ORIENTED_EDGE('',*,*,#44197,.T.);
#65061=ORIENTED_EDGE('',*,*,#44194,.T.);
#65062=ORIENTED_EDGE('',*,*,#44295,.T.);
#65063=ORIENTED_EDGE('',*,*,#44297,.F.);
#65064=ORIENTED_EDGE('',*,*,#44298,.F.);
#65065=ORIENTED_EDGE('',*,*,#44203,.T.);
#65066=ORIENTED_EDGE('',*,*,#44198,.T.);
#65067=ORIENTED_EDGE('',*,*,#44299,.F.);
#65068=ORIENTED_EDGE('',*,*,#44204,.T.);
#65069=ORIENTED_EDGE('',*,*,#44201,.T.);
#65070=ORIENTED_EDGE('',*,*,#44298,.T.);
#65071=ORIENTED_EDGE('',*,*,#44300,.F.);
#65072=ORIENTED_EDGE('',*,*,#44301,.F.);
#65073=ORIENTED_EDGE('',*,*,#44210,.T.);
#65074=ORIENTED_EDGE('',*,*,#44205,.T.);
#65075=ORIENTED_EDGE('',*,*,#44302,.F.);
#65076=ORIENTED_EDGE('',*,*,#44211,.T.);
#65077=ORIENTED_EDGE('',*,*,#44208,.T.);
#65078=ORIENTED_EDGE('',*,*,#44301,.T.);
#65079=ORIENTED_EDGE('',*,*,#44303,.F.);
#65080=ORIENTED_EDGE('',*,*,#44304,.F.);
#65081=ORIENTED_EDGE('',*,*,#44217,.T.);
#65082=ORIENTED_EDGE('',*,*,#44212,.T.);
#65083=ORIENTED_EDGE('',*,*,#44305,.F.);
#65084=ORIENTED_EDGE('',*,*,#44218,.T.);
#65085=ORIENTED_EDGE('',*,*,#44215,.T.);
#65086=ORIENTED_EDGE('',*,*,#44304,.T.);
#65087=ORIENTED_EDGE('',*,*,#44306,.F.);
#65088=ORIENTED_EDGE('',*,*,#44307,.F.);
#65089=ORIENTED_EDGE('',*,*,#34336,.T.);
#65090=ORIENTED_EDGE('',*,*,#44219,.T.);
#65091=ORIENTED_EDGE('',*,*,#44221,.T.);
#65092=ORIENTED_EDGE('',*,*,#34333,.T.);
#65093=ORIENTED_EDGE('',*,*,#44307,.T.);
#65094=ORIENTED_EDGE('',*,*,#44308,.F.);
#65095=ORIENTED_EDGE('',*,*,#34147,.F.);
#65096=ORIENTED_EDGE('',*,*,#34152,.T.);
#65097=ORIENTED_EDGE('',*,*,#44222,.T.);
#65098=ORIENTED_EDGE('',*,*,#44309,.F.);
#65099=ORIENTED_EDGE('',*,*,#34049,.T.);
#65100=ORIENTED_EDGE('',*,*,#44310,.F.);
#65101=ORIENTED_EDGE('',*,*,#44311,.F.);
#65102=ORIENTED_EDGE('',*,*,#44310,.T.);
#65103=ORIENTED_EDGE('',*,*,#34048,.T.);
#65104=ORIENTED_EDGE('',*,*,#44312,.F.);
#65105=ORIENTED_EDGE('',*,*,#44311,.T.);
#65106=ORIENTED_EDGE('',*,*,#34047,.T.);
#65107=ORIENTED_EDGE('',*,*,#44313,.F.);
#65108=ORIENTED_EDGE('',*,*,#44312,.T.);
#65109=ORIENTED_EDGE('',*,*,#34046,.T.);
#65110=ORIENTED_EDGE('',*,*,#44314,.F.);
#65111=ORIENTED_EDGE('',*,*,#44313,.T.);
#65112=ORIENTED_EDGE('',*,*,#34045,.T.);
#65113=ORIENTED_EDGE('',*,*,#44224,.T.);
#65114=ORIENTED_EDGE('',*,*,#44314,.T.);
#65115=ORIENTED_EDGE('',*,*,#34044,.T.);
#65116=ORIENTED_EDGE('',*,*,#44315,.F.);
#65117=ORIENTED_EDGE('',*,*,#44225,.T.);
#65118=ORIENTED_EDGE('',*,*,#44315,.T.);
#65119=ORIENTED_EDGE('',*,*,#34043,.T.);
#65120=ORIENTED_EDGE('',*,*,#44316,.F.);
#65121=ORIENTED_EDGE('',*,*,#44317,.F.);
#65122=ORIENTED_EDGE('',*,*,#44316,.T.);
#65123=ORIENTED_EDGE('',*,*,#34042,.T.);
#65124=ORIENTED_EDGE('',*,*,#44318,.F.);
#65125=ORIENTED_EDGE('',*,*,#44317,.T.);
#65126=ORIENTED_EDGE('',*,*,#34041,.T.);
#65127=ORIENTED_EDGE('',*,*,#44319,.F.);
#65128=ORIENTED_EDGE('',*,*,#44318,.T.);
#65129=ORIENTED_EDGE('',*,*,#34040,.T.);
#65130=ORIENTED_EDGE('',*,*,#44320,.F.);
#65131=ORIENTED_EDGE('',*,*,#44319,.T.);
#65132=ORIENTED_EDGE('',*,*,#34039,.T.);
#65133=ORIENTED_EDGE('',*,*,#44227,.T.);
#65134=ORIENTED_EDGE('',*,*,#44320,.T.);
#65135=ORIENTED_EDGE('',*,*,#34038,.T.);
#65136=ORIENTED_EDGE('',*,*,#44321,.F.);
#65137=ORIENTED_EDGE('',*,*,#44228,.T.);
#65138=ORIENTED_EDGE('',*,*,#44321,.T.);
#65139=ORIENTED_EDGE('',*,*,#34037,.T.);
#65140=ORIENTED_EDGE('',*,*,#44322,.F.);
#65141=ORIENTED_EDGE('',*,*,#44323,.F.);
#65142=ORIENTED_EDGE('',*,*,#44322,.T.);
#65143=ORIENTED_EDGE('',*,*,#34036,.T.);
#65144=ORIENTED_EDGE('',*,*,#44324,.F.);
#65145=ORIENTED_EDGE('',*,*,#44323,.T.);
#65146=ORIENTED_EDGE('',*,*,#34035,.T.);
#65147=ORIENTED_EDGE('',*,*,#44325,.F.);
#65148=ORIENTED_EDGE('',*,*,#44324,.T.);
#65149=ORIENTED_EDGE('',*,*,#34034,.T.);
#65150=ORIENTED_EDGE('',*,*,#44326,.F.);
#65151=ORIENTED_EDGE('',*,*,#44325,.T.);
#65152=ORIENTED_EDGE('',*,*,#34033,.T.);
#65153=ORIENTED_EDGE('',*,*,#44230,.T.);
#65154=ORIENTED_EDGE('',*,*,#44326,.T.);
#65155=ORIENTED_EDGE('',*,*,#34032,.T.);
#65156=ORIENTED_EDGE('',*,*,#44327,.F.);
#65157=ORIENTED_EDGE('',*,*,#44231,.T.);
#65158=ORIENTED_EDGE('',*,*,#44327,.T.);
#65159=ORIENTED_EDGE('',*,*,#34031,.T.);
#65160=ORIENTED_EDGE('',*,*,#44328,.F.);
#65161=ORIENTED_EDGE('',*,*,#44329,.F.);
#65162=ORIENTED_EDGE('',*,*,#44328,.T.);
#65163=ORIENTED_EDGE('',*,*,#34030,.T.);
#65164=ORIENTED_EDGE('',*,*,#44330,.F.);
#65165=ORIENTED_EDGE('',*,*,#44329,.T.);
#65166=ORIENTED_EDGE('',*,*,#34029,.T.);
#65167=ORIENTED_EDGE('',*,*,#44331,.F.);
#65168=ORIENTED_EDGE('',*,*,#44330,.T.);
#65169=ORIENTED_EDGE('',*,*,#34028,.T.);
#65170=ORIENTED_EDGE('',*,*,#44332,.F.);
#65171=ORIENTED_EDGE('',*,*,#44331,.T.);
#65172=ORIENTED_EDGE('',*,*,#34027,.T.);
#65173=ORIENTED_EDGE('',*,*,#44233,.T.);
#65174=ORIENTED_EDGE('',*,*,#44332,.T.);
#65175=ORIENTED_EDGE('',*,*,#34026,.T.);
#65176=ORIENTED_EDGE('',*,*,#44333,.F.);
#65177=ORIENTED_EDGE('',*,*,#44234,.T.);
#65178=ORIENTED_EDGE('',*,*,#44333,.T.);
#65179=ORIENTED_EDGE('',*,*,#34025,.T.);
#65180=ORIENTED_EDGE('',*,*,#44334,.F.);
#65181=ORIENTED_EDGE('',*,*,#44335,.F.);
#65182=ORIENTED_EDGE('',*,*,#44334,.T.);
#65183=ORIENTED_EDGE('',*,*,#34024,.T.);
#65184=ORIENTED_EDGE('',*,*,#44336,.F.);
#65185=ORIENTED_EDGE('',*,*,#44335,.T.);
#65186=ORIENTED_EDGE('',*,*,#34023,.T.);
#65187=ORIENTED_EDGE('',*,*,#44337,.F.);
#65188=ORIENTED_EDGE('',*,*,#44336,.T.);
#65189=ORIENTED_EDGE('',*,*,#34022,.T.);
#65190=ORIENTED_EDGE('',*,*,#44338,.F.);
#65191=ORIENTED_EDGE('',*,*,#44337,.T.);
#65192=ORIENTED_EDGE('',*,*,#34021,.T.);
#65193=ORIENTED_EDGE('',*,*,#44236,.T.);
#65194=ORIENTED_EDGE('',*,*,#44338,.T.);
#65195=ORIENTED_EDGE('',*,*,#34020,.T.);
#65196=ORIENTED_EDGE('',*,*,#44339,.F.);
#65197=ORIENTED_EDGE('',*,*,#44237,.T.);
#65198=ORIENTED_EDGE('',*,*,#44339,.T.);
#65199=ORIENTED_EDGE('',*,*,#34019,.T.);
#65200=ORIENTED_EDGE('',*,*,#44340,.F.);
#65201=ORIENTED_EDGE('',*,*,#44341,.F.);
#65202=ORIENTED_EDGE('',*,*,#44340,.T.);
#65203=ORIENTED_EDGE('',*,*,#34018,.T.);
#65204=ORIENTED_EDGE('',*,*,#44342,.F.);
#65205=ORIENTED_EDGE('',*,*,#44341,.T.);
#65206=ORIENTED_EDGE('',*,*,#34017,.T.);
#65207=ORIENTED_EDGE('',*,*,#44343,.F.);
#65208=ORIENTED_EDGE('',*,*,#44342,.T.);
#65209=ORIENTED_EDGE('',*,*,#34016,.T.);
#65210=ORIENTED_EDGE('',*,*,#44344,.F.);
#65211=ORIENTED_EDGE('',*,*,#44343,.T.);
#65212=ORIENTED_EDGE('',*,*,#34015,.T.);
#65213=ORIENTED_EDGE('',*,*,#44239,.T.);
#65214=ORIENTED_EDGE('',*,*,#44344,.T.);
#65215=ORIENTED_EDGE('',*,*,#34014,.T.);
#65216=ORIENTED_EDGE('',*,*,#44345,.F.);
#65217=ORIENTED_EDGE('',*,*,#44240,.T.);
#65218=ORIENTED_EDGE('',*,*,#44345,.T.);
#65219=ORIENTED_EDGE('',*,*,#34013,.T.);
#65220=ORIENTED_EDGE('',*,*,#44346,.F.);
#65221=ORIENTED_EDGE('',*,*,#44347,.F.);
#65222=ORIENTED_EDGE('',*,*,#44346,.T.);
#65223=ORIENTED_EDGE('',*,*,#34012,.T.);
#65224=ORIENTED_EDGE('',*,*,#44348,.F.);
#65225=ORIENTED_EDGE('',*,*,#44347,.T.);
#65226=ORIENTED_EDGE('',*,*,#34011,.T.);
#65227=ORIENTED_EDGE('',*,*,#44349,.F.);
#65228=ORIENTED_EDGE('',*,*,#44348,.T.);
#65229=ORIENTED_EDGE('',*,*,#34010,.T.);
#65230=ORIENTED_EDGE('',*,*,#44350,.F.);
#65231=ORIENTED_EDGE('',*,*,#44349,.T.);
#65232=ORIENTED_EDGE('',*,*,#34009,.T.);
#65233=ORIENTED_EDGE('',*,*,#44242,.T.);
#65234=ORIENTED_EDGE('',*,*,#44350,.T.);
#65235=ORIENTED_EDGE('',*,*,#34008,.T.);
#65236=ORIENTED_EDGE('',*,*,#44351,.F.);
#65237=ORIENTED_EDGE('',*,*,#44243,.T.);
#65238=ORIENTED_EDGE('',*,*,#44351,.T.);
#65239=ORIENTED_EDGE('',*,*,#34007,.T.);
#65240=ORIENTED_EDGE('',*,*,#44352,.F.);
#65241=ORIENTED_EDGE('',*,*,#44353,.F.);
#65242=ORIENTED_EDGE('',*,*,#44352,.T.);
#65243=ORIENTED_EDGE('',*,*,#34006,.T.);
#65244=ORIENTED_EDGE('',*,*,#44354,.F.);
#65245=ORIENTED_EDGE('',*,*,#44353,.T.);
#65246=ORIENTED_EDGE('',*,*,#34005,.T.);
#65247=ORIENTED_EDGE('',*,*,#44355,.F.);
#65248=ORIENTED_EDGE('',*,*,#44354,.T.);
#65249=ORIENTED_EDGE('',*,*,#34004,.T.);
#65250=ORIENTED_EDGE('',*,*,#44356,.F.);
#65251=ORIENTED_EDGE('',*,*,#44355,.T.);
#65252=ORIENTED_EDGE('',*,*,#34003,.T.);
#65253=ORIENTED_EDGE('',*,*,#44245,.T.);
#65254=ORIENTED_EDGE('',*,*,#44356,.T.);
#65255=ORIENTED_EDGE('',*,*,#34002,.T.);
#65256=ORIENTED_EDGE('',*,*,#44357,.F.);
#65257=ORIENTED_EDGE('',*,*,#44246,.T.);
#65258=ORIENTED_EDGE('',*,*,#44357,.T.);
#65259=ORIENTED_EDGE('',*,*,#34001,.T.);
#65260=ORIENTED_EDGE('',*,*,#44358,.F.);
#65261=ORIENTED_EDGE('',*,*,#44359,.F.);
#65262=ORIENTED_EDGE('',*,*,#44358,.T.);
#65263=ORIENTED_EDGE('',*,*,#34000,.T.);
#65264=ORIENTED_EDGE('',*,*,#44360,.F.);
#65265=ORIENTED_EDGE('',*,*,#44359,.T.);
#65266=ORIENTED_EDGE('',*,*,#33999,.T.);
#65267=ORIENTED_EDGE('',*,*,#44361,.F.);
#65268=ORIENTED_EDGE('',*,*,#44360,.T.);
#65269=ORIENTED_EDGE('',*,*,#33998,.T.);
#65270=ORIENTED_EDGE('',*,*,#44362,.F.);
#65271=ORIENTED_EDGE('',*,*,#44361,.T.);
#65272=ORIENTED_EDGE('',*,*,#33997,.T.);
#65273=ORIENTED_EDGE('',*,*,#44248,.T.);
#65274=ORIENTED_EDGE('',*,*,#44362,.T.);
#65275=ORIENTED_EDGE('',*,*,#33996,.T.);
#65276=ORIENTED_EDGE('',*,*,#44363,.F.);
#65277=ORIENTED_EDGE('',*,*,#44249,.T.);
#65278=ORIENTED_EDGE('',*,*,#44363,.T.);
#65279=ORIENTED_EDGE('',*,*,#33995,.T.);
#65280=ORIENTED_EDGE('',*,*,#44364,.F.);
#65281=ORIENTED_EDGE('',*,*,#44365,.F.);
#65282=ORIENTED_EDGE('',*,*,#44364,.T.);
#65283=ORIENTED_EDGE('',*,*,#33994,.T.);
#65284=ORIENTED_EDGE('',*,*,#44366,.F.);
#65285=ORIENTED_EDGE('',*,*,#44365,.T.);
#65286=ORIENTED_EDGE('',*,*,#33993,.T.);
#65287=ORIENTED_EDGE('',*,*,#44367,.F.);
#65288=ORIENTED_EDGE('',*,*,#44366,.T.);
#65289=ORIENTED_EDGE('',*,*,#33992,.T.);
#65290=ORIENTED_EDGE('',*,*,#44368,.F.);
#65291=ORIENTED_EDGE('',*,*,#44367,.T.);
#65292=ORIENTED_EDGE('',*,*,#33991,.T.);
#65293=ORIENTED_EDGE('',*,*,#44251,.T.);
#65294=ORIENTED_EDGE('',*,*,#44368,.T.);
#65295=ORIENTED_EDGE('',*,*,#33990,.T.);
#65296=ORIENTED_EDGE('',*,*,#44369,.F.);
#65297=ORIENTED_EDGE('',*,*,#44252,.T.);
#65298=ORIENTED_EDGE('',*,*,#44369,.T.);
#65299=ORIENTED_EDGE('',*,*,#33989,.T.);
#65300=ORIENTED_EDGE('',*,*,#44370,.F.);
#65301=ORIENTED_EDGE('',*,*,#44371,.F.);
#65302=ORIENTED_EDGE('',*,*,#44370,.T.);
#65303=ORIENTED_EDGE('',*,*,#33988,.T.);
#65304=ORIENTED_EDGE('',*,*,#44372,.F.);
#65305=ORIENTED_EDGE('',*,*,#44371,.T.);
#65306=ORIENTED_EDGE('',*,*,#33987,.T.);
#65307=ORIENTED_EDGE('',*,*,#44373,.F.);
#65308=ORIENTED_EDGE('',*,*,#44372,.T.);
#65309=ORIENTED_EDGE('',*,*,#33986,.T.);
#65310=ORIENTED_EDGE('',*,*,#44374,.F.);
#65311=ORIENTED_EDGE('',*,*,#44373,.T.);
#65312=ORIENTED_EDGE('',*,*,#33985,.T.);
#65313=ORIENTED_EDGE('',*,*,#44254,.T.);
#65314=ORIENTED_EDGE('',*,*,#44374,.T.);
#65315=ORIENTED_EDGE('',*,*,#33984,.T.);
#65316=ORIENTED_EDGE('',*,*,#44375,.F.);
#65317=ORIENTED_EDGE('',*,*,#44255,.T.);
#65318=ORIENTED_EDGE('',*,*,#44375,.T.);
#65319=ORIENTED_EDGE('',*,*,#33983,.T.);
#65320=ORIENTED_EDGE('',*,*,#44376,.F.);
#65321=ORIENTED_EDGE('',*,*,#44377,.F.);
#65322=ORIENTED_EDGE('',*,*,#44376,.T.);
#65323=ORIENTED_EDGE('',*,*,#33982,.T.);
#65324=ORIENTED_EDGE('',*,*,#44378,.F.);
#65325=ORIENTED_EDGE('',*,*,#44377,.T.);
#65326=ORIENTED_EDGE('',*,*,#33981,.T.);
#65327=ORIENTED_EDGE('',*,*,#44379,.F.);
#65328=ORIENTED_EDGE('',*,*,#44378,.T.);
#65329=ORIENTED_EDGE('',*,*,#33980,.T.);
#65330=ORIENTED_EDGE('',*,*,#44380,.F.);
#65331=ORIENTED_EDGE('',*,*,#44379,.T.);
#65332=ORIENTED_EDGE('',*,*,#33979,.T.);
#65333=ORIENTED_EDGE('',*,*,#44257,.T.);
#65334=ORIENTED_EDGE('',*,*,#44380,.T.);
#65335=ORIENTED_EDGE('',*,*,#33978,.T.);
#65336=ORIENTED_EDGE('',*,*,#44381,.F.);
#65337=ORIENTED_EDGE('',*,*,#44258,.T.);
#65338=ORIENTED_EDGE('',*,*,#44381,.T.);
#65339=ORIENTED_EDGE('',*,*,#33977,.T.);
#65340=ORIENTED_EDGE('',*,*,#44382,.F.);
#65341=ORIENTED_EDGE('',*,*,#44383,.F.);
#65342=ORIENTED_EDGE('',*,*,#44382,.T.);
#65343=ORIENTED_EDGE('',*,*,#33976,.T.);
#65344=ORIENTED_EDGE('',*,*,#44384,.F.);
#65345=ORIENTED_EDGE('',*,*,#44383,.T.);
#65346=ORIENTED_EDGE('',*,*,#33975,.T.);
#65347=ORIENTED_EDGE('',*,*,#44385,.F.);
#65348=ORIENTED_EDGE('',*,*,#44384,.T.);
#65349=ORIENTED_EDGE('',*,*,#33974,.T.);
#65350=ORIENTED_EDGE('',*,*,#44386,.F.);
#65351=ORIENTED_EDGE('',*,*,#44385,.T.);
#65352=ORIENTED_EDGE('',*,*,#33973,.T.);
#65353=ORIENTED_EDGE('',*,*,#44260,.T.);
#65354=ORIENTED_EDGE('',*,*,#44386,.T.);
#65355=ORIENTED_EDGE('',*,*,#33972,.T.);
#65356=ORIENTED_EDGE('',*,*,#44387,.F.);
#65357=ORIENTED_EDGE('',*,*,#44261,.T.);
#65358=ORIENTED_EDGE('',*,*,#44387,.T.);
#65359=ORIENTED_EDGE('',*,*,#33971,.T.);
#65360=ORIENTED_EDGE('',*,*,#44388,.F.);
#65361=ORIENTED_EDGE('',*,*,#44389,.F.);
#65362=ORIENTED_EDGE('',*,*,#44388,.T.);
#65363=ORIENTED_EDGE('',*,*,#33970,.T.);
#65364=ORIENTED_EDGE('',*,*,#44390,.F.);
#65365=ORIENTED_EDGE('',*,*,#44389,.T.);
#65366=ORIENTED_EDGE('',*,*,#33969,.T.);
#65367=ORIENTED_EDGE('',*,*,#44391,.F.);
#65368=ORIENTED_EDGE('',*,*,#44390,.T.);
#65369=ORIENTED_EDGE('',*,*,#33968,.T.);
#65370=ORIENTED_EDGE('',*,*,#44392,.F.);
#65371=ORIENTED_EDGE('',*,*,#44391,.T.);
#65372=ORIENTED_EDGE('',*,*,#33967,.T.);
#65373=ORIENTED_EDGE('',*,*,#44263,.T.);
#65374=ORIENTED_EDGE('',*,*,#44392,.T.);
#65375=ORIENTED_EDGE('',*,*,#33966,.T.);
#65376=ORIENTED_EDGE('',*,*,#44393,.F.);
#65377=ORIENTED_EDGE('',*,*,#44393,.T.);
#65378=ORIENTED_EDGE('',*,*,#33965,.T.);
#65379=ORIENTED_EDGE('',*,*,#34146,.T.);
#65380=ORIENTED_EDGE('',*,*,#44394,.F.);
#65381=ORIENTED_EDGE('',*,*,#44264,.T.);
#65382=ORIENTED_EDGE('',*,*,#44394,.T.);
#65383=ORIENTED_EDGE('',*,*,#34145,.T.);
#65384=ORIENTED_EDGE('',*,*,#34141,.T.);
#65385=ORIENTED_EDGE('',*,*,#44395,.F.);
#65386=ORIENTED_EDGE('',*,*,#44395,.T.);
#65387=ORIENTED_EDGE('',*,*,#34140,.T.);
#65388=ORIENTED_EDGE('',*,*,#34137,.T.);
#65389=ORIENTED_EDGE('',*,*,#44396,.F.);
#65390=ORIENTED_EDGE('',*,*,#44397,.F.);
#65391=ORIENTED_EDGE('',*,*,#44396,.T.);
#65392=ORIENTED_EDGE('',*,*,#34136,.T.);
#65393=ORIENTED_EDGE('',*,*,#44398,.F.);
#65394=ORIENTED_EDGE('',*,*,#44397,.T.);
#65395=ORIENTED_EDGE('',*,*,#34135,.T.);
#65396=ORIENTED_EDGE('',*,*,#44266,.T.);
#65397=ORIENTED_EDGE('',*,*,#44398,.T.);
#65398=ORIENTED_EDGE('',*,*,#34134,.T.);
#65399=ORIENTED_EDGE('',*,*,#44399,.F.);
#65400=ORIENTED_EDGE('',*,*,#44267,.T.);
#65401=ORIENTED_EDGE('',*,*,#44399,.T.);
#65402=ORIENTED_EDGE('',*,*,#34133,.T.);
#65403=ORIENTED_EDGE('',*,*,#44400,.F.);
#65404=ORIENTED_EDGE('',*,*,#44401,.F.);
#65405=ORIENTED_EDGE('',*,*,#44400,.T.);
#65406=ORIENTED_EDGE('',*,*,#34132,.T.);
#65407=ORIENTED_EDGE('',*,*,#44402,.F.);
#65408=ORIENTED_EDGE('',*,*,#44401,.T.);
#65409=ORIENTED_EDGE('',*,*,#34131,.T.);
#65410=ORIENTED_EDGE('',*,*,#44403,.F.);
#65411=ORIENTED_EDGE('',*,*,#44402,.T.);
#65412=ORIENTED_EDGE('',*,*,#34130,.T.);
#65413=ORIENTED_EDGE('',*,*,#44404,.F.);
#65414=ORIENTED_EDGE('',*,*,#44403,.T.);
#65415=ORIENTED_EDGE('',*,*,#34129,.T.);
#65416=ORIENTED_EDGE('',*,*,#44269,.T.);
#65417=ORIENTED_EDGE('',*,*,#44404,.T.);
#65418=ORIENTED_EDGE('',*,*,#34128,.T.);
#65419=ORIENTED_EDGE('',*,*,#44405,.F.);
#65420=ORIENTED_EDGE('',*,*,#44270,.T.);
#65421=ORIENTED_EDGE('',*,*,#44405,.T.);
#65422=ORIENTED_EDGE('',*,*,#34127,.T.);
#65423=ORIENTED_EDGE('',*,*,#44406,.F.);
#65424=ORIENTED_EDGE('',*,*,#44407,.F.);
#65425=ORIENTED_EDGE('',*,*,#44406,.T.);
#65426=ORIENTED_EDGE('',*,*,#34126,.T.);
#65427=ORIENTED_EDGE('',*,*,#44408,.F.);
#65428=ORIENTED_EDGE('',*,*,#44407,.T.);
#65429=ORIENTED_EDGE('',*,*,#34125,.T.);
#65430=ORIENTED_EDGE('',*,*,#44409,.F.);
#65431=ORIENTED_EDGE('',*,*,#44408,.T.);
#65432=ORIENTED_EDGE('',*,*,#34124,.T.);
#65433=ORIENTED_EDGE('',*,*,#44410,.F.);
#65434=ORIENTED_EDGE('',*,*,#44409,.T.);
#65435=ORIENTED_EDGE('',*,*,#34123,.T.);
#65436=ORIENTED_EDGE('',*,*,#44272,.T.);
#65437=ORIENTED_EDGE('',*,*,#44410,.T.);
#65438=ORIENTED_EDGE('',*,*,#34122,.T.);
#65439=ORIENTED_EDGE('',*,*,#44411,.F.);
#65440=ORIENTED_EDGE('',*,*,#44273,.T.);
#65441=ORIENTED_EDGE('',*,*,#44411,.T.);
#65442=ORIENTED_EDGE('',*,*,#34121,.T.);
#65443=ORIENTED_EDGE('',*,*,#44412,.F.);
#65444=ORIENTED_EDGE('',*,*,#44413,.F.);
#65445=ORIENTED_EDGE('',*,*,#44412,.T.);
#65446=ORIENTED_EDGE('',*,*,#34120,.T.);
#65447=ORIENTED_EDGE('',*,*,#44414,.F.);
#65448=ORIENTED_EDGE('',*,*,#44413,.T.);
#65449=ORIENTED_EDGE('',*,*,#34119,.T.);
#65450=ORIENTED_EDGE('',*,*,#44415,.F.);
#65451=ORIENTED_EDGE('',*,*,#44414,.T.);
#65452=ORIENTED_EDGE('',*,*,#34118,.T.);
#65453=ORIENTED_EDGE('',*,*,#44416,.F.);
#65454=ORIENTED_EDGE('',*,*,#44415,.T.);
#65455=ORIENTED_EDGE('',*,*,#34117,.T.);
#65456=ORIENTED_EDGE('',*,*,#44275,.T.);
#65457=ORIENTED_EDGE('',*,*,#44416,.T.);
#65458=ORIENTED_EDGE('',*,*,#34116,.T.);
#65459=ORIENTED_EDGE('',*,*,#44417,.F.);
#65460=ORIENTED_EDGE('',*,*,#44276,.T.);
#65461=ORIENTED_EDGE('',*,*,#44417,.T.);
#65462=ORIENTED_EDGE('',*,*,#34115,.T.);
#65463=ORIENTED_EDGE('',*,*,#44418,.F.);
#65464=ORIENTED_EDGE('',*,*,#44419,.F.);
#65465=ORIENTED_EDGE('',*,*,#44418,.T.);
#65466=ORIENTED_EDGE('',*,*,#34114,.T.);
#65467=ORIENTED_EDGE('',*,*,#44420,.F.);
#65468=ORIENTED_EDGE('',*,*,#44419,.T.);
#65469=ORIENTED_EDGE('',*,*,#34113,.T.);
#65470=ORIENTED_EDGE('',*,*,#44421,.F.);
#65471=ORIENTED_EDGE('',*,*,#44420,.T.);
#65472=ORIENTED_EDGE('',*,*,#34112,.T.);
#65473=ORIENTED_EDGE('',*,*,#44422,.F.);
#65474=ORIENTED_EDGE('',*,*,#44421,.T.);
#65475=ORIENTED_EDGE('',*,*,#34111,.T.);
#65476=ORIENTED_EDGE('',*,*,#44278,.T.);
#65477=ORIENTED_EDGE('',*,*,#44422,.T.);
#65478=ORIENTED_EDGE('',*,*,#34110,.T.);
#65479=ORIENTED_EDGE('',*,*,#44423,.F.);
#65480=ORIENTED_EDGE('',*,*,#44279,.T.);
#65481=ORIENTED_EDGE('',*,*,#44423,.T.);
#65482=ORIENTED_EDGE('',*,*,#34109,.T.);
#65483=ORIENTED_EDGE('',*,*,#44424,.F.);
#65484=ORIENTED_EDGE('',*,*,#44425,.F.);
#65485=ORIENTED_EDGE('',*,*,#44424,.T.);
#65486=ORIENTED_EDGE('',*,*,#34108,.T.);
#65487=ORIENTED_EDGE('',*,*,#44426,.F.);
#65488=ORIENTED_EDGE('',*,*,#44425,.T.);
#65489=ORIENTED_EDGE('',*,*,#34107,.T.);
#65490=ORIENTED_EDGE('',*,*,#44427,.F.);
#65491=ORIENTED_EDGE('',*,*,#44426,.T.);
#65492=ORIENTED_EDGE('',*,*,#34106,.T.);
#65493=ORIENTED_EDGE('',*,*,#44428,.F.);
#65494=ORIENTED_EDGE('',*,*,#44427,.T.);
#65495=ORIENTED_EDGE('',*,*,#34105,.T.);
#65496=ORIENTED_EDGE('',*,*,#44281,.T.);
#65497=ORIENTED_EDGE('',*,*,#44428,.T.);
#65498=ORIENTED_EDGE('',*,*,#34104,.T.);
#65499=ORIENTED_EDGE('',*,*,#44429,.F.);
#65500=ORIENTED_EDGE('',*,*,#44282,.T.);
#65501=ORIENTED_EDGE('',*,*,#44429,.T.);
#65502=ORIENTED_EDGE('',*,*,#34103,.T.);
#65503=ORIENTED_EDGE('',*,*,#44430,.F.);
#65504=ORIENTED_EDGE('',*,*,#44431,.F.);
#65505=ORIENTED_EDGE('',*,*,#44430,.T.);
#65506=ORIENTED_EDGE('',*,*,#34102,.T.);
#65507=ORIENTED_EDGE('',*,*,#44432,.F.);
#65508=ORIENTED_EDGE('',*,*,#44431,.T.);
#65509=ORIENTED_EDGE('',*,*,#34101,.T.);
#65510=ORIENTED_EDGE('',*,*,#44433,.F.);
#65511=ORIENTED_EDGE('',*,*,#44432,.T.);
#65512=ORIENTED_EDGE('',*,*,#34100,.T.);
#65513=ORIENTED_EDGE('',*,*,#44434,.F.);
#65514=ORIENTED_EDGE('',*,*,#44433,.T.);
#65515=ORIENTED_EDGE('',*,*,#34099,.T.);
#65516=ORIENTED_EDGE('',*,*,#44284,.T.);
#65517=ORIENTED_EDGE('',*,*,#44434,.T.);
#65518=ORIENTED_EDGE('',*,*,#34098,.T.);
#65519=ORIENTED_EDGE('',*,*,#44435,.F.);
#65520=ORIENTED_EDGE('',*,*,#44285,.T.);
#65521=ORIENTED_EDGE('',*,*,#44435,.T.);
#65522=ORIENTED_EDGE('',*,*,#34097,.T.);
#65523=ORIENTED_EDGE('',*,*,#44436,.F.);
#65524=ORIENTED_EDGE('',*,*,#44437,.F.);
#65525=ORIENTED_EDGE('',*,*,#44436,.T.);
#65526=ORIENTED_EDGE('',*,*,#34096,.T.);
#65527=ORIENTED_EDGE('',*,*,#44438,.F.);
#65528=ORIENTED_EDGE('',*,*,#44437,.T.);
#65529=ORIENTED_EDGE('',*,*,#34095,.T.);
#65530=ORIENTED_EDGE('',*,*,#44439,.F.);
#65531=ORIENTED_EDGE('',*,*,#44438,.T.);
#65532=ORIENTED_EDGE('',*,*,#34094,.T.);
#65533=ORIENTED_EDGE('',*,*,#44440,.F.);
#65534=ORIENTED_EDGE('',*,*,#44439,.T.);
#65535=ORIENTED_EDGE('',*,*,#34093,.T.);
#65536=ORIENTED_EDGE('',*,*,#44287,.T.);
#65537=ORIENTED_EDGE('',*,*,#44440,.T.);
#65538=ORIENTED_EDGE('',*,*,#34092,.T.);
#65539=ORIENTED_EDGE('',*,*,#44441,.F.);
#65540=ORIENTED_EDGE('',*,*,#44288,.T.);
#65541=ORIENTED_EDGE('',*,*,#44441,.T.);
#65542=ORIENTED_EDGE('',*,*,#34091,.T.);
#65543=ORIENTED_EDGE('',*,*,#44442,.F.);
#65544=ORIENTED_EDGE('',*,*,#44443,.F.);
#65545=ORIENTED_EDGE('',*,*,#44442,.T.);
#65546=ORIENTED_EDGE('',*,*,#34090,.T.);
#65547=ORIENTED_EDGE('',*,*,#44444,.F.);
#65548=ORIENTED_EDGE('',*,*,#44443,.T.);
#65549=ORIENTED_EDGE('',*,*,#34089,.T.);
#65550=ORIENTED_EDGE('',*,*,#44445,.F.);
#65551=ORIENTED_EDGE('',*,*,#44444,.T.);
#65552=ORIENTED_EDGE('',*,*,#34088,.T.);
#65553=ORIENTED_EDGE('',*,*,#44446,.F.);
#65554=ORIENTED_EDGE('',*,*,#44445,.T.);
#65555=ORIENTED_EDGE('',*,*,#34087,.T.);
#65556=ORIENTED_EDGE('',*,*,#44290,.T.);
#65557=ORIENTED_EDGE('',*,*,#44446,.T.);
#65558=ORIENTED_EDGE('',*,*,#34086,.T.);
#65559=ORIENTED_EDGE('',*,*,#44447,.F.);
#65560=ORIENTED_EDGE('',*,*,#44291,.T.);
#65561=ORIENTED_EDGE('',*,*,#44447,.T.);
#65562=ORIENTED_EDGE('',*,*,#34085,.T.);
#65563=ORIENTED_EDGE('',*,*,#44448,.F.);
#65564=ORIENTED_EDGE('',*,*,#44449,.F.);
#65565=ORIENTED_EDGE('',*,*,#44448,.T.);
#65566=ORIENTED_EDGE('',*,*,#34084,.T.);
#65567=ORIENTED_EDGE('',*,*,#44450,.F.);
#65568=ORIENTED_EDGE('',*,*,#44449,.T.);
#65569=ORIENTED_EDGE('',*,*,#34083,.T.);
#65570=ORIENTED_EDGE('',*,*,#44451,.F.);
#65571=ORIENTED_EDGE('',*,*,#44450,.T.);
#65572=ORIENTED_EDGE('',*,*,#34082,.T.);
#65573=ORIENTED_EDGE('',*,*,#44452,.F.);
#65574=ORIENTED_EDGE('',*,*,#44451,.T.);
#65575=ORIENTED_EDGE('',*,*,#34081,.T.);
#65576=ORIENTED_EDGE('',*,*,#44293,.T.);
#65577=ORIENTED_EDGE('',*,*,#44452,.T.);
#65578=ORIENTED_EDGE('',*,*,#34080,.T.);
#65579=ORIENTED_EDGE('',*,*,#44453,.F.);
#65580=ORIENTED_EDGE('',*,*,#44294,.T.);
#65581=ORIENTED_EDGE('',*,*,#44453,.T.);
#65582=ORIENTED_EDGE('',*,*,#34079,.T.);
#65583=ORIENTED_EDGE('',*,*,#44454,.F.);
#65584=ORIENTED_EDGE('',*,*,#44455,.F.);
#65585=ORIENTED_EDGE('',*,*,#44454,.T.);
#65586=ORIENTED_EDGE('',*,*,#34078,.T.);
#65587=ORIENTED_EDGE('',*,*,#44456,.F.);
#65588=ORIENTED_EDGE('',*,*,#44455,.T.);
#65589=ORIENTED_EDGE('',*,*,#34077,.T.);
#65590=ORIENTED_EDGE('',*,*,#44457,.F.);
#65591=ORIENTED_EDGE('',*,*,#44456,.T.);
#65592=ORIENTED_EDGE('',*,*,#34076,.T.);
#65593=ORIENTED_EDGE('',*,*,#44458,.F.);
#65594=ORIENTED_EDGE('',*,*,#44457,.T.);
#65595=ORIENTED_EDGE('',*,*,#34075,.T.);
#65596=ORIENTED_EDGE('',*,*,#44296,.T.);
#65597=ORIENTED_EDGE('',*,*,#44458,.T.);
#65598=ORIENTED_EDGE('',*,*,#34074,.T.);
#65599=ORIENTED_EDGE('',*,*,#44459,.F.);
#65600=ORIENTED_EDGE('',*,*,#44297,.T.);
#65601=ORIENTED_EDGE('',*,*,#44459,.T.);
#65602=ORIENTED_EDGE('',*,*,#34073,.T.);
#65603=ORIENTED_EDGE('',*,*,#44460,.F.);
#65604=ORIENTED_EDGE('',*,*,#44461,.F.);
#65605=ORIENTED_EDGE('',*,*,#44460,.T.);
#65606=ORIENTED_EDGE('',*,*,#34072,.T.);
#65607=ORIENTED_EDGE('',*,*,#44462,.F.);
#65608=ORIENTED_EDGE('',*,*,#44461,.T.);
#65609=ORIENTED_EDGE('',*,*,#34071,.T.);
#65610=ORIENTED_EDGE('',*,*,#44463,.F.);
#65611=ORIENTED_EDGE('',*,*,#44462,.T.);
#65612=ORIENTED_EDGE('',*,*,#34070,.T.);
#65613=ORIENTED_EDGE('',*,*,#44464,.F.);
#65614=ORIENTED_EDGE('',*,*,#44463,.T.);
#65615=ORIENTED_EDGE('',*,*,#34069,.T.);
#65616=ORIENTED_EDGE('',*,*,#44299,.T.);
#65617=ORIENTED_EDGE('',*,*,#44464,.T.);
#65618=ORIENTED_EDGE('',*,*,#34068,.T.);
#65619=ORIENTED_EDGE('',*,*,#44465,.F.);
#65620=ORIENTED_EDGE('',*,*,#44300,.T.);
#65621=ORIENTED_EDGE('',*,*,#44465,.T.);
#65622=ORIENTED_EDGE('',*,*,#34067,.T.);
#65623=ORIENTED_EDGE('',*,*,#44466,.F.);
#65624=ORIENTED_EDGE('',*,*,#44467,.F.);
#65625=ORIENTED_EDGE('',*,*,#44466,.T.);
#65626=ORIENTED_EDGE('',*,*,#34066,.T.);
#65627=ORIENTED_EDGE('',*,*,#44468,.F.);
#65628=ORIENTED_EDGE('',*,*,#44467,.T.);
#65629=ORIENTED_EDGE('',*,*,#34065,.T.);
#65630=ORIENTED_EDGE('',*,*,#44469,.F.);
#65631=ORIENTED_EDGE('',*,*,#44468,.T.);
#65632=ORIENTED_EDGE('',*,*,#34064,.T.);
#65633=ORIENTED_EDGE('',*,*,#44470,.F.);
#65634=ORIENTED_EDGE('',*,*,#44469,.T.);
#65635=ORIENTED_EDGE('',*,*,#34063,.T.);
#65636=ORIENTED_EDGE('',*,*,#44302,.T.);
#65637=ORIENTED_EDGE('',*,*,#44470,.T.);
#65638=ORIENTED_EDGE('',*,*,#34062,.T.);
#65639=ORIENTED_EDGE('',*,*,#44471,.F.);
#65640=ORIENTED_EDGE('',*,*,#44303,.T.);
#65641=ORIENTED_EDGE('',*,*,#44471,.T.);
#65642=ORIENTED_EDGE('',*,*,#34061,.T.);
#65643=ORIENTED_EDGE('',*,*,#44472,.F.);
#65644=ORIENTED_EDGE('',*,*,#44473,.F.);
#65645=ORIENTED_EDGE('',*,*,#44472,.T.);
#65646=ORIENTED_EDGE('',*,*,#34060,.T.);
#65647=ORIENTED_EDGE('',*,*,#44474,.F.);
#65648=ORIENTED_EDGE('',*,*,#44473,.T.);
#65649=ORIENTED_EDGE('',*,*,#34059,.T.);
#65650=ORIENTED_EDGE('',*,*,#44475,.F.);
#65651=ORIENTED_EDGE('',*,*,#44474,.T.);
#65652=ORIENTED_EDGE('',*,*,#34058,.T.);
#65653=ORIENTED_EDGE('',*,*,#44476,.F.);
#65654=ORIENTED_EDGE('',*,*,#44475,.T.);
#65655=ORIENTED_EDGE('',*,*,#34057,.T.);
#65656=ORIENTED_EDGE('',*,*,#44305,.T.);
#65657=ORIENTED_EDGE('',*,*,#44476,.T.);
#65658=ORIENTED_EDGE('',*,*,#34056,.T.);
#65659=ORIENTED_EDGE('',*,*,#44477,.F.);
#65660=ORIENTED_EDGE('',*,*,#44306,.T.);
#65661=ORIENTED_EDGE('',*,*,#44477,.T.);
#65662=ORIENTED_EDGE('',*,*,#34055,.T.);
#65663=ORIENTED_EDGE('',*,*,#44478,.F.);
#65664=ORIENTED_EDGE('',*,*,#44479,.F.);
#65665=ORIENTED_EDGE('',*,*,#44478,.T.);
#65666=ORIENTED_EDGE('',*,*,#34054,.T.);
#65667=ORIENTED_EDGE('',*,*,#44480,.F.);
#65668=ORIENTED_EDGE('',*,*,#44479,.T.);
#65669=ORIENTED_EDGE('',*,*,#34053,.T.);
#65670=ORIENTED_EDGE('',*,*,#44481,.F.);
#65671=ORIENTED_EDGE('',*,*,#44480,.T.);
#65672=ORIENTED_EDGE('',*,*,#34052,.T.);
#65673=ORIENTED_EDGE('',*,*,#44482,.F.);
#65674=ORIENTED_EDGE('',*,*,#44481,.T.);
#65675=ORIENTED_EDGE('',*,*,#34051,.T.);
#65676=ORIENTED_EDGE('',*,*,#44482,.T.);
#65677=ORIENTED_EDGE('',*,*,#34050,.T.);
#65678=ORIENTED_EDGE('',*,*,#44309,.T.);
#65679=ORIENTED_EDGE('',*,*,#44308,.T.);
#65680=ORIENTED_EDGE('',*,*,#34149,.T.);
#65681=ORIENTED_EDGE('',*,*,#34142,.F.);
#65682=ORIENTED_EDGE('',*,*,#34139,.T.);
#65683=ORIENTED_EDGE('',*,*,#34144,.F.);
#65684=ORIENTED_EDGE('',*,*,#44483,.F.);
#65685=ORIENTED_EDGE('',*,*,#44484,.T.);
#65686=ORIENTED_EDGE('',*,*,#44485,.F.);
#65687=ORIENTED_EDGE('',*,*,#44484,.F.);
#65688=ORIENTED_EDGE('',*,*,#44486,.T.);
#65689=ORIENTED_EDGE('',*,*,#44487,.T.);
#65690=ORIENTED_EDGE('',*,*,#44488,.T.);
#65691=ORIENTED_EDGE('',*,*,#44489,.T.);
#65692=ORIENTED_EDGE('',*,*,#44490,.T.);
#65693=ORIENTED_EDGE('',*,*,#44491,.T.);
#65694=ORIENTED_EDGE('',*,*,#44492,.T.);
#65695=ORIENTED_EDGE('',*,*,#44493,.T.);
#65696=ORIENTED_EDGE('',*,*,#44494,.F.);
#65697=ORIENTED_EDGE('',*,*,#44493,.F.);
#65698=ORIENTED_EDGE('',*,*,#44495,.T.);
#65699=ORIENTED_EDGE('',*,*,#44496,.T.);
#65700=ORIENTED_EDGE('',*,*,#44497,.T.);
#65701=ORIENTED_EDGE('',*,*,#44498,.T.);
#65702=ORIENTED_EDGE('',*,*,#44499,.T.);
#65703=ORIENTED_EDGE('',*,*,#44500,.T.);
#65704=ORIENTED_EDGE('',*,*,#44501,.F.);
#65705=ORIENTED_EDGE('',*,*,#44502,.F.);
#65706=ORIENTED_EDGE('',*,*,#44503,.T.);
#65707=ORIENTED_EDGE('',*,*,#44504,.T.);
#65708=ORIENTED_EDGE('',*,*,#44503,.F.);
#65709=ORIENTED_EDGE('',*,*,#44505,.T.);
#65710=ORIENTED_EDGE('',*,*,#44506,.T.);
#65711=ORIENTED_EDGE('',*,*,#44507,.F.);
#65712=ORIENTED_EDGE('',*,*,#44488,.F.);
#65713=ORIENTED_EDGE('',*,*,#44508,.T.);
#65714=ORIENTED_EDGE('',*,*,#44499,.F.);
#65715=ORIENTED_EDGE('',*,*,#44509,.T.);
#65716=ORIENTED_EDGE('',*,*,#44510,.T.);
#65717=ORIENTED_EDGE('',*,*,#44501,.T.);
#65718=ORIENTED_EDGE('',*,*,#44502,.T.);
#65719=ORIENTED_EDGE('',*,*,#44511,.T.);
#65720=ORIENTED_EDGE('',*,*,#44512,.F.);
#65721=ORIENTED_EDGE('',*,*,#44511,.F.);
#65722=ORIENTED_EDGE('',*,*,#44513,.F.);
#65723=ORIENTED_EDGE('',*,*,#44514,.F.);
#65724=ORIENTED_EDGE('',*,*,#44515,.F.);
#65725=ORIENTED_EDGE('',*,*,#44510,.F.);
#65726=ORIENTED_EDGE('',*,*,#44512,.T.);
#65727=ORIENTED_EDGE('',*,*,#44516,.T.);
#65728=ORIENTED_EDGE('',*,*,#44517,.F.);
#65729=ORIENTED_EDGE('',*,*,#44518,.F.);
#65730=ORIENTED_EDGE('',*,*,#44505,.F.);
#65731=ORIENTED_EDGE('',*,*,#44515,.T.);
#65732=ORIENTED_EDGE('',*,*,#44519,.F.);
#65733=ORIENTED_EDGE('',*,*,#44516,.F.);
#65734=ORIENTED_EDGE('',*,*,#44485,.T.);
#65735=ORIENTED_EDGE('',*,*,#44494,.T.);
#65736=ORIENTED_EDGE('',*,*,#44483,.T.);
#65737=ORIENTED_EDGE('',*,*,#44504,.F.);
#65738=ORIENTED_EDGE('',*,*,#44520,.T.);
#65739=ORIENTED_EDGE('',*,*,#44496,.F.);
#65740=ORIENTED_EDGE('',*,*,#44521,.T.);
#65741=ORIENTED_EDGE('',*,*,#44491,.F.);
#65742=ORIENTED_EDGE('',*,*,#44520,.F.);
#65743=ORIENTED_EDGE('',*,*,#44490,.F.);
#65744=ORIENTED_EDGE('',*,*,#44522,.T.);
#65745=ORIENTED_EDGE('',*,*,#44523,.T.);
#65746=ORIENTED_EDGE('',*,*,#44517,.T.);
#65747=ORIENTED_EDGE('',*,*,#44519,.T.);
#65748=ORIENTED_EDGE('',*,*,#44514,.T.);
#65749=ORIENTED_EDGE('',*,*,#44524,.T.);
#65750=ORIENTED_EDGE('',*,*,#44497,.F.);
#65751=ORIENTED_EDGE('',*,*,#44507,.T.);
#65752=ORIENTED_EDGE('',*,*,#44525,.T.);
#65753=ORIENTED_EDGE('',*,*,#44522,.F.);
#65754=ORIENTED_EDGE('',*,*,#44489,.F.);
#65755=ORIENTED_EDGE('',*,*,#44508,.F.);
#65756=ORIENTED_EDGE('',*,*,#44487,.F.);
#65757=ORIENTED_EDGE('',*,*,#44526,.T.);
#65758=ORIENTED_EDGE('',*,*,#44500,.F.);
#65759=ORIENTED_EDGE('',*,*,#44526,.F.);
#65760=ORIENTED_EDGE('',*,*,#44486,.F.);
#65761=ORIENTED_EDGE('',*,*,#44521,.F.);
#65762=ORIENTED_EDGE('',*,*,#44495,.F.);
#65763=ORIENTED_EDGE('',*,*,#44492,.F.);
#65764=ORIENTED_EDGE('',*,*,#44524,.F.);
#65765=ORIENTED_EDGE('',*,*,#44513,.T.);
#65766=ORIENTED_EDGE('',*,*,#44509,.F.);
#65767=ORIENTED_EDGE('',*,*,#44498,.F.);
#65768=ORIENTED_EDGE('',*,*,#44506,.F.);
#65769=ORIENTED_EDGE('',*,*,#44518,.T.);
#65770=ORIENTED_EDGE('',*,*,#44523,.F.);
#65771=ORIENTED_EDGE('',*,*,#44525,.F.);
#65772=ORIENTED_EDGE('',*,*,#44527,.F.);
#65773=ORIENTED_EDGE('',*,*,#44528,.F.);
#65774=ORIENTED_EDGE('',*,*,#44529,.F.);
#65775=ORIENTED_EDGE('',*,*,#44530,.F.);
#65776=ORIENTED_EDGE('',*,*,#44531,.F.);
#65777=ORIENTED_EDGE('',*,*,#44532,.F.);
#65778=ORIENTED_EDGE('',*,*,#44533,.T.);
#65779=ORIENTED_EDGE('',*,*,#44534,.T.);
#65780=ORIENTED_EDGE('',*,*,#44535,.T.);
#65781=ORIENTED_EDGE('',*,*,#44534,.F.);
#65782=ORIENTED_EDGE('',*,*,#44536,.T.);
#65783=ORIENTED_EDGE('',*,*,#44537,.T.);
#65784=ORIENTED_EDGE('',*,*,#44538,.T.);
#65785=ORIENTED_EDGE('',*,*,#44539,.F.);
#65786=ORIENTED_EDGE('',*,*,#44538,.F.);
#65787=ORIENTED_EDGE('',*,*,#44540,.T.);
#65788=ORIENTED_EDGE('',*,*,#44541,.T.);
#65789=ORIENTED_EDGE('',*,*,#44537,.F.);
#65790=ORIENTED_EDGE('',*,*,#44541,.F.);
#65791=ORIENTED_EDGE('',*,*,#44542,.T.);
#65792=ORIENTED_EDGE('',*,*,#44543,.T.);
#65793=ORIENTED_EDGE('',*,*,#44544,.F.);
#65794=ORIENTED_EDGE('',*,*,#44545,.F.);
#65795=ORIENTED_EDGE('',*,*,#44533,.F.);
#65796=ORIENTED_EDGE('',*,*,#44546,.T.);
#65797=ORIENTED_EDGE('',*,*,#44547,.T.);
#65798=ORIENTED_EDGE('',*,*,#44546,.F.);
#65799=ORIENTED_EDGE('',*,*,#44536,.F.);
#65800=ORIENTED_EDGE('',*,*,#44548,.F.);
#65801=ORIENTED_EDGE('',*,*,#44549,.F.);
#65802=ORIENTED_EDGE('',*,*,#44550,.F.);
#65803=ORIENTED_EDGE('',*,*,#44551,.F.);
#65804=ORIENTED_EDGE('',*,*,#44552,.T.);
#65805=ORIENTED_EDGE('',*,*,#44553,.F.);
#65806=ORIENTED_EDGE('',*,*,#44554,.F.);
#65807=ORIENTED_EDGE('',*,*,#44555,.F.);
#65808=ORIENTED_EDGE('',*,*,#44556,.T.);
#65809=ORIENTED_EDGE('',*,*,#44557,.F.);
#65810=ORIENTED_EDGE('',*,*,#44558,.T.);
#65811=ORIENTED_EDGE('',*,*,#44559,.F.);
#65812=ORIENTED_EDGE('',*,*,#44560,.T.);
#65813=ORIENTED_EDGE('',*,*,#44544,.T.);
#65814=ORIENTED_EDGE('',*,*,#44561,.F.);
#65815=ORIENTED_EDGE('',*,*,#44562,.T.);
#65816=ORIENTED_EDGE('',*,*,#44545,.T.);
#65817=ORIENTED_EDGE('',*,*,#44560,.F.);
#65818=ORIENTED_EDGE('',*,*,#44563,.F.);
#65819=ORIENTED_EDGE('',*,*,#44556,.F.);
#65820=ORIENTED_EDGE('',*,*,#44543,.F.);
#65821=ORIENTED_EDGE('',*,*,#44564,.T.);
#65822=ORIENTED_EDGE('',*,*,#44565,.F.);
#65823=ORIENTED_EDGE('',*,*,#44566,.F.);
#65824=ORIENTED_EDGE('',*,*,#44558,.F.);
#65825=ORIENTED_EDGE('',*,*,#44567,.F.);
#65826=ORIENTED_EDGE('',*,*,#44568,.F.);
#65827=ORIENTED_EDGE('',*,*,#44569,.F.);
#65828=ORIENTED_EDGE('',*,*,#44564,.F.);
#65829=ORIENTED_EDGE('',*,*,#44542,.F.);
#65830=ORIENTED_EDGE('',*,*,#44562,.F.);
#65831=ORIENTED_EDGE('',*,*,#44570,.F.);
#65832=ORIENTED_EDGE('',*,*,#44571,.T.);
#65833=ORIENTED_EDGE('',*,*,#44572,.F.);
#65834=ORIENTED_EDGE('',*,*,#44573,.T.);
#65835=ORIENTED_EDGE('',*,*,#44574,.T.);
#65836=ORIENTED_EDGE('',*,*,#44575,.F.);
#65837=ORIENTED_EDGE('',*,*,#44572,.T.);
#65838=ORIENTED_EDGE('',*,*,#44576,.T.);
#65839=ORIENTED_EDGE('',*,*,#44565,.T.);
#65840=ORIENTED_EDGE('',*,*,#44577,.F.);
#65841=ORIENTED_EDGE('',*,*,#44568,.T.);
#65842=ORIENTED_EDGE('',*,*,#44578,.T.);
#65843=ORIENTED_EDGE('',*,*,#44579,.F.);
#65844=ORIENTED_EDGE('',*,*,#44580,.T.);
#65845=ORIENTED_EDGE('',*,*,#44581,.F.);
#65846=ORIENTED_EDGE('',*,*,#44582,.F.);
#65847=ORIENTED_EDGE('',*,*,#44579,.T.);
#65848=ORIENTED_EDGE('',*,*,#44555,.T.);
#65849=ORIENTED_EDGE('',*,*,#44583,.T.);
#65850=ORIENTED_EDGE('',*,*,#44574,.F.);
#65851=ORIENTED_EDGE('',*,*,#44584,.F.);
#65852=ORIENTED_EDGE('',*,*,#44585,.F.);
#65853=ORIENTED_EDGE('',*,*,#44586,.T.);
#65854=ORIENTED_EDGE('',*,*,#44551,.T.);
#65855=ORIENTED_EDGE('',*,*,#44587,.T.);
#65856=ORIENTED_EDGE('',*,*,#44550,.T.);
#65857=ORIENTED_EDGE('',*,*,#44588,.F.);
#65858=ORIENTED_EDGE('',*,*,#44589,.F.);
#65859=ORIENTED_EDGE('',*,*,#44587,.F.);
#65860=ORIENTED_EDGE('',*,*,#44540,.F.);
#65861=ORIENTED_EDGE('',*,*,#44557,.T.);
#65862=ORIENTED_EDGE('',*,*,#44563,.T.);
#65863=ORIENTED_EDGE('',*,*,#44569,.T.);
#65864=ORIENTED_EDGE('',*,*,#44577,.T.);
#65865=ORIENTED_EDGE('',*,*,#44582,.T.);
#65866=ORIENTED_EDGE('',*,*,#44590,.F.);
#65867=ORIENTED_EDGE('',*,*,#44548,.T.);
#65868=ORIENTED_EDGE('',*,*,#44584,.T.);
#65869=ORIENTED_EDGE('',*,*,#44573,.F.);
#65870=ORIENTED_EDGE('',*,*,#44575,.T.);
#65871=ORIENTED_EDGE('',*,*,#44567,.T.);
#65872=ORIENTED_EDGE('',*,*,#44539,.T.);
#65873=ORIENTED_EDGE('',*,*,#44578,.F.);
#65874=ORIENTED_EDGE('',*,*,#44570,.T.);
#65875=ORIENTED_EDGE('',*,*,#44561,.T.);
#65876=ORIENTED_EDGE('',*,*,#44559,.T.);
#65877=ORIENTED_EDGE('',*,*,#44566,.T.);
#65878=ORIENTED_EDGE('',*,*,#44576,.F.);
#65879=ORIENTED_EDGE('',*,*,#44571,.F.);
#65880=ORIENTED_EDGE('',*,*,#44583,.F.);
#65881=ORIENTED_EDGE('',*,*,#44554,.T.);
#65882=ORIENTED_EDGE('',*,*,#44591,.F.);
#65883=ORIENTED_EDGE('',*,*,#44580,.F.);
#65884=ORIENTED_EDGE('',*,*,#44547,.F.);
#65885=ORIENTED_EDGE('',*,*,#44592,.T.);
#65886=ORIENTED_EDGE('',*,*,#44593,.F.);
#65887=ORIENTED_EDGE('',*,*,#44588,.T.);
#65888=ORIENTED_EDGE('',*,*,#44549,.T.);
#65889=ORIENTED_EDGE('',*,*,#44590,.T.);
#65890=ORIENTED_EDGE('',*,*,#44581,.T.);
#65891=ORIENTED_EDGE('',*,*,#44591,.T.);
#65892=ORIENTED_EDGE('',*,*,#44553,.T.);
#65893=ORIENTED_EDGE('',*,*,#44593,.T.);
#65894=ORIENTED_EDGE('',*,*,#44594,.T.);
#65895=ORIENTED_EDGE('',*,*,#44585,.T.);
#65896=ORIENTED_EDGE('',*,*,#44589,.T.);
#65897=ORIENTED_EDGE('',*,*,#44586,.F.);
#65898=ORIENTED_EDGE('',*,*,#44594,.F.);
#65899=ORIENTED_EDGE('',*,*,#44592,.F.);
#65900=ORIENTED_EDGE('',*,*,#44552,.F.);
#65901=ORIENTED_EDGE('',*,*,#44535,.F.);
#65902=ORIENTED_EDGE('',*,*,#44595,.T.);
#65903=ORIENTED_EDGE('',*,*,#44596,.T.);
#65904=ORIENTED_EDGE('',*,*,#44597,.T.);
#65905=ORIENTED_EDGE('',*,*,#44598,.T.);
#65906=ORIENTED_EDGE('',*,*,#44599,.T.);
#65907=ORIENTED_EDGE('',*,*,#44598,.F.);
#65908=ORIENTED_EDGE('',*,*,#44600,.T.);
#65909=ORIENTED_EDGE('',*,*,#44601,.T.);
#65910=ORIENTED_EDGE('',*,*,#44596,.F.);
#65911=ORIENTED_EDGE('',*,*,#44602,.T.);
#65912=ORIENTED_EDGE('',*,*,#44603,.T.);
#65913=ORIENTED_EDGE('',*,*,#44604,.F.);
#65914=ORIENTED_EDGE('',*,*,#44605,.T.);
#65915=ORIENTED_EDGE('',*,*,#44606,.F.);
#65916=ORIENTED_EDGE('',*,*,#44607,.F.);
#65917=ORIENTED_EDGE('',*,*,#44608,.T.);
#65918=ORIENTED_EDGE('',*,*,#44609,.F.);
#65919=ORIENTED_EDGE('',*,*,#44610,.F.);
#65920=ORIENTED_EDGE('',*,*,#44611,.F.);
#65921=ORIENTED_EDGE('',*,*,#44612,.T.);
#65922=ORIENTED_EDGE('',*,*,#44606,.T.);
#65923=ORIENTED_EDGE('',*,*,#44613,.T.);
#65924=ORIENTED_EDGE('',*,*,#44614,.F.);
#65925=ORIENTED_EDGE('',*,*,#44615,.T.);
#65926=ORIENTED_EDGE('',*,*,#44604,.T.);
#65927=ORIENTED_EDGE('',*,*,#44616,.T.);
#65928=ORIENTED_EDGE('',*,*,#44617,.F.);
#65929=ORIENTED_EDGE('',*,*,#44618,.T.);
#65930=ORIENTED_EDGE('',*,*,#44607,.T.);
#65931=ORIENTED_EDGE('',*,*,#44612,.F.);
#65932=ORIENTED_EDGE('',*,*,#44619,.F.);
#65933=ORIENTED_EDGE('',*,*,#44620,.T.);
#65934=ORIENTED_EDGE('',*,*,#44621,.T.);
#65935=ORIENTED_EDGE('',*,*,#44620,.F.);
#65936=ORIENTED_EDGE('',*,*,#44610,.T.);
#65937=ORIENTED_EDGE('',*,*,#44611,.T.);
#65938=ORIENTED_EDGE('',*,*,#44622,.T.);
#65939=ORIENTED_EDGE('',*,*,#44623,.F.);
#65940=ORIENTED_EDGE('',*,*,#44622,.F.);
#65941=ORIENTED_EDGE('',*,*,#44602,.F.);
#65942=ORIENTED_EDGE('',*,*,#44603,.F.);
#65943=ORIENTED_EDGE('',*,*,#44624,.T.);
#65944=ORIENTED_EDGE('',*,*,#44619,.T.);
#65945=ORIENTED_EDGE('',*,*,#44624,.F.);
#65946=ORIENTED_EDGE('',*,*,#44623,.T.);
#65947=ORIENTED_EDGE('',*,*,#44621,.F.);
#65948=ORIENTED_EDGE('',*,*,#44625,.T.);
#65949=ORIENTED_EDGE('',*,*,#44614,.T.);
#65950=ORIENTED_EDGE('',*,*,#44626,.T.);
#65951=ORIENTED_EDGE('',*,*,#44617,.T.);
#65952=ORIENTED_EDGE('',*,*,#44609,.T.);
#65953=ORIENTED_EDGE('',*,*,#44627,.T.);
#65954=ORIENTED_EDGE('',*,*,#44600,.F.);
#65955=ORIENTED_EDGE('',*,*,#44597,.F.);
#65956=ORIENTED_EDGE('',*,*,#44601,.F.);
#65957=ORIENTED_EDGE('',*,*,#44627,.F.);
#65958=ORIENTED_EDGE('',*,*,#44615,.F.);
#65959=ORIENTED_EDGE('',*,*,#44625,.F.);
#65960=ORIENTED_EDGE('',*,*,#44613,.F.);
#65961=ORIENTED_EDGE('',*,*,#44605,.F.);
#65962=ORIENTED_EDGE('',*,*,#44595,.F.);
#65963=ORIENTED_EDGE('',*,*,#44618,.F.);
#65964=ORIENTED_EDGE('',*,*,#44626,.F.);
#65965=ORIENTED_EDGE('',*,*,#44616,.F.);
#65966=ORIENTED_EDGE('',*,*,#44608,.F.);
#65967=ORIENTED_EDGE('',*,*,#44599,.F.);
#65968=ORIENTED_EDGE('',*,*,#44628,.F.);
#65969=ORIENTED_EDGE('',*,*,#44629,.F.);
#65970=ORIENTED_EDGE('',*,*,#44630,.T.);
#65971=ORIENTED_EDGE('',*,*,#44631,.F.);
#65972=ORIENTED_EDGE('',*,*,#44632,.F.);
#65973=ORIENTED_EDGE('',*,*,#44633,.T.);
#65974=ORIENTED_EDGE('',*,*,#44634,.F.);
#65975=ORIENTED_EDGE('',*,*,#44633,.F.);
#65976=ORIENTED_EDGE('',*,*,#44635,.F.);
#65977=ORIENTED_EDGE('',*,*,#44630,.F.);
#65978=ORIENTED_EDGE('',*,*,#44636,.F.);
#65979=ORIENTED_EDGE('',*,*,#44637,.F.);
#65980=ORIENTED_EDGE('',*,*,#44634,.T.);
#65981=ORIENTED_EDGE('',*,*,#44638,.T.);
#65982=ORIENTED_EDGE('',*,*,#44639,.F.);
#65983=ORIENTED_EDGE('',*,*,#44638,.F.);
#65984=ORIENTED_EDGE('',*,*,#44628,.T.);
#65985=ORIENTED_EDGE('',*,*,#44629,.T.);
#65986=ORIENTED_EDGE('',*,*,#44640,.T.);
#65987=ORIENTED_EDGE('',*,*,#44641,.F.);
#65988=ORIENTED_EDGE('',*,*,#44640,.F.);
#65989=ORIENTED_EDGE('',*,*,#44641,.T.);
#65990=ORIENTED_EDGE('',*,*,#44639,.T.);
#65991=ORIENTED_EDGE('',*,*,#44632,.T.);
#65992=ORIENTED_EDGE('',*,*,#44642,.T.);
#65993=ORIENTED_EDGE('',*,*,#44637,.T.);
#65994=ORIENTED_EDGE('',*,*,#44636,.T.);
#65995=ORIENTED_EDGE('',*,*,#44642,.F.);
#65996=ORIENTED_EDGE('',*,*,#44631,.T.);
#65997=ORIENTED_EDGE('',*,*,#44635,.T.);
#65998=ORIENTED_EDGE('',*,*,#44643,.F.);
#65999=ORIENTED_EDGE('',*,*,#44644,.T.);
#66000=ORIENTED_EDGE('',*,*,#44645,.F.);
#66001=ORIENTED_EDGE('',*,*,#44644,.F.);
#66002=ORIENTED_EDGE('',*,*,#44643,.T.);
#66003=ORIENTED_EDGE('',*,*,#44645,.T.);
#66004=CONICAL_SURFACE('',#71473,6.75,0.785398163397449);
#66005=CONICAL_SURFACE('',#71536,6.75,0.785398163397449);
#66006=CONICAL_SURFACE('',#71544,6.125,0.785398163397448);
#66007=CONICAL_SURFACE('',#71546,6.75,0.785398163397449);
#66008=CONICAL_SURFACE('',#71606,7.31092570000179,0.78539816339742);
#66009=CONICAL_SURFACE('',#71609,7.3109256999998,0.785398163397457);
#66010=CONICAL_SURFACE('',#71619,7.31092569999943,0.785398163397357);
#66011=CONICAL_SURFACE('',#71621,7.3529052680094,0.785398163397219);
#66012=CONICAL_SURFACE('',#71631,7.46402854799594,0.785398163398244);
#66013=CONICAL_SURFACE('',#76253,7.46402854800012,0.785398163397918);
#66014=CONICAL_SURFACE('',#76262,7.46402854799495,0.785398163396894);
#66015=CONICAL_SURFACE('',#76271,7.46402854801104,0.785398163397641);
#66016=CONICAL_SURFACE('',#76280,7.46402854800908,0.785398163396339);
#66017=CONICAL_SURFACE('',#76289,7.46402854799712,0.78539816339951);
#66018=CONICAL_SURFACE('',#76298,7.46402854799119,0.785398163398774);
#66019=CONICAL_SURFACE('',#76307,7.46402854800175,0.785398163396942);
#66020=CONICAL_SURFACE('',#76316,7.46402854798451,0.78539816339517);
#66021=CONICAL_SURFACE('',#76325,7.46402854799257,0.785398163397629);
#66022=CONICAL_SURFACE('',#76334,7.46402854800718,0.785398163399594);
#66023=CONICAL_SURFACE('',#76343,7.46402854800848,0.785398163399028);
#66024=CONICAL_SURFACE('',#76352,7.46402854798724,0.785398163396677);
#66025=CONICAL_SURFACE('',#76361,7.46402854800366,0.785398163396978);
#66026=CONICAL_SURFACE('',#76370,7.46402854801209,0.78539816339822);
#66027=CONICAL_SURFACE('',#76379,7.46402854800802,0.785398163399305);
#66028=CONICAL_SURFACE('',#76388,7.46402854799688,0.785398163397931);
#66029=CONICAL_SURFACE('',#76397,7.46402854799781,0.785398163396628);
#66030=CONICAL_SURFACE('',#76406,7.46402854800837,0.785398163398763);
#66031=CONICAL_SURFACE('',#76415,7.46402854800493,0.785398163399257);
#66032=CONICAL_SURFACE('',#76424,7.46402854799559,0.785398163397219);
#66033=CONICAL_SURFACE('',#76433,7.46402854800237,0.785398163397388);
#66034=CONICAL_SURFACE('',#76442,7.46402854799716,0.785398163397943);
#66035=CONICAL_SURFACE('',#76451,7.46402854800031,0.785398163398955);
#66036=CONICAL_SURFACE('',#76460,7.46402854800001,0.785398163396978);
#66037=CONICAL_SURFACE('',#76469,7.46402854801467,0.785398163399221);
#66038=CONICAL_SURFACE('',#76478,7.46402854801943,0.785398163397738);
#66039=CONICAL_SURFACE('',#76487,7.46402854798882,0.785398163396134);
#66040=CONICAL_SURFACE('',#76496,7.46402854799016,0.785398163396424);
#66041=CONICAL_SURFACE('',#76789,7.31092570000081,0.785398163397382);
#66042=CONICAL_SURFACE('',#76790,7.31092569999921,0.785398163397411);
#66043=CONICAL_SURFACE('',#76791,7.31092569999958,0.785398163397313);
#66044=CONICAL_SURFACE('',#76792,7.3109257000012,0.785398163397469);
#66045=CONICAL_SURFACE('',#76793,7.31092570000094,0.785398163397484);
#66046=CONICAL_SURFACE('',#76794,7.31092569999998,0.78539816339753);
#66047=CONICAL_SURFACE('',#76795,7.31092570000055,0.785398163397313);
#66048=CONICAL_SURFACE('',#76796,7.31092569999908,0.785398163397528);
#66049=CONICAL_SURFACE('',#76797,7.31092570000038,0.785398163397484);
#66050=CONICAL_SURFACE('',#76798,7.31092570000067,0.785398163397379);
#66051=CONICAL_SURFACE('',#76799,7.31092569999975,0.785398163397275);
#66052=CONICAL_SURFACE('',#76800,7.3109257,0.785398163397532);
#66053=CONICAL_SURFACE('',#76801,7.31092570000065,0.785398163397496);
#66054=CONICAL_SURFACE('',#76802,7.31092569999959,0.785398163397267);
#66055=CONICAL_SURFACE('',#76803,7.31092569999963,0.785398163397375);
#66056=CONICAL_SURFACE('',#76804,7.31092569999986,0.785398163397386);
#66057=CONICAL_SURFACE('',#76805,7.31092569999971,0.785398163397473);
#66058=CONICAL_SURFACE('',#76806,7.31092569999938,0.785398163397394);
#66059=CONICAL_SURFACE('',#76807,7.31092569999932,0.785398163397628);
#66060=CONICAL_SURFACE('',#76808,7.31092569999901,0.78539816339744);
#66061=CONICAL_SURFACE('',#76809,7.31092569999891,0.785398163397488);
#66062=CONICAL_SURFACE('',#76810,7.31092569999985,0.785398163397619);
#66063=CONICAL_SURFACE('',#76811,7.31092570000066,0.785398163397634);
#66064=CONICAL_SURFACE('',#76812,7.3109256999997,0.785398163397488);
#66065=CONICAL_SURFACE('',#76813,7.31092569999926,0.785398163397338);
#66066=CONICAL_SURFACE('',#76814,7.31092570000021,0.7853981633974);
#66067=CONICAL_SURFACE('',#76815,7.31092569999984,0.785398163397532);
#66068=CONICAL_SURFACE('',#77161,7.46402854799838,0.785398163397463);
#66069=CONICAL_SURFACE('',#77170,7.46402854800787,0.785398163397463);
#66070=CONICAL_SURFACE('',#77179,7.46402854801097,0.785398163397423);
#66071=CONICAL_SURFACE('',#77188,7.46402854799594,0.785398163397718);
#66072=CONICAL_SURFACE('',#77197,7.46402854800662,0.785398163397451);
#66073=CONICAL_SURFACE('',#77206,7.46402854799811,0.785398163397486);
#66074=CONICAL_SURFACE('',#77214,7.46402854799591,0.785398163397632);
#66075=CONICAL_SURFACE('',#77218,7.46402854799987,0.785398163397621);
#66076=CONICAL_SURFACE('',#77227,7.46402854798396,0.785398163397703);
#66077=CONICAL_SURFACE('',#77236,7.46402854798974,0.785398163397734);
#66078=CONICAL_SURFACE('',#77245,7.46402854799754,0.785398163397156);
#66079=CONICAL_SURFACE('',#77254,7.46402854799756,0.785398163397393);
#66080=CONICAL_SURFACE('',#77263,7.46402854798607,0.785398163397496);
#66081=CONICAL_SURFACE('',#77272,7.46402854798888,0.7853981633974);
#66082=CONICAL_SURFACE('',#77281,7.46402854799924,0.785398163397339);
#66083=CONICAL_SURFACE('',#77290,7.46402854800191,0.785398163397406);
#66084=CONICAL_SURFACE('',#77299,7.46402854799075,0.785398163397348);
#66085=CONICAL_SURFACE('',#77308,7.46402854800954,0.785398163397388);
#66086=CONICAL_SURFACE('',#77317,7.46402854799126,0.785398163397592);
#66087=CONICAL_SURFACE('',#77326,7.46402854799435,0.785398163397487);
#66088=CONICAL_SURFACE('',#77335,7.46402854800158,0.785398163397697);
#66089=CONICAL_SURFACE('',#77344,7.4640285480086,0.785398163397334);
#66090=CONICAL_SURFACE('',#77353,7.46402854800634,0.785398163397451);
#66091=CONICAL_SURFACE('',#77362,7.4640285480148,0.785398163397331);
#66092=CONICAL_SURFACE('',#77371,7.46402854800437,0.785398163397692);
#66093=CONICAL_SURFACE('',#77380,7.46402854799968,0.785398163397385);
#66094=CONICAL_SURFACE('',#77389,7.46402854800945,0.785398163397409);
#66095=CONICAL_SURFACE('',#77398,7.46402854799185,0.785398163397598);
#66096=CONICAL_SURFACE('',#77406,7.46402854799058,0.785398163397741);
#66097=CONICAL_SURFACE('',#77502,7.31092570000008,0.785398163397451);
#66098=CONICAL_SURFACE('',#77503,7.31092570000018,0.785398163397452);
#66099=CONICAL_SURFACE('',#77504,7.31092570000096,0.785398163397458);
#66100=CONICAL_SURFACE('',#77505,7.31092569999937,0.785398163397437);
#66101=CONICAL_SURFACE('',#77506,7.31092569999996,0.785398163397438);
#66102=CONICAL_SURFACE('',#77507,7.31092569999865,0.785398163397447);
#66103=CONICAL_SURFACE('',#77508,7.31092570000104,0.785398163397416);
#66104=CONICAL_SURFACE('',#77509,7.31092569999903,0.785398163397454);
#66105=CONICAL_SURFACE('',#77510,7.31092569999917,0.785398163397461);
#66106=CONICAL_SURFACE('',#77511,7.31092569999884,0.785398163397461);
#66107=CONICAL_SURFACE('',#77512,7.31092570000051,0.78539816339743);
#66108=CONICAL_SURFACE('',#77513,7.31092569999899,0.78539816339745);
#66109=CONICAL_SURFACE('',#77514,7.31092570000054,0.785398163397441);
#66110=CONICAL_SURFACE('',#77515,7.31092569999955,0.785398163397439);
#66111=CONICAL_SURFACE('',#77516,7.31092570000009,0.785398163397455);
#66112=CONICAL_SURFACE('',#77517,7.31092569999947,0.785398163397443);
#66113=CONICAL_SURFACE('',#77518,7.31092570000149,0.785398163397419);
#66114=CONICAL_SURFACE('',#77519,7.31092570000005,0.785398163397435);
#66115=CONICAL_SURFACE('',#77520,7.31092570000153,0.785398163397446);
#66116=CONICAL_SURFACE('',#77521,7.3109256999999,0.785398163397472);
#66117=CONICAL_SURFACE('',#77522,7.31092569999987,0.785398163397457);
#66118=CONICAL_SURFACE('',#77523,7.31092569999961,0.785398163397432);
#66119=CONICAL_SURFACE('',#77524,7.31092570000154,0.785398163397434);
#66120=CONICAL_SURFACE('',#77525,7.31092569999873,0.785398163397455);
#66121=CONICAL_SURFACE('',#77526,7.31092569999843,0.785398163397445);
#66122=CONICAL_SURFACE('',#77527,7.3109256999992,0.785398163397447);
#66123=CONICAL_SURFACE('',#77528,7.31092569999984,0.785398163397452);
#66124=CONICAL_SURFACE('',#77658,5.9,0.785398163397448);
#66125=CONICAL_SURFACE('',#77660,5.40000000000002,0.785398163397455);
#66126=CONICAL_SURFACE('',#77676,5.4,0.785398163397447);
#66127=CONICAL_SURFACE('',#77686,2.50000000008162,0.78539816269889);
#66128=CONICAL_SURFACE('',#77692,2.50000000013396,0.785398162698949);
#66129=CONICAL_SURFACE('',#77727,1.65,0.785398163397448);
#66130=CONICAL_SURFACE('',#77730,3.826794919,0.52359877620608);
#66131=CONICAL_SURFACE('',#77744,2.,0.785398163397448);
#66132=CONICAL_SURFACE('',#77746,2.,0.785398163397448);
#66133=ADVANCED_FACE('',(#5383),#66004,.T.);
#66134=ADVANCED_FACE('',(#5384),#4459,.F.);
#66135=ADVANCED_FACE('',(#5385),#66005,.T.);
#66136=ADVANCED_FACE('',(#5386),#4460,.F.);
#66137=ADVANCED_FACE('',(#5387),#4461,.F.);
#66138=ADVANCED_FACE('',(#5388),#66006,.F.);
#66139=ADVANCED_FACE('',(#5389),#66007,.T.);
#66140=ADVANCED_FACE('',(#5390),#66008,.T.);
#66141=ADVANCED_FACE('',(#5391),#66009,.T.);
#66142=ADVANCED_FACE('',(#5392),#4462,.T.);
#66143=ADVANCED_FACE('',(#5393),#4463,.T.);
#66144=ADVANCED_FACE('',(#5394),#66010,.T.);
#66145=ADVANCED_FACE('',(#5395),#66011,.T.);
#66146=ADVANCED_FACE('',(#5396),#4464,.T.);
#66147=ADVANCED_FACE('',(#5397),#4465,.T.);
#66148=ADVANCED_FACE('',(#5398),#66012,.T.);
#66149=ADVANCED_FACE('',(#5399),#4466,.T.);
#66150=ADVANCED_FACE('',(#5400),#4467,.T.);
#66151=ADVANCED_FACE('',(#5401),#4468,.T.);
#66152=ADVANCED_FACE('',(#5402),#4469,.T.);
#66153=ADVANCED_FACE('',(#5403),#4470,.T.);
#66154=ADVANCED_FACE('',(#5404),#4471,.T.);
#66155=ADVANCED_FACE('',(#5405),#4472,.T.);
#66156=ADVANCED_FACE('',(#5406),#4473,.T.);
#66157=ADVANCED_FACE('',(#5407),#4474,.T.);
#66158=ADVANCED_FACE('',(#5408),#4475,.T.);
#66159=ADVANCED_FACE('',(#5409),#4476,.T.);
#66160=ADVANCED_FACE('',(#5410),#4477,.T.);
#66161=ADVANCED_FACE('',(#5411),#4478,.T.);
#66162=ADVANCED_FACE('',(#5412),#4479,.T.);
#66163=ADVANCED_FACE('',(#5413),#4480,.T.);
#66164=ADVANCED_FACE('',(#5414),#4481,.T.);
#66165=ADVANCED_FACE('',(#5415),#4482,.T.);
#66166=ADVANCED_FACE('',(#5416),#4483,.T.);
#66167=ADVANCED_FACE('',(#5417),#4484,.T.);
#66168=ADVANCED_FACE('',(#5418),#4485,.T.);
#66169=ADVANCED_FACE('',(#5419),#4486,.T.);
#66170=ADVANCED_FACE('',(#5420),#4487,.T.);
#66171=ADVANCED_FACE('',(#5421),#4488,.T.);
#66172=ADVANCED_FACE('',(#5422),#4489,.T.);
#66173=ADVANCED_FACE('',(#5423),#4490,.T.);
#66174=ADVANCED_FACE('',(#5424),#194,.T.);
#66175=ADVANCED_FACE('',(#5425),#195,.T.);
#66176=ADVANCED_FACE('',(#5426),#4491,.T.);
#66177=ADVANCED_FACE('',(#5427),#196,.T.);
#66178=ADVANCED_FACE('',(#5428),#197,.T.);
#66179=ADVANCED_FACE('',(#5429),#4492,.T.);
#66180=ADVANCED_FACE('',(#5430),#198,.T.);
#66181=ADVANCED_FACE('',(#5431),#199,.T.);
#66182=ADVANCED_FACE('',(#5432),#4493,.T.);
#66183=ADVANCED_FACE('',(#5433),#200,.T.);
#66184=ADVANCED_FACE('',(#5434),#201,.T.);
#66185=ADVANCED_FACE('',(#5435),#4494,.T.);
#66186=ADVANCED_FACE('',(#5436),#202,.T.);
#66187=ADVANCED_FACE('',(#5437),#203,.T.);
#66188=ADVANCED_FACE('',(#5438),#4495,.T.);
#66189=ADVANCED_FACE('',(#5439),#204,.T.);
#66190=ADVANCED_FACE('',(#5440),#205,.T.);
#66191=ADVANCED_FACE('',(#5441),#4496,.T.);
#66192=ADVANCED_FACE('',(#5442),#206,.T.);
#66193=ADVANCED_FACE('',(#5443),#207,.T.);
#66194=ADVANCED_FACE('',(#5444),#208,.T.);
#66195=ADVANCED_FACE('',(#5445),#209,.T.);
#66196=ADVANCED_FACE('',(#5446),#4497,.T.);
#66197=ADVANCED_FACE('',(#5447),#210,.T.);
#66198=ADVANCED_FACE('',(#5448),#211,.T.);
#66199=ADVANCED_FACE('',(#5449),#4498,.T.);
#66200=ADVANCED_FACE('',(#5450),#212,.T.);
#66201=ADVANCED_FACE('',(#5451),#213,.T.);
#66202=ADVANCED_FACE('',(#5452),#4499,.T.);
#66203=ADVANCED_FACE('',(#5453),#214,.T.);
#66204=ADVANCED_FACE('',(#5454),#215,.T.);
#66205=ADVANCED_FACE('',(#5455),#4500,.T.);
#66206=ADVANCED_FACE('',(#5456),#216,.T.);
#66207=ADVANCED_FACE('',(#5457),#217,.T.);
#66208=ADVANCED_FACE('',(#5458),#4501,.T.);
#66209=ADVANCED_FACE('',(#5459),#218,.T.);
#66210=ADVANCED_FACE('',(#5460),#219,.T.);
#66211=ADVANCED_FACE('',(#5461),#4502,.T.);
#66212=ADVANCED_FACE('',(#5462),#220,.T.);
#66213=ADVANCED_FACE('',(#5463),#221,.T.);
#66214=ADVANCED_FACE('',(#5464),#4503,.T.);
#66215=ADVANCED_FACE('',(#5465),#222,.T.);
#66216=ADVANCED_FACE('',(#5466),#223,.T.);
#66217=ADVANCED_FACE('',(#5467),#4504,.T.);
#66218=ADVANCED_FACE('',(#5468),#224,.T.);
#66219=ADVANCED_FACE('',(#5469),#225,.T.);
#66220=ADVANCED_FACE('',(#5470),#4505,.T.);
#66221=ADVANCED_FACE('',(#5471),#226,.T.);
#66222=ADVANCED_FACE('',(#5472),#227,.T.);
#66223=ADVANCED_FACE('',(#5473),#4506,.T.);
#66224=ADVANCED_FACE('',(#5474),#228,.T.);
#66225=ADVANCED_FACE('',(#5475),#229,.T.);
#66226=ADVANCED_FACE('',(#5476),#4507,.T.);
#66227=ADVANCED_FACE('',(#5477),#230,.T.);
#66228=ADVANCED_FACE('',(#5478),#231,.T.);
#66229=ADVANCED_FACE('',(#5479),#4508,.T.);
#66230=ADVANCED_FACE('',(#5480),#232,.T.);
#66231=ADVANCED_FACE('',(#5481),#233,.T.);
#66232=ADVANCED_FACE('',(#5482),#4509,.T.);
#66233=ADVANCED_FACE('',(#5483),#234,.T.);
#66234=ADVANCED_FACE('',(#5484),#235,.T.);
#66235=ADVANCED_FACE('',(#5485),#4510,.T.);
#66236=ADVANCED_FACE('',(#5486),#236,.T.);
#66237=ADVANCED_FACE('',(#5487),#237,.T.);
#66238=ADVANCED_FACE('',(#5488),#4511,.T.);
#66239=ADVANCED_FACE('',(#5489),#238,.T.);
#66240=ADVANCED_FACE('',(#5490),#239,.T.);
#66241=ADVANCED_FACE('',(#5491),#4512,.T.);
#66242=ADVANCED_FACE('',(#5492),#240,.T.);
#66243=ADVANCED_FACE('',(#5493),#241,.T.);
#66244=ADVANCED_FACE('',(#5494),#4513,.T.);
#66245=ADVANCED_FACE('',(#5495),#242,.T.);
#66246=ADVANCED_FACE('',(#5496),#243,.T.);
#66247=ADVANCED_FACE('',(#5497),#244,.T.);
#66248=ADVANCED_FACE('',(#5498),#4514,.T.);
#66249=ADVANCED_FACE('',(#5499),#245,.T.);
#66250=ADVANCED_FACE('',(#5500),#4515,.T.);
#66251=ADVANCED_FACE('',(#5501),#246,.T.);
#66252=ADVANCED_FACE('',(#5502),#247,.T.);
#66253=ADVANCED_FACE('',(#5503),#4516,.T.);
#66254=ADVANCED_FACE('',(#5504),#248,.T.);
#66255=ADVANCED_FACE('',(#5505),#249,.T.);
#66256=ADVANCED_FACE('',(#5506),#4517,.T.);
#66257=ADVANCED_FACE('',(#5507),#250,.T.);
#66258=ADVANCED_FACE('',(#5508),#4518,.T.);
#66259=ADVANCED_FACE('',(#5509),#251,.T.);
#66260=ADVANCED_FACE('',(#5510),#252,.T.);
#66261=ADVANCED_FACE('',(#5511),#253,.T.);
#66262=ADVANCED_FACE('',(#5512),#254,.T.);
#66263=ADVANCED_FACE('',(#5513),#4519,.T.);
#66264=ADVANCED_FACE('',(#5514),#255,.T.);
#66265=ADVANCED_FACE('',(#5515),#256,.T.);
#66266=ADVANCED_FACE('',(#5516),#4520,.T.);
#66267=ADVANCED_FACE('',(#5517),#257,.T.);
#66268=ADVANCED_FACE('',(#5518),#258,.T.);
#66269=ADVANCED_FACE('',(#5519),#4521,.T.);
#66270=ADVANCED_FACE('',(#5520),#259,.T.);
#66271=ADVANCED_FACE('',(#5521),#260,.T.);
#66272=ADVANCED_FACE('',(#5522),#4522,.T.);
#66273=ADVANCED_FACE('',(#5523),#261,.T.);
#66274=ADVANCED_FACE('',(#5524),#262,.T.);
#66275=ADVANCED_FACE('',(#5525),#4523,.T.);
#66276=ADVANCED_FACE('',(#5526),#263,.T.);
#66277=ADVANCED_FACE('',(#5527),#264,.T.);
#66278=ADVANCED_FACE('',(#5528),#4524,.T.);
#66279=ADVANCED_FACE('',(#5529),#265,.T.);
#66280=ADVANCED_FACE('',(#5530),#266,.T.);
#66281=ADVANCED_FACE('',(#5531),#4525,.T.);
#66282=ADVANCED_FACE('',(#5532),#267,.T.);
#66283=ADVANCED_FACE('',(#5533),#268,.T.);
#66284=ADVANCED_FACE('',(#5534),#4526,.T.);
#66285=ADVANCED_FACE('',(#5535),#269,.T.);
#66286=ADVANCED_FACE('',(#5536),#270,.T.);
#66287=ADVANCED_FACE('',(#5537),#4527,.T.);
#66288=ADVANCED_FACE('',(#5538),#271,.T.);
#66289=ADVANCED_FACE('',(#5539),#272,.T.);
#66290=ADVANCED_FACE('',(#5540),#4528,.T.);
#66291=ADVANCED_FACE('',(#5541),#273,.T.);
#66292=ADVANCED_FACE('',(#5542),#274,.T.);
#66293=ADVANCED_FACE('',(#5543),#4529,.T.);
#66294=ADVANCED_FACE('',(#5544),#275,.T.);
#66295=ADVANCED_FACE('',(#5545),#276,.T.);
#66296=ADVANCED_FACE('',(#5546),#4530,.T.);
#66297=ADVANCED_FACE('',(#5547),#277,.T.);
#66298=ADVANCED_FACE('',(#5548),#278,.T.);
#66299=ADVANCED_FACE('',(#5549),#4531,.T.);
#66300=ADVANCED_FACE('',(#5550),#279,.T.);
#66301=ADVANCED_FACE('',(#5551),#280,.T.);
#66302=ADVANCED_FACE('',(#5552),#281,.T.);
#66303=ADVANCED_FACE('',(#5553),#282,.T.);
#66304=ADVANCED_FACE('',(#5554),#4532,.T.);
#66305=ADVANCED_FACE('',(#5555),#283,.T.);
#66306=ADVANCED_FACE('',(#5556),#284,.T.);
#66307=ADVANCED_FACE('',(#5557),#4533,.T.);
#66308=ADVANCED_FACE('',(#5558),#285,.T.);
#66309=ADVANCED_FACE('',(#5559),#286,.T.);
#66310=ADVANCED_FACE('',(#5560),#4534,.T.);
#66311=ADVANCED_FACE('',(#5561),#287,.T.);
#66312=ADVANCED_FACE('',(#5562),#288,.T.);
#66313=ADVANCED_FACE('',(#5563),#4535,.T.);
#66314=ADVANCED_FACE('',(#5564),#289,.T.);
#66315=ADVANCED_FACE('',(#5565),#290,.T.);
#66316=ADVANCED_FACE('',(#5566),#4536,.T.);
#66317=ADVANCED_FACE('',(#5567),#291,.T.);
#66318=ADVANCED_FACE('',(#5568),#292,.T.);
#66319=ADVANCED_FACE('',(#5569),#4537,.T.);
#66320=ADVANCED_FACE('',(#5570),#293,.T.);
#66321=ADVANCED_FACE('',(#5571),#294,.T.);
#66322=ADVANCED_FACE('',(#5572),#4538,.T.);
#66323=ADVANCED_FACE('',(#5573),#295,.T.);
#66324=ADVANCED_FACE('',(#5574),#296,.T.);
#66325=ADVANCED_FACE('',(#5575),#4539,.T.);
#66326=ADVANCED_FACE('',(#5576),#297,.T.);
#66327=ADVANCED_FACE('',(#5577),#298,.T.);
#66328=ADVANCED_FACE('',(#5578),#4540,.T.);
#66329=ADVANCED_FACE('',(#5579),#299,.T.);
#66330=ADVANCED_FACE('',(#5580),#300,.T.);
#66331=ADVANCED_FACE('',(#5581),#4541,.T.);
#66332=ADVANCED_FACE('',(#5582),#301,.T.);
#66333=ADVANCED_FACE('',(#5583),#302,.T.);
#66334=ADVANCED_FACE('',(#5584),#4542,.T.);
#66335=ADVANCED_FACE('',(#5585),#303,.T.);
#66336=ADVANCED_FACE('',(#5586),#304,.T.);
#66337=ADVANCED_FACE('',(#5587),#4543,.T.);
#66338=ADVANCED_FACE('',(#5588),#305,.T.);
#66339=ADVANCED_FACE('',(#5589),#306,.T.);
#66340=ADVANCED_FACE('',(#5590),#4544,.T.);
#66341=ADVANCED_FACE('',(#5591),#307,.T.);
#66342=ADVANCED_FACE('',(#5592),#308,.T.);
#66343=ADVANCED_FACE('',(#5593),#4545,.T.);
#66344=ADVANCED_FACE('',(#5594),#4546,.T.);
#66345=ADVANCED_FACE('',(#5595),#309,.T.);
#66346=ADVANCED_FACE('',(#5596),#310,.T.);
#66347=ADVANCED_FACE('',(#5597),#311,.T.);
#66348=ADVANCED_FACE('',(#5598),#312,.T.);
#66349=ADVANCED_FACE('',(#5599),#313,.T.);
#66350=ADVANCED_FACE('',(#5600),#314,.T.);
#66351=ADVANCED_FACE('',(#5601),#315,.T.);
#66352=ADVANCED_FACE('',(#5602),#316,.T.);
#66353=ADVANCED_FACE('',(#5603),#317,.T.);
#66354=ADVANCED_FACE('',(#5604),#318,.T.);
#66355=ADVANCED_FACE('',(#5605),#319,.T.);
#66356=ADVANCED_FACE('',(#5606),#320,.T.);
#66357=ADVANCED_FACE('',(#5607),#321,.T.);
#66358=ADVANCED_FACE('',(#5608),#322,.T.);
#66359=ADVANCED_FACE('',(#5609),#323,.T.);
#66360=ADVANCED_FACE('',(#5610),#324,.T.);
#66361=ADVANCED_FACE('',(#5611),#325,.T.);
#66362=ADVANCED_FACE('',(#5612),#326,.T.);
#66363=ADVANCED_FACE('',(#5613),#327,.T.);
#66364=ADVANCED_FACE('',(#5614),#328,.T.);
#66365=ADVANCED_FACE('',(#5615),#329,.T.);
#66366=ADVANCED_FACE('',(#5616),#330,.T.);
#66367=ADVANCED_FACE('',(#5617),#331,.T.);
#66368=ADVANCED_FACE('',(#5618),#332,.T.);
#66369=ADVANCED_FACE('',(#5619),#333,.T.);
#66370=ADVANCED_FACE('',(#5620),#334,.T.);
#66371=ADVANCED_FACE('',(#5621),#335,.T.);
#66372=ADVANCED_FACE('',(#5622),#336,.T.);
#66373=ADVANCED_FACE('',(#5623),#337,.T.);
#66374=ADVANCED_FACE('',(#5624),#338,.T.);
#66375=ADVANCED_FACE('',(#5625),#339,.T.);
#66376=ADVANCED_FACE('',(#5626),#340,.T.);
#66377=ADVANCED_FACE('',(#5627),#341,.T.);
#66378=ADVANCED_FACE('',(#5628),#342,.T.);
#66379=ADVANCED_FACE('',(#5629),#343,.T.);
#66380=ADVANCED_FACE('',(#5630),#344,.T.);
#66381=ADVANCED_FACE('',(#5631),#345,.T.);
#66382=ADVANCED_FACE('',(#5632),#346,.T.);
#66383=ADVANCED_FACE('',(#5633),#347,.T.);
#66384=ADVANCED_FACE('',(#5634),#348,.T.);
#66385=ADVANCED_FACE('',(#5635),#349,.T.);
#66386=ADVANCED_FACE('',(#5636),#350,.T.);
#66387=ADVANCED_FACE('',(#5637),#351,.T.);
#66388=ADVANCED_FACE('',(#5638),#352,.T.);
#66389=ADVANCED_FACE('',(#5639),#353,.T.);
#66390=ADVANCED_FACE('',(#5640),#354,.T.);
#66391=ADVANCED_FACE('',(#5641),#355,.T.);
#66392=ADVANCED_FACE('',(#5642),#356,.T.);
#66393=ADVANCED_FACE('',(#5643),#357,.T.);
#66394=ADVANCED_FACE('',(#5644),#358,.T.);
#66395=ADVANCED_FACE('',(#5645),#359,.T.);
#66396=ADVANCED_FACE('',(#5646),#360,.T.);
#66397=ADVANCED_FACE('',(#5647),#361,.T.);
#66398=ADVANCED_FACE('',(#5648),#362,.T.);
#66399=ADVANCED_FACE('',(#5649),#363,.T.);
#66400=ADVANCED_FACE('',(#5650),#364,.T.);
#66401=ADVANCED_FACE('',(#5651),#365,.T.);
#66402=ADVANCED_FACE('',(#5652),#366,.T.);
#66403=ADVANCED_FACE('',(#5653),#367,.T.);
#66404=ADVANCED_FACE('',(#5654),#368,.T.);
#66405=ADVANCED_FACE('',(#5655),#369,.T.);
#66406=ADVANCED_FACE('',(#5656),#370,.T.);
#66407=ADVANCED_FACE('',(#5657),#371,.T.);
#66408=ADVANCED_FACE('',(#5658),#372,.T.);
#66409=ADVANCED_FACE('',(#5659),#373,.T.);
#66410=ADVANCED_FACE('',(#5660),#374,.T.);
#66411=ADVANCED_FACE('',(#5661),#375,.T.);
#66412=ADVANCED_FACE('',(#5662),#376,.T.);
#66413=ADVANCED_FACE('',(#5663),#377,.T.);
#66414=ADVANCED_FACE('',(#5664),#378,.T.);
#66415=ADVANCED_FACE('',(#5665),#379,.T.);
#66416=ADVANCED_FACE('',(#5666),#380,.T.);
#66417=ADVANCED_FACE('',(#5667),#381,.T.);
#66418=ADVANCED_FACE('',(#5668),#382,.T.);
#66419=ADVANCED_FACE('',(#5669),#383,.T.);
#66420=ADVANCED_FACE('',(#5670),#384,.T.);
#66421=ADVANCED_FACE('',(#5671),#385,.T.);
#66422=ADVANCED_FACE('',(#5672),#386,.T.);
#66423=ADVANCED_FACE('',(#5673),#387,.T.);
#66424=ADVANCED_FACE('',(#5674),#388,.T.);
#66425=ADVANCED_FACE('',(#5675),#389,.T.);
#66426=ADVANCED_FACE('',(#5676),#390,.T.);
#66427=ADVANCED_FACE('',(#5677),#391,.T.);
#66428=ADVANCED_FACE('',(#5678),#392,.T.);
#66429=ADVANCED_FACE('',(#5679),#393,.T.);
#66430=ADVANCED_FACE('',(#5680),#394,.T.);
#66431=ADVANCED_FACE('',(#5681),#395,.T.);
#66432=ADVANCED_FACE('',(#5682),#396,.T.);
#66433=ADVANCED_FACE('',(#5683),#397,.T.);
#66434=ADVANCED_FACE('',(#5684),#398,.T.);
#66435=ADVANCED_FACE('',(#5685),#399,.T.);
#66436=ADVANCED_FACE('',(#5686),#400,.T.);
#66437=ADVANCED_FACE('',(#5687),#401,.T.);
#66438=ADVANCED_FACE('',(#5688),#402,.T.);
#66439=ADVANCED_FACE('',(#5689),#403,.T.);
#66440=ADVANCED_FACE('',(#5690),#404,.T.);
#66441=ADVANCED_FACE('',(#5691),#405,.T.);
#66442=ADVANCED_FACE('',(#5692),#406,.T.);
#66443=ADVANCED_FACE('',(#5693),#407,.T.);
#66444=ADVANCED_FACE('',(#5694),#408,.T.);
#66445=ADVANCED_FACE('',(#5695),#409,.T.);
#66446=ADVANCED_FACE('',(#5696),#410,.T.);
#66447=ADVANCED_FACE('',(#5697),#411,.T.);
#66448=ADVANCED_FACE('',(#5698),#412,.T.);
#66449=ADVANCED_FACE('',(#5699),#413,.T.);
#66450=ADVANCED_FACE('',(#5700),#414,.T.);
#66451=ADVANCED_FACE('',(#5701),#415,.T.);
#66452=ADVANCED_FACE('',(#5702),#416,.T.);
#66453=ADVANCED_FACE('',(#5703),#417,.T.);
#66454=ADVANCED_FACE('',(#5704),#418,.T.);
#66455=ADVANCED_FACE('',(#5705),#419,.T.);
#66456=ADVANCED_FACE('',(#5706),#420,.T.);
#66457=ADVANCED_FACE('',(#5707),#421,.T.);
#66458=ADVANCED_FACE('',(#5708),#422,.T.);
#66459=ADVANCED_FACE('',(#5709),#423,.T.);
#66460=ADVANCED_FACE('',(#5710),#424,.T.);
#66461=ADVANCED_FACE('',(#5711),#425,.T.);
#66462=ADVANCED_FACE('',(#5712),#426,.T.);
#66463=ADVANCED_FACE('',(#5713),#4547,.T.);
#66464=ADVANCED_FACE('',(#5714),#427,.T.);
#66465=ADVANCED_FACE('',(#5715),#428,.T.);
#66466=ADVANCED_FACE('',(#5716),#4548,.T.);
#66467=ADVANCED_FACE('',(#5717),#429,.T.);
#66468=ADVANCED_FACE('',(#5718),#430,.T.);
#66469=ADVANCED_FACE('',(#5719),#4549,.T.);
#66470=ADVANCED_FACE('',(#5720),#431,.T.);
#66471=ADVANCED_FACE('',(#5721),#432,.T.);
#66472=ADVANCED_FACE('',(#5722),#4550,.T.);
#66473=ADVANCED_FACE('',(#5723),#433,.T.);
#66474=ADVANCED_FACE('',(#5724),#434,.T.);
#66475=ADVANCED_FACE('',(#5725),#4551,.T.);
#66476=ADVANCED_FACE('',(#5726),#435,.T.);
#66477=ADVANCED_FACE('',(#5727),#436,.T.);
#66478=ADVANCED_FACE('',(#5728),#4552,.T.);
#66479=ADVANCED_FACE('',(#5729),#437,.T.);
#66480=ADVANCED_FACE('',(#5730),#438,.T.);
#66481=ADVANCED_FACE('',(#5731),#4553,.T.);
#66482=ADVANCED_FACE('',(#5732),#439,.T.);
#66483=ADVANCED_FACE('',(#5733),#440,.T.);
#66484=ADVANCED_FACE('',(#5734),#4554,.T.);
#66485=ADVANCED_FACE('',(#5735),#441,.T.);
#66486=ADVANCED_FACE('',(#5736),#442,.T.);
#66487=ADVANCED_FACE('',(#5737),#4555,.T.);
#66488=ADVANCED_FACE('',(#5738),#443,.T.);
#66489=ADVANCED_FACE('',(#5739),#444,.T.);
#66490=ADVANCED_FACE('',(#5740),#4556,.T.);
#66491=ADVANCED_FACE('',(#5741),#445,.T.);
#66492=ADVANCED_FACE('',(#5742),#446,.T.);
#66493=ADVANCED_FACE('',(#5743),#4557,.T.);
#66494=ADVANCED_FACE('',(#5744),#447,.T.);
#66495=ADVANCED_FACE('',(#5745),#448,.T.);
#66496=ADVANCED_FACE('',(#5746),#4558,.T.);
#66497=ADVANCED_FACE('',(#5747),#449,.T.);
#66498=ADVANCED_FACE('',(#5748),#450,.T.);
#66499=ADVANCED_FACE('',(#5749),#4559,.T.);
#66500=ADVANCED_FACE('',(#5750),#451,.T.);
#66501=ADVANCED_FACE('',(#5751),#452,.T.);
#66502=ADVANCED_FACE('',(#5752),#4560,.T.);
#66503=ADVANCED_FACE('',(#5753),#453,.T.);
#66504=ADVANCED_FACE('',(#5754),#454,.T.);
#66505=ADVANCED_FACE('',(#5755),#455,.T.);
#66506=ADVANCED_FACE('',(#5756),#456,.T.);
#66507=ADVANCED_FACE('',(#5757),#4561,.T.);
#66508=ADVANCED_FACE('',(#5758),#457,.T.);
#66509=ADVANCED_FACE('',(#5759),#458,.T.);
#66510=ADVANCED_FACE('',(#5760),#4562,.T.);
#66511=ADVANCED_FACE('',(#5761),#459,.T.);
#66512=ADVANCED_FACE('',(#5762),#460,.T.);
#66513=ADVANCED_FACE('',(#5763),#4563,.T.);
#66514=ADVANCED_FACE('',(#5764),#461,.T.);
#66515=ADVANCED_FACE('',(#5765),#462,.T.);
#66516=ADVANCED_FACE('',(#5766),#4564,.T.);
#66517=ADVANCED_FACE('',(#5767),#463,.T.);
#66518=ADVANCED_FACE('',(#5768),#464,.T.);
#66519=ADVANCED_FACE('',(#5769),#4565,.T.);
#66520=ADVANCED_FACE('',(#5770),#465,.T.);
#66521=ADVANCED_FACE('',(#5771),#466,.T.);
#66522=ADVANCED_FACE('',(#5772),#4566,.T.);
#66523=ADVANCED_FACE('',(#5773),#467,.T.);
#66524=ADVANCED_FACE('',(#5774),#468,.T.);
#66525=ADVANCED_FACE('',(#5775),#4567,.T.);
#66526=ADVANCED_FACE('',(#5776),#469,.T.);
#66527=ADVANCED_FACE('',(#5777),#470,.T.);
#66528=ADVANCED_FACE('',(#5778),#4568,.T.);
#66529=ADVANCED_FACE('',(#5779),#471,.T.);
#66530=ADVANCED_FACE('',(#5780),#472,.T.);
#66531=ADVANCED_FACE('',(#5781),#4569,.T.);
#66532=ADVANCED_FACE('',(#5782),#473,.T.);
#66533=ADVANCED_FACE('',(#5783),#474,.T.);
#66534=ADVANCED_FACE('',(#5784),#475,.T.);
#66535=ADVANCED_FACE('',(#5785),#4570,.T.);
#66536=ADVANCED_FACE('',(#5786),#476,.T.);
#66537=ADVANCED_FACE('',(#5787),#4571,.T.);
#66538=ADVANCED_FACE('',(#5788),#477,.T.);
#66539=ADVANCED_FACE('',(#5789),#478,.T.);
#66540=ADVANCED_FACE('',(#5790),#4572,.T.);
#66541=ADVANCED_FACE('',(#5791),#479,.T.);
#66542=ADVANCED_FACE('',(#5792),#480,.T.);
#66543=ADVANCED_FACE('',(#5793),#4573,.T.);
#66544=ADVANCED_FACE('',(#5794),#481,.T.);
#66545=ADVANCED_FACE('',(#5795),#482,.T.);
#66546=ADVANCED_FACE('',(#5796),#4574,.T.);
#66547=ADVANCED_FACE('',(#5797),#483,.T.);
#66548=ADVANCED_FACE('',(#5798),#484,.T.);
#66549=ADVANCED_FACE('',(#5799),#485,.T.);
#66550=ADVANCED_FACE('',(#5800),#4575,.T.);
#66551=ADVANCED_FACE('',(#5801),#486,.T.);
#66552=ADVANCED_FACE('',(#5802),#487,.T.);
#66553=ADVANCED_FACE('',(#5803),#4576,.T.);
#66554=ADVANCED_FACE('',(#5804),#488,.T.);
#66555=ADVANCED_FACE('',(#5805),#489,.T.);
#66556=ADVANCED_FACE('',(#5806),#4577,.T.);
#66557=ADVANCED_FACE('',(#5807),#490,.T.);
#66558=ADVANCED_FACE('',(#5808),#491,.T.);
#66559=ADVANCED_FACE('',(#5809),#4578,.T.);
#66560=ADVANCED_FACE('',(#5810),#492,.T.);
#66561=ADVANCED_FACE('',(#5811),#493,.T.);
#66562=ADVANCED_FACE('',(#5812),#4579,.T.);
#66563=ADVANCED_FACE('',(#5813),#494,.T.);
#66564=ADVANCED_FACE('',(#5814),#495,.T.);
#66565=ADVANCED_FACE('',(#5815),#4580,.T.);
#66566=ADVANCED_FACE('',(#5816),#496,.T.);
#66567=ADVANCED_FACE('',(#5817),#497,.T.);
#66568=ADVANCED_FACE('',(#5818),#4581,.T.);
#66569=ADVANCED_FACE('',(#5819),#498,.T.);
#66570=ADVANCED_FACE('',(#5820),#499,.T.);
#66571=ADVANCED_FACE('',(#5821),#4582,.T.);
#66572=ADVANCED_FACE('',(#5822),#500,.T.);
#66573=ADVANCED_FACE('',(#5823),#501,.T.);
#66574=ADVANCED_FACE('',(#5824),#4583,.T.);
#66575=ADVANCED_FACE('',(#5825),#502,.T.);
#66576=ADVANCED_FACE('',(#5826),#503,.T.);
#66577=ADVANCED_FACE('',(#5827),#4584,.T.);
#66578=ADVANCED_FACE('',(#5828),#504,.T.);
#66579=ADVANCED_FACE('',(#5829),#505,.T.);
#66580=ADVANCED_FACE('',(#5830),#4585,.T.);
#66581=ADVANCED_FACE('',(#5831),#506,.T.);
#66582=ADVANCED_FACE('',(#5832),#507,.T.);
#66583=ADVANCED_FACE('',(#5833),#4586,.T.);
#66584=ADVANCED_FACE('',(#5834),#508,.T.);
#66585=ADVANCED_FACE('',(#5835),#509,.T.);
#66586=ADVANCED_FACE('',(#5836),#4587,.T.);
#66587=ADVANCED_FACE('',(#5837),#510,.T.);
#66588=ADVANCED_FACE('',(#5838),#511,.T.);
#66589=ADVANCED_FACE('',(#5839),#4588,.T.);
#66590=ADVANCED_FACE('',(#5840),#512,.T.);
#66591=ADVANCED_FACE('',(#5841),#513,.T.);
#66592=ADVANCED_FACE('',(#5842),#4589,.T.);
#66593=ADVANCED_FACE('',(#5843),#514,.T.);
#66594=ADVANCED_FACE('',(#5844),#515,.T.);
#66595=ADVANCED_FACE('',(#5845),#4590,.T.);
#66596=ADVANCED_FACE('',(#5846),#516,.T.);
#66597=ADVANCED_FACE('',(#5847),#517,.T.);
#66598=ADVANCED_FACE('',(#5848),#4591,.T.);
#66599=ADVANCED_FACE('',(#5849),#518,.T.);
#66600=ADVANCED_FACE('',(#5850),#519,.T.);
#66601=ADVANCED_FACE('',(#5851),#4592,.T.);
#66602=ADVANCED_FACE('',(#5852),#520,.T.);
#66603=ADVANCED_FACE('',(#5853),#521,.T.);
#66604=ADVANCED_FACE('',(#5854),#4593,.T.);
#66605=ADVANCED_FACE('',(#5855),#522,.T.);
#66606=ADVANCED_FACE('',(#5856),#523,.T.);
#66607=ADVANCED_FACE('',(#5857),#4594,.T.);
#66608=ADVANCED_FACE('',(#5858),#524,.T.);
#66609=ADVANCED_FACE('',(#5859),#525,.T.);
#66610=ADVANCED_FACE('',(#5860),#4595,.T.);
#66611=ADVANCED_FACE('',(#5861),#526,.T.);
#66612=ADVANCED_FACE('',(#5862),#527,.T.);
#66613=ADVANCED_FACE('',(#5863),#528,.T.);
#66614=ADVANCED_FACE('',(#5864),#529,.T.);
#66615=ADVANCED_FACE('',(#5865),#4596,.T.);
#66616=ADVANCED_FACE('',(#5866),#530,.T.);
#66617=ADVANCED_FACE('',(#5867),#531,.T.);
#66618=ADVANCED_FACE('',(#5868),#4597,.T.);
#66619=ADVANCED_FACE('',(#5869),#532,.T.);
#66620=ADVANCED_FACE('',(#5870),#533,.T.);
#66621=ADVANCED_FACE('',(#5871),#4598,.T.);
#66622=ADVANCED_FACE('',(#5872),#534,.T.);
#66623=ADVANCED_FACE('',(#5873),#535,.T.);
#66624=ADVANCED_FACE('',(#5874),#4599,.T.);
#66625=ADVANCED_FACE('',(#5875),#536,.T.);
#66626=ADVANCED_FACE('',(#5876),#537,.T.);
#66627=ADVANCED_FACE('',(#5877),#4600,.T.);
#66628=ADVANCED_FACE('',(#5878),#538,.T.);
#66629=ADVANCED_FACE('',(#5879),#539,.T.);
#66630=ADVANCED_FACE('',(#5880),#4601,.T.);
#66631=ADVANCED_FACE('',(#5881),#540,.T.);
#66632=ADVANCED_FACE('',(#5882),#541,.T.);
#66633=ADVANCED_FACE('',(#5883),#4602,.T.);
#66634=ADVANCED_FACE('',(#5884),#542,.T.);
#66635=ADVANCED_FACE('',(#5885),#543,.T.);
#66636=ADVANCED_FACE('',(#5886),#544,.T.);
#66637=ADVANCED_FACE('',(#5887),#545,.T.);
#66638=ADVANCED_FACE('',(#5888),#546,.T.);
#66639=ADVANCED_FACE('',(#5889),#547,.T.);
#66640=ADVANCED_FACE('',(#5890),#548,.T.);
#66641=ADVANCED_FACE('',(#5891),#549,.T.);
#66642=ADVANCED_FACE('',(#5892),#550,.T.);
#66643=ADVANCED_FACE('',(#5893),#551,.T.);
#66644=ADVANCED_FACE('',(#5894),#552,.T.);
#66645=ADVANCED_FACE('',(#5895),#553,.T.);
#66646=ADVANCED_FACE('',(#5896),#554,.T.);
#66647=ADVANCED_FACE('',(#5897),#555,.T.);
#66648=ADVANCED_FACE('',(#5898),#556,.T.);
#66649=ADVANCED_FACE('',(#5899),#557,.T.);
#66650=ADVANCED_FACE('',(#5900),#558,.T.);
#66651=ADVANCED_FACE('',(#5901),#559,.T.);
#66652=ADVANCED_FACE('',(#5902),#560,.T.);
#66653=ADVANCED_FACE('',(#5903),#561,.T.);
#66654=ADVANCED_FACE('',(#5904),#562,.T.);
#66655=ADVANCED_FACE('',(#5905),#563,.T.);
#66656=ADVANCED_FACE('',(#5906),#564,.T.);
#66657=ADVANCED_FACE('',(#5907),#565,.T.);
#66658=ADVANCED_FACE('',(#5908),#566,.T.);
#66659=ADVANCED_FACE('',(#5909),#567,.T.);
#66660=ADVANCED_FACE('',(#5910),#568,.T.);
#66661=ADVANCED_FACE('',(#5911),#569,.T.);
#66662=ADVANCED_FACE('',(#5912),#570,.T.);
#66663=ADVANCED_FACE('',(#5913),#571,.T.);
#66664=ADVANCED_FACE('',(#5914),#572,.T.);
#66665=ADVANCED_FACE('',(#5915),#573,.T.);
#66666=ADVANCED_FACE('',(#5916),#574,.T.);
#66667=ADVANCED_FACE('',(#5917),#575,.T.);
#66668=ADVANCED_FACE('',(#5918),#576,.T.);
#66669=ADVANCED_FACE('',(#5919),#577,.T.);
#66670=ADVANCED_FACE('',(#5920),#578,.T.);
#66671=ADVANCED_FACE('',(#5921),#579,.T.);
#66672=ADVANCED_FACE('',(#5922),#580,.T.);
#66673=ADVANCED_FACE('',(#5923),#581,.T.);
#66674=ADVANCED_FACE('',(#5924),#582,.T.);
#66675=ADVANCED_FACE('',(#5925),#583,.T.);
#66676=ADVANCED_FACE('',(#5926),#584,.T.);
#66677=ADVANCED_FACE('',(#5927),#585,.T.);
#66678=ADVANCED_FACE('',(#5928),#586,.T.);
#66679=ADVANCED_FACE('',(#5929),#587,.T.);
#66680=ADVANCED_FACE('',(#5930),#588,.T.);
#66681=ADVANCED_FACE('',(#5931),#589,.T.);
#66682=ADVANCED_FACE('',(#5932),#590,.T.);
#66683=ADVANCED_FACE('',(#5933),#591,.T.);
#66684=ADVANCED_FACE('',(#5934),#592,.T.);
#66685=ADVANCED_FACE('',(#5935),#593,.T.);
#66686=ADVANCED_FACE('',(#5936),#594,.T.);
#66687=ADVANCED_FACE('',(#5937),#595,.T.);
#66688=ADVANCED_FACE('',(#5938),#596,.T.);
#66689=ADVANCED_FACE('',(#5939),#597,.T.);
#66690=ADVANCED_FACE('',(#5940),#598,.T.);
#66691=ADVANCED_FACE('',(#5941),#599,.T.);
#66692=ADVANCED_FACE('',(#5942),#600,.T.);
#66693=ADVANCED_FACE('',(#5943),#601,.T.);
#66694=ADVANCED_FACE('',(#5944),#602,.T.);
#66695=ADVANCED_FACE('',(#5945),#603,.T.);
#66696=ADVANCED_FACE('',(#5946),#604,.T.);
#66697=ADVANCED_FACE('',(#5947),#605,.T.);
#66698=ADVANCED_FACE('',(#5948),#606,.T.);
#66699=ADVANCED_FACE('',(#5949),#607,.T.);
#66700=ADVANCED_FACE('',(#5950),#608,.T.);
#66701=ADVANCED_FACE('',(#5951),#609,.T.);
#66702=ADVANCED_FACE('',(#5952),#610,.T.);
#66703=ADVANCED_FACE('',(#5953),#611,.T.);
#66704=ADVANCED_FACE('',(#5954),#612,.T.);
#66705=ADVANCED_FACE('',(#5955),#613,.T.);
#66706=ADVANCED_FACE('',(#5956),#614,.T.);
#66707=ADVANCED_FACE('',(#5957),#615,.T.);
#66708=ADVANCED_FACE('',(#5958),#616,.T.);
#66709=ADVANCED_FACE('',(#5959),#617,.T.);
#66710=ADVANCED_FACE('',(#5960),#618,.T.);
#66711=ADVANCED_FACE('',(#5961),#619,.T.);
#66712=ADVANCED_FACE('',(#5962),#620,.T.);
#66713=ADVANCED_FACE('',(#5963),#621,.T.);
#66714=ADVANCED_FACE('',(#5964),#622,.T.);
#66715=ADVANCED_FACE('',(#5965),#623,.T.);
#66716=ADVANCED_FACE('',(#5966),#624,.T.);
#66717=ADVANCED_FACE('',(#5967),#625,.T.);
#66718=ADVANCED_FACE('',(#5968),#626,.T.);
#66719=ADVANCED_FACE('',(#5969),#627,.T.);
#66720=ADVANCED_FACE('',(#5970),#628,.T.);
#66721=ADVANCED_FACE('',(#5971),#629,.T.);
#66722=ADVANCED_FACE('',(#5972),#630,.T.);
#66723=ADVANCED_FACE('',(#5973),#631,.T.);
#66724=ADVANCED_FACE('',(#5974),#632,.T.);
#66725=ADVANCED_FACE('',(#5975),#633,.T.);
#66726=ADVANCED_FACE('',(#5976),#634,.T.);
#66727=ADVANCED_FACE('',(#5977),#635,.T.);
#66728=ADVANCED_FACE('',(#5978),#636,.T.);
#66729=ADVANCED_FACE('',(#5979),#637,.T.);
#66730=ADVANCED_FACE('',(#5980),#638,.T.);
#66731=ADVANCED_FACE('',(#5981),#639,.T.);
#66732=ADVANCED_FACE('',(#5982),#640,.T.);
#66733=ADVANCED_FACE('',(#5983),#641,.T.);
#66734=ADVANCED_FACE('',(#5984),#642,.T.);
#66735=ADVANCED_FACE('',(#5985),#643,.T.);
#66736=ADVANCED_FACE('',(#5986),#644,.T.);
#66737=ADVANCED_FACE('',(#5987),#645,.T.);
#66738=ADVANCED_FACE('',(#5988),#646,.T.);
#66739=ADVANCED_FACE('',(#5989),#647,.T.);
#66740=ADVANCED_FACE('',(#5990),#648,.T.);
#66741=ADVANCED_FACE('',(#5991),#649,.T.);
#66742=ADVANCED_FACE('',(#5992),#650,.T.);
#66743=ADVANCED_FACE('',(#5993),#651,.T.);
#66744=ADVANCED_FACE('',(#5994),#652,.T.);
#66745=ADVANCED_FACE('',(#5995),#653,.T.);
#66746=ADVANCED_FACE('',(#5996),#654,.T.);
#66747=ADVANCED_FACE('',(#5997),#655,.T.);
#66748=ADVANCED_FACE('',(#5998),#656,.T.);
#66749=ADVANCED_FACE('',(#5999),#657,.T.);
#66750=ADVANCED_FACE('',(#6000),#658,.T.);
#66751=ADVANCED_FACE('',(#6001),#659,.T.);
#66752=ADVANCED_FACE('',(#6002),#4603,.T.);
#66753=ADVANCED_FACE('',(#6003),#660,.T.);
#66754=ADVANCED_FACE('',(#6004),#661,.T.);
#66755=ADVANCED_FACE('',(#6005),#4604,.T.);
#66756=ADVANCED_FACE('',(#6006),#662,.T.);
#66757=ADVANCED_FACE('',(#6007),#663,.T.);
#66758=ADVANCED_FACE('',(#6008),#4605,.T.);
#66759=ADVANCED_FACE('',(#6009),#664,.T.);
#66760=ADVANCED_FACE('',(#6010),#665,.T.);
#66761=ADVANCED_FACE('',(#6011),#4606,.T.);
#66762=ADVANCED_FACE('',(#6012),#666,.T.);
#66763=ADVANCED_FACE('',(#6013),#667,.T.);
#66764=ADVANCED_FACE('',(#6014),#4607,.T.);
#66765=ADVANCED_FACE('',(#6015),#668,.T.);
#66766=ADVANCED_FACE('',(#6016),#669,.T.);
#66767=ADVANCED_FACE('',(#6017),#4608,.T.);
#66768=ADVANCED_FACE('',(#6018),#670,.T.);
#66769=ADVANCED_FACE('',(#6019),#671,.T.);
#66770=ADVANCED_FACE('',(#6020),#672,.T.);
#66771=ADVANCED_FACE('',(#6021),#673,.T.);
#66772=ADVANCED_FACE('',(#6022),#4609,.T.);
#66773=ADVANCED_FACE('',(#6023),#674,.T.);
#66774=ADVANCED_FACE('',(#6024),#675,.T.);
#66775=ADVANCED_FACE('',(#6025),#4610,.T.);
#66776=ADVANCED_FACE('',(#6026),#676,.T.);
#66777=ADVANCED_FACE('',(#6027),#677,.T.);
#66778=ADVANCED_FACE('',(#6028),#4611,.T.);
#66779=ADVANCED_FACE('',(#6029),#678,.T.);
#66780=ADVANCED_FACE('',(#6030),#679,.T.);
#66781=ADVANCED_FACE('',(#6031),#4612,.T.);
#66782=ADVANCED_FACE('',(#6032),#680,.T.);
#66783=ADVANCED_FACE('',(#6033),#681,.T.);
#66784=ADVANCED_FACE('',(#6034),#4613,.T.);
#66785=ADVANCED_FACE('',(#6035),#682,.T.);
#66786=ADVANCED_FACE('',(#6036),#683,.T.);
#66787=ADVANCED_FACE('',(#6037),#4614,.T.);
#66788=ADVANCED_FACE('',(#6038),#684,.T.);
#66789=ADVANCED_FACE('',(#6039),#685,.T.);
#66790=ADVANCED_FACE('',(#6040),#4615,.T.);
#66791=ADVANCED_FACE('',(#6041),#686,.T.);
#66792=ADVANCED_FACE('',(#6042),#687,.T.);
#66793=ADVANCED_FACE('',(#6043),#4616,.T.);
#66794=ADVANCED_FACE('',(#6044),#688,.T.);
#66795=ADVANCED_FACE('',(#6045),#689,.T.);
#66796=ADVANCED_FACE('',(#6046),#4617,.T.);
#66797=ADVANCED_FACE('',(#6047),#690,.T.);
#66798=ADVANCED_FACE('',(#6048),#691,.T.);
#66799=ADVANCED_FACE('',(#6049),#4618,.T.);
#66800=ADVANCED_FACE('',(#6050),#692,.T.);
#66801=ADVANCED_FACE('',(#6051),#693,.T.);
#66802=ADVANCED_FACE('',(#6052),#4619,.T.);
#66803=ADVANCED_FACE('',(#6053),#694,.T.);
#66804=ADVANCED_FACE('',(#6054),#695,.T.);
#66805=ADVANCED_FACE('',(#6055),#4620,.T.);
#66806=ADVANCED_FACE('',(#6056),#696,.T.);
#66807=ADVANCED_FACE('',(#6057),#697,.T.);
#66808=ADVANCED_FACE('',(#6058),#4621,.T.);
#66809=ADVANCED_FACE('',(#6059),#698,.T.);
#66810=ADVANCED_FACE('',(#6060),#699,.T.);
#66811=ADVANCED_FACE('',(#6061),#4622,.T.);
#66812=ADVANCED_FACE('',(#6062),#700,.T.);
#66813=ADVANCED_FACE('',(#6063),#701,.T.);
#66814=ADVANCED_FACE('',(#6064),#4623,.T.);
#66815=ADVANCED_FACE('',(#6065),#702,.T.);
#66816=ADVANCED_FACE('',(#6066),#703,.T.);
#66817=ADVANCED_FACE('',(#6067),#4624,.T.);
#66818=ADVANCED_FACE('',(#6068),#704,.T.);
#66819=ADVANCED_FACE('',(#6069),#705,.T.);
#66820=ADVANCED_FACE('',(#6070),#706,.T.);
#66821=ADVANCED_FACE('',(#6071),#4625,.T.);
#66822=ADVANCED_FACE('',(#6072),#707,.T.);
#66823=ADVANCED_FACE('',(#6073),#4626,.T.);
#66824=ADVANCED_FACE('',(#6074),#708,.T.);
#66825=ADVANCED_FACE('',(#6075),#709,.T.);
#66826=ADVANCED_FACE('',(#6076),#4627,.T.);
#66827=ADVANCED_FACE('',(#6077),#710,.T.);
#66828=ADVANCED_FACE('',(#6078),#711,.T.);
#66829=ADVANCED_FACE('',(#6079),#4628,.T.);
#66830=ADVANCED_FACE('',(#6080),#712,.T.);
#66831=ADVANCED_FACE('',(#6081),#713,.T.);
#66832=ADVANCED_FACE('',(#6082),#4629,.T.);
#66833=ADVANCED_FACE('',(#6083),#714,.T.);
#66834=ADVANCED_FACE('',(#6084),#4630,.T.);
#66835=ADVANCED_FACE('',(#6085),#715,.T.);
#66836=ADVANCED_FACE('',(#6086),#716,.T.);
#66837=ADVANCED_FACE('',(#6087),#717,.T.);
#66838=ADVANCED_FACE('',(#6088),#718,.T.);
#66839=ADVANCED_FACE('',(#6089),#4631,.T.);
#66840=ADVANCED_FACE('',(#6090),#719,.T.);
#66841=ADVANCED_FACE('',(#6091),#720,.T.);
#66842=ADVANCED_FACE('',(#6092),#4632,.T.);
#66843=ADVANCED_FACE('',(#6093),#721,.T.);
#66844=ADVANCED_FACE('',(#6094),#722,.T.);
#66845=ADVANCED_FACE('',(#6095),#4633,.T.);
#66846=ADVANCED_FACE('',(#6096),#723,.T.);
#66847=ADVANCED_FACE('',(#6097),#724,.T.);
#66848=ADVANCED_FACE('',(#6098),#4634,.T.);
#66849=ADVANCED_FACE('',(#6099),#725,.T.);
#66850=ADVANCED_FACE('',(#6100),#726,.T.);
#66851=ADVANCED_FACE('',(#6101),#4635,.T.);
#66852=ADVANCED_FACE('',(#6102),#727,.T.);
#66853=ADVANCED_FACE('',(#6103),#728,.T.);
#66854=ADVANCED_FACE('',(#6104),#4636,.T.);
#66855=ADVANCED_FACE('',(#6105),#729,.T.);
#66856=ADVANCED_FACE('',(#6106),#730,.T.);
#66857=ADVANCED_FACE('',(#6107),#4637,.T.);
#66858=ADVANCED_FACE('',(#6108),#731,.T.);
#66859=ADVANCED_FACE('',(#6109),#732,.T.);
#66860=ADVANCED_FACE('',(#6110),#4638,.T.);
#66861=ADVANCED_FACE('',(#6111),#733,.T.);
#66862=ADVANCED_FACE('',(#6112),#734,.T.);
#66863=ADVANCED_FACE('',(#6113),#4639,.T.);
#66864=ADVANCED_FACE('',(#6114),#735,.T.);
#66865=ADVANCED_FACE('',(#6115),#736,.T.);
#66866=ADVANCED_FACE('',(#6116),#4640,.T.);
#66867=ADVANCED_FACE('',(#6117),#737,.T.);
#66868=ADVANCED_FACE('',(#6118),#738,.T.);
#66869=ADVANCED_FACE('',(#6119),#4641,.T.);
#66870=ADVANCED_FACE('',(#6120),#739,.T.);
#66871=ADVANCED_FACE('',(#6121),#740,.T.);
#66872=ADVANCED_FACE('',(#6122),#4642,.T.);
#66873=ADVANCED_FACE('',(#6123),#741,.T.);
#66874=ADVANCED_FACE('',(#6124),#742,.T.);
#66875=ADVANCED_FACE('',(#6125),#4643,.T.);
#66876=ADVANCED_FACE('',(#6126),#743,.T.);
#66877=ADVANCED_FACE('',(#6127),#744,.T.);
#66878=ADVANCED_FACE('',(#6128),#745,.T.);
#66879=ADVANCED_FACE('',(#6129),#746,.T.);
#66880=ADVANCED_FACE('',(#6130),#4644,.T.);
#66881=ADVANCED_FACE('',(#6131),#747,.T.);
#66882=ADVANCED_FACE('',(#6132),#748,.T.);
#66883=ADVANCED_FACE('',(#6133),#4645,.T.);
#66884=ADVANCED_FACE('',(#6134),#749,.T.);
#66885=ADVANCED_FACE('',(#6135),#750,.T.);
#66886=ADVANCED_FACE('',(#6136),#4646,.T.);
#66887=ADVANCED_FACE('',(#6137),#751,.T.);
#66888=ADVANCED_FACE('',(#6138),#752,.T.);
#66889=ADVANCED_FACE('',(#6139),#4647,.T.);
#66890=ADVANCED_FACE('',(#6140),#753,.T.);
#66891=ADVANCED_FACE('',(#6141),#754,.T.);
#66892=ADVANCED_FACE('',(#6142),#4648,.T.);
#66893=ADVANCED_FACE('',(#6143),#755,.T.);
#66894=ADVANCED_FACE('',(#6144),#756,.T.);
#66895=ADVANCED_FACE('',(#6145),#4649,.T.);
#66896=ADVANCED_FACE('',(#6146),#757,.T.);
#66897=ADVANCED_FACE('',(#6147),#758,.T.);
#66898=ADVANCED_FACE('',(#6148),#4650,.T.);
#66899=ADVANCED_FACE('',(#6149),#759,.T.);
#66900=ADVANCED_FACE('',(#6150),#760,.T.);
#66901=ADVANCED_FACE('',(#6151),#4651,.T.);
#66902=ADVANCED_FACE('',(#6152),#761,.T.);
#66903=ADVANCED_FACE('',(#6153),#762,.T.);
#66904=ADVANCED_FACE('',(#6154),#4652,.T.);
#66905=ADVANCED_FACE('',(#6155),#763,.T.);
#66906=ADVANCED_FACE('',(#6156),#764,.T.);
#66907=ADVANCED_FACE('',(#6157),#4653,.T.);
#66908=ADVANCED_FACE('',(#6158),#765,.T.);
#66909=ADVANCED_FACE('',(#6159),#766,.T.);
#66910=ADVANCED_FACE('',(#6160),#4654,.T.);
#66911=ADVANCED_FACE('',(#6161),#767,.T.);
#66912=ADVANCED_FACE('',(#6162),#768,.T.);
#66913=ADVANCED_FACE('',(#6163),#4655,.T.);
#66914=ADVANCED_FACE('',(#6164),#769,.T.);
#66915=ADVANCED_FACE('',(#6165),#770,.T.);
#66916=ADVANCED_FACE('',(#6166),#4656,.T.);
#66917=ADVANCED_FACE('',(#6167),#771,.T.);
#66918=ADVANCED_FACE('',(#6168),#772,.T.);
#66919=ADVANCED_FACE('',(#6169),#4657,.T.);
#66920=ADVANCED_FACE('',(#6170),#4658,.T.);
#66921=ADVANCED_FACE('',(#6171),#773,.T.);
#66922=ADVANCED_FACE('',(#6172),#774,.T.);
#66923=ADVANCED_FACE('',(#6173),#775,.T.);
#66924=ADVANCED_FACE('',(#6174),#776,.T.);
#66925=ADVANCED_FACE('',(#6175),#777,.T.);
#66926=ADVANCED_FACE('',(#6176),#778,.T.);
#66927=ADVANCED_FACE('',(#6177),#779,.T.);
#66928=ADVANCED_FACE('',(#6178),#780,.T.);
#66929=ADVANCED_FACE('',(#6179),#781,.T.);
#66930=ADVANCED_FACE('',(#6180),#782,.T.);
#66931=ADVANCED_FACE('',(#6181),#783,.T.);
#66932=ADVANCED_FACE('',(#6182),#784,.T.);
#66933=ADVANCED_FACE('',(#6183),#785,.T.);
#66934=ADVANCED_FACE('',(#6184),#786,.T.);
#66935=ADVANCED_FACE('',(#6185),#787,.T.);
#66936=ADVANCED_FACE('',(#6186),#788,.T.);
#66937=ADVANCED_FACE('',(#6187),#789,.T.);
#66938=ADVANCED_FACE('',(#6188),#790,.T.);
#66939=ADVANCED_FACE('',(#6189),#791,.T.);
#66940=ADVANCED_FACE('',(#6190),#792,.T.);
#66941=ADVANCED_FACE('',(#6191),#793,.T.);
#66942=ADVANCED_FACE('',(#6192),#794,.T.);
#66943=ADVANCED_FACE('',(#6193),#795,.T.);
#66944=ADVANCED_FACE('',(#6194),#796,.T.);
#66945=ADVANCED_FACE('',(#6195),#797,.T.);
#66946=ADVANCED_FACE('',(#6196),#798,.T.);
#66947=ADVANCED_FACE('',(#6197),#799,.T.);
#66948=ADVANCED_FACE('',(#6198),#800,.T.);
#66949=ADVANCED_FACE('',(#6199),#801,.T.);
#66950=ADVANCED_FACE('',(#6200),#802,.T.);
#66951=ADVANCED_FACE('',(#6201),#803,.T.);
#66952=ADVANCED_FACE('',(#6202),#804,.T.);
#66953=ADVANCED_FACE('',(#6203),#805,.T.);
#66954=ADVANCED_FACE('',(#6204),#806,.T.);
#66955=ADVANCED_FACE('',(#6205),#807,.T.);
#66956=ADVANCED_FACE('',(#6206),#808,.T.);
#66957=ADVANCED_FACE('',(#6207),#809,.T.);
#66958=ADVANCED_FACE('',(#6208),#810,.T.);
#66959=ADVANCED_FACE('',(#6209),#811,.T.);
#66960=ADVANCED_FACE('',(#6210),#812,.T.);
#66961=ADVANCED_FACE('',(#6211),#813,.T.);
#66962=ADVANCED_FACE('',(#6212),#814,.T.);
#66963=ADVANCED_FACE('',(#6213),#815,.T.);
#66964=ADVANCED_FACE('',(#6214),#816,.T.);
#66965=ADVANCED_FACE('',(#6215),#817,.T.);
#66966=ADVANCED_FACE('',(#6216),#818,.T.);
#66967=ADVANCED_FACE('',(#6217),#819,.T.);
#66968=ADVANCED_FACE('',(#6218),#820,.T.);
#66969=ADVANCED_FACE('',(#6219),#821,.T.);
#66970=ADVANCED_FACE('',(#6220),#822,.T.);
#66971=ADVANCED_FACE('',(#6221),#823,.T.);
#66972=ADVANCED_FACE('',(#6222),#824,.T.);
#66973=ADVANCED_FACE('',(#6223),#825,.T.);
#66974=ADVANCED_FACE('',(#6224),#826,.T.);
#66975=ADVANCED_FACE('',(#6225),#827,.T.);
#66976=ADVANCED_FACE('',(#6226),#828,.T.);
#66977=ADVANCED_FACE('',(#6227),#829,.T.);
#66978=ADVANCED_FACE('',(#6228),#830,.T.);
#66979=ADVANCED_FACE('',(#6229),#831,.T.);
#66980=ADVANCED_FACE('',(#6230),#832,.T.);
#66981=ADVANCED_FACE('',(#6231),#833,.T.);
#66982=ADVANCED_FACE('',(#6232),#834,.T.);
#66983=ADVANCED_FACE('',(#6233),#835,.T.);
#66984=ADVANCED_FACE('',(#6234),#836,.T.);
#66985=ADVANCED_FACE('',(#6235),#837,.T.);
#66986=ADVANCED_FACE('',(#6236),#838,.T.);
#66987=ADVANCED_FACE('',(#6237),#839,.T.);
#66988=ADVANCED_FACE('',(#6238),#840,.T.);
#66989=ADVANCED_FACE('',(#6239),#841,.T.);
#66990=ADVANCED_FACE('',(#6240),#842,.T.);
#66991=ADVANCED_FACE('',(#6241),#843,.T.);
#66992=ADVANCED_FACE('',(#6242),#844,.T.);
#66993=ADVANCED_FACE('',(#6243),#845,.T.);
#66994=ADVANCED_FACE('',(#6244),#846,.T.);
#66995=ADVANCED_FACE('',(#6245),#847,.T.);
#66996=ADVANCED_FACE('',(#6246),#848,.T.);
#66997=ADVANCED_FACE('',(#6247),#849,.T.);
#66998=ADVANCED_FACE('',(#6248),#850,.T.);
#66999=ADVANCED_FACE('',(#6249),#851,.T.);
#67000=ADVANCED_FACE('',(#6250),#852,.T.);
#67001=ADVANCED_FACE('',(#6251),#853,.T.);
#67002=ADVANCED_FACE('',(#6252),#854,.T.);
#67003=ADVANCED_FACE('',(#6253),#855,.T.);
#67004=ADVANCED_FACE('',(#6254),#856,.T.);
#67005=ADVANCED_FACE('',(#6255),#857,.T.);
#67006=ADVANCED_FACE('',(#6256),#858,.T.);
#67007=ADVANCED_FACE('',(#6257),#859,.T.);
#67008=ADVANCED_FACE('',(#6258),#860,.T.);
#67009=ADVANCED_FACE('',(#6259),#861,.T.);
#67010=ADVANCED_FACE('',(#6260),#862,.T.);
#67011=ADVANCED_FACE('',(#6261),#863,.T.);
#67012=ADVANCED_FACE('',(#6262),#864,.T.);
#67013=ADVANCED_FACE('',(#6263),#865,.T.);
#67014=ADVANCED_FACE('',(#6264),#866,.T.);
#67015=ADVANCED_FACE('',(#6265),#867,.T.);
#67016=ADVANCED_FACE('',(#6266),#868,.T.);
#67017=ADVANCED_FACE('',(#6267),#869,.T.);
#67018=ADVANCED_FACE('',(#6268),#870,.T.);
#67019=ADVANCED_FACE('',(#6269),#871,.T.);
#67020=ADVANCED_FACE('',(#6270),#872,.T.);
#67021=ADVANCED_FACE('',(#6271),#873,.T.);
#67022=ADVANCED_FACE('',(#6272),#874,.T.);
#67023=ADVANCED_FACE('',(#6273),#875,.T.);
#67024=ADVANCED_FACE('',(#6274),#876,.T.);
#67025=ADVANCED_FACE('',(#6275),#877,.T.);
#67026=ADVANCED_FACE('',(#6276),#878,.T.);
#67027=ADVANCED_FACE('',(#6277),#879,.T.);
#67028=ADVANCED_FACE('',(#6278),#880,.T.);
#67029=ADVANCED_FACE('',(#6279),#881,.T.);
#67030=ADVANCED_FACE('',(#6280),#882,.T.);
#67031=ADVANCED_FACE('',(#6281),#883,.T.);
#67032=ADVANCED_FACE('',(#6282),#884,.T.);
#67033=ADVANCED_FACE('',(#6283),#885,.T.);
#67034=ADVANCED_FACE('',(#6284),#886,.T.);
#67035=ADVANCED_FACE('',(#6285),#887,.T.);
#67036=ADVANCED_FACE('',(#6286),#888,.T.);
#67037=ADVANCED_FACE('',(#6287),#889,.T.);
#67038=ADVANCED_FACE('',(#6288),#890,.T.);
#67039=ADVANCED_FACE('',(#6289),#4659,.T.);
#67040=ADVANCED_FACE('',(#6290),#891,.T.);
#67041=ADVANCED_FACE('',(#6291),#892,.T.);
#67042=ADVANCED_FACE('',(#6292),#4660,.T.);
#67043=ADVANCED_FACE('',(#6293),#893,.T.);
#67044=ADVANCED_FACE('',(#6294),#894,.T.);
#67045=ADVANCED_FACE('',(#6295),#4661,.T.);
#67046=ADVANCED_FACE('',(#6296),#895,.T.);
#67047=ADVANCED_FACE('',(#6297),#896,.T.);
#67048=ADVANCED_FACE('',(#6298),#4662,.T.);
#67049=ADVANCED_FACE('',(#6299),#897,.T.);
#67050=ADVANCED_FACE('',(#6300),#898,.T.);
#67051=ADVANCED_FACE('',(#6301),#4663,.T.);
#67052=ADVANCED_FACE('',(#6302),#899,.T.);
#67053=ADVANCED_FACE('',(#6303),#900,.T.);
#67054=ADVANCED_FACE('',(#6304),#4664,.T.);
#67055=ADVANCED_FACE('',(#6305),#901,.T.);
#67056=ADVANCED_FACE('',(#6306),#902,.T.);
#67057=ADVANCED_FACE('',(#6307),#4665,.T.);
#67058=ADVANCED_FACE('',(#6308),#903,.T.);
#67059=ADVANCED_FACE('',(#6309),#904,.T.);
#67060=ADVANCED_FACE('',(#6310),#4666,.T.);
#67061=ADVANCED_FACE('',(#6311),#905,.T.);
#67062=ADVANCED_FACE('',(#6312),#906,.T.);
#67063=ADVANCED_FACE('',(#6313),#4667,.T.);
#67064=ADVANCED_FACE('',(#6314),#907,.T.);
#67065=ADVANCED_FACE('',(#6315),#908,.T.);
#67066=ADVANCED_FACE('',(#6316),#4668,.T.);
#67067=ADVANCED_FACE('',(#6317),#909,.T.);
#67068=ADVANCED_FACE('',(#6318),#910,.T.);
#67069=ADVANCED_FACE('',(#6319),#4669,.T.);
#67070=ADVANCED_FACE('',(#6320),#911,.T.);
#67071=ADVANCED_FACE('',(#6321),#912,.T.);
#67072=ADVANCED_FACE('',(#6322),#4670,.T.);
#67073=ADVANCED_FACE('',(#6323),#913,.T.);
#67074=ADVANCED_FACE('',(#6324),#914,.T.);
#67075=ADVANCED_FACE('',(#6325),#4671,.T.);
#67076=ADVANCED_FACE('',(#6326),#915,.T.);
#67077=ADVANCED_FACE('',(#6327),#916,.T.);
#67078=ADVANCED_FACE('',(#6328),#4672,.T.);
#67079=ADVANCED_FACE('',(#6329),#917,.T.);
#67080=ADVANCED_FACE('',(#6330),#918,.T.);
#67081=ADVANCED_FACE('',(#6331),#919,.T.);
#67082=ADVANCED_FACE('',(#6332),#920,.T.);
#67083=ADVANCED_FACE('',(#6333),#4673,.T.);
#67084=ADVANCED_FACE('',(#6334),#921,.T.);
#67085=ADVANCED_FACE('',(#6335),#922,.T.);
#67086=ADVANCED_FACE('',(#6336),#4674,.T.);
#67087=ADVANCED_FACE('',(#6337),#923,.T.);
#67088=ADVANCED_FACE('',(#6338),#924,.T.);
#67089=ADVANCED_FACE('',(#6339),#4675,.T.);
#67090=ADVANCED_FACE('',(#6340),#925,.T.);
#67091=ADVANCED_FACE('',(#6341),#926,.T.);
#67092=ADVANCED_FACE('',(#6342),#4676,.T.);
#67093=ADVANCED_FACE('',(#6343),#927,.T.);
#67094=ADVANCED_FACE('',(#6344),#928,.T.);
#67095=ADVANCED_FACE('',(#6345),#4677,.T.);
#67096=ADVANCED_FACE('',(#6346),#929,.T.);
#67097=ADVANCED_FACE('',(#6347),#930,.T.);
#67098=ADVANCED_FACE('',(#6348),#4678,.T.);
#67099=ADVANCED_FACE('',(#6349),#931,.T.);
#67100=ADVANCED_FACE('',(#6350),#932,.T.);
#67101=ADVANCED_FACE('',(#6351),#4679,.T.);
#67102=ADVANCED_FACE('',(#6352),#933,.T.);
#67103=ADVANCED_FACE('',(#6353),#934,.T.);
#67104=ADVANCED_FACE('',(#6354),#4680,.T.);
#67105=ADVANCED_FACE('',(#6355),#935,.T.);
#67106=ADVANCED_FACE('',(#6356),#936,.T.);
#67107=ADVANCED_FACE('',(#6357),#937,.T.);
#67108=ADVANCED_FACE('',(#6358),#4681,.T.);
#67109=ADVANCED_FACE('',(#6359),#938,.T.);
#67110=ADVANCED_FACE('',(#6360),#4682,.T.);
#67111=ADVANCED_FACE('',(#6361),#939,.T.);
#67112=ADVANCED_FACE('',(#6362),#940,.T.);
#67113=ADVANCED_FACE('',(#6363),#4683,.T.);
#67114=ADVANCED_FACE('',(#6364),#941,.T.);
#67115=ADVANCED_FACE('',(#6365),#942,.T.);
#67116=ADVANCED_FACE('',(#6366),#4684,.T.);
#67117=ADVANCED_FACE('',(#6367),#943,.T.);
#67118=ADVANCED_FACE('',(#6368),#944,.T.);
#67119=ADVANCED_FACE('',(#6369),#4685,.T.);
#67120=ADVANCED_FACE('',(#6370),#945,.T.);
#67121=ADVANCED_FACE('',(#6371),#946,.T.);
#67122=ADVANCED_FACE('',(#6372),#4686,.T.);
#67123=ADVANCED_FACE('',(#6373),#947,.T.);
#67124=ADVANCED_FACE('',(#6374),#948,.T.);
#67125=ADVANCED_FACE('',(#6375),#949,.T.);
#67126=ADVANCED_FACE('',(#6376),#4687,.T.);
#67127=ADVANCED_FACE('',(#6377),#950,.T.);
#67128=ADVANCED_FACE('',(#6378),#951,.T.);
#67129=ADVANCED_FACE('',(#6379),#4688,.T.);
#67130=ADVANCED_FACE('',(#6380),#952,.T.);
#67131=ADVANCED_FACE('',(#6381),#953,.T.);
#67132=ADVANCED_FACE('',(#6382),#4689,.T.);
#67133=ADVANCED_FACE('',(#6383),#954,.T.);
#67134=ADVANCED_FACE('',(#6384),#955,.T.);
#67135=ADVANCED_FACE('',(#6385),#4690,.T.);
#67136=ADVANCED_FACE('',(#6386),#956,.T.);
#67137=ADVANCED_FACE('',(#6387),#957,.T.);
#67138=ADVANCED_FACE('',(#6388),#4691,.T.);
#67139=ADVANCED_FACE('',(#6389),#958,.T.);
#67140=ADVANCED_FACE('',(#6390),#959,.T.);
#67141=ADVANCED_FACE('',(#6391),#4692,.T.);
#67142=ADVANCED_FACE('',(#6392),#960,.T.);
#67143=ADVANCED_FACE('',(#6393),#961,.T.);
#67144=ADVANCED_FACE('',(#6394),#4693,.T.);
#67145=ADVANCED_FACE('',(#6395),#962,.T.);
#67146=ADVANCED_FACE('',(#6396),#963,.T.);
#67147=ADVANCED_FACE('',(#6397),#4694,.T.);
#67148=ADVANCED_FACE('',(#6398),#964,.T.);
#67149=ADVANCED_FACE('',(#6399),#965,.T.);
#67150=ADVANCED_FACE('',(#6400),#4695,.T.);
#67151=ADVANCED_FACE('',(#6401),#966,.T.);
#67152=ADVANCED_FACE('',(#6402),#967,.T.);
#67153=ADVANCED_FACE('',(#6403),#4696,.T.);
#67154=ADVANCED_FACE('',(#6404),#968,.T.);
#67155=ADVANCED_FACE('',(#6405),#969,.T.);
#67156=ADVANCED_FACE('',(#6406),#4697,.T.);
#67157=ADVANCED_FACE('',(#6407),#970,.T.);
#67158=ADVANCED_FACE('',(#6408),#971,.T.);
#67159=ADVANCED_FACE('',(#6409),#4698,.T.);
#67160=ADVANCED_FACE('',(#6410),#972,.T.);
#67161=ADVANCED_FACE('',(#6411),#973,.T.);
#67162=ADVANCED_FACE('',(#6412),#4699,.T.);
#67163=ADVANCED_FACE('',(#6413),#974,.T.);
#67164=ADVANCED_FACE('',(#6414),#975,.T.);
#67165=ADVANCED_FACE('',(#6415),#4700,.T.);
#67166=ADVANCED_FACE('',(#6416),#976,.T.);
#67167=ADVANCED_FACE('',(#6417),#977,.T.);
#67168=ADVANCED_FACE('',(#6418),#4701,.T.);
#67169=ADVANCED_FACE('',(#6419),#978,.T.);
#67170=ADVANCED_FACE('',(#6420),#979,.T.);
#67171=ADVANCED_FACE('',(#6421),#4702,.T.);
#67172=ADVANCED_FACE('',(#6422),#980,.T.);
#67173=ADVANCED_FACE('',(#6423),#981,.T.);
#67174=ADVANCED_FACE('',(#6424),#4703,.T.);
#67175=ADVANCED_FACE('',(#6425),#982,.T.);
#67176=ADVANCED_FACE('',(#6426),#983,.T.);
#67177=ADVANCED_FACE('',(#6427),#4704,.T.);
#67178=ADVANCED_FACE('',(#6428),#984,.T.);
#67179=ADVANCED_FACE('',(#6429),#985,.T.);
#67180=ADVANCED_FACE('',(#6430),#4705,.T.);
#67181=ADVANCED_FACE('',(#6431),#986,.T.);
#67182=ADVANCED_FACE('',(#6432),#987,.T.);
#67183=ADVANCED_FACE('',(#6433),#4706,.T.);
#67184=ADVANCED_FACE('',(#6434),#988,.T.);
#67185=ADVANCED_FACE('',(#6435),#989,.T.);
#67186=ADVANCED_FACE('',(#6436),#4707,.T.);
#67187=ADVANCED_FACE('',(#6437),#990,.T.);
#67188=ADVANCED_FACE('',(#6438),#991,.T.);
#67189=ADVANCED_FACE('',(#6439),#4708,.T.);
#67190=ADVANCED_FACE('',(#6440),#992,.T.);
#67191=ADVANCED_FACE('',(#6441),#993,.T.);
#67192=ADVANCED_FACE('',(#6442),#4709,.T.);
#67193=ADVANCED_FACE('',(#6443),#994,.T.);
#67194=ADVANCED_FACE('',(#6444),#995,.T.);
#67195=ADVANCED_FACE('',(#6445),#4710,.T.);
#67196=ADVANCED_FACE('',(#6446),#996,.T.);
#67197=ADVANCED_FACE('',(#6447),#997,.T.);
#67198=ADVANCED_FACE('',(#6448),#4711,.T.);
#67199=ADVANCED_FACE('',(#6449),#998,.T.);
#67200=ADVANCED_FACE('',(#6450),#999,.T.);
#67201=ADVANCED_FACE('',(#6451),#4712,.T.);
#67202=ADVANCED_FACE('',(#6452),#1000,.T.);
#67203=ADVANCED_FACE('',(#6453),#1001,.T.);
#67204=ADVANCED_FACE('',(#6454),#4713,.T.);
#67205=ADVANCED_FACE('',(#6455),#1002,.T.);
#67206=ADVANCED_FACE('',(#6456),#1003,.T.);
#67207=ADVANCED_FACE('',(#6457),#4714,.T.);
#67208=ADVANCED_FACE('',(#6458),#1004,.T.);
#67209=ADVANCED_FACE('',(#6459),#1005,.T.);
#67210=ADVANCED_FACE('',(#6460),#4715,.T.);
#67211=ADVANCED_FACE('',(#6461),#1006,.T.);
#67212=ADVANCED_FACE('',(#6462),#1007,.T.);
#67213=ADVANCED_FACE('',(#6463),#1008,.T.);
#67214=ADVANCED_FACE('',(#6464),#1009,.T.);
#67215=ADVANCED_FACE('',(#6465),#1010,.T.);
#67216=ADVANCED_FACE('',(#6466),#1011,.T.);
#67217=ADVANCED_FACE('',(#6467),#1012,.T.);
#67218=ADVANCED_FACE('',(#6468),#1013,.T.);
#67219=ADVANCED_FACE('',(#6469),#1014,.T.);
#67220=ADVANCED_FACE('',(#6470),#1015,.T.);
#67221=ADVANCED_FACE('',(#6471),#1016,.T.);
#67222=ADVANCED_FACE('',(#6472),#1017,.T.);
#67223=ADVANCED_FACE('',(#6473),#1018,.T.);
#67224=ADVANCED_FACE('',(#6474),#1019,.T.);
#67225=ADVANCED_FACE('',(#6475),#1020,.T.);
#67226=ADVANCED_FACE('',(#6476),#1021,.T.);
#67227=ADVANCED_FACE('',(#6477),#1022,.T.);
#67228=ADVANCED_FACE('',(#6478),#1023,.T.);
#67229=ADVANCED_FACE('',(#6479),#1024,.T.);
#67230=ADVANCED_FACE('',(#6480),#1025,.T.);
#67231=ADVANCED_FACE('',(#6481),#1026,.T.);
#67232=ADVANCED_FACE('',(#6482),#1027,.T.);
#67233=ADVANCED_FACE('',(#6483),#1028,.T.);
#67234=ADVANCED_FACE('',(#6484),#1029,.T.);
#67235=ADVANCED_FACE('',(#6485),#1030,.T.);
#67236=ADVANCED_FACE('',(#6486),#1031,.T.);
#67237=ADVANCED_FACE('',(#6487),#1032,.T.);
#67238=ADVANCED_FACE('',(#6488),#1033,.T.);
#67239=ADVANCED_FACE('',(#6489),#1034,.T.);
#67240=ADVANCED_FACE('',(#6490),#1035,.T.);
#67241=ADVANCED_FACE('',(#6491),#1036,.T.);
#67242=ADVANCED_FACE('',(#6492),#1037,.T.);
#67243=ADVANCED_FACE('',(#6493),#1038,.T.);
#67244=ADVANCED_FACE('',(#6494),#1039,.T.);
#67245=ADVANCED_FACE('',(#6495),#1040,.T.);
#67246=ADVANCED_FACE('',(#6496),#1041,.T.);
#67247=ADVANCED_FACE('',(#6497),#1042,.T.);
#67248=ADVANCED_FACE('',(#6498),#1043,.T.);
#67249=ADVANCED_FACE('',(#6499),#1044,.T.);
#67250=ADVANCED_FACE('',(#6500),#1045,.T.);
#67251=ADVANCED_FACE('',(#6501),#1046,.T.);
#67252=ADVANCED_FACE('',(#6502),#1047,.T.);
#67253=ADVANCED_FACE('',(#6503),#1048,.T.);
#67254=ADVANCED_FACE('',(#6504),#1049,.T.);
#67255=ADVANCED_FACE('',(#6505),#1050,.T.);
#67256=ADVANCED_FACE('',(#6506),#1051,.T.);
#67257=ADVANCED_FACE('',(#6507),#1052,.T.);
#67258=ADVANCED_FACE('',(#6508),#1053,.T.);
#67259=ADVANCED_FACE('',(#6509),#1054,.T.);
#67260=ADVANCED_FACE('',(#6510),#1055,.T.);
#67261=ADVANCED_FACE('',(#6511),#1056,.T.);
#67262=ADVANCED_FACE('',(#6512),#1057,.T.);
#67263=ADVANCED_FACE('',(#6513),#1058,.T.);
#67264=ADVANCED_FACE('',(#6514),#1059,.T.);
#67265=ADVANCED_FACE('',(#6515),#1060,.T.);
#67266=ADVANCED_FACE('',(#6516),#1061,.T.);
#67267=ADVANCED_FACE('',(#6517),#1062,.T.);
#67268=ADVANCED_FACE('',(#6518),#1063,.T.);
#67269=ADVANCED_FACE('',(#6519),#1064,.T.);
#67270=ADVANCED_FACE('',(#6520),#1065,.T.);
#67271=ADVANCED_FACE('',(#6521),#1066,.T.);
#67272=ADVANCED_FACE('',(#6522),#1067,.T.);
#67273=ADVANCED_FACE('',(#6523),#1068,.T.);
#67274=ADVANCED_FACE('',(#6524),#1069,.T.);
#67275=ADVANCED_FACE('',(#6525),#1070,.T.);
#67276=ADVANCED_FACE('',(#6526),#1071,.T.);
#67277=ADVANCED_FACE('',(#6527),#1072,.T.);
#67278=ADVANCED_FACE('',(#6528),#1073,.T.);
#67279=ADVANCED_FACE('',(#6529),#1074,.T.);
#67280=ADVANCED_FACE('',(#6530),#1075,.T.);
#67281=ADVANCED_FACE('',(#6531),#1076,.T.);
#67282=ADVANCED_FACE('',(#6532),#1077,.T.);
#67283=ADVANCED_FACE('',(#6533),#1078,.T.);
#67284=ADVANCED_FACE('',(#6534),#1079,.T.);
#67285=ADVANCED_FACE('',(#6535),#1080,.T.);
#67286=ADVANCED_FACE('',(#6536),#1081,.T.);
#67287=ADVANCED_FACE('',(#6537),#1082,.T.);
#67288=ADVANCED_FACE('',(#6538),#1083,.T.);
#67289=ADVANCED_FACE('',(#6539),#1084,.T.);
#67290=ADVANCED_FACE('',(#6540),#1085,.T.);
#67291=ADVANCED_FACE('',(#6541),#1086,.T.);
#67292=ADVANCED_FACE('',(#6542),#1087,.T.);
#67293=ADVANCED_FACE('',(#6543),#1088,.T.);
#67294=ADVANCED_FACE('',(#6544),#1089,.T.);
#67295=ADVANCED_FACE('',(#6545),#1090,.T.);
#67296=ADVANCED_FACE('',(#6546),#1091,.T.);
#67297=ADVANCED_FACE('',(#6547),#1092,.T.);
#67298=ADVANCED_FACE('',(#6548),#1093,.T.);
#67299=ADVANCED_FACE('',(#6549),#1094,.T.);
#67300=ADVANCED_FACE('',(#6550),#1095,.T.);
#67301=ADVANCED_FACE('',(#6551),#1096,.T.);
#67302=ADVANCED_FACE('',(#6552),#1097,.T.);
#67303=ADVANCED_FACE('',(#6553),#1098,.T.);
#67304=ADVANCED_FACE('',(#6554),#1099,.T.);
#67305=ADVANCED_FACE('',(#6555),#1100,.T.);
#67306=ADVANCED_FACE('',(#6556),#1101,.T.);
#67307=ADVANCED_FACE('',(#6557),#1102,.T.);
#67308=ADVANCED_FACE('',(#6558),#1103,.T.);
#67309=ADVANCED_FACE('',(#6559),#1104,.T.);
#67310=ADVANCED_FACE('',(#6560),#1105,.T.);
#67311=ADVANCED_FACE('',(#6561),#1106,.T.);
#67312=ADVANCED_FACE('',(#6562),#1107,.T.);
#67313=ADVANCED_FACE('',(#6563),#1108,.T.);
#67314=ADVANCED_FACE('',(#6564),#1109,.T.);
#67315=ADVANCED_FACE('',(#6565),#1110,.T.);
#67316=ADVANCED_FACE('',(#6566),#1111,.T.);
#67317=ADVANCED_FACE('',(#6567),#1112,.T.);
#67318=ADVANCED_FACE('',(#6568),#1113,.T.);
#67319=ADVANCED_FACE('',(#6569),#1114,.T.);
#67320=ADVANCED_FACE('',(#6570),#1115,.T.);
#67321=ADVANCED_FACE('',(#6571),#1116,.T.);
#67322=ADVANCED_FACE('',(#6572),#1117,.T.);
#67323=ADVANCED_FACE('',(#6573),#1118,.T.);
#67324=ADVANCED_FACE('',(#6574),#1119,.T.);
#67325=ADVANCED_FACE('',(#6575),#1120,.T.);
#67326=ADVANCED_FACE('',(#6576),#1121,.T.);
#67327=ADVANCED_FACE('',(#6577),#1122,.T.);
#67328=ADVANCED_FACE('',(#6578),#1123,.T.);
#67329=ADVANCED_FACE('',(#6579),#4716,.T.);
#67330=ADVANCED_FACE('',(#6580),#1124,.T.);
#67331=ADVANCED_FACE('',(#6581),#1125,.T.);
#67332=ADVANCED_FACE('',(#6582),#4717,.T.);
#67333=ADVANCED_FACE('',(#6583),#1126,.T.);
#67334=ADVANCED_FACE('',(#6584),#1127,.T.);
#67335=ADVANCED_FACE('',(#6585),#4718,.T.);
#67336=ADVANCED_FACE('',(#6586),#1128,.T.);
#67337=ADVANCED_FACE('',(#6587),#1129,.T.);
#67338=ADVANCED_FACE('',(#6588),#4719,.T.);
#67339=ADVANCED_FACE('',(#6589),#1130,.T.);
#67340=ADVANCED_FACE('',(#6590),#1131,.T.);
#67341=ADVANCED_FACE('',(#6591),#4720,.T.);
#67342=ADVANCED_FACE('',(#6592),#1132,.T.);
#67343=ADVANCED_FACE('',(#6593),#1133,.T.);
#67344=ADVANCED_FACE('',(#6594),#4721,.T.);
#67345=ADVANCED_FACE('',(#6595),#1134,.T.);
#67346=ADVANCED_FACE('',(#6596),#1135,.T.);
#67347=ADVANCED_FACE('',(#6597),#1136,.T.);
#67348=ADVANCED_FACE('',(#6598),#1137,.T.);
#67349=ADVANCED_FACE('',(#6599),#4722,.T.);
#67350=ADVANCED_FACE('',(#6600),#1138,.T.);
#67351=ADVANCED_FACE('',(#6601),#1139,.T.);
#67352=ADVANCED_FACE('',(#6602),#4723,.T.);
#67353=ADVANCED_FACE('',(#6603),#1140,.T.);
#67354=ADVANCED_FACE('',(#6604),#1141,.T.);
#67355=ADVANCED_FACE('',(#6605),#4724,.T.);
#67356=ADVANCED_FACE('',(#6606),#1142,.T.);
#67357=ADVANCED_FACE('',(#6607),#1143,.T.);
#67358=ADVANCED_FACE('',(#6608),#4725,.T.);
#67359=ADVANCED_FACE('',(#6609),#1144,.T.);
#67360=ADVANCED_FACE('',(#6610),#1145,.T.);
#67361=ADVANCED_FACE('',(#6611),#4726,.T.);
#67362=ADVANCED_FACE('',(#6612),#1146,.T.);
#67363=ADVANCED_FACE('',(#6613),#1147,.T.);
#67364=ADVANCED_FACE('',(#6614),#4727,.T.);
#67365=ADVANCED_FACE('',(#6615),#1148,.T.);
#67366=ADVANCED_FACE('',(#6616),#1149,.T.);
#67367=ADVANCED_FACE('',(#6617),#4728,.T.);
#67368=ADVANCED_FACE('',(#6618),#1150,.T.);
#67369=ADVANCED_FACE('',(#6619),#1151,.T.);
#67370=ADVANCED_FACE('',(#6620),#4729,.T.);
#67371=ADVANCED_FACE('',(#6621),#1152,.T.);
#67372=ADVANCED_FACE('',(#6622),#1153,.T.);
#67373=ADVANCED_FACE('',(#6623),#4730,.T.);
#67374=ADVANCED_FACE('',(#6624),#1154,.T.);
#67375=ADVANCED_FACE('',(#6625),#1155,.T.);
#67376=ADVANCED_FACE('',(#6626),#4731,.T.);
#67377=ADVANCED_FACE('',(#6627),#1156,.T.);
#67378=ADVANCED_FACE('',(#6628),#1157,.T.);
#67379=ADVANCED_FACE('',(#6629),#4732,.T.);
#67380=ADVANCED_FACE('',(#6630),#1158,.T.);
#67381=ADVANCED_FACE('',(#6631),#1159,.T.);
#67382=ADVANCED_FACE('',(#6632),#4733,.T.);
#67383=ADVANCED_FACE('',(#6633),#1160,.T.);
#67384=ADVANCED_FACE('',(#6634),#1161,.T.);
#67385=ADVANCED_FACE('',(#6635),#4734,.T.);
#67386=ADVANCED_FACE('',(#6636),#1162,.T.);
#67387=ADVANCED_FACE('',(#6637),#1163,.T.);
#67388=ADVANCED_FACE('',(#6638),#4735,.T.);
#67389=ADVANCED_FACE('',(#6639),#1164,.T.);
#67390=ADVANCED_FACE('',(#6640),#1165,.T.);
#67391=ADVANCED_FACE('',(#6641),#4736,.T.);
#67392=ADVANCED_FACE('',(#6642),#1166,.T.);
#67393=ADVANCED_FACE('',(#6643),#1167,.T.);
#67394=ADVANCED_FACE('',(#6644),#1168,.T.);
#67395=ADVANCED_FACE('',(#6645),#4737,.T.);
#67396=ADVANCED_FACE('',(#6646),#1169,.T.);
#67397=ADVANCED_FACE('',(#6647),#4738,.T.);
#67398=ADVANCED_FACE('',(#6648),#1170,.T.);
#67399=ADVANCED_FACE('',(#6649),#1171,.T.);
#67400=ADVANCED_FACE('',(#6650),#4739,.T.);
#67401=ADVANCED_FACE('',(#6651),#1172,.T.);
#67402=ADVANCED_FACE('',(#6652),#1173,.T.);
#67403=ADVANCED_FACE('',(#6653),#4740,.T.);
#67404=ADVANCED_FACE('',(#6654),#1174,.T.);
#67405=ADVANCED_FACE('',(#6655),#1175,.T.);
#67406=ADVANCED_FACE('',(#6656),#4741,.T.);
#67407=ADVANCED_FACE('',(#6657),#1176,.T.);
#67408=ADVANCED_FACE('',(#6658),#1177,.T.);
#67409=ADVANCED_FACE('',(#6659),#4742,.T.);
#67410=ADVANCED_FACE('',(#6660),#1178,.T.);
#67411=ADVANCED_FACE('',(#6661),#4743,.T.);
#67412=ADVANCED_FACE('',(#6662),#1179,.T.);
#67413=ADVANCED_FACE('',(#6663),#1180,.T.);
#67414=ADVANCED_FACE('',(#6664),#1181,.T.);
#67415=ADVANCED_FACE('',(#6665),#1182,.T.);
#67416=ADVANCED_FACE('',(#6666),#4744,.T.);
#67417=ADVANCED_FACE('',(#6667),#1183,.T.);
#67418=ADVANCED_FACE('',(#6668),#1184,.T.);
#67419=ADVANCED_FACE('',(#6669),#4745,.T.);
#67420=ADVANCED_FACE('',(#6670),#1185,.T.);
#67421=ADVANCED_FACE('',(#6671),#1186,.T.);
#67422=ADVANCED_FACE('',(#6672),#4746,.T.);
#67423=ADVANCED_FACE('',(#6673),#1187,.T.);
#67424=ADVANCED_FACE('',(#6674),#1188,.T.);
#67425=ADVANCED_FACE('',(#6675),#4747,.T.);
#67426=ADVANCED_FACE('',(#6676),#1189,.T.);
#67427=ADVANCED_FACE('',(#6677),#1190,.T.);
#67428=ADVANCED_FACE('',(#6678),#4748,.T.);
#67429=ADVANCED_FACE('',(#6679),#1191,.T.);
#67430=ADVANCED_FACE('',(#6680),#1192,.T.);
#67431=ADVANCED_FACE('',(#6681),#4749,.T.);
#67432=ADVANCED_FACE('',(#6682),#1193,.T.);
#67433=ADVANCED_FACE('',(#6683),#1194,.T.);
#67434=ADVANCED_FACE('',(#6684),#4750,.T.);
#67435=ADVANCED_FACE('',(#6685),#1195,.T.);
#67436=ADVANCED_FACE('',(#6686),#1196,.T.);
#67437=ADVANCED_FACE('',(#6687),#4751,.T.);
#67438=ADVANCED_FACE('',(#6688),#1197,.T.);
#67439=ADVANCED_FACE('',(#6689),#1198,.T.);
#67440=ADVANCED_FACE('',(#6690),#4752,.T.);
#67441=ADVANCED_FACE('',(#6691),#1199,.T.);
#67442=ADVANCED_FACE('',(#6692),#1200,.T.);
#67443=ADVANCED_FACE('',(#6693),#4753,.T.);
#67444=ADVANCED_FACE('',(#6694),#1201,.T.);
#67445=ADVANCED_FACE('',(#6695),#1202,.T.);
#67446=ADVANCED_FACE('',(#6696),#4754,.T.);
#67447=ADVANCED_FACE('',(#6697),#1203,.T.);
#67448=ADVANCED_FACE('',(#6698),#1204,.T.);
#67449=ADVANCED_FACE('',(#6699),#4755,.T.);
#67450=ADVANCED_FACE('',(#6700),#1205,.T.);
#67451=ADVANCED_FACE('',(#6701),#1206,.T.);
#67452=ADVANCED_FACE('',(#6702),#4756,.T.);
#67453=ADVANCED_FACE('',(#6703),#1207,.T.);
#67454=ADVANCED_FACE('',(#6704),#1208,.T.);
#67455=ADVANCED_FACE('',(#6705),#1209,.T.);
#67456=ADVANCED_FACE('',(#6706),#1210,.T.);
#67457=ADVANCED_FACE('',(#6707),#4757,.T.);
#67458=ADVANCED_FACE('',(#6708),#1211,.T.);
#67459=ADVANCED_FACE('',(#6709),#1212,.T.);
#67460=ADVANCED_FACE('',(#6710),#4758,.T.);
#67461=ADVANCED_FACE('',(#6711),#1213,.T.);
#67462=ADVANCED_FACE('',(#6712),#1214,.T.);
#67463=ADVANCED_FACE('',(#6713),#4759,.T.);
#67464=ADVANCED_FACE('',(#6714),#1215,.T.);
#67465=ADVANCED_FACE('',(#6715),#1216,.T.);
#67466=ADVANCED_FACE('',(#6716),#4760,.T.);
#67467=ADVANCED_FACE('',(#6717),#1217,.T.);
#67468=ADVANCED_FACE('',(#6718),#1218,.T.);
#67469=ADVANCED_FACE('',(#6719),#4761,.T.);
#67470=ADVANCED_FACE('',(#6720),#1219,.T.);
#67471=ADVANCED_FACE('',(#6721),#1220,.T.);
#67472=ADVANCED_FACE('',(#6722),#4762,.T.);
#67473=ADVANCED_FACE('',(#6723),#1221,.T.);
#67474=ADVANCED_FACE('',(#6724),#1222,.T.);
#67475=ADVANCED_FACE('',(#6725),#4763,.T.);
#67476=ADVANCED_FACE('',(#6726),#1223,.T.);
#67477=ADVANCED_FACE('',(#6727),#1224,.T.);
#67478=ADVANCED_FACE('',(#6728),#4764,.T.);
#67479=ADVANCED_FACE('',(#6729),#1225,.T.);
#67480=ADVANCED_FACE('',(#6730),#1226,.T.);
#67481=ADVANCED_FACE('',(#6731),#4765,.T.);
#67482=ADVANCED_FACE('',(#6732),#1227,.T.);
#67483=ADVANCED_FACE('',(#6733),#1228,.T.);
#67484=ADVANCED_FACE('',(#6734),#4766,.T.);
#67485=ADVANCED_FACE('',(#6735),#1229,.T.);
#67486=ADVANCED_FACE('',(#6736),#1230,.T.);
#67487=ADVANCED_FACE('',(#6737),#4767,.T.);
#67488=ADVANCED_FACE('',(#6738),#1231,.T.);
#67489=ADVANCED_FACE('',(#6739),#1232,.T.);
#67490=ADVANCED_FACE('',(#6740),#4768,.T.);
#67491=ADVANCED_FACE('',(#6741),#1233,.T.);
#67492=ADVANCED_FACE('',(#6742),#1234,.T.);
#67493=ADVANCED_FACE('',(#6743),#4769,.T.);
#67494=ADVANCED_FACE('',(#6744),#1235,.T.);
#67495=ADVANCED_FACE('',(#6745),#1236,.T.);
#67496=ADVANCED_FACE('',(#6746),#4770,.T.);
#67497=ADVANCED_FACE('',(#6747),#4771,.T.);
#67498=ADVANCED_FACE('',(#6748),#1237,.T.);
#67499=ADVANCED_FACE('',(#6749),#1238,.T.);
#67500=ADVANCED_FACE('',(#6750),#1239,.T.);
#67501=ADVANCED_FACE('',(#6751),#1240,.T.);
#67502=ADVANCED_FACE('',(#6752),#1241,.T.);
#67503=ADVANCED_FACE('',(#6753),#1242,.T.);
#67504=ADVANCED_FACE('',(#6754),#1243,.T.);
#67505=ADVANCED_FACE('',(#6755),#1244,.T.);
#67506=ADVANCED_FACE('',(#6756),#1245,.T.);
#67507=ADVANCED_FACE('',(#6757),#1246,.T.);
#67508=ADVANCED_FACE('',(#6758),#1247,.T.);
#67509=ADVANCED_FACE('',(#6759),#1248,.T.);
#67510=ADVANCED_FACE('',(#6760),#1249,.T.);
#67511=ADVANCED_FACE('',(#6761),#1250,.T.);
#67512=ADVANCED_FACE('',(#6762),#1251,.T.);
#67513=ADVANCED_FACE('',(#6763),#1252,.T.);
#67514=ADVANCED_FACE('',(#6764),#1253,.T.);
#67515=ADVANCED_FACE('',(#6765),#1254,.T.);
#67516=ADVANCED_FACE('',(#6766),#1255,.T.);
#67517=ADVANCED_FACE('',(#6767),#1256,.T.);
#67518=ADVANCED_FACE('',(#6768),#1257,.T.);
#67519=ADVANCED_FACE('',(#6769),#1258,.T.);
#67520=ADVANCED_FACE('',(#6770),#1259,.T.);
#67521=ADVANCED_FACE('',(#6771),#1260,.T.);
#67522=ADVANCED_FACE('',(#6772),#1261,.T.);
#67523=ADVANCED_FACE('',(#6773),#1262,.T.);
#67524=ADVANCED_FACE('',(#6774),#1263,.T.);
#67525=ADVANCED_FACE('',(#6775),#1264,.T.);
#67526=ADVANCED_FACE('',(#6776),#1265,.T.);
#67527=ADVANCED_FACE('',(#6777),#1266,.T.);
#67528=ADVANCED_FACE('',(#6778),#1267,.T.);
#67529=ADVANCED_FACE('',(#6779),#1268,.T.);
#67530=ADVANCED_FACE('',(#6780),#1269,.T.);
#67531=ADVANCED_FACE('',(#6781),#1270,.T.);
#67532=ADVANCED_FACE('',(#6782),#1271,.T.);
#67533=ADVANCED_FACE('',(#6783),#1272,.T.);
#67534=ADVANCED_FACE('',(#6784),#1273,.T.);
#67535=ADVANCED_FACE('',(#6785),#1274,.T.);
#67536=ADVANCED_FACE('',(#6786),#1275,.T.);
#67537=ADVANCED_FACE('',(#6787),#1276,.T.);
#67538=ADVANCED_FACE('',(#6788),#1277,.T.);
#67539=ADVANCED_FACE('',(#6789),#1278,.T.);
#67540=ADVANCED_FACE('',(#6790),#1279,.T.);
#67541=ADVANCED_FACE('',(#6791),#1280,.T.);
#67542=ADVANCED_FACE('',(#6792),#1281,.T.);
#67543=ADVANCED_FACE('',(#6793),#1282,.T.);
#67544=ADVANCED_FACE('',(#6794),#1283,.T.);
#67545=ADVANCED_FACE('',(#6795),#1284,.T.);
#67546=ADVANCED_FACE('',(#6796),#1285,.T.);
#67547=ADVANCED_FACE('',(#6797),#1286,.T.);
#67548=ADVANCED_FACE('',(#6798),#1287,.T.);
#67549=ADVANCED_FACE('',(#6799),#1288,.T.);
#67550=ADVANCED_FACE('',(#6800),#1289,.T.);
#67551=ADVANCED_FACE('',(#6801),#1290,.T.);
#67552=ADVANCED_FACE('',(#6802),#1291,.T.);
#67553=ADVANCED_FACE('',(#6803),#1292,.T.);
#67554=ADVANCED_FACE('',(#6804),#1293,.T.);
#67555=ADVANCED_FACE('',(#6805),#1294,.T.);
#67556=ADVANCED_FACE('',(#6806),#1295,.T.);
#67557=ADVANCED_FACE('',(#6807),#1296,.T.);
#67558=ADVANCED_FACE('',(#6808),#1297,.T.);
#67559=ADVANCED_FACE('',(#6809),#1298,.T.);
#67560=ADVANCED_FACE('',(#6810),#1299,.T.);
#67561=ADVANCED_FACE('',(#6811),#1300,.T.);
#67562=ADVANCED_FACE('',(#6812),#1301,.T.);
#67563=ADVANCED_FACE('',(#6813),#1302,.T.);
#67564=ADVANCED_FACE('',(#6814),#1303,.T.);
#67565=ADVANCED_FACE('',(#6815),#1304,.T.);
#67566=ADVANCED_FACE('',(#6816),#1305,.T.);
#67567=ADVANCED_FACE('',(#6817),#1306,.T.);
#67568=ADVANCED_FACE('',(#6818),#1307,.T.);
#67569=ADVANCED_FACE('',(#6819),#1308,.T.);
#67570=ADVANCED_FACE('',(#6820),#1309,.T.);
#67571=ADVANCED_FACE('',(#6821),#1310,.T.);
#67572=ADVANCED_FACE('',(#6822),#1311,.T.);
#67573=ADVANCED_FACE('',(#6823),#1312,.T.);
#67574=ADVANCED_FACE('',(#6824),#1313,.T.);
#67575=ADVANCED_FACE('',(#6825),#1314,.T.);
#67576=ADVANCED_FACE('',(#6826),#1315,.T.);
#67577=ADVANCED_FACE('',(#6827),#1316,.T.);
#67578=ADVANCED_FACE('',(#6828),#1317,.T.);
#67579=ADVANCED_FACE('',(#6829),#1318,.T.);
#67580=ADVANCED_FACE('',(#6830),#1319,.T.);
#67581=ADVANCED_FACE('',(#6831),#1320,.T.);
#67582=ADVANCED_FACE('',(#6832),#1321,.T.);
#67583=ADVANCED_FACE('',(#6833),#1322,.T.);
#67584=ADVANCED_FACE('',(#6834),#1323,.T.);
#67585=ADVANCED_FACE('',(#6835),#1324,.T.);
#67586=ADVANCED_FACE('',(#6836),#1325,.T.);
#67587=ADVANCED_FACE('',(#6837),#1326,.T.);
#67588=ADVANCED_FACE('',(#6838),#1327,.T.);
#67589=ADVANCED_FACE('',(#6839),#1328,.T.);
#67590=ADVANCED_FACE('',(#6840),#1329,.T.);
#67591=ADVANCED_FACE('',(#6841),#1330,.T.);
#67592=ADVANCED_FACE('',(#6842),#1331,.T.);
#67593=ADVANCED_FACE('',(#6843),#1332,.T.);
#67594=ADVANCED_FACE('',(#6844),#1333,.T.);
#67595=ADVANCED_FACE('',(#6845),#1334,.T.);
#67596=ADVANCED_FACE('',(#6846),#1335,.T.);
#67597=ADVANCED_FACE('',(#6847),#1336,.T.);
#67598=ADVANCED_FACE('',(#6848),#1337,.T.);
#67599=ADVANCED_FACE('',(#6849),#1338,.T.);
#67600=ADVANCED_FACE('',(#6850),#1339,.T.);
#67601=ADVANCED_FACE('',(#6851),#1340,.T.);
#67602=ADVANCED_FACE('',(#6852),#1341,.T.);
#67603=ADVANCED_FACE('',(#6853),#1342,.T.);
#67604=ADVANCED_FACE('',(#6854),#1343,.T.);
#67605=ADVANCED_FACE('',(#6855),#1344,.T.);
#67606=ADVANCED_FACE('',(#6856),#1345,.T.);
#67607=ADVANCED_FACE('',(#6857),#1346,.T.);
#67608=ADVANCED_FACE('',(#6858),#1347,.T.);
#67609=ADVANCED_FACE('',(#6859),#1348,.T.);
#67610=ADVANCED_FACE('',(#6860),#1349,.T.);
#67611=ADVANCED_FACE('',(#6861),#1350,.T.);
#67612=ADVANCED_FACE('',(#6862),#1351,.T.);
#67613=ADVANCED_FACE('',(#6863),#1352,.T.);
#67614=ADVANCED_FACE('',(#6864),#1353,.T.);
#67615=ADVANCED_FACE('',(#6865),#1354,.T.);
#67616=ADVANCED_FACE('',(#6866),#4772,.T.);
#67617=ADVANCED_FACE('',(#6867),#1355,.T.);
#67618=ADVANCED_FACE('',(#6868),#1356,.T.);
#67619=ADVANCED_FACE('',(#6869),#4773,.T.);
#67620=ADVANCED_FACE('',(#6870),#1357,.T.);
#67621=ADVANCED_FACE('',(#6871),#1358,.T.);
#67622=ADVANCED_FACE('',(#6872),#4774,.T.);
#67623=ADVANCED_FACE('',(#6873),#1359,.T.);
#67624=ADVANCED_FACE('',(#6874),#1360,.T.);
#67625=ADVANCED_FACE('',(#6875),#4775,.T.);
#67626=ADVANCED_FACE('',(#6876),#1361,.T.);
#67627=ADVANCED_FACE('',(#6877),#1362,.T.);
#67628=ADVANCED_FACE('',(#6878),#4776,.T.);
#67629=ADVANCED_FACE('',(#6879),#1363,.T.);
#67630=ADVANCED_FACE('',(#6880),#1364,.T.);
#67631=ADVANCED_FACE('',(#6881),#4777,.T.);
#67632=ADVANCED_FACE('',(#6882),#1365,.T.);
#67633=ADVANCED_FACE('',(#6883),#1366,.T.);
#67634=ADVANCED_FACE('',(#6884),#4778,.T.);
#67635=ADVANCED_FACE('',(#6885),#1367,.T.);
#67636=ADVANCED_FACE('',(#6886),#1368,.T.);
#67637=ADVANCED_FACE('',(#6887),#4779,.T.);
#67638=ADVANCED_FACE('',(#6888),#1369,.T.);
#67639=ADVANCED_FACE('',(#6889),#1370,.T.);
#67640=ADVANCED_FACE('',(#6890),#4780,.T.);
#67641=ADVANCED_FACE('',(#6891),#1371,.T.);
#67642=ADVANCED_FACE('',(#6892),#1372,.T.);
#67643=ADVANCED_FACE('',(#6893),#4781,.T.);
#67644=ADVANCED_FACE('',(#6894),#1373,.T.);
#67645=ADVANCED_FACE('',(#6895),#1374,.T.);
#67646=ADVANCED_FACE('',(#6896),#4782,.T.);
#67647=ADVANCED_FACE('',(#6897),#1375,.T.);
#67648=ADVANCED_FACE('',(#6898),#1376,.T.);
#67649=ADVANCED_FACE('',(#6899),#4783,.T.);
#67650=ADVANCED_FACE('',(#6900),#1377,.T.);
#67651=ADVANCED_FACE('',(#6901),#1378,.T.);
#67652=ADVANCED_FACE('',(#6902),#4784,.T.);
#67653=ADVANCED_FACE('',(#6903),#1379,.T.);
#67654=ADVANCED_FACE('',(#6904),#1380,.T.);
#67655=ADVANCED_FACE('',(#6905),#4785,.T.);
#67656=ADVANCED_FACE('',(#6906),#1381,.T.);
#67657=ADVANCED_FACE('',(#6907),#1382,.T.);
#67658=ADVANCED_FACE('',(#6908),#1383,.T.);
#67659=ADVANCED_FACE('',(#6909),#1384,.T.);
#67660=ADVANCED_FACE('',(#6910),#4786,.T.);
#67661=ADVANCED_FACE('',(#6911),#1385,.T.);
#67662=ADVANCED_FACE('',(#6912),#1386,.T.);
#67663=ADVANCED_FACE('',(#6913),#4787,.T.);
#67664=ADVANCED_FACE('',(#6914),#1387,.T.);
#67665=ADVANCED_FACE('',(#6915),#1388,.T.);
#67666=ADVANCED_FACE('',(#6916),#4788,.T.);
#67667=ADVANCED_FACE('',(#6917),#1389,.T.);
#67668=ADVANCED_FACE('',(#6918),#1390,.T.);
#67669=ADVANCED_FACE('',(#6919),#4789,.T.);
#67670=ADVANCED_FACE('',(#6920),#1391,.T.);
#67671=ADVANCED_FACE('',(#6921),#1392,.T.);
#67672=ADVANCED_FACE('',(#6922),#4790,.T.);
#67673=ADVANCED_FACE('',(#6923),#1393,.T.);
#67674=ADVANCED_FACE('',(#6924),#1394,.T.);
#67675=ADVANCED_FACE('',(#6925),#4791,.T.);
#67676=ADVANCED_FACE('',(#6926),#1395,.T.);
#67677=ADVANCED_FACE('',(#6927),#1396,.T.);
#67678=ADVANCED_FACE('',(#6928),#4792,.T.);
#67679=ADVANCED_FACE('',(#6929),#1397,.T.);
#67680=ADVANCED_FACE('',(#6930),#1398,.T.);
#67681=ADVANCED_FACE('',(#6931),#1399,.T.);
#67682=ADVANCED_FACE('',(#6932),#4793,.T.);
#67683=ADVANCED_FACE('',(#6933),#1400,.T.);
#67684=ADVANCED_FACE('',(#6934),#4794,.T.);
#67685=ADVANCED_FACE('',(#6935),#1401,.T.);
#67686=ADVANCED_FACE('',(#6936),#1402,.T.);
#67687=ADVANCED_FACE('',(#6937),#4795,.T.);
#67688=ADVANCED_FACE('',(#6938),#1403,.T.);
#67689=ADVANCED_FACE('',(#6939),#1404,.T.);
#67690=ADVANCED_FACE('',(#6940),#4796,.T.);
#67691=ADVANCED_FACE('',(#6941),#1405,.T.);
#67692=ADVANCED_FACE('',(#6942),#1406,.T.);
#67693=ADVANCED_FACE('',(#6943),#4797,.T.);
#67694=ADVANCED_FACE('',(#6944),#1407,.T.);
#67695=ADVANCED_FACE('',(#6945),#1408,.T.);
#67696=ADVANCED_FACE('',(#6946),#4798,.T.);
#67697=ADVANCED_FACE('',(#6947),#1409,.T.);
#67698=ADVANCED_FACE('',(#6948),#1410,.T.);
#67699=ADVANCED_FACE('',(#6949),#4799,.T.);
#67700=ADVANCED_FACE('',(#6950),#1411,.T.);
#67701=ADVANCED_FACE('',(#6951),#1412,.T.);
#67702=ADVANCED_FACE('',(#6952),#1413,.T.);
#67703=ADVANCED_FACE('',(#6953),#4800,.T.);
#67704=ADVANCED_FACE('',(#6954),#1414,.T.);
#67705=ADVANCED_FACE('',(#6955),#1415,.T.);
#67706=ADVANCED_FACE('',(#6956),#4801,.T.);
#67707=ADVANCED_FACE('',(#6957),#1416,.T.);
#67708=ADVANCED_FACE('',(#6958),#1417,.T.);
#67709=ADVANCED_FACE('',(#6959),#4802,.T.);
#67710=ADVANCED_FACE('',(#6960),#1418,.T.);
#67711=ADVANCED_FACE('',(#6961),#1419,.T.);
#67712=ADVANCED_FACE('',(#6962),#4803,.T.);
#67713=ADVANCED_FACE('',(#6963),#1420,.T.);
#67714=ADVANCED_FACE('',(#6964),#1421,.T.);
#67715=ADVANCED_FACE('',(#6965),#4804,.T.);
#67716=ADVANCED_FACE('',(#6966),#1422,.T.);
#67717=ADVANCED_FACE('',(#6967),#1423,.T.);
#67718=ADVANCED_FACE('',(#6968),#4805,.T.);
#67719=ADVANCED_FACE('',(#6969),#1424,.T.);
#67720=ADVANCED_FACE('',(#6970),#1425,.T.);
#67721=ADVANCED_FACE('',(#6971),#4806,.T.);
#67722=ADVANCED_FACE('',(#6972),#1426,.T.);
#67723=ADVANCED_FACE('',(#6973),#1427,.T.);
#67724=ADVANCED_FACE('',(#6974),#4807,.T.);
#67725=ADVANCED_FACE('',(#6975),#1428,.T.);
#67726=ADVANCED_FACE('',(#6976),#1429,.T.);
#67727=ADVANCED_FACE('',(#6977),#4808,.T.);
#67728=ADVANCED_FACE('',(#6978),#1430,.T.);
#67729=ADVANCED_FACE('',(#6979),#1431,.T.);
#67730=ADVANCED_FACE('',(#6980),#4809,.T.);
#67731=ADVANCED_FACE('',(#6981),#1432,.T.);
#67732=ADVANCED_FACE('',(#6982),#1433,.T.);
#67733=ADVANCED_FACE('',(#6983),#4810,.T.);
#67734=ADVANCED_FACE('',(#6984),#1434,.T.);
#67735=ADVANCED_FACE('',(#6985),#1435,.T.);
#67736=ADVANCED_FACE('',(#6986),#4811,.T.);
#67737=ADVANCED_FACE('',(#6987),#1436,.T.);
#67738=ADVANCED_FACE('',(#6988),#1437,.T.);
#67739=ADVANCED_FACE('',(#6989),#4812,.T.);
#67740=ADVANCED_FACE('',(#6990),#1438,.T.);
#67741=ADVANCED_FACE('',(#6991),#1439,.T.);
#67742=ADVANCED_FACE('',(#6992),#4813,.T.);
#67743=ADVANCED_FACE('',(#6993),#1440,.T.);
#67744=ADVANCED_FACE('',(#6994),#1441,.T.);
#67745=ADVANCED_FACE('',(#6995),#4814,.T.);
#67746=ADVANCED_FACE('',(#6996),#1442,.T.);
#67747=ADVANCED_FACE('',(#6997),#1443,.T.);
#67748=ADVANCED_FACE('',(#6998),#4815,.T.);
#67749=ADVANCED_FACE('',(#6999),#1444,.T.);
#67750=ADVANCED_FACE('',(#7000),#1445,.T.);
#67751=ADVANCED_FACE('',(#7001),#4816,.T.);
#67752=ADVANCED_FACE('',(#7002),#1446,.T.);
#67753=ADVANCED_FACE('',(#7003),#1447,.T.);
#67754=ADVANCED_FACE('',(#7004),#4817,.T.);
#67755=ADVANCED_FACE('',(#7005),#1448,.T.);
#67756=ADVANCED_FACE('',(#7006),#1449,.T.);
#67757=ADVANCED_FACE('',(#7007),#4818,.T.);
#67758=ADVANCED_FACE('',(#7008),#1450,.T.);
#67759=ADVANCED_FACE('',(#7009),#1451,.T.);
#67760=ADVANCED_FACE('',(#7010),#4819,.T.);
#67761=ADVANCED_FACE('',(#7011),#1452,.T.);
#67762=ADVANCED_FACE('',(#7012),#1453,.T.);
#67763=ADVANCED_FACE('',(#7013),#4820,.T.);
#67764=ADVANCED_FACE('',(#7014),#1454,.T.);
#67765=ADVANCED_FACE('',(#7015),#1455,.T.);
#67766=ADVANCED_FACE('',(#7016),#1456,.T.);
#67767=ADVANCED_FACE('',(#7017),#1457,.T.);
#67768=ADVANCED_FACE('',(#7018),#4821,.T.);
#67769=ADVANCED_FACE('',(#7019),#1458,.T.);
#67770=ADVANCED_FACE('',(#7020),#1459,.T.);
#67771=ADVANCED_FACE('',(#7021),#4822,.T.);
#67772=ADVANCED_FACE('',(#7022),#1460,.T.);
#67773=ADVANCED_FACE('',(#7023),#1461,.T.);
#67774=ADVANCED_FACE('',(#7024),#4823,.T.);
#67775=ADVANCED_FACE('',(#7025),#1462,.T.);
#67776=ADVANCED_FACE('',(#7026),#1463,.T.);
#67777=ADVANCED_FACE('',(#7027),#4824,.T.);
#67778=ADVANCED_FACE('',(#7028),#1464,.T.);
#67779=ADVANCED_FACE('',(#7029),#1465,.T.);
#67780=ADVANCED_FACE('',(#7030),#4825,.T.);
#67781=ADVANCED_FACE('',(#7031),#1466,.T.);
#67782=ADVANCED_FACE('',(#7032),#1467,.T.);
#67783=ADVANCED_FACE('',(#7033),#4826,.T.);
#67784=ADVANCED_FACE('',(#7034),#1468,.T.);
#67785=ADVANCED_FACE('',(#7035),#1469,.T.);
#67786=ADVANCED_FACE('',(#7036),#4827,.T.);
#67787=ADVANCED_FACE('',(#7037),#1470,.T.);
#67788=ADVANCED_FACE('',(#7038),#1471,.T.);
#67789=ADVANCED_FACE('',(#7039),#1472,.T.);
#67790=ADVANCED_FACE('',(#7040),#1473,.T.);
#67791=ADVANCED_FACE('',(#7041),#1474,.T.);
#67792=ADVANCED_FACE('',(#7042),#1475,.T.);
#67793=ADVANCED_FACE('',(#7043),#1476,.T.);
#67794=ADVANCED_FACE('',(#7044),#1477,.T.);
#67795=ADVANCED_FACE('',(#7045),#1478,.T.);
#67796=ADVANCED_FACE('',(#7046),#1479,.T.);
#67797=ADVANCED_FACE('',(#7047),#1480,.T.);
#67798=ADVANCED_FACE('',(#7048),#1481,.T.);
#67799=ADVANCED_FACE('',(#7049),#1482,.T.);
#67800=ADVANCED_FACE('',(#7050),#1483,.T.);
#67801=ADVANCED_FACE('',(#7051),#1484,.T.);
#67802=ADVANCED_FACE('',(#7052),#1485,.T.);
#67803=ADVANCED_FACE('',(#7053),#1486,.T.);
#67804=ADVANCED_FACE('',(#7054),#1487,.T.);
#67805=ADVANCED_FACE('',(#7055),#1488,.T.);
#67806=ADVANCED_FACE('',(#7056),#1489,.T.);
#67807=ADVANCED_FACE('',(#7057),#1490,.T.);
#67808=ADVANCED_FACE('',(#7058),#1491,.T.);
#67809=ADVANCED_FACE('',(#7059),#1492,.T.);
#67810=ADVANCED_FACE('',(#7060),#1493,.T.);
#67811=ADVANCED_FACE('',(#7061),#1494,.T.);
#67812=ADVANCED_FACE('',(#7062),#1495,.T.);
#67813=ADVANCED_FACE('',(#7063),#1496,.T.);
#67814=ADVANCED_FACE('',(#7064),#1497,.T.);
#67815=ADVANCED_FACE('',(#7065),#1498,.T.);
#67816=ADVANCED_FACE('',(#7066),#1499,.T.);
#67817=ADVANCED_FACE('',(#7067),#1500,.T.);
#67818=ADVANCED_FACE('',(#7068),#1501,.T.);
#67819=ADVANCED_FACE('',(#7069),#1502,.T.);
#67820=ADVANCED_FACE('',(#7070),#1503,.T.);
#67821=ADVANCED_FACE('',(#7071),#1504,.T.);
#67822=ADVANCED_FACE('',(#7072),#1505,.T.);
#67823=ADVANCED_FACE('',(#7073),#1506,.T.);
#67824=ADVANCED_FACE('',(#7074),#1507,.T.);
#67825=ADVANCED_FACE('',(#7075),#1508,.T.);
#67826=ADVANCED_FACE('',(#7076),#1509,.T.);
#67827=ADVANCED_FACE('',(#7077),#1510,.T.);
#67828=ADVANCED_FACE('',(#7078),#1511,.T.);
#67829=ADVANCED_FACE('',(#7079),#1512,.T.);
#67830=ADVANCED_FACE('',(#7080),#1513,.T.);
#67831=ADVANCED_FACE('',(#7081),#1514,.T.);
#67832=ADVANCED_FACE('',(#7082),#1515,.T.);
#67833=ADVANCED_FACE('',(#7083),#1516,.T.);
#67834=ADVANCED_FACE('',(#7084),#1517,.T.);
#67835=ADVANCED_FACE('',(#7085),#1518,.T.);
#67836=ADVANCED_FACE('',(#7086),#1519,.T.);
#67837=ADVANCED_FACE('',(#7087),#1520,.T.);
#67838=ADVANCED_FACE('',(#7088),#1521,.T.);
#67839=ADVANCED_FACE('',(#7089),#1522,.T.);
#67840=ADVANCED_FACE('',(#7090),#1523,.T.);
#67841=ADVANCED_FACE('',(#7091),#1524,.T.);
#67842=ADVANCED_FACE('',(#7092),#1525,.T.);
#67843=ADVANCED_FACE('',(#7093),#1526,.T.);
#67844=ADVANCED_FACE('',(#7094),#1527,.T.);
#67845=ADVANCED_FACE('',(#7095),#1528,.T.);
#67846=ADVANCED_FACE('',(#7096),#1529,.T.);
#67847=ADVANCED_FACE('',(#7097),#1530,.T.);
#67848=ADVANCED_FACE('',(#7098),#1531,.T.);
#67849=ADVANCED_FACE('',(#7099),#1532,.T.);
#67850=ADVANCED_FACE('',(#7100),#1533,.T.);
#67851=ADVANCED_FACE('',(#7101),#1534,.T.);
#67852=ADVANCED_FACE('',(#7102),#1535,.T.);
#67853=ADVANCED_FACE('',(#7103),#1536,.T.);
#67854=ADVANCED_FACE('',(#7104),#1537,.T.);
#67855=ADVANCED_FACE('',(#7105),#1538,.T.);
#67856=ADVANCED_FACE('',(#7106),#1539,.T.);
#67857=ADVANCED_FACE('',(#7107),#1540,.T.);
#67858=ADVANCED_FACE('',(#7108),#1541,.T.);
#67859=ADVANCED_FACE('',(#7109),#1542,.T.);
#67860=ADVANCED_FACE('',(#7110),#1543,.T.);
#67861=ADVANCED_FACE('',(#7111),#1544,.T.);
#67862=ADVANCED_FACE('',(#7112),#1545,.T.);
#67863=ADVANCED_FACE('',(#7113),#1546,.T.);
#67864=ADVANCED_FACE('',(#7114),#1547,.T.);
#67865=ADVANCED_FACE('',(#7115),#1548,.T.);
#67866=ADVANCED_FACE('',(#7116),#1549,.T.);
#67867=ADVANCED_FACE('',(#7117),#1550,.T.);
#67868=ADVANCED_FACE('',(#7118),#1551,.T.);
#67869=ADVANCED_FACE('',(#7119),#1552,.T.);
#67870=ADVANCED_FACE('',(#7120),#1553,.T.);
#67871=ADVANCED_FACE('',(#7121),#1554,.T.);
#67872=ADVANCED_FACE('',(#7122),#1555,.T.);
#67873=ADVANCED_FACE('',(#7123),#1556,.T.);
#67874=ADVANCED_FACE('',(#7124),#1557,.T.);
#67875=ADVANCED_FACE('',(#7125),#1558,.T.);
#67876=ADVANCED_FACE('',(#7126),#1559,.T.);
#67877=ADVANCED_FACE('',(#7127),#1560,.T.);
#67878=ADVANCED_FACE('',(#7128),#1561,.T.);
#67879=ADVANCED_FACE('',(#7129),#1562,.T.);
#67880=ADVANCED_FACE('',(#7130),#1563,.T.);
#67881=ADVANCED_FACE('',(#7131),#1564,.T.);
#67882=ADVANCED_FACE('',(#7132),#1565,.T.);
#67883=ADVANCED_FACE('',(#7133),#1566,.T.);
#67884=ADVANCED_FACE('',(#7134),#1567,.T.);
#67885=ADVANCED_FACE('',(#7135),#1568,.T.);
#67886=ADVANCED_FACE('',(#7136),#1569,.T.);
#67887=ADVANCED_FACE('',(#7137),#1570,.T.);
#67888=ADVANCED_FACE('',(#7138),#1571,.T.);
#67889=ADVANCED_FACE('',(#7139),#1572,.T.);
#67890=ADVANCED_FACE('',(#7140),#1573,.T.);
#67891=ADVANCED_FACE('',(#7141),#1574,.T.);
#67892=ADVANCED_FACE('',(#7142),#1575,.T.);
#67893=ADVANCED_FACE('',(#7143),#1576,.T.);
#67894=ADVANCED_FACE('',(#7144),#1577,.T.);
#67895=ADVANCED_FACE('',(#7145),#1578,.T.);
#67896=ADVANCED_FACE('',(#7146),#1579,.T.);
#67897=ADVANCED_FACE('',(#7147),#1580,.T.);
#67898=ADVANCED_FACE('',(#7148),#1581,.T.);
#67899=ADVANCED_FACE('',(#7149),#1582,.T.);
#67900=ADVANCED_FACE('',(#7150),#1583,.T.);
#67901=ADVANCED_FACE('',(#7151),#1584,.T.);
#67902=ADVANCED_FACE('',(#7152),#1585,.T.);
#67903=ADVANCED_FACE('',(#7153),#1586,.T.);
#67904=ADVANCED_FACE('',(#7154),#1587,.T.);
#67905=ADVANCED_FACE('',(#7155),#4828,.T.);
#67906=ADVANCED_FACE('',(#7156),#1588,.T.);
#67907=ADVANCED_FACE('',(#7157),#1589,.T.);
#67908=ADVANCED_FACE('',(#7158),#4829,.T.);
#67909=ADVANCED_FACE('',(#7159),#1590,.T.);
#67910=ADVANCED_FACE('',(#7160),#1591,.T.);
#67911=ADVANCED_FACE('',(#7161),#4830,.T.);
#67912=ADVANCED_FACE('',(#7162),#1592,.T.);
#67913=ADVANCED_FACE('',(#7163),#1593,.T.);
#67914=ADVANCED_FACE('',(#7164),#4831,.T.);
#67915=ADVANCED_FACE('',(#7165),#1594,.T.);
#67916=ADVANCED_FACE('',(#7166),#1595,.T.);
#67917=ADVANCED_FACE('',(#7167),#4832,.T.);
#67918=ADVANCED_FACE('',(#7168),#1596,.T.);
#67919=ADVANCED_FACE('',(#7169),#1597,.T.);
#67920=ADVANCED_FACE('',(#7170),#4833,.T.);
#67921=ADVANCED_FACE('',(#7171),#1598,.T.);
#67922=ADVANCED_FACE('',(#7172),#1599,.T.);
#67923=ADVANCED_FACE('',(#7173),#1600,.T.);
#67924=ADVANCED_FACE('',(#7174),#1601,.T.);
#67925=ADVANCED_FACE('',(#7175),#4834,.T.);
#67926=ADVANCED_FACE('',(#7176),#1602,.T.);
#67927=ADVANCED_FACE('',(#7177),#1603,.T.);
#67928=ADVANCED_FACE('',(#7178),#4835,.T.);
#67929=ADVANCED_FACE('',(#7179),#1604,.T.);
#67930=ADVANCED_FACE('',(#7180),#1605,.T.);
#67931=ADVANCED_FACE('',(#7181),#4836,.T.);
#67932=ADVANCED_FACE('',(#7182),#1606,.T.);
#67933=ADVANCED_FACE('',(#7183),#1607,.T.);
#67934=ADVANCED_FACE('',(#7184),#4837,.T.);
#67935=ADVANCED_FACE('',(#7185),#1608,.T.);
#67936=ADVANCED_FACE('',(#7186),#1609,.T.);
#67937=ADVANCED_FACE('',(#7187),#4838,.T.);
#67938=ADVANCED_FACE('',(#7188),#1610,.T.);
#67939=ADVANCED_FACE('',(#7189),#1611,.T.);
#67940=ADVANCED_FACE('',(#7190),#4839,.T.);
#67941=ADVANCED_FACE('',(#7191),#1612,.T.);
#67942=ADVANCED_FACE('',(#7192),#1613,.T.);
#67943=ADVANCED_FACE('',(#7193),#4840,.T.);
#67944=ADVANCED_FACE('',(#7194),#1614,.T.);
#67945=ADVANCED_FACE('',(#7195),#1615,.T.);
#67946=ADVANCED_FACE('',(#7196),#4841,.T.);
#67947=ADVANCED_FACE('',(#7197),#1616,.T.);
#67948=ADVANCED_FACE('',(#7198),#1617,.T.);
#67949=ADVANCED_FACE('',(#7199),#4842,.T.);
#67950=ADVANCED_FACE('',(#7200),#1618,.T.);
#67951=ADVANCED_FACE('',(#7201),#1619,.T.);
#67952=ADVANCED_FACE('',(#7202),#4843,.T.);
#67953=ADVANCED_FACE('',(#7203),#1620,.T.);
#67954=ADVANCED_FACE('',(#7204),#1621,.T.);
#67955=ADVANCED_FACE('',(#7205),#4844,.T.);
#67956=ADVANCED_FACE('',(#7206),#1622,.T.);
#67957=ADVANCED_FACE('',(#7207),#1623,.T.);
#67958=ADVANCED_FACE('',(#7208),#4845,.T.);
#67959=ADVANCED_FACE('',(#7209),#1624,.T.);
#67960=ADVANCED_FACE('',(#7210),#1625,.T.);
#67961=ADVANCED_FACE('',(#7211),#4846,.T.);
#67962=ADVANCED_FACE('',(#7212),#1626,.T.);
#67963=ADVANCED_FACE('',(#7213),#1627,.T.);
#67964=ADVANCED_FACE('',(#7214),#4847,.T.);
#67965=ADVANCED_FACE('',(#7215),#1628,.T.);
#67966=ADVANCED_FACE('',(#7216),#1629,.T.);
#67967=ADVANCED_FACE('',(#7217),#1630,.T.);
#67968=ADVANCED_FACE('',(#7218),#4848,.T.);
#67969=ADVANCED_FACE('',(#7219),#1631,.T.);
#67970=ADVANCED_FACE('',(#7220),#4849,.T.);
#67971=ADVANCED_FACE('',(#7221),#1632,.T.);
#67972=ADVANCED_FACE('',(#7222),#1633,.T.);
#67973=ADVANCED_FACE('',(#7223),#4850,.T.);
#67974=ADVANCED_FACE('',(#7224),#1634,.T.);
#67975=ADVANCED_FACE('',(#7225),#1635,.T.);
#67976=ADVANCED_FACE('',(#7226),#4851,.T.);
#67977=ADVANCED_FACE('',(#7227),#1636,.T.);
#67978=ADVANCED_FACE('',(#7228),#1637,.T.);
#67979=ADVANCED_FACE('',(#7229),#4852,.T.);
#67980=ADVANCED_FACE('',(#7230),#1638,.T.);
#67981=ADVANCED_FACE('',(#7231),#1639,.T.);
#67982=ADVANCED_FACE('',(#7232),#4853,.T.);
#67983=ADVANCED_FACE('',(#7233),#1640,.T.);
#67984=ADVANCED_FACE('',(#7234),#1641,.T.);
#67985=ADVANCED_FACE('',(#7235),#4854,.T.);
#67986=ADVANCED_FACE('',(#7236),#1642,.T.);
#67987=ADVANCED_FACE('',(#7237),#4855,.T.);
#67988=ADVANCED_FACE('',(#7238),#1643,.T.);
#67989=ADVANCED_FACE('',(#7239),#1644,.T.);
#67990=ADVANCED_FACE('',(#7240),#1645,.T.);
#67991=ADVANCED_FACE('',(#7241),#1646,.T.);
#67992=ADVANCED_FACE('',(#7242),#4856,.T.);
#67993=ADVANCED_FACE('',(#7243),#1647,.T.);
#67994=ADVANCED_FACE('',(#7244),#1648,.T.);
#67995=ADVANCED_FACE('',(#7245),#4857,.T.);
#67996=ADVANCED_FACE('',(#7246),#1649,.T.);
#67997=ADVANCED_FACE('',(#7247),#1650,.T.);
#67998=ADVANCED_FACE('',(#7248),#4858,.T.);
#67999=ADVANCED_FACE('',(#7249),#1651,.T.);
#68000=ADVANCED_FACE('',(#7250),#1652,.T.);
#68001=ADVANCED_FACE('',(#7251),#4859,.T.);
#68002=ADVANCED_FACE('',(#7252),#1653,.T.);
#68003=ADVANCED_FACE('',(#7253),#1654,.T.);
#68004=ADVANCED_FACE('',(#7254),#4860,.T.);
#68005=ADVANCED_FACE('',(#7255),#1655,.T.);
#68006=ADVANCED_FACE('',(#7256),#1656,.T.);
#68007=ADVANCED_FACE('',(#7257),#4861,.T.);
#68008=ADVANCED_FACE('',(#7258),#1657,.T.);
#68009=ADVANCED_FACE('',(#7259),#1658,.T.);
#68010=ADVANCED_FACE('',(#7260),#4862,.T.);
#68011=ADVANCED_FACE('',(#7261),#1659,.T.);
#68012=ADVANCED_FACE('',(#7262),#1660,.T.);
#68013=ADVANCED_FACE('',(#7263),#4863,.T.);
#68014=ADVANCED_FACE('',(#7264),#1661,.T.);
#68015=ADVANCED_FACE('',(#7265),#1662,.T.);
#68016=ADVANCED_FACE('',(#7266),#4864,.T.);
#68017=ADVANCED_FACE('',(#7267),#1663,.T.);
#68018=ADVANCED_FACE('',(#7268),#1664,.T.);
#68019=ADVANCED_FACE('',(#7269),#4865,.T.);
#68020=ADVANCED_FACE('',(#7270),#1665,.T.);
#68021=ADVANCED_FACE('',(#7271),#1666,.T.);
#68022=ADVANCED_FACE('',(#7272),#4866,.T.);
#68023=ADVANCED_FACE('',(#7273),#1667,.T.);
#68024=ADVANCED_FACE('',(#7274),#1668,.T.);
#68025=ADVANCED_FACE('',(#7275),#4867,.T.);
#68026=ADVANCED_FACE('',(#7276),#1669,.T.);
#68027=ADVANCED_FACE('',(#7277),#1670,.T.);
#68028=ADVANCED_FACE('',(#7278),#4868,.T.);
#68029=ADVANCED_FACE('',(#7279),#1671,.T.);
#68030=ADVANCED_FACE('',(#7280),#1672,.T.);
#68031=ADVANCED_FACE('',(#7281),#1673,.T.);
#68032=ADVANCED_FACE('',(#7282),#1674,.T.);
#68033=ADVANCED_FACE('',(#7283),#4869,.T.);
#68034=ADVANCED_FACE('',(#7284),#1675,.T.);
#68035=ADVANCED_FACE('',(#7285),#1676,.T.);
#68036=ADVANCED_FACE('',(#7286),#4870,.T.);
#68037=ADVANCED_FACE('',(#7287),#1677,.T.);
#68038=ADVANCED_FACE('',(#7288),#1678,.T.);
#68039=ADVANCED_FACE('',(#7289),#4871,.T.);
#68040=ADVANCED_FACE('',(#7290),#1679,.T.);
#68041=ADVANCED_FACE('',(#7291),#1680,.T.);
#68042=ADVANCED_FACE('',(#7292),#4872,.T.);
#68043=ADVANCED_FACE('',(#7293),#1681,.T.);
#68044=ADVANCED_FACE('',(#7294),#1682,.T.);
#68045=ADVANCED_FACE('',(#7295),#4873,.T.);
#68046=ADVANCED_FACE('',(#7296),#1683,.T.);
#68047=ADVANCED_FACE('',(#7297),#1684,.T.);
#68048=ADVANCED_FACE('',(#7298),#4874,.T.);
#68049=ADVANCED_FACE('',(#7299),#1685,.T.);
#68050=ADVANCED_FACE('',(#7300),#1686,.T.);
#68051=ADVANCED_FACE('',(#7301),#4875,.T.);
#68052=ADVANCED_FACE('',(#7302),#1687,.T.);
#68053=ADVANCED_FACE('',(#7303),#1688,.T.);
#68054=ADVANCED_FACE('',(#7304),#4876,.T.);
#68055=ADVANCED_FACE('',(#7305),#1689,.T.);
#68056=ADVANCED_FACE('',(#7306),#1690,.T.);
#68057=ADVANCED_FACE('',(#7307),#4877,.T.);
#68058=ADVANCED_FACE('',(#7308),#1691,.T.);
#68059=ADVANCED_FACE('',(#7309),#1692,.T.);
#68060=ADVANCED_FACE('',(#7310),#4878,.T.);
#68061=ADVANCED_FACE('',(#7311),#1693,.T.);
#68062=ADVANCED_FACE('',(#7312),#1694,.T.);
#68063=ADVANCED_FACE('',(#7313),#4879,.T.);
#68064=ADVANCED_FACE('',(#7314),#1695,.T.);
#68065=ADVANCED_FACE('',(#7315),#1696,.T.);
#68066=ADVANCED_FACE('',(#7316),#4880,.T.);
#68067=ADVANCED_FACE('',(#7317),#1697,.T.);
#68068=ADVANCED_FACE('',(#7318),#1698,.T.);
#68069=ADVANCED_FACE('',(#7319),#4881,.T.);
#68070=ADVANCED_FACE('',(#7320),#1699,.T.);
#68071=ADVANCED_FACE('',(#7321),#1700,.T.);
#68072=ADVANCED_FACE('',(#7322),#4882,.T.);
#68073=ADVANCED_FACE('',(#7323),#4883,.T.);
#68074=ADVANCED_FACE('',(#7324),#1701,.T.);
#68075=ADVANCED_FACE('',(#7325),#1702,.T.);
#68076=ADVANCED_FACE('',(#7326),#1703,.T.);
#68077=ADVANCED_FACE('',(#7327),#1704,.T.);
#68078=ADVANCED_FACE('',(#7328),#1705,.T.);
#68079=ADVANCED_FACE('',(#7329),#1706,.T.);
#68080=ADVANCED_FACE('',(#7330),#1707,.T.);
#68081=ADVANCED_FACE('',(#7331),#1708,.T.);
#68082=ADVANCED_FACE('',(#7332),#1709,.T.);
#68083=ADVANCED_FACE('',(#7333),#1710,.T.);
#68084=ADVANCED_FACE('',(#7334),#1711,.T.);
#68085=ADVANCED_FACE('',(#7335),#1712,.T.);
#68086=ADVANCED_FACE('',(#7336),#1713,.T.);
#68087=ADVANCED_FACE('',(#7337),#1714,.T.);
#68088=ADVANCED_FACE('',(#7338),#1715,.T.);
#68089=ADVANCED_FACE('',(#7339),#1716,.T.);
#68090=ADVANCED_FACE('',(#7340),#1717,.T.);
#68091=ADVANCED_FACE('',(#7341),#1718,.T.);
#68092=ADVANCED_FACE('',(#7342),#1719,.T.);
#68093=ADVANCED_FACE('',(#7343),#1720,.T.);
#68094=ADVANCED_FACE('',(#7344),#1721,.T.);
#68095=ADVANCED_FACE('',(#7345),#1722,.T.);
#68096=ADVANCED_FACE('',(#7346),#1723,.T.);
#68097=ADVANCED_FACE('',(#7347),#1724,.T.);
#68098=ADVANCED_FACE('',(#7348),#1725,.T.);
#68099=ADVANCED_FACE('',(#7349),#1726,.T.);
#68100=ADVANCED_FACE('',(#7350),#1727,.T.);
#68101=ADVANCED_FACE('',(#7351),#1728,.T.);
#68102=ADVANCED_FACE('',(#7352),#1729,.T.);
#68103=ADVANCED_FACE('',(#7353),#1730,.T.);
#68104=ADVANCED_FACE('',(#7354),#1731,.T.);
#68105=ADVANCED_FACE('',(#7355),#1732,.T.);
#68106=ADVANCED_FACE('',(#7356),#1733,.T.);
#68107=ADVANCED_FACE('',(#7357),#1734,.T.);
#68108=ADVANCED_FACE('',(#7358),#1735,.T.);
#68109=ADVANCED_FACE('',(#7359),#1736,.T.);
#68110=ADVANCED_FACE('',(#7360),#1737,.T.);
#68111=ADVANCED_FACE('',(#7361),#1738,.T.);
#68112=ADVANCED_FACE('',(#7362),#1739,.T.);
#68113=ADVANCED_FACE('',(#7363),#1740,.T.);
#68114=ADVANCED_FACE('',(#7364),#1741,.T.);
#68115=ADVANCED_FACE('',(#7365),#1742,.T.);
#68116=ADVANCED_FACE('',(#7366),#1743,.T.);
#68117=ADVANCED_FACE('',(#7367),#1744,.T.);
#68118=ADVANCED_FACE('',(#7368),#1745,.T.);
#68119=ADVANCED_FACE('',(#7369),#1746,.T.);
#68120=ADVANCED_FACE('',(#7370),#1747,.T.);
#68121=ADVANCED_FACE('',(#7371),#1748,.T.);
#68122=ADVANCED_FACE('',(#7372),#1749,.T.);
#68123=ADVANCED_FACE('',(#7373),#1750,.T.);
#68124=ADVANCED_FACE('',(#7374),#1751,.T.);
#68125=ADVANCED_FACE('',(#7375),#1752,.T.);
#68126=ADVANCED_FACE('',(#7376),#1753,.T.);
#68127=ADVANCED_FACE('',(#7377),#1754,.T.);
#68128=ADVANCED_FACE('',(#7378),#1755,.T.);
#68129=ADVANCED_FACE('',(#7379),#1756,.T.);
#68130=ADVANCED_FACE('',(#7380),#1757,.T.);
#68131=ADVANCED_FACE('',(#7381),#1758,.T.);
#68132=ADVANCED_FACE('',(#7382),#1759,.T.);
#68133=ADVANCED_FACE('',(#7383),#1760,.T.);
#68134=ADVANCED_FACE('',(#7384),#1761,.T.);
#68135=ADVANCED_FACE('',(#7385),#1762,.T.);
#68136=ADVANCED_FACE('',(#7386),#1763,.T.);
#68137=ADVANCED_FACE('',(#7387),#1764,.T.);
#68138=ADVANCED_FACE('',(#7388),#1765,.T.);
#68139=ADVANCED_FACE('',(#7389),#1766,.T.);
#68140=ADVANCED_FACE('',(#7390),#1767,.T.);
#68141=ADVANCED_FACE('',(#7391),#1768,.T.);
#68142=ADVANCED_FACE('',(#7392),#1769,.T.);
#68143=ADVANCED_FACE('',(#7393),#1770,.T.);
#68144=ADVANCED_FACE('',(#7394),#1771,.T.);
#68145=ADVANCED_FACE('',(#7395),#1772,.T.);
#68146=ADVANCED_FACE('',(#7396),#1773,.T.);
#68147=ADVANCED_FACE('',(#7397),#1774,.T.);
#68148=ADVANCED_FACE('',(#7398),#1775,.T.);
#68149=ADVANCED_FACE('',(#7399),#1776,.T.);
#68150=ADVANCED_FACE('',(#7400),#1777,.T.);
#68151=ADVANCED_FACE('',(#7401),#1778,.T.);
#68152=ADVANCED_FACE('',(#7402),#1779,.T.);
#68153=ADVANCED_FACE('',(#7403),#1780,.T.);
#68154=ADVANCED_FACE('',(#7404),#1781,.T.);
#68155=ADVANCED_FACE('',(#7405),#1782,.T.);
#68156=ADVANCED_FACE('',(#7406),#1783,.T.);
#68157=ADVANCED_FACE('',(#7407),#1784,.T.);
#68158=ADVANCED_FACE('',(#7408),#1785,.T.);
#68159=ADVANCED_FACE('',(#7409),#1786,.T.);
#68160=ADVANCED_FACE('',(#7410),#1787,.T.);
#68161=ADVANCED_FACE('',(#7411),#1788,.T.);
#68162=ADVANCED_FACE('',(#7412),#1789,.T.);
#68163=ADVANCED_FACE('',(#7413),#1790,.T.);
#68164=ADVANCED_FACE('',(#7414),#1791,.T.);
#68165=ADVANCED_FACE('',(#7415),#1792,.T.);
#68166=ADVANCED_FACE('',(#7416),#1793,.T.);
#68167=ADVANCED_FACE('',(#7417),#1794,.T.);
#68168=ADVANCED_FACE('',(#7418),#1795,.T.);
#68169=ADVANCED_FACE('',(#7419),#1796,.T.);
#68170=ADVANCED_FACE('',(#7420),#1797,.T.);
#68171=ADVANCED_FACE('',(#7421),#1798,.T.);
#68172=ADVANCED_FACE('',(#7422),#1799,.T.);
#68173=ADVANCED_FACE('',(#7423),#1800,.T.);
#68174=ADVANCED_FACE('',(#7424),#1801,.T.);
#68175=ADVANCED_FACE('',(#7425),#1802,.T.);
#68176=ADVANCED_FACE('',(#7426),#1803,.T.);
#68177=ADVANCED_FACE('',(#7427),#1804,.T.);
#68178=ADVANCED_FACE('',(#7428),#1805,.T.);
#68179=ADVANCED_FACE('',(#7429),#1806,.T.);
#68180=ADVANCED_FACE('',(#7430),#1807,.T.);
#68181=ADVANCED_FACE('',(#7431),#1808,.T.);
#68182=ADVANCED_FACE('',(#7432),#1809,.T.);
#68183=ADVANCED_FACE('',(#7433),#1810,.T.);
#68184=ADVANCED_FACE('',(#7434),#1811,.T.);
#68185=ADVANCED_FACE('',(#7435),#1812,.T.);
#68186=ADVANCED_FACE('',(#7436),#1813,.T.);
#68187=ADVANCED_FACE('',(#7437),#1814,.T.);
#68188=ADVANCED_FACE('',(#7438),#1815,.T.);
#68189=ADVANCED_FACE('',(#7439),#1816,.T.);
#68190=ADVANCED_FACE('',(#7440),#1817,.T.);
#68191=ADVANCED_FACE('',(#7441),#1818,.T.);
#68192=ADVANCED_FACE('',(#7442),#4884,.T.);
#68193=ADVANCED_FACE('',(#7443),#1819,.T.);
#68194=ADVANCED_FACE('',(#7444),#1820,.T.);
#68195=ADVANCED_FACE('',(#7445),#4885,.T.);
#68196=ADVANCED_FACE('',(#7446),#1821,.T.);
#68197=ADVANCED_FACE('',(#7447),#1822,.T.);
#68198=ADVANCED_FACE('',(#7448),#4886,.T.);
#68199=ADVANCED_FACE('',(#7449),#1823,.T.);
#68200=ADVANCED_FACE('',(#7450),#1824,.T.);
#68201=ADVANCED_FACE('',(#7451),#4887,.T.);
#68202=ADVANCED_FACE('',(#7452),#1825,.T.);
#68203=ADVANCED_FACE('',(#7453),#1826,.T.);
#68204=ADVANCED_FACE('',(#7454),#4888,.T.);
#68205=ADVANCED_FACE('',(#7455),#1827,.T.);
#68206=ADVANCED_FACE('',(#7456),#1828,.T.);
#68207=ADVANCED_FACE('',(#7457),#4889,.T.);
#68208=ADVANCED_FACE('',(#7458),#1829,.T.);
#68209=ADVANCED_FACE('',(#7459),#1830,.T.);
#68210=ADVANCED_FACE('',(#7460),#4890,.T.);
#68211=ADVANCED_FACE('',(#7461),#1831,.T.);
#68212=ADVANCED_FACE('',(#7462),#1832,.T.);
#68213=ADVANCED_FACE('',(#7463),#4891,.T.);
#68214=ADVANCED_FACE('',(#7464),#1833,.T.);
#68215=ADVANCED_FACE('',(#7465),#1834,.T.);
#68216=ADVANCED_FACE('',(#7466),#4892,.T.);
#68217=ADVANCED_FACE('',(#7467),#1835,.T.);
#68218=ADVANCED_FACE('',(#7468),#1836,.T.);
#68219=ADVANCED_FACE('',(#7469),#4893,.T.);
#68220=ADVANCED_FACE('',(#7470),#1837,.T.);
#68221=ADVANCED_FACE('',(#7471),#1838,.T.);
#68222=ADVANCED_FACE('',(#7472),#4894,.T.);
#68223=ADVANCED_FACE('',(#7473),#1839,.T.);
#68224=ADVANCED_FACE('',(#7474),#1840,.T.);
#68225=ADVANCED_FACE('',(#7475),#4895,.T.);
#68226=ADVANCED_FACE('',(#7476),#1841,.T.);
#68227=ADVANCED_FACE('',(#7477),#1842,.T.);
#68228=ADVANCED_FACE('',(#7478),#4896,.T.);
#68229=ADVANCED_FACE('',(#7479),#1843,.T.);
#68230=ADVANCED_FACE('',(#7480),#1844,.T.);
#68231=ADVANCED_FACE('',(#7481),#4897,.T.);
#68232=ADVANCED_FACE('',(#7482),#1845,.T.);
#68233=ADVANCED_FACE('',(#7483),#1846,.T.);
#68234=ADVANCED_FACE('',(#7484),#1847,.T.);
#68235=ADVANCED_FACE('',(#7485),#1848,.T.);
#68236=ADVANCED_FACE('',(#7486),#4898,.T.);
#68237=ADVANCED_FACE('',(#7487),#1849,.T.);
#68238=ADVANCED_FACE('',(#7488),#1850,.T.);
#68239=ADVANCED_FACE('',(#7489),#4899,.T.);
#68240=ADVANCED_FACE('',(#7490),#1851,.T.);
#68241=ADVANCED_FACE('',(#7491),#1852,.T.);
#68242=ADVANCED_FACE('',(#7492),#4900,.T.);
#68243=ADVANCED_FACE('',(#7493),#1853,.T.);
#68244=ADVANCED_FACE('',(#7494),#1854,.T.);
#68245=ADVANCED_FACE('',(#7495),#4901,.T.);
#68246=ADVANCED_FACE('',(#7496),#1855,.T.);
#68247=ADVANCED_FACE('',(#7497),#1856,.T.);
#68248=ADVANCED_FACE('',(#7498),#4902,.T.);
#68249=ADVANCED_FACE('',(#7499),#1857,.T.);
#68250=ADVANCED_FACE('',(#7500),#1858,.T.);
#68251=ADVANCED_FACE('',(#7501),#4903,.T.);
#68252=ADVANCED_FACE('',(#7502),#1859,.T.);
#68253=ADVANCED_FACE('',(#7503),#1860,.T.);
#68254=ADVANCED_FACE('',(#7504),#1861,.T.);
#68255=ADVANCED_FACE('',(#7505),#4904,.T.);
#68256=ADVANCED_FACE('',(#7506),#1862,.T.);
#68257=ADVANCED_FACE('',(#7507),#4905,.T.);
#68258=ADVANCED_FACE('',(#7508),#1863,.T.);
#68259=ADVANCED_FACE('',(#7509),#1864,.T.);
#68260=ADVANCED_FACE('',(#7510),#4906,.T.);
#68261=ADVANCED_FACE('',(#7511),#1865,.T.);
#68262=ADVANCED_FACE('',(#7512),#1866,.T.);
#68263=ADVANCED_FACE('',(#7513),#4907,.T.);
#68264=ADVANCED_FACE('',(#7514),#1867,.T.);
#68265=ADVANCED_FACE('',(#7515),#1868,.T.);
#68266=ADVANCED_FACE('',(#7516),#4908,.T.);
#68267=ADVANCED_FACE('',(#7517),#1869,.T.);
#68268=ADVANCED_FACE('',(#7518),#1870,.T.);
#68269=ADVANCED_FACE('',(#7519),#4909,.T.);
#68270=ADVANCED_FACE('',(#7520),#1871,.T.);
#68271=ADVANCED_FACE('',(#7521),#1872,.T.);
#68272=ADVANCED_FACE('',(#7522),#4910,.T.);
#68273=ADVANCED_FACE('',(#7523),#1873,.T.);
#68274=ADVANCED_FACE('',(#7524),#1874,.T.);
#68275=ADVANCED_FACE('',(#7525),#4911,.T.);
#68276=ADVANCED_FACE('',(#7526),#1875,.T.);
#68277=ADVANCED_FACE('',(#7527),#1876,.T.);
#68278=ADVANCED_FACE('',(#7528),#1877,.T.);
#68279=ADVANCED_FACE('',(#7529),#4912,.T.);
#68280=ADVANCED_FACE('',(#7530),#1878,.T.);
#68281=ADVANCED_FACE('',(#7531),#1879,.T.);
#68282=ADVANCED_FACE('',(#7532),#4913,.T.);
#68283=ADVANCED_FACE('',(#7533),#1880,.T.);
#68284=ADVANCED_FACE('',(#7534),#1881,.T.);
#68285=ADVANCED_FACE('',(#7535),#4914,.T.);
#68286=ADVANCED_FACE('',(#7536),#1882,.T.);
#68287=ADVANCED_FACE('',(#7537),#1883,.T.);
#68288=ADVANCED_FACE('',(#7538),#4915,.T.);
#68289=ADVANCED_FACE('',(#7539),#1884,.T.);
#68290=ADVANCED_FACE('',(#7540),#1885,.T.);
#68291=ADVANCED_FACE('',(#7541),#4916,.T.);
#68292=ADVANCED_FACE('',(#7542),#1886,.T.);
#68293=ADVANCED_FACE('',(#7543),#1887,.T.);
#68294=ADVANCED_FACE('',(#7544),#4917,.T.);
#68295=ADVANCED_FACE('',(#7545),#1888,.T.);
#68296=ADVANCED_FACE('',(#7546),#1889,.T.);
#68297=ADVANCED_FACE('',(#7547),#4918,.T.);
#68298=ADVANCED_FACE('',(#7548),#1890,.T.);
#68299=ADVANCED_FACE('',(#7549),#1891,.T.);
#68300=ADVANCED_FACE('',(#7550),#4919,.T.);
#68301=ADVANCED_FACE('',(#7551),#1892,.T.);
#68302=ADVANCED_FACE('',(#7552),#1893,.T.);
#68303=ADVANCED_FACE('',(#7553),#4920,.T.);
#68304=ADVANCED_FACE('',(#7554),#1894,.T.);
#68305=ADVANCED_FACE('',(#7555),#1895,.T.);
#68306=ADVANCED_FACE('',(#7556),#4921,.T.);
#68307=ADVANCED_FACE('',(#7557),#1896,.T.);
#68308=ADVANCED_FACE('',(#7558),#1897,.T.);
#68309=ADVANCED_FACE('',(#7559),#4922,.T.);
#68310=ADVANCED_FACE('',(#7560),#1898,.T.);
#68311=ADVANCED_FACE('',(#7561),#1899,.T.);
#68312=ADVANCED_FACE('',(#7562),#4923,.T.);
#68313=ADVANCED_FACE('',(#7563),#1900,.T.);
#68314=ADVANCED_FACE('',(#7564),#1901,.T.);
#68315=ADVANCED_FACE('',(#7565),#4924,.T.);
#68316=ADVANCED_FACE('',(#7566),#1902,.T.);
#68317=ADVANCED_FACE('',(#7567),#1903,.T.);
#68318=ADVANCED_FACE('',(#7568),#4925,.T.);
#68319=ADVANCED_FACE('',(#7569),#1904,.T.);
#68320=ADVANCED_FACE('',(#7570),#1905,.T.);
#68321=ADVANCED_FACE('',(#7571),#4926,.T.);
#68322=ADVANCED_FACE('',(#7572),#1906,.T.);
#68323=ADVANCED_FACE('',(#7573),#1907,.T.);
#68324=ADVANCED_FACE('',(#7574),#4927,.T.);
#68325=ADVANCED_FACE('',(#7575),#1908,.T.);
#68326=ADVANCED_FACE('',(#7576),#1909,.T.);
#68327=ADVANCED_FACE('',(#7577),#4928,.T.);
#68328=ADVANCED_FACE('',(#7578),#1910,.T.);
#68329=ADVANCED_FACE('',(#7579),#1911,.T.);
#68330=ADVANCED_FACE('',(#7580),#4929,.T.);
#68331=ADVANCED_FACE('',(#7581),#1912,.T.);
#68332=ADVANCED_FACE('',(#7582),#1913,.T.);
#68333=ADVANCED_FACE('',(#7583),#4930,.T.);
#68334=ADVANCED_FACE('',(#7584),#1914,.T.);
#68335=ADVANCED_FACE('',(#7585),#1915,.T.);
#68336=ADVANCED_FACE('',(#7586),#4931,.T.);
#68337=ADVANCED_FACE('',(#7587),#1916,.T.);
#68338=ADVANCED_FACE('',(#7588),#1917,.T.);
#68339=ADVANCED_FACE('',(#7589),#4932,.T.);
#68340=ADVANCED_FACE('',(#7590),#1918,.T.);
#68341=ADVANCED_FACE('',(#7591),#1919,.T.);
#68342=ADVANCED_FACE('',(#7592),#1920,.T.);
#68343=ADVANCED_FACE('',(#7593),#1921,.T.);
#68344=ADVANCED_FACE('',(#7594),#4933,.T.);
#68345=ADVANCED_FACE('',(#7595),#1922,.T.);
#68346=ADVANCED_FACE('',(#7596),#1923,.T.);
#68347=ADVANCED_FACE('',(#7597),#4934,.T.);
#68348=ADVANCED_FACE('',(#7598),#1924,.T.);
#68349=ADVANCED_FACE('',(#7599),#1925,.T.);
#68350=ADVANCED_FACE('',(#7600),#4935,.T.);
#68351=ADVANCED_FACE('',(#7601),#1926,.T.);
#68352=ADVANCED_FACE('',(#7602),#1927,.T.);
#68353=ADVANCED_FACE('',(#7603),#4936,.T.);
#68354=ADVANCED_FACE('',(#7604),#1928,.T.);
#68355=ADVANCED_FACE('',(#7605),#1929,.T.);
#68356=ADVANCED_FACE('',(#7606),#4937,.T.);
#68357=ADVANCED_FACE('',(#7607),#1930,.T.);
#68358=ADVANCED_FACE('',(#7608),#1931,.T.);
#68359=ADVANCED_FACE('',(#7609),#4938,.T.);
#68360=ADVANCED_FACE('',(#7610),#1932,.T.);
#68361=ADVANCED_FACE('',(#7611),#1933,.T.);
#68362=ADVANCED_FACE('',(#7612),#4939,.T.);
#68363=ADVANCED_FACE('',(#7613),#1934,.T.);
#68364=ADVANCED_FACE('',(#7614),#1935,.T.);
#68365=ADVANCED_FACE('',(#7615),#1936,.T.);
#68366=ADVANCED_FACE('',(#7616),#1937,.T.);
#68367=ADVANCED_FACE('',(#7617),#1938,.T.);
#68368=ADVANCED_FACE('',(#7618),#1939,.T.);
#68369=ADVANCED_FACE('',(#7619),#1940,.T.);
#68370=ADVANCED_FACE('',(#7620),#1941,.T.);
#68371=ADVANCED_FACE('',(#7621),#1942,.T.);
#68372=ADVANCED_FACE('',(#7622),#1943,.T.);
#68373=ADVANCED_FACE('',(#7623),#1944,.T.);
#68374=ADVANCED_FACE('',(#7624),#1945,.T.);
#68375=ADVANCED_FACE('',(#7625),#1946,.T.);
#68376=ADVANCED_FACE('',(#7626),#1947,.T.);
#68377=ADVANCED_FACE('',(#7627),#1948,.T.);
#68378=ADVANCED_FACE('',(#7628),#1949,.T.);
#68379=ADVANCED_FACE('',(#7629),#1950,.T.);
#68380=ADVANCED_FACE('',(#7630),#1951,.T.);
#68381=ADVANCED_FACE('',(#7631),#1952,.T.);
#68382=ADVANCED_FACE('',(#7632),#1953,.T.);
#68383=ADVANCED_FACE('',(#7633),#1954,.T.);
#68384=ADVANCED_FACE('',(#7634),#1955,.T.);
#68385=ADVANCED_FACE('',(#7635),#1956,.T.);
#68386=ADVANCED_FACE('',(#7636),#1957,.T.);
#68387=ADVANCED_FACE('',(#7637),#1958,.T.);
#68388=ADVANCED_FACE('',(#7638),#1959,.T.);
#68389=ADVANCED_FACE('',(#7639),#1960,.T.);
#68390=ADVANCED_FACE('',(#7640),#1961,.T.);
#68391=ADVANCED_FACE('',(#7641),#1962,.T.);
#68392=ADVANCED_FACE('',(#7642),#1963,.T.);
#68393=ADVANCED_FACE('',(#7643),#1964,.T.);
#68394=ADVANCED_FACE('',(#7644),#1965,.T.);
#68395=ADVANCED_FACE('',(#7645),#1966,.T.);
#68396=ADVANCED_FACE('',(#7646),#1967,.T.);
#68397=ADVANCED_FACE('',(#7647),#1968,.T.);
#68398=ADVANCED_FACE('',(#7648),#1969,.T.);
#68399=ADVANCED_FACE('',(#7649),#1970,.T.);
#68400=ADVANCED_FACE('',(#7650),#1971,.T.);
#68401=ADVANCED_FACE('',(#7651),#1972,.T.);
#68402=ADVANCED_FACE('',(#7652),#1973,.T.);
#68403=ADVANCED_FACE('',(#7653),#1974,.T.);
#68404=ADVANCED_FACE('',(#7654),#1975,.T.);
#68405=ADVANCED_FACE('',(#7655),#1976,.T.);
#68406=ADVANCED_FACE('',(#7656),#1977,.T.);
#68407=ADVANCED_FACE('',(#7657),#1978,.T.);
#68408=ADVANCED_FACE('',(#7658),#1979,.T.);
#68409=ADVANCED_FACE('',(#7659),#1980,.T.);
#68410=ADVANCED_FACE('',(#7660),#1981,.T.);
#68411=ADVANCED_FACE('',(#7661),#1982,.T.);
#68412=ADVANCED_FACE('',(#7662),#1983,.T.);
#68413=ADVANCED_FACE('',(#7663),#1984,.T.);
#68414=ADVANCED_FACE('',(#7664),#1985,.T.);
#68415=ADVANCED_FACE('',(#7665),#1986,.T.);
#68416=ADVANCED_FACE('',(#7666),#1987,.T.);
#68417=ADVANCED_FACE('',(#7667),#1988,.T.);
#68418=ADVANCED_FACE('',(#7668),#1989,.T.);
#68419=ADVANCED_FACE('',(#7669),#1990,.T.);
#68420=ADVANCED_FACE('',(#7670),#1991,.T.);
#68421=ADVANCED_FACE('',(#7671),#1992,.T.);
#68422=ADVANCED_FACE('',(#7672),#1993,.T.);
#68423=ADVANCED_FACE('',(#7673),#1994,.T.);
#68424=ADVANCED_FACE('',(#7674),#1995,.T.);
#68425=ADVANCED_FACE('',(#7675),#1996,.T.);
#68426=ADVANCED_FACE('',(#7676),#1997,.T.);
#68427=ADVANCED_FACE('',(#7677),#1998,.T.);
#68428=ADVANCED_FACE('',(#7678),#1999,.T.);
#68429=ADVANCED_FACE('',(#7679),#2000,.T.);
#68430=ADVANCED_FACE('',(#7680),#2001,.T.);
#68431=ADVANCED_FACE('',(#7681),#2002,.T.);
#68432=ADVANCED_FACE('',(#7682),#2003,.T.);
#68433=ADVANCED_FACE('',(#7683),#2004,.T.);
#68434=ADVANCED_FACE('',(#7684),#2005,.T.);
#68435=ADVANCED_FACE('',(#7685),#2006,.T.);
#68436=ADVANCED_FACE('',(#7686),#2007,.T.);
#68437=ADVANCED_FACE('',(#7687),#2008,.T.);
#68438=ADVANCED_FACE('',(#7688),#2009,.T.);
#68439=ADVANCED_FACE('',(#7689),#2010,.T.);
#68440=ADVANCED_FACE('',(#7690),#2011,.T.);
#68441=ADVANCED_FACE('',(#7691),#2012,.T.);
#68442=ADVANCED_FACE('',(#7692),#2013,.T.);
#68443=ADVANCED_FACE('',(#7693),#2014,.T.);
#68444=ADVANCED_FACE('',(#7694),#2015,.T.);
#68445=ADVANCED_FACE('',(#7695),#2016,.T.);
#68446=ADVANCED_FACE('',(#7696),#2017,.T.);
#68447=ADVANCED_FACE('',(#7697),#2018,.T.);
#68448=ADVANCED_FACE('',(#7698),#2019,.T.);
#68449=ADVANCED_FACE('',(#7699),#2020,.T.);
#68450=ADVANCED_FACE('',(#7700),#2021,.T.);
#68451=ADVANCED_FACE('',(#7701),#2022,.T.);
#68452=ADVANCED_FACE('',(#7702),#2023,.T.);
#68453=ADVANCED_FACE('',(#7703),#2024,.T.);
#68454=ADVANCED_FACE('',(#7704),#2025,.T.);
#68455=ADVANCED_FACE('',(#7705),#2026,.T.);
#68456=ADVANCED_FACE('',(#7706),#2027,.T.);
#68457=ADVANCED_FACE('',(#7707),#2028,.T.);
#68458=ADVANCED_FACE('',(#7708),#2029,.T.);
#68459=ADVANCED_FACE('',(#7709),#2030,.T.);
#68460=ADVANCED_FACE('',(#7710),#2031,.T.);
#68461=ADVANCED_FACE('',(#7711),#2032,.T.);
#68462=ADVANCED_FACE('',(#7712),#2033,.T.);
#68463=ADVANCED_FACE('',(#7713),#2034,.T.);
#68464=ADVANCED_FACE('',(#7714),#2035,.T.);
#68465=ADVANCED_FACE('',(#7715),#2036,.T.);
#68466=ADVANCED_FACE('',(#7716),#2037,.T.);
#68467=ADVANCED_FACE('',(#7717),#2038,.T.);
#68468=ADVANCED_FACE('',(#7718),#2039,.T.);
#68469=ADVANCED_FACE('',(#7719),#2040,.T.);
#68470=ADVANCED_FACE('',(#7720),#2041,.T.);
#68471=ADVANCED_FACE('',(#7721),#2042,.T.);
#68472=ADVANCED_FACE('',(#7722),#2043,.T.);
#68473=ADVANCED_FACE('',(#7723),#2044,.T.);
#68474=ADVANCED_FACE('',(#7724),#2045,.T.);
#68475=ADVANCED_FACE('',(#7725),#2046,.T.);
#68476=ADVANCED_FACE('',(#7726),#2047,.T.);
#68477=ADVANCED_FACE('',(#7727),#2048,.T.);
#68478=ADVANCED_FACE('',(#7728),#2049,.T.);
#68479=ADVANCED_FACE('',(#7729),#2050,.T.);
#68480=ADVANCED_FACE('',(#7730),#2051,.T.);
#68481=ADVANCED_FACE('',(#7731),#4940,.T.);
#68482=ADVANCED_FACE('',(#7732),#2052,.T.);
#68483=ADVANCED_FACE('',(#7733),#2053,.T.);
#68484=ADVANCED_FACE('',(#7734),#4941,.T.);
#68485=ADVANCED_FACE('',(#7735),#2054,.T.);
#68486=ADVANCED_FACE('',(#7736),#2055,.T.);
#68487=ADVANCED_FACE('',(#7737),#4942,.T.);
#68488=ADVANCED_FACE('',(#7738),#2056,.T.);
#68489=ADVANCED_FACE('',(#7739),#2057,.T.);
#68490=ADVANCED_FACE('',(#7740),#4943,.T.);
#68491=ADVANCED_FACE('',(#7741),#2058,.T.);
#68492=ADVANCED_FACE('',(#7742),#2059,.T.);
#68493=ADVANCED_FACE('',(#7743),#4944,.T.);
#68494=ADVANCED_FACE('',(#7744),#2060,.T.);
#68495=ADVANCED_FACE('',(#7745),#2061,.T.);
#68496=ADVANCED_FACE('',(#7746),#4945,.T.);
#68497=ADVANCED_FACE('',(#7747),#2062,.T.);
#68498=ADVANCED_FACE('',(#7748),#2063,.T.);
#68499=ADVANCED_FACE('',(#7749),#2064,.T.);
#68500=ADVANCED_FACE('',(#7750),#2065,.T.);
#68501=ADVANCED_FACE('',(#7751),#4946,.T.);
#68502=ADVANCED_FACE('',(#7752),#2066,.T.);
#68503=ADVANCED_FACE('',(#7753),#2067,.T.);
#68504=ADVANCED_FACE('',(#7754),#4947,.T.);
#68505=ADVANCED_FACE('',(#7755),#2068,.T.);
#68506=ADVANCED_FACE('',(#7756),#2069,.T.);
#68507=ADVANCED_FACE('',(#7757),#4948,.T.);
#68508=ADVANCED_FACE('',(#7758),#2070,.T.);
#68509=ADVANCED_FACE('',(#7759),#2071,.T.);
#68510=ADVANCED_FACE('',(#7760),#4949,.T.);
#68511=ADVANCED_FACE('',(#7761),#2072,.T.);
#68512=ADVANCED_FACE('',(#7762),#2073,.T.);
#68513=ADVANCED_FACE('',(#7763),#4950,.T.);
#68514=ADVANCED_FACE('',(#7764),#2074,.T.);
#68515=ADVANCED_FACE('',(#7765),#2075,.T.);
#68516=ADVANCED_FACE('',(#7766),#4951,.T.);
#68517=ADVANCED_FACE('',(#7767),#2076,.T.);
#68518=ADVANCED_FACE('',(#7768),#2077,.T.);
#68519=ADVANCED_FACE('',(#7769),#4952,.T.);
#68520=ADVANCED_FACE('',(#7770),#2078,.T.);
#68521=ADVANCED_FACE('',(#7771),#2079,.T.);
#68522=ADVANCED_FACE('',(#7772),#4953,.T.);
#68523=ADVANCED_FACE('',(#7773),#2080,.T.);
#68524=ADVANCED_FACE('',(#7774),#2081,.T.);
#68525=ADVANCED_FACE('',(#7775),#4954,.T.);
#68526=ADVANCED_FACE('',(#7776),#2082,.T.);
#68527=ADVANCED_FACE('',(#7777),#2083,.T.);
#68528=ADVANCED_FACE('',(#7778),#4955,.T.);
#68529=ADVANCED_FACE('',(#7779),#2084,.T.);
#68530=ADVANCED_FACE('',(#7780),#2085,.T.);
#68531=ADVANCED_FACE('',(#7781),#4956,.T.);
#68532=ADVANCED_FACE('',(#7782),#2086,.T.);
#68533=ADVANCED_FACE('',(#7783),#2087,.T.);
#68534=ADVANCED_FACE('',(#7784),#4957,.T.);
#68535=ADVANCED_FACE('',(#7785),#2088,.T.);
#68536=ADVANCED_FACE('',(#7786),#2089,.T.);
#68537=ADVANCED_FACE('',(#7787),#4958,.T.);
#68538=ADVANCED_FACE('',(#7788),#2090,.T.);
#68539=ADVANCED_FACE('',(#7789),#2091,.T.);
#68540=ADVANCED_FACE('',(#7790),#2092,.T.);
#68541=ADVANCED_FACE('',(#7791),#4959,.T.);
#68542=ADVANCED_FACE('',(#7792),#2093,.T.);
#68543=ADVANCED_FACE('',(#7793),#4960,.T.);
#68544=ADVANCED_FACE('',(#7794),#2094,.T.);
#68545=ADVANCED_FACE('',(#7795),#2095,.T.);
#68546=ADVANCED_FACE('',(#7796),#4961,.T.);
#68547=ADVANCED_FACE('',(#7797),#2096,.T.);
#68548=ADVANCED_FACE('',(#7798),#2097,.T.);
#68549=ADVANCED_FACE('',(#7799),#4962,.T.);
#68550=ADVANCED_FACE('',(#7800),#2098,.T.);
#68551=ADVANCED_FACE('',(#7801),#2099,.T.);
#68552=ADVANCED_FACE('',(#7802),#4963,.T.);
#68553=ADVANCED_FACE('',(#7803),#2100,.T.);
#68554=ADVANCED_FACE('',(#7804),#2101,.T.);
#68555=ADVANCED_FACE('',(#7805),#4964,.T.);
#68556=ADVANCED_FACE('',(#7806),#2102,.T.);
#68557=ADVANCED_FACE('',(#7807),#2103,.T.);
#68558=ADVANCED_FACE('',(#7808),#4965,.T.);
#68559=ADVANCED_FACE('',(#7809),#2104,.T.);
#68560=ADVANCED_FACE('',(#7810),#2105,.T.);
#68561=ADVANCED_FACE('',(#7811),#4966,.T.);
#68562=ADVANCED_FACE('',(#7812),#2106,.T.);
#68563=ADVANCED_FACE('',(#7813),#4967,.T.);
#68564=ADVANCED_FACE('',(#7814),#2107,.T.);
#68565=ADVANCED_FACE('',(#7815),#2108,.T.);
#68566=ADVANCED_FACE('',(#7816),#2109,.T.);
#68567=ADVANCED_FACE('',(#7817),#2110,.T.);
#68568=ADVANCED_FACE('',(#7818),#4968,.T.);
#68569=ADVANCED_FACE('',(#7819),#2111,.T.);
#68570=ADVANCED_FACE('',(#7820),#2112,.T.);
#68571=ADVANCED_FACE('',(#7821),#4969,.T.);
#68572=ADVANCED_FACE('',(#7822),#2113,.T.);
#68573=ADVANCED_FACE('',(#7823),#2114,.T.);
#68574=ADVANCED_FACE('',(#7824),#4970,.T.);
#68575=ADVANCED_FACE('',(#7825),#2115,.T.);
#68576=ADVANCED_FACE('',(#7826),#2116,.T.);
#68577=ADVANCED_FACE('',(#7827),#4971,.T.);
#68578=ADVANCED_FACE('',(#7828),#2117,.T.);
#68579=ADVANCED_FACE('',(#7829),#2118,.T.);
#68580=ADVANCED_FACE('',(#7830),#4972,.T.);
#68581=ADVANCED_FACE('',(#7831),#2119,.T.);
#68582=ADVANCED_FACE('',(#7832),#2120,.T.);
#68583=ADVANCED_FACE('',(#7833),#4973,.T.);
#68584=ADVANCED_FACE('',(#7834),#2121,.T.);
#68585=ADVANCED_FACE('',(#7835),#2122,.T.);
#68586=ADVANCED_FACE('',(#7836),#4974,.T.);
#68587=ADVANCED_FACE('',(#7837),#2123,.T.);
#68588=ADVANCED_FACE('',(#7838),#2124,.T.);
#68589=ADVANCED_FACE('',(#7839),#4975,.T.);
#68590=ADVANCED_FACE('',(#7840),#2125,.T.);
#68591=ADVANCED_FACE('',(#7841),#2126,.T.);
#68592=ADVANCED_FACE('',(#7842),#4976,.T.);
#68593=ADVANCED_FACE('',(#7843),#2127,.T.);
#68594=ADVANCED_FACE('',(#7844),#2128,.T.);
#68595=ADVANCED_FACE('',(#7845),#4977,.T.);
#68596=ADVANCED_FACE('',(#7846),#2129,.T.);
#68597=ADVANCED_FACE('',(#7847),#2130,.T.);
#68598=ADVANCED_FACE('',(#7848),#4978,.T.);
#68599=ADVANCED_FACE('',(#7849),#2131,.T.);
#68600=ADVANCED_FACE('',(#7850),#2132,.T.);
#68601=ADVANCED_FACE('',(#7851),#4979,.T.);
#68602=ADVANCED_FACE('',(#7852),#2133,.T.);
#68603=ADVANCED_FACE('',(#7853),#2134,.T.);
#68604=ADVANCED_FACE('',(#7854),#4980,.T.);
#68605=ADVANCED_FACE('',(#7855),#2135,.T.);
#68606=ADVANCED_FACE('',(#7856),#2136,.T.);
#68607=ADVANCED_FACE('',(#7857),#2137,.T.);
#68608=ADVANCED_FACE('',(#7858),#2138,.T.);
#68609=ADVANCED_FACE('',(#7859),#4981,.T.);
#68610=ADVANCED_FACE('',(#7860),#2139,.T.);
#68611=ADVANCED_FACE('',(#7861),#2140,.T.);
#68612=ADVANCED_FACE('',(#7862),#4982,.T.);
#68613=ADVANCED_FACE('',(#7863),#2141,.T.);
#68614=ADVANCED_FACE('',(#7864),#2142,.T.);
#68615=ADVANCED_FACE('',(#7865),#4983,.T.);
#68616=ADVANCED_FACE('',(#7866),#2143,.T.);
#68617=ADVANCED_FACE('',(#7867),#2144,.T.);
#68618=ADVANCED_FACE('',(#7868),#4984,.T.);
#68619=ADVANCED_FACE('',(#7869),#2145,.T.);
#68620=ADVANCED_FACE('',(#7870),#2146,.T.);
#68621=ADVANCED_FACE('',(#7871),#4985,.T.);
#68622=ADVANCED_FACE('',(#7872),#2147,.T.);
#68623=ADVANCED_FACE('',(#7873),#2148,.T.);
#68624=ADVANCED_FACE('',(#7874),#4986,.T.);
#68625=ADVANCED_FACE('',(#7875),#2149,.T.);
#68626=ADVANCED_FACE('',(#7876),#2150,.T.);
#68627=ADVANCED_FACE('',(#7877),#4987,.T.);
#68628=ADVANCED_FACE('',(#7878),#2151,.T.);
#68629=ADVANCED_FACE('',(#7879),#2152,.T.);
#68630=ADVANCED_FACE('',(#7880),#4988,.T.);
#68631=ADVANCED_FACE('',(#7881),#2153,.T.);
#68632=ADVANCED_FACE('',(#7882),#2154,.T.);
#68633=ADVANCED_FACE('',(#7883),#4989,.T.);
#68634=ADVANCED_FACE('',(#7884),#2155,.T.);
#68635=ADVANCED_FACE('',(#7885),#2156,.T.);
#68636=ADVANCED_FACE('',(#7886),#4990,.T.);
#68637=ADVANCED_FACE('',(#7887),#2157,.T.);
#68638=ADVANCED_FACE('',(#7888),#2158,.T.);
#68639=ADVANCED_FACE('',(#7889),#4991,.T.);
#68640=ADVANCED_FACE('',(#7890),#2159,.T.);
#68641=ADVANCED_FACE('',(#7891),#2160,.T.);
#68642=ADVANCED_FACE('',(#7892),#4992,.T.);
#68643=ADVANCED_FACE('',(#7893),#2161,.T.);
#68644=ADVANCED_FACE('',(#7894),#2162,.T.);
#68645=ADVANCED_FACE('',(#7895),#4993,.T.);
#68646=ADVANCED_FACE('',(#7896),#2163,.T.);
#68647=ADVANCED_FACE('',(#7897),#2164,.T.);
#68648=ADVANCED_FACE('',(#7898),#4994,.T.);
#68649=ADVANCED_FACE('',(#7899),#4995,.T.);
#68650=ADVANCED_FACE('',(#7900),#2165,.T.);
#68651=ADVANCED_FACE('',(#7901),#2166,.T.);
#68652=ADVANCED_FACE('',(#7902),#2167,.T.);
#68653=ADVANCED_FACE('',(#7903),#2168,.T.);
#68654=ADVANCED_FACE('',(#7904),#2169,.T.);
#68655=ADVANCED_FACE('',(#7905),#2170,.T.);
#68656=ADVANCED_FACE('',(#7906),#2171,.T.);
#68657=ADVANCED_FACE('',(#7907),#2172,.T.);
#68658=ADVANCED_FACE('',(#7908),#2173,.T.);
#68659=ADVANCED_FACE('',(#7909),#2174,.T.);
#68660=ADVANCED_FACE('',(#7910),#2175,.T.);
#68661=ADVANCED_FACE('',(#7911),#2176,.T.);
#68662=ADVANCED_FACE('',(#7912),#2177,.T.);
#68663=ADVANCED_FACE('',(#7913),#2178,.T.);
#68664=ADVANCED_FACE('',(#7914),#2179,.T.);
#68665=ADVANCED_FACE('',(#7915),#2180,.T.);
#68666=ADVANCED_FACE('',(#7916),#2181,.T.);
#68667=ADVANCED_FACE('',(#7917),#2182,.T.);
#68668=ADVANCED_FACE('',(#7918),#2183,.T.);
#68669=ADVANCED_FACE('',(#7919),#2184,.T.);
#68670=ADVANCED_FACE('',(#7920),#2185,.T.);
#68671=ADVANCED_FACE('',(#7921),#2186,.T.);
#68672=ADVANCED_FACE('',(#7922),#2187,.T.);
#68673=ADVANCED_FACE('',(#7923),#2188,.T.);
#68674=ADVANCED_FACE('',(#7924),#2189,.T.);
#68675=ADVANCED_FACE('',(#7925),#2190,.T.);
#68676=ADVANCED_FACE('',(#7926),#2191,.T.);
#68677=ADVANCED_FACE('',(#7927),#2192,.T.);
#68678=ADVANCED_FACE('',(#7928),#2193,.T.);
#68679=ADVANCED_FACE('',(#7929),#2194,.T.);
#68680=ADVANCED_FACE('',(#7930),#2195,.T.);
#68681=ADVANCED_FACE('',(#7931),#2196,.T.);
#68682=ADVANCED_FACE('',(#7932),#2197,.T.);
#68683=ADVANCED_FACE('',(#7933),#2198,.T.);
#68684=ADVANCED_FACE('',(#7934),#2199,.T.);
#68685=ADVANCED_FACE('',(#7935),#2200,.T.);
#68686=ADVANCED_FACE('',(#7936),#2201,.T.);
#68687=ADVANCED_FACE('',(#7937),#2202,.T.);
#68688=ADVANCED_FACE('',(#7938),#2203,.T.);
#68689=ADVANCED_FACE('',(#7939),#2204,.T.);
#68690=ADVANCED_FACE('',(#7940),#2205,.T.);
#68691=ADVANCED_FACE('',(#7941),#2206,.T.);
#68692=ADVANCED_FACE('',(#7942),#2207,.T.);
#68693=ADVANCED_FACE('',(#7943),#2208,.T.);
#68694=ADVANCED_FACE('',(#7944),#2209,.T.);
#68695=ADVANCED_FACE('',(#7945),#2210,.T.);
#68696=ADVANCED_FACE('',(#7946),#2211,.T.);
#68697=ADVANCED_FACE('',(#7947),#2212,.T.);
#68698=ADVANCED_FACE('',(#7948),#2213,.T.);
#68699=ADVANCED_FACE('',(#7949),#2214,.T.);
#68700=ADVANCED_FACE('',(#7950),#2215,.T.);
#68701=ADVANCED_FACE('',(#7951),#2216,.T.);
#68702=ADVANCED_FACE('',(#7952),#2217,.T.);
#68703=ADVANCED_FACE('',(#7953),#2218,.T.);
#68704=ADVANCED_FACE('',(#7954),#2219,.T.);
#68705=ADVANCED_FACE('',(#7955),#2220,.T.);
#68706=ADVANCED_FACE('',(#7956),#2221,.T.);
#68707=ADVANCED_FACE('',(#7957),#2222,.T.);
#68708=ADVANCED_FACE('',(#7958),#2223,.T.);
#68709=ADVANCED_FACE('',(#7959),#2224,.T.);
#68710=ADVANCED_FACE('',(#7960),#2225,.T.);
#68711=ADVANCED_FACE('',(#7961),#2226,.T.);
#68712=ADVANCED_FACE('',(#7962),#2227,.T.);
#68713=ADVANCED_FACE('',(#7963),#2228,.T.);
#68714=ADVANCED_FACE('',(#7964),#2229,.T.);
#68715=ADVANCED_FACE('',(#7965),#2230,.T.);
#68716=ADVANCED_FACE('',(#7966),#2231,.T.);
#68717=ADVANCED_FACE('',(#7967),#2232,.T.);
#68718=ADVANCED_FACE('',(#7968),#2233,.T.);
#68719=ADVANCED_FACE('',(#7969),#2234,.T.);
#68720=ADVANCED_FACE('',(#7970),#2235,.T.);
#68721=ADVANCED_FACE('',(#7971),#2236,.T.);
#68722=ADVANCED_FACE('',(#7972),#2237,.T.);
#68723=ADVANCED_FACE('',(#7973),#2238,.T.);
#68724=ADVANCED_FACE('',(#7974),#2239,.T.);
#68725=ADVANCED_FACE('',(#7975),#2240,.T.);
#68726=ADVANCED_FACE('',(#7976),#2241,.T.);
#68727=ADVANCED_FACE('',(#7977),#2242,.T.);
#68728=ADVANCED_FACE('',(#7978),#2243,.T.);
#68729=ADVANCED_FACE('',(#7979),#2244,.T.);
#68730=ADVANCED_FACE('',(#7980),#2245,.T.);
#68731=ADVANCED_FACE('',(#7981),#2246,.T.);
#68732=ADVANCED_FACE('',(#7982),#2247,.T.);
#68733=ADVANCED_FACE('',(#7983),#2248,.T.);
#68734=ADVANCED_FACE('',(#7984),#2249,.T.);
#68735=ADVANCED_FACE('',(#7985),#2250,.T.);
#68736=ADVANCED_FACE('',(#7986),#2251,.T.);
#68737=ADVANCED_FACE('',(#7987),#2252,.T.);
#68738=ADVANCED_FACE('',(#7988),#2253,.T.);
#68739=ADVANCED_FACE('',(#7989),#2254,.T.);
#68740=ADVANCED_FACE('',(#7990),#2255,.T.);
#68741=ADVANCED_FACE('',(#7991),#2256,.T.);
#68742=ADVANCED_FACE('',(#7992),#2257,.T.);
#68743=ADVANCED_FACE('',(#7993),#2258,.T.);
#68744=ADVANCED_FACE('',(#7994),#2259,.T.);
#68745=ADVANCED_FACE('',(#7995),#2260,.T.);
#68746=ADVANCED_FACE('',(#7996),#2261,.T.);
#68747=ADVANCED_FACE('',(#7997),#2262,.T.);
#68748=ADVANCED_FACE('',(#7998),#2263,.T.);
#68749=ADVANCED_FACE('',(#7999),#2264,.T.);
#68750=ADVANCED_FACE('',(#8000),#2265,.T.);
#68751=ADVANCED_FACE('',(#8001),#2266,.T.);
#68752=ADVANCED_FACE('',(#8002),#2267,.T.);
#68753=ADVANCED_FACE('',(#8003),#2268,.T.);
#68754=ADVANCED_FACE('',(#8004),#2269,.T.);
#68755=ADVANCED_FACE('',(#8005),#2270,.T.);
#68756=ADVANCED_FACE('',(#8006),#2271,.T.);
#68757=ADVANCED_FACE('',(#8007),#2272,.T.);
#68758=ADVANCED_FACE('',(#8008),#2273,.T.);
#68759=ADVANCED_FACE('',(#8009),#2274,.T.);
#68760=ADVANCED_FACE('',(#8010),#2275,.T.);
#68761=ADVANCED_FACE('',(#8011),#2276,.T.);
#68762=ADVANCED_FACE('',(#8012),#2277,.T.);
#68763=ADVANCED_FACE('',(#8013),#2278,.T.);
#68764=ADVANCED_FACE('',(#8014),#2279,.T.);
#68765=ADVANCED_FACE('',(#8015),#2280,.T.);
#68766=ADVANCED_FACE('',(#8016),#2281,.T.);
#68767=ADVANCED_FACE('',(#8017),#2282,.T.);
#68768=ADVANCED_FACE('',(#8018),#4996,.T.);
#68769=ADVANCED_FACE('',(#8019),#2283,.T.);
#68770=ADVANCED_FACE('',(#8020),#2284,.T.);
#68771=ADVANCED_FACE('',(#8021),#4997,.T.);
#68772=ADVANCED_FACE('',(#8022),#2285,.T.);
#68773=ADVANCED_FACE('',(#8023),#2286,.T.);
#68774=ADVANCED_FACE('',(#8024),#4998,.T.);
#68775=ADVANCED_FACE('',(#8025),#2287,.T.);
#68776=ADVANCED_FACE('',(#8026),#2288,.T.);
#68777=ADVANCED_FACE('',(#8027),#4999,.T.);
#68778=ADVANCED_FACE('',(#8028),#2289,.T.);
#68779=ADVANCED_FACE('',(#8029),#2290,.T.);
#68780=ADVANCED_FACE('',(#8030),#5000,.T.);
#68781=ADVANCED_FACE('',(#8031),#2291,.T.);
#68782=ADVANCED_FACE('',(#8032),#2292,.T.);
#68783=ADVANCED_FACE('',(#8033),#5001,.T.);
#68784=ADVANCED_FACE('',(#8034),#2293,.T.);
#68785=ADVANCED_FACE('',(#8035),#2294,.T.);
#68786=ADVANCED_FACE('',(#8036),#5002,.T.);
#68787=ADVANCED_FACE('',(#8037),#2295,.T.);
#68788=ADVANCED_FACE('',(#8038),#2296,.T.);
#68789=ADVANCED_FACE('',(#8039),#5003,.T.);
#68790=ADVANCED_FACE('',(#8040),#2297,.T.);
#68791=ADVANCED_FACE('',(#8041),#2298,.T.);
#68792=ADVANCED_FACE('',(#8042),#5004,.T.);
#68793=ADVANCED_FACE('',(#8043),#2299,.T.);
#68794=ADVANCED_FACE('',(#8044),#2300,.T.);
#68795=ADVANCED_FACE('',(#8045),#5005,.T.);
#68796=ADVANCED_FACE('',(#8046),#2301,.T.);
#68797=ADVANCED_FACE('',(#8047),#2302,.T.);
#68798=ADVANCED_FACE('',(#8048),#5006,.T.);
#68799=ADVANCED_FACE('',(#8049),#2303,.T.);
#68800=ADVANCED_FACE('',(#8050),#2304,.T.);
#68801=ADVANCED_FACE('',(#8051),#5007,.T.);
#68802=ADVANCED_FACE('',(#8052),#2305,.T.);
#68803=ADVANCED_FACE('',(#8053),#2306,.T.);
#68804=ADVANCED_FACE('',(#8054),#5008,.T.);
#68805=ADVANCED_FACE('',(#8055),#2307,.T.);
#68806=ADVANCED_FACE('',(#8056),#2308,.T.);
#68807=ADVANCED_FACE('',(#8057),#5009,.T.);
#68808=ADVANCED_FACE('',(#8058),#2309,.T.);
#68809=ADVANCED_FACE('',(#8059),#2310,.T.);
#68810=ADVANCED_FACE('',(#8060),#2311,.T.);
#68811=ADVANCED_FACE('',(#8061),#2312,.T.);
#68812=ADVANCED_FACE('',(#8062),#5010,.T.);
#68813=ADVANCED_FACE('',(#8063),#2313,.T.);
#68814=ADVANCED_FACE('',(#8064),#2314,.T.);
#68815=ADVANCED_FACE('',(#8065),#5011,.T.);
#68816=ADVANCED_FACE('',(#8066),#2315,.T.);
#68817=ADVANCED_FACE('',(#8067),#2316,.T.);
#68818=ADVANCED_FACE('',(#8068),#5012,.T.);
#68819=ADVANCED_FACE('',(#8069),#2317,.T.);
#68820=ADVANCED_FACE('',(#8070),#2318,.T.);
#68821=ADVANCED_FACE('',(#8071),#5013,.T.);
#68822=ADVANCED_FACE('',(#8072),#2319,.T.);
#68823=ADVANCED_FACE('',(#8073),#2320,.T.);
#68824=ADVANCED_FACE('',(#8074),#5014,.T.);
#68825=ADVANCED_FACE('',(#8075),#2321,.T.);
#68826=ADVANCED_FACE('',(#8076),#2322,.T.);
#68827=ADVANCED_FACE('',(#8077),#2323,.T.);
#68828=ADVANCED_FACE('',(#8078),#5015,.T.);
#68829=ADVANCED_FACE('',(#8079),#2324,.T.);
#68830=ADVANCED_FACE('',(#8080),#5016,.T.);
#68831=ADVANCED_FACE('',(#8081),#2325,.T.);
#68832=ADVANCED_FACE('',(#8082),#2326,.T.);
#68833=ADVANCED_FACE('',(#8083),#5017,.T.);
#68834=ADVANCED_FACE('',(#8084),#2327,.T.);
#68835=ADVANCED_FACE('',(#8085),#2328,.T.);
#68836=ADVANCED_FACE('',(#8086),#5018,.T.);
#68837=ADVANCED_FACE('',(#8087),#2329,.T.);
#68838=ADVANCED_FACE('',(#8088),#2330,.T.);
#68839=ADVANCED_FACE('',(#8089),#5019,.T.);
#68840=ADVANCED_FACE('',(#8090),#2331,.T.);
#68841=ADVANCED_FACE('',(#8091),#2332,.T.);
#68842=ADVANCED_FACE('',(#8092),#5020,.T.);
#68843=ADVANCED_FACE('',(#8093),#2333,.T.);
#68844=ADVANCED_FACE('',(#8094),#2334,.T.);
#68845=ADVANCED_FACE('',(#8095),#5021,.T.);
#68846=ADVANCED_FACE('',(#8096),#2335,.T.);
#68847=ADVANCED_FACE('',(#8097),#2336,.T.);
#68848=ADVANCED_FACE('',(#8098),#5022,.T.);
#68849=ADVANCED_FACE('',(#8099),#2337,.T.);
#68850=ADVANCED_FACE('',(#8100),#2338,.T.);
#68851=ADVANCED_FACE('',(#8101),#5023,.T.);
#68852=ADVANCED_FACE('',(#8102),#2339,.T.);
#68853=ADVANCED_FACE('',(#8103),#2340,.T.);
#68854=ADVANCED_FACE('',(#8104),#2341,.T.);
#68855=ADVANCED_FACE('',(#8105),#5024,.T.);
#68856=ADVANCED_FACE('',(#8106),#2342,.T.);
#68857=ADVANCED_FACE('',(#8107),#2343,.T.);
#68858=ADVANCED_FACE('',(#8108),#5025,.T.);
#68859=ADVANCED_FACE('',(#8109),#2344,.T.);
#68860=ADVANCED_FACE('',(#8110),#2345,.T.);
#68861=ADVANCED_FACE('',(#8111),#5026,.T.);
#68862=ADVANCED_FACE('',(#8112),#2346,.T.);
#68863=ADVANCED_FACE('',(#8113),#2347,.T.);
#68864=ADVANCED_FACE('',(#8114),#5027,.T.);
#68865=ADVANCED_FACE('',(#8115),#2348,.T.);
#68866=ADVANCED_FACE('',(#8116),#2349,.T.);
#68867=ADVANCED_FACE('',(#8117),#5028,.T.);
#68868=ADVANCED_FACE('',(#8118),#2350,.T.);
#68869=ADVANCED_FACE('',(#8119),#2351,.T.);
#68870=ADVANCED_FACE('',(#8120),#5029,.T.);
#68871=ADVANCED_FACE('',(#8121),#2352,.T.);
#68872=ADVANCED_FACE('',(#8122),#2353,.T.);
#68873=ADVANCED_FACE('',(#8123),#5030,.T.);
#68874=ADVANCED_FACE('',(#8124),#2354,.T.);
#68875=ADVANCED_FACE('',(#8125),#2355,.T.);
#68876=ADVANCED_FACE('',(#8126),#5031,.T.);
#68877=ADVANCED_FACE('',(#8127),#2356,.T.);
#68878=ADVANCED_FACE('',(#8128),#2357,.T.);
#68879=ADVANCED_FACE('',(#8129),#5032,.T.);
#68880=ADVANCED_FACE('',(#8130),#2358,.T.);
#68881=ADVANCED_FACE('',(#8131),#2359,.T.);
#68882=ADVANCED_FACE('',(#8132),#5033,.T.);
#68883=ADVANCED_FACE('',(#8133),#2360,.T.);
#68884=ADVANCED_FACE('',(#8134),#2361,.T.);
#68885=ADVANCED_FACE('',(#8135),#5034,.T.);
#68886=ADVANCED_FACE('',(#8136),#2362,.T.);
#68887=ADVANCED_FACE('',(#8137),#2363,.T.);
#68888=ADVANCED_FACE('',(#8138),#5035,.T.);
#68889=ADVANCED_FACE('',(#8139),#2364,.T.);
#68890=ADVANCED_FACE('',(#8140),#2365,.T.);
#68891=ADVANCED_FACE('',(#8141),#5036,.T.);
#68892=ADVANCED_FACE('',(#8142),#2366,.T.);
#68893=ADVANCED_FACE('',(#8143),#2367,.T.);
#68894=ADVANCED_FACE('',(#8144),#5037,.T.);
#68895=ADVANCED_FACE('',(#8145),#2368,.T.);
#68896=ADVANCED_FACE('',(#8146),#2369,.T.);
#68897=ADVANCED_FACE('',(#8147),#5038,.T.);
#68898=ADVANCED_FACE('',(#8148),#2370,.T.);
#68899=ADVANCED_FACE('',(#8149),#2371,.T.);
#68900=ADVANCED_FACE('',(#8150),#5039,.T.);
#68901=ADVANCED_FACE('',(#8151),#2372,.T.);
#68902=ADVANCED_FACE('',(#8152),#2373,.T.);
#68903=ADVANCED_FACE('',(#8153),#5040,.T.);
#68904=ADVANCED_FACE('',(#8154),#2374,.T.);
#68905=ADVANCED_FACE('',(#8155),#2375,.T.);
#68906=ADVANCED_FACE('',(#8156),#5041,.T.);
#68907=ADVANCED_FACE('',(#8157),#2376,.T.);
#68908=ADVANCED_FACE('',(#8158),#2377,.T.);
#68909=ADVANCED_FACE('',(#8159),#5042,.T.);
#68910=ADVANCED_FACE('',(#8160),#2378,.T.);
#68911=ADVANCED_FACE('',(#8161),#2379,.T.);
#68912=ADVANCED_FACE('',(#8162),#5043,.T.);
#68913=ADVANCED_FACE('',(#8163),#2380,.T.);
#68914=ADVANCED_FACE('',(#8164),#2381,.T.);
#68915=ADVANCED_FACE('',(#8165),#5044,.T.);
#68916=ADVANCED_FACE('',(#8166),#2382,.T.);
#68917=ADVANCED_FACE('',(#8167),#2383,.T.);
#68918=ADVANCED_FACE('',(#8168),#5045,.T.);
#68919=ADVANCED_FACE('',(#8169),#2384,.T.);
#68920=ADVANCED_FACE('',(#8170),#2385,.T.);
#68921=ADVANCED_FACE('',(#8171),#5046,.T.);
#68922=ADVANCED_FACE('',(#8172),#2386,.T.);
#68923=ADVANCED_FACE('',(#8173),#2387,.T.);
#68924=ADVANCED_FACE('',(#8174),#5047,.T.);
#68925=ADVANCED_FACE('',(#8175),#2388,.T.);
#68926=ADVANCED_FACE('',(#8176),#2389,.T.);
#68927=ADVANCED_FACE('',(#8177),#5048,.T.);
#68928=ADVANCED_FACE('',(#8178),#2390,.T.);
#68929=ADVANCED_FACE('',(#8179),#2391,.T.);
#68930=ADVANCED_FACE('',(#8180),#5049,.T.);
#68931=ADVANCED_FACE('',(#8181),#2392,.T.);
#68932=ADVANCED_FACE('',(#8182),#2393,.T.);
#68933=ADVANCED_FACE('',(#8183),#5050,.T.);
#68934=ADVANCED_FACE('',(#8184),#2394,.T.);
#68935=ADVANCED_FACE('',(#8185),#2395,.T.);
#68936=ADVANCED_FACE('',(#8186),#5051,.T.);
#68937=ADVANCED_FACE('',(#8187),#2396,.T.);
#68938=ADVANCED_FACE('',(#8188),#2397,.T.);
#68939=ADVANCED_FACE('',(#8189),#5052,.T.);
#68940=ADVANCED_FACE('',(#8190),#2398,.T.);
#68941=ADVANCED_FACE('',(#8191),#2399,.T.);
#68942=ADVANCED_FACE('',(#8192),#2400,.T.);
#68943=ADVANCED_FACE('',(#8193),#2401,.T.);
#68944=ADVANCED_FACE('',(#8194),#2402,.T.);
#68945=ADVANCED_FACE('',(#8195),#2403,.T.);
#68946=ADVANCED_FACE('',(#8196),#2404,.T.);
#68947=ADVANCED_FACE('',(#8197),#2405,.T.);
#68948=ADVANCED_FACE('',(#8198),#2406,.T.);
#68949=ADVANCED_FACE('',(#8199),#2407,.T.);
#68950=ADVANCED_FACE('',(#8200),#2408,.T.);
#68951=ADVANCED_FACE('',(#8201),#2409,.T.);
#68952=ADVANCED_FACE('',(#8202),#2410,.T.);
#68953=ADVANCED_FACE('',(#8203),#2411,.T.);
#68954=ADVANCED_FACE('',(#8204),#2412,.T.);
#68955=ADVANCED_FACE('',(#8205),#2413,.T.);
#68956=ADVANCED_FACE('',(#8206),#2414,.T.);
#68957=ADVANCED_FACE('',(#8207),#2415,.T.);
#68958=ADVANCED_FACE('',(#8208),#2416,.T.);
#68959=ADVANCED_FACE('',(#8209),#2417,.T.);
#68960=ADVANCED_FACE('',(#8210),#2418,.T.);
#68961=ADVANCED_FACE('',(#8211),#2419,.T.);
#68962=ADVANCED_FACE('',(#8212),#2420,.T.);
#68963=ADVANCED_FACE('',(#8213),#2421,.T.);
#68964=ADVANCED_FACE('',(#8214),#2422,.T.);
#68965=ADVANCED_FACE('',(#8215),#2423,.T.);
#68966=ADVANCED_FACE('',(#8216),#2424,.T.);
#68967=ADVANCED_FACE('',(#8217),#2425,.T.);
#68968=ADVANCED_FACE('',(#8218),#2426,.T.);
#68969=ADVANCED_FACE('',(#8219),#2427,.T.);
#68970=ADVANCED_FACE('',(#8220),#2428,.T.);
#68971=ADVANCED_FACE('',(#8221),#2429,.T.);
#68972=ADVANCED_FACE('',(#8222),#2430,.T.);
#68973=ADVANCED_FACE('',(#8223),#2431,.T.);
#68974=ADVANCED_FACE('',(#8224),#2432,.T.);
#68975=ADVANCED_FACE('',(#8225),#2433,.T.);
#68976=ADVANCED_FACE('',(#8226),#2434,.T.);
#68977=ADVANCED_FACE('',(#8227),#2435,.T.);
#68978=ADVANCED_FACE('',(#8228),#2436,.T.);
#68979=ADVANCED_FACE('',(#8229),#2437,.T.);
#68980=ADVANCED_FACE('',(#8230),#2438,.T.);
#68981=ADVANCED_FACE('',(#8231),#2439,.T.);
#68982=ADVANCED_FACE('',(#8232),#2440,.T.);
#68983=ADVANCED_FACE('',(#8233),#2441,.T.);
#68984=ADVANCED_FACE('',(#8234),#2442,.T.);
#68985=ADVANCED_FACE('',(#8235),#2443,.T.);
#68986=ADVANCED_FACE('',(#8236),#2444,.T.);
#68987=ADVANCED_FACE('',(#8237),#2445,.T.);
#68988=ADVANCED_FACE('',(#8238),#2446,.T.);
#68989=ADVANCED_FACE('',(#8239),#2447,.T.);
#68990=ADVANCED_FACE('',(#8240),#2448,.T.);
#68991=ADVANCED_FACE('',(#8241),#2449,.T.);
#68992=ADVANCED_FACE('',(#8242),#2450,.T.);
#68993=ADVANCED_FACE('',(#8243),#2451,.T.);
#68994=ADVANCED_FACE('',(#8244),#2452,.T.);
#68995=ADVANCED_FACE('',(#8245),#2453,.T.);
#68996=ADVANCED_FACE('',(#8246),#2454,.T.);
#68997=ADVANCED_FACE('',(#8247),#2455,.T.);
#68998=ADVANCED_FACE('',(#8248),#2456,.T.);
#68999=ADVANCED_FACE('',(#8249),#2457,.T.);
#69000=ADVANCED_FACE('',(#8250),#2458,.T.);
#69001=ADVANCED_FACE('',(#8251),#2459,.T.);
#69002=ADVANCED_FACE('',(#8252),#2460,.T.);
#69003=ADVANCED_FACE('',(#8253),#2461,.T.);
#69004=ADVANCED_FACE('',(#8254),#2462,.T.);
#69005=ADVANCED_FACE('',(#8255),#2463,.T.);
#69006=ADVANCED_FACE('',(#8256),#2464,.T.);
#69007=ADVANCED_FACE('',(#8257),#2465,.T.);
#69008=ADVANCED_FACE('',(#8258),#2466,.T.);
#69009=ADVANCED_FACE('',(#8259),#2467,.T.);
#69010=ADVANCED_FACE('',(#8260),#2468,.T.);
#69011=ADVANCED_FACE('',(#8261),#2469,.T.);
#69012=ADVANCED_FACE('',(#8262),#2470,.T.);
#69013=ADVANCED_FACE('',(#8263),#2471,.T.);
#69014=ADVANCED_FACE('',(#8264),#2472,.T.);
#69015=ADVANCED_FACE('',(#8265),#2473,.T.);
#69016=ADVANCED_FACE('',(#8266),#2474,.T.);
#69017=ADVANCED_FACE('',(#8267),#2475,.T.);
#69018=ADVANCED_FACE('',(#8268),#2476,.T.);
#69019=ADVANCED_FACE('',(#8269),#2477,.T.);
#69020=ADVANCED_FACE('',(#8270),#2478,.T.);
#69021=ADVANCED_FACE('',(#8271),#2479,.T.);
#69022=ADVANCED_FACE('',(#8272),#2480,.T.);
#69023=ADVANCED_FACE('',(#8273),#2481,.T.);
#69024=ADVANCED_FACE('',(#8274),#2482,.T.);
#69025=ADVANCED_FACE('',(#8275),#2483,.T.);
#69026=ADVANCED_FACE('',(#8276),#2484,.T.);
#69027=ADVANCED_FACE('',(#8277),#2485,.T.);
#69028=ADVANCED_FACE('',(#8278),#2486,.T.);
#69029=ADVANCED_FACE('',(#8279),#2487,.T.);
#69030=ADVANCED_FACE('',(#8280),#2488,.T.);
#69031=ADVANCED_FACE('',(#8281),#2489,.T.);
#69032=ADVANCED_FACE('',(#8282),#2490,.T.);
#69033=ADVANCED_FACE('',(#8283),#2491,.T.);
#69034=ADVANCED_FACE('',(#8284),#2492,.T.);
#69035=ADVANCED_FACE('',(#8285),#2493,.T.);
#69036=ADVANCED_FACE('',(#8286),#2494,.T.);
#69037=ADVANCED_FACE('',(#8287),#2495,.T.);
#69038=ADVANCED_FACE('',(#8288),#2496,.T.);
#69039=ADVANCED_FACE('',(#8289),#2497,.T.);
#69040=ADVANCED_FACE('',(#8290),#2498,.T.);
#69041=ADVANCED_FACE('',(#8291),#2499,.T.);
#69042=ADVANCED_FACE('',(#8292),#2500,.T.);
#69043=ADVANCED_FACE('',(#8293),#2501,.T.);
#69044=ADVANCED_FACE('',(#8294),#2502,.T.);
#69045=ADVANCED_FACE('',(#8295),#2503,.T.);
#69046=ADVANCED_FACE('',(#8296),#2504,.T.);
#69047=ADVANCED_FACE('',(#8297),#2505,.T.);
#69048=ADVANCED_FACE('',(#8298),#2506,.T.);
#69049=ADVANCED_FACE('',(#8299),#2507,.T.);
#69050=ADVANCED_FACE('',(#8300),#2508,.T.);
#69051=ADVANCED_FACE('',(#8301),#2509,.T.);
#69052=ADVANCED_FACE('',(#8302),#2510,.T.);
#69053=ADVANCED_FACE('',(#8303),#2511,.T.);
#69054=ADVANCED_FACE('',(#8304),#2512,.T.);
#69055=ADVANCED_FACE('',(#8305),#2513,.T.);
#69056=ADVANCED_FACE('',(#8306),#2514,.T.);
#69057=ADVANCED_FACE('',(#8307),#2515,.T.);
#69058=ADVANCED_FACE('',(#8308),#5053,.T.);
#69059=ADVANCED_FACE('',(#8309),#2516,.T.);
#69060=ADVANCED_FACE('',(#8310),#2517,.T.);
#69061=ADVANCED_FACE('',(#8311),#5054,.T.);
#69062=ADVANCED_FACE('',(#8312),#2518,.T.);
#69063=ADVANCED_FACE('',(#8313),#2519,.T.);
#69064=ADVANCED_FACE('',(#8314),#5055,.T.);
#69065=ADVANCED_FACE('',(#8315),#2520,.T.);
#69066=ADVANCED_FACE('',(#8316),#2521,.T.);
#69067=ADVANCED_FACE('',(#8317),#5056,.T.);
#69068=ADVANCED_FACE('',(#8318),#2522,.T.);
#69069=ADVANCED_FACE('',(#8319),#2523,.T.);
#69070=ADVANCED_FACE('',(#8320),#5057,.T.);
#69071=ADVANCED_FACE('',(#8321),#2524,.T.);
#69072=ADVANCED_FACE('',(#8322),#2525,.T.);
#69073=ADVANCED_FACE('',(#8323),#5058,.T.);
#69074=ADVANCED_FACE('',(#8324),#2526,.T.);
#69075=ADVANCED_FACE('',(#8325),#2527,.T.);
#69076=ADVANCED_FACE('',(#8326),#2528,.T.);
#69077=ADVANCED_FACE('',(#8327),#2529,.T.);
#69078=ADVANCED_FACE('',(#8328),#5059,.T.);
#69079=ADVANCED_FACE('',(#8329),#2530,.T.);
#69080=ADVANCED_FACE('',(#8330),#2531,.T.);
#69081=ADVANCED_FACE('',(#8331),#5060,.T.);
#69082=ADVANCED_FACE('',(#8332),#2532,.T.);
#69083=ADVANCED_FACE('',(#8333),#2533,.T.);
#69084=ADVANCED_FACE('',(#8334),#5061,.T.);
#69085=ADVANCED_FACE('',(#8335),#2534,.T.);
#69086=ADVANCED_FACE('',(#8336),#2535,.T.);
#69087=ADVANCED_FACE('',(#8337),#5062,.T.);
#69088=ADVANCED_FACE('',(#8338),#2536,.T.);
#69089=ADVANCED_FACE('',(#8339),#2537,.T.);
#69090=ADVANCED_FACE('',(#8340),#5063,.T.);
#69091=ADVANCED_FACE('',(#8341),#2538,.T.);
#69092=ADVANCED_FACE('',(#8342),#2539,.T.);
#69093=ADVANCED_FACE('',(#8343),#5064,.T.);
#69094=ADVANCED_FACE('',(#8344),#2540,.T.);
#69095=ADVANCED_FACE('',(#8345),#2541,.T.);
#69096=ADVANCED_FACE('',(#8346),#5065,.T.);
#69097=ADVANCED_FACE('',(#8347),#2542,.T.);
#69098=ADVANCED_FACE('',(#8348),#2543,.T.);
#69099=ADVANCED_FACE('',(#8349),#5066,.T.);
#69100=ADVANCED_FACE('',(#8350),#2544,.T.);
#69101=ADVANCED_FACE('',(#8351),#2545,.T.);
#69102=ADVANCED_FACE('',(#8352),#5067,.T.);
#69103=ADVANCED_FACE('',(#8353),#2546,.T.);
#69104=ADVANCED_FACE('',(#8354),#2547,.T.);
#69105=ADVANCED_FACE('',(#8355),#5068,.T.);
#69106=ADVANCED_FACE('',(#8356),#2548,.T.);
#69107=ADVANCED_FACE('',(#8357),#2549,.T.);
#69108=ADVANCED_FACE('',(#8358),#5069,.T.);
#69109=ADVANCED_FACE('',(#8359),#2550,.T.);
#69110=ADVANCED_FACE('',(#8360),#2551,.T.);
#69111=ADVANCED_FACE('',(#8361),#5070,.T.);
#69112=ADVANCED_FACE('',(#8362),#2552,.T.);
#69113=ADVANCED_FACE('',(#8363),#2553,.T.);
#69114=ADVANCED_FACE('',(#8364),#2554,.T.);
#69115=ADVANCED_FACE('',(#8365),#5071,.T.);
#69116=ADVANCED_FACE('',(#8366),#2555,.T.);
#69117=ADVANCED_FACE('',(#8367),#5072,.T.);
#69118=ADVANCED_FACE('',(#8368),#2556,.T.);
#69119=ADVANCED_FACE('',(#8369),#2557,.T.);
#69120=ADVANCED_FACE('',(#8370),#5073,.T.);
#69121=ADVANCED_FACE('',(#8371),#2558,.T.);
#69122=ADVANCED_FACE('',(#8372),#2559,.T.);
#69123=ADVANCED_FACE('',(#8373),#5074,.T.);
#69124=ADVANCED_FACE('',(#8374),#2560,.T.);
#69125=ADVANCED_FACE('',(#8375),#2561,.T.);
#69126=ADVANCED_FACE('',(#8376),#5075,.T.);
#69127=ADVANCED_FACE('',(#8377),#2562,.T.);
#69128=ADVANCED_FACE('',(#8378),#2563,.T.);
#69129=ADVANCED_FACE('',(#8379),#5076,.T.);
#69130=ADVANCED_FACE('',(#8380),#2564,.T.);
#69131=ADVANCED_FACE('',(#8381),#2565,.T.);
#69132=ADVANCED_FACE('',(#8382),#5077,.T.);
#69133=ADVANCED_FACE('',(#8383),#2566,.T.);
#69134=ADVANCED_FACE('',(#8384),#2567,.T.);
#69135=ADVANCED_FACE('',(#8385),#5078,.T.);
#69136=ADVANCED_FACE('',(#8386),#2568,.T.);
#69137=ADVANCED_FACE('',(#8387),#2569,.T.);
#69138=ADVANCED_FACE('',(#8388),#5079,.T.);
#69139=ADVANCED_FACE('',(#8389),#2570,.T.);
#69140=ADVANCED_FACE('',(#8390),#5080,.T.);
#69141=ADVANCED_FACE('',(#8391),#2571,.T.);
#69142=ADVANCED_FACE('',(#8392),#2572,.T.);
#69143=ADVANCED_FACE('',(#8393),#2573,.T.);
#69144=ADVANCED_FACE('',(#8394),#2574,.T.);
#69145=ADVANCED_FACE('',(#8395),#5081,.T.);
#69146=ADVANCED_FACE('',(#8396),#2575,.T.);
#69147=ADVANCED_FACE('',(#8397),#2576,.T.);
#69148=ADVANCED_FACE('',(#8398),#5082,.T.);
#69149=ADVANCED_FACE('',(#8399),#2577,.T.);
#69150=ADVANCED_FACE('',(#8400),#2578,.T.);
#69151=ADVANCED_FACE('',(#8401),#5083,.T.);
#69152=ADVANCED_FACE('',(#8402),#2579,.T.);
#69153=ADVANCED_FACE('',(#8403),#2580,.T.);
#69154=ADVANCED_FACE('',(#8404),#5084,.T.);
#69155=ADVANCED_FACE('',(#8405),#2581,.T.);
#69156=ADVANCED_FACE('',(#8406),#2582,.T.);
#69157=ADVANCED_FACE('',(#8407),#5085,.T.);
#69158=ADVANCED_FACE('',(#8408),#2583,.T.);
#69159=ADVANCED_FACE('',(#8409),#2584,.T.);
#69160=ADVANCED_FACE('',(#8410),#5086,.T.);
#69161=ADVANCED_FACE('',(#8411),#2585,.T.);
#69162=ADVANCED_FACE('',(#8412),#2586,.T.);
#69163=ADVANCED_FACE('',(#8413),#5087,.T.);
#69164=ADVANCED_FACE('',(#8414),#2587,.T.);
#69165=ADVANCED_FACE('',(#8415),#2588,.T.);
#69166=ADVANCED_FACE('',(#8416),#5088,.T.);
#69167=ADVANCED_FACE('',(#8417),#2589,.T.);
#69168=ADVANCED_FACE('',(#8418),#2590,.T.);
#69169=ADVANCED_FACE('',(#8419),#5089,.T.);
#69170=ADVANCED_FACE('',(#8420),#2591,.T.);
#69171=ADVANCED_FACE('',(#8421),#2592,.T.);
#69172=ADVANCED_FACE('',(#8422),#5090,.T.);
#69173=ADVANCED_FACE('',(#8423),#2593,.T.);
#69174=ADVANCED_FACE('',(#8424),#2594,.T.);
#69175=ADVANCED_FACE('',(#8425),#5091,.T.);
#69176=ADVANCED_FACE('',(#8426),#2595,.T.);
#69177=ADVANCED_FACE('',(#8427),#2596,.T.);
#69178=ADVANCED_FACE('',(#8428),#5092,.T.);
#69179=ADVANCED_FACE('',(#8429),#2597,.T.);
#69180=ADVANCED_FACE('',(#8430),#2598,.T.);
#69181=ADVANCED_FACE('',(#8431),#5093,.T.);
#69182=ADVANCED_FACE('',(#8432),#2599,.T.);
#69183=ADVANCED_FACE('',(#8433),#2600,.T.);
#69184=ADVANCED_FACE('',(#8434),#2601,.T.);
#69185=ADVANCED_FACE('',(#8435),#2602,.T.);
#69186=ADVANCED_FACE('',(#8436),#5094,.T.);
#69187=ADVANCED_FACE('',(#8437),#2603,.T.);
#69188=ADVANCED_FACE('',(#8438),#2604,.T.);
#69189=ADVANCED_FACE('',(#8439),#5095,.T.);
#69190=ADVANCED_FACE('',(#8440),#2605,.T.);
#69191=ADVANCED_FACE('',(#8441),#2606,.T.);
#69192=ADVANCED_FACE('',(#8442),#5096,.T.);
#69193=ADVANCED_FACE('',(#8443),#2607,.T.);
#69194=ADVANCED_FACE('',(#8444),#2608,.T.);
#69195=ADVANCED_FACE('',(#8445),#5097,.T.);
#69196=ADVANCED_FACE('',(#8446),#2609,.T.);
#69197=ADVANCED_FACE('',(#8447),#2610,.T.);
#69198=ADVANCED_FACE('',(#8448),#5098,.T.);
#69199=ADVANCED_FACE('',(#8449),#2611,.T.);
#69200=ADVANCED_FACE('',(#8450),#2612,.T.);
#69201=ADVANCED_FACE('',(#8451),#5099,.T.);
#69202=ADVANCED_FACE('',(#8452),#2613,.T.);
#69203=ADVANCED_FACE('',(#8453),#2614,.T.);
#69204=ADVANCED_FACE('',(#8454),#5100,.T.);
#69205=ADVANCED_FACE('',(#8455),#2615,.T.);
#69206=ADVANCED_FACE('',(#8456),#2616,.T.);
#69207=ADVANCED_FACE('',(#8457),#5101,.T.);
#69208=ADVANCED_FACE('',(#8458),#2617,.T.);
#69209=ADVANCED_FACE('',(#8459),#2618,.T.);
#69210=ADVANCED_FACE('',(#8460),#5102,.T.);
#69211=ADVANCED_FACE('',(#8461),#2619,.T.);
#69212=ADVANCED_FACE('',(#8462),#2620,.T.);
#69213=ADVANCED_FACE('',(#8463),#5103,.T.);
#69214=ADVANCED_FACE('',(#8464),#2621,.T.);
#69215=ADVANCED_FACE('',(#8465),#2622,.T.);
#69216=ADVANCED_FACE('',(#8466),#5104,.T.);
#69217=ADVANCED_FACE('',(#8467),#2623,.T.);
#69218=ADVANCED_FACE('',(#8468),#2624,.T.);
#69219=ADVANCED_FACE('',(#8469),#5105,.T.);
#69220=ADVANCED_FACE('',(#8470),#2625,.T.);
#69221=ADVANCED_FACE('',(#8471),#2626,.T.);
#69222=ADVANCED_FACE('',(#8472),#5106,.T.);
#69223=ADVANCED_FACE('',(#8473),#2627,.T.);
#69224=ADVANCED_FACE('',(#8474),#2628,.T.);
#69225=ADVANCED_FACE('',(#8475),#5107,.T.);
#69226=ADVANCED_FACE('',(#8476),#5108,.T.);
#69227=ADVANCED_FACE('',(#8477),#2629,.T.);
#69228=ADVANCED_FACE('',(#8478),#2630,.T.);
#69229=ADVANCED_FACE('',(#8479),#2631,.T.);
#69230=ADVANCED_FACE('',(#8480),#2632,.T.);
#69231=ADVANCED_FACE('',(#8481),#2633,.T.);
#69232=ADVANCED_FACE('',(#8482),#2634,.T.);
#69233=ADVANCED_FACE('',(#8483),#2635,.T.);
#69234=ADVANCED_FACE('',(#8484),#2636,.T.);
#69235=ADVANCED_FACE('',(#8485),#2637,.T.);
#69236=ADVANCED_FACE('',(#8486),#2638,.T.);
#69237=ADVANCED_FACE('',(#8487),#2639,.T.);
#69238=ADVANCED_FACE('',(#8488),#2640,.T.);
#69239=ADVANCED_FACE('',(#8489),#2641,.T.);
#69240=ADVANCED_FACE('',(#8490),#2642,.T.);
#69241=ADVANCED_FACE('',(#8491),#2643,.T.);
#69242=ADVANCED_FACE('',(#8492),#2644,.T.);
#69243=ADVANCED_FACE('',(#8493),#2645,.T.);
#69244=ADVANCED_FACE('',(#8494),#2646,.T.);
#69245=ADVANCED_FACE('',(#8495),#2647,.T.);
#69246=ADVANCED_FACE('',(#8496),#2648,.T.);
#69247=ADVANCED_FACE('',(#8497),#2649,.T.);
#69248=ADVANCED_FACE('',(#8498),#2650,.T.);
#69249=ADVANCED_FACE('',(#8499),#2651,.T.);
#69250=ADVANCED_FACE('',(#8500),#2652,.T.);
#69251=ADVANCED_FACE('',(#8501),#2653,.T.);
#69252=ADVANCED_FACE('',(#8502),#2654,.T.);
#69253=ADVANCED_FACE('',(#8503),#2655,.T.);
#69254=ADVANCED_FACE('',(#8504),#2656,.T.);
#69255=ADVANCED_FACE('',(#8505),#2657,.T.);
#69256=ADVANCED_FACE('',(#8506),#2658,.T.);
#69257=ADVANCED_FACE('',(#8507),#2659,.T.);
#69258=ADVANCED_FACE('',(#8508),#2660,.T.);
#69259=ADVANCED_FACE('',(#8509),#2661,.T.);
#69260=ADVANCED_FACE('',(#8510),#2662,.T.);
#69261=ADVANCED_FACE('',(#8511),#2663,.T.);
#69262=ADVANCED_FACE('',(#8512),#2664,.T.);
#69263=ADVANCED_FACE('',(#8513),#2665,.T.);
#69264=ADVANCED_FACE('',(#8514),#2666,.T.);
#69265=ADVANCED_FACE('',(#8515),#2667,.T.);
#69266=ADVANCED_FACE('',(#8516),#2668,.T.);
#69267=ADVANCED_FACE('',(#8517),#2669,.T.);
#69268=ADVANCED_FACE('',(#8518),#2670,.T.);
#69269=ADVANCED_FACE('',(#8519),#2671,.T.);
#69270=ADVANCED_FACE('',(#8520),#2672,.T.);
#69271=ADVANCED_FACE('',(#8521),#2673,.T.);
#69272=ADVANCED_FACE('',(#8522),#2674,.T.);
#69273=ADVANCED_FACE('',(#8523),#2675,.T.);
#69274=ADVANCED_FACE('',(#8524),#2676,.T.);
#69275=ADVANCED_FACE('',(#8525),#2677,.T.);
#69276=ADVANCED_FACE('',(#8526),#2678,.T.);
#69277=ADVANCED_FACE('',(#8527),#2679,.T.);
#69278=ADVANCED_FACE('',(#8528),#2680,.T.);
#69279=ADVANCED_FACE('',(#8529),#2681,.T.);
#69280=ADVANCED_FACE('',(#8530),#2682,.T.);
#69281=ADVANCED_FACE('',(#8531),#2683,.T.);
#69282=ADVANCED_FACE('',(#8532),#2684,.T.);
#69283=ADVANCED_FACE('',(#8533),#2685,.T.);
#69284=ADVANCED_FACE('',(#8534),#2686,.T.);
#69285=ADVANCED_FACE('',(#8535),#2687,.T.);
#69286=ADVANCED_FACE('',(#8536),#2688,.T.);
#69287=ADVANCED_FACE('',(#8537),#2689,.T.);
#69288=ADVANCED_FACE('',(#8538),#2690,.T.);
#69289=ADVANCED_FACE('',(#8539),#2691,.T.);
#69290=ADVANCED_FACE('',(#8540),#2692,.T.);
#69291=ADVANCED_FACE('',(#8541),#2693,.T.);
#69292=ADVANCED_FACE('',(#8542),#2694,.T.);
#69293=ADVANCED_FACE('',(#8543),#2695,.T.);
#69294=ADVANCED_FACE('',(#8544),#2696,.T.);
#69295=ADVANCED_FACE('',(#8545),#2697,.T.);
#69296=ADVANCED_FACE('',(#8546),#2698,.T.);
#69297=ADVANCED_FACE('',(#8547),#2699,.T.);
#69298=ADVANCED_FACE('',(#8548),#2700,.T.);
#69299=ADVANCED_FACE('',(#8549),#2701,.T.);
#69300=ADVANCED_FACE('',(#8550),#2702,.T.);
#69301=ADVANCED_FACE('',(#8551),#2703,.T.);
#69302=ADVANCED_FACE('',(#8552),#2704,.T.);
#69303=ADVANCED_FACE('',(#8553),#2705,.T.);
#69304=ADVANCED_FACE('',(#8554),#2706,.T.);
#69305=ADVANCED_FACE('',(#8555),#2707,.T.);
#69306=ADVANCED_FACE('',(#8556),#2708,.T.);
#69307=ADVANCED_FACE('',(#8557),#2709,.T.);
#69308=ADVANCED_FACE('',(#8558),#2710,.T.);
#69309=ADVANCED_FACE('',(#8559),#2711,.T.);
#69310=ADVANCED_FACE('',(#8560),#2712,.T.);
#69311=ADVANCED_FACE('',(#8561),#2713,.T.);
#69312=ADVANCED_FACE('',(#8562),#2714,.T.);
#69313=ADVANCED_FACE('',(#8563),#2715,.T.);
#69314=ADVANCED_FACE('',(#8564),#2716,.T.);
#69315=ADVANCED_FACE('',(#8565),#2717,.T.);
#69316=ADVANCED_FACE('',(#8566),#2718,.T.);
#69317=ADVANCED_FACE('',(#8567),#2719,.T.);
#69318=ADVANCED_FACE('',(#8568),#2720,.T.);
#69319=ADVANCED_FACE('',(#8569),#2721,.T.);
#69320=ADVANCED_FACE('',(#8570),#2722,.T.);
#69321=ADVANCED_FACE('',(#8571),#2723,.T.);
#69322=ADVANCED_FACE('',(#8572),#2724,.T.);
#69323=ADVANCED_FACE('',(#8573),#2725,.T.);
#69324=ADVANCED_FACE('',(#8574),#2726,.T.);
#69325=ADVANCED_FACE('',(#8575),#2727,.T.);
#69326=ADVANCED_FACE('',(#8576),#2728,.T.);
#69327=ADVANCED_FACE('',(#8577),#2729,.T.);
#69328=ADVANCED_FACE('',(#8578),#2730,.T.);
#69329=ADVANCED_FACE('',(#8579),#2731,.T.);
#69330=ADVANCED_FACE('',(#8580),#2732,.T.);
#69331=ADVANCED_FACE('',(#8581),#2733,.T.);
#69332=ADVANCED_FACE('',(#8582),#2734,.T.);
#69333=ADVANCED_FACE('',(#8583),#2735,.T.);
#69334=ADVANCED_FACE('',(#8584),#2736,.T.);
#69335=ADVANCED_FACE('',(#8585),#2737,.T.);
#69336=ADVANCED_FACE('',(#8586),#2738,.T.);
#69337=ADVANCED_FACE('',(#8587),#2739,.T.);
#69338=ADVANCED_FACE('',(#8588),#2740,.T.);
#69339=ADVANCED_FACE('',(#8589),#2741,.T.);
#69340=ADVANCED_FACE('',(#8590),#2742,.T.);
#69341=ADVANCED_FACE('',(#8591),#2743,.T.);
#69342=ADVANCED_FACE('',(#8592),#2744,.T.);
#69343=ADVANCED_FACE('',(#8593),#2745,.T.);
#69344=ADVANCED_FACE('',(#8594),#2746,.T.);
#69345=ADVANCED_FACE('',(#8595),#5109,.T.);
#69346=ADVANCED_FACE('',(#8596),#2747,.T.);
#69347=ADVANCED_FACE('',(#8597),#2748,.T.);
#69348=ADVANCED_FACE('',(#8598),#5110,.T.);
#69349=ADVANCED_FACE('',(#8599),#2749,.T.);
#69350=ADVANCED_FACE('',(#8600),#2750,.T.);
#69351=ADVANCED_FACE('',(#8601),#5111,.T.);
#69352=ADVANCED_FACE('',(#8602),#2751,.T.);
#69353=ADVANCED_FACE('',(#8603),#2752,.T.);
#69354=ADVANCED_FACE('',(#8604),#5112,.T.);
#69355=ADVANCED_FACE('',(#8605),#2753,.T.);
#69356=ADVANCED_FACE('',(#8606),#2754,.T.);
#69357=ADVANCED_FACE('',(#8607),#5113,.T.);
#69358=ADVANCED_FACE('',(#8608),#2755,.T.);
#69359=ADVANCED_FACE('',(#8609),#2756,.T.);
#69360=ADVANCED_FACE('',(#8610),#5114,.T.);
#69361=ADVANCED_FACE('',(#8611),#2757,.T.);
#69362=ADVANCED_FACE('',(#8612),#2758,.T.);
#69363=ADVANCED_FACE('',(#8613),#5115,.T.);
#69364=ADVANCED_FACE('',(#8614),#2759,.T.);
#69365=ADVANCED_FACE('',(#8615),#2760,.T.);
#69366=ADVANCED_FACE('',(#8616),#5116,.T.);
#69367=ADVANCED_FACE('',(#8617),#2761,.T.);
#69368=ADVANCED_FACE('',(#8618),#2762,.T.);
#69369=ADVANCED_FACE('',(#8619),#5117,.T.);
#69370=ADVANCED_FACE('',(#8620),#2763,.T.);
#69371=ADVANCED_FACE('',(#8621),#2764,.T.);
#69372=ADVANCED_FACE('',(#8622),#5118,.T.);
#69373=ADVANCED_FACE('',(#8623),#2765,.T.);
#69374=ADVANCED_FACE('',(#8624),#2766,.T.);
#69375=ADVANCED_FACE('',(#8625),#5119,.T.);
#69376=ADVANCED_FACE('',(#8626),#2767,.T.);
#69377=ADVANCED_FACE('',(#8627),#2768,.T.);
#69378=ADVANCED_FACE('',(#8628),#5120,.T.);
#69379=ADVANCED_FACE('',(#8629),#2769,.T.);
#69380=ADVANCED_FACE('',(#8630),#2770,.T.);
#69381=ADVANCED_FACE('',(#8631),#5121,.T.);
#69382=ADVANCED_FACE('',(#8632),#2771,.T.);
#69383=ADVANCED_FACE('',(#8633),#2772,.T.);
#69384=ADVANCED_FACE('',(#8634),#5122,.T.);
#69385=ADVANCED_FACE('',(#8635),#2773,.T.);
#69386=ADVANCED_FACE('',(#8636),#2774,.T.);
#69387=ADVANCED_FACE('',(#8637),#2775,.T.);
#69388=ADVANCED_FACE('',(#8638),#2776,.T.);
#69389=ADVANCED_FACE('',(#8639),#5123,.T.);
#69390=ADVANCED_FACE('',(#8640),#2777,.T.);
#69391=ADVANCED_FACE('',(#8641),#2778,.T.);
#69392=ADVANCED_FACE('',(#8642),#5124,.T.);
#69393=ADVANCED_FACE('',(#8643),#2779,.T.);
#69394=ADVANCED_FACE('',(#8644),#2780,.T.);
#69395=ADVANCED_FACE('',(#8645),#5125,.T.);
#69396=ADVANCED_FACE('',(#8646),#2781,.T.);
#69397=ADVANCED_FACE('',(#8647),#2782,.T.);
#69398=ADVANCED_FACE('',(#8648),#5126,.T.);
#69399=ADVANCED_FACE('',(#8649),#2783,.T.);
#69400=ADVANCED_FACE('',(#8650),#2784,.T.);
#69401=ADVANCED_FACE('',(#8651),#2785,.T.);
#69402=ADVANCED_FACE('',(#8652),#5127,.T.);
#69403=ADVANCED_FACE('',(#8653),#2786,.T.);
#69404=ADVANCED_FACE('',(#8654),#5128,.T.);
#69405=ADVANCED_FACE('',(#8655),#2787,.T.);
#69406=ADVANCED_FACE('',(#8656),#2788,.T.);
#69407=ADVANCED_FACE('',(#8657),#5129,.T.);
#69408=ADVANCED_FACE('',(#8658),#2789,.T.);
#69409=ADVANCED_FACE('',(#8659),#2790,.T.);
#69410=ADVANCED_FACE('',(#8660),#5130,.T.);
#69411=ADVANCED_FACE('',(#8661),#2791,.T.);
#69412=ADVANCED_FACE('',(#8662),#2792,.T.);
#69413=ADVANCED_FACE('',(#8663),#5131,.T.);
#69414=ADVANCED_FACE('',(#8664),#2793,.T.);
#69415=ADVANCED_FACE('',(#8665),#2794,.T.);
#69416=ADVANCED_FACE('',(#8666),#5132,.T.);
#69417=ADVANCED_FACE('',(#8667),#2795,.T.);
#69418=ADVANCED_FACE('',(#8668),#2796,.T.);
#69419=ADVANCED_FACE('',(#8669),#5133,.T.);
#69420=ADVANCED_FACE('',(#8670),#2797,.T.);
#69421=ADVANCED_FACE('',(#8671),#2798,.T.);
#69422=ADVANCED_FACE('',(#8672),#5134,.T.);
#69423=ADVANCED_FACE('',(#8673),#2799,.T.);
#69424=ADVANCED_FACE('',(#8674),#2800,.T.);
#69425=ADVANCED_FACE('',(#8675),#5135,.T.);
#69426=ADVANCED_FACE('',(#8676),#2801,.T.);
#69427=ADVANCED_FACE('',(#8677),#2802,.T.);
#69428=ADVANCED_FACE('',(#8678),#5136,.T.);
#69429=ADVANCED_FACE('',(#8679),#2803,.T.);
#69430=ADVANCED_FACE('',(#8680),#2804,.T.);
#69431=ADVANCED_FACE('',(#8681),#2805,.T.);
#69432=ADVANCED_FACE('',(#8682),#5137,.T.);
#69433=ADVANCED_FACE('',(#8683),#2806,.T.);
#69434=ADVANCED_FACE('',(#8684),#2807,.T.);
#69435=ADVANCED_FACE('',(#8685),#5138,.T.);
#69436=ADVANCED_FACE('',(#8686),#2808,.T.);
#69437=ADVANCED_FACE('',(#8687),#2809,.T.);
#69438=ADVANCED_FACE('',(#8688),#5139,.T.);
#69439=ADVANCED_FACE('',(#8689),#2810,.T.);
#69440=ADVANCED_FACE('',(#8690),#2811,.T.);
#69441=ADVANCED_FACE('',(#8691),#5140,.T.);
#69442=ADVANCED_FACE('',(#8692),#2812,.T.);
#69443=ADVANCED_FACE('',(#8693),#2813,.T.);
#69444=ADVANCED_FACE('',(#8694),#5141,.T.);
#69445=ADVANCED_FACE('',(#8695),#2814,.T.);
#69446=ADVANCED_FACE('',(#8696),#2815,.T.);
#69447=ADVANCED_FACE('',(#8697),#5142,.T.);
#69448=ADVANCED_FACE('',(#8698),#2816,.T.);
#69449=ADVANCED_FACE('',(#8699),#2817,.T.);
#69450=ADVANCED_FACE('',(#8700),#5143,.T.);
#69451=ADVANCED_FACE('',(#8701),#2818,.T.);
#69452=ADVANCED_FACE('',(#8702),#2819,.T.);
#69453=ADVANCED_FACE('',(#8703),#5144,.T.);
#69454=ADVANCED_FACE('',(#8704),#2820,.T.);
#69455=ADVANCED_FACE('',(#8705),#2821,.T.);
#69456=ADVANCED_FACE('',(#8706),#5145,.T.);
#69457=ADVANCED_FACE('',(#8707),#2822,.T.);
#69458=ADVANCED_FACE('',(#8708),#2823,.T.);
#69459=ADVANCED_FACE('',(#8709),#5146,.T.);
#69460=ADVANCED_FACE('',(#8710),#2824,.T.);
#69461=ADVANCED_FACE('',(#8711),#2825,.T.);
#69462=ADVANCED_FACE('',(#8712),#5147,.T.);
#69463=ADVANCED_FACE('',(#8713),#2826,.T.);
#69464=ADVANCED_FACE('',(#8714),#2827,.T.);
#69465=ADVANCED_FACE('',(#8715),#5148,.T.);
#69466=ADVANCED_FACE('',(#8716),#2828,.T.);
#69467=ADVANCED_FACE('',(#8717),#2829,.T.);
#69468=ADVANCED_FACE('',(#8718),#5149,.T.);
#69469=ADVANCED_FACE('',(#8719),#2830,.T.);
#69470=ADVANCED_FACE('',(#8720),#2831,.T.);
#69471=ADVANCED_FACE('',(#8721),#5150,.T.);
#69472=ADVANCED_FACE('',(#8722),#2832,.T.);
#69473=ADVANCED_FACE('',(#8723),#2833,.T.);
#69474=ADVANCED_FACE('',(#8724),#5151,.T.);
#69475=ADVANCED_FACE('',(#8725),#2834,.T.);
#69476=ADVANCED_FACE('',(#8726),#2835,.T.);
#69477=ADVANCED_FACE('',(#8727),#5152,.T.);
#69478=ADVANCED_FACE('',(#8728),#2836,.T.);
#69479=ADVANCED_FACE('',(#8729),#2837,.T.);
#69480=ADVANCED_FACE('',(#8730),#5153,.T.);
#69481=ADVANCED_FACE('',(#8731),#2838,.T.);
#69482=ADVANCED_FACE('',(#8732),#2839,.T.);
#69483=ADVANCED_FACE('',(#8733),#5154,.T.);
#69484=ADVANCED_FACE('',(#8734),#2840,.T.);
#69485=ADVANCED_FACE('',(#8735),#2841,.T.);
#69486=ADVANCED_FACE('',(#8736),#5155,.T.);
#69487=ADVANCED_FACE('',(#8737),#2842,.T.);
#69488=ADVANCED_FACE('',(#8738),#2843,.T.);
#69489=ADVANCED_FACE('',(#8739),#5156,.T.);
#69490=ADVANCED_FACE('',(#8740),#2844,.T.);
#69491=ADVANCED_FACE('',(#8741),#2845,.T.);
#69492=ADVANCED_FACE('',(#8742),#5157,.T.);
#69493=ADVANCED_FACE('',(#8743),#2846,.T.);
#69494=ADVANCED_FACE('',(#8744),#2847,.T.);
#69495=ADVANCED_FACE('',(#8745),#2848,.T.);
#69496=ADVANCED_FACE('',(#8746),#2849,.T.);
#69497=ADVANCED_FACE('',(#8747),#5158,.T.);
#69498=ADVANCED_FACE('',(#8748),#2850,.T.);
#69499=ADVANCED_FACE('',(#8749),#2851,.T.);
#69500=ADVANCED_FACE('',(#8750),#5159,.T.);
#69501=ADVANCED_FACE('',(#8751),#2852,.T.);
#69502=ADVANCED_FACE('',(#8752),#2853,.T.);
#69503=ADVANCED_FACE('',(#8753),#5160,.T.);
#69504=ADVANCED_FACE('',(#8754),#2854,.T.);
#69505=ADVANCED_FACE('',(#8755),#2855,.T.);
#69506=ADVANCED_FACE('',(#8756),#5161,.T.);
#69507=ADVANCED_FACE('',(#8757),#2856,.T.);
#69508=ADVANCED_FACE('',(#8758),#2857,.T.);
#69509=ADVANCED_FACE('',(#8759),#5162,.T.);
#69510=ADVANCED_FACE('',(#8760),#2858,.T.);
#69511=ADVANCED_FACE('',(#8761),#2859,.T.);
#69512=ADVANCED_FACE('',(#8762),#5163,.T.);
#69513=ADVANCED_FACE('',(#8763),#2860,.T.);
#69514=ADVANCED_FACE('',(#8764),#2861,.T.);
#69515=ADVANCED_FACE('',(#8765),#5164,.T.);
#69516=ADVANCED_FACE('',(#8766),#2862,.T.);
#69517=ADVANCED_FACE('',(#8767),#2863,.T.);
#69518=ADVANCED_FACE('',(#8768),#2864,.T.);
#69519=ADVANCED_FACE('',(#8769),#2865,.T.);
#69520=ADVANCED_FACE('',(#8770),#2866,.T.);
#69521=ADVANCED_FACE('',(#8771),#2867,.T.);
#69522=ADVANCED_FACE('',(#8772),#2868,.T.);
#69523=ADVANCED_FACE('',(#8773),#2869,.T.);
#69524=ADVANCED_FACE('',(#8774),#2870,.T.);
#69525=ADVANCED_FACE('',(#8775),#2871,.T.);
#69526=ADVANCED_FACE('',(#8776),#2872,.T.);
#69527=ADVANCED_FACE('',(#8777),#2873,.T.);
#69528=ADVANCED_FACE('',(#8778),#2874,.T.);
#69529=ADVANCED_FACE('',(#8779),#2875,.T.);
#69530=ADVANCED_FACE('',(#8780),#2876,.T.);
#69531=ADVANCED_FACE('',(#8781),#2877,.T.);
#69532=ADVANCED_FACE('',(#8782),#2878,.T.);
#69533=ADVANCED_FACE('',(#8783),#2879,.T.);
#69534=ADVANCED_FACE('',(#8784),#2880,.T.);
#69535=ADVANCED_FACE('',(#8785),#2881,.T.);
#69536=ADVANCED_FACE('',(#8786),#2882,.T.);
#69537=ADVANCED_FACE('',(#8787),#2883,.T.);
#69538=ADVANCED_FACE('',(#8788),#2884,.T.);
#69539=ADVANCED_FACE('',(#8789),#2885,.T.);
#69540=ADVANCED_FACE('',(#8790),#2886,.T.);
#69541=ADVANCED_FACE('',(#8791),#2887,.T.);
#69542=ADVANCED_FACE('',(#8792),#2888,.T.);
#69543=ADVANCED_FACE('',(#8793),#2889,.T.);
#69544=ADVANCED_FACE('',(#8794),#2890,.T.);
#69545=ADVANCED_FACE('',(#8795),#2891,.T.);
#69546=ADVANCED_FACE('',(#8796),#2892,.T.);
#69547=ADVANCED_FACE('',(#8797),#2893,.T.);
#69548=ADVANCED_FACE('',(#8798),#2894,.T.);
#69549=ADVANCED_FACE('',(#8799),#2895,.T.);
#69550=ADVANCED_FACE('',(#8800),#2896,.T.);
#69551=ADVANCED_FACE('',(#8801),#2897,.T.);
#69552=ADVANCED_FACE('',(#8802),#2898,.T.);
#69553=ADVANCED_FACE('',(#8803),#2899,.T.);
#69554=ADVANCED_FACE('',(#8804),#2900,.T.);
#69555=ADVANCED_FACE('',(#8805),#2901,.T.);
#69556=ADVANCED_FACE('',(#8806),#2902,.T.);
#69557=ADVANCED_FACE('',(#8807),#2903,.T.);
#69558=ADVANCED_FACE('',(#8808),#2904,.T.);
#69559=ADVANCED_FACE('',(#8809),#2905,.T.);
#69560=ADVANCED_FACE('',(#8810),#2906,.T.);
#69561=ADVANCED_FACE('',(#8811),#2907,.T.);
#69562=ADVANCED_FACE('',(#8812),#2908,.T.);
#69563=ADVANCED_FACE('',(#8813),#2909,.T.);
#69564=ADVANCED_FACE('',(#8814),#2910,.T.);
#69565=ADVANCED_FACE('',(#8815),#2911,.T.);
#69566=ADVANCED_FACE('',(#8816),#2912,.T.);
#69567=ADVANCED_FACE('',(#8817),#2913,.T.);
#69568=ADVANCED_FACE('',(#8818),#2914,.T.);
#69569=ADVANCED_FACE('',(#8819),#2915,.T.);
#69570=ADVANCED_FACE('',(#8820),#2916,.T.);
#69571=ADVANCED_FACE('',(#8821),#2917,.T.);
#69572=ADVANCED_FACE('',(#8822),#2918,.T.);
#69573=ADVANCED_FACE('',(#8823),#2919,.T.);
#69574=ADVANCED_FACE('',(#8824),#2920,.T.);
#69575=ADVANCED_FACE('',(#8825),#2921,.T.);
#69576=ADVANCED_FACE('',(#8826),#2922,.T.);
#69577=ADVANCED_FACE('',(#8827),#2923,.T.);
#69578=ADVANCED_FACE('',(#8828),#2924,.T.);
#69579=ADVANCED_FACE('',(#8829),#2925,.T.);
#69580=ADVANCED_FACE('',(#8830),#2926,.T.);
#69581=ADVANCED_FACE('',(#8831),#2927,.T.);
#69582=ADVANCED_FACE('',(#8832),#2928,.T.);
#69583=ADVANCED_FACE('',(#8833),#2929,.T.);
#69584=ADVANCED_FACE('',(#8834),#2930,.T.);
#69585=ADVANCED_FACE('',(#8835),#2931,.T.);
#69586=ADVANCED_FACE('',(#8836),#2932,.T.);
#69587=ADVANCED_FACE('',(#8837),#2933,.T.);
#69588=ADVANCED_FACE('',(#8838),#2934,.T.);
#69589=ADVANCED_FACE('',(#8839),#2935,.T.);
#69590=ADVANCED_FACE('',(#8840),#2936,.T.);
#69591=ADVANCED_FACE('',(#8841),#2937,.T.);
#69592=ADVANCED_FACE('',(#8842),#2938,.T.);
#69593=ADVANCED_FACE('',(#8843),#2939,.T.);
#69594=ADVANCED_FACE('',(#8844),#2940,.T.);
#69595=ADVANCED_FACE('',(#8845),#2941,.T.);
#69596=ADVANCED_FACE('',(#8846),#2942,.T.);
#69597=ADVANCED_FACE('',(#8847),#2943,.T.);
#69598=ADVANCED_FACE('',(#8848),#2944,.T.);
#69599=ADVANCED_FACE('',(#8849),#2945,.T.);
#69600=ADVANCED_FACE('',(#8850),#2946,.T.);
#69601=ADVANCED_FACE('',(#8851),#2947,.T.);
#69602=ADVANCED_FACE('',(#8852),#2948,.T.);
#69603=ADVANCED_FACE('',(#8853),#2949,.T.);
#69604=ADVANCED_FACE('',(#8854),#2950,.T.);
#69605=ADVANCED_FACE('',(#8855),#2951,.T.);
#69606=ADVANCED_FACE('',(#8856),#2952,.T.);
#69607=ADVANCED_FACE('',(#8857),#2953,.T.);
#69608=ADVANCED_FACE('',(#8858),#2954,.T.);
#69609=ADVANCED_FACE('',(#8859),#2955,.T.);
#69610=ADVANCED_FACE('',(#8860),#2956,.T.);
#69611=ADVANCED_FACE('',(#8861),#2957,.T.);
#69612=ADVANCED_FACE('',(#8862),#2958,.T.);
#69613=ADVANCED_FACE('',(#8863),#2959,.T.);
#69614=ADVANCED_FACE('',(#8864),#2960,.T.);
#69615=ADVANCED_FACE('',(#8865),#2961,.T.);
#69616=ADVANCED_FACE('',(#8866),#2962,.T.);
#69617=ADVANCED_FACE('',(#8867),#2963,.T.);
#69618=ADVANCED_FACE('',(#8868),#2964,.T.);
#69619=ADVANCED_FACE('',(#8869),#2965,.T.);
#69620=ADVANCED_FACE('',(#8870),#2966,.T.);
#69621=ADVANCED_FACE('',(#8871),#2967,.T.);
#69622=ADVANCED_FACE('',(#8872),#2968,.T.);
#69623=ADVANCED_FACE('',(#8873),#2969,.T.);
#69624=ADVANCED_FACE('',(#8874),#2970,.T.);
#69625=ADVANCED_FACE('',(#8875),#2971,.T.);
#69626=ADVANCED_FACE('',(#8876),#2972,.T.);
#69627=ADVANCED_FACE('',(#8877),#2973,.T.);
#69628=ADVANCED_FACE('',(#8878),#2974,.T.);
#69629=ADVANCED_FACE('',(#8879),#2975,.T.);
#69630=ADVANCED_FACE('',(#8880),#2976,.T.);
#69631=ADVANCED_FACE('',(#8881),#2977,.T.);
#69632=ADVANCED_FACE('',(#8882),#2978,.T.);
#69633=ADVANCED_FACE('',(#8883),#2979,.T.);
#69634=ADVANCED_FACE('',(#8884),#5165,.T.);
#69635=ADVANCED_FACE('',(#8885),#2980,.T.);
#69636=ADVANCED_FACE('',(#8886),#2981,.T.);
#69637=ADVANCED_FACE('',(#8887),#5166,.T.);
#69638=ADVANCED_FACE('',(#8888),#2982,.T.);
#69639=ADVANCED_FACE('',(#8889),#2983,.T.);
#69640=ADVANCED_FACE('',(#8890),#5167,.T.);
#69641=ADVANCED_FACE('',(#8891),#2984,.T.);
#69642=ADVANCED_FACE('',(#8892),#2985,.T.);
#69643=ADVANCED_FACE('',(#8893),#5168,.T.);
#69644=ADVANCED_FACE('',(#8894),#2986,.T.);
#69645=ADVANCED_FACE('',(#8895),#2987,.T.);
#69646=ADVANCED_FACE('',(#8896),#5169,.T.);
#69647=ADVANCED_FACE('',(#8897),#2988,.T.);
#69648=ADVANCED_FACE('',(#8898),#2989,.T.);
#69649=ADVANCED_FACE('',(#8899),#5170,.T.);
#69650=ADVANCED_FACE('',(#8900),#2990,.T.);
#69651=ADVANCED_FACE('',(#8901),#2991,.T.);
#69652=ADVANCED_FACE('',(#8902),#2992,.T.);
#69653=ADVANCED_FACE('',(#8903),#2993,.T.);
#69654=ADVANCED_FACE('',(#8904),#5171,.T.);
#69655=ADVANCED_FACE('',(#8905),#2994,.T.);
#69656=ADVANCED_FACE('',(#8906),#2995,.T.);
#69657=ADVANCED_FACE('',(#8907),#5172,.T.);
#69658=ADVANCED_FACE('',(#8908),#2996,.T.);
#69659=ADVANCED_FACE('',(#8909),#2997,.T.);
#69660=ADVANCED_FACE('',(#8910),#5173,.T.);
#69661=ADVANCED_FACE('',(#8911),#2998,.T.);
#69662=ADVANCED_FACE('',(#8912),#2999,.T.);
#69663=ADVANCED_FACE('',(#8913),#5174,.T.);
#69664=ADVANCED_FACE('',(#8914),#3000,.T.);
#69665=ADVANCED_FACE('',(#8915),#3001,.T.);
#69666=ADVANCED_FACE('',(#8916),#5175,.T.);
#69667=ADVANCED_FACE('',(#8917),#3002,.T.);
#69668=ADVANCED_FACE('',(#8918),#3003,.T.);
#69669=ADVANCED_FACE('',(#8919),#5176,.T.);
#69670=ADVANCED_FACE('',(#8920),#3004,.T.);
#69671=ADVANCED_FACE('',(#8921),#3005,.T.);
#69672=ADVANCED_FACE('',(#8922),#5177,.T.);
#69673=ADVANCED_FACE('',(#8923),#3006,.T.);
#69674=ADVANCED_FACE('',(#8924),#3007,.T.);
#69675=ADVANCED_FACE('',(#8925),#5178,.T.);
#69676=ADVANCED_FACE('',(#8926),#3008,.T.);
#69677=ADVANCED_FACE('',(#8927),#3009,.T.);
#69678=ADVANCED_FACE('',(#8928),#5179,.T.);
#69679=ADVANCED_FACE('',(#8929),#3010,.T.);
#69680=ADVANCED_FACE('',(#8930),#3011,.T.);
#69681=ADVANCED_FACE('',(#8931),#5180,.T.);
#69682=ADVANCED_FACE('',(#8932),#3012,.T.);
#69683=ADVANCED_FACE('',(#8933),#3013,.T.);
#69684=ADVANCED_FACE('',(#8934),#5181,.T.);
#69685=ADVANCED_FACE('',(#8935),#3014,.T.);
#69686=ADVANCED_FACE('',(#8936),#3015,.T.);
#69687=ADVANCED_FACE('',(#8937),#3016,.T.);
#69688=ADVANCED_FACE('',(#8938),#5182,.T.);
#69689=ADVANCED_FACE('',(#8939),#3017,.T.);
#69690=ADVANCED_FACE('',(#8940),#5183,.T.);
#69691=ADVANCED_FACE('',(#8941),#3018,.T.);
#69692=ADVANCED_FACE('',(#8942),#3019,.T.);
#69693=ADVANCED_FACE('',(#8943),#5184,.T.);
#69694=ADVANCED_FACE('',(#8944),#3020,.T.);
#69695=ADVANCED_FACE('',(#8945),#3021,.T.);
#69696=ADVANCED_FACE('',(#8946),#5185,.T.);
#69697=ADVANCED_FACE('',(#8947),#3022,.T.);
#69698=ADVANCED_FACE('',(#8948),#3023,.T.);
#69699=ADVANCED_FACE('',(#8949),#5186,.T.);
#69700=ADVANCED_FACE('',(#8950),#3024,.T.);
#69701=ADVANCED_FACE('',(#8951),#3025,.T.);
#69702=ADVANCED_FACE('',(#8952),#5187,.T.);
#69703=ADVANCED_FACE('',(#8953),#3026,.T.);
#69704=ADVANCED_FACE('',(#8954),#3027,.T.);
#69705=ADVANCED_FACE('',(#8955),#5188,.T.);
#69706=ADVANCED_FACE('',(#8956),#3028,.T.);
#69707=ADVANCED_FACE('',(#8957),#3029,.T.);
#69708=ADVANCED_FACE('',(#8958),#5189,.T.);
#69709=ADVANCED_FACE('',(#8959),#3030,.T.);
#69710=ADVANCED_FACE('',(#8960),#3031,.T.);
#69711=ADVANCED_FACE('',(#8961),#5190,.T.);
#69712=ADVANCED_FACE('',(#8962),#3032,.T.);
#69713=ADVANCED_FACE('',(#8963),#3033,.T.);
#69714=ADVANCED_FACE('',(#8964),#5191,.T.);
#69715=ADVANCED_FACE('',(#8965),#3034,.T.);
#69716=ADVANCED_FACE('',(#8966),#5192,.T.);
#69717=ADVANCED_FACE('',(#8967),#3035,.T.);
#69718=ADVANCED_FACE('',(#8968),#3036,.T.);
#69719=ADVANCED_FACE('',(#8969),#3037,.T.);
#69720=ADVANCED_FACE('',(#8970),#3038,.T.);
#69721=ADVANCED_FACE('',(#8971),#5193,.T.);
#69722=ADVANCED_FACE('',(#8972),#3039,.T.);
#69723=ADVANCED_FACE('',(#8973),#3040,.T.);
#69724=ADVANCED_FACE('',(#8974),#5194,.T.);
#69725=ADVANCED_FACE('',(#8975),#3041,.T.);
#69726=ADVANCED_FACE('',(#8976),#3042,.T.);
#69727=ADVANCED_FACE('',(#8977),#5195,.T.);
#69728=ADVANCED_FACE('',(#8978),#3043,.T.);
#69729=ADVANCED_FACE('',(#8979),#3044,.T.);
#69730=ADVANCED_FACE('',(#8980),#5196,.T.);
#69731=ADVANCED_FACE('',(#8981),#3045,.T.);
#69732=ADVANCED_FACE('',(#8982),#3046,.T.);
#69733=ADVANCED_FACE('',(#8983),#5197,.T.);
#69734=ADVANCED_FACE('',(#8984),#3047,.T.);
#69735=ADVANCED_FACE('',(#8985),#3048,.T.);
#69736=ADVANCED_FACE('',(#8986),#5198,.T.);
#69737=ADVANCED_FACE('',(#8987),#3049,.T.);
#69738=ADVANCED_FACE('',(#8988),#3050,.T.);
#69739=ADVANCED_FACE('',(#8989),#5199,.T.);
#69740=ADVANCED_FACE('',(#8990),#3051,.T.);
#69741=ADVANCED_FACE('',(#8991),#3052,.T.);
#69742=ADVANCED_FACE('',(#8992),#5200,.T.);
#69743=ADVANCED_FACE('',(#8993),#3053,.T.);
#69744=ADVANCED_FACE('',(#8994),#3054,.T.);
#69745=ADVANCED_FACE('',(#8995),#5201,.T.);
#69746=ADVANCED_FACE('',(#8996),#3055,.T.);
#69747=ADVANCED_FACE('',(#8997),#3056,.T.);
#69748=ADVANCED_FACE('',(#8998),#5202,.T.);
#69749=ADVANCED_FACE('',(#8999),#3057,.T.);
#69750=ADVANCED_FACE('',(#9000),#3058,.T.);
#69751=ADVANCED_FACE('',(#9001),#5203,.T.);
#69752=ADVANCED_FACE('',(#9002),#3059,.T.);
#69753=ADVANCED_FACE('',(#9003),#3060,.T.);
#69754=ADVANCED_FACE('',(#9004),#5204,.T.);
#69755=ADVANCED_FACE('',(#9005),#3061,.T.);
#69756=ADVANCED_FACE('',(#9006),#3062,.T.);
#69757=ADVANCED_FACE('',(#9007),#5205,.T.);
#69758=ADVANCED_FACE('',(#9008),#3063,.T.);
#69759=ADVANCED_FACE('',(#9009),#3064,.T.);
#69760=ADVANCED_FACE('',(#9010),#3065,.T.);
#69761=ADVANCED_FACE('',(#9011),#3066,.T.);
#69762=ADVANCED_FACE('',(#9012),#5206,.T.);
#69763=ADVANCED_FACE('',(#9013),#3067,.T.);
#69764=ADVANCED_FACE('',(#9014),#3068,.T.);
#69765=ADVANCED_FACE('',(#9015),#5207,.T.);
#69766=ADVANCED_FACE('',(#9016),#3069,.T.);
#69767=ADVANCED_FACE('',(#9017),#3070,.T.);
#69768=ADVANCED_FACE('',(#9018),#5208,.T.);
#69769=ADVANCED_FACE('',(#9019),#3071,.T.);
#69770=ADVANCED_FACE('',(#9020),#3072,.T.);
#69771=ADVANCED_FACE('',(#9021),#5209,.T.);
#69772=ADVANCED_FACE('',(#9022),#3073,.T.);
#69773=ADVANCED_FACE('',(#9023),#3074,.T.);
#69774=ADVANCED_FACE('',(#9024),#5210,.T.);
#69775=ADVANCED_FACE('',(#9025),#3075,.T.);
#69776=ADVANCED_FACE('',(#9026),#3076,.T.);
#69777=ADVANCED_FACE('',(#9027),#5211,.T.);
#69778=ADVANCED_FACE('',(#9028),#3077,.T.);
#69779=ADVANCED_FACE('',(#9029),#3078,.T.);
#69780=ADVANCED_FACE('',(#9030),#5212,.T.);
#69781=ADVANCED_FACE('',(#9031),#3079,.T.);
#69782=ADVANCED_FACE('',(#9032),#3080,.T.);
#69783=ADVANCED_FACE('',(#9033),#5213,.T.);
#69784=ADVANCED_FACE('',(#9034),#3081,.T.);
#69785=ADVANCED_FACE('',(#9035),#3082,.T.);
#69786=ADVANCED_FACE('',(#9036),#5214,.T.);
#69787=ADVANCED_FACE('',(#9037),#3083,.T.);
#69788=ADVANCED_FACE('',(#9038),#3084,.T.);
#69789=ADVANCED_FACE('',(#9039),#5215,.T.);
#69790=ADVANCED_FACE('',(#9040),#3085,.T.);
#69791=ADVANCED_FACE('',(#9041),#3086,.T.);
#69792=ADVANCED_FACE('',(#9042),#5216,.T.);
#69793=ADVANCED_FACE('',(#9043),#3087,.T.);
#69794=ADVANCED_FACE('',(#9044),#3088,.T.);
#69795=ADVANCED_FACE('',(#9045),#5217,.T.);
#69796=ADVANCED_FACE('',(#9046),#3089,.T.);
#69797=ADVANCED_FACE('',(#9047),#3090,.T.);
#69798=ADVANCED_FACE('',(#9048),#5218,.T.);
#69799=ADVANCED_FACE('',(#9049),#3091,.T.);
#69800=ADVANCED_FACE('',(#9050),#3092,.T.);
#69801=ADVANCED_FACE('',(#9051),#5219,.T.);
#69802=ADVANCED_FACE('',(#9052),#5220,.T.);
#69803=ADVANCED_FACE('',(#9053),#3093,.T.);
#69804=ADVANCED_FACE('',(#9054),#3094,.T.);
#69805=ADVANCED_FACE('',(#9055),#3095,.T.);
#69806=ADVANCED_FACE('',(#9056),#3096,.T.);
#69807=ADVANCED_FACE('',(#9057),#3097,.T.);
#69808=ADVANCED_FACE('',(#9058),#3098,.T.);
#69809=ADVANCED_FACE('',(#9059),#3099,.T.);
#69810=ADVANCED_FACE('',(#9060),#3100,.T.);
#69811=ADVANCED_FACE('',(#9061),#3101,.T.);
#69812=ADVANCED_FACE('',(#9062),#3102,.T.);
#69813=ADVANCED_FACE('',(#9063),#3103,.T.);
#69814=ADVANCED_FACE('',(#9064),#3104,.T.);
#69815=ADVANCED_FACE('',(#9065),#3105,.T.);
#69816=ADVANCED_FACE('',(#9066),#3106,.T.);
#69817=ADVANCED_FACE('',(#9067),#3107,.T.);
#69818=ADVANCED_FACE('',(#9068),#3108,.T.);
#69819=ADVANCED_FACE('',(#9069),#3109,.T.);
#69820=ADVANCED_FACE('',(#9070),#3110,.T.);
#69821=ADVANCED_FACE('',(#9071),#3111,.T.);
#69822=ADVANCED_FACE('',(#9072),#3112,.T.);
#69823=ADVANCED_FACE('',(#9073),#3113,.T.);
#69824=ADVANCED_FACE('',(#9074),#3114,.T.);
#69825=ADVANCED_FACE('',(#9075),#3115,.T.);
#69826=ADVANCED_FACE('',(#9076),#3116,.T.);
#69827=ADVANCED_FACE('',(#9077),#3117,.T.);
#69828=ADVANCED_FACE('',(#9078),#3118,.T.);
#69829=ADVANCED_FACE('',(#9079),#3119,.T.);
#69830=ADVANCED_FACE('',(#9080),#3120,.T.);
#69831=ADVANCED_FACE('',(#9081),#3121,.T.);
#69832=ADVANCED_FACE('',(#9082),#3122,.T.);
#69833=ADVANCED_FACE('',(#9083),#3123,.T.);
#69834=ADVANCED_FACE('',(#9084),#3124,.T.);
#69835=ADVANCED_FACE('',(#9085),#3125,.T.);
#69836=ADVANCED_FACE('',(#9086),#3126,.T.);
#69837=ADVANCED_FACE('',(#9087),#3127,.T.);
#69838=ADVANCED_FACE('',(#9088),#3128,.T.);
#69839=ADVANCED_FACE('',(#9089),#3129,.T.);
#69840=ADVANCED_FACE('',(#9090),#3130,.T.);
#69841=ADVANCED_FACE('',(#9091),#3131,.T.);
#69842=ADVANCED_FACE('',(#9092),#3132,.T.);
#69843=ADVANCED_FACE('',(#9093),#3133,.T.);
#69844=ADVANCED_FACE('',(#9094),#3134,.T.);
#69845=ADVANCED_FACE('',(#9095),#3135,.T.);
#69846=ADVANCED_FACE('',(#9096),#3136,.T.);
#69847=ADVANCED_FACE('',(#9097),#3137,.T.);
#69848=ADVANCED_FACE('',(#9098),#3138,.T.);
#69849=ADVANCED_FACE('',(#9099),#3139,.T.);
#69850=ADVANCED_FACE('',(#9100),#3140,.T.);
#69851=ADVANCED_FACE('',(#9101),#3141,.T.);
#69852=ADVANCED_FACE('',(#9102),#3142,.T.);
#69853=ADVANCED_FACE('',(#9103),#3143,.T.);
#69854=ADVANCED_FACE('',(#9104),#3144,.T.);
#69855=ADVANCED_FACE('',(#9105),#3145,.T.);
#69856=ADVANCED_FACE('',(#9106),#3146,.T.);
#69857=ADVANCED_FACE('',(#9107),#3147,.T.);
#69858=ADVANCED_FACE('',(#9108),#3148,.T.);
#69859=ADVANCED_FACE('',(#9109),#3149,.T.);
#69860=ADVANCED_FACE('',(#9110),#3150,.T.);
#69861=ADVANCED_FACE('',(#9111),#3151,.T.);
#69862=ADVANCED_FACE('',(#9112),#3152,.T.);
#69863=ADVANCED_FACE('',(#9113),#3153,.T.);
#69864=ADVANCED_FACE('',(#9114),#3154,.T.);
#69865=ADVANCED_FACE('',(#9115),#3155,.T.);
#69866=ADVANCED_FACE('',(#9116),#3156,.T.);
#69867=ADVANCED_FACE('',(#9117),#3157,.T.);
#69868=ADVANCED_FACE('',(#9118),#3158,.T.);
#69869=ADVANCED_FACE('',(#9119),#3159,.T.);
#69870=ADVANCED_FACE('',(#9120),#3160,.T.);
#69871=ADVANCED_FACE('',(#9121),#3161,.T.);
#69872=ADVANCED_FACE('',(#9122),#3162,.T.);
#69873=ADVANCED_FACE('',(#9123),#3163,.T.);
#69874=ADVANCED_FACE('',(#9124),#3164,.T.);
#69875=ADVANCED_FACE('',(#9125),#3165,.T.);
#69876=ADVANCED_FACE('',(#9126),#3166,.T.);
#69877=ADVANCED_FACE('',(#9127),#3167,.T.);
#69878=ADVANCED_FACE('',(#9128),#3168,.T.);
#69879=ADVANCED_FACE('',(#9129),#3169,.T.);
#69880=ADVANCED_FACE('',(#9130),#3170,.T.);
#69881=ADVANCED_FACE('',(#9131),#3171,.T.);
#69882=ADVANCED_FACE('',(#9132),#3172,.T.);
#69883=ADVANCED_FACE('',(#9133),#3173,.T.);
#69884=ADVANCED_FACE('',(#9134),#3174,.T.);
#69885=ADVANCED_FACE('',(#9135),#3175,.T.);
#69886=ADVANCED_FACE('',(#9136),#3176,.T.);
#69887=ADVANCED_FACE('',(#9137),#3177,.T.);
#69888=ADVANCED_FACE('',(#9138),#3178,.T.);
#69889=ADVANCED_FACE('',(#9139),#3179,.T.);
#69890=ADVANCED_FACE('',(#9140),#3180,.T.);
#69891=ADVANCED_FACE('',(#9141),#3181,.T.);
#69892=ADVANCED_FACE('',(#9142),#3182,.T.);
#69893=ADVANCED_FACE('',(#9143),#3183,.T.);
#69894=ADVANCED_FACE('',(#9144),#3184,.T.);
#69895=ADVANCED_FACE('',(#9145),#3185,.T.);
#69896=ADVANCED_FACE('',(#9146),#3186,.T.);
#69897=ADVANCED_FACE('',(#9147),#3187,.T.);
#69898=ADVANCED_FACE('',(#9148),#3188,.T.);
#69899=ADVANCED_FACE('',(#9149),#3189,.T.);
#69900=ADVANCED_FACE('',(#9150),#3190,.T.);
#69901=ADVANCED_FACE('',(#9151),#3191,.T.);
#69902=ADVANCED_FACE('',(#9152),#3192,.T.);
#69903=ADVANCED_FACE('',(#9153),#3193,.T.);
#69904=ADVANCED_FACE('',(#9154),#3194,.T.);
#69905=ADVANCED_FACE('',(#9155),#3195,.T.);
#69906=ADVANCED_FACE('',(#9156),#3196,.T.);
#69907=ADVANCED_FACE('',(#9157),#3197,.T.);
#69908=ADVANCED_FACE('',(#9158),#3198,.T.);
#69909=ADVANCED_FACE('',(#9159),#3199,.T.);
#69910=ADVANCED_FACE('',(#9160),#3200,.T.);
#69911=ADVANCED_FACE('',(#9161),#3201,.T.);
#69912=ADVANCED_FACE('',(#9162),#3202,.T.);
#69913=ADVANCED_FACE('',(#9163),#3203,.T.);
#69914=ADVANCED_FACE('',(#9164),#3204,.T.);
#69915=ADVANCED_FACE('',(#9165),#3205,.T.);
#69916=ADVANCED_FACE('',(#9166),#3206,.T.);
#69917=ADVANCED_FACE('',(#9167),#3207,.T.);
#69918=ADVANCED_FACE('',(#9168),#3208,.T.);
#69919=ADVANCED_FACE('',(#9169),#3209,.T.);
#69920=ADVANCED_FACE('',(#9170),#3210,.T.);
#69921=ADVANCED_FACE('',(#9171),#5221,.T.);
#69922=ADVANCED_FACE('',(#9172),#3211,.T.);
#69923=ADVANCED_FACE('',(#9173),#3212,.T.);
#69924=ADVANCED_FACE('',(#9174),#5222,.T.);
#69925=ADVANCED_FACE('',(#9175),#3213,.T.);
#69926=ADVANCED_FACE('',(#9176),#3214,.T.);
#69927=ADVANCED_FACE('',(#9177),#5223,.T.);
#69928=ADVANCED_FACE('',(#9178),#3215,.T.);
#69929=ADVANCED_FACE('',(#9179),#3216,.T.);
#69930=ADVANCED_FACE('',(#9180),#5224,.T.);
#69931=ADVANCED_FACE('',(#9181),#3217,.T.);
#69932=ADVANCED_FACE('',(#9182),#3218,.T.);
#69933=ADVANCED_FACE('',(#9183),#5225,.T.);
#69934=ADVANCED_FACE('',(#9184),#3219,.T.);
#69935=ADVANCED_FACE('',(#9185),#3220,.T.);
#69936=ADVANCED_FACE('',(#9186),#5226,.T.);
#69937=ADVANCED_FACE('',(#9187),#3221,.T.);
#69938=ADVANCED_FACE('',(#9188),#3222,.T.);
#69939=ADVANCED_FACE('',(#9189),#5227,.T.);
#69940=ADVANCED_FACE('',(#9190),#3223,.T.);
#69941=ADVANCED_FACE('',(#9191),#3224,.T.);
#69942=ADVANCED_FACE('',(#9192),#5228,.T.);
#69943=ADVANCED_FACE('',(#9193),#3225,.T.);
#69944=ADVANCED_FACE('',(#9194),#3226,.T.);
#69945=ADVANCED_FACE('',(#9195),#5229,.T.);
#69946=ADVANCED_FACE('',(#9196),#3227,.T.);
#69947=ADVANCED_FACE('',(#9197),#3228,.T.);
#69948=ADVANCED_FACE('',(#9198),#5230,.T.);
#69949=ADVANCED_FACE('',(#9199),#3229,.T.);
#69950=ADVANCED_FACE('',(#9200),#3230,.T.);
#69951=ADVANCED_FACE('',(#9201),#5231,.T.);
#69952=ADVANCED_FACE('',(#9202),#3231,.T.);
#69953=ADVANCED_FACE('',(#9203),#3232,.T.);
#69954=ADVANCED_FACE('',(#9204),#5232,.T.);
#69955=ADVANCED_FACE('',(#9205),#3233,.T.);
#69956=ADVANCED_FACE('',(#9206),#3234,.T.);
#69957=ADVANCED_FACE('',(#9207),#5233,.T.);
#69958=ADVANCED_FACE('',(#9208),#3235,.T.);
#69959=ADVANCED_FACE('',(#9209),#3236,.T.);
#69960=ADVANCED_FACE('',(#9210),#5234,.T.);
#69961=ADVANCED_FACE('',(#9211),#3237,.T.);
#69962=ADVANCED_FACE('',(#9212),#3238,.T.);
#69963=ADVANCED_FACE('',(#9213),#3239,.T.);
#69964=ADVANCED_FACE('',(#9214),#3240,.T.);
#69965=ADVANCED_FACE('',(#9215),#5235,.T.);
#69966=ADVANCED_FACE('',(#9216),#3241,.T.);
#69967=ADVANCED_FACE('',(#9217),#3242,.T.);
#69968=ADVANCED_FACE('',(#9218),#5236,.T.);
#69969=ADVANCED_FACE('',(#9219),#3243,.T.);
#69970=ADVANCED_FACE('',(#9220),#3244,.T.);
#69971=ADVANCED_FACE('',(#9221),#5237,.T.);
#69972=ADVANCED_FACE('',(#9222),#3245,.T.);
#69973=ADVANCED_FACE('',(#9223),#3246,.T.);
#69974=ADVANCED_FACE('',(#9224),#3247,.T.);
#69975=ADVANCED_FACE('',(#9225),#5238,.T.);
#69976=ADVANCED_FACE('',(#9226),#3248,.T.);
#69977=ADVANCED_FACE('',(#9227),#5239,.T.);
#69978=ADVANCED_FACE('',(#9228),#3249,.T.);
#69979=ADVANCED_FACE('',(#9229),#3250,.T.);
#69980=ADVANCED_FACE('',(#9230),#5240,.T.);
#69981=ADVANCED_FACE('',(#9231),#3251,.T.);
#69982=ADVANCED_FACE('',(#9232),#3252,.T.);
#69983=ADVANCED_FACE('',(#9233),#5241,.T.);
#69984=ADVANCED_FACE('',(#9234),#3253,.T.);
#69985=ADVANCED_FACE('',(#9235),#3254,.T.);
#69986=ADVANCED_FACE('',(#9236),#5242,.T.);
#69987=ADVANCED_FACE('',(#9237),#3255,.T.);
#69988=ADVANCED_FACE('',(#9238),#3256,.T.);
#69989=ADVANCED_FACE('',(#9239),#5243,.T.);
#69990=ADVANCED_FACE('',(#9240),#3257,.T.);
#69991=ADVANCED_FACE('',(#9241),#3258,.T.);
#69992=ADVANCED_FACE('',(#9242),#5244,.T.);
#69993=ADVANCED_FACE('',(#9243),#3259,.T.);
#69994=ADVANCED_FACE('',(#9244),#3260,.T.);
#69995=ADVANCED_FACE('',(#9245),#5245,.T.);
#69996=ADVANCED_FACE('',(#9246),#3261,.T.);
#69997=ADVANCED_FACE('',(#9247),#3262,.T.);
#69998=ADVANCED_FACE('',(#9248),#5246,.T.);
#69999=ADVANCED_FACE('',(#9249),#3263,.T.);
#70000=ADVANCED_FACE('',(#9250),#3264,.T.);
#70001=ADVANCED_FACE('',(#9251),#5247,.T.);
#70002=ADVANCED_FACE('',(#9252),#3265,.T.);
#70003=ADVANCED_FACE('',(#9253),#3266,.T.);
#70004=ADVANCED_FACE('',(#9254),#5248,.T.);
#70005=ADVANCED_FACE('',(#9255),#3267,.T.);
#70006=ADVANCED_FACE('',(#9256),#3268,.T.);
#70007=ADVANCED_FACE('',(#9257),#66013,.T.);
#70008=ADVANCED_FACE('',(#9258),#3269,.T.);
#70009=ADVANCED_FACE('',(#9259),#5249,.T.);
#70010=ADVANCED_FACE('',(#9260),#3270,.T.);
#70011=ADVANCED_FACE('',(#9261),#66014,.T.);
#70012=ADVANCED_FACE('',(#9262),#3271,.T.);
#70013=ADVANCED_FACE('',(#9263),#5250,.T.);
#70014=ADVANCED_FACE('',(#9264),#3272,.T.);
#70015=ADVANCED_FACE('',(#9265),#66015,.T.);
#70016=ADVANCED_FACE('',(#9266),#3273,.T.);
#70017=ADVANCED_FACE('',(#9267),#5251,.T.);
#70018=ADVANCED_FACE('',(#9268),#3274,.T.);
#70019=ADVANCED_FACE('',(#9269),#66016,.T.);
#70020=ADVANCED_FACE('',(#9270),#3275,.T.);
#70021=ADVANCED_FACE('',(#9271),#5252,.T.);
#70022=ADVANCED_FACE('',(#9272),#3276,.T.);
#70023=ADVANCED_FACE('',(#9273),#66017,.T.);
#70024=ADVANCED_FACE('',(#9274),#3277,.T.);
#70025=ADVANCED_FACE('',(#9275),#5253,.T.);
#70026=ADVANCED_FACE('',(#9276),#3278,.T.);
#70027=ADVANCED_FACE('',(#9277),#66018,.T.);
#70028=ADVANCED_FACE('',(#9278),#3279,.T.);
#70029=ADVANCED_FACE('',(#9279),#5254,.T.);
#70030=ADVANCED_FACE('',(#9280),#3280,.T.);
#70031=ADVANCED_FACE('',(#9281),#66019,.T.);
#70032=ADVANCED_FACE('',(#9282),#3281,.T.);
#70033=ADVANCED_FACE('',(#9283),#5255,.T.);
#70034=ADVANCED_FACE('',(#9284),#3282,.T.);
#70035=ADVANCED_FACE('',(#9285),#66020,.T.);
#70036=ADVANCED_FACE('',(#9286),#3283,.T.);
#70037=ADVANCED_FACE('',(#9287),#5256,.T.);
#70038=ADVANCED_FACE('',(#9288),#3284,.T.);
#70039=ADVANCED_FACE('',(#9289),#66021,.T.);
#70040=ADVANCED_FACE('',(#9290),#3285,.T.);
#70041=ADVANCED_FACE('',(#9291),#5257,.T.);
#70042=ADVANCED_FACE('',(#9292),#3286,.T.);
#70043=ADVANCED_FACE('',(#9293),#66022,.T.);
#70044=ADVANCED_FACE('',(#9294),#3287,.T.);
#70045=ADVANCED_FACE('',(#9295),#5258,.T.);
#70046=ADVANCED_FACE('',(#9296),#3288,.T.);
#70047=ADVANCED_FACE('',(#9297),#66023,.T.);
#70048=ADVANCED_FACE('',(#9298),#3289,.T.);
#70049=ADVANCED_FACE('',(#9299),#5259,.T.);
#70050=ADVANCED_FACE('',(#9300),#3290,.T.);
#70051=ADVANCED_FACE('',(#9301),#66024,.T.);
#70052=ADVANCED_FACE('',(#9302),#3291,.T.);
#70053=ADVANCED_FACE('',(#9303),#5260,.T.);
#70054=ADVANCED_FACE('',(#9304),#3292,.T.);
#70055=ADVANCED_FACE('',(#9305),#66025,.T.);
#70056=ADVANCED_FACE('',(#9306),#3293,.T.);
#70057=ADVANCED_FACE('',(#9307),#5261,.T.);
#70058=ADVANCED_FACE('',(#9308),#3294,.T.);
#70059=ADVANCED_FACE('',(#9309),#66026,.T.);
#70060=ADVANCED_FACE('',(#9310),#3295,.T.);
#70061=ADVANCED_FACE('',(#9311),#5262,.T.);
#70062=ADVANCED_FACE('',(#9312),#3296,.T.);
#70063=ADVANCED_FACE('',(#9313),#66027,.T.);
#70064=ADVANCED_FACE('',(#9314),#3297,.T.);
#70065=ADVANCED_FACE('',(#9315),#5263,.T.);
#70066=ADVANCED_FACE('',(#9316),#3298,.T.);
#70067=ADVANCED_FACE('',(#9317),#66028,.T.);
#70068=ADVANCED_FACE('',(#9318),#3299,.T.);
#70069=ADVANCED_FACE('',(#9319),#5264,.T.);
#70070=ADVANCED_FACE('',(#9320),#3300,.T.);
#70071=ADVANCED_FACE('',(#9321),#66029,.T.);
#70072=ADVANCED_FACE('',(#9322),#3301,.T.);
#70073=ADVANCED_FACE('',(#9323),#5265,.T.);
#70074=ADVANCED_FACE('',(#9324),#3302,.T.);
#70075=ADVANCED_FACE('',(#9325),#66030,.T.);
#70076=ADVANCED_FACE('',(#9326),#3303,.T.);
#70077=ADVANCED_FACE('',(#9327),#5266,.T.);
#70078=ADVANCED_FACE('',(#9328),#3304,.T.);
#70079=ADVANCED_FACE('',(#9329),#66031,.T.);
#70080=ADVANCED_FACE('',(#9330),#3305,.T.);
#70081=ADVANCED_FACE('',(#9331),#5267,.T.);
#70082=ADVANCED_FACE('',(#9332),#3306,.T.);
#70083=ADVANCED_FACE('',(#9333),#66032,.T.);
#70084=ADVANCED_FACE('',(#9334),#3307,.T.);
#70085=ADVANCED_FACE('',(#9335),#5268,.T.);
#70086=ADVANCED_FACE('',(#9336),#3308,.T.);
#70087=ADVANCED_FACE('',(#9337),#66033,.T.);
#70088=ADVANCED_FACE('',(#9338),#3309,.T.);
#70089=ADVANCED_FACE('',(#9339),#5269,.T.);
#70090=ADVANCED_FACE('',(#9340),#3310,.T.);
#70091=ADVANCED_FACE('',(#9341),#3311,.T.);
#70092=ADVANCED_FACE('',(#9342),#3312,.T.);
#70093=ADVANCED_FACE('',(#9343),#66034,.T.);
#70094=ADVANCED_FACE('',(#9344),#3313,.T.);
#70095=ADVANCED_FACE('',(#9345),#5270,.T.);
#70096=ADVANCED_FACE('',(#9346),#3314,.T.);
#70097=ADVANCED_FACE('',(#9347),#66035,.T.);
#70098=ADVANCED_FACE('',(#9348),#3315,.T.);
#70099=ADVANCED_FACE('',(#9349),#5271,.T.);
#70100=ADVANCED_FACE('',(#9350),#3316,.T.);
#70101=ADVANCED_FACE('',(#9351),#66036,.T.);
#70102=ADVANCED_FACE('',(#9352),#3317,.T.);
#70103=ADVANCED_FACE('',(#9353),#5272,.T.);
#70104=ADVANCED_FACE('',(#9354),#3318,.T.);
#70105=ADVANCED_FACE('',(#9355),#66037,.T.);
#70106=ADVANCED_FACE('',(#9356),#3319,.T.);
#70107=ADVANCED_FACE('',(#9357),#5273,.T.);
#70108=ADVANCED_FACE('',(#9358),#3320,.T.);
#70109=ADVANCED_FACE('',(#9359),#66038,.T.);
#70110=ADVANCED_FACE('',(#9360),#3321,.T.);
#70111=ADVANCED_FACE('',(#9361),#5274,.T.);
#70112=ADVANCED_FACE('',(#9362),#3322,.T.);
#70113=ADVANCED_FACE('',(#9363),#66039,.T.);
#70114=ADVANCED_FACE('',(#9364),#3323,.T.);
#70115=ADVANCED_FACE('',(#9365),#5275,.T.);
#70116=ADVANCED_FACE('',(#9366),#3324,.T.);
#70117=ADVANCED_FACE('',(#9367),#66040,.T.);
#70118=ADVANCED_FACE('',(#9368),#3325,.T.);
#70119=ADVANCED_FACE('',(#9369),#5276,.T.);
#70120=ADVANCED_FACE('',(#9370),#3326,.T.);
#70121=ADVANCED_FACE('',(#9371),#3327,.T.);
#70122=ADVANCED_FACE('',(#9372),#3328,.T.);
#70123=ADVANCED_FACE('',(#9373),#3329,.T.);
#70124=ADVANCED_FACE('',(#9374),#3330,.T.);
#70125=ADVANCED_FACE('',(#9375),#3331,.T.);
#70126=ADVANCED_FACE('',(#9376),#3332,.T.);
#70127=ADVANCED_FACE('',(#9377),#3333,.T.);
#70128=ADVANCED_FACE('',(#9378),#3334,.T.);
#70129=ADVANCED_FACE('',(#9379),#3335,.T.);
#70130=ADVANCED_FACE('',(#9380),#3336,.T.);
#70131=ADVANCED_FACE('',(#9381),#3337,.T.);
#70132=ADVANCED_FACE('',(#9382),#3338,.T.);
#70133=ADVANCED_FACE('',(#9383),#3339,.T.);
#70134=ADVANCED_FACE('',(#9384),#3340,.T.);
#70135=ADVANCED_FACE('',(#9385),#3341,.T.);
#70136=ADVANCED_FACE('',(#9386),#3342,.T.);
#70137=ADVANCED_FACE('',(#9387),#3343,.T.);
#70138=ADVANCED_FACE('',(#9388),#3344,.T.);
#70139=ADVANCED_FACE('',(#9389),#3345,.T.);
#70140=ADVANCED_FACE('',(#9390),#3346,.T.);
#70141=ADVANCED_FACE('',(#9391),#3347,.T.);
#70142=ADVANCED_FACE('',(#9392),#3348,.T.);
#70143=ADVANCED_FACE('',(#9393),#3349,.T.);
#70144=ADVANCED_FACE('',(#9394),#3350,.T.);
#70145=ADVANCED_FACE('',(#9395),#3351,.T.);
#70146=ADVANCED_FACE('',(#9396),#3352,.T.);
#70147=ADVANCED_FACE('',(#9397),#3353,.T.);
#70148=ADVANCED_FACE('',(#9398),#3354,.T.);
#70149=ADVANCED_FACE('',(#9399),#3355,.T.);
#70150=ADVANCED_FACE('',(#9400),#3356,.T.);
#70151=ADVANCED_FACE('',(#9401),#3357,.T.);
#70152=ADVANCED_FACE('',(#9402),#3358,.T.);
#70153=ADVANCED_FACE('',(#9403),#3359,.T.);
#70154=ADVANCED_FACE('',(#9404),#3360,.T.);
#70155=ADVANCED_FACE('',(#9405),#3361,.T.);
#70156=ADVANCED_FACE('',(#9406),#3362,.T.);
#70157=ADVANCED_FACE('',(#9407),#3363,.T.);
#70158=ADVANCED_FACE('',(#9408),#3364,.T.);
#70159=ADVANCED_FACE('',(#9409),#3365,.T.);
#70160=ADVANCED_FACE('',(#9410),#3366,.T.);
#70161=ADVANCED_FACE('',(#9411),#3367,.T.);
#70162=ADVANCED_FACE('',(#9412),#3368,.T.);
#70163=ADVANCED_FACE('',(#9413),#3369,.T.);
#70164=ADVANCED_FACE('',(#9414),#3370,.T.);
#70165=ADVANCED_FACE('',(#9415),#3371,.T.);
#70166=ADVANCED_FACE('',(#9416),#3372,.T.);
#70167=ADVANCED_FACE('',(#9417),#3373,.T.);
#70168=ADVANCED_FACE('',(#9418),#3374,.T.);
#70169=ADVANCED_FACE('',(#9419),#3375,.T.);
#70170=ADVANCED_FACE('',(#9420),#3376,.T.);
#70171=ADVANCED_FACE('',(#9421),#3377,.T.);
#70172=ADVANCED_FACE('',(#9422),#3378,.T.);
#70173=ADVANCED_FACE('',(#9423),#3379,.T.);
#70174=ADVANCED_FACE('',(#9424),#3380,.T.);
#70175=ADVANCED_FACE('',(#9425),#3381,.T.);
#70176=ADVANCED_FACE('',(#9426),#3382,.T.);
#70177=ADVANCED_FACE('',(#9427),#3383,.T.);
#70178=ADVANCED_FACE('',(#9428),#3384,.T.);
#70179=ADVANCED_FACE('',(#9429),#3385,.T.);
#70180=ADVANCED_FACE('',(#9430),#3386,.T.);
#70181=ADVANCED_FACE('',(#9431),#3387,.T.);
#70182=ADVANCED_FACE('',(#9432),#3388,.T.);
#70183=ADVANCED_FACE('',(#9433),#3389,.T.);
#70184=ADVANCED_FACE('',(#9434),#3390,.T.);
#70185=ADVANCED_FACE('',(#9435),#3391,.T.);
#70186=ADVANCED_FACE('',(#9436),#3392,.T.);
#70187=ADVANCED_FACE('',(#9437),#3393,.T.);
#70188=ADVANCED_FACE('',(#9438),#3394,.T.);
#70189=ADVANCED_FACE('',(#9439),#3395,.T.);
#70190=ADVANCED_FACE('',(#9440),#3396,.T.);
#70191=ADVANCED_FACE('',(#9441),#3397,.T.);
#70192=ADVANCED_FACE('',(#9442),#3398,.T.);
#70193=ADVANCED_FACE('',(#9443),#3399,.T.);
#70194=ADVANCED_FACE('',(#9444),#3400,.T.);
#70195=ADVANCED_FACE('',(#9445),#3401,.T.);
#70196=ADVANCED_FACE('',(#9446),#3402,.T.);
#70197=ADVANCED_FACE('',(#9447),#3403,.T.);
#70198=ADVANCED_FACE('',(#9448),#3404,.T.);
#70199=ADVANCED_FACE('',(#9449),#3405,.T.);
#70200=ADVANCED_FACE('',(#9450),#3406,.T.);
#70201=ADVANCED_FACE('',(#9451),#3407,.T.);
#70202=ADVANCED_FACE('',(#9452),#3408,.T.);
#70203=ADVANCED_FACE('',(#9453),#3409,.T.);
#70204=ADVANCED_FACE('',(#9454),#3410,.T.);
#70205=ADVANCED_FACE('',(#9455),#3411,.T.);
#70206=ADVANCED_FACE('',(#9456),#3412,.T.);
#70207=ADVANCED_FACE('',(#9457),#3413,.T.);
#70208=ADVANCED_FACE('',(#9458),#3414,.T.);
#70209=ADVANCED_FACE('',(#9459),#3415,.T.);
#70210=ADVANCED_FACE('',(#9460),#3416,.T.);
#70211=ADVANCED_FACE('',(#9461),#3417,.T.);
#70212=ADVANCED_FACE('',(#9462),#3418,.T.);
#70213=ADVANCED_FACE('',(#9463),#3419,.T.);
#70214=ADVANCED_FACE('',(#9464),#3420,.T.);
#70215=ADVANCED_FACE('',(#9465),#3421,.T.);
#70216=ADVANCED_FACE('',(#9466),#3422,.T.);
#70217=ADVANCED_FACE('',(#9467),#3423,.T.);
#70218=ADVANCED_FACE('',(#9468),#3424,.T.);
#70219=ADVANCED_FACE('',(#9469),#3425,.T.);
#70220=ADVANCED_FACE('',(#9470),#3426,.T.);
#70221=ADVANCED_FACE('',(#9471),#3427,.T.);
#70222=ADVANCED_FACE('',(#9472),#3428,.T.);
#70223=ADVANCED_FACE('',(#9473),#3429,.T.);
#70224=ADVANCED_FACE('',(#9474),#3430,.T.);
#70225=ADVANCED_FACE('',(#9475),#3431,.T.);
#70226=ADVANCED_FACE('',(#9476),#3432,.T.);
#70227=ADVANCED_FACE('',(#9477),#3433,.T.);
#70228=ADVANCED_FACE('',(#9478),#3434,.T.);
#70229=ADVANCED_FACE('',(#9479),#3435,.T.);
#70230=ADVANCED_FACE('',(#9480),#3436,.T.);
#70231=ADVANCED_FACE('',(#9481),#3437,.T.);
#70232=ADVANCED_FACE('',(#9482),#3438,.T.);
#70233=ADVANCED_FACE('',(#9483),#3439,.T.);
#70234=ADVANCED_FACE('',(#9484),#3440,.T.);
#70235=ADVANCED_FACE('',(#9485),#3441,.T.);
#70236=ADVANCED_FACE('',(#9486),#3442,.T.);
#70237=ADVANCED_FACE('',(#9487),#3443,.T.);
#70238=ADVANCED_FACE('',(#9488),#5277,.T.);
#70239=ADVANCED_FACE('',(#9489),#3444,.T.);
#70240=ADVANCED_FACE('',(#9490),#3445,.T.);
#70241=ADVANCED_FACE('',(#9491),#5278,.T.);
#70242=ADVANCED_FACE('',(#9492),#3446,.T.);
#70243=ADVANCED_FACE('',(#9493),#3447,.T.);
#70244=ADVANCED_FACE('',(#9494),#5279,.T.);
#70245=ADVANCED_FACE('',(#9495),#3448,.T.);
#70246=ADVANCED_FACE('',(#9496),#3449,.T.);
#70247=ADVANCED_FACE('',(#9497),#5280,.T.);
#70248=ADVANCED_FACE('',(#9498),#3450,.T.);
#70249=ADVANCED_FACE('',(#9499),#3451,.T.);
#70250=ADVANCED_FACE('',(#9500),#5281,.T.);
#70251=ADVANCED_FACE('',(#9501),#3452,.T.);
#70252=ADVANCED_FACE('',(#9502),#3453,.T.);
#70253=ADVANCED_FACE('',(#9503),#5282,.T.);
#70254=ADVANCED_FACE('',(#9504),#3454,.T.);
#70255=ADVANCED_FACE('',(#9505),#3455,.T.);
#70256=ADVANCED_FACE('',(#9506),#3456,.T.);
#70257=ADVANCED_FACE('',(#9507),#3457,.T.);
#70258=ADVANCED_FACE('',(#9508),#5283,.T.);
#70259=ADVANCED_FACE('',(#9509),#3458,.T.);
#70260=ADVANCED_FACE('',(#9510),#3459,.T.);
#70261=ADVANCED_FACE('',(#9511),#5284,.T.);
#70262=ADVANCED_FACE('',(#9512),#3460,.T.);
#70263=ADVANCED_FACE('',(#9513),#3461,.T.);
#70264=ADVANCED_FACE('',(#9514),#5285,.T.);
#70265=ADVANCED_FACE('',(#9515),#3462,.T.);
#70266=ADVANCED_FACE('',(#9516),#3463,.T.);
#70267=ADVANCED_FACE('',(#9517),#5286,.T.);
#70268=ADVANCED_FACE('',(#9518),#3464,.T.);
#70269=ADVANCED_FACE('',(#9519),#3465,.T.);
#70270=ADVANCED_FACE('',(#9520),#5287,.T.);
#70271=ADVANCED_FACE('',(#9521),#3466,.T.);
#70272=ADVANCED_FACE('',(#9522),#3467,.T.);
#70273=ADVANCED_FACE('',(#9523),#5288,.T.);
#70274=ADVANCED_FACE('',(#9524),#3468,.T.);
#70275=ADVANCED_FACE('',(#9525),#3469,.T.);
#70276=ADVANCED_FACE('',(#9526),#5289,.T.);
#70277=ADVANCED_FACE('',(#9527),#3470,.T.);
#70278=ADVANCED_FACE('',(#9528),#3471,.T.);
#70279=ADVANCED_FACE('',(#9529),#5290,.T.);
#70280=ADVANCED_FACE('',(#9530),#3472,.T.);
#70281=ADVANCED_FACE('',(#9531),#3473,.T.);
#70282=ADVANCED_FACE('',(#9532),#5291,.T.);
#70283=ADVANCED_FACE('',(#9533),#3474,.T.);
#70284=ADVANCED_FACE('',(#9534),#3475,.T.);
#70285=ADVANCED_FACE('',(#9535),#5292,.T.);
#70286=ADVANCED_FACE('',(#9536),#3476,.T.);
#70287=ADVANCED_FACE('',(#9537),#3477,.T.);
#70288=ADVANCED_FACE('',(#9538),#3478,.T.);
#70289=ADVANCED_FACE('',(#9539),#5293,.T.);
#70290=ADVANCED_FACE('',(#9540),#3479,.T.);
#70291=ADVANCED_FACE('',(#9541),#5294,.T.);
#70292=ADVANCED_FACE('',(#9542),#3480,.T.);
#70293=ADVANCED_FACE('',(#9543),#3481,.T.);
#70294=ADVANCED_FACE('',(#9544),#5295,.T.);
#70295=ADVANCED_FACE('',(#9545),#3482,.T.);
#70296=ADVANCED_FACE('',(#9546),#3483,.T.);
#70297=ADVANCED_FACE('',(#9547),#5296,.T.);
#70298=ADVANCED_FACE('',(#9548),#3484,.T.);
#70299=ADVANCED_FACE('',(#9549),#3485,.T.);
#70300=ADVANCED_FACE('',(#9550),#5297,.T.);
#70301=ADVANCED_FACE('',(#9551),#3486,.T.);
#70302=ADVANCED_FACE('',(#9552),#3487,.T.);
#70303=ADVANCED_FACE('',(#9553),#5298,.T.);
#70304=ADVANCED_FACE('',(#9554),#3488,.T.);
#70305=ADVANCED_FACE('',(#9555),#3489,.T.);
#70306=ADVANCED_FACE('',(#9556),#5299,.T.);
#70307=ADVANCED_FACE('',(#9557),#3490,.T.);
#70308=ADVANCED_FACE('',(#9558),#3491,.T.);
#70309=ADVANCED_FACE('',(#9559),#5300,.T.);
#70310=ADVANCED_FACE('',(#9560),#3492,.T.);
#70311=ADVANCED_FACE('',(#9561),#3493,.T.);
#70312=ADVANCED_FACE('',(#9562),#5301,.T.);
#70313=ADVANCED_FACE('',(#9563),#3494,.T.);
#70314=ADVANCED_FACE('',(#9564),#3495,.T.);
#70315=ADVANCED_FACE('',(#9565),#5302,.T.);
#70316=ADVANCED_FACE('',(#9566),#3496,.T.);
#70317=ADVANCED_FACE('',(#9567),#3497,.T.);
#70318=ADVANCED_FACE('',(#9568),#5303,.T.);
#70319=ADVANCED_FACE('',(#9569),#3498,.T.);
#70320=ADVANCED_FACE('',(#9570),#5304,.T.);
#70321=ADVANCED_FACE('',(#9571),#3499,.T.);
#70322=ADVANCED_FACE('',(#9572),#3500,.T.);
#70323=ADVANCED_FACE('',(#9573),#3501,.T.);
#70324=ADVANCED_FACE('',(#9574),#66041,.T.);
#70325=ADVANCED_FACE('',(#9575),#3502,.T.);
#70326=ADVANCED_FACE('',(#9576),#3503,.T.);
#70327=ADVANCED_FACE('',(#9577),#66042,.T.);
#70328=ADVANCED_FACE('',(#9578),#3504,.T.);
#70329=ADVANCED_FACE('',(#9579),#3505,.T.);
#70330=ADVANCED_FACE('',(#9580),#66043,.T.);
#70331=ADVANCED_FACE('',(#9581),#3506,.T.);
#70332=ADVANCED_FACE('',(#9582),#3507,.T.);
#70333=ADVANCED_FACE('',(#9583),#66044,.T.);
#70334=ADVANCED_FACE('',(#9584),#3508,.T.);
#70335=ADVANCED_FACE('',(#9585),#3509,.T.);
#70336=ADVANCED_FACE('',(#9586),#66045,.T.);
#70337=ADVANCED_FACE('',(#9587),#3510,.T.);
#70338=ADVANCED_FACE('',(#9588),#3511,.T.);
#70339=ADVANCED_FACE('',(#9589),#66046,.T.);
#70340=ADVANCED_FACE('',(#9590),#3512,.T.);
#70341=ADVANCED_FACE('',(#9591),#3513,.T.);
#70342=ADVANCED_FACE('',(#9592),#66047,.T.);
#70343=ADVANCED_FACE('',(#9593),#3514,.T.);
#70344=ADVANCED_FACE('',(#9594),#3515,.T.);
#70345=ADVANCED_FACE('',(#9595),#66048,.T.);
#70346=ADVANCED_FACE('',(#9596),#3516,.T.);
#70347=ADVANCED_FACE('',(#9597),#3517,.T.);
#70348=ADVANCED_FACE('',(#9598),#66049,.T.);
#70349=ADVANCED_FACE('',(#9599),#3518,.T.);
#70350=ADVANCED_FACE('',(#9600),#3519,.T.);
#70351=ADVANCED_FACE('',(#9601),#66050,.T.);
#70352=ADVANCED_FACE('',(#9602),#3520,.T.);
#70353=ADVANCED_FACE('',(#9603),#3521,.T.);
#70354=ADVANCED_FACE('',(#9604),#66051,.T.);
#70355=ADVANCED_FACE('',(#9605),#3522,.T.);
#70356=ADVANCED_FACE('',(#9606),#3523,.T.);
#70357=ADVANCED_FACE('',(#9607),#66052,.T.);
#70358=ADVANCED_FACE('',(#9608),#3524,.T.);
#70359=ADVANCED_FACE('',(#9609),#3525,.T.);
#70360=ADVANCED_FACE('',(#9610),#66053,.T.);
#70361=ADVANCED_FACE('',(#9611),#3526,.T.);
#70362=ADVANCED_FACE('',(#9612),#3527,.T.);
#70363=ADVANCED_FACE('',(#9613),#3528,.T.);
#70364=ADVANCED_FACE('',(#9614),#3529,.T.);
#70365=ADVANCED_FACE('',(#9615),#66054,.T.);
#70366=ADVANCED_FACE('',(#9616),#3530,.T.);
#70367=ADVANCED_FACE('',(#9617),#3531,.T.);
#70368=ADVANCED_FACE('',(#9618),#66055,.T.);
#70369=ADVANCED_FACE('',(#9619),#3532,.T.);
#70370=ADVANCED_FACE('',(#9620),#3533,.T.);
#70371=ADVANCED_FACE('',(#9621),#66056,.T.);
#70372=ADVANCED_FACE('',(#9622),#3534,.T.);
#70373=ADVANCED_FACE('',(#9623),#3535,.T.);
#70374=ADVANCED_FACE('',(#9624),#66057,.T.);
#70375=ADVANCED_FACE('',(#9625),#3536,.T.);
#70376=ADVANCED_FACE('',(#9626),#3537,.T.);
#70377=ADVANCED_FACE('',(#9627),#66058,.T.);
#70378=ADVANCED_FACE('',(#9628),#3538,.T.);
#70379=ADVANCED_FACE('',(#9629),#3539,.T.);
#70380=ADVANCED_FACE('',(#9630),#66059,.T.);
#70381=ADVANCED_FACE('',(#9631),#3540,.T.);
#70382=ADVANCED_FACE('',(#9632),#3541,.T.);
#70383=ADVANCED_FACE('',(#9633),#3542,.T.);
#70384=ADVANCED_FACE('',(#9634),#3543,.T.);
#70385=ADVANCED_FACE('',(#9635),#66060,.T.);
#70386=ADVANCED_FACE('',(#9636),#3544,.T.);
#70387=ADVANCED_FACE('',(#9637),#3545,.T.);
#70388=ADVANCED_FACE('',(#9638),#66061,.T.);
#70389=ADVANCED_FACE('',(#9639),#3546,.T.);
#70390=ADVANCED_FACE('',(#9640),#3547,.T.);
#70391=ADVANCED_FACE('',(#9641),#66062,.T.);
#70392=ADVANCED_FACE('',(#9642),#3548,.T.);
#70393=ADVANCED_FACE('',(#9643),#3549,.T.);
#70394=ADVANCED_FACE('',(#9644),#66063,.T.);
#70395=ADVANCED_FACE('',(#9645),#3550,.T.);
#70396=ADVANCED_FACE('',(#9646),#3551,.T.);
#70397=ADVANCED_FACE('',(#9647),#66064,.T.);
#70398=ADVANCED_FACE('',(#9648),#3552,.T.);
#70399=ADVANCED_FACE('',(#9649),#3553,.T.);
#70400=ADVANCED_FACE('',(#9650),#66065,.T.);
#70401=ADVANCED_FACE('',(#9651),#3554,.T.);
#70402=ADVANCED_FACE('',(#9652),#3555,.T.);
#70403=ADVANCED_FACE('',(#9653),#66066,.T.);
#70404=ADVANCED_FACE('',(#9654),#3556,.T.);
#70405=ADVANCED_FACE('',(#9655),#66067,.T.);
#70406=ADVANCED_FACE('',(#9656),#3557,.T.);
#70407=ADVANCED_FACE('',(#9657),#3558,.T.);
#70408=ADVANCED_FACE('',(#9658),#3559,.T.);
#70409=ADVANCED_FACE('',(#9659),#3560,.T.);
#70410=ADVANCED_FACE('',(#9660),#3561,.T.);
#70411=ADVANCED_FACE('',(#9661),#3562,.T.);
#70412=ADVANCED_FACE('',(#9662),#3563,.T.);
#70413=ADVANCED_FACE('',(#9663),#3564,.T.);
#70414=ADVANCED_FACE('',(#9664),#3565,.T.);
#70415=ADVANCED_FACE('',(#9665),#3566,.T.);
#70416=ADVANCED_FACE('',(#9666),#3567,.T.);
#70417=ADVANCED_FACE('',(#9667),#3568,.T.);
#70418=ADVANCED_FACE('',(#9668),#3569,.T.);
#70419=ADVANCED_FACE('',(#9669),#3570,.T.);
#70420=ADVANCED_FACE('',(#9670),#3571,.T.);
#70421=ADVANCED_FACE('',(#9671),#3572,.T.);
#70422=ADVANCED_FACE('',(#9672),#3573,.T.);
#70423=ADVANCED_FACE('',(#9673),#3574,.T.);
#70424=ADVANCED_FACE('',(#9674),#3575,.T.);
#70425=ADVANCED_FACE('',(#9675),#3576,.T.);
#70426=ADVANCED_FACE('',(#9676),#3577,.T.);
#70427=ADVANCED_FACE('',(#9677),#3578,.T.);
#70428=ADVANCED_FACE('',(#9678),#3579,.T.);
#70429=ADVANCED_FACE('',(#9679),#3580,.T.);
#70430=ADVANCED_FACE('',(#9680),#3581,.T.);
#70431=ADVANCED_FACE('',(#9681),#3582,.T.);
#70432=ADVANCED_FACE('',(#9682),#3583,.T.);
#70433=ADVANCED_FACE('',(#9683),#3584,.T.);
#70434=ADVANCED_FACE('',(#9684),#3585,.T.);
#70435=ADVANCED_FACE('',(#9685),#3586,.T.);
#70436=ADVANCED_FACE('',(#9686),#3587,.T.);
#70437=ADVANCED_FACE('',(#9687),#3588,.T.);
#70438=ADVANCED_FACE('',(#9688),#3589,.T.);
#70439=ADVANCED_FACE('',(#9689),#3590,.T.);
#70440=ADVANCED_FACE('',(#9690),#3591,.T.);
#70441=ADVANCED_FACE('',(#9691),#3592,.T.);
#70442=ADVANCED_FACE('',(#9692),#3593,.T.);
#70443=ADVANCED_FACE('',(#9693),#3594,.T.);
#70444=ADVANCED_FACE('',(#9694),#3595,.T.);
#70445=ADVANCED_FACE('',(#9695),#3596,.T.);
#70446=ADVANCED_FACE('',(#9696),#3597,.T.);
#70447=ADVANCED_FACE('',(#9697),#3598,.T.);
#70448=ADVANCED_FACE('',(#9698),#3599,.T.);
#70449=ADVANCED_FACE('',(#9699),#3600,.T.);
#70450=ADVANCED_FACE('',(#9700),#3601,.T.);
#70451=ADVANCED_FACE('',(#9701),#3602,.T.);
#70452=ADVANCED_FACE('',(#9702),#3603,.T.);
#70453=ADVANCED_FACE('',(#9703),#3604,.T.);
#70454=ADVANCED_FACE('',(#9704),#3605,.T.);
#70455=ADVANCED_FACE('',(#9705),#3606,.T.);
#70456=ADVANCED_FACE('',(#9706),#3607,.T.);
#70457=ADVANCED_FACE('',(#9707),#3608,.T.);
#70458=ADVANCED_FACE('',(#9708),#3609,.T.);
#70459=ADVANCED_FACE('',(#9709),#3610,.T.);
#70460=ADVANCED_FACE('',(#9710),#3611,.T.);
#70461=ADVANCED_FACE('',(#9711),#3612,.T.);
#70462=ADVANCED_FACE('',(#9712),#3613,.T.);
#70463=ADVANCED_FACE('',(#9713),#3614,.T.);
#70464=ADVANCED_FACE('',(#9714),#3615,.T.);
#70465=ADVANCED_FACE('',(#9715),#3616,.T.);
#70466=ADVANCED_FACE('',(#9716),#3617,.T.);
#70467=ADVANCED_FACE('',(#9717),#3618,.T.);
#70468=ADVANCED_FACE('',(#9718),#3619,.T.);
#70469=ADVANCED_FACE('',(#9719),#3620,.T.);
#70470=ADVANCED_FACE('',(#9720),#3621,.T.);
#70471=ADVANCED_FACE('',(#9721),#3622,.T.);
#70472=ADVANCED_FACE('',(#9722),#3623,.T.);
#70473=ADVANCED_FACE('',(#9723),#3624,.T.);
#70474=ADVANCED_FACE('',(#9724),#3625,.T.);
#70475=ADVANCED_FACE('',(#9725),#3626,.T.);
#70476=ADVANCED_FACE('',(#9726),#3627,.T.);
#70477=ADVANCED_FACE('',(#9727),#3628,.T.);
#70478=ADVANCED_FACE('',(#9728),#3629,.T.);
#70479=ADVANCED_FACE('',(#9729),#3630,.T.);
#70480=ADVANCED_FACE('',(#9730),#3631,.T.);
#70481=ADVANCED_FACE('',(#9731),#3632,.T.);
#70482=ADVANCED_FACE('',(#9732),#3633,.T.);
#70483=ADVANCED_FACE('',(#9733),#3634,.T.);
#70484=ADVANCED_FACE('',(#9734),#3635,.T.);
#70485=ADVANCED_FACE('',(#9735),#3636,.T.);
#70486=ADVANCED_FACE('',(#9736),#3637,.T.);
#70487=ADVANCED_FACE('',(#9737),#3638,.T.);
#70488=ADVANCED_FACE('',(#9738),#3639,.T.);
#70489=ADVANCED_FACE('',(#9739),#3640,.T.);
#70490=ADVANCED_FACE('',(#9740),#3641,.T.);
#70491=ADVANCED_FACE('',(#9741),#3642,.T.);
#70492=ADVANCED_FACE('',(#9742),#3643,.T.);
#70493=ADVANCED_FACE('',(#9743),#3644,.T.);
#70494=ADVANCED_FACE('',(#9744),#3645,.T.);
#70495=ADVANCED_FACE('',(#9745),#3646,.T.);
#70496=ADVANCED_FACE('',(#9746),#3647,.T.);
#70497=ADVANCED_FACE('',(#9747),#3648,.T.);
#70498=ADVANCED_FACE('',(#9748),#3649,.T.);
#70499=ADVANCED_FACE('',(#9749),#3650,.T.);
#70500=ADVANCED_FACE('',(#9750),#3651,.T.);
#70501=ADVANCED_FACE('',(#9751),#3652,.T.);
#70502=ADVANCED_FACE('',(#9752),#3653,.T.);
#70503=ADVANCED_FACE('',(#9753),#3654,.T.);
#70504=ADVANCED_FACE('',(#9754),#3655,.T.);
#70505=ADVANCED_FACE('',(#9755),#3656,.T.);
#70506=ADVANCED_FACE('',(#9756),#3657,.T.);
#70507=ADVANCED_FACE('',(#9757),#3658,.T.);
#70508=ADVANCED_FACE('',(#9758),#3659,.T.);
#70509=ADVANCED_FACE('',(#9759),#3660,.T.);
#70510=ADVANCED_FACE('',(#9760),#3661,.T.);
#70511=ADVANCED_FACE('',(#9761),#3662,.T.);
#70512=ADVANCED_FACE('',(#9762),#3663,.T.);
#70513=ADVANCED_FACE('',(#9763),#3664,.T.);
#70514=ADVANCED_FACE('',(#9764),#3665,.T.);
#70515=ADVANCED_FACE('',(#9765),#3666,.T.);
#70516=ADVANCED_FACE('',(#9766),#3667,.T.);
#70517=ADVANCED_FACE('',(#9767),#3668,.T.);
#70518=ADVANCED_FACE('',(#9768),#3669,.T.);
#70519=ADVANCED_FACE('',(#9769),#3670,.T.);
#70520=ADVANCED_FACE('',(#9770),#3671,.T.);
#70521=ADVANCED_FACE('',(#9771),#3672,.T.);
#70522=ADVANCED_FACE('',(#9772),#3673,.T.);
#70523=ADVANCED_FACE('',(#9773),#3674,.T.);
#70524=ADVANCED_FACE('',(#9774),#5305,.T.);
#70525=ADVANCED_FACE('',(#9775),#3675,.T.);
#70526=ADVANCED_FACE('',(#9776),#3676,.T.);
#70527=ADVANCED_FACE('',(#9777),#5306,.T.);
#70528=ADVANCED_FACE('',(#9778),#3677,.T.);
#70529=ADVANCED_FACE('',(#9779),#3678,.T.);
#70530=ADVANCED_FACE('',(#9780),#5307,.T.);
#70531=ADVANCED_FACE('',(#9781),#3679,.T.);
#70532=ADVANCED_FACE('',(#9782),#3680,.T.);
#70533=ADVANCED_FACE('',(#9783),#5308,.T.);
#70534=ADVANCED_FACE('',(#9784),#3681,.T.);
#70535=ADVANCED_FACE('',(#9785),#3682,.T.);
#70536=ADVANCED_FACE('',(#9786),#5309,.T.);
#70537=ADVANCED_FACE('',(#9787),#3683,.T.);
#70538=ADVANCED_FACE('',(#9788),#3684,.T.);
#70539=ADVANCED_FACE('',(#9789),#5310,.T.);
#70540=ADVANCED_FACE('',(#9790),#3685,.T.);
#70541=ADVANCED_FACE('',(#9791),#3686,.T.);
#70542=ADVANCED_FACE('',(#9792),#5311,.T.);
#70543=ADVANCED_FACE('',(#9793),#3687,.T.);
#70544=ADVANCED_FACE('',(#9794),#3688,.T.);
#70545=ADVANCED_FACE('',(#9795),#5312,.T.);
#70546=ADVANCED_FACE('',(#9796),#3689,.T.);
#70547=ADVANCED_FACE('',(#9797),#3690,.T.);
#70548=ADVANCED_FACE('',(#9798),#5313,.T.);
#70549=ADVANCED_FACE('',(#9799),#3691,.T.);
#70550=ADVANCED_FACE('',(#9800),#3692,.T.);
#70551=ADVANCED_FACE('',(#9801),#5314,.T.);
#70552=ADVANCED_FACE('',(#9802),#3693,.T.);
#70553=ADVANCED_FACE('',(#9803),#3694,.T.);
#70554=ADVANCED_FACE('',(#9804),#5315,.T.);
#70555=ADVANCED_FACE('',(#9805),#3695,.T.);
#70556=ADVANCED_FACE('',(#9806),#3696,.T.);
#70557=ADVANCED_FACE('',(#9807),#5316,.T.);
#70558=ADVANCED_FACE('',(#9808),#3697,.T.);
#70559=ADVANCED_FACE('',(#9809),#3698,.T.);
#70560=ADVANCED_FACE('',(#9810),#5317,.T.);
#70561=ADVANCED_FACE('',(#9811),#3699,.T.);
#70562=ADVANCED_FACE('',(#9812),#3700,.T.);
#70563=ADVANCED_FACE('',(#9813),#5318,.T.);
#70564=ADVANCED_FACE('',(#9814),#3701,.T.);
#70565=ADVANCED_FACE('',(#9815),#3702,.T.);
#70566=ADVANCED_FACE('',(#9816),#3703,.T.);
#70567=ADVANCED_FACE('',(#9817),#3704,.T.);
#70568=ADVANCED_FACE('',(#9818),#5319,.T.);
#70569=ADVANCED_FACE('',(#9819),#3705,.T.);
#70570=ADVANCED_FACE('',(#9820),#3706,.T.);
#70571=ADVANCED_FACE('',(#9821),#5320,.T.);
#70572=ADVANCED_FACE('',(#9822),#3707,.T.);
#70573=ADVANCED_FACE('',(#9823),#3708,.T.);
#70574=ADVANCED_FACE('',(#9824),#3709,.T.);
#70575=ADVANCED_FACE('',(#9825),#5321,.T.);
#70576=ADVANCED_FACE('',(#9826),#3710,.T.);
#70577=ADVANCED_FACE('',(#9827),#5322,.T.);
#70578=ADVANCED_FACE('',(#9828),#3711,.T.);
#70579=ADVANCED_FACE('',(#9829),#3712,.T.);
#70580=ADVANCED_FACE('',(#9830),#5323,.T.);
#70581=ADVANCED_FACE('',(#9831),#3713,.T.);
#70582=ADVANCED_FACE('',(#9832),#3714,.T.);
#70583=ADVANCED_FACE('',(#9833),#5324,.T.);
#70584=ADVANCED_FACE('',(#9834),#3715,.T.);
#70585=ADVANCED_FACE('',(#9835),#3716,.T.);
#70586=ADVANCED_FACE('',(#9836),#5325,.T.);
#70587=ADVANCED_FACE('',(#9837),#3717,.T.);
#70588=ADVANCED_FACE('',(#9838),#3718,.T.);
#70589=ADVANCED_FACE('',(#9839),#5326,.T.);
#70590=ADVANCED_FACE('',(#9840),#3719,.T.);
#70591=ADVANCED_FACE('',(#9841),#3720,.T.);
#70592=ADVANCED_FACE('',(#9842),#5327,.T.);
#70593=ADVANCED_FACE('',(#9843),#3721,.T.);
#70594=ADVANCED_FACE('',(#9844),#3722,.T.);
#70595=ADVANCED_FACE('',(#9845),#5328,.T.);
#70596=ADVANCED_FACE('',(#9846),#3723,.T.);
#70597=ADVANCED_FACE('',(#9847),#3724,.T.);
#70598=ADVANCED_FACE('',(#9848),#5329,.T.);
#70599=ADVANCED_FACE('',(#9849),#3725,.T.);
#70600=ADVANCED_FACE('',(#9850),#3726,.T.);
#70601=ADVANCED_FACE('',(#9851),#5330,.T.);
#70602=ADVANCED_FACE('',(#9852),#3727,.T.);
#70603=ADVANCED_FACE('',(#9853),#3728,.T.);
#70604=ADVANCED_FACE('',(#9854),#5331,.T.);
#70605=ADVANCED_FACE('',(#9855),#3729,.T.);
#70606=ADVANCED_FACE('',(#9856),#3730,.T.);
#70607=ADVANCED_FACE('',(#9857),#5332,.T.);
#70608=ADVANCED_FACE('',(#9858),#3731,.T.);
#70609=ADVANCED_FACE('',(#9859),#3732,.T.);
#70610=ADVANCED_FACE('',(#9860),#3733,.T.);
#70611=ADVANCED_FACE('',(#9861),#3734,.T.);
#70612=ADVANCED_FACE('',(#9862),#3735,.T.);
#70613=ADVANCED_FACE('',(#9863),#3736,.T.);
#70614=ADVANCED_FACE('',(#9864),#3737,.T.);
#70615=ADVANCED_FACE('',(#9865),#3738,.T.);
#70616=ADVANCED_FACE('',(#9866),#3739,.T.);
#70617=ADVANCED_FACE('',(#9867),#3740,.T.);
#70618=ADVANCED_FACE('',(#9868),#3741,.T.);
#70619=ADVANCED_FACE('',(#9869),#3742,.T.);
#70620=ADVANCED_FACE('',(#9870),#3743,.T.);
#70621=ADVANCED_FACE('',(#9871),#3744,.T.);
#70622=ADVANCED_FACE('',(#9872),#3745,.T.);
#70623=ADVANCED_FACE('',(#9873),#3746,.T.);
#70624=ADVANCED_FACE('',(#9874),#3747,.T.);
#70625=ADVANCED_FACE('',(#9875),#3748,.T.);
#70626=ADVANCED_FACE('',(#9876),#3749,.T.);
#70627=ADVANCED_FACE('',(#9877),#3750,.T.);
#70628=ADVANCED_FACE('',(#9878),#3751,.T.);
#70629=ADVANCED_FACE('',(#9879),#3752,.T.);
#70630=ADVANCED_FACE('',(#9880),#3753,.T.);
#70631=ADVANCED_FACE('',(#9881),#3754,.T.);
#70632=ADVANCED_FACE('',(#9882),#3755,.T.);
#70633=ADVANCED_FACE('',(#9883),#3756,.T.);
#70634=ADVANCED_FACE('',(#9884),#3757,.T.);
#70635=ADVANCED_FACE('',(#9885),#3758,.T.);
#70636=ADVANCED_FACE('',(#9886),#3759,.T.);
#70637=ADVANCED_FACE('',(#9887),#3760,.T.);
#70638=ADVANCED_FACE('',(#9888),#3761,.T.);
#70639=ADVANCED_FACE('',(#9889),#3762,.T.);
#70640=ADVANCED_FACE('',(#9890),#3763,.T.);
#70641=ADVANCED_FACE('',(#9891),#3764,.T.);
#70642=ADVANCED_FACE('',(#9892),#3765,.T.);
#70643=ADVANCED_FACE('',(#9893),#3766,.T.);
#70644=ADVANCED_FACE('',(#9894),#3767,.T.);
#70645=ADVANCED_FACE('',(#9895),#3768,.T.);
#70646=ADVANCED_FACE('',(#9896),#3769,.T.);
#70647=ADVANCED_FACE('',(#9897),#3770,.T.);
#70648=ADVANCED_FACE('',(#9898),#3771,.T.);
#70649=ADVANCED_FACE('',(#9899),#3772,.T.);
#70650=ADVANCED_FACE('',(#9900),#3773,.T.);
#70651=ADVANCED_FACE('',(#9901),#3774,.T.);
#70652=ADVANCED_FACE('',(#9902),#3775,.T.);
#70653=ADVANCED_FACE('',(#9903),#3776,.T.);
#70654=ADVANCED_FACE('',(#9904),#3777,.T.);
#70655=ADVANCED_FACE('',(#9905),#3778,.T.);
#70656=ADVANCED_FACE('',(#9906),#3779,.T.);
#70657=ADVANCED_FACE('',(#9907),#3780,.T.);
#70658=ADVANCED_FACE('',(#9908),#3781,.T.);
#70659=ADVANCED_FACE('',(#9909),#3782,.T.);
#70660=ADVANCED_FACE('',(#9910),#3783,.T.);
#70661=ADVANCED_FACE('',(#9911),#3784,.T.);
#70662=ADVANCED_FACE('',(#9912),#3785,.T.);
#70663=ADVANCED_FACE('',(#9913),#3786,.T.);
#70664=ADVANCED_FACE('',(#9914),#3787,.T.);
#70665=ADVANCED_FACE('',(#9915),#3788,.T.);
#70666=ADVANCED_FACE('',(#9916),#3789,.T.);
#70667=ADVANCED_FACE('',(#9917),#3790,.T.);
#70668=ADVANCED_FACE('',(#9918),#3791,.T.);
#70669=ADVANCED_FACE('',(#9919),#3792,.T.);
#70670=ADVANCED_FACE('',(#9920),#3793,.T.);
#70671=ADVANCED_FACE('',(#9921),#3794,.T.);
#70672=ADVANCED_FACE('',(#9922),#3795,.T.);
#70673=ADVANCED_FACE('',(#9923),#3796,.T.);
#70674=ADVANCED_FACE('',(#9924),#3797,.T.);
#70675=ADVANCED_FACE('',(#9925),#3798,.T.);
#70676=ADVANCED_FACE('',(#9926),#3799,.T.);
#70677=ADVANCED_FACE('',(#9927),#3800,.T.);
#70678=ADVANCED_FACE('',(#9928),#3801,.T.);
#70679=ADVANCED_FACE('',(#9929),#3802,.T.);
#70680=ADVANCED_FACE('',(#9930),#3803,.T.);
#70681=ADVANCED_FACE('',(#9931),#3804,.T.);
#70682=ADVANCED_FACE('',(#9932),#3805,.T.);
#70683=ADVANCED_FACE('',(#9933),#3806,.T.);
#70684=ADVANCED_FACE('',(#9934),#3807,.T.);
#70685=ADVANCED_FACE('',(#9935),#3808,.T.);
#70686=ADVANCED_FACE('',(#9936),#3809,.T.);
#70687=ADVANCED_FACE('',(#9937),#3810,.T.);
#70688=ADVANCED_FACE('',(#9938),#3811,.T.);
#70689=ADVANCED_FACE('',(#9939),#3812,.T.);
#70690=ADVANCED_FACE('',(#9940),#3813,.T.);
#70691=ADVANCED_FACE('',(#9941),#3814,.T.);
#70692=ADVANCED_FACE('',(#9942),#3815,.T.);
#70693=ADVANCED_FACE('',(#9943),#3816,.T.);
#70694=ADVANCED_FACE('',(#9944),#3817,.T.);
#70695=ADVANCED_FACE('',(#9945),#3818,.T.);
#70696=ADVANCED_FACE('',(#9946),#3819,.T.);
#70697=ADVANCED_FACE('',(#9947),#3820,.T.);
#70698=ADVANCED_FACE('',(#9948),#3821,.T.);
#70699=ADVANCED_FACE('',(#9949),#3822,.T.);
#70700=ADVANCED_FACE('',(#9950),#3823,.T.);
#70701=ADVANCED_FACE('',(#9951),#3824,.T.);
#70702=ADVANCED_FACE('',(#9952),#3825,.T.);
#70703=ADVANCED_FACE('',(#9953),#3826,.T.);
#70704=ADVANCED_FACE('',(#9954),#3827,.T.);
#70705=ADVANCED_FACE('',(#9955),#3828,.T.);
#70706=ADVANCED_FACE('',(#9956),#3829,.T.);
#70707=ADVANCED_FACE('',(#9957),#3830,.T.);
#70708=ADVANCED_FACE('',(#9958),#3831,.T.);
#70709=ADVANCED_FACE('',(#9959),#3832,.T.);
#70710=ADVANCED_FACE('',(#9960),#3833,.T.);
#70711=ADVANCED_FACE('',(#9961),#3834,.T.);
#70712=ADVANCED_FACE('',(#9962),#3835,.T.);
#70713=ADVANCED_FACE('',(#9963),#3836,.T.);
#70714=ADVANCED_FACE('',(#9964),#3837,.T.);
#70715=ADVANCED_FACE('',(#9965),#3838,.T.);
#70716=ADVANCED_FACE('',(#9966),#3839,.T.);
#70717=ADVANCED_FACE('',(#9967),#3840,.T.);
#70718=ADVANCED_FACE('',(#9968),#3841,.T.);
#70719=ADVANCED_FACE('',(#9969),#3842,.T.);
#70720=ADVANCED_FACE('',(#9970),#3843,.T.);
#70721=ADVANCED_FACE('',(#9971),#3844,.T.);
#70722=ADVANCED_FACE('',(#9972),#3845,.T.);
#70723=ADVANCED_FACE('',(#9973),#3846,.T.);
#70724=ADVANCED_FACE('',(#9974),#3847,.T.);
#70725=ADVANCED_FACE('',(#9975),#3848,.T.);
#70726=ADVANCED_FACE('',(#9976),#3849,.T.);
#70727=ADVANCED_FACE('',(#9977),#3850,.T.);
#70728=ADVANCED_FACE('',(#9978),#3851,.T.);
#70729=ADVANCED_FACE('',(#9979),#3852,.T.);
#70730=ADVANCED_FACE('',(#9980),#3853,.T.);
#70731=ADVANCED_FACE('',(#9981),#3854,.T.);
#70732=ADVANCED_FACE('',(#9982),#3855,.T.);
#70733=ADVANCED_FACE('',(#9983),#3856,.T.);
#70734=ADVANCED_FACE('',(#9984),#3857,.T.);
#70735=ADVANCED_FACE('',(#9985),#3858,.T.);
#70736=ADVANCED_FACE('',(#9986),#3859,.T.);
#70737=ADVANCED_FACE('',(#9987),#3860,.T.);
#70738=ADVANCED_FACE('',(#9988),#3861,.T.);
#70739=ADVANCED_FACE('',(#9989),#3862,.T.);
#70740=ADVANCED_FACE('',(#9990),#3863,.T.);
#70741=ADVANCED_FACE('',(#9991),#3864,.T.);
#70742=ADVANCED_FACE('',(#9992),#3865,.T.);
#70743=ADVANCED_FACE('',(#9993),#3866,.T.);
#70744=ADVANCED_FACE('',(#9994),#3867,.T.);
#70745=ADVANCED_FACE('',(#9995),#3868,.T.);
#70746=ADVANCED_FACE('',(#9996),#3869,.T.);
#70747=ADVANCED_FACE('',(#9997),#3870,.T.);
#70748=ADVANCED_FACE('',(#9998),#3871,.T.);
#70749=ADVANCED_FACE('',(#9999),#3872,.T.);
#70750=ADVANCED_FACE('',(#10000),#3873,.T.);
#70751=ADVANCED_FACE('',(#10001),#3874,.T.);
#70752=ADVANCED_FACE('',(#10002),#3875,.T.);
#70753=ADVANCED_FACE('',(#10003),#3876,.T.);
#70754=ADVANCED_FACE('',(#10004),#3877,.T.);
#70755=ADVANCED_FACE('',(#10005),#3878,.T.);
#70756=ADVANCED_FACE('',(#10006),#3879,.T.);
#70757=ADVANCED_FACE('',(#10007),#3880,.T.);
#70758=ADVANCED_FACE('',(#10008),#3881,.T.);
#70759=ADVANCED_FACE('',(#10009),#3882,.T.);
#70760=ADVANCED_FACE('',(#10010),#3883,.T.);
#70761=ADVANCED_FACE('',(#10011),#3884,.T.);
#70762=ADVANCED_FACE('',(#10012),#3885,.T.);
#70763=ADVANCED_FACE('',(#10013),#3886,.T.);
#70764=ADVANCED_FACE('',(#10014),#3887,.T.);
#70765=ADVANCED_FACE('',(#10015),#3888,.T.);
#70766=ADVANCED_FACE('',(#10016),#3889,.T.);
#70767=ADVANCED_FACE('',(#10017),#3890,.T.);
#70768=ADVANCED_FACE('',(#10018),#3891,.T.);
#70769=ADVANCED_FACE('',(#10019),#3892,.T.);
#70770=ADVANCED_FACE('',(#10020),#3893,.T.);
#70771=ADVANCED_FACE('',(#10021),#3894,.T.);
#70772=ADVANCED_FACE('',(#10022),#3895,.T.);
#70773=ADVANCED_FACE('',(#10023),#3896,.T.);
#70774=ADVANCED_FACE('',(#10024),#3897,.T.);
#70775=ADVANCED_FACE('',(#10025),#3898,.T.);
#70776=ADVANCED_FACE('',(#10026),#3899,.T.);
#70777=ADVANCED_FACE('',(#10027),#3900,.T.);
#70778=ADVANCED_FACE('',(#10028),#3901,.T.);
#70779=ADVANCED_FACE('',(#10029),#3902,.T.);
#70780=ADVANCED_FACE('',(#10030),#3903,.T.);
#70781=ADVANCED_FACE('',(#10031),#3904,.T.);
#70782=ADVANCED_FACE('',(#10032),#3905,.T.);
#70783=ADVANCED_FACE('',(#10033),#3906,.T.);
#70784=ADVANCED_FACE('',(#10034),#3907,.T.);
#70785=ADVANCED_FACE('',(#10035),#3908,.T.);
#70786=ADVANCED_FACE('',(#10036),#3909,.T.);
#70787=ADVANCED_FACE('',(#10037),#3910,.T.);
#70788=ADVANCED_FACE('',(#10038),#3911,.T.);
#70789=ADVANCED_FACE('',(#10039),#3912,.T.);
#70790=ADVANCED_FACE('',(#10040),#3913,.T.);
#70791=ADVANCED_FACE('',(#10041),#3914,.T.);
#70792=ADVANCED_FACE('',(#10042),#3915,.T.);
#70793=ADVANCED_FACE('',(#10043),#3916,.T.);
#70794=ADVANCED_FACE('',(#10044),#3917,.T.);
#70795=ADVANCED_FACE('',(#10045),#3918,.T.);
#70796=ADVANCED_FACE('',(#10046),#3919,.T.);
#70797=ADVANCED_FACE('',(#10047),#3920,.T.);
#70798=ADVANCED_FACE('',(#10048),#3921,.T.);
#70799=ADVANCED_FACE('',(#10049),#3922,.T.);
#70800=ADVANCED_FACE('',(#10050),#3923,.T.);
#70801=ADVANCED_FACE('',(#10051),#3924,.T.);
#70802=ADVANCED_FACE('',(#10052),#3925,.T.);
#70803=ADVANCED_FACE('',(#10053),#3926,.T.);
#70804=ADVANCED_FACE('',(#10054),#3927,.T.);
#70805=ADVANCED_FACE('',(#10055),#3928,.T.);
#70806=ADVANCED_FACE('',(#10056),#3929,.T.);
#70807=ADVANCED_FACE('',(#10057),#3930,.T.);
#70808=ADVANCED_FACE('',(#10058),#3931,.T.);
#70809=ADVANCED_FACE('',(#10059),#3932,.T.);
#70810=ADVANCED_FACE('',(#10060),#3933,.T.);
#70811=ADVANCED_FACE('',(#10061),#3934,.T.);
#70812=ADVANCED_FACE('',(#10062),#3935,.T.);
#70813=ADVANCED_FACE('',(#10063),#3936,.T.);
#70814=ADVANCED_FACE('',(#10064),#3937,.T.);
#70815=ADVANCED_FACE('',(#10065),#3938,.T.);
#70816=ADVANCED_FACE('',(#10066),#3939,.T.);
#70817=ADVANCED_FACE('',(#10067),#3940,.T.);
#70818=ADVANCED_FACE('',(#10068),#3941,.T.);
#70819=ADVANCED_FACE('',(#10069),#3942,.T.);
#70820=ADVANCED_FACE('',(#10070),#3943,.T.);
#70821=ADVANCED_FACE('',(#10071),#3944,.T.);
#70822=ADVANCED_FACE('',(#10072),#3945,.T.);
#70823=ADVANCED_FACE('',(#10073),#3946,.T.);
#70824=ADVANCED_FACE('',(#10074),#3947,.T.);
#70825=ADVANCED_FACE('',(#10075),#3948,.T.);
#70826=ADVANCED_FACE('',(#10076),#3949,.T.);
#70827=ADVANCED_FACE('',(#10077),#3950,.T.);
#70828=ADVANCED_FACE('',(#10078),#3951,.T.);
#70829=ADVANCED_FACE('',(#10079),#3952,.T.);
#70830=ADVANCED_FACE('',(#10080),#3953,.T.);
#70831=ADVANCED_FACE('',(#10081),#3954,.T.);
#70832=ADVANCED_FACE('',(#10082),#3955,.T.);
#70833=ADVANCED_FACE('',(#10083),#3956,.T.);
#70834=ADVANCED_FACE('',(#10084),#3957,.T.);
#70835=ADVANCED_FACE('',(#10085),#3958,.T.);
#70836=ADVANCED_FACE('',(#10086),#3959,.T.);
#70837=ADVANCED_FACE('',(#10087),#3960,.T.);
#70838=ADVANCED_FACE('',(#10088),#3961,.T.);
#70839=ADVANCED_FACE('',(#10089),#3962,.T.);
#70840=ADVANCED_FACE('',(#10090),#3963,.T.);
#70841=ADVANCED_FACE('',(#10091),#3964,.T.);
#70842=ADVANCED_FACE('',(#10092),#3965,.T.);
#70843=ADVANCED_FACE('',(#10093),#66068,.T.);
#70844=ADVANCED_FACE('',(#10094),#3966,.T.);
#70845=ADVANCED_FACE('',(#10095),#5333,.T.);
#70846=ADVANCED_FACE('',(#10096),#3967,.T.);
#70847=ADVANCED_FACE('',(#10097),#66069,.T.);
#70848=ADVANCED_FACE('',(#10098),#3968,.T.);
#70849=ADVANCED_FACE('',(#10099),#5334,.T.);
#70850=ADVANCED_FACE('',(#10100),#3969,.T.);
#70851=ADVANCED_FACE('',(#10101),#66070,.T.);
#70852=ADVANCED_FACE('',(#10102),#3970,.T.);
#70853=ADVANCED_FACE('',(#10103),#5335,.T.);
#70854=ADVANCED_FACE('',(#10104),#3971,.T.);
#70855=ADVANCED_FACE('',(#10105),#66071,.T.);
#70856=ADVANCED_FACE('',(#10106),#3972,.T.);
#70857=ADVANCED_FACE('',(#10107),#5336,.T.);
#70858=ADVANCED_FACE('',(#10108),#3973,.T.);
#70859=ADVANCED_FACE('',(#10109),#66072,.T.);
#70860=ADVANCED_FACE('',(#10110),#3974,.T.);
#70861=ADVANCED_FACE('',(#10111),#5337,.T.);
#70862=ADVANCED_FACE('',(#10112),#3975,.T.);
#70863=ADVANCED_FACE('',(#10113),#66073,.T.);
#70864=ADVANCED_FACE('',(#10114),#3976,.T.);
#70865=ADVANCED_FACE('',(#10115),#5338,.T.);
#70866=ADVANCED_FACE('',(#10116),#3977,.T.);
#70867=ADVANCED_FACE('',(#10117),#66074,.T.);
#70868=ADVANCED_FACE('',(#10118),#3978,.T.);
#70869=ADVANCED_FACE('',(#10119),#3979,.T.);
#70870=ADVANCED_FACE('',(#10120),#66075,.T.);
#70871=ADVANCED_FACE('',(#10121),#3980,.T.);
#70872=ADVANCED_FACE('',(#10122),#5339,.T.);
#70873=ADVANCED_FACE('',(#10123),#3981,.T.);
#70874=ADVANCED_FACE('',(#10124),#66076,.T.);
#70875=ADVANCED_FACE('',(#10125),#3982,.T.);
#70876=ADVANCED_FACE('',(#10126),#5340,.T.);
#70877=ADVANCED_FACE('',(#10127),#3983,.T.);
#70878=ADVANCED_FACE('',(#10128),#66077,.T.);
#70879=ADVANCED_FACE('',(#10129),#3984,.T.);
#70880=ADVANCED_FACE('',(#10130),#5341,.T.);
#70881=ADVANCED_FACE('',(#10131),#3985,.T.);
#70882=ADVANCED_FACE('',(#10132),#66078,.T.);
#70883=ADVANCED_FACE('',(#10133),#3986,.T.);
#70884=ADVANCED_FACE('',(#10134),#5342,.T.);
#70885=ADVANCED_FACE('',(#10135),#3987,.T.);
#70886=ADVANCED_FACE('',(#10136),#66079,.T.);
#70887=ADVANCED_FACE('',(#10137),#3988,.T.);
#70888=ADVANCED_FACE('',(#10138),#5343,.T.);
#70889=ADVANCED_FACE('',(#10139),#3989,.T.);
#70890=ADVANCED_FACE('',(#10140),#66080,.T.);
#70891=ADVANCED_FACE('',(#10141),#3990,.T.);
#70892=ADVANCED_FACE('',(#10142),#5344,.T.);
#70893=ADVANCED_FACE('',(#10143),#3991,.T.);
#70894=ADVANCED_FACE('',(#10144),#66081,.T.);
#70895=ADVANCED_FACE('',(#10145),#3992,.T.);
#70896=ADVANCED_FACE('',(#10146),#5345,.T.);
#70897=ADVANCED_FACE('',(#10147),#3993,.T.);
#70898=ADVANCED_FACE('',(#10148),#66082,.T.);
#70899=ADVANCED_FACE('',(#10149),#3994,.T.);
#70900=ADVANCED_FACE('',(#10150),#5346,.T.);
#70901=ADVANCED_FACE('',(#10151),#3995,.T.);
#70902=ADVANCED_FACE('',(#10152),#66083,.T.);
#70903=ADVANCED_FACE('',(#10153),#3996,.T.);
#70904=ADVANCED_FACE('',(#10154),#5347,.T.);
#70905=ADVANCED_FACE('',(#10155),#3997,.T.);
#70906=ADVANCED_FACE('',(#10156),#66084,.T.);
#70907=ADVANCED_FACE('',(#10157),#3998,.T.);
#70908=ADVANCED_FACE('',(#10158),#5348,.T.);
#70909=ADVANCED_FACE('',(#10159),#3999,.T.);
#70910=ADVANCED_FACE('',(#10160),#66085,.T.);
#70911=ADVANCED_FACE('',(#10161),#4000,.T.);
#70912=ADVANCED_FACE('',(#10162),#5349,.T.);
#70913=ADVANCED_FACE('',(#10163),#4001,.T.);
#70914=ADVANCED_FACE('',(#10164),#66086,.T.);
#70915=ADVANCED_FACE('',(#10165),#4002,.T.);
#70916=ADVANCED_FACE('',(#10166),#5350,.T.);
#70917=ADVANCED_FACE('',(#10167),#4003,.T.);
#70918=ADVANCED_FACE('',(#10168),#66087,.T.);
#70919=ADVANCED_FACE('',(#10169),#4004,.T.);
#70920=ADVANCED_FACE('',(#10170),#5351,.T.);
#70921=ADVANCED_FACE('',(#10171),#4005,.T.);
#70922=ADVANCED_FACE('',(#10172),#66088,.T.);
#70923=ADVANCED_FACE('',(#10173),#4006,.T.);
#70924=ADVANCED_FACE('',(#10174),#5352,.T.);
#70925=ADVANCED_FACE('',(#10175),#4007,.T.);
#70926=ADVANCED_FACE('',(#10176),#66089,.T.);
#70927=ADVANCED_FACE('',(#10177),#4008,.T.);
#70928=ADVANCED_FACE('',(#10178),#5353,.T.);
#70929=ADVANCED_FACE('',(#10179),#4009,.T.);
#70930=ADVANCED_FACE('',(#10180),#66090,.T.);
#70931=ADVANCED_FACE('',(#10181),#4010,.T.);
#70932=ADVANCED_FACE('',(#10182),#5354,.T.);
#70933=ADVANCED_FACE('',(#10183),#4011,.T.);
#70934=ADVANCED_FACE('',(#10184),#66091,.T.);
#70935=ADVANCED_FACE('',(#10185),#4012,.T.);
#70936=ADVANCED_FACE('',(#10186),#5355,.T.);
#70937=ADVANCED_FACE('',(#10187),#4013,.T.);
#70938=ADVANCED_FACE('',(#10188),#66092,.T.);
#70939=ADVANCED_FACE('',(#10189),#4014,.T.);
#70940=ADVANCED_FACE('',(#10190),#5356,.T.);
#70941=ADVANCED_FACE('',(#10191),#4015,.T.);
#70942=ADVANCED_FACE('',(#10192),#66093,.T.);
#70943=ADVANCED_FACE('',(#10193),#4016,.T.);
#70944=ADVANCED_FACE('',(#10194),#5357,.T.);
#70945=ADVANCED_FACE('',(#10195),#4017,.T.);
#70946=ADVANCED_FACE('',(#10196),#66094,.T.);
#70947=ADVANCED_FACE('',(#10197),#4018,.T.);
#70948=ADVANCED_FACE('',(#10198),#5358,.T.);
#70949=ADVANCED_FACE('',(#10199),#4019,.T.);
#70950=ADVANCED_FACE('',(#10200),#66095,.T.);
#70951=ADVANCED_FACE('',(#10201),#4020,.T.);
#70952=ADVANCED_FACE('',(#10202),#5359,.T.);
#70953=ADVANCED_FACE('',(#10203),#66096,.T.);
#70954=ADVANCED_FACE('',(#10204),#5360,.T.);
#70955=ADVANCED_FACE('',(#10205),#4021,.T.);
#70956=ADVANCED_FACE('',(#10206,#70),#86,.T.);
#70957=ADVANCED_FACE('',(#10207),#4022,.T.);
#70958=ADVANCED_FACE('',(#10208),#4023,.T.);
#70959=ADVANCED_FACE('',(#10209),#4024,.T.);
#70960=ADVANCED_FACE('',(#10210),#4025,.T.);
#70961=ADVANCED_FACE('',(#10211),#4026,.T.);
#70962=ADVANCED_FACE('',(#10212),#4027,.T.);
#70963=ADVANCED_FACE('',(#10213),#4028,.T.);
#70964=ADVANCED_FACE('',(#10214),#4029,.T.);
#70965=ADVANCED_FACE('',(#10215),#4030,.T.);
#70966=ADVANCED_FACE('',(#10216),#4031,.T.);
#70967=ADVANCED_FACE('',(#10217),#4032,.T.);
#70968=ADVANCED_FACE('',(#10218),#4033,.T.);
#70969=ADVANCED_FACE('',(#10219),#4034,.T.);
#70970=ADVANCED_FACE('',(#10220),#4035,.T.);
#70971=ADVANCED_FACE('',(#10221),#4036,.T.);
#70972=ADVANCED_FACE('',(#10222),#4037,.T.);
#70973=ADVANCED_FACE('',(#10223),#4038,.T.);
#70974=ADVANCED_FACE('',(#10224),#4039,.T.);
#70975=ADVANCED_FACE('',(#10225),#4040,.T.);
#70976=ADVANCED_FACE('',(#10226),#4041,.T.);
#70977=ADVANCED_FACE('',(#10227),#4042,.T.);
#70978=ADVANCED_FACE('',(#10228),#4043,.T.);
#70979=ADVANCED_FACE('',(#10229),#4044,.T.);
#70980=ADVANCED_FACE('',(#10230),#4045,.T.);
#70981=ADVANCED_FACE('',(#10231),#4046,.T.);
#70982=ADVANCED_FACE('',(#10232),#4047,.T.);
#70983=ADVANCED_FACE('',(#10233),#4048,.T.);
#70984=ADVANCED_FACE('',(#10234),#4049,.T.);
#70985=ADVANCED_FACE('',(#10235),#4050,.T.);
#70986=ADVANCED_FACE('',(#10236),#4051,.T.);
#70987=ADVANCED_FACE('',(#10237),#4052,.T.);
#70988=ADVANCED_FACE('',(#10238),#4053,.T.);
#70989=ADVANCED_FACE('',(#10239),#4054,.T.);
#70990=ADVANCED_FACE('',(#10240),#4055,.T.);
#70991=ADVANCED_FACE('',(#10241),#4056,.T.);
#70992=ADVANCED_FACE('',(#10242),#4057,.T.);
#70993=ADVANCED_FACE('',(#10243),#4058,.T.);
#70994=ADVANCED_FACE('',(#10244),#4059,.T.);
#70995=ADVANCED_FACE('',(#10245),#4060,.T.);
#70996=ADVANCED_FACE('',(#10246),#4061,.T.);
#70997=ADVANCED_FACE('',(#10247),#4062,.T.);
#70998=ADVANCED_FACE('',(#10248),#4063,.T.);
#70999=ADVANCED_FACE('',(#10249),#4064,.T.);
#71000=ADVANCED_FACE('',(#10250),#4065,.T.);
#71001=ADVANCED_FACE('',(#10251),#4066,.T.);
#71002=ADVANCED_FACE('',(#10252),#4067,.T.);
#71003=ADVANCED_FACE('',(#10253),#4068,.T.);
#71004=ADVANCED_FACE('',(#10254),#4069,.T.);
#71005=ADVANCED_FACE('',(#10255),#4070,.T.);
#71006=ADVANCED_FACE('',(#10256),#4071,.T.);
#71007=ADVANCED_FACE('',(#10257),#4072,.T.);
#71008=ADVANCED_FACE('',(#10258),#4073,.T.);
#71009=ADVANCED_FACE('',(#10259),#4074,.T.);
#71010=ADVANCED_FACE('',(#10260),#4075,.T.);
#71011=ADVANCED_FACE('',(#10261),#4076,.T.);
#71012=ADVANCED_FACE('',(#10262),#4077,.T.);
#71013=ADVANCED_FACE('',(#10263),#4078,.T.);
#71014=ADVANCED_FACE('',(#10264),#4079,.T.);
#71015=ADVANCED_FACE('',(#10265),#4080,.T.);
#71016=ADVANCED_FACE('',(#10266),#66097,.T.);
#71017=ADVANCED_FACE('',(#10267),#4081,.T.);
#71018=ADVANCED_FACE('',(#10268),#4082,.T.);
#71019=ADVANCED_FACE('',(#10269),#66098,.T.);
#71020=ADVANCED_FACE('',(#10270),#4083,.T.);
#71021=ADVANCED_FACE('',(#10271),#4084,.T.);
#71022=ADVANCED_FACE('',(#10272),#66099,.T.);
#71023=ADVANCED_FACE('',(#10273),#4085,.T.);
#71024=ADVANCED_FACE('',(#10274),#4086,.T.);
#71025=ADVANCED_FACE('',(#10275),#66100,.T.);
#71026=ADVANCED_FACE('',(#10276),#4087,.T.);
#71027=ADVANCED_FACE('',(#10277),#4088,.T.);
#71028=ADVANCED_FACE('',(#10278),#66101,.T.);
#71029=ADVANCED_FACE('',(#10279),#4089,.T.);
#71030=ADVANCED_FACE('',(#10280),#4090,.T.);
#71031=ADVANCED_FACE('',(#10281),#66102,.T.);
#71032=ADVANCED_FACE('',(#10282),#4091,.T.);
#71033=ADVANCED_FACE('',(#10283),#4092,.T.);
#71034=ADVANCED_FACE('',(#10284),#66103,.T.);
#71035=ADVANCED_FACE('',(#10285),#4093,.T.);
#71036=ADVANCED_FACE('',(#10286),#4094,.T.);
#71037=ADVANCED_FACE('',(#10287),#66104,.T.);
#71038=ADVANCED_FACE('',(#10288),#4095,.T.);
#71039=ADVANCED_FACE('',(#10289),#4096,.T.);
#71040=ADVANCED_FACE('',(#10290),#66105,.T.);
#71041=ADVANCED_FACE('',(#10291),#4097,.T.);
#71042=ADVANCED_FACE('',(#10292),#4098,.T.);
#71043=ADVANCED_FACE('',(#10293),#66106,.T.);
#71044=ADVANCED_FACE('',(#10294),#4099,.T.);
#71045=ADVANCED_FACE('',(#10295),#4100,.T.);
#71046=ADVANCED_FACE('',(#10296),#66107,.T.);
#71047=ADVANCED_FACE('',(#10297),#4101,.T.);
#71048=ADVANCED_FACE('',(#10298),#4102,.T.);
#71049=ADVANCED_FACE('',(#10299),#66108,.T.);
#71050=ADVANCED_FACE('',(#10300),#4103,.T.);
#71051=ADVANCED_FACE('',(#10301),#4104,.T.);
#71052=ADVANCED_FACE('',(#10302),#66109,.T.);
#71053=ADVANCED_FACE('',(#10303),#4105,.T.);
#71054=ADVANCED_FACE('',(#10304),#4106,.T.);
#71055=ADVANCED_FACE('',(#10305),#66110,.T.);
#71056=ADVANCED_FACE('',(#10306),#4107,.T.);
#71057=ADVANCED_FACE('',(#10307),#4108,.T.);
#71058=ADVANCED_FACE('',(#10308),#66111,.T.);
#71059=ADVANCED_FACE('',(#10309),#4109,.T.);
#71060=ADVANCED_FACE('',(#10310),#4110,.T.);
#71061=ADVANCED_FACE('',(#10311),#66112,.T.);
#71062=ADVANCED_FACE('',(#10312),#4111,.T.);
#71063=ADVANCED_FACE('',(#10313),#4112,.T.);
#71064=ADVANCED_FACE('',(#10314),#66113,.T.);
#71065=ADVANCED_FACE('',(#10315),#4113,.T.);
#71066=ADVANCED_FACE('',(#10316),#4114,.T.);
#71067=ADVANCED_FACE('',(#10317),#66114,.T.);
#71068=ADVANCED_FACE('',(#10318),#4115,.T.);
#71069=ADVANCED_FACE('',(#10319),#4116,.T.);
#71070=ADVANCED_FACE('',(#10320),#66115,.T.);
#71071=ADVANCED_FACE('',(#10321),#4117,.T.);
#71072=ADVANCED_FACE('',(#10322),#4118,.T.);
#71073=ADVANCED_FACE('',(#10323),#66116,.T.);
#71074=ADVANCED_FACE('',(#10324),#4119,.T.);
#71075=ADVANCED_FACE('',(#10325),#4120,.T.);
#71076=ADVANCED_FACE('',(#10326),#66117,.T.);
#71077=ADVANCED_FACE('',(#10327),#4121,.T.);
#71078=ADVANCED_FACE('',(#10328),#4122,.T.);
#71079=ADVANCED_FACE('',(#10329),#4123,.T.);
#71080=ADVANCED_FACE('',(#10330),#4124,.T.);
#71081=ADVANCED_FACE('',(#10331),#66118,.T.);
#71082=ADVANCED_FACE('',(#10332),#4125,.T.);
#71083=ADVANCED_FACE('',(#10333),#4126,.T.);
#71084=ADVANCED_FACE('',(#10334),#66119,.T.);
#71085=ADVANCED_FACE('',(#10335),#4127,.T.);
#71086=ADVANCED_FACE('',(#10336),#4128,.T.);
#71087=ADVANCED_FACE('',(#10337),#66120,.T.);
#71088=ADVANCED_FACE('',(#10338),#4129,.T.);
#71089=ADVANCED_FACE('',(#10339),#4130,.T.);
#71090=ADVANCED_FACE('',(#10340),#66121,.T.);
#71091=ADVANCED_FACE('',(#10341),#4131,.T.);
#71092=ADVANCED_FACE('',(#10342),#4132,.T.);
#71093=ADVANCED_FACE('',(#10343),#66122,.T.);
#71094=ADVANCED_FACE('',(#10344),#4133,.T.);
#71095=ADVANCED_FACE('',(#10345),#4134,.T.);
#71096=ADVANCED_FACE('',(#10346),#66123,.T.);
#71097=ADVANCED_FACE('',(#10347),#4135,.T.);
#71098=ADVANCED_FACE('',(#10348),#4136,.T.);
#71099=ADVANCED_FACE('',(#10349),#4137,.T.);
#71100=ADVANCED_FACE('',(#10350),#4138,.T.);
#71101=ADVANCED_FACE('',(#10351),#4139,.T.);
#71102=ADVANCED_FACE('',(#10352),#4140,.T.);
#71103=ADVANCED_FACE('',(#10353),#4141,.T.);
#71104=ADVANCED_FACE('',(#10354),#4142,.T.);
#71105=ADVANCED_FACE('',(#10355),#4143,.T.);
#71106=ADVANCED_FACE('',(#10356),#4144,.T.);
#71107=ADVANCED_FACE('',(#10357),#4145,.T.);
#71108=ADVANCED_FACE('',(#10358),#4146,.T.);
#71109=ADVANCED_FACE('',(#10359),#4147,.T.);
#71110=ADVANCED_FACE('',(#10360),#4148,.T.);
#71111=ADVANCED_FACE('',(#10361),#4149,.T.);
#71112=ADVANCED_FACE('',(#10362),#4150,.T.);
#71113=ADVANCED_FACE('',(#10363),#4151,.T.);
#71114=ADVANCED_FACE('',(#10364),#4152,.T.);
#71115=ADVANCED_FACE('',(#10365),#4153,.T.);
#71116=ADVANCED_FACE('',(#10366),#4154,.T.);
#71117=ADVANCED_FACE('',(#10367),#4155,.T.);
#71118=ADVANCED_FACE('',(#10368),#4156,.T.);
#71119=ADVANCED_FACE('',(#10369),#4157,.T.);
#71120=ADVANCED_FACE('',(#10370),#4158,.T.);
#71121=ADVANCED_FACE('',(#10371),#4159,.T.);
#71122=ADVANCED_FACE('',(#10372),#4160,.T.);
#71123=ADVANCED_FACE('',(#10373),#4161,.T.);
#71124=ADVANCED_FACE('',(#10374),#4162,.T.);
#71125=ADVANCED_FACE('',(#10375),#4163,.T.);
#71126=ADVANCED_FACE('',(#10376),#4164,.T.);
#71127=ADVANCED_FACE('',(#10377),#4165,.T.);
#71128=ADVANCED_FACE('',(#10378),#4166,.T.);
#71129=ADVANCED_FACE('',(#10379),#4167,.T.);
#71130=ADVANCED_FACE('',(#10380),#4168,.T.);
#71131=ADVANCED_FACE('',(#10381),#4169,.T.);
#71132=ADVANCED_FACE('',(#10382),#4170,.T.);
#71133=ADVANCED_FACE('',(#10383),#4171,.T.);
#71134=ADVANCED_FACE('',(#10384),#4172,.T.);
#71135=ADVANCED_FACE('',(#10385),#4173,.T.);
#71136=ADVANCED_FACE('',(#10386),#4174,.T.);
#71137=ADVANCED_FACE('',(#10387),#4175,.T.);
#71138=ADVANCED_FACE('',(#10388),#4176,.T.);
#71139=ADVANCED_FACE('',(#10389),#4177,.T.);
#71140=ADVANCED_FACE('',(#10390),#4178,.T.);
#71141=ADVANCED_FACE('',(#10391),#4179,.T.);
#71142=ADVANCED_FACE('',(#10392),#4180,.T.);
#71143=ADVANCED_FACE('',(#10393),#4181,.T.);
#71144=ADVANCED_FACE('',(#10394),#4182,.T.);
#71145=ADVANCED_FACE('',(#10395),#4183,.T.);
#71146=ADVANCED_FACE('',(#10396),#4184,.T.);
#71147=ADVANCED_FACE('',(#10397),#4185,.T.);
#71148=ADVANCED_FACE('',(#10398),#4186,.T.);
#71149=ADVANCED_FACE('',(#10399),#4187,.T.);
#71150=ADVANCED_FACE('',(#10400),#4188,.T.);
#71151=ADVANCED_FACE('',(#10401),#4189,.T.);
#71152=ADVANCED_FACE('',(#10402),#4190,.T.);
#71153=ADVANCED_FACE('',(#10403),#4191,.T.);
#71154=ADVANCED_FACE('',(#10404),#4192,.T.);
#71155=ADVANCED_FACE('',(#10405),#4193,.T.);
#71156=ADVANCED_FACE('',(#10406),#4194,.T.);
#71157=ADVANCED_FACE('',(#10407),#4195,.T.);
#71158=ADVANCED_FACE('',(#10408,#71),#87,.T.);
#71159=ADVANCED_FACE('',(#10409),#4196,.T.);
#71160=ADVANCED_FACE('',(#10410),#4197,.T.);
#71161=ADVANCED_FACE('',(#10411),#4198,.T.);
#71162=ADVANCED_FACE('',(#10412),#4199,.T.);
#71163=ADVANCED_FACE('',(#10413),#4200,.T.);
#71164=ADVANCED_FACE('',(#10414),#4201,.T.);
#71165=ADVANCED_FACE('',(#10415),#4202,.T.);
#71166=ADVANCED_FACE('',(#10416),#4203,.T.);
#71167=ADVANCED_FACE('',(#10417),#4204,.T.);
#71168=ADVANCED_FACE('',(#10418),#4205,.T.);
#71169=ADVANCED_FACE('',(#10419),#4206,.T.);
#71170=ADVANCED_FACE('',(#10420),#4207,.T.);
#71171=ADVANCED_FACE('',(#10421),#4208,.T.);
#71172=ADVANCED_FACE('',(#10422),#4209,.T.);
#71173=ADVANCED_FACE('',(#10423),#4210,.T.);
#71174=ADVANCED_FACE('',(#10424),#4211,.T.);
#71175=ADVANCED_FACE('',(#10425),#4212,.T.);
#71176=ADVANCED_FACE('',(#10426),#4213,.T.);
#71177=ADVANCED_FACE('',(#10427),#4214,.T.);
#71178=ADVANCED_FACE('',(#10428),#4215,.T.);
#71179=ADVANCED_FACE('',(#10429),#4216,.T.);
#71180=ADVANCED_FACE('',(#10430),#4217,.T.);
#71181=ADVANCED_FACE('',(#10431),#4218,.T.);
#71182=ADVANCED_FACE('',(#10432),#4219,.T.);
#71183=ADVANCED_FACE('',(#10433),#4220,.T.);
#71184=ADVANCED_FACE('',(#10434),#4221,.T.);
#71185=ADVANCED_FACE('',(#10435),#4222,.T.);
#71186=ADVANCED_FACE('',(#10436),#4223,.T.);
#71187=ADVANCED_FACE('',(#10437),#4224,.T.);
#71188=ADVANCED_FACE('',(#10438),#4225,.T.);
#71189=ADVANCED_FACE('',(#10439),#4226,.T.);
#71190=ADVANCED_FACE('',(#10440),#4227,.T.);
#71191=ADVANCED_FACE('',(#10441),#4228,.T.);
#71192=ADVANCED_FACE('',(#10442),#4229,.T.);
#71193=ADVANCED_FACE('',(#10443),#4230,.T.);
#71194=ADVANCED_FACE('',(#10444),#4231,.T.);
#71195=ADVANCED_FACE('',(#10445),#4232,.T.);
#71196=ADVANCED_FACE('',(#10446),#4233,.T.);
#71197=ADVANCED_FACE('',(#10447),#4234,.T.);
#71198=ADVANCED_FACE('',(#10448),#4235,.T.);
#71199=ADVANCED_FACE('',(#10449),#4236,.T.);
#71200=ADVANCED_FACE('',(#10450),#4237,.T.);
#71201=ADVANCED_FACE('',(#10451),#4238,.T.);
#71202=ADVANCED_FACE('',(#10452),#4239,.T.);
#71203=ADVANCED_FACE('',(#10453),#4240,.T.);
#71204=ADVANCED_FACE('',(#10454),#4241,.T.);
#71205=ADVANCED_FACE('',(#10455),#4242,.T.);
#71206=ADVANCED_FACE('',(#10456),#4243,.T.);
#71207=ADVANCED_FACE('',(#10457),#4244,.T.);
#71208=ADVANCED_FACE('',(#10458),#4245,.T.);
#71209=ADVANCED_FACE('',(#10459),#4246,.T.);
#71210=ADVANCED_FACE('',(#10460),#4247,.T.);
#71211=ADVANCED_FACE('',(#10461),#4248,.T.);
#71212=ADVANCED_FACE('',(#10462),#4249,.T.);
#71213=ADVANCED_FACE('',(#10463),#4250,.T.);
#71214=ADVANCED_FACE('',(#10464),#4251,.T.);
#71215=ADVANCED_FACE('',(#10465),#4252,.T.);
#71216=ADVANCED_FACE('',(#10466),#4253,.T.);
#71217=ADVANCED_FACE('',(#10467),#4254,.T.);
#71218=ADVANCED_FACE('',(#10468),#4255,.T.);
#71219=ADVANCED_FACE('',(#10469),#4256,.T.);
#71220=ADVANCED_FACE('',(#10470),#4257,.T.);
#71221=ADVANCED_FACE('',(#10471),#4258,.T.);
#71222=ADVANCED_FACE('',(#10472),#4259,.T.);
#71223=ADVANCED_FACE('',(#10473),#4260,.T.);
#71224=ADVANCED_FACE('',(#10474),#4261,.T.);
#71225=ADVANCED_FACE('',(#10475),#4262,.T.);
#71226=ADVANCED_FACE('',(#10476),#4263,.T.);
#71227=ADVANCED_FACE('',(#10477),#4264,.T.);
#71228=ADVANCED_FACE('',(#10478),#4265,.T.);
#71229=ADVANCED_FACE('',(#10479),#4266,.T.);
#71230=ADVANCED_FACE('',(#10480),#4267,.T.);
#71231=ADVANCED_FACE('',(#10481),#4268,.T.);
#71232=ADVANCED_FACE('',(#10482),#4269,.T.);
#71233=ADVANCED_FACE('',(#10483),#4270,.T.);
#71234=ADVANCED_FACE('',(#10484),#4271,.T.);
#71235=ADVANCED_FACE('',(#10485),#4272,.T.);
#71236=ADVANCED_FACE('',(#10486),#4273,.T.);
#71237=ADVANCED_FACE('',(#10487),#4274,.T.);
#71238=ADVANCED_FACE('',(#10488),#4275,.T.);
#71239=ADVANCED_FACE('',(#10489),#4276,.T.);
#71240=ADVANCED_FACE('',(#10490),#4277,.T.);
#71241=ADVANCED_FACE('',(#10491),#4278,.T.);
#71242=ADVANCED_FACE('',(#10492),#4279,.T.);
#71243=ADVANCED_FACE('',(#10493),#4280,.T.);
#71244=ADVANCED_FACE('',(#10494),#4281,.T.);
#71245=ADVANCED_FACE('',(#10495),#4282,.T.);
#71246=ADVANCED_FACE('',(#10496),#4283,.T.);
#71247=ADVANCED_FACE('',(#10497),#4284,.T.);
#71248=ADVANCED_FACE('',(#10498),#4285,.T.);
#71249=ADVANCED_FACE('',(#10499),#4286,.T.);
#71250=ADVANCED_FACE('',(#10500),#4287,.T.);
#71251=ADVANCED_FACE('',(#10501),#4288,.T.);
#71252=ADVANCED_FACE('',(#10502),#4289,.T.);
#71253=ADVANCED_FACE('',(#10503),#4290,.T.);
#71254=ADVANCED_FACE('',(#10504),#4291,.T.);
#71255=ADVANCED_FACE('',(#10505),#4292,.T.);
#71256=ADVANCED_FACE('',(#10506),#4293,.T.);
#71257=ADVANCED_FACE('',(#10507),#4294,.T.);
#71258=ADVANCED_FACE('',(#10508),#4295,.T.);
#71259=ADVANCED_FACE('',(#10509),#4296,.T.);
#71260=ADVANCED_FACE('',(#10510),#4297,.T.);
#71261=ADVANCED_FACE('',(#10511),#4298,.T.);
#71262=ADVANCED_FACE('',(#10512),#4299,.T.);
#71263=ADVANCED_FACE('',(#10513),#4300,.T.);
#71264=ADVANCED_FACE('',(#10514),#4301,.T.);
#71265=ADVANCED_FACE('',(#10515),#4302,.T.);
#71266=ADVANCED_FACE('',(#10516),#4303,.T.);
#71267=ADVANCED_FACE('',(#10517),#4304,.T.);
#71268=ADVANCED_FACE('',(#10518),#4305,.T.);
#71269=ADVANCED_FACE('',(#10519),#4306,.T.);
#71270=ADVANCED_FACE('',(#10520),#4307,.T.);
#71271=ADVANCED_FACE('',(#10521),#4308,.T.);
#71272=ADVANCED_FACE('',(#10522),#4309,.T.);
#71273=ADVANCED_FACE('',(#10523),#4310,.T.);
#71274=ADVANCED_FACE('',(#10524),#4311,.T.);
#71275=ADVANCED_FACE('',(#10525),#4312,.T.);
#71276=ADVANCED_FACE('',(#10526),#4313,.T.);
#71277=ADVANCED_FACE('',(#10527),#4314,.T.);
#71278=ADVANCED_FACE('',(#10528),#4315,.T.);
#71279=ADVANCED_FACE('',(#10529),#4316,.T.);
#71280=ADVANCED_FACE('',(#10530),#4317,.T.);
#71281=ADVANCED_FACE('',(#10531),#4318,.T.);
#71282=ADVANCED_FACE('',(#10532),#4319,.T.);
#71283=ADVANCED_FACE('',(#10533),#4320,.T.);
#71284=ADVANCED_FACE('',(#10534),#4321,.T.);
#71285=ADVANCED_FACE('',(#10535),#4322,.T.);
#71286=ADVANCED_FACE('',(#10536),#4323,.T.);
#71287=ADVANCED_FACE('',(#10537),#4324,.T.);
#71288=ADVANCED_FACE('',(#10538),#4325,.T.);
#71289=ADVANCED_FACE('',(#10539),#4326,.T.);
#71290=ADVANCED_FACE('',(#10540),#4327,.T.);
#71291=ADVANCED_FACE('',(#10541),#4328,.T.);
#71292=ADVANCED_FACE('',(#10542),#4329,.T.);
#71293=ADVANCED_FACE('',(#10543),#4330,.T.);
#71294=ADVANCED_FACE('',(#10544),#4331,.T.);
#71295=ADVANCED_FACE('',(#10545),#4332,.T.);
#71296=ADVANCED_FACE('',(#10546),#4333,.T.);
#71297=ADVANCED_FACE('',(#10547),#4334,.T.);
#71298=ADVANCED_FACE('',(#10548),#4335,.T.);
#71299=ADVANCED_FACE('',(#10549),#4336,.T.);
#71300=ADVANCED_FACE('',(#10550),#4337,.T.);
#71301=ADVANCED_FACE('',(#10551),#4338,.T.);
#71302=ADVANCED_FACE('',(#10552),#4339,.T.);
#71303=ADVANCED_FACE('',(#10553),#4340,.T.);
#71304=ADVANCED_FACE('',(#10554),#4341,.T.);
#71305=ADVANCED_FACE('',(#10555),#4342,.T.);
#71306=ADVANCED_FACE('',(#10556),#4343,.T.);
#71307=ADVANCED_FACE('',(#10557),#4344,.T.);
#71308=ADVANCED_FACE('',(#10558),#4345,.T.);
#71309=ADVANCED_FACE('',(#10559),#4346,.T.);
#71310=ADVANCED_FACE('',(#10560),#4347,.T.);
#71311=ADVANCED_FACE('',(#10561),#4348,.T.);
#71312=ADVANCED_FACE('',(#10562),#4349,.T.);
#71313=ADVANCED_FACE('',(#10563),#4350,.T.);
#71314=ADVANCED_FACE('',(#10564),#4351,.T.);
#71315=ADVANCED_FACE('',(#10565),#4352,.T.);
#71316=ADVANCED_FACE('',(#10566),#4353,.T.);
#71317=ADVANCED_FACE('',(#10567),#4354,.T.);
#71318=ADVANCED_FACE('',(#10568),#4355,.T.);
#71319=ADVANCED_FACE('',(#10569),#4356,.T.);
#71320=ADVANCED_FACE('',(#10570),#4357,.T.);
#71321=ADVANCED_FACE('',(#10571),#4358,.T.);
#71322=ADVANCED_FACE('',(#10572),#4359,.T.);
#71323=ADVANCED_FACE('',(#10573),#4360,.T.);
#71324=ADVANCED_FACE('',(#10574),#4361,.T.);
#71325=ADVANCED_FACE('',(#10575),#4362,.T.);
#71326=ADVANCED_FACE('',(#10576),#4363,.T.);
#71327=ADVANCED_FACE('',(#10577),#4364,.T.);
#71328=ADVANCED_FACE('',(#10578),#4365,.T.);
#71329=ADVANCED_FACE('',(#10579),#4366,.T.);
#71330=ADVANCED_FACE('',(#10580),#4367,.T.);
#71331=ADVANCED_FACE('',(#10581),#4368,.T.);
#71332=ADVANCED_FACE('',(#10582),#4369,.T.);
#71333=ADVANCED_FACE('',(#10583,#72),#88,.T.);
#71334=ADVANCED_FACE('',(#10584,#73),#89,.T.);
#71335=ADVANCED_FACE('',(#10585),#5361,.T.);
#71336=ADVANCED_FACE('',(#10586),#5362,.F.);
#71337=ADVANCED_FACE('',(#10587),#5363,.T.);
#71338=ADVANCED_FACE('',(#10588),#5364,.F.);
#71339=ADVANCED_FACE('',(#10589),#66124,.T.);
#71340=ADVANCED_FACE('',(#10590),#66125,.T.);
#71341=ADVANCED_FACE('',(#10591),#5365,.T.);
#71342=ADVANCED_FACE('',(#10592,#74),#90,.T.);
#71343=ADVANCED_FACE('',(#10593,#75),#91,.F.);
#71344=ADVANCED_FACE('',(#10594),#92,.T.);
#71345=ADVANCED_FACE('',(#10595),#5366,.F.);
#71346=ADVANCED_FACE('',(#10596),#93,.T.);
#71347=ADVANCED_FACE('',(#10597),#94,.T.);
#71348=ADVANCED_FACE('',(#10598),#95,.T.);
#71349=ADVANCED_FACE('',(#10599),#96,.T.);
#71350=ADVANCED_FACE('',(#10600),#97,.T.);
#71351=ADVANCED_FACE('',(#10601),#66126,.T.);
#71352=ADVANCED_FACE('',(#10602),#5367,.T.);
#71353=ADVANCED_FACE('',(#10603),#5368,.T.);
#71354=ADVANCED_FACE('',(#10604),#5369,.F.);
#71355=ADVANCED_FACE('',(#10605),#66127,.F.);
#71356=ADVANCED_FACE('',(#10606),#5370,.F.);
#71357=ADVANCED_FACE('',(#10607),#5371,.T.);
#71358=ADVANCED_FACE('',(#10608),#66128,.F.);
#71359=ADVANCED_FACE('',(#10609),#5372,.T.);
#71360=ADVANCED_FACE('',(#10610),#4370,.F.);
#71361=ADVANCED_FACE('',(#10611),#5373,.T.);
#71362=ADVANCED_FACE('',(#10612),#5374,.T.);
#71363=ADVANCED_FACE('',(#10613),#4371,.F.);
#71364=ADVANCED_FACE('',(#10614),#4372,.F.);
#71365=ADVANCED_FACE('',(#10615),#36,.T.);
#71366=ADVANCED_FACE('',(#10616),#37,.T.);
#71367=ADVANCED_FACE('',(#10617),#4373,.T.);
#71368=ADVANCED_FACE('',(#10618),#38,.T.);
#71369=ADVANCED_FACE('',(#10619),#4374,.F.);
#71370=ADVANCED_FACE('',(#10620),#98,.T.);
#71371=ADVANCED_FACE('',(#10621,#76),#99,.F.);
#71372=ADVANCED_FACE('',(#10622,#77),#100,.T.);
#71373=ADVANCED_FACE('',(#10623,#78),#101,.F.);
#71374=ADVANCED_FACE('',(#10624),#39,.T.);
#71375=ADVANCED_FACE('',(#10625),#5375,.F.);
#71376=ADVANCED_FACE('',(#10626,#79),#102,.F.);
#71377=ADVANCED_FACE('',(#10627,#80),#5376,.F.);
#71378=ADVANCED_FACE('',(#10628,#81),#35,.T.);
#71379=ADVANCED_FACE('',(#10629),#5377,.T.);
#71380=ADVANCED_FACE('',(#10630),#66129,.F.);
#71381=ADVANCED_FACE('',(#10631),#66130,.T.);
#71382=ADVANCED_FACE('',(#10632),#5378,.F.);
#71383=ADVANCED_FACE('',(#10633,#82),#103,.T.);
#71384=ADVANCED_FACE('',(#10634),#104,.F.);
#71385=ADVANCED_FACE('',(#10635),#105,.F.);
#71386=ADVANCED_FACE('',(#10636),#5379,.F.);
#71387=ADVANCED_FACE('',(#10637,#83),#106,.F.);
#71388=ADVANCED_FACE('',(#10638,#84),#107,.F.);
#71389=ADVANCED_FACE('',(#10639,#85),#5380,.T.);
#71390=ADVANCED_FACE('',(#10640),#66131,.T.);
#71391=ADVANCED_FACE('',(#10641),#66132,.T.);
#71392=ADVANCED_FACE('',(#10642),#108,.F.);
#71393=ADVANCED_FACE('',(#10643),#109,.T.);
#71394=ADVANCED_FACE('',(#10644),#5381,.F.);
#71395=ADVANCED_FACE('',(#10645),#5382,.T.);
#71396=ADVANCED_FACE('',(#10646),#110,.T.);
#71397=ADVANCED_FACE('',(#10647),#111,.F.);
#71398=CLOSED_SHELL('',(#66133,#66134,#66135,#66136,#66137,#66138,#66139,
#66140,#66141,#66142,#66143,#66144,#66145,#66146,#66147,#66148,#66149,#66150,
#66151,#66152,#66153,#66154,#66155,#66156,#66157,#66158,#66159,#66160,#66161,
#66162,#66163,#66164,#66165,#66166,#66167,#66168,#66169,#66170,#66171,#66172,
#66173,#66174,#66175,#66176,#66177,#66178,#66179,#66180,#66181,#66182,#66183,
#66184,#66185,#66186,#66187,#66188,#66189,#66190,#66191,#66192,#66193,#66194,
#66195,#66196,#66197,#66198,#66199,#66200,#66201,#66202,#66203,#66204,#66205,
#66206,#66207,#66208,#66209,#66210,#66211,#66212,#66213,#66214,#66215,#66216,
#66217,#66218,#66219,#66220,#66221,#66222,#66223,#66224,#66225,#66226,#66227,
#66228,#66229,#66230,#66231,#66232,#66233,#66234,#66235,#66236,#66237,#66238,
#66239,#66240,#66241,#66242,#66243,#66244,#66245,#66246,#66247,#66248,#66249,
#66250,#66251,#66252,#66253,#66254,#66255,#66256,#66257,#66258,#66259,#66260,
#66261,#66262,#66263,#66264,#66265,#66266,#66267,#66268,#66269,#66270,#66271,
#66272,#66273,#66274,#66275,#66276,#66277,#66278,#66279,#66280,#66281,#66282,
#66283,#66284,#66285,#66286,#66287,#66288,#66289,#66290,#66291,#66292,#66293,
#66294,#66295,#66296,#66297,#66298,#66299,#66300,#66301,#66302,#66303,#66304,
#66305,#66306,#66307,#66308,#66309,#66310,#66311,#66312,#66313,#66314,#66315,
#66316,#66317,#66318,#66319,#66320,#66321,#66322,#66323,#66324,#66325,#66326,
#66327,#66328,#66329,#66330,#66331,#66332,#66333,#66334,#66335,#66336,#66337,
#66338,#66339,#66340,#66341,#66342,#66343,#66344,#66345,#66346,#66347,#66348,
#66349,#66350,#66351,#66352,#66353,#66354,#66355,#66356,#66357,#66358,#66359,
#66360,#66361,#66362,#66363,#66364,#66365,#66366,#66367,#66368,#66369,#66370,
#66371,#66372,#66373,#66374,#66375,#66376,#66377,#66378,#66379,#66380,#66381,
#66382,#66383,#66384,#66385,#66386,#66387,#66388,#66389,#66390,#66391,#66392,
#66393,#66394,#66395,#66396,#66397,#66398,#66399,#66400,#66401,#66402,#66403,
#66404,#66405,#66406,#66407,#66408,#66409,#66410,#66411,#66412,#66413,#66414,
#66415,#66416,#66417,#66418,#66419,#66420,#66421,#66422,#66423,#66424,#66425,
#66426,#66427,#66428,#66429,#66430,#66431,#66432,#66433,#66434,#66435,#66436,
#66437,#66438,#66439,#66440,#66441,#66442,#66443,#66444,#66445,#66446,#66447,
#66448,#66449,#66450,#66451,#66452,#66453,#66454,#66455,#66456,#66457,#66458,
#66459,#66460,#66461,#66462,#66463,#66464,#66465,#66466,#66467,#66468,#66469,
#66470,#66471,#66472,#66473,#66474,#66475,#66476,#66477,#66478,#66479,#66480,
#66481,#66482,#66483,#66484,#66485,#66486,#66487,#66488,#66489,#66490,#66491,
#66492,#66493,#66494,#66495,#66496,#66497,#66498,#66499,#66500,#66501,#66502,
#66503,#66504,#66505,#66506,#66507,#66508,#66509,#66510,#66511,#66512,#66513,
#66514,#66515,#66516,#66517,#66518,#66519,#66520,#66521,#66522,#66523,#66524,
#66525,#66526,#66527,#66528,#66529,#66530,#66531,#66532,#66533,#66534,#66535,
#66536,#66537,#66538,#66539,#66540,#66541,#66542,#66543,#66544,#66545,#66546,
#66547,#66548,#66549,#66550,#66551,#66552,#66553,#66554,#66555,#66556,#66557,
#66558,#66559,#66560,#66561,#66562,#66563,#66564,#66565,#66566,#66567,#66568,
#66569,#66570,#66571,#66572,#66573,#66574,#66575,#66576,#66577,#66578,#66579,
#66580,#66581,#66582,#66583,#66584,#66585,#66586,#66587,#66588,#66589,#66590,
#66591,#66592,#66593,#66594,#66595,#66596,#66597,#66598,#66599,#66600,#66601,
#66602,#66603,#66604,#66605,#66606,#66607,#66608,#66609,#66610,#66611,#66612,
#66613,#66614,#66615,#66616,#66617,#66618,#66619,#66620,#66621,#66622,#66623,
#66624,#66625,#66626,#66627,#66628,#66629,#66630,#66631,#66632,#66633,#66634,
#66635,#66636,#66637,#66638,#66639,#66640,#66641,#66642,#66643,#66644,#66645,
#66646,#66647,#66648,#66649,#66650,#66651,#66652,#66653,#66654,#66655,#66656,
#66657,#66658,#66659,#66660,#66661,#66662,#66663,#66664,#66665,#66666,#66667,
#66668,#66669,#66670,#66671,#66672,#66673,#66674,#66675,#66676,#66677,#66678,
#66679,#66680,#66681,#66682,#66683,#66684,#66685,#66686,#66687,#66688,#66689,
#66690,#66691,#66692,#66693,#66694,#66695,#66696,#66697,#66698,#66699,#66700,
#66701,#66702,#66703,#66704,#66705,#66706,#66707,#66708,#66709,#66710,#66711,
#66712,#66713,#66714,#66715,#66716,#66717,#66718,#66719,#66720,#66721,#66722,
#66723,#66724,#66725,#66726,#66727,#66728,#66729,#66730,#66731,#66732,#66733,
#66734,#66735,#66736,#66737,#66738,#66739,#66740,#66741,#66742,#66743,#66744,
#66745,#66746,#66747,#66748,#66749,#66750,#66751,#66752,#66753,#66754,#66755,
#66756,#66757,#66758,#66759,#66760,#66761,#66762,#66763,#66764,#66765,#66766,
#66767,#66768,#66769,#66770,#66771,#66772,#66773,#66774,#66775,#66776,#66777,
#66778,#66779,#66780,#66781,#66782,#66783,#66784,#66785,#66786,#66787,#66788,
#66789,#66790,#66791,#66792,#66793,#66794,#66795,#66796,#66797,#66798,#66799,
#66800,#66801,#66802,#66803,#66804,#66805,#66806,#66807,#66808,#66809,#66810,
#66811,#66812,#66813,#66814,#66815,#66816,#66817,#66818,#66819,#66820,#66821,
#66822,#66823,#66824,#66825,#66826,#66827,#66828,#66829,#66830,#66831,#66832,
#66833,#66834,#66835,#66836,#66837,#66838,#66839,#66840,#66841,#66842,#66843,
#66844,#66845,#66846,#66847,#66848,#66849,#66850,#66851,#66852,#66853,#66854,
#66855,#66856,#66857,#66858,#66859,#66860,#66861,#66862,#66863,#66864,#66865,
#66866,#66867,#66868,#66869,#66870,#66871,#66872,#66873,#66874,#66875,#66876,
#66877,#66878,#66879,#66880,#66881,#66882,#66883,#66884,#66885,#66886,#66887,
#66888,#66889,#66890,#66891,#66892,#66893,#66894,#66895,#66896,#66897,#66898,
#66899,#66900,#66901,#66902,#66903,#66904,#66905,#66906,#66907,#66908,#66909,
#66910,#66911,#66912,#66913,#66914,#66915,#66916,#66917,#66918,#66919,#66920,
#66921,#66922,#66923,#66924,#66925,#66926,#66927,#66928,#66929,#66930,#66931,
#66932,#66933,#66934,#66935,#66936,#66937,#66938,#66939,#66940,#66941,#66942,
#66943,#66944,#66945,#66946,#66947,#66948,#66949,#66950,#66951,#66952,#66953,
#66954,#66955,#66956,#66957,#66958,#66959,#66960,#66961,#66962,#66963,#66964,
#66965,#66966,#66967,#66968,#66969,#66970,#66971,#66972,#66973,#66974,#66975,
#66976,#66977,#66978,#66979,#66980,#66981,#66982,#66983,#66984,#66985,#66986,
#66987,#66988,#66989,#66990,#66991,#66992,#66993,#66994,#66995,#66996,#66997,
#66998,#66999,#67000,#67001,#67002,#67003,#67004,#67005,#67006,#67007,#67008,
#67009,#67010,#67011,#67012,#67013,#67014,#67015,#67016,#67017,#67018,#67019,
#67020,#67021,#67022,#67023,#67024,#67025,#67026,#67027,#67028,#67029,#67030,
#67031,#67032,#67033,#67034,#67035,#67036,#67037,#67038,#67039,#67040,#67041,
#67042,#67043,#67044,#67045,#67046,#67047,#67048,#67049,#67050,#67051,#67052,
#67053,#67054,#67055,#67056,#67057,#67058,#67059,#67060,#67061,#67062,#67063,
#67064,#67065,#67066,#67067,#67068,#67069,#67070,#67071,#67072,#67073,#67074,
#67075,#67076,#67077,#67078,#67079,#67080,#67081,#67082,#67083,#67084,#67085,
#67086,#67087,#67088,#67089,#67090,#67091,#67092,#67093,#67094,#67095,#67096,
#67097,#67098,#67099,#67100,#67101,#67102,#67103,#67104,#67105,#67106,#67107,
#67108,#67109,#67110,#67111,#67112,#67113,#67114,#67115,#67116,#67117,#67118,
#67119,#67120,#67121,#67122,#67123,#67124,#67125,#67126,#67127,#67128,#67129,
#67130,#67131,#67132,#67133,#67134,#67135,#67136,#67137,#67138,#67139,#67140,
#67141,#67142,#67143,#67144,#67145,#67146,#67147,#67148,#67149,#67150,#67151,
#67152,#67153,#67154,#67155,#67156,#67157,#67158,#67159,#67160,#67161,#67162,
#67163,#67164,#67165,#67166,#67167,#67168,#67169,#67170,#67171,#67172,#67173,
#67174,#67175,#67176,#67177,#67178,#67179,#67180,#67181,#67182,#67183,#67184,
#67185,#67186,#67187,#67188,#67189,#67190,#67191,#67192,#67193,#67194,#67195,
#67196,#67197,#67198,#67199,#67200,#67201,#67202,#67203,#67204,#67205,#67206,
#67207,#67208,#67209,#67210,#67211,#67212,#67213,#67214,#67215,#67216,#67217,
#67218,#67219,#67220,#67221,#67222,#67223,#67224,#67225,#67226,#67227,#67228,
#67229,#67230,#67231,#67232,#67233,#67234,#67235,#67236,#67237,#67238,#67239,
#67240,#67241,#67242,#67243,#67244,#67245,#67246,#67247,#67248,#67249,#67250,
#67251,#67252,#67253,#67254,#67255,#67256,#67257,#67258,#67259,#67260,#67261,
#67262,#67263,#67264,#67265,#67266,#67267,#67268,#67269,#67270,#67271,#67272,
#67273,#67274,#67275,#67276,#67277,#67278,#67279,#67280,#67281,#67282,#67283,
#67284,#67285,#67286,#67287,#67288,#67289,#67290,#67291,#67292,#67293,#67294,
#67295,#67296,#67297,#67298,#67299,#67300,#67301,#67302,#67303,#67304,#67305,
#67306,#67307,#67308,#67309,#67310,#67311,#67312,#67313,#67314,#67315,#67316,
#67317,#67318,#67319,#67320,#67321,#67322,#67323,#67324,#67325,#67326,#67327,
#67328,#67329,#67330,#67331,#67332,#67333,#67334,#67335,#67336,#67337,#67338,
#67339,#67340,#67341,#67342,#67343,#67344,#67345,#67346,#67347,#67348,#67349,
#67350,#67351,#67352,#67353,#67354,#67355,#67356,#67357,#67358,#67359,#67360,
#67361,#67362,#67363,#67364,#67365,#67366,#67367,#67368,#67369,#67370,#67371,
#67372,#67373,#67374,#67375,#67376,#67377,#67378,#67379,#67380,#67381,#67382,
#67383,#67384,#67385,#67386,#67387,#67388,#67389,#67390,#67391,#67392,#67393,
#67394,#67395,#67396,#67397,#67398,#67399,#67400,#67401,#67402,#67403,#67404,
#67405,#67406,#67407,#67408,#67409,#67410,#67411,#67412,#67413,#67414,#67415,
#67416,#67417,#67418,#67419,#67420,#67421,#67422,#67423,#67424,#67425,#67426,
#67427,#67428,#67429,#67430,#67431,#67432,#67433,#67434,#67435,#67436,#67437,
#67438,#67439,#67440,#67441,#67442,#67443,#67444,#67445,#67446,#67447,#67448,
#67449,#67450,#67451,#67452,#67453,#67454,#67455,#67456,#67457,#67458,#67459,
#67460,#67461,#67462,#67463,#67464,#67465,#67466,#67467,#67468,#67469,#67470,
#67471,#67472,#67473,#67474,#67475,#67476,#67477,#67478,#67479,#67480,#67481,
#67482,#67483,#67484,#67485,#67486,#67487,#67488,#67489,#67490,#67491,#67492,
#67493,#67494,#67495,#67496,#67497,#67498,#67499,#67500,#67501,#67502,#67503,
#67504,#67505,#67506,#67507,#67508,#67509,#67510,#67511,#67512,#67513,#67514,
#67515,#67516,#67517,#67518,#67519,#67520,#67521,#67522,#67523,#67524,#67525,
#67526,#67527,#67528,#67529,#67530,#67531,#67532,#67533,#67534,#67535,#67536,
#67537,#67538,#67539,#67540,#67541,#67542,#67543,#67544,#67545,#67546,#67547,
#67548,#67549,#67550,#67551,#67552,#67553,#67554,#67555,#67556,#67557,#67558,
#67559,#67560,#67561,#67562,#67563,#67564,#67565,#67566,#67567,#67568,#67569,
#67570,#67571,#67572,#67573,#67574,#67575,#67576,#67577,#67578,#67579,#67580,
#67581,#67582,#67583,#67584,#67585,#67586,#67587,#67588,#67589,#67590,#67591,
#67592,#67593,#67594,#67595,#67596,#67597,#67598,#67599,#67600,#67601,#67602,
#67603,#67604,#67605,#67606,#67607,#67608,#67609,#67610,#67611,#67612,#67613,
#67614,#67615,#67616,#67617,#67618,#67619,#67620,#67621,#67622,#67623,#67624,
#67625,#67626,#67627,#67628,#67629,#67630,#67631,#67632,#67633,#67634,#67635,
#67636,#67637,#67638,#67639,#67640,#67641,#67642,#67643,#67644,#67645,#67646,
#67647,#67648,#67649,#67650,#67651,#67652,#67653,#67654,#67655,#67656,#67657,
#67658,#67659,#67660,#67661,#67662,#67663,#67664,#67665,#67666,#67667,#67668,
#67669,#67670,#67671,#67672,#67673,#67674,#67675,#67676,#67677,#67678,#67679,
#67680,#67681,#67682,#67683,#67684,#67685,#67686,#67687,#67688,#67689,#67690,
#67691,#67692,#67693,#67694,#67695,#67696,#67697,#67698,#67699,#67700,#67701,
#67702,#67703,#67704,#67705,#67706,#67707,#67708,#67709,#67710,#67711,#67712,
#67713,#67714,#67715,#67716,#67717,#67718,#67719,#67720,#67721,#67722,#67723,
#67724,#67725,#67726,#67727,#67728,#67729,#67730,#67731,#67732,#67733,#67734,
#67735,#67736,#67737,#67738,#67739,#67740,#67741,#67742,#67743,#67744,#67745,
#67746,#67747,#67748,#67749,#67750,#67751,#67752,#67753,#67754,#67755,#67756,
#67757,#67758,#67759,#67760,#67761,#67762,#67763,#67764,#67765,#67766,#67767,
#67768,#67769,#67770,#67771,#67772,#67773,#67774,#67775,#67776,#67777,#67778,
#67779,#67780,#67781,#67782,#67783,#67784,#67785,#67786,#67787,#67788,#67789,
#67790,#67791,#67792,#67793,#67794,#67795,#67796,#67797,#67798,#67799,#67800,
#67801,#67802,#67803,#67804,#67805,#67806,#67807,#67808,#67809,#67810,#67811,
#67812,#67813,#67814,#67815,#67816,#67817,#67818,#67819,#67820,#67821,#67822,
#67823,#67824,#67825,#67826,#67827,#67828,#67829,#67830,#67831,#67832,#67833,
#67834,#67835,#67836,#67837,#67838,#67839,#67840,#67841,#67842,#67843,#67844,
#67845,#67846,#67847,#67848,#67849,#67850,#67851,#67852,#67853,#67854,#67855,
#67856,#67857,#67858,#67859,#67860,#67861,#67862,#67863,#67864,#67865,#67866,
#67867,#67868,#67869,#67870,#67871,#67872,#67873,#67874,#67875,#67876,#67877,
#67878,#67879,#67880,#67881,#67882,#67883,#67884,#67885,#67886,#67887,#67888,
#67889,#67890,#67891,#67892,#67893,#67894,#67895,#67896,#67897,#67898,#67899,
#67900,#67901,#67902,#67903,#67904,#67905,#67906,#67907,#67908,#67909,#67910,
#67911,#67912,#67913,#67914,#67915,#67916,#67917,#67918,#67919,#67920,#67921,
#67922,#67923,#67924,#67925,#67926,#67927,#67928,#67929,#67930,#67931,#67932,
#67933,#67934,#67935,#67936,#67937,#67938,#67939,#67940,#67941,#67942,#67943,
#67944,#67945,#67946,#67947,#67948,#67949,#67950,#67951,#67952,#67953,#67954,
#67955,#67956,#67957,#67958,#67959,#67960,#67961,#67962,#67963,#67964,#67965,
#67966,#67967,#67968,#67969,#67970,#67971,#67972,#67973,#67974,#67975,#67976,
#67977,#67978,#67979,#67980,#67981,#67982,#67983,#67984,#67985,#67986,#67987,
#67988,#67989,#67990,#67991,#67992,#67993,#67994,#67995,#67996,#67997,#67998,
#67999,#68000,#68001,#68002,#68003,#68004,#68005,#68006,#68007,#68008,#68009,
#68010,#68011,#68012,#68013,#68014,#68015,#68016,#68017,#68018,#68019,#68020,
#68021,#68022,#68023,#68024,#68025,#68026,#68027,#68028,#68029,#68030,#68031,
#68032,#68033,#68034,#68035,#68036,#68037,#68038,#68039,#68040,#68041,#68042,
#68043,#68044,#68045,#68046,#68047,#68048,#68049,#68050,#68051,#68052,#68053,
#68054,#68055,#68056,#68057,#68058,#68059,#68060,#68061,#68062,#68063,#68064,
#68065,#68066,#68067,#68068,#68069,#68070,#68071,#68072,#68073,#68074,#68075,
#68076,#68077,#68078,#68079,#68080,#68081,#68082,#68083,#68084,#68085,#68086,
#68087,#68088,#68089,#68090,#68091,#68092,#68093,#68094,#68095,#68096,#68097,
#68098,#68099,#68100,#68101,#68102,#68103,#68104,#68105,#68106,#68107,#68108,
#68109,#68110,#68111,#68112,#68113,#68114,#68115,#68116,#68117,#68118,#68119,
#68120,#68121,#68122,#68123,#68124,#68125,#68126,#68127,#68128,#68129,#68130,
#68131,#68132,#68133,#68134,#68135,#68136,#68137,#68138,#68139,#68140,#68141,
#68142,#68143,#68144,#68145,#68146,#68147,#68148,#68149,#68150,#68151,#68152,
#68153,#68154,#68155,#68156,#68157,#68158,#68159,#68160,#68161,#68162,#68163,
#68164,#68165,#68166,#68167,#68168,#68169,#68170,#68171,#68172,#68173,#68174,
#68175,#68176,#68177,#68178,#68179,#68180,#68181,#68182,#68183,#68184,#68185,
#68186,#68187,#68188,#68189,#68190,#68191,#68192,#68193,#68194,#68195,#68196,
#68197,#68198,#68199,#68200,#68201,#68202,#68203,#68204,#68205,#68206,#68207,
#68208,#68209,#68210,#68211,#68212,#68213,#68214,#68215,#68216,#68217,#68218,
#68219,#68220,#68221,#68222,#68223,#68224,#68225,#68226,#68227,#68228,#68229,
#68230,#68231,#68232,#68233,#68234,#68235,#68236,#68237,#68238,#68239,#68240,
#68241,#68242,#68243,#68244,#68245,#68246,#68247,#68248,#68249,#68250,#68251,
#68252,#68253,#68254,#68255,#68256,#68257,#68258,#68259,#68260,#68261,#68262,
#68263,#68264,#68265,#68266,#68267,#68268,#68269,#68270,#68271,#68272,#68273,
#68274,#68275,#68276,#68277,#68278,#68279,#68280,#68281,#68282,#68283,#68284,
#68285,#68286,#68287,#68288,#68289,#68290,#68291,#68292,#68293,#68294,#68295,
#68296,#68297,#68298,#68299,#68300,#68301,#68302,#68303,#68304,#68305,#68306,
#68307,#68308,#68309,#68310,#68311,#68312,#68313,#68314,#68315,#68316,#68317,
#68318,#68319,#68320,#68321,#68322,#68323,#68324,#68325,#68326,#68327,#68328,
#68329,#68330,#68331,#68332,#68333,#68334,#68335,#68336,#68337,#68338,#68339,
#68340,#68341,#68342,#68343,#68344,#68345,#68346,#68347,#68348,#68349,#68350,
#68351,#68352,#68353,#68354,#68355,#68356,#68357,#68358,#68359,#68360,#68361,
#68362,#68363,#68364,#68365,#68366,#68367,#68368,#68369,#68370,#68371,#68372,
#68373,#68374,#68375,#68376,#68377,#68378,#68379,#68380,#68381,#68382,#68383,
#68384,#68385,#68386,#68387,#68388,#68389,#68390,#68391,#68392,#68393,#68394,
#68395,#68396,#68397,#68398,#68399,#68400,#68401,#68402,#68403,#68404,#68405,
#68406,#68407,#68408,#68409,#68410,#68411,#68412,#68413,#68414,#68415,#68416,
#68417,#68418,#68419,#68420,#68421,#68422,#68423,#68424,#68425,#68426,#68427,
#68428,#68429,#68430,#68431,#68432,#68433,#68434,#68435,#68436,#68437,#68438,
#68439,#68440,#68441,#68442,#68443,#68444,#68445,#68446,#68447,#68448,#68449,
#68450,#68451,#68452,#68453,#68454,#68455,#68456,#68457,#68458,#68459,#68460,
#68461,#68462,#68463,#68464,#68465,#68466,#68467,#68468,#68469,#68470,#68471,
#68472,#68473,#68474,#68475,#68476,#68477,#68478,#68479,#68480,#68481,#68482,
#68483,#68484,#68485,#68486,#68487,#68488,#68489,#68490,#68491,#68492,#68493,
#68494,#68495,#68496,#68497,#68498,#68499,#68500,#68501,#68502,#68503,#68504,
#68505,#68506,#68507,#68508,#68509,#68510,#68511,#68512,#68513,#68514,#68515,
#68516,#68517,#68518,#68519,#68520,#68521,#68522,#68523,#68524,#68525,#68526,
#68527,#68528,#68529,#68530,#68531,#68532,#68533,#68534,#68535,#68536,#68537,
#68538,#68539,#68540,#68541,#68542,#68543,#68544,#68545,#68546,#68547,#68548,
#68549,#68550,#68551,#68552,#68553,#68554,#68555,#68556,#68557,#68558,#68559,
#68560,#68561,#68562,#68563,#68564,#68565,#68566,#68567,#68568,#68569,#68570,
#68571,#68572,#68573,#68574,#68575,#68576,#68577,#68578,#68579,#68580,#68581,
#68582,#68583,#68584,#68585,#68586,#68587,#68588,#68589,#68590,#68591,#68592,
#68593,#68594,#68595,#68596,#68597,#68598,#68599,#68600,#68601,#68602,#68603,
#68604,#68605,#68606,#68607,#68608,#68609,#68610,#68611,#68612,#68613,#68614,
#68615,#68616,#68617,#68618,#68619,#68620,#68621,#68622,#68623,#68624,#68625,
#68626,#68627,#68628,#68629,#68630,#68631,#68632,#68633,#68634,#68635,#68636,
#68637,#68638,#68639,#68640,#68641,#68642,#68643,#68644,#68645,#68646,#68647,
#68648,#68649,#68650,#68651,#68652,#68653,#68654,#68655,#68656,#68657,#68658,
#68659,#68660,#68661,#68662,#68663,#68664,#68665,#68666,#68667,#68668,#68669,
#68670,#68671,#68672,#68673,#68674,#68675,#68676,#68677,#68678,#68679,#68680,
#68681,#68682,#68683,#68684,#68685,#68686,#68687,#68688,#68689,#68690,#68691,
#68692,#68693,#68694,#68695,#68696,#68697,#68698,#68699,#68700,#68701,#68702,
#68703,#68704,#68705,#68706,#68707,#68708,#68709,#68710,#68711,#68712,#68713,
#68714,#68715,#68716,#68717,#68718,#68719,#68720,#68721,#68722,#68723,#68724,
#68725,#68726,#68727,#68728,#68729,#68730,#68731,#68732,#68733,#68734,#68735,
#68736,#68737,#68738,#68739,#68740,#68741,#68742,#68743,#68744,#68745,#68746,
#68747,#68748,#68749,#68750,#68751,#68752,#68753,#68754,#68755,#68756,#68757,
#68758,#68759,#68760,#68761,#68762,#68763,#68764,#68765,#68766,#68767,#68768,
#68769,#68770,#68771,#68772,#68773,#68774,#68775,#68776,#68777,#68778,#68779,
#68780,#68781,#68782,#68783,#68784,#68785,#68786,#68787,#68788,#68789,#68790,
#68791,#68792,#68793,#68794,#68795,#68796,#68797,#68798,#68799,#68800,#68801,
#68802,#68803,#68804,#68805,#68806,#68807,#68808,#68809,#68810,#68811,#68812,
#68813,#68814,#68815,#68816,#68817,#68818,#68819,#68820,#68821,#68822,#68823,
#68824,#68825,#68826,#68827,#68828,#68829,#68830,#68831,#68832,#68833,#68834,
#68835,#68836,#68837,#68838,#68839,#68840,#68841,#68842,#68843,#68844,#68845,
#68846,#68847,#68848,#68849,#68850,#68851,#68852,#68853,#68854,#68855,#68856,
#68857,#68858,#68859,#68860,#68861,#68862,#68863,#68864,#68865,#68866,#68867,
#68868,#68869,#68870,#68871,#68872,#68873,#68874,#68875,#68876,#68877,#68878,
#68879,#68880,#68881,#68882,#68883,#68884,#68885,#68886,#68887,#68888,#68889,
#68890,#68891,#68892,#68893,#68894,#68895,#68896,#68897,#68898,#68899,#68900,
#68901,#68902,#68903,#68904,#68905,#68906,#68907,#68908,#68909,#68910,#68911,
#68912,#68913,#68914,#68915,#68916,#68917,#68918,#68919,#68920,#68921,#68922,
#68923,#68924,#68925,#68926,#68927,#68928,#68929,#68930,#68931,#68932,#68933,
#68934,#68935,#68936,#68937,#68938,#68939,#68940,#68941,#68942,#68943,#68944,
#68945,#68946,#68947,#68948,#68949,#68950,#68951,#68952,#68953,#68954,#68955,
#68956,#68957,#68958,#68959,#68960,#68961,#68962,#68963,#68964,#68965,#68966,
#68967,#68968,#68969,#68970,#68971,#68972,#68973,#68974,#68975,#68976,#68977,
#68978,#68979,#68980,#68981,#68982,#68983,#68984,#68985,#68986,#68987,#68988,
#68989,#68990,#68991,#68992,#68993,#68994,#68995,#68996,#68997,#68998,#68999,
#69000,#69001,#69002,#69003,#69004,#69005,#69006,#69007,#69008,#69009,#69010,
#69011,#69012,#69013,#69014,#69015,#69016,#69017,#69018,#69019,#69020,#69021,
#69022,#69023,#69024,#69025,#69026,#69027,#69028,#69029,#69030,#69031,#69032,
#69033,#69034,#69035,#69036,#69037,#69038,#69039,#69040,#69041,#69042,#69043,
#69044,#69045,#69046,#69047,#69048,#69049,#69050,#69051,#69052,#69053,#69054,
#69055,#69056,#69057,#69058,#69059,#69060,#69061,#69062,#69063,#69064,#69065,
#69066,#69067,#69068,#69069,#69070,#69071,#69072,#69073,#69074,#69075,#69076,
#69077,#69078,#69079,#69080,#69081,#69082,#69083,#69084,#69085,#69086,#69087,
#69088,#69089,#69090,#69091,#69092,#69093,#69094,#69095,#69096,#69097,#69098,
#69099,#69100,#69101,#69102,#69103,#69104,#69105,#69106,#69107,#69108,#69109,
#69110,#69111,#69112,#69113,#69114,#69115,#69116,#69117,#69118,#69119,#69120,
#69121,#69122,#69123,#69124,#69125,#69126,#69127,#69128,#69129,#69130,#69131,
#69132,#69133,#69134,#69135,#69136,#69137,#69138,#69139,#69140,#69141,#69142,
#69143,#69144,#69145,#69146,#69147,#69148,#69149,#69150,#69151,#69152,#69153,
#69154,#69155,#69156,#69157,#69158,#69159,#69160,#69161,#69162,#69163,#69164,
#69165,#69166,#69167,#69168,#69169,#69170,#69171,#69172,#69173,#69174,#69175,
#69176,#69177,#69178,#69179,#69180,#69181,#69182,#69183,#69184,#69185,#69186,
#69187,#69188,#69189,#69190,#69191,#69192,#69193,#69194,#69195,#69196,#69197,
#69198,#69199,#69200,#69201,#69202,#69203,#69204,#69205,#69206,#69207,#69208,
#69209,#69210,#69211,#69212,#69213,#69214,#69215,#69216,#69217,#69218,#69219,
#69220,#69221,#69222,#69223,#69224,#69225,#69226,#69227,#69228,#69229,#69230,
#69231,#69232,#69233,#69234,#69235,#69236,#69237,#69238,#69239,#69240,#69241,
#69242,#69243,#69244,#69245,#69246,#69247,#69248,#69249,#69250,#69251,#69252,
#69253,#69254,#69255,#69256,#69257,#69258,#69259,#69260,#69261,#69262,#69263,
#69264,#69265,#69266,#69267,#69268,#69269,#69270,#69271,#69272,#69273,#69274,
#69275,#69276,#69277,#69278,#69279,#69280,#69281,#69282,#69283,#69284,#69285,
#69286,#69287,#69288,#69289,#69290,#69291,#69292,#69293,#69294,#69295,#69296,
#69297,#69298,#69299,#69300,#69301,#69302,#69303,#69304,#69305,#69306,#69307,
#69308,#69309,#69310,#69311,#69312,#69313,#69314,#69315,#69316,#69317,#69318,
#69319,#69320,#69321,#69322,#69323,#69324,#69325,#69326,#69327,#69328,#69329,
#69330,#69331,#69332,#69333,#69334,#69335,#69336,#69337,#69338,#69339,#69340,
#69341,#69342,#69343,#69344,#69345,#69346,#69347,#69348,#69349,#69350,#69351,
#69352,#69353,#69354,#69355,#69356,#69357,#69358,#69359,#69360,#69361,#69362,
#69363,#69364,#69365,#69366,#69367,#69368,#69369,#69370,#69371,#69372,#69373,
#69374,#69375,#69376,#69377,#69378,#69379,#69380,#69381,#69382,#69383,#69384,
#69385,#69386,#69387,#69388,#69389,#69390,#69391,#69392,#69393,#69394,#69395,
#69396,#69397,#69398,#69399,#69400,#69401,#69402,#69403,#69404,#69405,#69406,
#69407,#69408,#69409,#69410,#69411,#69412,#69413,#69414,#69415,#69416,#69417,
#69418,#69419,#69420,#69421,#69422,#69423,#69424,#69425,#69426,#69427,#69428,
#69429,#69430,#69431,#69432,#69433,#69434,#69435,#69436,#69437,#69438,#69439,
#69440,#69441,#69442,#69443,#69444,#69445,#69446,#69447,#69448,#69449,#69450,
#69451,#69452,#69453,#69454,#69455,#69456,#69457,#69458,#69459,#69460,#69461,
#69462,#69463,#69464,#69465,#69466,#69467,#69468,#69469,#69470,#69471,#69472,
#69473,#69474,#69475,#69476,#69477,#69478,#69479,#69480,#69481,#69482,#69483,
#69484,#69485,#69486,#69487,#69488,#69489,#69490,#69491,#69492,#69493,#69494,
#69495,#69496,#69497,#69498,#69499,#69500,#69501,#69502,#69503,#69504,#69505,
#69506,#69507,#69508,#69509,#69510,#69511,#69512,#69513,#69514,#69515,#69516,
#69517,#69518,#69519,#69520,#69521,#69522,#69523,#69524,#69525,#69526,#69527,
#69528,#69529,#69530,#69531,#69532,#69533,#69534,#69535,#69536,#69537,#69538,
#69539,#69540,#69541,#69542,#69543,#69544,#69545,#69546,#69547,#69548,#69549,
#69550,#69551,#69552,#69553,#69554,#69555,#69556,#69557,#69558,#69559,#69560,
#69561,#69562,#69563,#69564,#69565,#69566,#69567,#69568,#69569,#69570,#69571,
#69572,#69573,#69574,#69575,#69576,#69577,#69578,#69579,#69580,#69581,#69582,
#69583,#69584,#69585,#69586,#69587,#69588,#69589,#69590,#69591,#69592,#69593,
#69594,#69595,#69596,#69597,#69598,#69599,#69600,#69601,#69602,#69603,#69604,
#69605,#69606,#69607,#69608,#69609,#69610,#69611,#69612,#69613,#69614,#69615,
#69616,#69617,#69618,#69619,#69620,#69621,#69622,#69623,#69624,#69625,#69626,
#69627,#69628,#69629,#69630,#69631,#69632,#69633,#69634,#69635,#69636,#69637,
#69638,#69639,#69640,#69641,#69642,#69643,#69644,#69645,#69646,#69647,#69648,
#69649,#69650,#69651,#69652,#69653,#69654,#69655,#69656,#69657,#69658,#69659,
#69660,#69661,#69662,#69663,#69664,#69665,#69666,#69667,#69668,#69669,#69670,
#69671,#69672,#69673,#69674,#69675,#69676,#69677,#69678,#69679,#69680,#69681,
#69682,#69683,#69684,#69685,#69686,#69687,#69688,#69689,#69690,#69691,#69692,
#69693,#69694,#69695,#69696,#69697,#69698,#69699,#69700,#69701,#69702,#69703,
#69704,#69705,#69706,#69707,#69708,#69709,#69710,#69711,#69712,#69713,#69714,
#69715,#69716,#69717,#69718,#69719,#69720,#69721,#69722,#69723,#69724,#69725,
#69726,#69727,#69728,#69729,#69730,#69731,#69732,#69733,#69734,#69735,#69736,
#69737,#69738,#69739,#69740,#69741,#69742,#69743,#69744,#69745,#69746,#69747,
#69748,#69749,#69750,#69751,#69752,#69753,#69754,#69755,#69756,#69757,#69758,
#69759,#69760,#69761,#69762,#69763,#69764,#69765,#69766,#69767,#69768,#69769,
#69770,#69771,#69772,#69773,#69774,#69775,#69776,#69777,#69778,#69779,#69780,
#69781,#69782,#69783,#69784,#69785,#69786,#69787,#69788,#69789,#69790,#69791,
#69792,#69793,#69794,#69795,#69796,#69797,#69798,#69799,#69800,#69801,#69802,
#69803,#69804,#69805,#69806,#69807,#69808,#69809,#69810,#69811,#69812,#69813,
#69814,#69815,#69816,#69817,#69818,#69819,#69820,#69821,#69822,#69823,#69824,
#69825,#69826,#69827,#69828,#69829,#69830,#69831,#69832,#69833,#69834,#69835,
#69836,#69837,#69838,#69839,#69840,#69841,#69842,#69843,#69844,#69845,#69846,
#69847,#69848,#69849,#69850,#69851,#69852,#69853,#69854,#69855,#69856,#69857,
#69858,#69859,#69860,#69861,#69862,#69863,#69864,#69865,#69866,#69867,#69868,
#69869,#69870,#69871,#69872,#69873,#69874,#69875,#69876,#69877,#69878,#69879,
#69880,#69881,#69882,#69883,#69884,#69885,#69886,#69887,#69888,#69889,#69890,
#69891,#69892,#69893,#69894,#69895,#69896,#69897,#69898,#69899,#69900,#69901,
#69902,#69903,#69904,#69905,#69906,#69907,#69908,#69909,#69910,#69911,#69912,
#69913,#69914,#69915,#69916,#69917,#69918,#69919,#69920,#69921,#69922,#69923,
#69924,#69925,#69926,#69927,#69928,#69929,#69930,#69931,#69932,#69933,#69934,
#69935,#69936,#69937,#69938,#69939,#69940,#69941,#69942,#69943,#69944,#69945,
#69946,#69947,#69948,#69949,#69950,#69951,#69952,#69953,#69954,#69955,#69956,
#69957,#69958,#69959,#69960,#69961,#69962,#69963,#69964,#69965,#69966,#69967,
#69968,#69969,#69970,#69971,#69972,#69973,#69974,#69975,#69976,#69977,#69978,
#69979,#69980,#69981,#69982,#69983,#69984,#69985,#69986,#69987,#69988,#69989,
#69990,#69991,#69992,#69993,#69994,#69995,#69996,#69997,#69998,#69999,#70000,
#70001,#70002,#70003,#70004,#70005,#70006,#70007,#70008,#70009,#70010,#70011,
#70012,#70013,#70014,#70015,#70016,#70017,#70018,#70019,#70020,#70021,#70022,
#70023,#70024,#70025,#70026,#70027,#70028,#70029,#70030,#70031,#70032,#70033,
#70034,#70035,#70036,#70037,#70038,#70039,#70040,#70041,#70042,#70043,#70044,
#70045,#70046,#70047,#70048,#70049,#70050,#70051,#70052,#70053,#70054,#70055,
#70056,#70057,#70058,#70059,#70060,#70061,#70062,#70063,#70064,#70065,#70066,
#70067,#70068,#70069,#70070,#70071,#70072,#70073,#70074,#70075,#70076,#70077,
#70078,#70079,#70080,#70081,#70082,#70083,#70084,#70085,#70086,#70087,#70088,
#70089,#70090,#70091,#70092,#70093,#70094,#70095,#70096,#70097,#70098,#70099,
#70100,#70101,#70102,#70103,#70104,#70105,#70106,#70107,#70108,#70109,#70110,
#70111,#70112,#70113,#70114,#70115,#70116,#70117,#70118,#70119,#70120,#70121,
#70122,#70123,#70124,#70125,#70126,#70127,#70128,#70129,#70130,#70131,#70132,
#70133,#70134,#70135,#70136,#70137,#70138,#70139,#70140,#70141,#70142,#70143,
#70144,#70145,#70146,#70147,#70148,#70149,#70150,#70151,#70152,#70153,#70154,
#70155,#70156,#70157,#70158,#70159,#70160,#70161,#70162,#70163,#70164,#70165,
#70166,#70167,#70168,#70169,#70170,#70171,#70172,#70173,#70174,#70175,#70176,
#70177,#70178,#70179,#70180,#70181,#70182,#70183,#70184,#70185,#70186,#70187,
#70188,#70189,#70190,#70191,#70192,#70193,#70194,#70195,#70196,#70197,#70198,
#70199,#70200,#70201,#70202,#70203,#70204,#70205,#70206,#70207,#70208,#70209,
#70210,#70211,#70212,#70213,#70214,#70215,#70216,#70217,#70218,#70219,#70220,
#70221,#70222,#70223,#70224,#70225,#70226,#70227,#70228,#70229,#70230,#70231,
#70232,#70233,#70234,#70235,#70236,#70237,#70238,#70239,#70240,#70241,#70242,
#70243,#70244,#70245,#70246,#70247,#70248,#70249,#70250,#70251,#70252,#70253,
#70254,#70255,#70256,#70257,#70258,#70259,#70260,#70261,#70262,#70263,#70264,
#70265,#70266,#70267,#70268,#70269,#70270,#70271,#70272,#70273,#70274,#70275,
#70276,#70277,#70278,#70279,#70280,#70281,#70282,#70283,#70284,#70285,#70286,
#70287,#70288,#70289,#70290,#70291,#70292,#70293,#70294,#70295,#70296,#70297,
#70298,#70299,#70300,#70301,#70302,#70303,#70304,#70305,#70306,#70307,#70308,
#70309,#70310,#70311,#70312,#70313,#70314,#70315,#70316,#70317,#70318,#70319,
#70320,#70321,#70322,#70323,#70324,#70325,#70326,#70327,#70328,#70329,#70330,
#70331,#70332,#70333,#70334,#70335,#70336,#70337,#70338,#70339,#70340,#70341,
#70342,#70343,#70344,#70345,#70346,#70347,#70348,#70349,#70350,#70351,#70352,
#70353,#70354,#70355,#70356,#70357,#70358,#70359,#70360,#70361,#70362,#70363,
#70364,#70365,#70366,#70367,#70368,#70369,#70370,#70371,#70372,#70373,#70374,
#70375,#70376,#70377,#70378,#70379,#70380,#70381,#70382,#70383,#70384,#70385,
#70386,#70387,#70388,#70389,#70390,#70391,#70392,#70393,#70394,#70395,#70396,
#70397,#70398,#70399,#70400,#70401,#70402,#70403,#70404,#70405,#70406,#70407,
#70408,#70409,#70410,#70411,#70412,#70413,#70414,#70415,#70416,#70417,#70418,
#70419,#70420,#70421,#70422,#70423,#70424,#70425,#70426,#70427,#70428,#70429,
#70430,#70431,#70432,#70433,#70434,#70435,#70436,#70437,#70438,#70439,#70440,
#70441,#70442,#70443,#70444,#70445,#70446,#70447,#70448,#70449,#70450,#70451,
#70452,#70453,#70454,#70455,#70456,#70457,#70458,#70459,#70460,#70461,#70462,
#70463,#70464,#70465,#70466,#70467,#70468,#70469,#70470,#70471,#70472,#70473,
#70474,#70475,#70476,#70477,#70478,#70479,#70480,#70481,#70482,#70483,#70484,
#70485,#70486,#70487,#70488,#70489,#70490,#70491,#70492,#70493,#70494,#70495,
#70496,#70497,#70498,#70499,#70500,#70501,#70502,#70503,#70504,#70505,#70506,
#70507,#70508,#70509,#70510,#70511,#70512,#70513,#70514,#70515,#70516,#70517,
#70518,#70519,#70520,#70521,#70522,#70523,#70524,#70525,#70526,#70527,#70528,
#70529,#70530,#70531,#70532,#70533,#70534,#70535,#70536,#70537,#70538,#70539,
#70540,#70541,#70542,#70543,#70544,#70545,#70546,#70547,#70548,#70549,#70550,
#70551,#70552,#70553,#70554,#70555,#70556,#70557,#70558,#70559,#70560,#70561,
#70562,#70563,#70564,#70565,#70566,#70567,#70568,#70569,#70570,#70571,#70572,
#70573,#70574,#70575,#70576,#70577,#70578,#70579,#70580,#70581,#70582,#70583,
#70584,#70585,#70586,#70587,#70588,#70589,#70590,#70591,#70592,#70593,#70594,
#70595,#70596,#70597,#70598,#70599,#70600,#70601,#70602,#70603,#70604,#70605,
#70606,#70607,#70608,#70609,#70610,#70611,#70612,#70613,#70614,#70615,#70616,
#70617,#70618,#70619,#70620,#70621,#70622,#70623,#70624,#70625,#70626,#70627,
#70628,#70629,#70630,#70631,#70632,#70633,#70634,#70635,#70636,#70637,#70638,
#70639,#70640,#70641,#70642,#70643,#70644,#70645,#70646,#70647,#70648,#70649,
#70650,#70651,#70652,#70653,#70654,#70655,#70656,#70657,#70658,#70659,#70660,
#70661,#70662,#70663,#70664,#70665,#70666,#70667,#70668,#70669,#70670,#70671,
#70672,#70673,#70674,#70675,#70676,#70677,#70678,#70679,#70680,#70681,#70682,
#70683,#70684,#70685,#70686,#70687,#70688,#70689,#70690,#70691,#70692,#70693,
#70694,#70695,#70696,#70697,#70698,#70699,#70700,#70701,#70702,#70703,#70704,
#70705,#70706,#70707,#70708,#70709,#70710,#70711,#70712,#70713,#70714,#70715,
#70716,#70717,#70718,#70719,#70720,#70721,#70722,#70723,#70724,#70725,#70726,
#70727,#70728,#70729,#70730,#70731,#70732,#70733,#70734,#70735,#70736,#70737,
#70738,#70739,#70740,#70741,#70742,#70743,#70744,#70745,#70746,#70747,#70748,
#70749,#70750,#70751,#70752,#70753,#70754,#70755,#70756,#70757,#70758,#70759,
#70760,#70761,#70762,#70763,#70764,#70765,#70766,#70767,#70768,#70769,#70770,
#70771,#70772,#70773,#70774,#70775,#70776,#70777,#70778,#70779,#70780,#70781,
#70782,#70783,#70784,#70785,#70786,#70787,#70788,#70789,#70790,#70791,#70792,
#70793,#70794,#70795,#70796,#70797,#70798,#70799,#70800,#70801,#70802,#70803,
#70804,#70805,#70806,#70807,#70808,#70809,#70810,#70811,#70812,#70813,#70814,
#70815,#70816,#70817,#70818,#70819,#70820,#70821,#70822,#70823,#70824,#70825,
#70826,#70827,#70828,#70829,#70830,#70831,#70832,#70833,#70834,#70835,#70836,
#70837,#70838,#70839,#70840,#70841,#70842,#70843,#70844,#70845,#70846,#70847,
#70848,#70849,#70850,#70851,#70852,#70853,#70854,#70855,#70856,#70857,#70858,
#70859,#70860,#70861,#70862,#70863,#70864,#70865,#70866,#70867,#70868,#70869,
#70870,#70871,#70872,#70873,#70874,#70875,#70876,#70877,#70878,#70879,#70880,
#70881,#70882,#70883,#70884,#70885,#70886,#70887,#70888,#70889,#70890,#70891,
#70892,#70893,#70894,#70895,#70896,#70897,#70898,#70899,#70900,#70901,#70902,
#70903,#70904,#70905,#70906,#70907,#70908,#70909,#70910,#70911,#70912,#70913,
#70914,#70915,#70916,#70917,#70918,#70919,#70920,#70921,#70922,#70923,#70924,
#70925,#70926,#70927,#70928,#70929,#70930,#70931,#70932,#70933,#70934,#70935,
#70936,#70937,#70938,#70939,#70940,#70941,#70942,#70943,#70944,#70945,#70946,
#70947,#70948,#70949,#70950,#70951,#70952,#70953,#70954,#70955,#70956,#70957,
#70958,#70959,#70960,#70961,#70962,#70963,#70964,#70965,#70966,#70967,#70968,
#70969,#70970,#70971,#70972,#70973,#70974,#70975,#70976,#70977,#70978,#70979,
#70980,#70981,#70982,#70983,#70984,#70985,#70986,#70987,#70988,#70989,#70990,
#70991,#70992,#70993,#70994,#70995,#70996,#70997,#70998,#70999,#71000,#71001,
#71002,#71003,#71004,#71005,#71006,#71007,#71008,#71009,#71010,#71011,#71012,
#71013,#71014,#71015,#71016,#71017,#71018,#71019,#71020,#71021,#71022,#71023,
#71024,#71025,#71026,#71027,#71028,#71029,#71030,#71031,#71032,#71033,#71034,
#71035,#71036,#71037,#71038,#71039,#71040,#71041,#71042,#71043,#71044,#71045,
#71046,#71047,#71048,#71049,#71050,#71051,#71052,#71053,#71054,#71055,#71056,
#71057,#71058,#71059,#71060,#71061,#71062,#71063,#71064,#71065,#71066,#71067,
#71068,#71069,#71070,#71071,#71072,#71073,#71074,#71075,#71076,#71077,#71078,
#71079,#71080,#71081,#71082,#71083,#71084,#71085,#71086,#71087,#71088,#71089,
#71090,#71091,#71092,#71093,#71094,#71095,#71096,#71097,#71098,#71099,#71100,
#71101,#71102,#71103,#71104,#71105,#71106,#71107,#71108,#71109,#71110,#71111,
#71112,#71113,#71114,#71115,#71116,#71117,#71118,#71119,#71120,#71121,#71122,
#71123,#71124,#71125,#71126,#71127,#71128,#71129,#71130,#71131,#71132,#71133,
#71134,#71135,#71136,#71137,#71138,#71139,#71140,#71141,#71142,#71143,#71144,
#71145,#71146,#71147,#71148,#71149,#71150,#71151,#71152,#71153,#71154,#71155,
#71156,#71157,#71158,#71159,#71160,#71161,#71162,#71163,#71164,#71165,#71166,
#71167,#71168,#71169,#71170,#71171,#71172,#71173,#71174,#71175,#71176,#71177,
#71178,#71179,#71180,#71181,#71182,#71183,#71184,#71185,#71186,#71187,#71188,
#71189,#71190,#71191,#71192,#71193,#71194,#71195,#71196,#71197,#71198,#71199,
#71200,#71201,#71202,#71203,#71204,#71205,#71206,#71207,#71208,#71209,#71210,
#71211,#71212,#71213,#71214,#71215,#71216,#71217,#71218,#71219,#71220,#71221,
#71222,#71223,#71224,#71225,#71226,#71227,#71228,#71229,#71230,#71231,#71232,
#71233,#71234,#71235,#71236,#71237,#71238,#71239,#71240,#71241,#71242,#71243,
#71244,#71245,#71246,#71247,#71248,#71249,#71250,#71251,#71252,#71253,#71254,
#71255,#71256,#71257,#71258,#71259,#71260,#71261,#71262,#71263,#71264,#71265,
#71266,#71267,#71268,#71269,#71270,#71271,#71272,#71273,#71274,#71275,#71276,
#71277,#71278,#71279,#71280,#71281,#71282,#71283,#71284,#71285,#71286,#71287,
#71288,#71289,#71290,#71291,#71292,#71293,#71294,#71295,#71296,#71297,#71298,
#71299,#71300,#71301,#71302,#71303,#71304,#71305,#71306,#71307,#71308,#71309,
#71310,#71311,#71312,#71313,#71314,#71315,#71316,#71317,#71318,#71319,#71320,
#71321,#71322,#71323,#71324,#71325,#71326,#71327,#71328,#71329,#71330,#71331,
#71332,#71333,#71334));
#71399=CLOSED_SHELL('',(#71335,#71336,#71337,#71338,#71339,#71340,#71341,
#71342,#71343,#71344,#71345,#71346,#71347,#71348,#71349,#71350,#71351));
#71400=CLOSED_SHELL('',(#71354,#71355,#71356,#71357,#71358,#71359,#71360,
#71361,#71362,#71363,#71364,#71365,#71366,#71367,#71368,#71369,#71370,#71371,
#71372,#71373,#71374,#71375,#71376));
#71401=CLOSED_SHELL('',(#71377,#71378,#71379,#71380,#71381,#71382,#71383,
#71384,#71385,#71386,#71387,#71388));
#71402=CLOSED_SHELL('',(#71389,#71390,#71391,#71392,#71393,#71394));
#71403=CLOSED_SHELL('',(#71395,#71396,#71397));
#71404=DERIVED_UNIT_ELEMENT(#71416,1.);
#71405=DERIVED_UNIT_ELEMENT(#170252,-3.);
#71406=DERIVED_UNIT_ELEMENT(#71416,1.);
#71407=DERIVED_UNIT_ELEMENT(#170252,-3.);
#71408=DERIVED_UNIT_ELEMENT(#71416,1.);
#71409=DERIVED_UNIT_ELEMENT(#170252,-3.);
#71410=DERIVED_UNIT_ELEMENT(#71416,1.);
#71411=DERIVED_UNIT_ELEMENT(#170252,-3.);
#71412=DERIVED_UNIT_ELEMENT(#71416,1.);
#71413=DERIVED_UNIT_ELEMENT(#170252,-3.);
#71414=DERIVED_UNIT_ELEMENT(#71416,1.);
#71415=DERIVED_UNIT_ELEMENT(#170252,-3.);
#71416=(
MASS_UNIT()
NAMED_UNIT(*)
SI_UNIT(.KILO.,.GRAM.)
);
#71417=DERIVED_UNIT((#71404,#71405));
#71418=DERIVED_UNIT((#71406,#71407));
#71419=DERIVED_UNIT((#71408,#71409));
#71420=DERIVED_UNIT((#71410,#71411));
#71421=DERIVED_UNIT((#71412,#71413));
#71422=DERIVED_UNIT((#71414,#71415));
#71423=MEASURE_REPRESENTATION_ITEM('density measure',
POSITIVE_RATIO_MEASURE(7850.),#71417);
#71424=MEASURE_REPRESENTATION_ITEM('density measure',
POSITIVE_RATIO_MEASURE(7850.),#71418);
#71425=MEASURE_REPRESENTATION_ITEM('density measure',
POSITIVE_RATIO_MEASURE(7850.),#71419);
#71426=MEASURE_REPRESENTATION_ITEM('density measure',
POSITIVE_RATIO_MEASURE(7850.),#71420);
#71427=MEASURE_REPRESENTATION_ITEM('density measure',
POSITIVE_RATIO_MEASURE(7850.),#71421);
#71428=MEASURE_REPRESENTATION_ITEM('density measure',
POSITIVE_RATIO_MEASURE(7850.),#71422);
#71429=PROPERTY_DEFINITION_REPRESENTATION(#71459,#71441);
#71430=PROPERTY_DEFINITION_REPRESENTATION(#71460,#71442);
#71431=PROPERTY_DEFINITION_REPRESENTATION(#71461,#71443);
#71432=PROPERTY_DEFINITION_REPRESENTATION(#71462,#71444);
#71433=PROPERTY_DEFINITION_REPRESENTATION(#71463,#71445);
#71434=PROPERTY_DEFINITION_REPRESENTATION(#71464,#71446);
#71435=PROPERTY_DEFINITION_REPRESENTATION(#71465,#71447);
#71436=PROPERTY_DEFINITION_REPRESENTATION(#71466,#71448);
#71437=PROPERTY_DEFINITION_REPRESENTATION(#71467,#71449);
#71438=PROPERTY_DEFINITION_REPRESENTATION(#71468,#71450);
#71439=PROPERTY_DEFINITION_REPRESENTATION(#71469,#71451);
#71440=PROPERTY_DEFINITION_REPRESENTATION(#71470,#71452);
#71441=REPRESENTATION('material name',(#71453),#170244);
#71442=REPRESENTATION('density',(#71423),#170244);
#71443=REPRESENTATION('material name',(#71454),#170245);
#71444=REPRESENTATION('density',(#71424),#170245);
#71445=REPRESENTATION('material name',(#71455),#170246);
#71446=REPRESENTATION('density',(#71425),#170246);
#71447=REPRESENTATION('material name',(#71456),#170247);
#71448=REPRESENTATION('density',(#71426),#170247);
#71449=REPRESENTATION('material name',(#71457),#170248);
#71450=REPRESENTATION('density',(#71427),#170248);
#71451=REPRESENTATION('material name',(#71458),#170249);
#71452=REPRESENTATION('density',(#71428),#170249);
#71453=DESCRIPTIVE_REPRESENTATION_ITEM('Steel','Steel');
#71454=DESCRIPTIVE_REPRESENTATION_ITEM('Steel','Steel');
#71455=DESCRIPTIVE_REPRESENTATION_ITEM('Steel','Steel');
#71456=DESCRIPTIVE_REPRESENTATION_ITEM('Steel','Steel');
#71457=DESCRIPTIVE_REPRESENTATION_ITEM('Steel','Steel');
#71458=DESCRIPTIVE_REPRESENTATION_ITEM('Steel','Steel');
#71459=PROPERTY_DEFINITION('material property','material name',#170284);
#71460=PROPERTY_DEFINITION('material property','density of part',#170284);
#71461=PROPERTY_DEFINITION('material property','material name',#170285);
#71462=PROPERTY_DEFINITION('material property','density of part',#170285);
#71463=PROPERTY_DEFINITION('material property','material name',#170286);
#71464=PROPERTY_DEFINITION('material property','density of part',#170286);
#71465=PROPERTY_DEFINITION('material property','material name',#170287);
#71466=PROPERTY_DEFINITION('material property','density of part',#170287);
#71467=PROPERTY_DEFINITION('material property','material name',#170288);
#71468=PROPERTY_DEFINITION('material property','density of part',#170288);
#71469=PROPERTY_DEFINITION('material property','material name',#170289);
#71470=PROPERTY_DEFINITION('material property','density of part',#170289);
#71471=AXIS2_PLACEMENT_3D('',#92435,#77763,#77764);
#71472=AXIS2_PLACEMENT_3D('',#92436,#77765,#77766);
#71473=AXIS2_PLACEMENT_3D('',#92437,#77767,#77768);
#71474=AXIS2_PLACEMENT_3D('',#92460,#77770,#77771);
#71475=AXIS2_PLACEMENT_3D('',#92462,#77772,#77773);
#71476=AXIS2_PLACEMENT_3D('',#92500,#77774,#77775);
#71477=AXIS2_PLACEMENT_3D('',#92502,#77776,#77777);
#71478=AXIS2_PLACEMENT_3D('',#92540,#77778,#77779);
#71479=AXIS2_PLACEMENT_3D('',#92542,#77780,#77781);
#71480=AXIS2_PLACEMENT_3D('',#92580,#77782,#77783);
#71481=AXIS2_PLACEMENT_3D('',#92582,#77784,#77785);
#71482=AXIS2_PLACEMENT_3D('',#92620,#77786,#77787);
#71483=AXIS2_PLACEMENT_3D('',#92622,#77788,#77789);
#71484=AXIS2_PLACEMENT_3D('',#92660,#77790,#77791);
#71485=AXIS2_PLACEMENT_3D('',#92662,#77792,#77793);
#71486=AXIS2_PLACEMENT_3D('',#92700,#77794,#77795);
#71487=AXIS2_PLACEMENT_3D('',#92702,#77796,#77797);
#71488=AXIS2_PLACEMENT_3D('',#92740,#77798,#77799);
#71489=AXIS2_PLACEMENT_3D('',#92742,#77800,#77801);
#71490=AXIS2_PLACEMENT_3D('',#92780,#77802,#77803);
#71491=AXIS2_PLACEMENT_3D('',#92782,#77804,#77805);
#71492=AXIS2_PLACEMENT_3D('',#92820,#77806,#77807);
#71493=AXIS2_PLACEMENT_3D('',#92822,#77808,#77809);
#71494=AXIS2_PLACEMENT_3D('',#92860,#77810,#77811);
#71495=AXIS2_PLACEMENT_3D('',#92862,#77812,#77813);
#71496=AXIS2_PLACEMENT_3D('',#92900,#77814,#77815);
#71497=AXIS2_PLACEMENT_3D('',#92902,#77816,#77817);
#71498=AXIS2_PLACEMENT_3D('',#92940,#77818,#77819);
#71499=AXIS2_PLACEMENT_3D('',#92942,#77820,#77821);
#71500=AXIS2_PLACEMENT_3D('',#92980,#77822,#77823);
#71501=AXIS2_PLACEMENT_3D('',#92982,#77824,#77825);
#71502=AXIS2_PLACEMENT_3D('',#93020,#77826,#77827);
#71503=AXIS2_PLACEMENT_3D('',#93022,#77828,#77829);
#71504=AXIS2_PLACEMENT_3D('',#93060,#77830,#77831);
#71505=AXIS2_PLACEMENT_3D('',#93062,#77832,#77833);
#71506=AXIS2_PLACEMENT_3D('',#93100,#77834,#77835);
#71507=AXIS2_PLACEMENT_3D('',#93102,#77836,#77837);
#71508=AXIS2_PLACEMENT_3D('',#93140,#77838,#77839);
#71509=AXIS2_PLACEMENT_3D('',#93142,#77840,#77841);
#71510=AXIS2_PLACEMENT_3D('',#93180,#77842,#77843);
#71511=AXIS2_PLACEMENT_3D('',#93182,#77844,#77845);
#71512=AXIS2_PLACEMENT_3D('',#93220,#77846,#77847);
#71513=AXIS2_PLACEMENT_3D('',#93222,#77848,#77849);
#71514=AXIS2_PLACEMENT_3D('',#93260,#77850,#77851);
#71515=AXIS2_PLACEMENT_3D('',#93262,#77852,#77853);
#71516=AXIS2_PLACEMENT_3D('',#93300,#77854,#77855);
#71517=AXIS2_PLACEMENT_3D('',#93302,#77856,#77857);
#71518=AXIS2_PLACEMENT_3D('',#93340,#77858,#77859);
#71519=AXIS2_PLACEMENT_3D('',#93342,#77860,#77861);
#71520=AXIS2_PLACEMENT_3D('',#93380,#77862,#77863);
#71521=AXIS2_PLACEMENT_3D('',#93382,#77864,#77865);
#71522=AXIS2_PLACEMENT_3D('',#93420,#77866,#77867);
#71523=AXIS2_PLACEMENT_3D('',#93422,#77868,#77869);
#71524=AXIS2_PLACEMENT_3D('',#93460,#77870,#77871);
#71525=AXIS2_PLACEMENT_3D('',#93462,#77872,#77873);
#71526=AXIS2_PLACEMENT_3D('',#93500,#77874,#77875);
#71527=AXIS2_PLACEMENT_3D('',#93502,#77876,#77877);
#71528=AXIS2_PLACEMENT_3D('',#93540,#77878,#77879);
#71529=AXIS2_PLACEMENT_3D('',#93542,#77880,#77881);
#71530=AXIS2_PLACEMENT_3D('',#93580,#77882,#77883);
#71531=AXIS2_PLACEMENT_3D('',#93582,#77884,#77885);
#71532=AXIS2_PLACEMENT_3D('',#93592,#77887,#77888);
#71533=AXIS2_PLACEMENT_3D('',#93604,#77889,#77890);
#71534=AXIS2_PLACEMENT_3D('',#93606,#77891,#77892);
#71535=AXIS2_PLACEMENT_3D('',#93609,#77894,#77895);
#71536=AXIS2_PLACEMENT_3D('',#93610,#77896,#77897);
#71537=AXIS2_PLACEMENT_3D('',#93622,#77898,#77899);
#71538=AXIS2_PLACEMENT_3D('',#93624,#77900,#77901);
#71539=AXIS2_PLACEMENT_3D('',#93627,#77903,#77904);
#71540=AXIS2_PLACEMENT_3D('',#93628,#77905,#77906);
#71541=AXIS2_PLACEMENT_3D('',#93631,#77907,#77908);
#71542=AXIS2_PLACEMENT_3D('',#93634,#77910,#77911);
#71543=AXIS2_PLACEMENT_3D('',#93635,#77912,#77913);
#71544=AXIS2_PLACEMENT_3D('',#93636,#77914,#77915);
#71545=AXIS2_PLACEMENT_3D('',#93639,#77917,#77918);
#71546=AXIS2_PLACEMENT_3D('',#93640,#77919,#77920);
#71547=AXIS2_PLACEMENT_3D('',#93650,#77921,#77922);
#71548=AXIS2_PLACEMENT_3D('',#93652,#77923,#77924);
#71549=AXIS2_PLACEMENT_3D('',#93686,#77925,#77926);
#71550=AXIS2_PLACEMENT_3D('',#93688,#77927,#77928);
#71551=AXIS2_PLACEMENT_3D('',#93722,#77929,#77930);
#71552=AXIS2_PLACEMENT_3D('',#93724,#77931,#77932);
#71553=AXIS2_PLACEMENT_3D('',#93758,#77933,#77934);
#71554=AXIS2_PLACEMENT_3D('',#93760,#77935,#77936);
#71555=AXIS2_PLACEMENT_3D('',#93794,#77937,#77938);
#71556=AXIS2_PLACEMENT_3D('',#93796,#77939,#77940);
#71557=AXIS2_PLACEMENT_3D('',#93830,#77941,#77942);
#71558=AXIS2_PLACEMENT_3D('',#93832,#77943,#77944);
#71559=AXIS2_PLACEMENT_3D('',#93866,#77945,#77946);
#71560=AXIS2_PLACEMENT_3D('',#93868,#77947,#77948);
#71561=AXIS2_PLACEMENT_3D('',#93902,#77949,#77950);
#71562=AXIS2_PLACEMENT_3D('',#93904,#77951,#77952);
#71563=AXIS2_PLACEMENT_3D('',#93938,#77953,#77954);
#71564=AXIS2_PLACEMENT_3D('',#93940,#77955,#77956);
#71565=AXIS2_PLACEMENT_3D('',#93974,#77957,#77958);
#71566=AXIS2_PLACEMENT_3D('',#93976,#77959,#77960);
#71567=AXIS2_PLACEMENT_3D('',#94010,#77961,#77962);
#71568=AXIS2_PLACEMENT_3D('',#94012,#77963,#77964);
#71569=AXIS2_PLACEMENT_3D('',#94046,#77965,#77966);
#71570=AXIS2_PLACEMENT_3D('',#94048,#77967,#77968);
#71571=AXIS2_PLACEMENT_3D('',#94082,#77969,#77970);
#71572=AXIS2_PLACEMENT_3D('',#94084,#77971,#77972);
#71573=AXIS2_PLACEMENT_3D('',#94118,#77973,#77974);
#71574=AXIS2_PLACEMENT_3D('',#94120,#77975,#77976);
#71575=AXIS2_PLACEMENT_3D('',#94154,#77977,#77978);
#71576=AXIS2_PLACEMENT_3D('',#94156,#77979,#77980);
#71577=AXIS2_PLACEMENT_3D('',#94170,#77982,#77983);
#71578=AXIS2_PLACEMENT_3D('',#94198,#77984,#77985);
#71579=AXIS2_PLACEMENT_3D('',#94200,#77986,#77987);
#71580=AXIS2_PLACEMENT_3D('',#94234,#77988,#77989);
#71581=AXIS2_PLACEMENT_3D('',#94236,#77990,#77991);
#71582=AXIS2_PLACEMENT_3D('',#94270,#77992,#77993);
#71583=AXIS2_PLACEMENT_3D('',#94272,#77994,#77995);
#71584=AXIS2_PLACEMENT_3D('',#94306,#77996,#77997);
#71585=AXIS2_PLACEMENT_3D('',#94308,#77998,#77999);
#71586=AXIS2_PLACEMENT_3D('',#94342,#78000,#78001);
#71587=AXIS2_PLACEMENT_3D('',#94344,#78002,#78003);
#71588=AXIS2_PLACEMENT_3D('',#94378,#78004,#78005);
#71589=AXIS2_PLACEMENT_3D('',#94380,#78006,#78007);
#71590=AXIS2_PLACEMENT_3D('',#94414,#78008,#78009);
#71591=AXIS2_PLACEMENT_3D('',#94416,#78010,#78011);
#71592=AXIS2_PLACEMENT_3D('',#94450,#78012,#78013);
#71593=AXIS2_PLACEMENT_3D('',#94452,#78014,#78015);
#71594=AXIS2_PLACEMENT_3D('',#94486,#78016,#78017);
#71595=AXIS2_PLACEMENT_3D('',#94488,#78018,#78019);
#71596=AXIS2_PLACEMENT_3D('',#94522,#78020,#78021);
#71597=AXIS2_PLACEMENT_3D('',#94524,#78022,#78023);
#71598=AXIS2_PLACEMENT_3D('',#94558,#78024,#78025);
#71599=AXIS2_PLACEMENT_3D('',#94560,#78026,#78027);
#71600=AXIS2_PLACEMENT_3D('',#94594,#78028,#78029);
#71601=AXIS2_PLACEMENT_3D('',#94596,#78030,#78031);
#71602=AXIS2_PLACEMENT_3D('',#94630,#78032,#78033);
#71603=AXIS2_PLACEMENT_3D('',#94632,#78034,#78035);
#71604=AXIS2_PLACEMENT_3D('',#94666,#78036,#78037);
#71605=AXIS2_PLACEMENT_3D('',#94668,#78038,#78039);
#71606=AXIS2_PLACEMENT_3D('',#94693,#78040,#78041);
#71607=AXIS2_PLACEMENT_3D('',#94696,#78042,#78043);
#71608=AXIS2_PLACEMENT_3D('',#94698,#78044,#78045);
#71609=AXIS2_PLACEMENT_3D('',#94714,#78046,#78047);
#71610=AXIS2_PLACEMENT_3D('',#94726,#78048,#78049);
#71611=AXIS2_PLACEMENT_3D('',#94742,#78050,#78051);
#71612=AXIS2_PLACEMENT_3D('',#94758,#78052,#78053);
#71613=AXIS2_PLACEMENT_3D('',#94760,#78054,#78055);
#71614=AXIS2_PLACEMENT_3D('',#94762,#78056,#78057);
#71615=AXIS2_PLACEMENT_3D('',#94763,#78058,#78059);
#71616=AXIS2_PLACEMENT_3D('',#94764,#78060,#78061);
#71617=AXIS2_PLACEMENT_3D('',#94781,#78062,#78063);
#71618=AXIS2_PLACEMENT_3D('',#94782,#78064,#78065);
#71619=AXIS2_PLACEMENT_3D('',#94783,#78066,#78067);
#71620=AXIS2_PLACEMENT_3D('',#94795,#78068,#78069);
#71621=AXIS2_PLACEMENT_3D('',#94811,#78070,#78071);
#71622=AXIS2_PLACEMENT_3D('',#94823,#78072,#78073);
#71623=AXIS2_PLACEMENT_3D('',#94839,#78074,#78075);
#71624=AXIS2_PLACEMENT_3D('',#94849,#78076,#78077);
#71625=AXIS2_PLACEMENT_3D('',#94851,#78078,#78079);
#71626=AXIS2_PLACEMENT_3D('',#94858,#78080,#78081);
#71627=AXIS2_PLACEMENT_3D('',#94861,#78082,#78083);
#71628=AXIS2_PLACEMENT_3D('',#94863,#78084,#78085);
#71629=AXIS2_PLACEMENT_3D('',#94865,#78086,#78087);
#71630=AXIS2_PLACEMENT_3D('',#94879,#78088,#78089);
#71631=AXIS2_PLACEMENT_3D('',#94880,#78090,#78091);
#71632=AXIS2_PLACEMENT_3D('',#94888,#78092,#78093);
#71633=AXIS2_PLACEMENT_3D('',#94889,#78094,#78095);
#71634=AXIS2_PLACEMENT_3D('',#94918,#78096,#78097);
#71635=AXIS2_PLACEMENT_3D('',#94926,#78098,#78099);
#71636=AXIS2_PLACEMENT_3D('',#94943,#78100,#78101);
#71637=AXIS2_PLACEMENT_3D('',#94944,#78102,#78103);
#71638=AXIS2_PLACEMENT_3D('',#94945,#78104,#78105);
#71639=AXIS2_PLACEMENT_3D('',#94955,#78106,#78107);
#71640=AXIS2_PLACEMENT_3D('',#94957,#78108,#78109);
#71641=AXIS2_PLACEMENT_3D('',#94970,#78110,#78111);
#71642=AXIS2_PLACEMENT_3D('',#94980,#78112,#78113);
#71643=AXIS2_PLACEMENT_3D('',#94982,#78114,#78115);
#71644=AXIS2_PLACEMENT_3D('',#94989,#78116,#78117);
#71645=AXIS2_PLACEMENT_3D('',#95006,#78118,#78119);
#71646=AXIS2_PLACEMENT_3D('',#95007,#78120,#78121);
#71647=AXIS2_PLACEMENT_3D('',#95008,#78122,#78123);
#71648=AXIS2_PLACEMENT_3D('',#95032,#78124,#78125);
#71649=AXIS2_PLACEMENT_3D('',#95033,#78126,#78127);
#71650=AXIS2_PLACEMENT_3D('',#95057,#78128,#78129);
#71651=AXIS2_PLACEMENT_3D('',#95070,#78130,#78131);
#71652=AXIS2_PLACEMENT_3D('',#95087,#78132,#78133);
#71653=AXIS2_PLACEMENT_3D('',#95095,#78134,#78135);
#71654=AXIS2_PLACEMENT_3D('',#95112,#78136,#78137);
#71655=AXIS2_PLACEMENT_3D('',#95113,#78138,#78139);
#71656=AXIS2_PLACEMENT_3D('',#95114,#78140,#78141);
#71657=AXIS2_PLACEMENT_3D('',#95130,#78142,#78143);
#71658=AXIS2_PLACEMENT_3D('',#95132,#78144,#78145);
#71659=AXIS2_PLACEMENT_3D('',#95139,#78146,#78147);
#71660=AXIS2_PLACEMENT_3D('',#95155,#78148,#78149);
#71661=AXIS2_PLACEMENT_3D('',#95176,#78150,#78151);
#71662=AXIS2_PLACEMENT_3D('',#95205,#78152,#78153);
#71663=AXIS2_PLACEMENT_3D('',#95206,#78154,#78155);
#71664=AXIS2_PLACEMENT_3D('',#95207,#78156,#78157);
#71665=AXIS2_PLACEMENT_3D('',#95231,#78158,#78159);
#71666=AXIS2_PLACEMENT_3D('',#95232,#78160,#78161);
#71667=AXIS2_PLACEMENT_3D('',#95250,#78162,#78163);
#71668=AXIS2_PLACEMENT_3D('',#95257,#78164,#78165);
#71669=AXIS2_PLACEMENT_3D('',#95267,#78166,#78167);
#71670=AXIS2_PLACEMENT_3D('',#95269,#78168,#78169);
#71671=AXIS2_PLACEMENT_3D('',#95282,#78170,#78171);
#71672=AXIS2_PLACEMENT_3D('',#95305,#78172,#78173);
#71673=AXIS2_PLACEMENT_3D('',#95313,#78174,#78175);
#71674=AXIS2_PLACEMENT_3D('',#95342,#78176,#78177);
#71675=AXIS2_PLACEMENT_3D('',#95343,#78178,#78179);
#71676=AXIS2_PLACEMENT_3D('',#95344,#78180,#78181);
#71677=AXIS2_PLACEMENT_3D('',#95360,#78182,#78183);
#71678=AXIS2_PLACEMENT_3D('',#95378,#78184,#78185);
#71679=AXIS2_PLACEMENT_3D('',#95407,#78186,#78187);
#71680=AXIS2_PLACEMENT_3D('',#95408,#78188,#78189);
#71681=AXIS2_PLACEMENT_3D('',#95409,#78190,#78191);
#71682=AXIS2_PLACEMENT_3D('',#95439,#78192,#78193);
#71683=AXIS2_PLACEMENT_3D('',#95440,#78194,#78195);
#71684=AXIS2_PLACEMENT_3D('',#95458,#78196,#78197);
#71685=AXIS2_PLACEMENT_3D('',#95465,#78198,#78199);
#71686=AXIS2_PLACEMENT_3D('',#95481,#78200,#78201);
#71687=AXIS2_PLACEMENT_3D('',#95494,#78202,#78203);
#71688=AXIS2_PLACEMENT_3D('',#95525,#78204,#78205);
#71689=AXIS2_PLACEMENT_3D('',#95554,#78206,#78207);
#71690=AXIS2_PLACEMENT_3D('',#95555,#78208,#78209);
#71691=AXIS2_PLACEMENT_3D('',#95556,#78210,#78211);
#71692=AXIS2_PLACEMENT_3D('',#95566,#78212,#78213);
#71693=AXIS2_PLACEMENT_3D('',#95589,#78214,#78215);
#71694=AXIS2_PLACEMENT_3D('',#95593,#78217,#78218);
#71695=AXIS2_PLACEMENT_3D('',#95617,#78219,#78220);
#71696=AXIS2_PLACEMENT_3D('',#95625,#78221,#78222);
#71697=AXIS2_PLACEMENT_3D('',#95627,#78224,#78225);
#71698=AXIS2_PLACEMENT_3D('',#95637,#78226,#78227);
#71699=AXIS2_PLACEMENT_3D('',#95638,#78228,#78229);
#71700=AXIS2_PLACEMENT_3D('',#95647,#78231,#78232);
#71701=AXIS2_PLACEMENT_3D('',#95665,#78233,#78234);
#71702=AXIS2_PLACEMENT_3D('',#95673,#78235,#78236);
#71703=AXIS2_PLACEMENT_3D('',#95675,#78238,#78239);
#71704=AXIS2_PLACEMENT_3D('',#95685,#78240,#78241);
#71705=AXIS2_PLACEMENT_3D('',#95686,#78242,#78243);
#71706=AXIS2_PLACEMENT_3D('',#95695,#78245,#78246);
#71707=AXIS2_PLACEMENT_3D('',#95713,#78247,#78248);
#71708=AXIS2_PLACEMENT_3D('',#95721,#78249,#78250);
#71709=AXIS2_PLACEMENT_3D('',#95723,#78252,#78253);
#71710=AXIS2_PLACEMENT_3D('',#95733,#78254,#78255);
#71711=AXIS2_PLACEMENT_3D('',#95734,#78256,#78257);
#71712=AXIS2_PLACEMENT_3D('',#95743,#78259,#78260);
#71713=AXIS2_PLACEMENT_3D('',#95761,#78261,#78262);
#71714=AXIS2_PLACEMENT_3D('',#95769,#78263,#78264);
#71715=AXIS2_PLACEMENT_3D('',#95771,#78266,#78267);
#71716=AXIS2_PLACEMENT_3D('',#95781,#78268,#78269);
#71717=AXIS2_PLACEMENT_3D('',#95782,#78270,#78271);
#71718=AXIS2_PLACEMENT_3D('',#95791,#78273,#78274);
#71719=AXIS2_PLACEMENT_3D('',#95809,#78275,#78276);
#71720=AXIS2_PLACEMENT_3D('',#95817,#78277,#78278);
#71721=AXIS2_PLACEMENT_3D('',#95819,#78280,#78281);
#71722=AXIS2_PLACEMENT_3D('',#95829,#78282,#78283);
#71723=AXIS2_PLACEMENT_3D('',#95830,#78284,#78285);
#71724=AXIS2_PLACEMENT_3D('',#95839,#78287,#78288);
#71725=AXIS2_PLACEMENT_3D('',#95857,#78289,#78290);
#71726=AXIS2_PLACEMENT_3D('',#95865,#78291,#78292);
#71727=AXIS2_PLACEMENT_3D('',#95867,#78294,#78295);
#71728=AXIS2_PLACEMENT_3D('',#95877,#78296,#78297);
#71729=AXIS2_PLACEMENT_3D('',#95878,#78298,#78299);
#71730=AXIS2_PLACEMENT_3D('',#95887,#78301,#78302);
#71731=AXIS2_PLACEMENT_3D('',#95910,#78303,#78304);
#71732=AXIS2_PLACEMENT_3D('',#95920,#78307,#78308);
#71733=AXIS2_PLACEMENT_3D('',#95938,#78309,#78310);
#71734=AXIS2_PLACEMENT_3D('',#95946,#78311,#78312);
#71735=AXIS2_PLACEMENT_3D('',#95948,#78314,#78315);
#71736=AXIS2_PLACEMENT_3D('',#95958,#78316,#78317);
#71737=AXIS2_PLACEMENT_3D('',#95959,#78318,#78319);
#71738=AXIS2_PLACEMENT_3D('',#95968,#78321,#78322);
#71739=AXIS2_PLACEMENT_3D('',#95986,#78323,#78324);
#71740=AXIS2_PLACEMENT_3D('',#95994,#78325,#78326);
#71741=AXIS2_PLACEMENT_3D('',#95996,#78328,#78329);
#71742=AXIS2_PLACEMENT_3D('',#96006,#78330,#78331);
#71743=AXIS2_PLACEMENT_3D('',#96007,#78332,#78333);
#71744=AXIS2_PLACEMENT_3D('',#96016,#78335,#78336);
#71745=AXIS2_PLACEMENT_3D('',#96034,#78337,#78338);
#71746=AXIS2_PLACEMENT_3D('',#96042,#78339,#78340);
#71747=AXIS2_PLACEMENT_3D('',#96044,#78342,#78343);
#71748=AXIS2_PLACEMENT_3D('',#96054,#78344,#78345);
#71749=AXIS2_PLACEMENT_3D('',#96055,#78346,#78347);
#71750=AXIS2_PLACEMENT_3D('',#96064,#78349,#78350);
#71751=AXIS2_PLACEMENT_3D('',#96082,#78351,#78352);
#71752=AXIS2_PLACEMENT_3D('',#96090,#78353,#78354);
#71753=AXIS2_PLACEMENT_3D('',#96092,#78356,#78357);
#71754=AXIS2_PLACEMENT_3D('',#96102,#78358,#78359);
#71755=AXIS2_PLACEMENT_3D('',#96103,#78360,#78361);
#71756=AXIS2_PLACEMENT_3D('',#96112,#78363,#78364);
#71757=AXIS2_PLACEMENT_3D('',#96130,#78365,#78366);
#71758=AXIS2_PLACEMENT_3D('',#96138,#78367,#78368);
#71759=AXIS2_PLACEMENT_3D('',#96140,#78370,#78371);
#71760=AXIS2_PLACEMENT_3D('',#96150,#78372,#78373);
#71761=AXIS2_PLACEMENT_3D('',#96151,#78374,#78375);
#71762=AXIS2_PLACEMENT_3D('',#96160,#78377,#78378);
#71763=AXIS2_PLACEMENT_3D('',#96178,#78379,#78380);
#71764=AXIS2_PLACEMENT_3D('',#96186,#78381,#78382);
#71765=AXIS2_PLACEMENT_3D('',#96188,#78384,#78385);
#71766=AXIS2_PLACEMENT_3D('',#96198,#78386,#78387);
#71767=AXIS2_PLACEMENT_3D('',#96199,#78388,#78389);
#71768=AXIS2_PLACEMENT_3D('',#96208,#78391,#78392);
#71769=AXIS2_PLACEMENT_3D('',#96226,#78393,#78394);
#71770=AXIS2_PLACEMENT_3D('',#96234,#78395,#78396);
#71771=AXIS2_PLACEMENT_3D('',#96236,#78398,#78399);
#71772=AXIS2_PLACEMENT_3D('',#96246,#78400,#78401);
#71773=AXIS2_PLACEMENT_3D('',#96247,#78402,#78403);
#71774=AXIS2_PLACEMENT_3D('',#96256,#78405,#78406);
#71775=AXIS2_PLACEMENT_3D('',#96274,#78407,#78408);
#71776=AXIS2_PLACEMENT_3D('',#96282,#78409,#78410);
#71777=AXIS2_PLACEMENT_3D('',#96284,#78412,#78413);
#71778=AXIS2_PLACEMENT_3D('',#96294,#78414,#78415);
#71779=AXIS2_PLACEMENT_3D('',#96295,#78416,#78417);
#71780=AXIS2_PLACEMENT_3D('',#96304,#78419,#78420);
#71781=AXIS2_PLACEMENT_3D('',#96322,#78421,#78422);
#71782=AXIS2_PLACEMENT_3D('',#96330,#78423,#78424);
#71783=AXIS2_PLACEMENT_3D('',#96332,#78426,#78427);
#71784=AXIS2_PLACEMENT_3D('',#96342,#78428,#78429);
#71785=AXIS2_PLACEMENT_3D('',#96343,#78430,#78431);
#71786=AXIS2_PLACEMENT_3D('',#96352,#78433,#78434);
#71787=AXIS2_PLACEMENT_3D('',#96370,#78435,#78436);
#71788=AXIS2_PLACEMENT_3D('',#96378,#78437,#78438);
#71789=AXIS2_PLACEMENT_3D('',#96380,#78440,#78441);
#71790=AXIS2_PLACEMENT_3D('',#96390,#78442,#78443);
#71791=AXIS2_PLACEMENT_3D('',#96391,#78444,#78445);
#71792=AXIS2_PLACEMENT_3D('',#96400,#78447,#78448);
#71793=AXIS2_PLACEMENT_3D('',#96418,#78449,#78450);
#71794=AXIS2_PLACEMENT_3D('',#96426,#78451,#78452);
#71795=AXIS2_PLACEMENT_3D('',#96428,#78454,#78455);
#71796=AXIS2_PLACEMENT_3D('',#96438,#78456,#78457);
#71797=AXIS2_PLACEMENT_3D('',#96439,#78458,#78459);
#71798=AXIS2_PLACEMENT_3D('',#96448,#78461,#78462);
#71799=AXIS2_PLACEMENT_3D('',#96466,#78463,#78464);
#71800=AXIS2_PLACEMENT_3D('',#96474,#78465,#78466);
#71801=AXIS2_PLACEMENT_3D('',#96476,#78468,#78469);
#71802=AXIS2_PLACEMENT_3D('',#96486,#78470,#78471);
#71803=AXIS2_PLACEMENT_3D('',#96487,#78472,#78473);
#71804=AXIS2_PLACEMENT_3D('',#96496,#78475,#78476);
#71805=AXIS2_PLACEMENT_3D('',#96514,#78477,#78478);
#71806=AXIS2_PLACEMENT_3D('',#96522,#78479,#78480);
#71807=AXIS2_PLACEMENT_3D('',#96524,#78482,#78483);
#71808=AXIS2_PLACEMENT_3D('',#96534,#78484,#78485);
#71809=AXIS2_PLACEMENT_3D('',#96535,#78486,#78487);
#71810=AXIS2_PLACEMENT_3D('',#96544,#78489,#78490);
#71811=AXIS2_PLACEMENT_3D('',#96562,#78491,#78492);
#71812=AXIS2_PLACEMENT_3D('',#96570,#78493,#78494);
#71813=AXIS2_PLACEMENT_3D('',#96572,#78496,#78497);
#71814=AXIS2_PLACEMENT_3D('',#96582,#78498,#78499);
#71815=AXIS2_PLACEMENT_3D('',#96583,#78500,#78501);
#71816=AXIS2_PLACEMENT_3D('',#96592,#78503,#78504);
#71817=AXIS2_PLACEMENT_3D('',#96610,#78505,#78506);
#71818=AXIS2_PLACEMENT_3D('',#96618,#78507,#78508);
#71819=AXIS2_PLACEMENT_3D('',#96620,#78510,#78511);
#71820=AXIS2_PLACEMENT_3D('',#96630,#78512,#78513);
#71821=AXIS2_PLACEMENT_3D('',#96631,#78514,#78515);
#71822=AXIS2_PLACEMENT_3D('',#96640,#78517,#78518);
#71823=AXIS2_PLACEMENT_3D('',#96658,#78519,#78520);
#71824=AXIS2_PLACEMENT_3D('',#96666,#78521,#78522);
#71825=AXIS2_PLACEMENT_3D('',#96668,#78524,#78525);
#71826=AXIS2_PLACEMENT_3D('',#96678,#78526,#78527);
#71827=AXIS2_PLACEMENT_3D('',#96679,#78528,#78529);
#71828=AXIS2_PLACEMENT_3D('',#96688,#78531,#78532);
#71829=AXIS2_PLACEMENT_3D('',#96706,#78533,#78534);
#71830=AXIS2_PLACEMENT_3D('',#96714,#78535,#78536);
#71831=AXIS2_PLACEMENT_3D('',#96716,#78538,#78539);
#71832=AXIS2_PLACEMENT_3D('',#96726,#78540,#78541);
#71833=AXIS2_PLACEMENT_3D('',#96727,#78542,#78543);
#71834=AXIS2_PLACEMENT_3D('',#96736,#78545,#78546);
#71835=AXIS2_PLACEMENT_3D('',#96754,#78547,#78548);
#71836=AXIS2_PLACEMENT_3D('',#96762,#78549,#78550);
#71837=AXIS2_PLACEMENT_3D('',#96771,#78552,#78553);
#71838=AXIS2_PLACEMENT_3D('',#96774,#78555,#78556);
#71839=AXIS2_PLACEMENT_3D('',#96775,#78557,#78558);
#71840=AXIS2_PLACEMENT_3D('',#96784,#78559,#78560);
#71841=AXIS2_PLACEMENT_3D('',#96802,#78561,#78562);
#71842=AXIS2_PLACEMENT_3D('',#96810,#78563,#78564);
#71843=AXIS2_PLACEMENT_3D('',#96812,#78566,#78567);
#71844=AXIS2_PLACEMENT_3D('',#96814,#78568,#78569);
#71845=AXIS2_PLACEMENT_3D('',#96823,#78570,#78571);
#71846=AXIS2_PLACEMENT_3D('',#96831,#78572,#78573);
#71847=AXIS2_PLACEMENT_3D('',#96850,#78575,#78576);
#71848=AXIS2_PLACEMENT_3D('',#96858,#78577,#78578);
#71849=AXIS2_PLACEMENT_3D('',#96860,#78580,#78581);
#71850=AXIS2_PLACEMENT_3D('',#96870,#78582,#78583);
#71851=AXIS2_PLACEMENT_3D('',#96871,#78584,#78585);
#71852=AXIS2_PLACEMENT_3D('',#96880,#78587,#78588);
#71853=AXIS2_PLACEMENT_3D('',#96898,#78589,#78590);
#71854=AXIS2_PLACEMENT_3D('',#96906,#78591,#78592);
#71855=AXIS2_PLACEMENT_3D('',#96908,#78594,#78595);
#71856=AXIS2_PLACEMENT_3D('',#96918,#78596,#78597);
#71857=AXIS2_PLACEMENT_3D('',#96919,#78598,#78599);
#71858=AXIS2_PLACEMENT_3D('',#96928,#78601,#78602);
#71859=AXIS2_PLACEMENT_3D('',#96929,#78603,#78604);
#71860=AXIS2_PLACEMENT_3D('',#96939,#78605,#78606);
#71861=AXIS2_PLACEMENT_3D('',#96940,#78607,#78608);
#71862=AXIS2_PLACEMENT_3D('',#96956,#78609,#78610);
#71863=AXIS2_PLACEMENT_3D('',#96976,#78612,#78613);
#71864=AXIS2_PLACEMENT_3D('',#96990,#78616,#78617);
#71865=AXIS2_PLACEMENT_3D('',#97008,#78618,#78619);
#71866=AXIS2_PLACEMENT_3D('',#97010,#78621,#78622);
#71867=AXIS2_PLACEMENT_3D('',#97012,#78623,#78624);
#71868=AXIS2_PLACEMENT_3D('',#97013,#78625,#78626);
#71869=AXIS2_PLACEMENT_3D('',#97026,#78628,#78629);
#71870=AXIS2_PLACEMENT_3D('',#97044,#78630,#78631);
#71871=AXIS2_PLACEMENT_3D('',#97046,#78633,#78634);
#71872=AXIS2_PLACEMENT_3D('',#97048,#78635,#78636);
#71873=AXIS2_PLACEMENT_3D('',#97049,#78637,#78638);
#71874=AXIS2_PLACEMENT_3D('',#97062,#78640,#78641);
#71875=AXIS2_PLACEMENT_3D('',#97080,#78642,#78643);
#71876=AXIS2_PLACEMENT_3D('',#97082,#78645,#78646);
#71877=AXIS2_PLACEMENT_3D('',#97084,#78647,#78648);
#71878=AXIS2_PLACEMENT_3D('',#97085,#78649,#78650);
#71879=AXIS2_PLACEMENT_3D('',#97098,#78652,#78653);
#71880=AXIS2_PLACEMENT_3D('',#97116,#78654,#78655);
#71881=AXIS2_PLACEMENT_3D('',#97118,#78657,#78658);
#71882=AXIS2_PLACEMENT_3D('',#97120,#78659,#78660);
#71883=AXIS2_PLACEMENT_3D('',#97121,#78661,#78662);
#71884=AXIS2_PLACEMENT_3D('',#97134,#78664,#78665);
#71885=AXIS2_PLACEMENT_3D('',#97152,#78666,#78667);
#71886=AXIS2_PLACEMENT_3D('',#97154,#78669,#78670);
#71887=AXIS2_PLACEMENT_3D('',#97156,#78671,#78672);
#71888=AXIS2_PLACEMENT_3D('',#97157,#78673,#78674);
#71889=AXIS2_PLACEMENT_3D('',#97170,#78676,#78677);
#71890=AXIS2_PLACEMENT_3D('',#97188,#78678,#78679);
#71891=AXIS2_PLACEMENT_3D('',#97190,#78681,#78682);
#71892=AXIS2_PLACEMENT_3D('',#97192,#78683,#78684);
#71893=AXIS2_PLACEMENT_3D('',#97193,#78685,#78686);
#71894=AXIS2_PLACEMENT_3D('',#97206,#78688,#78689);
#71895=AXIS2_PLACEMENT_3D('',#97224,#78690,#78691);
#71896=AXIS2_PLACEMENT_3D('',#97226,#78693,#78694);
#71897=AXIS2_PLACEMENT_3D('',#97228,#78695,#78696);
#71898=AXIS2_PLACEMENT_3D('',#97229,#78697,#78698);
#71899=AXIS2_PLACEMENT_3D('',#97242,#78700,#78701);
#71900=AXIS2_PLACEMENT_3D('',#97260,#78702,#78703);
#71901=AXIS2_PLACEMENT_3D('',#97262,#78705,#78706);
#71902=AXIS2_PLACEMENT_3D('',#97264,#78707,#78708);
#71903=AXIS2_PLACEMENT_3D('',#97265,#78709,#78710);
#71904=AXIS2_PLACEMENT_3D('',#97278,#78712,#78713);
#71905=AXIS2_PLACEMENT_3D('',#97296,#78714,#78715);
#71906=AXIS2_PLACEMENT_3D('',#97298,#78717,#78718);
#71907=AXIS2_PLACEMENT_3D('',#97300,#78719,#78720);
#71908=AXIS2_PLACEMENT_3D('',#97301,#78721,#78722);
#71909=AXIS2_PLACEMENT_3D('',#97314,#78724,#78725);
#71910=AXIS2_PLACEMENT_3D('',#97332,#78726,#78727);
#71911=AXIS2_PLACEMENT_3D('',#97334,#78729,#78730);
#71912=AXIS2_PLACEMENT_3D('',#97336,#78731,#78732);
#71913=AXIS2_PLACEMENT_3D('',#97337,#78733,#78734);
#71914=AXIS2_PLACEMENT_3D('',#97350,#78736,#78737);
#71915=AXIS2_PLACEMENT_3D('',#97368,#78738,#78739);
#71916=AXIS2_PLACEMENT_3D('',#97370,#78741,#78742);
#71917=AXIS2_PLACEMENT_3D('',#97372,#78743,#78744);
#71918=AXIS2_PLACEMENT_3D('',#97373,#78745,#78746);
#71919=AXIS2_PLACEMENT_3D('',#97386,#78748,#78749);
#71920=AXIS2_PLACEMENT_3D('',#97404,#78750,#78751);
#71921=AXIS2_PLACEMENT_3D('',#97406,#78753,#78754);
#71922=AXIS2_PLACEMENT_3D('',#97408,#78755,#78756);
#71923=AXIS2_PLACEMENT_3D('',#97409,#78757,#78758);
#71924=AXIS2_PLACEMENT_3D('',#97422,#78760,#78761);
#71925=AXIS2_PLACEMENT_3D('',#97440,#78762,#78763);
#71926=AXIS2_PLACEMENT_3D('',#97442,#78765,#78766);
#71927=AXIS2_PLACEMENT_3D('',#97444,#78767,#78768);
#71928=AXIS2_PLACEMENT_3D('',#97445,#78769,#78770);
#71929=AXIS2_PLACEMENT_3D('',#97485,#78774,#78775);
#71930=AXIS2_PLACEMENT_3D('',#97503,#78776,#78777);
#71931=AXIS2_PLACEMENT_3D('',#97505,#78779,#78780);
#71932=AXIS2_PLACEMENT_3D('',#97507,#78781,#78782);
#71933=AXIS2_PLACEMENT_3D('',#97508,#78783,#78784);
#71934=AXIS2_PLACEMENT_3D('',#97521,#78786,#78787);
#71935=AXIS2_PLACEMENT_3D('',#97539,#78788,#78789);
#71936=AXIS2_PLACEMENT_3D('',#97541,#78791,#78792);
#71937=AXIS2_PLACEMENT_3D('',#97543,#78793,#78794);
#71938=AXIS2_PLACEMENT_3D('',#97544,#78795,#78796);
#71939=AXIS2_PLACEMENT_3D('',#97557,#78798,#78799);
#71940=AXIS2_PLACEMENT_3D('',#97575,#78800,#78801);
#71941=AXIS2_PLACEMENT_3D('',#97577,#78803,#78804);
#71942=AXIS2_PLACEMENT_3D('',#97579,#78805,#78806);
#71943=AXIS2_PLACEMENT_3D('',#97580,#78807,#78808);
#71944=AXIS2_PLACEMENT_3D('',#97593,#78810,#78811);
#71945=AXIS2_PLACEMENT_3D('',#97611,#78812,#78813);
#71946=AXIS2_PLACEMENT_3D('',#97613,#78815,#78816);
#71947=AXIS2_PLACEMENT_3D('',#97615,#78817,#78818);
#71948=AXIS2_PLACEMENT_3D('',#97616,#78819,#78820);
#71949=AXIS2_PLACEMENT_3D('',#97629,#78822,#78823);
#71950=AXIS2_PLACEMENT_3D('',#97647,#78824,#78825);
#71951=AXIS2_PLACEMENT_3D('',#97649,#78827,#78828);
#71952=AXIS2_PLACEMENT_3D('',#97651,#78829,#78830);
#71953=AXIS2_PLACEMENT_3D('',#97652,#78831,#78832);
#71954=AXIS2_PLACEMENT_3D('',#97665,#78834,#78835);
#71955=AXIS2_PLACEMENT_3D('',#97683,#78836,#78837);
#71956=AXIS2_PLACEMENT_3D('',#97685,#78839,#78840);
#71957=AXIS2_PLACEMENT_3D('',#97687,#78841,#78842);
#71958=AXIS2_PLACEMENT_3D('',#97688,#78843,#78844);
#71959=AXIS2_PLACEMENT_3D('',#97701,#78846,#78847);
#71960=AXIS2_PLACEMENT_3D('',#97719,#78848,#78849);
#71961=AXIS2_PLACEMENT_3D('',#97721,#78851,#78852);
#71962=AXIS2_PLACEMENT_3D('',#97723,#78853,#78854);
#71963=AXIS2_PLACEMENT_3D('',#97724,#78855,#78856);
#71964=AXIS2_PLACEMENT_3D('',#97737,#78858,#78859);
#71965=AXIS2_PLACEMENT_3D('',#97755,#78860,#78861);
#71966=AXIS2_PLACEMENT_3D('',#97757,#78863,#78864);
#71967=AXIS2_PLACEMENT_3D('',#97759,#78865,#78866);
#71968=AXIS2_PLACEMENT_3D('',#97760,#78867,#78868);
#71969=AXIS2_PLACEMENT_3D('',#97773,#78870,#78871);
#71970=AXIS2_PLACEMENT_3D('',#97791,#78872,#78873);
#71971=AXIS2_PLACEMENT_3D('',#97793,#78875,#78876);
#71972=AXIS2_PLACEMENT_3D('',#97795,#78877,#78878);
#71973=AXIS2_PLACEMENT_3D('',#97796,#78879,#78880);
#71974=AXIS2_PLACEMENT_3D('',#97809,#78882,#78883);
#71975=AXIS2_PLACEMENT_3D('',#97827,#78884,#78885);
#71976=AXIS2_PLACEMENT_3D('',#97829,#78887,#78888);
#71977=AXIS2_PLACEMENT_3D('',#97831,#78889,#78890);
#71978=AXIS2_PLACEMENT_3D('',#97832,#78891,#78892);
#71979=AXIS2_PLACEMENT_3D('',#97845,#78894,#78895);
#71980=AXIS2_PLACEMENT_3D('',#97863,#78896,#78897);
#71981=AXIS2_PLACEMENT_3D('',#97865,#78899,#78900);
#71982=AXIS2_PLACEMENT_3D('',#97867,#78901,#78902);
#71983=AXIS2_PLACEMENT_3D('',#97868,#78903,#78904);
#71984=AXIS2_PLACEMENT_3D('',#97881,#78906,#78907);
#71985=AXIS2_PLACEMENT_3D('',#97899,#78908,#78909);
#71986=AXIS2_PLACEMENT_3D('',#97901,#78911,#78912);
#71987=AXIS2_PLACEMENT_3D('',#97903,#78913,#78914);
#71988=AXIS2_PLACEMENT_3D('',#97904,#78915,#78916);
#71989=AXIS2_PLACEMENT_3D('',#97917,#78918,#78919);
#71990=AXIS2_PLACEMENT_3D('',#97935,#78920,#78921);
#71991=AXIS2_PLACEMENT_3D('',#97937,#78923,#78924);
#71992=AXIS2_PLACEMENT_3D('',#97939,#78925,#78926);
#71993=AXIS2_PLACEMENT_3D('',#97940,#78927,#78928);
#71994=AXIS2_PLACEMENT_3D('',#97953,#78930,#78931);
#71995=AXIS2_PLACEMENT_3D('',#97971,#78932,#78933);
#71996=AXIS2_PLACEMENT_3D('',#97973,#78935,#78936);
#71997=AXIS2_PLACEMENT_3D('',#97975,#78937,#78938);
#71998=AXIS2_PLACEMENT_3D('',#97976,#78939,#78940);
#71999=AXIS2_PLACEMENT_3D('',#97977,#78941,#78942);
#72000=AXIS2_PLACEMENT_3D('',#97979,#78943,#78944);
#72001=AXIS2_PLACEMENT_3D('',#97981,#78945,#78946);
#72002=AXIS2_PLACEMENT_3D('',#97982,#78947,#78948);
#72003=AXIS2_PLACEMENT_3D('',#98000,#78950,#78951);
#72004=AXIS2_PLACEMENT_3D('',#98039,#78952,#78953);
#72005=AXIS2_PLACEMENT_3D('',#98072,#78954,#78955);
#72006=AXIS2_PLACEMENT_3D('',#98105,#78956,#78957);
#72007=AXIS2_PLACEMENT_3D('',#98138,#78958,#78959);
#72008=AXIS2_PLACEMENT_3D('',#98171,#78960,#78961);
#72009=AXIS2_PLACEMENT_3D('',#98204,#78962,#78963);
#72010=AXIS2_PLACEMENT_3D('',#98237,#78964,#78965);
#72011=AXIS2_PLACEMENT_3D('',#98272,#78966,#78967);
#72012=AXIS2_PLACEMENT_3D('',#98305,#78968,#78969);
#72013=AXIS2_PLACEMENT_3D('',#98338,#78970,#78971);
#72014=AXIS2_PLACEMENT_3D('',#98371,#78972,#78973);
#72015=AXIS2_PLACEMENT_3D('',#98404,#78974,#78975);
#72016=AXIS2_PLACEMENT_3D('',#98439,#78976,#78977);
#72017=AXIS2_PLACEMENT_3D('',#98474,#78978,#78979);
#72018=AXIS2_PLACEMENT_3D('',#98507,#78980,#78981);
#72019=AXIS2_PLACEMENT_3D('',#98540,#78982,#78983);
#72020=AXIS2_PLACEMENT_3D('',#98575,#78984,#78985);
#72021=AXIS2_PLACEMENT_3D('',#98608,#78986,#78987);
#72022=AXIS2_PLACEMENT_3D('',#98641,#78988,#78989);
#72023=AXIS2_PLACEMENT_3D('',#98674,#78990,#78991);
#72024=AXIS2_PLACEMENT_3D('',#98707,#78992,#78993);
#72025=AXIS2_PLACEMENT_3D('',#98740,#78994,#78995);
#72026=AXIS2_PLACEMENT_3D('',#98775,#78996,#78997);
#72027=AXIS2_PLACEMENT_3D('',#98810,#78998,#78999);
#72028=AXIS2_PLACEMENT_3D('',#98845,#79000,#79001);
#72029=AXIS2_PLACEMENT_3D('',#98878,#79002,#79003);
#72030=AXIS2_PLACEMENT_3D('',#98911,#79004,#79005);
#72031=AXIS2_PLACEMENT_3D('',#98944,#79006,#79007);
#72032=AXIS2_PLACEMENT_3D('',#98983,#79008,#79009);
#72033=AXIS2_PLACEMENT_3D('',#98991,#79010,#79011);
#72034=AXIS2_PLACEMENT_3D('',#99008,#79012,#79013);
#72035=AXIS2_PLACEMENT_3D('',#99016,#79014,#79015);
#72036=AXIS2_PLACEMENT_3D('',#99033,#79016,#79017);
#72037=AXIS2_PLACEMENT_3D('',#99041,#79018,#79019);
#72038=AXIS2_PLACEMENT_3D('',#99058,#79020,#79021);
#72039=AXIS2_PLACEMENT_3D('',#99066,#79022,#79023);
#72040=AXIS2_PLACEMENT_3D('',#99083,#79024,#79025);
#72041=AXIS2_PLACEMENT_3D('',#99091,#79026,#79027);
#72042=AXIS2_PLACEMENT_3D('',#99108,#79028,#79029);
#72043=AXIS2_PLACEMENT_3D('',#99116,#79030,#79031);
#72044=AXIS2_PLACEMENT_3D('',#99133,#79032,#79033);
#72045=AXIS2_PLACEMENT_3D('',#99141,#79034,#79035);
#72046=AXIS2_PLACEMENT_3D('',#99158,#79036,#79037);
#72047=AXIS2_PLACEMENT_3D('',#99166,#79038,#79039);
#72048=AXIS2_PLACEMENT_3D('',#99183,#79040,#79041);
#72049=AXIS2_PLACEMENT_3D('',#99191,#79042,#79043);
#72050=AXIS2_PLACEMENT_3D('',#99208,#79044,#79045);
#72051=AXIS2_PLACEMENT_3D('',#99216,#79046,#79047);
#72052=AXIS2_PLACEMENT_3D('',#99233,#79048,#79049);
#72053=AXIS2_PLACEMENT_3D('',#99241,#79050,#79051);
#72054=AXIS2_PLACEMENT_3D('',#99258,#79052,#79053);
#72055=AXIS2_PLACEMENT_3D('',#99266,#79054,#79055);
#72056=AXIS2_PLACEMENT_3D('',#99283,#79056,#79057);
#72057=AXIS2_PLACEMENT_3D('',#99291,#79058,#79059);
#72058=AXIS2_PLACEMENT_3D('',#99308,#79060,#79061);
#72059=AXIS2_PLACEMENT_3D('',#99316,#79062,#79063);
#72060=AXIS2_PLACEMENT_3D('',#99333,#79064,#79065);
#72061=AXIS2_PLACEMENT_3D('',#99341,#79066,#79067);
#72062=AXIS2_PLACEMENT_3D('',#99358,#79068,#79069);
#72063=AXIS2_PLACEMENT_3D('',#99366,#79070,#79071);
#72064=AXIS2_PLACEMENT_3D('',#99383,#79072,#79073);
#72065=AXIS2_PLACEMENT_3D('',#99391,#79074,#79075);
#72066=AXIS2_PLACEMENT_3D('',#99408,#79076,#79077);
#72067=AXIS2_PLACEMENT_3D('',#99416,#79078,#79079);
#72068=AXIS2_PLACEMENT_3D('',#99433,#79080,#79081);
#72069=AXIS2_PLACEMENT_3D('',#99441,#79082,#79083);
#72070=AXIS2_PLACEMENT_3D('',#99458,#79084,#79085);
#72071=AXIS2_PLACEMENT_3D('',#99466,#79086,#79087);
#72072=AXIS2_PLACEMENT_3D('',#99483,#79088,#79089);
#72073=AXIS2_PLACEMENT_3D('',#99491,#79090,#79091);
#72074=AXIS2_PLACEMENT_3D('',#99508,#79092,#79093);
#72075=AXIS2_PLACEMENT_3D('',#99516,#79094,#79095);
#72076=AXIS2_PLACEMENT_3D('',#99533,#79096,#79097);
#72077=AXIS2_PLACEMENT_3D('',#99541,#79098,#79099);
#72078=AXIS2_PLACEMENT_3D('',#99558,#79100,#79101);
#72079=AXIS2_PLACEMENT_3D('',#99566,#79102,#79103);
#72080=AXIS2_PLACEMENT_3D('',#99583,#79104,#79105);
#72081=AXIS2_PLACEMENT_3D('',#99591,#79106,#79107);
#72082=AXIS2_PLACEMENT_3D('',#99608,#79108,#79109);
#72083=AXIS2_PLACEMENT_3D('',#99616,#79110,#79111);
#72084=AXIS2_PLACEMENT_3D('',#99633,#79112,#79113);
#72085=AXIS2_PLACEMENT_3D('',#99641,#79114,#79115);
#72086=AXIS2_PLACEMENT_3D('',#99658,#79116,#79117);
#72087=AXIS2_PLACEMENT_3D('',#99666,#79118,#79119);
#72088=AXIS2_PLACEMENT_3D('',#99683,#79120,#79121);
#72089=AXIS2_PLACEMENT_3D('',#99690,#79122,#79123);
#72090=AXIS2_PLACEMENT_3D('',#99699,#79124,#79125);
#72091=AXIS2_PLACEMENT_3D('',#99707,#79127,#79128);
#72092=AXIS2_PLACEMENT_3D('',#99709,#79129,#79130);
#72093=AXIS2_PLACEMENT_3D('',#99748,#79132,#79133);
#72094=AXIS2_PLACEMENT_3D('',#99756,#79135,#79136);
#72095=AXIS2_PLACEMENT_3D('',#99758,#79137,#79138);
#72096=AXIS2_PLACEMENT_3D('',#99797,#79140,#79141);
#72097=AXIS2_PLACEMENT_3D('',#99805,#79143,#79144);
#72098=AXIS2_PLACEMENT_3D('',#99807,#79145,#79146);
#72099=AXIS2_PLACEMENT_3D('',#99846,#79148,#79149);
#72100=AXIS2_PLACEMENT_3D('',#99854,#79151,#79152);
#72101=AXIS2_PLACEMENT_3D('',#99856,#79153,#79154);
#72102=AXIS2_PLACEMENT_3D('',#99895,#79156,#79157);
#72103=AXIS2_PLACEMENT_3D('',#99903,#79159,#79160);
#72104=AXIS2_PLACEMENT_3D('',#99905,#79161,#79162);
#72105=AXIS2_PLACEMENT_3D('',#99944,#79164,#79165);
#72106=AXIS2_PLACEMENT_3D('',#99952,#79167,#79168);
#72107=AXIS2_PLACEMENT_3D('',#99954,#79169,#79170);
#72108=AXIS2_PLACEMENT_3D('',#99993,#79172,#79173);
#72109=AXIS2_PLACEMENT_3D('',#100001,#79175,#79176);
#72110=AXIS2_PLACEMENT_3D('',#100003,#79177,#79178);
#72111=AXIS2_PLACEMENT_3D('',#100042,#79180,#79181);
#72112=AXIS2_PLACEMENT_3D('',#100050,#79183,#79184);
#72113=AXIS2_PLACEMENT_3D('',#100052,#79185,#79186);
#72114=AXIS2_PLACEMENT_3D('',#100091,#79188,#79189);
#72115=AXIS2_PLACEMENT_3D('',#100099,#79191,#79192);
#72116=AXIS2_PLACEMENT_3D('',#100101,#79193,#79194);
#72117=AXIS2_PLACEMENT_3D('',#100140,#79196,#79197);
#72118=AXIS2_PLACEMENT_3D('',#100148,#79199,#79200);
#72119=AXIS2_PLACEMENT_3D('',#100150,#79201,#79202);
#72120=AXIS2_PLACEMENT_3D('',#100189,#79204,#79205);
#72121=AXIS2_PLACEMENT_3D('',#100197,#79207,#79208);
#72122=AXIS2_PLACEMENT_3D('',#100199,#79209,#79210);
#72123=AXIS2_PLACEMENT_3D('',#100238,#79212,#79213);
#72124=AXIS2_PLACEMENT_3D('',#100246,#79215,#79216);
#72125=AXIS2_PLACEMENT_3D('',#100248,#79217,#79218);
#72126=AXIS2_PLACEMENT_3D('',#100287,#79220,#79221);
#72127=AXIS2_PLACEMENT_3D('',#100295,#79223,#79224);
#72128=AXIS2_PLACEMENT_3D('',#100297,#79225,#79226);
#72129=AXIS2_PLACEMENT_3D('',#100336,#79228,#79229);
#72130=AXIS2_PLACEMENT_3D('',#100344,#79231,#79232);
#72131=AXIS2_PLACEMENT_3D('',#100346,#79233,#79234);
#72132=AXIS2_PLACEMENT_3D('',#100413,#79238,#79239);
#72133=AXIS2_PLACEMENT_3D('',#100421,#79241,#79242);
#72134=AXIS2_PLACEMENT_3D('',#100423,#79243,#79244);
#72135=AXIS2_PLACEMENT_3D('',#100462,#79246,#79247);
#72136=AXIS2_PLACEMENT_3D('',#100470,#79249,#79250);
#72137=AXIS2_PLACEMENT_3D('',#100472,#79251,#79252);
#72138=AXIS2_PLACEMENT_3D('',#100511,#79254,#79255);
#72139=AXIS2_PLACEMENT_3D('',#100519,#79257,#79258);
#72140=AXIS2_PLACEMENT_3D('',#100521,#79259,#79260);
#72141=AXIS2_PLACEMENT_3D('',#100560,#79262,#79263);
#72142=AXIS2_PLACEMENT_3D('',#100568,#79265,#79266);
#72143=AXIS2_PLACEMENT_3D('',#100570,#79267,#79268);
#72144=AXIS2_PLACEMENT_3D('',#100609,#79270,#79271);
#72145=AXIS2_PLACEMENT_3D('',#100617,#79273,#79274);
#72146=AXIS2_PLACEMENT_3D('',#100619,#79275,#79276);
#72147=AXIS2_PLACEMENT_3D('',#100658,#79278,#79279);
#72148=AXIS2_PLACEMENT_3D('',#100666,#79281,#79282);
#72149=AXIS2_PLACEMENT_3D('',#100668,#79283,#79284);
#72150=AXIS2_PLACEMENT_3D('',#100707,#79286,#79287);
#72151=AXIS2_PLACEMENT_3D('',#100715,#79289,#79290);
#72152=AXIS2_PLACEMENT_3D('',#100717,#79291,#79292);
#72153=AXIS2_PLACEMENT_3D('',#100756,#79294,#79295);
#72154=AXIS2_PLACEMENT_3D('',#100764,#79297,#79298);
#72155=AXIS2_PLACEMENT_3D('',#100766,#79299,#79300);
#72156=AXIS2_PLACEMENT_3D('',#100805,#79302,#79303);
#72157=AXIS2_PLACEMENT_3D('',#100813,#79305,#79306);
#72158=AXIS2_PLACEMENT_3D('',#100815,#79307,#79308);
#72159=AXIS2_PLACEMENT_3D('',#100854,#79310,#79311);
#72160=AXIS2_PLACEMENT_3D('',#100885,#79314,#79315);
#72161=AXIS2_PLACEMENT_3D('',#100887,#79316,#79317);
#72162=AXIS2_PLACEMENT_3D('',#100904,#79319,#79320);
#72163=AXIS2_PLACEMENT_3D('',#100911,#79321,#79322);
#72164=AXIS2_PLACEMENT_3D('',#100921,#79323,#79324);
#72165=AXIS2_PLACEMENT_3D('',#100952,#79326,#79327);
#72166=AXIS2_PLACEMENT_3D('',#100960,#79329,#79330);
#72167=AXIS2_PLACEMENT_3D('',#100962,#79331,#79332);
#72168=AXIS2_PLACEMENT_3D('',#101001,#79334,#79335);
#72169=AXIS2_PLACEMENT_3D('',#101009,#79337,#79338);
#72170=AXIS2_PLACEMENT_3D('',#101011,#79339,#79340);
#72171=AXIS2_PLACEMENT_3D('',#101050,#79342,#79343);
#72172=AXIS2_PLACEMENT_3D('',#101058,#79345,#79346);
#72173=AXIS2_PLACEMENT_3D('',#101060,#79347,#79348);
#72174=AXIS2_PLACEMENT_3D('',#101104,#79351,#79352);
#72175=AXIS2_PLACEMENT_3D('',#101122,#79353,#79354);
#72176=AXIS2_PLACEMENT_3D('',#101124,#79356,#79357);
#72177=AXIS2_PLACEMENT_3D('',#101126,#79358,#79359);
#72178=AXIS2_PLACEMENT_3D('',#101145,#79361,#79362);
#72179=AXIS2_PLACEMENT_3D('',#101163,#79363,#79364);
#72180=AXIS2_PLACEMENT_3D('',#101165,#79366,#79367);
#72181=AXIS2_PLACEMENT_3D('',#101167,#79368,#79369);
#72182=AXIS2_PLACEMENT_3D('',#101186,#79371,#79372);
#72183=AXIS2_PLACEMENT_3D('',#101204,#79373,#79374);
#72184=AXIS2_PLACEMENT_3D('',#101206,#79376,#79377);
#72185=AXIS2_PLACEMENT_3D('',#101208,#79378,#79379);
#72186=AXIS2_PLACEMENT_3D('',#101227,#79381,#79382);
#72187=AXIS2_PLACEMENT_3D('',#101245,#79383,#79384);
#72188=AXIS2_PLACEMENT_3D('',#101247,#79386,#79387);
#72189=AXIS2_PLACEMENT_3D('',#101249,#79388,#79389);
#72190=AXIS2_PLACEMENT_3D('',#101268,#79391,#79392);
#72191=AXIS2_PLACEMENT_3D('',#101286,#79393,#79394);
#72192=AXIS2_PLACEMENT_3D('',#101288,#79396,#79397);
#72193=AXIS2_PLACEMENT_3D('',#101290,#79398,#79399);
#72194=AXIS2_PLACEMENT_3D('',#101309,#79401,#79402);
#72195=AXIS2_PLACEMENT_3D('',#101327,#79403,#79404);
#72196=AXIS2_PLACEMENT_3D('',#101329,#79406,#79407);
#72197=AXIS2_PLACEMENT_3D('',#101331,#79408,#79409);
#72198=AXIS2_PLACEMENT_3D('',#101350,#79411,#79412);
#72199=AXIS2_PLACEMENT_3D('',#101368,#79413,#79414);
#72200=AXIS2_PLACEMENT_3D('',#101370,#79416,#79417);
#72201=AXIS2_PLACEMENT_3D('',#101372,#79418,#79419);
#72202=AXIS2_PLACEMENT_3D('',#101391,#79421,#79422);
#72203=AXIS2_PLACEMENT_3D('',#101409,#79423,#79424);
#72204=AXIS2_PLACEMENT_3D('',#101411,#79426,#79427);
#72205=AXIS2_PLACEMENT_3D('',#101413,#79428,#79429);
#72206=AXIS2_PLACEMENT_3D('',#101432,#79431,#79432);
#72207=AXIS2_PLACEMENT_3D('',#101450,#79433,#79434);
#72208=AXIS2_PLACEMENT_3D('',#101452,#79436,#79437);
#72209=AXIS2_PLACEMENT_3D('',#101454,#79438,#79439);
#72210=AXIS2_PLACEMENT_3D('',#101473,#79441,#79442);
#72211=AXIS2_PLACEMENT_3D('',#101491,#79443,#79444);
#72212=AXIS2_PLACEMENT_3D('',#101493,#79446,#79447);
#72213=AXIS2_PLACEMENT_3D('',#101495,#79448,#79449);
#72214=AXIS2_PLACEMENT_3D('',#101514,#79451,#79452);
#72215=AXIS2_PLACEMENT_3D('',#101532,#79453,#79454);
#72216=AXIS2_PLACEMENT_3D('',#101534,#79456,#79457);
#72217=AXIS2_PLACEMENT_3D('',#101536,#79458,#79459);
#72218=AXIS2_PLACEMENT_3D('',#101555,#79461,#79462);
#72219=AXIS2_PLACEMENT_3D('',#101573,#79463,#79464);
#72220=AXIS2_PLACEMENT_3D('',#101575,#79466,#79467);
#72221=AXIS2_PLACEMENT_3D('',#101577,#79468,#79469);
#72222=AXIS2_PLACEMENT_3D('',#101596,#79471,#79472);
#72223=AXIS2_PLACEMENT_3D('',#101614,#79473,#79474);
#72224=AXIS2_PLACEMENT_3D('',#101616,#79476,#79477);
#72225=AXIS2_PLACEMENT_3D('',#101618,#79478,#79479);
#72226=AXIS2_PLACEMENT_3D('',#101637,#79481,#79482);
#72227=AXIS2_PLACEMENT_3D('',#101655,#79483,#79484);
#72228=AXIS2_PLACEMENT_3D('',#101657,#79486,#79487);
#72229=AXIS2_PLACEMENT_3D('',#101659,#79488,#79489);
#72230=AXIS2_PLACEMENT_3D('',#101678,#79491,#79492);
#72231=AXIS2_PLACEMENT_3D('',#101696,#79493,#79494);
#72232=AXIS2_PLACEMENT_3D('',#101698,#79496,#79497);
#72233=AXIS2_PLACEMENT_3D('',#101700,#79498,#79499);
#72234=AXIS2_PLACEMENT_3D('',#101719,#79501,#79502);
#72235=AXIS2_PLACEMENT_3D('',#101737,#79503,#79504);
#72236=AXIS2_PLACEMENT_3D('',#101739,#79506,#79507);
#72237=AXIS2_PLACEMENT_3D('',#101741,#79508,#79509);
#72238=AXIS2_PLACEMENT_3D('',#101760,#79511,#79512);
#72239=AXIS2_PLACEMENT_3D('',#101778,#79513,#79514);
#72240=AXIS2_PLACEMENT_3D('',#101780,#79516,#79517);
#72241=AXIS2_PLACEMENT_3D('',#101782,#79518,#79519);
#72242=AXIS2_PLACEMENT_3D('',#101801,#79521,#79522);
#72243=AXIS2_PLACEMENT_3D('',#101819,#79523,#79524);
#72244=AXIS2_PLACEMENT_3D('',#101821,#79526,#79527);
#72245=AXIS2_PLACEMENT_3D('',#101823,#79528,#79529);
#72246=AXIS2_PLACEMENT_3D('',#101842,#79531,#79532);
#72247=AXIS2_PLACEMENT_3D('',#101860,#79533,#79534);
#72248=AXIS2_PLACEMENT_3D('',#101862,#79536,#79537);
#72249=AXIS2_PLACEMENT_3D('',#101864,#79538,#79539);
#72250=AXIS2_PLACEMENT_3D('',#101883,#79541,#79542);
#72251=AXIS2_PLACEMENT_3D('',#101901,#79543,#79544);
#72252=AXIS2_PLACEMENT_3D('',#101903,#79546,#79547);
#72253=AXIS2_PLACEMENT_3D('',#101905,#79548,#79549);
#72254=AXIS2_PLACEMENT_3D('',#101924,#79551,#79552);
#72255=AXIS2_PLACEMENT_3D('',#101942,#79553,#79554);
#72256=AXIS2_PLACEMENT_3D('',#101944,#79556,#79557);
#72257=AXIS2_PLACEMENT_3D('',#101946,#79558,#79559);
#72258=AXIS2_PLACEMENT_3D('',#101993,#79563,#79564);
#72259=AXIS2_PLACEMENT_3D('',#102011,#79565,#79566);
#72260=AXIS2_PLACEMENT_3D('',#102013,#79568,#79569);
#72261=AXIS2_PLACEMENT_3D('',#102015,#79570,#79571);
#72262=AXIS2_PLACEMENT_3D('',#102034,#79573,#79574);
#72263=AXIS2_PLACEMENT_3D('',#102052,#79575,#79576);
#72264=AXIS2_PLACEMENT_3D('',#102054,#79578,#79579);
#72265=AXIS2_PLACEMENT_3D('',#102056,#79580,#79581);
#72266=AXIS2_PLACEMENT_3D('',#102075,#79583,#79584);
#72267=AXIS2_PLACEMENT_3D('',#102093,#79585,#79586);
#72268=AXIS2_PLACEMENT_3D('',#102095,#79588,#79589);
#72269=AXIS2_PLACEMENT_3D('',#102097,#79590,#79591);
#72270=AXIS2_PLACEMENT_3D('',#102116,#79593,#79594);
#72271=AXIS2_PLACEMENT_3D('',#102134,#79595,#79596);
#72272=AXIS2_PLACEMENT_3D('',#102136,#79598,#79599);
#72273=AXIS2_PLACEMENT_3D('',#102138,#79600,#79601);
#72274=AXIS2_PLACEMENT_3D('',#102157,#79603,#79604);
#72275=AXIS2_PLACEMENT_3D('',#102175,#79605,#79606);
#72276=AXIS2_PLACEMENT_3D('',#102177,#79608,#79609);
#72277=AXIS2_PLACEMENT_3D('',#102179,#79610,#79611);
#72278=AXIS2_PLACEMENT_3D('',#102198,#79613,#79614);
#72279=AXIS2_PLACEMENT_3D('',#102216,#79615,#79616);
#72280=AXIS2_PLACEMENT_3D('',#102218,#79618,#79619);
#72281=AXIS2_PLACEMENT_3D('',#102220,#79620,#79621);
#72282=AXIS2_PLACEMENT_3D('',#102239,#79623,#79624);
#72283=AXIS2_PLACEMENT_3D('',#102257,#79625,#79626);
#72284=AXIS2_PLACEMENT_3D('',#102259,#79628,#79629);
#72285=AXIS2_PLACEMENT_3D('',#102261,#79630,#79631);
#72286=AXIS2_PLACEMENT_3D('',#102274,#79632,#79633);
#72287=AXIS2_PLACEMENT_3D('',#102309,#79634,#79635);
#72288=AXIS2_PLACEMENT_3D('',#102344,#79636,#79637);
#72289=AXIS2_PLACEMENT_3D('',#102379,#79638,#79639);
#72290=AXIS2_PLACEMENT_3D('',#102414,#79640,#79641);
#72291=AXIS2_PLACEMENT_3D('',#102449,#79642,#79643);
#72292=AXIS2_PLACEMENT_3D('',#102484,#79644,#79645);
#72293=AXIS2_PLACEMENT_3D('',#102519,#79646,#79647);
#72294=AXIS2_PLACEMENT_3D('',#102554,#79648,#79649);
#72295=AXIS2_PLACEMENT_3D('',#102589,#79650,#79651);
#72296=AXIS2_PLACEMENT_3D('',#102624,#79652,#79653);
#72297=AXIS2_PLACEMENT_3D('',#102659,#79654,#79655);
#72298=AXIS2_PLACEMENT_3D('',#102694,#79656,#79657);
#72299=AXIS2_PLACEMENT_3D('',#102729,#79658,#79659);
#72300=AXIS2_PLACEMENT_3D('',#102764,#79660,#79661);
#72301=AXIS2_PLACEMENT_3D('',#102799,#79662,#79663);
#72302=AXIS2_PLACEMENT_3D('',#102834,#79664,#79665);
#72303=AXIS2_PLACEMENT_3D('',#102869,#79666,#79667);
#72304=AXIS2_PLACEMENT_3D('',#102904,#79668,#79669);
#72305=AXIS2_PLACEMENT_3D('',#102939,#79670,#79671);
#72306=AXIS2_PLACEMENT_3D('',#102974,#79672,#79673);
#72307=AXIS2_PLACEMENT_3D('',#103009,#79674,#79675);
#72308=AXIS2_PLACEMENT_3D('',#103044,#79676,#79677);
#72309=AXIS2_PLACEMENT_3D('',#103079,#79678,#79679);
#72310=AXIS2_PLACEMENT_3D('',#103114,#79680,#79681);
#72311=AXIS2_PLACEMENT_3D('',#103149,#79682,#79683);
#72312=AXIS2_PLACEMENT_3D('',#103184,#79684,#79685);
#72313=AXIS2_PLACEMENT_3D('',#103219,#79686,#79687);
#72314=AXIS2_PLACEMENT_3D('',#103254,#79688,#79689);
#72315=AXIS2_PLACEMENT_3D('',#103289,#79690,#79691);
#72316=AXIS2_PLACEMENT_3D('',#103320,#79692,#79693);
#72317=AXIS2_PLACEMENT_3D('',#103351,#79694,#79695);
#72318=AXIS2_PLACEMENT_3D('',#103382,#79696,#79697);
#72319=AXIS2_PLACEMENT_3D('',#103413,#79698,#79699);
#72320=AXIS2_PLACEMENT_3D('',#103444,#79700,#79701);
#72321=AXIS2_PLACEMENT_3D('',#103475,#79702,#79703);
#72322=AXIS2_PLACEMENT_3D('',#103506,#79704,#79705);
#72323=AXIS2_PLACEMENT_3D('',#103537,#79706,#79707);
#72324=AXIS2_PLACEMENT_3D('',#103568,#79708,#79709);
#72325=AXIS2_PLACEMENT_3D('',#103599,#79710,#79711);
#72326=AXIS2_PLACEMENT_3D('',#103630,#79712,#79713);
#72327=AXIS2_PLACEMENT_3D('',#103661,#79714,#79715);
#72328=AXIS2_PLACEMENT_3D('',#103692,#79716,#79717);
#72329=AXIS2_PLACEMENT_3D('',#103723,#79718,#79719);
#72330=AXIS2_PLACEMENT_3D('',#103754,#79720,#79721);
#72331=AXIS2_PLACEMENT_3D('',#103785,#79722,#79723);
#72332=AXIS2_PLACEMENT_3D('',#103816,#79724,#79725);
#72333=AXIS2_PLACEMENT_3D('',#103847,#79726,#79727);
#72334=AXIS2_PLACEMENT_3D('',#103878,#79728,#79729);
#72335=AXIS2_PLACEMENT_3D('',#103909,#79730,#79731);
#72336=AXIS2_PLACEMENT_3D('',#103940,#79732,#79733);
#72337=AXIS2_PLACEMENT_3D('',#103971,#79734,#79735);
#72338=AXIS2_PLACEMENT_3D('',#104002,#79736,#79737);
#72339=AXIS2_PLACEMENT_3D('',#104033,#79738,#79739);
#72340=AXIS2_PLACEMENT_3D('',#104064,#79740,#79741);
#72341=AXIS2_PLACEMENT_3D('',#104095,#79742,#79743);
#72342=AXIS2_PLACEMENT_3D('',#104126,#79744,#79745);
#72343=AXIS2_PLACEMENT_3D('',#104157,#79746,#79747);
#72344=AXIS2_PLACEMENT_3D('',#104189,#79748,#79749);
#72345=AXIS2_PLACEMENT_3D('',#104227,#79752,#79753);
#72346=AXIS2_PLACEMENT_3D('',#104229,#79754,#79755);
#72347=AXIS2_PLACEMENT_3D('',#104231,#79756,#79757);
#72348=AXIS2_PLACEMENT_3D('',#104232,#79758,#79759);
#72349=AXIS2_PLACEMENT_3D('',#104270,#79762,#79763);
#72350=AXIS2_PLACEMENT_3D('',#104272,#79764,#79765);
#72351=AXIS2_PLACEMENT_3D('',#104274,#79766,#79767);
#72352=AXIS2_PLACEMENT_3D('',#104275,#79768,#79769);
#72353=AXIS2_PLACEMENT_3D('',#104313,#79772,#79773);
#72354=AXIS2_PLACEMENT_3D('',#104315,#79774,#79775);
#72355=AXIS2_PLACEMENT_3D('',#104317,#79776,#79777);
#72356=AXIS2_PLACEMENT_3D('',#104318,#79778,#79779);
#72357=AXIS2_PLACEMENT_3D('',#104356,#79782,#79783);
#72358=AXIS2_PLACEMENT_3D('',#104358,#79784,#79785);
#72359=AXIS2_PLACEMENT_3D('',#104360,#79786,#79787);
#72360=AXIS2_PLACEMENT_3D('',#104361,#79788,#79789);
#72361=AXIS2_PLACEMENT_3D('',#104399,#79792,#79793);
#72362=AXIS2_PLACEMENT_3D('',#104401,#79794,#79795);
#72363=AXIS2_PLACEMENT_3D('',#104403,#79796,#79797);
#72364=AXIS2_PLACEMENT_3D('',#104404,#79798,#79799);
#72365=AXIS2_PLACEMENT_3D('',#104442,#79802,#79803);
#72366=AXIS2_PLACEMENT_3D('',#104444,#79804,#79805);
#72367=AXIS2_PLACEMENT_3D('',#104446,#79806,#79807);
#72368=AXIS2_PLACEMENT_3D('',#104447,#79808,#79809);
#72369=AXIS2_PLACEMENT_3D('',#104513,#79814,#79815);
#72370=AXIS2_PLACEMENT_3D('',#104515,#79816,#79817);
#72371=AXIS2_PLACEMENT_3D('',#104517,#79818,#79819);
#72372=AXIS2_PLACEMENT_3D('',#104518,#79820,#79821);
#72373=AXIS2_PLACEMENT_3D('',#104556,#79824,#79825);
#72374=AXIS2_PLACEMENT_3D('',#104558,#79826,#79827);
#72375=AXIS2_PLACEMENT_3D('',#104560,#79828,#79829);
#72376=AXIS2_PLACEMENT_3D('',#104561,#79830,#79831);
#72377=AXIS2_PLACEMENT_3D('',#104599,#79834,#79835);
#72378=AXIS2_PLACEMENT_3D('',#104601,#79836,#79837);
#72379=AXIS2_PLACEMENT_3D('',#104603,#79838,#79839);
#72380=AXIS2_PLACEMENT_3D('',#104604,#79840,#79841);
#72381=AXIS2_PLACEMENT_3D('',#104642,#79844,#79845);
#72382=AXIS2_PLACEMENT_3D('',#104644,#79846,#79847);
#72383=AXIS2_PLACEMENT_3D('',#104646,#79848,#79849);
#72384=AXIS2_PLACEMENT_3D('',#104647,#79850,#79851);
#72385=AXIS2_PLACEMENT_3D('',#104685,#79854,#79855);
#72386=AXIS2_PLACEMENT_3D('',#104687,#79856,#79857);
#72387=AXIS2_PLACEMENT_3D('',#104689,#79858,#79859);
#72388=AXIS2_PLACEMENT_3D('',#104690,#79860,#79861);
#72389=AXIS2_PLACEMENT_3D('',#104728,#79864,#79865);
#72390=AXIS2_PLACEMENT_3D('',#104730,#79866,#79867);
#72391=AXIS2_PLACEMENT_3D('',#104732,#79868,#79869);
#72392=AXIS2_PLACEMENT_3D('',#104733,#79870,#79871);
#72393=AXIS2_PLACEMENT_3D('',#104771,#79874,#79875);
#72394=AXIS2_PLACEMENT_3D('',#104773,#79876,#79877);
#72395=AXIS2_PLACEMENT_3D('',#104775,#79878,#79879);
#72396=AXIS2_PLACEMENT_3D('',#104776,#79880,#79881);
#72397=AXIS2_PLACEMENT_3D('',#104814,#79884,#79885);
#72398=AXIS2_PLACEMENT_3D('',#104816,#79886,#79887);
#72399=AXIS2_PLACEMENT_3D('',#104818,#79888,#79889);
#72400=AXIS2_PLACEMENT_3D('',#104819,#79890,#79891);
#72401=AXIS2_PLACEMENT_3D('',#104857,#79894,#79895);
#72402=AXIS2_PLACEMENT_3D('',#104859,#79896,#79897);
#72403=AXIS2_PLACEMENT_3D('',#104861,#79898,#79899);
#72404=AXIS2_PLACEMENT_3D('',#104862,#79900,#79901);
#72405=AXIS2_PLACEMENT_3D('',#104900,#79904,#79905);
#72406=AXIS2_PLACEMENT_3D('',#104902,#79906,#79907);
#72407=AXIS2_PLACEMENT_3D('',#104904,#79908,#79909);
#72408=AXIS2_PLACEMENT_3D('',#104905,#79910,#79911);
#72409=AXIS2_PLACEMENT_3D('',#104943,#79914,#79915);
#72410=AXIS2_PLACEMENT_3D('',#104945,#79916,#79917);
#72411=AXIS2_PLACEMENT_3D('',#104947,#79918,#79919);
#72412=AXIS2_PLACEMENT_3D('',#104948,#79920,#79921);
#72413=AXIS2_PLACEMENT_3D('',#104986,#79924,#79925);
#72414=AXIS2_PLACEMENT_3D('',#104988,#79926,#79927);
#72415=AXIS2_PLACEMENT_3D('',#104990,#79928,#79929);
#72416=AXIS2_PLACEMENT_3D('',#104991,#79930,#79931);
#72417=AXIS2_PLACEMENT_3D('',#105029,#79934,#79935);
#72418=AXIS2_PLACEMENT_3D('',#105031,#79936,#79937);
#72419=AXIS2_PLACEMENT_3D('',#105033,#79938,#79939);
#72420=AXIS2_PLACEMENT_3D('',#105034,#79940,#79941);
#72421=AXIS2_PLACEMENT_3D('',#105072,#79944,#79945);
#72422=AXIS2_PLACEMENT_3D('',#105074,#79946,#79947);
#72423=AXIS2_PLACEMENT_3D('',#105076,#79948,#79949);
#72424=AXIS2_PLACEMENT_3D('',#105077,#79950,#79951);
#72425=AXIS2_PLACEMENT_3D('',#105115,#79954,#79955);
#72426=AXIS2_PLACEMENT_3D('',#105117,#79956,#79957);
#72427=AXIS2_PLACEMENT_3D('',#105119,#79958,#79959);
#72428=AXIS2_PLACEMENT_3D('',#105120,#79960,#79961);
#72429=AXIS2_PLACEMENT_3D('',#105158,#79964,#79965);
#72430=AXIS2_PLACEMENT_3D('',#105160,#79966,#79967);
#72431=AXIS2_PLACEMENT_3D('',#105162,#79968,#79969);
#72432=AXIS2_PLACEMENT_3D('',#105163,#79970,#79971);
#72433=AXIS2_PLACEMENT_3D('',#105208,#79974,#79975);
#72434=AXIS2_PLACEMENT_3D('',#105210,#79977,#79978);
#72435=AXIS2_PLACEMENT_3D('',#105212,#79979,#79980);
#72436=AXIS2_PLACEMENT_3D('',#105213,#79981,#79982);
#72437=AXIS2_PLACEMENT_3D('',#105244,#79984,#79985);
#72438=AXIS2_PLACEMENT_3D('',#105246,#79986,#79987);
#72439=AXIS2_PLACEMENT_3D('',#105248,#79988,#79989);
#72440=AXIS2_PLACEMENT_3D('',#105249,#79990,#79991);
#72441=AXIS2_PLACEMENT_3D('',#105287,#79994,#79995);
#72442=AXIS2_PLACEMENT_3D('',#105289,#79996,#79997);
#72443=AXIS2_PLACEMENT_3D('',#105291,#79998,#79999);
#72444=AXIS2_PLACEMENT_3D('',#105292,#80000,#80001);
#72445=AXIS2_PLACEMENT_3D('',#105330,#80004,#80005);
#72446=AXIS2_PLACEMENT_3D('',#105332,#80006,#80007);
#72447=AXIS2_PLACEMENT_3D('',#105334,#80008,#80009);
#72448=AXIS2_PLACEMENT_3D('',#105335,#80010,#80011);
#72449=AXIS2_PLACEMENT_3D('',#105373,#80014,#80015);
#72450=AXIS2_PLACEMENT_3D('',#105375,#80016,#80017);
#72451=AXIS2_PLACEMENT_3D('',#105377,#80018,#80019);
#72452=AXIS2_PLACEMENT_3D('',#105378,#80020,#80021);
#72453=AXIS2_PLACEMENT_3D('',#105386,#80023,#80024);
#72454=AXIS2_PLACEMENT_3D('',#105389,#80025,#80026);
#72455=AXIS2_PLACEMENT_3D('',#105390,#80027,#80028);
#72456=AXIS2_PLACEMENT_3D('',#105431,#80030,#80031);
#72457=AXIS2_PLACEMENT_3D('',#105474,#80034,#80035);
#72458=AXIS2_PLACEMENT_3D('',#105476,#80037,#80038);
#72459=AXIS2_PLACEMENT_3D('',#105478,#80039,#80040);
#72460=AXIS2_PLACEMENT_3D('',#105479,#80041,#80042);
#72461=AXIS2_PLACEMENT_3D('',#105521,#80044,#80045);
#72462=AXIS2_PLACEMENT_3D('',#105523,#80047,#80048);
#72463=AXIS2_PLACEMENT_3D('',#105525,#80049,#80050);
#72464=AXIS2_PLACEMENT_3D('',#105526,#80051,#80052);
#72465=AXIS2_PLACEMENT_3D('',#105568,#80054,#80055);
#72466=AXIS2_PLACEMENT_3D('',#105570,#80057,#80058);
#72467=AXIS2_PLACEMENT_3D('',#105572,#80059,#80060);
#72468=AXIS2_PLACEMENT_3D('',#105573,#80061,#80062);
#72469=AXIS2_PLACEMENT_3D('',#105615,#80064,#80065);
#72470=AXIS2_PLACEMENT_3D('',#105617,#80067,#80068);
#72471=AXIS2_PLACEMENT_3D('',#105619,#80069,#80070);
#72472=AXIS2_PLACEMENT_3D('',#105620,#80071,#80072);
#72473=AXIS2_PLACEMENT_3D('',#105662,#80074,#80075);
#72474=AXIS2_PLACEMENT_3D('',#105664,#80077,#80078);
#72475=AXIS2_PLACEMENT_3D('',#105666,#80079,#80080);
#72476=AXIS2_PLACEMENT_3D('',#105667,#80081,#80082);
#72477=AXIS2_PLACEMENT_3D('',#105709,#80084,#80085);
#72478=AXIS2_PLACEMENT_3D('',#105711,#80087,#80088);
#72479=AXIS2_PLACEMENT_3D('',#105713,#80089,#80090);
#72480=AXIS2_PLACEMENT_3D('',#105714,#80091,#80092);
#72481=AXIS2_PLACEMENT_3D('',#105756,#80094,#80095);
#72482=AXIS2_PLACEMENT_3D('',#105758,#80097,#80098);
#72483=AXIS2_PLACEMENT_3D('',#105760,#80099,#80100);
#72484=AXIS2_PLACEMENT_3D('',#105761,#80101,#80102);
#72485=AXIS2_PLACEMENT_3D('',#105803,#80104,#80105);
#72486=AXIS2_PLACEMENT_3D('',#105805,#80107,#80108);
#72487=AXIS2_PLACEMENT_3D('',#105807,#80109,#80110);
#72488=AXIS2_PLACEMENT_3D('',#105808,#80111,#80112);
#72489=AXIS2_PLACEMENT_3D('',#105850,#80114,#80115);
#72490=AXIS2_PLACEMENT_3D('',#105852,#80117,#80118);
#72491=AXIS2_PLACEMENT_3D('',#105854,#80119,#80120);
#72492=AXIS2_PLACEMENT_3D('',#105855,#80121,#80122);
#72493=AXIS2_PLACEMENT_3D('',#105897,#80124,#80125);
#72494=AXIS2_PLACEMENT_3D('',#105899,#80127,#80128);
#72495=AXIS2_PLACEMENT_3D('',#105901,#80129,#80130);
#72496=AXIS2_PLACEMENT_3D('',#105902,#80131,#80132);
#72497=AXIS2_PLACEMENT_3D('',#105944,#80134,#80135);
#72498=AXIS2_PLACEMENT_3D('',#105946,#80137,#80138);
#72499=AXIS2_PLACEMENT_3D('',#105948,#80139,#80140);
#72500=AXIS2_PLACEMENT_3D('',#105949,#80141,#80142);
#72501=AXIS2_PLACEMENT_3D('',#105991,#80144,#80145);
#72502=AXIS2_PLACEMENT_3D('',#105993,#80147,#80148);
#72503=AXIS2_PLACEMENT_3D('',#105995,#80149,#80150);
#72504=AXIS2_PLACEMENT_3D('',#105996,#80151,#80152);
#72505=AXIS2_PLACEMENT_3D('',#106038,#80154,#80155);
#72506=AXIS2_PLACEMENT_3D('',#106040,#80157,#80158);
#72507=AXIS2_PLACEMENT_3D('',#106042,#80159,#80160);
#72508=AXIS2_PLACEMENT_3D('',#106043,#80161,#80162);
#72509=AXIS2_PLACEMENT_3D('',#106117,#80166,#80167);
#72510=AXIS2_PLACEMENT_3D('',#106119,#80169,#80170);
#72511=AXIS2_PLACEMENT_3D('',#106121,#80171,#80172);
#72512=AXIS2_PLACEMENT_3D('',#106122,#80173,#80174);
#72513=AXIS2_PLACEMENT_3D('',#106164,#80176,#80177);
#72514=AXIS2_PLACEMENT_3D('',#106166,#80179,#80180);
#72515=AXIS2_PLACEMENT_3D('',#106168,#80181,#80182);
#72516=AXIS2_PLACEMENT_3D('',#106169,#80183,#80184);
#72517=AXIS2_PLACEMENT_3D('',#106211,#80186,#80187);
#72518=AXIS2_PLACEMENT_3D('',#106213,#80189,#80190);
#72519=AXIS2_PLACEMENT_3D('',#106215,#80191,#80192);
#72520=AXIS2_PLACEMENT_3D('',#106216,#80193,#80194);
#72521=AXIS2_PLACEMENT_3D('',#106258,#80196,#80197);
#72522=AXIS2_PLACEMENT_3D('',#106260,#80199,#80200);
#72523=AXIS2_PLACEMENT_3D('',#106262,#80201,#80202);
#72524=AXIS2_PLACEMENT_3D('',#106263,#80203,#80204);
#72525=AXIS2_PLACEMENT_3D('',#106305,#80206,#80207);
#72526=AXIS2_PLACEMENT_3D('',#106307,#80209,#80210);
#72527=AXIS2_PLACEMENT_3D('',#106309,#80211,#80212);
#72528=AXIS2_PLACEMENT_3D('',#106310,#80213,#80214);
#72529=AXIS2_PLACEMENT_3D('',#106352,#80216,#80217);
#72530=AXIS2_PLACEMENT_3D('',#106354,#80219,#80220);
#72531=AXIS2_PLACEMENT_3D('',#106356,#80221,#80222);
#72532=AXIS2_PLACEMENT_3D('',#106357,#80223,#80224);
#72533=AXIS2_PLACEMENT_3D('',#106399,#80226,#80227);
#72534=AXIS2_PLACEMENT_3D('',#106401,#80229,#80230);
#72535=AXIS2_PLACEMENT_3D('',#106403,#80231,#80232);
#72536=AXIS2_PLACEMENT_3D('',#106404,#80233,#80234);
#72537=AXIS2_PLACEMENT_3D('',#106446,#80236,#80237);
#72538=AXIS2_PLACEMENT_3D('',#106448,#80239,#80240);
#72539=AXIS2_PLACEMENT_3D('',#106450,#80241,#80242);
#72540=AXIS2_PLACEMENT_3D('',#106451,#80243,#80244);
#72541=AXIS2_PLACEMENT_3D('',#106493,#80246,#80247);
#72542=AXIS2_PLACEMENT_3D('',#106495,#80249,#80250);
#72543=AXIS2_PLACEMENT_3D('',#106497,#80251,#80252);
#72544=AXIS2_PLACEMENT_3D('',#106498,#80253,#80254);
#72545=AXIS2_PLACEMENT_3D('',#106540,#80256,#80257);
#72546=AXIS2_PLACEMENT_3D('',#106542,#80259,#80260);
#72547=AXIS2_PLACEMENT_3D('',#106544,#80261,#80262);
#72548=AXIS2_PLACEMENT_3D('',#106545,#80263,#80264);
#72549=AXIS2_PLACEMENT_3D('',#106587,#80266,#80267);
#72550=AXIS2_PLACEMENT_3D('',#106589,#80269,#80270);
#72551=AXIS2_PLACEMENT_3D('',#106591,#80271,#80272);
#72552=AXIS2_PLACEMENT_3D('',#106592,#80273,#80274);
#72553=AXIS2_PLACEMENT_3D('',#106634,#80276,#80277);
#72554=AXIS2_PLACEMENT_3D('',#106636,#80279,#80280);
#72555=AXIS2_PLACEMENT_3D('',#106638,#80281,#80282);
#72556=AXIS2_PLACEMENT_3D('',#106639,#80283,#80284);
#72557=AXIS2_PLACEMENT_3D('',#106681,#80286,#80287);
#72558=AXIS2_PLACEMENT_3D('',#106683,#80289,#80290);
#72559=AXIS2_PLACEMENT_3D('',#106685,#80291,#80292);
#72560=AXIS2_PLACEMENT_3D('',#106686,#80293,#80294);
#72561=AXIS2_PLACEMENT_3D('',#106728,#80296,#80297);
#72562=AXIS2_PLACEMENT_3D('',#106730,#80299,#80300);
#72563=AXIS2_PLACEMENT_3D('',#106732,#80301,#80302);
#72564=AXIS2_PLACEMENT_3D('',#106733,#80303,#80304);
#72565=AXIS2_PLACEMENT_3D('',#106734,#80305,#80306);
#72566=AXIS2_PLACEMENT_3D('',#106744,#80307,#80308);
#72567=AXIS2_PLACEMENT_3D('',#106745,#80309,#80310);
#72568=AXIS2_PLACEMENT_3D('',#106768,#80312,#80313);
#72569=AXIS2_PLACEMENT_3D('',#106791,#80314,#80315);
#72570=AXIS2_PLACEMENT_3D('',#106804,#80316,#80317);
#72571=AXIS2_PLACEMENT_3D('',#106821,#80318,#80319);
#72572=AXIS2_PLACEMENT_3D('',#106834,#80320,#80321);
#72573=AXIS2_PLACEMENT_3D('',#106851,#80322,#80323);
#72574=AXIS2_PLACEMENT_3D('',#106864,#80324,#80325);
#72575=AXIS2_PLACEMENT_3D('',#106881,#80326,#80327);
#72576=AXIS2_PLACEMENT_3D('',#106894,#80328,#80329);
#72577=AXIS2_PLACEMENT_3D('',#106911,#80330,#80331);
#72578=AXIS2_PLACEMENT_3D('',#106924,#80332,#80333);
#72579=AXIS2_PLACEMENT_3D('',#106941,#80334,#80335);
#72580=AXIS2_PLACEMENT_3D('',#106954,#80336,#80337);
#72581=AXIS2_PLACEMENT_3D('',#106971,#80338,#80339);
#72582=AXIS2_PLACEMENT_3D('',#106984,#80340,#80341);
#72583=AXIS2_PLACEMENT_3D('',#107001,#80342,#80343);
#72584=AXIS2_PLACEMENT_3D('',#107014,#80344,#80345);
#72585=AXIS2_PLACEMENT_3D('',#107031,#80346,#80347);
#72586=AXIS2_PLACEMENT_3D('',#107044,#80348,#80349);
#72587=AXIS2_PLACEMENT_3D('',#107061,#80350,#80351);
#72588=AXIS2_PLACEMENT_3D('',#107074,#80352,#80353);
#72589=AXIS2_PLACEMENT_3D('',#107091,#80354,#80355);
#72590=AXIS2_PLACEMENT_3D('',#107104,#80356,#80357);
#72591=AXIS2_PLACEMENT_3D('',#107121,#80358,#80359);
#72592=AXIS2_PLACEMENT_3D('',#107134,#80360,#80361);
#72593=AXIS2_PLACEMENT_3D('',#107151,#80362,#80363);
#72594=AXIS2_PLACEMENT_3D('',#107164,#80364,#80365);
#72595=AXIS2_PLACEMENT_3D('',#107181,#80366,#80367);
#72596=AXIS2_PLACEMENT_3D('',#107194,#80368,#80369);
#72597=AXIS2_PLACEMENT_3D('',#107211,#80370,#80371);
#72598=AXIS2_PLACEMENT_3D('',#107224,#80372,#80373);
#72599=AXIS2_PLACEMENT_3D('',#107241,#80374,#80375);
#72600=AXIS2_PLACEMENT_3D('',#107254,#80376,#80377);
#72601=AXIS2_PLACEMENT_3D('',#107271,#80378,#80379);
#72602=AXIS2_PLACEMENT_3D('',#107284,#80380,#80381);
#72603=AXIS2_PLACEMENT_3D('',#107301,#80382,#80383);
#72604=AXIS2_PLACEMENT_3D('',#107314,#80384,#80385);
#72605=AXIS2_PLACEMENT_3D('',#107331,#80386,#80387);
#72606=AXIS2_PLACEMENT_3D('',#107344,#80388,#80389);
#72607=AXIS2_PLACEMENT_3D('',#107361,#80390,#80391);
#72608=AXIS2_PLACEMENT_3D('',#107374,#80392,#80393);
#72609=AXIS2_PLACEMENT_3D('',#107391,#80394,#80395);
#72610=AXIS2_PLACEMENT_3D('',#107404,#80396,#80397);
#72611=AXIS2_PLACEMENT_3D('',#107421,#80398,#80399);
#72612=AXIS2_PLACEMENT_3D('',#107434,#80400,#80401);
#72613=AXIS2_PLACEMENT_3D('',#107451,#80402,#80403);
#72614=AXIS2_PLACEMENT_3D('',#107464,#80404,#80405);
#72615=AXIS2_PLACEMENT_3D('',#107481,#80406,#80407);
#72616=AXIS2_PLACEMENT_3D('',#107494,#80408,#80409);
#72617=AXIS2_PLACEMENT_3D('',#107511,#80410,#80411);
#72618=AXIS2_PLACEMENT_3D('',#107524,#80412,#80413);
#72619=AXIS2_PLACEMENT_3D('',#107541,#80414,#80415);
#72620=AXIS2_PLACEMENT_3D('',#107554,#80416,#80417);
#72621=AXIS2_PLACEMENT_3D('',#107571,#80418,#80419);
#72622=AXIS2_PLACEMENT_3D('',#107584,#80420,#80421);
#72623=AXIS2_PLACEMENT_3D('',#107601,#80422,#80423);
#72624=AXIS2_PLACEMENT_3D('',#107614,#80424,#80425);
#72625=AXIS2_PLACEMENT_3D('',#107630,#80426,#80427);
#72626=AXIS2_PLACEMENT_3D('',#107644,#80428,#80429);
#72627=AXIS2_PLACEMENT_3D('',#107678,#80430,#80431);
#72628=AXIS2_PLACEMENT_3D('',#107712,#80432,#80433);
#72629=AXIS2_PLACEMENT_3D('',#107746,#80434,#80435);
#72630=AXIS2_PLACEMENT_3D('',#107780,#80436,#80437);
#72631=AXIS2_PLACEMENT_3D('',#107814,#80438,#80439);
#72632=AXIS2_PLACEMENT_3D('',#107848,#80440,#80441);
#72633=AXIS2_PLACEMENT_3D('',#107882,#80442,#80443);
#72634=AXIS2_PLACEMENT_3D('',#107916,#80444,#80445);
#72635=AXIS2_PLACEMENT_3D('',#107950,#80446,#80447);
#72636=AXIS2_PLACEMENT_3D('',#107984,#80448,#80449);
#72637=AXIS2_PLACEMENT_3D('',#108018,#80450,#80451);
#72638=AXIS2_PLACEMENT_3D('',#108052,#80452,#80453);
#72639=AXIS2_PLACEMENT_3D('',#108086,#80454,#80455);
#72640=AXIS2_PLACEMENT_3D('',#108120,#80456,#80457);
#72641=AXIS2_PLACEMENT_3D('',#108154,#80458,#80459);
#72642=AXIS2_PLACEMENT_3D('',#108188,#80460,#80461);
#72643=AXIS2_PLACEMENT_3D('',#108222,#80462,#80463);
#72644=AXIS2_PLACEMENT_3D('',#108256,#80464,#80465);
#72645=AXIS2_PLACEMENT_3D('',#108290,#80466,#80467);
#72646=AXIS2_PLACEMENT_3D('',#108324,#80468,#80469);
#72647=AXIS2_PLACEMENT_3D('',#108358,#80470,#80471);
#72648=AXIS2_PLACEMENT_3D('',#108392,#80472,#80473);
#72649=AXIS2_PLACEMENT_3D('',#108426,#80474,#80475);
#72650=AXIS2_PLACEMENT_3D('',#108460,#80476,#80477);
#72651=AXIS2_PLACEMENT_3D('',#108494,#80478,#80479);
#72652=AXIS2_PLACEMENT_3D('',#108528,#80480,#80481);
#72653=AXIS2_PLACEMENT_3D('',#108562,#80482,#80483);
#72654=AXIS2_PLACEMENT_3D('',#108596,#80484,#80485);
#72655=AXIS2_PLACEMENT_3D('',#108624,#80486,#80487);
#72656=AXIS2_PLACEMENT_3D('',#108632,#80489,#80490);
#72657=AXIS2_PLACEMENT_3D('',#108634,#80491,#80492);
#72658=AXIS2_PLACEMENT_3D('',#108636,#80493,#80494);
#72659=AXIS2_PLACEMENT_3D('',#108637,#80495,#80496);
#72660=AXIS2_PLACEMENT_3D('',#108660,#80498,#80499);
#72661=AXIS2_PLACEMENT_3D('',#108668,#80501,#80502);
#72662=AXIS2_PLACEMENT_3D('',#108670,#80503,#80504);
#72663=AXIS2_PLACEMENT_3D('',#108672,#80505,#80506);
#72664=AXIS2_PLACEMENT_3D('',#108673,#80507,#80508);
#72665=AXIS2_PLACEMENT_3D('',#108696,#80510,#80511);
#72666=AXIS2_PLACEMENT_3D('',#108704,#80513,#80514);
#72667=AXIS2_PLACEMENT_3D('',#108706,#80515,#80516);
#72668=AXIS2_PLACEMENT_3D('',#108708,#80517,#80518);
#72669=AXIS2_PLACEMENT_3D('',#108709,#80519,#80520);
#72670=AXIS2_PLACEMENT_3D('',#108732,#80522,#80523);
#72671=AXIS2_PLACEMENT_3D('',#108740,#80525,#80526);
#72672=AXIS2_PLACEMENT_3D('',#108742,#80527,#80528);
#72673=AXIS2_PLACEMENT_3D('',#108744,#80529,#80530);
#72674=AXIS2_PLACEMENT_3D('',#108745,#80531,#80532);
#72675=AXIS2_PLACEMENT_3D('',#108768,#80534,#80535);
#72676=AXIS2_PLACEMENT_3D('',#108776,#80537,#80538);
#72677=AXIS2_PLACEMENT_3D('',#108778,#80539,#80540);
#72678=AXIS2_PLACEMENT_3D('',#108780,#80541,#80542);
#72679=AXIS2_PLACEMENT_3D('',#108781,#80543,#80544);
#72680=AXIS2_PLACEMENT_3D('',#108804,#80546,#80547);
#72681=AXIS2_PLACEMENT_3D('',#108812,#80549,#80550);
#72682=AXIS2_PLACEMENT_3D('',#108814,#80551,#80552);
#72683=AXIS2_PLACEMENT_3D('',#108816,#80553,#80554);
#72684=AXIS2_PLACEMENT_3D('',#108817,#80555,#80556);
#72685=AXIS2_PLACEMENT_3D('',#108840,#80558,#80559);
#72686=AXIS2_PLACEMENT_3D('',#108848,#80561,#80562);
#72687=AXIS2_PLACEMENT_3D('',#108850,#80563,#80564);
#72688=AXIS2_PLACEMENT_3D('',#108852,#80565,#80566);
#72689=AXIS2_PLACEMENT_3D('',#108853,#80567,#80568);
#72690=AXIS2_PLACEMENT_3D('',#108876,#80570,#80571);
#72691=AXIS2_PLACEMENT_3D('',#108884,#80573,#80574);
#72692=AXIS2_PLACEMENT_3D('',#108886,#80575,#80576);
#72693=AXIS2_PLACEMENT_3D('',#108888,#80577,#80578);
#72694=AXIS2_PLACEMENT_3D('',#108889,#80579,#80580);
#72695=AXIS2_PLACEMENT_3D('',#108912,#80582,#80583);
#72696=AXIS2_PLACEMENT_3D('',#108920,#80585,#80586);
#72697=AXIS2_PLACEMENT_3D('',#108922,#80587,#80588);
#72698=AXIS2_PLACEMENT_3D('',#108924,#80589,#80590);
#72699=AXIS2_PLACEMENT_3D('',#108925,#80591,#80592);
#72700=AXIS2_PLACEMENT_3D('',#108948,#80594,#80595);
#72701=AXIS2_PLACEMENT_3D('',#108956,#80597,#80598);
#72702=AXIS2_PLACEMENT_3D('',#108958,#80599,#80600);
#72703=AXIS2_PLACEMENT_3D('',#108960,#80601,#80602);
#72704=AXIS2_PLACEMENT_3D('',#108961,#80603,#80604);
#72705=AXIS2_PLACEMENT_3D('',#108984,#80606,#80607);
#72706=AXIS2_PLACEMENT_3D('',#108992,#80609,#80610);
#72707=AXIS2_PLACEMENT_3D('',#108994,#80611,#80612);
#72708=AXIS2_PLACEMENT_3D('',#108996,#80613,#80614);
#72709=AXIS2_PLACEMENT_3D('',#108997,#80615,#80616);
#72710=AXIS2_PLACEMENT_3D('',#109020,#80618,#80619);
#72711=AXIS2_PLACEMENT_3D('',#109028,#80621,#80622);
#72712=AXIS2_PLACEMENT_3D('',#109030,#80623,#80624);
#72713=AXIS2_PLACEMENT_3D('',#109032,#80625,#80626);
#72714=AXIS2_PLACEMENT_3D('',#109033,#80627,#80628);
#72715=AXIS2_PLACEMENT_3D('',#109056,#80630,#80631);
#72716=AXIS2_PLACEMENT_3D('',#109064,#80633,#80634);
#72717=AXIS2_PLACEMENT_3D('',#109066,#80635,#80636);
#72718=AXIS2_PLACEMENT_3D('',#109068,#80637,#80638);
#72719=AXIS2_PLACEMENT_3D('',#109069,#80639,#80640);
#72720=AXIS2_PLACEMENT_3D('',#109092,#80642,#80643);
#72721=AXIS2_PLACEMENT_3D('',#109100,#80645,#80646);
#72722=AXIS2_PLACEMENT_3D('',#109102,#80647,#80648);
#72723=AXIS2_PLACEMENT_3D('',#109104,#80649,#80650);
#72724=AXIS2_PLACEMENT_3D('',#109105,#80651,#80652);
#72725=AXIS2_PLACEMENT_3D('',#109155,#80656,#80657);
#72726=AXIS2_PLACEMENT_3D('',#109163,#80659,#80660);
#72727=AXIS2_PLACEMENT_3D('',#109165,#80661,#80662);
#72728=AXIS2_PLACEMENT_3D('',#109167,#80663,#80664);
#72729=AXIS2_PLACEMENT_3D('',#109168,#80665,#80666);
#72730=AXIS2_PLACEMENT_3D('',#109191,#80668,#80669);
#72731=AXIS2_PLACEMENT_3D('',#109199,#80671,#80672);
#72732=AXIS2_PLACEMENT_3D('',#109201,#80673,#80674);
#72733=AXIS2_PLACEMENT_3D('',#109203,#80675,#80676);
#72734=AXIS2_PLACEMENT_3D('',#109204,#80677,#80678);
#72735=AXIS2_PLACEMENT_3D('',#109227,#80680,#80681);
#72736=AXIS2_PLACEMENT_3D('',#109235,#80683,#80684);
#72737=AXIS2_PLACEMENT_3D('',#109237,#80685,#80686);
#72738=AXIS2_PLACEMENT_3D('',#109239,#80687,#80688);
#72739=AXIS2_PLACEMENT_3D('',#109240,#80689,#80690);
#72740=AXIS2_PLACEMENT_3D('',#109263,#80692,#80693);
#72741=AXIS2_PLACEMENT_3D('',#109271,#80695,#80696);
#72742=AXIS2_PLACEMENT_3D('',#109273,#80697,#80698);
#72743=AXIS2_PLACEMENT_3D('',#109275,#80699,#80700);
#72744=AXIS2_PLACEMENT_3D('',#109276,#80701,#80702);
#72745=AXIS2_PLACEMENT_3D('',#109299,#80704,#80705);
#72746=AXIS2_PLACEMENT_3D('',#109307,#80707,#80708);
#72747=AXIS2_PLACEMENT_3D('',#109309,#80709,#80710);
#72748=AXIS2_PLACEMENT_3D('',#109311,#80711,#80712);
#72749=AXIS2_PLACEMENT_3D('',#109312,#80713,#80714);
#72750=AXIS2_PLACEMENT_3D('',#109335,#80716,#80717);
#72751=AXIS2_PLACEMENT_3D('',#109343,#80719,#80720);
#72752=AXIS2_PLACEMENT_3D('',#109345,#80721,#80722);
#72753=AXIS2_PLACEMENT_3D('',#109347,#80723,#80724);
#72754=AXIS2_PLACEMENT_3D('',#109348,#80725,#80726);
#72755=AXIS2_PLACEMENT_3D('',#109371,#80728,#80729);
#72756=AXIS2_PLACEMENT_3D('',#109379,#80731,#80732);
#72757=AXIS2_PLACEMENT_3D('',#109381,#80733,#80734);
#72758=AXIS2_PLACEMENT_3D('',#109383,#80735,#80736);
#72759=AXIS2_PLACEMENT_3D('',#109384,#80737,#80738);
#72760=AXIS2_PLACEMENT_3D('',#109407,#80740,#80741);
#72761=AXIS2_PLACEMENT_3D('',#109415,#80743,#80744);
#72762=AXIS2_PLACEMENT_3D('',#109417,#80745,#80746);
#72763=AXIS2_PLACEMENT_3D('',#109419,#80747,#80748);
#72764=AXIS2_PLACEMENT_3D('',#109420,#80749,#80750);
#72765=AXIS2_PLACEMENT_3D('',#109443,#80752,#80753);
#72766=AXIS2_PLACEMENT_3D('',#109461,#80755,#80756);
#72767=AXIS2_PLACEMENT_3D('',#109463,#80758,#80759);
#72768=AXIS2_PLACEMENT_3D('',#109465,#80760,#80761);
#72769=AXIS2_PLACEMENT_3D('',#109466,#80762,#80763);
#72770=AXIS2_PLACEMENT_3D('',#109480,#80765,#80766);
#72771=AXIS2_PLACEMENT_3D('',#109487,#80767,#80768);
#72772=AXIS2_PLACEMENT_3D('',#109489,#80769,#80770);
#72773=AXIS2_PLACEMENT_3D('',#109491,#80771,#80772);
#72774=AXIS2_PLACEMENT_3D('',#109492,#80773,#80774);
#72775=AXIS2_PLACEMENT_3D('',#109515,#80776,#80777);
#72776=AXIS2_PLACEMENT_3D('',#109523,#80779,#80780);
#72777=AXIS2_PLACEMENT_3D('',#109525,#80781,#80782);
#72778=AXIS2_PLACEMENT_3D('',#109527,#80783,#80784);
#72779=AXIS2_PLACEMENT_3D('',#109528,#80785,#80786);
#72780=AXIS2_PLACEMENT_3D('',#109551,#80788,#80789);
#72781=AXIS2_PLACEMENT_3D('',#109559,#80791,#80792);
#72782=AXIS2_PLACEMENT_3D('',#109561,#80793,#80794);
#72783=AXIS2_PLACEMENT_3D('',#109563,#80795,#80796);
#72784=AXIS2_PLACEMENT_3D('',#109564,#80797,#80798);
#72785=AXIS2_PLACEMENT_3D('',#109587,#80800,#80801);
#72786=AXIS2_PLACEMENT_3D('',#109595,#80803,#80804);
#72787=AXIS2_PLACEMENT_3D('',#109597,#80805,#80806);
#72788=AXIS2_PLACEMENT_3D('',#109599,#80807,#80808);
#72789=AXIS2_PLACEMENT_3D('',#109600,#80809,#80810);
#72790=AXIS2_PLACEMENT_3D('',#109623,#80812,#80813);
#72791=AXIS2_PLACEMENT_3D('',#109631,#80815,#80816);
#72792=AXIS2_PLACEMENT_3D('',#109633,#80817,#80818);
#72793=AXIS2_PLACEMENT_3D('',#109635,#80819,#80820);
#72794=AXIS2_PLACEMENT_3D('',#109636,#80821,#80822);
#72795=AXIS2_PLACEMENT_3D('',#109656,#80825,#80826);
#72796=AXIS2_PLACEMENT_3D('',#109686,#80828,#80829);
#72797=AXIS2_PLACEMENT_3D('',#109688,#80830,#80831);
#72798=AXIS2_PLACEMENT_3D('',#109689,#80832,#80833);
#72799=AXIS2_PLACEMENT_3D('',#109699,#80835,#80836);
#72800=AXIS2_PLACEMENT_3D('',#109729,#80838,#80839);
#72801=AXIS2_PLACEMENT_3D('',#109731,#80840,#80841);
#72802=AXIS2_PLACEMENT_3D('',#109732,#80842,#80843);
#72803=AXIS2_PLACEMENT_3D('',#109742,#80845,#80846);
#72804=AXIS2_PLACEMENT_3D('',#109772,#80848,#80849);
#72805=AXIS2_PLACEMENT_3D('',#109774,#80850,#80851);
#72806=AXIS2_PLACEMENT_3D('',#109775,#80852,#80853);
#72807=AXIS2_PLACEMENT_3D('',#109785,#80855,#80856);
#72808=AXIS2_PLACEMENT_3D('',#109815,#80858,#80859);
#72809=AXIS2_PLACEMENT_3D('',#109817,#80860,#80861);
#72810=AXIS2_PLACEMENT_3D('',#109818,#80862,#80863);
#72811=AXIS2_PLACEMENT_3D('',#109828,#80865,#80866);
#72812=AXIS2_PLACEMENT_3D('',#109858,#80868,#80869);
#72813=AXIS2_PLACEMENT_3D('',#109860,#80870,#80871);
#72814=AXIS2_PLACEMENT_3D('',#109861,#80872,#80873);
#72815=AXIS2_PLACEMENT_3D('',#109871,#80875,#80876);
#72816=AXIS2_PLACEMENT_3D('',#109901,#80878,#80879);
#72817=AXIS2_PLACEMENT_3D('',#109903,#80880,#80881);
#72818=AXIS2_PLACEMENT_3D('',#109904,#80882,#80883);
#72819=AXIS2_PLACEMENT_3D('',#109914,#80885,#80886);
#72820=AXIS2_PLACEMENT_3D('',#109944,#80888,#80889);
#72821=AXIS2_PLACEMENT_3D('',#109946,#80890,#80891);
#72822=AXIS2_PLACEMENT_3D('',#109947,#80892,#80893);
#72823=AXIS2_PLACEMENT_3D('',#109957,#80895,#80896);
#72824=AXIS2_PLACEMENT_3D('',#109987,#80898,#80899);
#72825=AXIS2_PLACEMENT_3D('',#109989,#80900,#80901);
#72826=AXIS2_PLACEMENT_3D('',#109990,#80902,#80903);
#72827=AXIS2_PLACEMENT_3D('',#110000,#80905,#80906);
#72828=AXIS2_PLACEMENT_3D('',#110030,#80908,#80909);
#72829=AXIS2_PLACEMENT_3D('',#110032,#80910,#80911);
#72830=AXIS2_PLACEMENT_3D('',#110033,#80912,#80913);
#72831=AXIS2_PLACEMENT_3D('',#110043,#80915,#80916);
#72832=AXIS2_PLACEMENT_3D('',#110073,#80918,#80919);
#72833=AXIS2_PLACEMENT_3D('',#110075,#80920,#80921);
#72834=AXIS2_PLACEMENT_3D('',#110076,#80922,#80923);
#72835=AXIS2_PLACEMENT_3D('',#110086,#80925,#80926);
#72836=AXIS2_PLACEMENT_3D('',#110116,#80928,#80929);
#72837=AXIS2_PLACEMENT_3D('',#110118,#80930,#80931);
#72838=AXIS2_PLACEMENT_3D('',#110119,#80932,#80933);
#72839=AXIS2_PLACEMENT_3D('',#110129,#80935,#80936);
#72840=AXIS2_PLACEMENT_3D('',#110159,#80938,#80939);
#72841=AXIS2_PLACEMENT_3D('',#110161,#80940,#80941);
#72842=AXIS2_PLACEMENT_3D('',#110162,#80942,#80943);
#72843=AXIS2_PLACEMENT_3D('',#110172,#80945,#80946);
#72844=AXIS2_PLACEMENT_3D('',#110202,#80948,#80949);
#72845=AXIS2_PLACEMENT_3D('',#110204,#80950,#80951);
#72846=AXIS2_PLACEMENT_3D('',#110205,#80952,#80953);
#72847=AXIS2_PLACEMENT_3D('',#110215,#80955,#80956);
#72848=AXIS2_PLACEMENT_3D('',#110245,#80958,#80959);
#72849=AXIS2_PLACEMENT_3D('',#110247,#80960,#80961);
#72850=AXIS2_PLACEMENT_3D('',#110248,#80962,#80963);
#72851=AXIS2_PLACEMENT_3D('',#110258,#80965,#80966);
#72852=AXIS2_PLACEMENT_3D('',#110288,#80968,#80969);
#72853=AXIS2_PLACEMENT_3D('',#110290,#80970,#80971);
#72854=AXIS2_PLACEMENT_3D('',#110291,#80972,#80973);
#72855=AXIS2_PLACEMENT_3D('',#110301,#80975,#80976);
#72856=AXIS2_PLACEMENT_3D('',#110331,#80978,#80979);
#72857=AXIS2_PLACEMENT_3D('',#110333,#80980,#80981);
#72858=AXIS2_PLACEMENT_3D('',#110334,#80982,#80983);
#72859=AXIS2_PLACEMENT_3D('',#110344,#80985,#80986);
#72860=AXIS2_PLACEMENT_3D('',#110374,#80988,#80989);
#72861=AXIS2_PLACEMENT_3D('',#110376,#80990,#80991);
#72862=AXIS2_PLACEMENT_3D('',#110377,#80992,#80993);
#72863=AXIS2_PLACEMENT_3D('',#110387,#80995,#80996);
#72864=AXIS2_PLACEMENT_3D('',#110417,#80998,#80999);
#72865=AXIS2_PLACEMENT_3D('',#110419,#81000,#81001);
#72866=AXIS2_PLACEMENT_3D('',#110420,#81002,#81003);
#72867=AXIS2_PLACEMENT_3D('',#110430,#81005,#81006);
#72868=AXIS2_PLACEMENT_3D('',#110460,#81008,#81009);
#72869=AXIS2_PLACEMENT_3D('',#110462,#81010,#81011);
#72870=AXIS2_PLACEMENT_3D('',#110463,#81012,#81013);
#72871=AXIS2_PLACEMENT_3D('',#110473,#81015,#81016);
#72872=AXIS2_PLACEMENT_3D('',#110503,#81018,#81019);
#72873=AXIS2_PLACEMENT_3D('',#110505,#81020,#81021);
#72874=AXIS2_PLACEMENT_3D('',#110506,#81022,#81023);
#72875=AXIS2_PLACEMENT_3D('',#110516,#81025,#81026);
#72876=AXIS2_PLACEMENT_3D('',#110546,#81028,#81029);
#72877=AXIS2_PLACEMENT_3D('',#110548,#81030,#81031);
#72878=AXIS2_PLACEMENT_3D('',#110549,#81032,#81033);
#72879=AXIS2_PLACEMENT_3D('',#110559,#81035,#81036);
#72880=AXIS2_PLACEMENT_3D('',#110589,#81038,#81039);
#72881=AXIS2_PLACEMENT_3D('',#110591,#81040,#81041);
#72882=AXIS2_PLACEMENT_3D('',#110592,#81042,#81043);
#72883=AXIS2_PLACEMENT_3D('',#110602,#81045,#81046);
#72884=AXIS2_PLACEMENT_3D('',#110632,#81048,#81049);
#72885=AXIS2_PLACEMENT_3D('',#110634,#81050,#81051);
#72886=AXIS2_PLACEMENT_3D('',#110635,#81052,#81053);
#72887=AXIS2_PLACEMENT_3D('',#110645,#81055,#81056);
#72888=AXIS2_PLACEMENT_3D('',#110675,#81058,#81059);
#72889=AXIS2_PLACEMENT_3D('',#110677,#81060,#81061);
#72890=AXIS2_PLACEMENT_3D('',#110678,#81062,#81063);
#72891=AXIS2_PLACEMENT_3D('',#110688,#81065,#81066);
#72892=AXIS2_PLACEMENT_3D('',#110718,#81068,#81069);
#72893=AXIS2_PLACEMENT_3D('',#110720,#81070,#81071);
#72894=AXIS2_PLACEMENT_3D('',#110721,#81072,#81073);
#72895=AXIS2_PLACEMENT_3D('',#110731,#81075,#81076);
#72896=AXIS2_PLACEMENT_3D('',#110761,#81078,#81079);
#72897=AXIS2_PLACEMENT_3D('',#110763,#81080,#81081);
#72898=AXIS2_PLACEMENT_3D('',#110764,#81082,#81083);
#72899=AXIS2_PLACEMENT_3D('',#110774,#81085,#81086);
#72900=AXIS2_PLACEMENT_3D('',#110804,#81088,#81089);
#72901=AXIS2_PLACEMENT_3D('',#110806,#81090,#81091);
#72902=AXIS2_PLACEMENT_3D('',#110807,#81092,#81093);
#72903=AXIS2_PLACEMENT_3D('',#110817,#81095,#81096);
#72904=AXIS2_PLACEMENT_3D('',#110847,#81098,#81099);
#72905=AXIS2_PLACEMENT_3D('',#110849,#81100,#81101);
#72906=AXIS2_PLACEMENT_3D('',#110850,#81102,#81103);
#72907=AXIS2_PLACEMENT_3D('',#110860,#81105,#81106);
#72908=AXIS2_PLACEMENT_3D('',#110890,#81108,#81109);
#72909=AXIS2_PLACEMENT_3D('',#110892,#81110,#81111);
#72910=AXIS2_PLACEMENT_3D('',#110893,#81112,#81113);
#72911=AXIS2_PLACEMENT_3D('',#110905,#81114,#81115);
#72912=AXIS2_PLACEMENT_3D('',#110918,#81116,#81117);
#72913=AXIS2_PLACEMENT_3D('',#110930,#81118,#81119);
#72914=AXIS2_PLACEMENT_3D('',#110943,#81120,#81121);
#72915=AXIS2_PLACEMENT_3D('',#110955,#81122,#81123);
#72916=AXIS2_PLACEMENT_3D('',#110968,#81124,#81125);
#72917=AXIS2_PLACEMENT_3D('',#110980,#81126,#81127);
#72918=AXIS2_PLACEMENT_3D('',#110993,#81128,#81129);
#72919=AXIS2_PLACEMENT_3D('',#111005,#81130,#81131);
#72920=AXIS2_PLACEMENT_3D('',#111018,#81132,#81133);
#72921=AXIS2_PLACEMENT_3D('',#111030,#81134,#81135);
#72922=AXIS2_PLACEMENT_3D('',#111043,#81136,#81137);
#72923=AXIS2_PLACEMENT_3D('',#111055,#81138,#81139);
#72924=AXIS2_PLACEMENT_3D('',#111068,#81140,#81141);
#72925=AXIS2_PLACEMENT_3D('',#111080,#81142,#81143);
#72926=AXIS2_PLACEMENT_3D('',#111093,#81144,#81145);
#72927=AXIS2_PLACEMENT_3D('',#111105,#81146,#81147);
#72928=AXIS2_PLACEMENT_3D('',#111118,#81148,#81149);
#72929=AXIS2_PLACEMENT_3D('',#111130,#81150,#81151);
#72930=AXIS2_PLACEMENT_3D('',#111143,#81152,#81153);
#72931=AXIS2_PLACEMENT_3D('',#111155,#81154,#81155);
#72932=AXIS2_PLACEMENT_3D('',#111168,#81156,#81157);
#72933=AXIS2_PLACEMENT_3D('',#111180,#81158,#81159);
#72934=AXIS2_PLACEMENT_3D('',#111193,#81160,#81161);
#72935=AXIS2_PLACEMENT_3D('',#111205,#81162,#81163);
#72936=AXIS2_PLACEMENT_3D('',#111218,#81164,#81165);
#72937=AXIS2_PLACEMENT_3D('',#111230,#81166,#81167);
#72938=AXIS2_PLACEMENT_3D('',#111243,#81168,#81169);
#72939=AXIS2_PLACEMENT_3D('',#111255,#81170,#81171);
#72940=AXIS2_PLACEMENT_3D('',#111268,#81172,#81173);
#72941=AXIS2_PLACEMENT_3D('',#111280,#81174,#81175);
#72942=AXIS2_PLACEMENT_3D('',#111293,#81176,#81177);
#72943=AXIS2_PLACEMENT_3D('',#111305,#81178,#81179);
#72944=AXIS2_PLACEMENT_3D('',#111318,#81180,#81181);
#72945=AXIS2_PLACEMENT_3D('',#111330,#81182,#81183);
#72946=AXIS2_PLACEMENT_3D('',#111343,#81184,#81185);
#72947=AXIS2_PLACEMENT_3D('',#111355,#81186,#81187);
#72948=AXIS2_PLACEMENT_3D('',#111368,#81188,#81189);
#72949=AXIS2_PLACEMENT_3D('',#111380,#81190,#81191);
#72950=AXIS2_PLACEMENT_3D('',#111393,#81192,#81193);
#72951=AXIS2_PLACEMENT_3D('',#111405,#81194,#81195);
#72952=AXIS2_PLACEMENT_3D('',#111418,#81196,#81197);
#72953=AXIS2_PLACEMENT_3D('',#111430,#81198,#81199);
#72954=AXIS2_PLACEMENT_3D('',#111443,#81200,#81201);
#72955=AXIS2_PLACEMENT_3D('',#111455,#81202,#81203);
#72956=AXIS2_PLACEMENT_3D('',#111468,#81204,#81205);
#72957=AXIS2_PLACEMENT_3D('',#111480,#81206,#81207);
#72958=AXIS2_PLACEMENT_3D('',#111493,#81208,#81209);
#72959=AXIS2_PLACEMENT_3D('',#111505,#81210,#81211);
#72960=AXIS2_PLACEMENT_3D('',#111518,#81212,#81213);
#72961=AXIS2_PLACEMENT_3D('',#111530,#81214,#81215);
#72962=AXIS2_PLACEMENT_3D('',#111543,#81216,#81217);
#72963=AXIS2_PLACEMENT_3D('',#111555,#81218,#81219);
#72964=AXIS2_PLACEMENT_3D('',#111568,#81220,#81221);
#72965=AXIS2_PLACEMENT_3D('',#111580,#81222,#81223);
#72966=AXIS2_PLACEMENT_3D('',#111593,#81224,#81225);
#72967=AXIS2_PLACEMENT_3D('',#111605,#81226,#81227);
#72968=AXIS2_PLACEMENT_3D('',#111618,#81228,#81229);
#72969=AXIS2_PLACEMENT_3D('',#111626,#81230,#81231);
#72970=AXIS2_PLACEMENT_3D('',#111643,#81232,#81233);
#72971=AXIS2_PLACEMENT_3D('',#111651,#81234,#81235);
#72972=AXIS2_PLACEMENT_3D('',#111668,#81236,#81237);
#72973=AXIS2_PLACEMENT_3D('',#111676,#81238,#81239);
#72974=AXIS2_PLACEMENT_3D('',#111693,#81240,#81241);
#72975=AXIS2_PLACEMENT_3D('',#111701,#81242,#81243);
#72976=AXIS2_PLACEMENT_3D('',#111718,#81244,#81245);
#72977=AXIS2_PLACEMENT_3D('',#111726,#81246,#81247);
#72978=AXIS2_PLACEMENT_3D('',#111743,#81248,#81249);
#72979=AXIS2_PLACEMENT_3D('',#111751,#81250,#81251);
#72980=AXIS2_PLACEMENT_3D('',#111768,#81252,#81253);
#72981=AXIS2_PLACEMENT_3D('',#111776,#81254,#81255);
#72982=AXIS2_PLACEMENT_3D('',#111793,#81256,#81257);
#72983=AXIS2_PLACEMENT_3D('',#111801,#81258,#81259);
#72984=AXIS2_PLACEMENT_3D('',#111818,#81260,#81261);
#72985=AXIS2_PLACEMENT_3D('',#111826,#81262,#81263);
#72986=AXIS2_PLACEMENT_3D('',#111843,#81264,#81265);
#72987=AXIS2_PLACEMENT_3D('',#111851,#81266,#81267);
#72988=AXIS2_PLACEMENT_3D('',#111868,#81268,#81269);
#72989=AXIS2_PLACEMENT_3D('',#111876,#81270,#81271);
#72990=AXIS2_PLACEMENT_3D('',#111893,#81272,#81273);
#72991=AXIS2_PLACEMENT_3D('',#111901,#81274,#81275);
#72992=AXIS2_PLACEMENT_3D('',#111918,#81276,#81277);
#72993=AXIS2_PLACEMENT_3D('',#111926,#81278,#81279);
#72994=AXIS2_PLACEMENT_3D('',#111943,#81280,#81281);
#72995=AXIS2_PLACEMENT_3D('',#111951,#81282,#81283);
#72996=AXIS2_PLACEMENT_3D('',#111968,#81284,#81285);
#72997=AXIS2_PLACEMENT_3D('',#111976,#81286,#81287);
#72998=AXIS2_PLACEMENT_3D('',#111993,#81288,#81289);
#72999=AXIS2_PLACEMENT_3D('',#112001,#81290,#81291);
#73000=AXIS2_PLACEMENT_3D('',#112018,#81292,#81293);
#73001=AXIS2_PLACEMENT_3D('',#112026,#81294,#81295);
#73002=AXIS2_PLACEMENT_3D('',#112043,#81296,#81297);
#73003=AXIS2_PLACEMENT_3D('',#112051,#81298,#81299);
#73004=AXIS2_PLACEMENT_3D('',#112068,#81300,#81301);
#73005=AXIS2_PLACEMENT_3D('',#112076,#81302,#81303);
#73006=AXIS2_PLACEMENT_3D('',#112093,#81304,#81305);
#73007=AXIS2_PLACEMENT_3D('',#112101,#81306,#81307);
#73008=AXIS2_PLACEMENT_3D('',#112118,#81308,#81309);
#73009=AXIS2_PLACEMENT_3D('',#112126,#81310,#81311);
#73010=AXIS2_PLACEMENT_3D('',#112143,#81312,#81313);
#73011=AXIS2_PLACEMENT_3D('',#112151,#81314,#81315);
#73012=AXIS2_PLACEMENT_3D('',#112168,#81316,#81317);
#73013=AXIS2_PLACEMENT_3D('',#112176,#81318,#81319);
#73014=AXIS2_PLACEMENT_3D('',#112193,#81320,#81321);
#73015=AXIS2_PLACEMENT_3D('',#112201,#81322,#81323);
#73016=AXIS2_PLACEMENT_3D('',#112218,#81324,#81325);
#73017=AXIS2_PLACEMENT_3D('',#112226,#81326,#81327);
#73018=AXIS2_PLACEMENT_3D('',#112243,#81328,#81329);
#73019=AXIS2_PLACEMENT_3D('',#112251,#81330,#81331);
#73020=AXIS2_PLACEMENT_3D('',#112268,#81332,#81333);
#73021=AXIS2_PLACEMENT_3D('',#112276,#81334,#81335);
#73022=AXIS2_PLACEMENT_3D('',#112293,#81336,#81337);
#73023=AXIS2_PLACEMENT_3D('',#112301,#81338,#81339);
#73024=AXIS2_PLACEMENT_3D('',#112318,#81340,#81341);
#73025=AXIS2_PLACEMENT_3D('',#112326,#81342,#81343);
#73026=AXIS2_PLACEMENT_3D('',#112343,#81344,#81345);
#73027=AXIS2_PLACEMENT_3D('',#112356,#81346,#81347);
#73028=AXIS2_PLACEMENT_3D('',#112376,#81349,#81350);
#73029=AXIS2_PLACEMENT_3D('',#112384,#81352,#81353);
#73030=AXIS2_PLACEMENT_3D('',#112397,#81354,#81355);
#73031=AXIS2_PLACEMENT_3D('',#112398,#81356,#81357);
#73032=AXIS2_PLACEMENT_3D('',#112422,#81359,#81360);
#73033=AXIS2_PLACEMENT_3D('',#112430,#81362,#81363);
#73034=AXIS2_PLACEMENT_3D('',#112443,#81364,#81365);
#73035=AXIS2_PLACEMENT_3D('',#112444,#81366,#81367);
#73036=AXIS2_PLACEMENT_3D('',#112468,#81369,#81370);
#73037=AXIS2_PLACEMENT_3D('',#112476,#81372,#81373);
#73038=AXIS2_PLACEMENT_3D('',#112489,#81374,#81375);
#73039=AXIS2_PLACEMENT_3D('',#112490,#81376,#81377);
#73040=AXIS2_PLACEMENT_3D('',#112514,#81379,#81380);
#73041=AXIS2_PLACEMENT_3D('',#112522,#81382,#81383);
#73042=AXIS2_PLACEMENT_3D('',#112535,#81384,#81385);
#73043=AXIS2_PLACEMENT_3D('',#112536,#81386,#81387);
#73044=AXIS2_PLACEMENT_3D('',#112560,#81389,#81390);
#73045=AXIS2_PLACEMENT_3D('',#112568,#81392,#81393);
#73046=AXIS2_PLACEMENT_3D('',#112581,#81394,#81395);
#73047=AXIS2_PLACEMENT_3D('',#112582,#81396,#81397);
#73048=AXIS2_PLACEMENT_3D('',#112606,#81399,#81400);
#73049=AXIS2_PLACEMENT_3D('',#112614,#81402,#81403);
#73050=AXIS2_PLACEMENT_3D('',#112627,#81404,#81405);
#73051=AXIS2_PLACEMENT_3D('',#112628,#81406,#81407);
#73052=AXIS2_PLACEMENT_3D('',#112680,#81411,#81412);
#73053=AXIS2_PLACEMENT_3D('',#112688,#81414,#81415);
#73054=AXIS2_PLACEMENT_3D('',#112701,#81416,#81417);
#73055=AXIS2_PLACEMENT_3D('',#112702,#81418,#81419);
#73056=AXIS2_PLACEMENT_3D('',#112726,#81421,#81422);
#73057=AXIS2_PLACEMENT_3D('',#112734,#81424,#81425);
#73058=AXIS2_PLACEMENT_3D('',#112747,#81426,#81427);
#73059=AXIS2_PLACEMENT_3D('',#112748,#81428,#81429);
#73060=AXIS2_PLACEMENT_3D('',#112772,#81431,#81432);
#73061=AXIS2_PLACEMENT_3D('',#112780,#81434,#81435);
#73062=AXIS2_PLACEMENT_3D('',#112793,#81436,#81437);
#73063=AXIS2_PLACEMENT_3D('',#112794,#81438,#81439);
#73064=AXIS2_PLACEMENT_3D('',#112818,#81441,#81442);
#73065=AXIS2_PLACEMENT_3D('',#112826,#81444,#81445);
#73066=AXIS2_PLACEMENT_3D('',#112839,#81446,#81447);
#73067=AXIS2_PLACEMENT_3D('',#112840,#81448,#81449);
#73068=AXIS2_PLACEMENT_3D('',#112864,#81451,#81452);
#73069=AXIS2_PLACEMENT_3D('',#112872,#81454,#81455);
#73070=AXIS2_PLACEMENT_3D('',#112885,#81456,#81457);
#73071=AXIS2_PLACEMENT_3D('',#112886,#81458,#81459);
#73072=AXIS2_PLACEMENT_3D('',#112910,#81461,#81462);
#73073=AXIS2_PLACEMENT_3D('',#112918,#81464,#81465);
#73074=AXIS2_PLACEMENT_3D('',#112931,#81466,#81467);
#73075=AXIS2_PLACEMENT_3D('',#112932,#81468,#81469);
#73076=AXIS2_PLACEMENT_3D('',#112956,#81471,#81472);
#73077=AXIS2_PLACEMENT_3D('',#112964,#81474,#81475);
#73078=AXIS2_PLACEMENT_3D('',#112977,#81476,#81477);
#73079=AXIS2_PLACEMENT_3D('',#112978,#81478,#81479);
#73080=AXIS2_PLACEMENT_3D('',#113002,#81481,#81482);
#73081=AXIS2_PLACEMENT_3D('',#113010,#81484,#81485);
#73082=AXIS2_PLACEMENT_3D('',#113023,#81486,#81487);
#73083=AXIS2_PLACEMENT_3D('',#113024,#81488,#81489);
#73084=AXIS2_PLACEMENT_3D('',#113048,#81491,#81492);
#73085=AXIS2_PLACEMENT_3D('',#113056,#81494,#81495);
#73086=AXIS2_PLACEMENT_3D('',#113069,#81496,#81497);
#73087=AXIS2_PLACEMENT_3D('',#113070,#81498,#81499);
#73088=AXIS2_PLACEMENT_3D('',#113094,#81501,#81502);
#73089=AXIS2_PLACEMENT_3D('',#113102,#81504,#81505);
#73090=AXIS2_PLACEMENT_3D('',#113115,#81506,#81507);
#73091=AXIS2_PLACEMENT_3D('',#113116,#81508,#81509);
#73092=AXIS2_PLACEMENT_3D('',#113140,#81511,#81512);
#73093=AXIS2_PLACEMENT_3D('',#113148,#81514,#81515);
#73094=AXIS2_PLACEMENT_3D('',#113161,#81516,#81517);
#73095=AXIS2_PLACEMENT_3D('',#113162,#81518,#81519);
#73096=AXIS2_PLACEMENT_3D('',#113186,#81521,#81522);
#73097=AXIS2_PLACEMENT_3D('',#113194,#81524,#81525);
#73098=AXIS2_PLACEMENT_3D('',#113207,#81526,#81527);
#73099=AXIS2_PLACEMENT_3D('',#113208,#81528,#81529);
#73100=AXIS2_PLACEMENT_3D('',#113232,#81531,#81532);
#73101=AXIS2_PLACEMENT_3D('',#113240,#81534,#81535);
#73102=AXIS2_PLACEMENT_3D('',#113253,#81536,#81537);
#73103=AXIS2_PLACEMENT_3D('',#113254,#81538,#81539);
#73104=AXIS2_PLACEMENT_3D('',#113278,#81541,#81542);
#73105=AXIS2_PLACEMENT_3D('',#113286,#81544,#81545);
#73106=AXIS2_PLACEMENT_3D('',#113299,#81546,#81547);
#73107=AXIS2_PLACEMENT_3D('',#113300,#81548,#81549);
#73108=AXIS2_PLACEMENT_3D('',#113324,#81551,#81552);
#73109=AXIS2_PLACEMENT_3D('',#113332,#81554,#81555);
#73110=AXIS2_PLACEMENT_3D('',#113345,#81556,#81557);
#73111=AXIS2_PLACEMENT_3D('',#113346,#81558,#81559);
#73112=AXIS2_PLACEMENT_3D('',#113370,#81561,#81562);
#73113=AXIS2_PLACEMENT_3D('',#113389,#81564,#81565);
#73114=AXIS2_PLACEMENT_3D('',#113391,#81567,#81568);
#73115=AXIS2_PLACEMENT_3D('',#113403,#81569,#81570);
#73116=AXIS2_PLACEMENT_3D('',#113417,#81572,#81573);
#73117=AXIS2_PLACEMENT_3D('',#113424,#81574,#81575);
#73118=AXIS2_PLACEMENT_3D('',#113426,#81576,#81577);
#73119=AXIS2_PLACEMENT_3D('',#113438,#81578,#81579);
#73120=AXIS2_PLACEMENT_3D('',#113462,#81581,#81582);
#73121=AXIS2_PLACEMENT_3D('',#113470,#81584,#81585);
#73122=AXIS2_PLACEMENT_3D('',#113483,#81586,#81587);
#73123=AXIS2_PLACEMENT_3D('',#113484,#81588,#81589);
#73124=AXIS2_PLACEMENT_3D('',#113508,#81591,#81592);
#73125=AXIS2_PLACEMENT_3D('',#113516,#81594,#81595);
#73126=AXIS2_PLACEMENT_3D('',#113529,#81596,#81597);
#73127=AXIS2_PLACEMENT_3D('',#113530,#81598,#81599);
#73128=AXIS2_PLACEMENT_3D('',#113554,#81601,#81602);
#73129=AXIS2_PLACEMENT_3D('',#113562,#81604,#81605);
#73130=AXIS2_PLACEMENT_3D('',#113575,#81606,#81607);
#73131=AXIS2_PLACEMENT_3D('',#113576,#81608,#81609);
#73132=AXIS2_PLACEMENT_3D('',#113600,#81611,#81612);
#73133=AXIS2_PLACEMENT_3D('',#113608,#81614,#81615);
#73134=AXIS2_PLACEMENT_3D('',#113621,#81616,#81617);
#73135=AXIS2_PLACEMENT_3D('',#113622,#81618,#81619);
#73136=AXIS2_PLACEMENT_3D('',#113634,#81621,#81622);
#73137=AXIS2_PLACEMENT_3D('',#113647,#81623,#81624);
#73138=AXIS2_PLACEMENT_3D('',#113648,#81625,#81626);
#73139=AXIS2_PLACEMENT_3D('',#113672,#81628,#81629);
#73140=AXIS2_PLACEMENT_3D('',#113689,#81632,#81633);
#73141=AXIS2_PLACEMENT_3D('',#113707,#81634,#81635);
#73142=AXIS2_PLACEMENT_3D('',#113709,#81637,#81638);
#73143=AXIS2_PLACEMENT_3D('',#113711,#81639,#81640);
#73144=AXIS2_PLACEMENT_3D('',#113712,#81641,#81642);
#73145=AXIS2_PLACEMENT_3D('',#113722,#81644,#81645);
#73146=AXIS2_PLACEMENT_3D('',#113740,#81646,#81647);
#73147=AXIS2_PLACEMENT_3D('',#113742,#81649,#81650);
#73148=AXIS2_PLACEMENT_3D('',#113744,#81651,#81652);
#73149=AXIS2_PLACEMENT_3D('',#113745,#81653,#81654);
#73150=AXIS2_PLACEMENT_3D('',#113755,#81656,#81657);
#73151=AXIS2_PLACEMENT_3D('',#113773,#81658,#81659);
#73152=AXIS2_PLACEMENT_3D('',#113775,#81661,#81662);
#73153=AXIS2_PLACEMENT_3D('',#113777,#81663,#81664);
#73154=AXIS2_PLACEMENT_3D('',#113778,#81665,#81666);
#73155=AXIS2_PLACEMENT_3D('',#113788,#81668,#81669);
#73156=AXIS2_PLACEMENT_3D('',#113806,#81670,#81671);
#73157=AXIS2_PLACEMENT_3D('',#113808,#81673,#81674);
#73158=AXIS2_PLACEMENT_3D('',#113810,#81675,#81676);
#73159=AXIS2_PLACEMENT_3D('',#113811,#81677,#81678);
#73160=AXIS2_PLACEMENT_3D('',#113821,#81680,#81681);
#73161=AXIS2_PLACEMENT_3D('',#113839,#81682,#81683);
#73162=AXIS2_PLACEMENT_3D('',#113841,#81685,#81686);
#73163=AXIS2_PLACEMENT_3D('',#113843,#81687,#81688);
#73164=AXIS2_PLACEMENT_3D('',#113844,#81689,#81690);
#73165=AXIS2_PLACEMENT_3D('',#113854,#81692,#81693);
#73166=AXIS2_PLACEMENT_3D('',#113872,#81694,#81695);
#73167=AXIS2_PLACEMENT_3D('',#113874,#81697,#81698);
#73168=AXIS2_PLACEMENT_3D('',#113876,#81699,#81700);
#73169=AXIS2_PLACEMENT_3D('',#113877,#81701,#81702);
#73170=AXIS2_PLACEMENT_3D('',#113887,#81704,#81705);
#73171=AXIS2_PLACEMENT_3D('',#113905,#81706,#81707);
#73172=AXIS2_PLACEMENT_3D('',#113907,#81709,#81710);
#73173=AXIS2_PLACEMENT_3D('',#113909,#81711,#81712);
#73174=AXIS2_PLACEMENT_3D('',#113910,#81713,#81714);
#73175=AXIS2_PLACEMENT_3D('',#113920,#81716,#81717);
#73176=AXIS2_PLACEMENT_3D('',#113938,#81718,#81719);
#73177=AXIS2_PLACEMENT_3D('',#113940,#81721,#81722);
#73178=AXIS2_PLACEMENT_3D('',#113942,#81723,#81724);
#73179=AXIS2_PLACEMENT_3D('',#113943,#81725,#81726);
#73180=AXIS2_PLACEMENT_3D('',#113953,#81728,#81729);
#73181=AXIS2_PLACEMENT_3D('',#113971,#81730,#81731);
#73182=AXIS2_PLACEMENT_3D('',#113973,#81733,#81734);
#73183=AXIS2_PLACEMENT_3D('',#113975,#81735,#81736);
#73184=AXIS2_PLACEMENT_3D('',#113976,#81737,#81738);
#73185=AXIS2_PLACEMENT_3D('',#113986,#81740,#81741);
#73186=AXIS2_PLACEMENT_3D('',#114004,#81742,#81743);
#73187=AXIS2_PLACEMENT_3D('',#114006,#81745,#81746);
#73188=AXIS2_PLACEMENT_3D('',#114008,#81747,#81748);
#73189=AXIS2_PLACEMENT_3D('',#114009,#81749,#81750);
#73190=AXIS2_PLACEMENT_3D('',#114019,#81752,#81753);
#73191=AXIS2_PLACEMENT_3D('',#114037,#81754,#81755);
#73192=AXIS2_PLACEMENT_3D('',#114039,#81757,#81758);
#73193=AXIS2_PLACEMENT_3D('',#114041,#81759,#81760);
#73194=AXIS2_PLACEMENT_3D('',#114042,#81761,#81762);
#73195=AXIS2_PLACEMENT_3D('',#114052,#81764,#81765);
#73196=AXIS2_PLACEMENT_3D('',#114070,#81766,#81767);
#73197=AXIS2_PLACEMENT_3D('',#114072,#81769,#81770);
#73198=AXIS2_PLACEMENT_3D('',#114074,#81771,#81772);
#73199=AXIS2_PLACEMENT_3D('',#114075,#81773,#81774);
#73200=AXIS2_PLACEMENT_3D('',#114085,#81776,#81777);
#73201=AXIS2_PLACEMENT_3D('',#114103,#81778,#81779);
#73202=AXIS2_PLACEMENT_3D('',#114105,#81781,#81782);
#73203=AXIS2_PLACEMENT_3D('',#114107,#81783,#81784);
#73204=AXIS2_PLACEMENT_3D('',#114108,#81785,#81786);
#73205=AXIS2_PLACEMENT_3D('',#114142,#81790,#81791);
#73206=AXIS2_PLACEMENT_3D('',#114160,#81792,#81793);
#73207=AXIS2_PLACEMENT_3D('',#114162,#81795,#81796);
#73208=AXIS2_PLACEMENT_3D('',#114164,#81797,#81798);
#73209=AXIS2_PLACEMENT_3D('',#114165,#81799,#81800);
#73210=AXIS2_PLACEMENT_3D('',#114175,#81802,#81803);
#73211=AXIS2_PLACEMENT_3D('',#114193,#81804,#81805);
#73212=AXIS2_PLACEMENT_3D('',#114195,#81807,#81808);
#73213=AXIS2_PLACEMENT_3D('',#114197,#81809,#81810);
#73214=AXIS2_PLACEMENT_3D('',#114198,#81811,#81812);
#73215=AXIS2_PLACEMENT_3D('',#114208,#81814,#81815);
#73216=AXIS2_PLACEMENT_3D('',#114226,#81816,#81817);
#73217=AXIS2_PLACEMENT_3D('',#114228,#81819,#81820);
#73218=AXIS2_PLACEMENT_3D('',#114230,#81821,#81822);
#73219=AXIS2_PLACEMENT_3D('',#114231,#81823,#81824);
#73220=AXIS2_PLACEMENT_3D('',#114241,#81826,#81827);
#73221=AXIS2_PLACEMENT_3D('',#114259,#81828,#81829);
#73222=AXIS2_PLACEMENT_3D('',#114261,#81831,#81832);
#73223=AXIS2_PLACEMENT_3D('',#114263,#81833,#81834);
#73224=AXIS2_PLACEMENT_3D('',#114264,#81835,#81836);
#73225=AXIS2_PLACEMENT_3D('',#114274,#81838,#81839);
#73226=AXIS2_PLACEMENT_3D('',#114292,#81840,#81841);
#73227=AXIS2_PLACEMENT_3D('',#114294,#81843,#81844);
#73228=AXIS2_PLACEMENT_3D('',#114296,#81845,#81846);
#73229=AXIS2_PLACEMENT_3D('',#114297,#81847,#81848);
#73230=AXIS2_PLACEMENT_3D('',#114307,#81850,#81851);
#73231=AXIS2_PLACEMENT_3D('',#114325,#81852,#81853);
#73232=AXIS2_PLACEMENT_3D('',#114327,#81855,#81856);
#73233=AXIS2_PLACEMENT_3D('',#114329,#81857,#81858);
#73234=AXIS2_PLACEMENT_3D('',#114330,#81859,#81860);
#73235=AXIS2_PLACEMENT_3D('',#114340,#81862,#81863);
#73236=AXIS2_PLACEMENT_3D('',#114358,#81864,#81865);
#73237=AXIS2_PLACEMENT_3D('',#114360,#81867,#81868);
#73238=AXIS2_PLACEMENT_3D('',#114362,#81869,#81870);
#73239=AXIS2_PLACEMENT_3D('',#114363,#81871,#81872);
#73240=AXIS2_PLACEMENT_3D('',#114373,#81874,#81875);
#73241=AXIS2_PLACEMENT_3D('',#114391,#81876,#81877);
#73242=AXIS2_PLACEMENT_3D('',#114393,#81879,#81880);
#73243=AXIS2_PLACEMENT_3D('',#114395,#81881,#81882);
#73244=AXIS2_PLACEMENT_3D('',#114396,#81883,#81884);
#73245=AXIS2_PLACEMENT_3D('',#114406,#81886,#81887);
#73246=AXIS2_PLACEMENT_3D('',#114424,#81888,#81889);
#73247=AXIS2_PLACEMENT_3D('',#114426,#81891,#81892);
#73248=AXIS2_PLACEMENT_3D('',#114428,#81893,#81894);
#73249=AXIS2_PLACEMENT_3D('',#114429,#81895,#81896);
#73250=AXIS2_PLACEMENT_3D('',#114439,#81898,#81899);
#73251=AXIS2_PLACEMENT_3D('',#114457,#81900,#81901);
#73252=AXIS2_PLACEMENT_3D('',#114459,#81903,#81904);
#73253=AXIS2_PLACEMENT_3D('',#114461,#81905,#81906);
#73254=AXIS2_PLACEMENT_3D('',#114462,#81907,#81908);
#73255=AXIS2_PLACEMENT_3D('',#114472,#81910,#81911);
#73256=AXIS2_PLACEMENT_3D('',#114490,#81912,#81913);
#73257=AXIS2_PLACEMENT_3D('',#114492,#81915,#81916);
#73258=AXIS2_PLACEMENT_3D('',#114494,#81917,#81918);
#73259=AXIS2_PLACEMENT_3D('',#114495,#81919,#81920);
#73260=AXIS2_PLACEMENT_3D('',#114505,#81922,#81923);
#73261=AXIS2_PLACEMENT_3D('',#114523,#81924,#81925);
#73262=AXIS2_PLACEMENT_3D('',#114525,#81927,#81928);
#73263=AXIS2_PLACEMENT_3D('',#114527,#81929,#81930);
#73264=AXIS2_PLACEMENT_3D('',#114528,#81931,#81932);
#73265=AXIS2_PLACEMENT_3D('',#114538,#81934,#81935);
#73266=AXIS2_PLACEMENT_3D('',#114556,#81936,#81937);
#73267=AXIS2_PLACEMENT_3D('',#114558,#81939,#81940);
#73268=AXIS2_PLACEMENT_3D('',#114560,#81941,#81942);
#73269=AXIS2_PLACEMENT_3D('',#114561,#81943,#81944);
#73270=AXIS2_PLACEMENT_3D('',#114571,#81946,#81947);
#73271=AXIS2_PLACEMENT_3D('',#114589,#81948,#81949);
#73272=AXIS2_PLACEMENT_3D('',#114591,#81951,#81952);
#73273=AXIS2_PLACEMENT_3D('',#114593,#81953,#81954);
#73274=AXIS2_PLACEMENT_3D('',#114594,#81955,#81956);
#73275=AXIS2_PLACEMENT_3D('',#114595,#81957,#81958);
#73276=AXIS2_PLACEMENT_3D('',#114598,#81959,#81960);
#73277=AXIS2_PLACEMENT_3D('',#114599,#81961,#81962);
#73278=AXIS2_PLACEMENT_3D('',#114600,#81963,#81964);
#73279=AXIS2_PLACEMENT_3D('',#114615,#81966,#81967);
#73280=AXIS2_PLACEMENT_3D('',#114652,#81968,#81969);
#73281=AXIS2_PLACEMENT_3D('',#114683,#81970,#81971);
#73282=AXIS2_PLACEMENT_3D('',#114714,#81972,#81973);
#73283=AXIS2_PLACEMENT_3D('',#114745,#81974,#81975);
#73284=AXIS2_PLACEMENT_3D('',#114776,#81976,#81977);
#73285=AXIS2_PLACEMENT_3D('',#114807,#81978,#81979);
#73286=AXIS2_PLACEMENT_3D('',#114838,#81980,#81981);
#73287=AXIS2_PLACEMENT_3D('',#114869,#81982,#81983);
#73288=AXIS2_PLACEMENT_3D('',#114900,#81984,#81985);
#73289=AXIS2_PLACEMENT_3D('',#114931,#81986,#81987);
#73290=AXIS2_PLACEMENT_3D('',#114962,#81988,#81989);
#73291=AXIS2_PLACEMENT_3D('',#114993,#81990,#81991);
#73292=AXIS2_PLACEMENT_3D('',#115024,#81992,#81993);
#73293=AXIS2_PLACEMENT_3D('',#115055,#81994,#81995);
#73294=AXIS2_PLACEMENT_3D('',#115086,#81996,#81997);
#73295=AXIS2_PLACEMENT_3D('',#115117,#81998,#81999);
#73296=AXIS2_PLACEMENT_3D('',#115148,#82000,#82001);
#73297=AXIS2_PLACEMENT_3D('',#115179,#82002,#82003);
#73298=AXIS2_PLACEMENT_3D('',#115210,#82004,#82005);
#73299=AXIS2_PLACEMENT_3D('',#115241,#82006,#82007);
#73300=AXIS2_PLACEMENT_3D('',#115272,#82008,#82009);
#73301=AXIS2_PLACEMENT_3D('',#115303,#82010,#82011);
#73302=AXIS2_PLACEMENT_3D('',#115334,#82012,#82013);
#73303=AXIS2_PLACEMENT_3D('',#115365,#82014,#82015);
#73304=AXIS2_PLACEMENT_3D('',#115396,#82016,#82017);
#73305=AXIS2_PLACEMENT_3D('',#115427,#82018,#82019);
#73306=AXIS2_PLACEMENT_3D('',#115458,#82020,#82021);
#73307=AXIS2_PLACEMENT_3D('',#115489,#82022,#82023);
#73308=AXIS2_PLACEMENT_3D('',#115524,#82024,#82025);
#73309=AXIS2_PLACEMENT_3D('',#115532,#82026,#82027);
#73310=AXIS2_PLACEMENT_3D('',#115549,#82028,#82029);
#73311=AXIS2_PLACEMENT_3D('',#115557,#82030,#82031);
#73312=AXIS2_PLACEMENT_3D('',#115574,#82032,#82033);
#73313=AXIS2_PLACEMENT_3D('',#115582,#82034,#82035);
#73314=AXIS2_PLACEMENT_3D('',#115599,#82036,#82037);
#73315=AXIS2_PLACEMENT_3D('',#115607,#82038,#82039);
#73316=AXIS2_PLACEMENT_3D('',#115624,#82040,#82041);
#73317=AXIS2_PLACEMENT_3D('',#115632,#82042,#82043);
#73318=AXIS2_PLACEMENT_3D('',#115649,#82044,#82045);
#73319=AXIS2_PLACEMENT_3D('',#115657,#82046,#82047);
#73320=AXIS2_PLACEMENT_3D('',#115674,#82048,#82049);
#73321=AXIS2_PLACEMENT_3D('',#115682,#82050,#82051);
#73322=AXIS2_PLACEMENT_3D('',#115699,#82052,#82053);
#73323=AXIS2_PLACEMENT_3D('',#115707,#82054,#82055);
#73324=AXIS2_PLACEMENT_3D('',#115724,#82056,#82057);
#73325=AXIS2_PLACEMENT_3D('',#115732,#82058,#82059);
#73326=AXIS2_PLACEMENT_3D('',#115749,#82060,#82061);
#73327=AXIS2_PLACEMENT_3D('',#115757,#82062,#82063);
#73328=AXIS2_PLACEMENT_3D('',#115774,#82064,#82065);
#73329=AXIS2_PLACEMENT_3D('',#115782,#82066,#82067);
#73330=AXIS2_PLACEMENT_3D('',#115799,#82068,#82069);
#73331=AXIS2_PLACEMENT_3D('',#115807,#82070,#82071);
#73332=AXIS2_PLACEMENT_3D('',#115824,#82072,#82073);
#73333=AXIS2_PLACEMENT_3D('',#115832,#82074,#82075);
#73334=AXIS2_PLACEMENT_3D('',#115849,#82076,#82077);
#73335=AXIS2_PLACEMENT_3D('',#115857,#82078,#82079);
#73336=AXIS2_PLACEMENT_3D('',#115874,#82080,#82081);
#73337=AXIS2_PLACEMENT_3D('',#115882,#82082,#82083);
#73338=AXIS2_PLACEMENT_3D('',#115899,#82084,#82085);
#73339=AXIS2_PLACEMENT_3D('',#115907,#82086,#82087);
#73340=AXIS2_PLACEMENT_3D('',#115924,#82088,#82089);
#73341=AXIS2_PLACEMENT_3D('',#115932,#82090,#82091);
#73342=AXIS2_PLACEMENT_3D('',#115949,#82092,#82093);
#73343=AXIS2_PLACEMENT_3D('',#115957,#82094,#82095);
#73344=AXIS2_PLACEMENT_3D('',#115974,#82096,#82097);
#73345=AXIS2_PLACEMENT_3D('',#115982,#82098,#82099);
#73346=AXIS2_PLACEMENT_3D('',#115999,#82100,#82101);
#73347=AXIS2_PLACEMENT_3D('',#116007,#82102,#82103);
#73348=AXIS2_PLACEMENT_3D('',#116024,#82104,#82105);
#73349=AXIS2_PLACEMENT_3D('',#116032,#82106,#82107);
#73350=AXIS2_PLACEMENT_3D('',#116049,#82108,#82109);
#73351=AXIS2_PLACEMENT_3D('',#116057,#82110,#82111);
#73352=AXIS2_PLACEMENT_3D('',#116074,#82112,#82113);
#73353=AXIS2_PLACEMENT_3D('',#116082,#82114,#82115);
#73354=AXIS2_PLACEMENT_3D('',#116099,#82116,#82117);
#73355=AXIS2_PLACEMENT_3D('',#116107,#82118,#82119);
#73356=AXIS2_PLACEMENT_3D('',#116124,#82120,#82121);
#73357=AXIS2_PLACEMENT_3D('',#116132,#82122,#82123);
#73358=AXIS2_PLACEMENT_3D('',#116149,#82124,#82125);
#73359=AXIS2_PLACEMENT_3D('',#116157,#82126,#82127);
#73360=AXIS2_PLACEMENT_3D('',#116174,#82128,#82129);
#73361=AXIS2_PLACEMENT_3D('',#116182,#82130,#82131);
#73362=AXIS2_PLACEMENT_3D('',#116199,#82132,#82133);
#73363=AXIS2_PLACEMENT_3D('',#116207,#82134,#82135);
#73364=AXIS2_PLACEMENT_3D('',#116224,#82136,#82137);
#73365=AXIS2_PLACEMENT_3D('',#116231,#82138,#82139);
#73366=AXIS2_PLACEMENT_3D('',#116244,#82140,#82141);
#73367=AXIS2_PLACEMENT_3D('',#116252,#82143,#82144);
#73368=AXIS2_PLACEMENT_3D('',#116254,#82145,#82146);
#73369=AXIS2_PLACEMENT_3D('',#116256,#82147,#82148);
#73370=AXIS2_PLACEMENT_3D('',#116291,#82150,#82151);
#73371=AXIS2_PLACEMENT_3D('',#116299,#82153,#82154);
#73372=AXIS2_PLACEMENT_3D('',#116301,#82155,#82156);
#73373=AXIS2_PLACEMENT_3D('',#116303,#82157,#82158);
#73374=AXIS2_PLACEMENT_3D('',#116338,#82160,#82161);
#73375=AXIS2_PLACEMENT_3D('',#116346,#82163,#82164);
#73376=AXIS2_PLACEMENT_3D('',#116348,#82165,#82166);
#73377=AXIS2_PLACEMENT_3D('',#116350,#82167,#82168);
#73378=AXIS2_PLACEMENT_3D('',#116385,#82170,#82171);
#73379=AXIS2_PLACEMENT_3D('',#116393,#82173,#82174);
#73380=AXIS2_PLACEMENT_3D('',#116395,#82175,#82176);
#73381=AXIS2_PLACEMENT_3D('',#116397,#82177,#82178);
#73382=AXIS2_PLACEMENT_3D('',#116432,#82180,#82181);
#73383=AXIS2_PLACEMENT_3D('',#116440,#82183,#82184);
#73384=AXIS2_PLACEMENT_3D('',#116442,#82185,#82186);
#73385=AXIS2_PLACEMENT_3D('',#116444,#82187,#82188);
#73386=AXIS2_PLACEMENT_3D('',#116479,#82190,#82191);
#73387=AXIS2_PLACEMENT_3D('',#116487,#82193,#82194);
#73388=AXIS2_PLACEMENT_3D('',#116489,#82195,#82196);
#73389=AXIS2_PLACEMENT_3D('',#116491,#82197,#82198);
#73390=AXIS2_PLACEMENT_3D('',#116526,#82200,#82201);
#73391=AXIS2_PLACEMENT_3D('',#116534,#82203,#82204);
#73392=AXIS2_PLACEMENT_3D('',#116536,#82205,#82206);
#73393=AXIS2_PLACEMENT_3D('',#116538,#82207,#82208);
#73394=AXIS2_PLACEMENT_3D('',#116573,#82210,#82211);
#73395=AXIS2_PLACEMENT_3D('',#116581,#82213,#82214);
#73396=AXIS2_PLACEMENT_3D('',#116583,#82215,#82216);
#73397=AXIS2_PLACEMENT_3D('',#116585,#82217,#82218);
#73398=AXIS2_PLACEMENT_3D('',#116620,#82220,#82221);
#73399=AXIS2_PLACEMENT_3D('',#116628,#82223,#82224);
#73400=AXIS2_PLACEMENT_3D('',#116630,#82225,#82226);
#73401=AXIS2_PLACEMENT_3D('',#116632,#82227,#82228);
#73402=AXIS2_PLACEMENT_3D('',#116667,#82230,#82231);
#73403=AXIS2_PLACEMENT_3D('',#116675,#82233,#82234);
#73404=AXIS2_PLACEMENT_3D('',#116677,#82235,#82236);
#73405=AXIS2_PLACEMENT_3D('',#116679,#82237,#82238);
#73406=AXIS2_PLACEMENT_3D('',#116714,#82240,#82241);
#73407=AXIS2_PLACEMENT_3D('',#116722,#82243,#82244);
#73408=AXIS2_PLACEMENT_3D('',#116724,#82245,#82246);
#73409=AXIS2_PLACEMENT_3D('',#116726,#82247,#82248);
#73410=AXIS2_PLACEMENT_3D('',#116761,#82250,#82251);
#73411=AXIS2_PLACEMENT_3D('',#116769,#82253,#82254);
#73412=AXIS2_PLACEMENT_3D('',#116771,#82255,#82256);
#73413=AXIS2_PLACEMENT_3D('',#116773,#82257,#82258);
#73414=AXIS2_PLACEMENT_3D('',#116808,#82260,#82261);
#73415=AXIS2_PLACEMENT_3D('',#116816,#82263,#82264);
#73416=AXIS2_PLACEMENT_3D('',#116818,#82265,#82266);
#73417=AXIS2_PLACEMENT_3D('',#116820,#82267,#82268);
#73418=AXIS2_PLACEMENT_3D('',#116855,#82270,#82271);
#73419=AXIS2_PLACEMENT_3D('',#116863,#82273,#82274);
#73420=AXIS2_PLACEMENT_3D('',#116865,#82275,#82276);
#73421=AXIS2_PLACEMENT_3D('',#116867,#82277,#82278);
#73422=AXIS2_PLACEMENT_3D('',#116934,#82282,#82283);
#73423=AXIS2_PLACEMENT_3D('',#116942,#82285,#82286);
#73424=AXIS2_PLACEMENT_3D('',#116944,#82287,#82288);
#73425=AXIS2_PLACEMENT_3D('',#116946,#82289,#82290);
#73426=AXIS2_PLACEMENT_3D('',#116981,#82292,#82293);
#73427=AXIS2_PLACEMENT_3D('',#116989,#82295,#82296);
#73428=AXIS2_PLACEMENT_3D('',#116991,#82297,#82298);
#73429=AXIS2_PLACEMENT_3D('',#116993,#82299,#82300);
#73430=AXIS2_PLACEMENT_3D('',#117028,#82302,#82303);
#73431=AXIS2_PLACEMENT_3D('',#117036,#82305,#82306);
#73432=AXIS2_PLACEMENT_3D('',#117038,#82307,#82308);
#73433=AXIS2_PLACEMENT_3D('',#117040,#82309,#82310);
#73434=AXIS2_PLACEMENT_3D('',#117075,#82312,#82313);
#73435=AXIS2_PLACEMENT_3D('',#117083,#82315,#82316);
#73436=AXIS2_PLACEMENT_3D('',#117085,#82317,#82318);
#73437=AXIS2_PLACEMENT_3D('',#117087,#82319,#82320);
#73438=AXIS2_PLACEMENT_3D('',#117122,#82322,#82323);
#73439=AXIS2_PLACEMENT_3D('',#117130,#82325,#82326);
#73440=AXIS2_PLACEMENT_3D('',#117132,#82327,#82328);
#73441=AXIS2_PLACEMENT_3D('',#117134,#82329,#82330);
#73442=AXIS2_PLACEMENT_3D('',#117169,#82332,#82333);
#73443=AXIS2_PLACEMENT_3D('',#117177,#82335,#82336);
#73444=AXIS2_PLACEMENT_3D('',#117179,#82337,#82338);
#73445=AXIS2_PLACEMENT_3D('',#117181,#82339,#82340);
#73446=AXIS2_PLACEMENT_3D('',#117216,#82342,#82343);
#73447=AXIS2_PLACEMENT_3D('',#117224,#82345,#82346);
#73448=AXIS2_PLACEMENT_3D('',#117226,#82347,#82348);
#73449=AXIS2_PLACEMENT_3D('',#117228,#82349,#82350);
#73450=AXIS2_PLACEMENT_3D('',#117263,#82352,#82353);
#73451=AXIS2_PLACEMENT_3D('',#117294,#82356,#82357);
#73452=AXIS2_PLACEMENT_3D('',#117296,#82358,#82359);
#73453=AXIS2_PLACEMENT_3D('',#117297,#82360,#82361);
#73454=AXIS2_PLACEMENT_3D('',#117311,#82363,#82364);
#73455=AXIS2_PLACEMENT_3D('',#117318,#82365,#82366);
#73456=AXIS2_PLACEMENT_3D('',#117328,#82367,#82368);
#73457=AXIS2_PLACEMENT_3D('',#117329,#82369,#82370);
#73458=AXIS2_PLACEMENT_3D('',#117357,#82372,#82373);
#73459=AXIS2_PLACEMENT_3D('',#117365,#82375,#82376);
#73460=AXIS2_PLACEMENT_3D('',#117367,#82377,#82378);
#73461=AXIS2_PLACEMENT_3D('',#117369,#82379,#82380);
#73462=AXIS2_PLACEMENT_3D('',#117404,#82382,#82383);
#73463=AXIS2_PLACEMENT_3D('',#117412,#82385,#82386);
#73464=AXIS2_PLACEMENT_3D('',#117414,#82387,#82388);
#73465=AXIS2_PLACEMENT_3D('',#117416,#82389,#82390);
#73466=AXIS2_PLACEMENT_3D('',#117451,#82392,#82393);
#73467=AXIS2_PLACEMENT_3D('',#117459,#82395,#82396);
#73468=AXIS2_PLACEMENT_3D('',#117461,#82397,#82398);
#73469=AXIS2_PLACEMENT_3D('',#117463,#82399,#82400);
#73470=AXIS2_PLACEMENT_3D('',#117498,#82402,#82403);
#73471=AXIS2_PLACEMENT_3D('',#117506,#82405,#82406);
#73472=AXIS2_PLACEMENT_3D('',#117508,#82407,#82408);
#73473=AXIS2_PLACEMENT_3D('',#117510,#82409,#82410);
#73474=AXIS2_PLACEMENT_3D('',#117545,#82412,#82413);
#73475=AXIS2_PLACEMENT_3D('',#117553,#82415,#82416);
#73476=AXIS2_PLACEMENT_3D('',#117555,#82417,#82418);
#73477=AXIS2_PLACEMENT_3D('',#117557,#82419,#82420);
#73478=AXIS2_PLACEMENT_3D('',#117593,#82423,#82424);
#73479=AXIS2_PLACEMENT_3D('',#117611,#82425,#82426);
#73480=AXIS2_PLACEMENT_3D('',#117613,#82428,#82429);
#73481=AXIS2_PLACEMENT_3D('',#117615,#82430,#82431);
#73482=AXIS2_PLACEMENT_3D('',#117616,#82432,#82433);
#73483=AXIS2_PLACEMENT_3D('',#117630,#82435,#82436);
#73484=AXIS2_PLACEMENT_3D('',#117648,#82437,#82438);
#73485=AXIS2_PLACEMENT_3D('',#117650,#82440,#82441);
#73486=AXIS2_PLACEMENT_3D('',#117652,#82442,#82443);
#73487=AXIS2_PLACEMENT_3D('',#117653,#82444,#82445);
#73488=AXIS2_PLACEMENT_3D('',#117667,#82447,#82448);
#73489=AXIS2_PLACEMENT_3D('',#117685,#82449,#82450);
#73490=AXIS2_PLACEMENT_3D('',#117687,#82452,#82453);
#73491=AXIS2_PLACEMENT_3D('',#117689,#82454,#82455);
#73492=AXIS2_PLACEMENT_3D('',#117690,#82456,#82457);
#73493=AXIS2_PLACEMENT_3D('',#117704,#82459,#82460);
#73494=AXIS2_PLACEMENT_3D('',#117722,#82461,#82462);
#73495=AXIS2_PLACEMENT_3D('',#117724,#82464,#82465);
#73496=AXIS2_PLACEMENT_3D('',#117726,#82466,#82467);
#73497=AXIS2_PLACEMENT_3D('',#117727,#82468,#82469);
#73498=AXIS2_PLACEMENT_3D('',#117741,#82471,#82472);
#73499=AXIS2_PLACEMENT_3D('',#117759,#82473,#82474);
#73500=AXIS2_PLACEMENT_3D('',#117761,#82476,#82477);
#73501=AXIS2_PLACEMENT_3D('',#117763,#82478,#82479);
#73502=AXIS2_PLACEMENT_3D('',#117764,#82480,#82481);
#73503=AXIS2_PLACEMENT_3D('',#117778,#82483,#82484);
#73504=AXIS2_PLACEMENT_3D('',#117796,#82485,#82486);
#73505=AXIS2_PLACEMENT_3D('',#117798,#82488,#82489);
#73506=AXIS2_PLACEMENT_3D('',#117800,#82490,#82491);
#73507=AXIS2_PLACEMENT_3D('',#117801,#82492,#82493);
#73508=AXIS2_PLACEMENT_3D('',#117815,#82495,#82496);
#73509=AXIS2_PLACEMENT_3D('',#117833,#82497,#82498);
#73510=AXIS2_PLACEMENT_3D('',#117835,#82500,#82501);
#73511=AXIS2_PLACEMENT_3D('',#117837,#82502,#82503);
#73512=AXIS2_PLACEMENT_3D('',#117838,#82504,#82505);
#73513=AXIS2_PLACEMENT_3D('',#117852,#82507,#82508);
#73514=AXIS2_PLACEMENT_3D('',#117870,#82509,#82510);
#73515=AXIS2_PLACEMENT_3D('',#117872,#82512,#82513);
#73516=AXIS2_PLACEMENT_3D('',#117874,#82514,#82515);
#73517=AXIS2_PLACEMENT_3D('',#117875,#82516,#82517);
#73518=AXIS2_PLACEMENT_3D('',#117889,#82519,#82520);
#73519=AXIS2_PLACEMENT_3D('',#117907,#82521,#82522);
#73520=AXIS2_PLACEMENT_3D('',#117909,#82524,#82525);
#73521=AXIS2_PLACEMENT_3D('',#117911,#82526,#82527);
#73522=AXIS2_PLACEMENT_3D('',#117912,#82528,#82529);
#73523=AXIS2_PLACEMENT_3D('',#117926,#82531,#82532);
#73524=AXIS2_PLACEMENT_3D('',#117944,#82533,#82534);
#73525=AXIS2_PLACEMENT_3D('',#117946,#82536,#82537);
#73526=AXIS2_PLACEMENT_3D('',#117948,#82538,#82539);
#73527=AXIS2_PLACEMENT_3D('',#117949,#82540,#82541);
#73528=AXIS2_PLACEMENT_3D('',#117963,#82543,#82544);
#73529=AXIS2_PLACEMENT_3D('',#117981,#82545,#82546);
#73530=AXIS2_PLACEMENT_3D('',#117983,#82548,#82549);
#73531=AXIS2_PLACEMENT_3D('',#117985,#82550,#82551);
#73532=AXIS2_PLACEMENT_3D('',#117986,#82552,#82553);
#73533=AXIS2_PLACEMENT_3D('',#118000,#82555,#82556);
#73534=AXIS2_PLACEMENT_3D('',#118018,#82557,#82558);
#73535=AXIS2_PLACEMENT_3D('',#118020,#82560,#82561);
#73536=AXIS2_PLACEMENT_3D('',#118022,#82562,#82563);
#73537=AXIS2_PLACEMENT_3D('',#118023,#82564,#82565);
#73538=AXIS2_PLACEMENT_3D('',#118037,#82567,#82568);
#73539=AXIS2_PLACEMENT_3D('',#118055,#82569,#82570);
#73540=AXIS2_PLACEMENT_3D('',#118057,#82572,#82573);
#73541=AXIS2_PLACEMENT_3D('',#118059,#82574,#82575);
#73542=AXIS2_PLACEMENT_3D('',#118060,#82576,#82577);
#73543=AXIS2_PLACEMENT_3D('',#118074,#82579,#82580);
#73544=AXIS2_PLACEMENT_3D('',#118092,#82581,#82582);
#73545=AXIS2_PLACEMENT_3D('',#118094,#82584,#82585);
#73546=AXIS2_PLACEMENT_3D('',#118096,#82586,#82587);
#73547=AXIS2_PLACEMENT_3D('',#118097,#82588,#82589);
#73548=AXIS2_PLACEMENT_3D('',#118111,#82591,#82592);
#73549=AXIS2_PLACEMENT_3D('',#118129,#82593,#82594);
#73550=AXIS2_PLACEMENT_3D('',#118131,#82596,#82597);
#73551=AXIS2_PLACEMENT_3D('',#118133,#82598,#82599);
#73552=AXIS2_PLACEMENT_3D('',#118134,#82600,#82601);
#73553=AXIS2_PLACEMENT_3D('',#118148,#82603,#82604);
#73554=AXIS2_PLACEMENT_3D('',#118166,#82605,#82606);
#73555=AXIS2_PLACEMENT_3D('',#118168,#82608,#82609);
#73556=AXIS2_PLACEMENT_3D('',#118170,#82610,#82611);
#73557=AXIS2_PLACEMENT_3D('',#118171,#82612,#82613);
#73558=AXIS2_PLACEMENT_3D('',#118185,#82615,#82616);
#73559=AXIS2_PLACEMENT_3D('',#118203,#82617,#82618);
#73560=AXIS2_PLACEMENT_3D('',#118205,#82620,#82621);
#73561=AXIS2_PLACEMENT_3D('',#118207,#82622,#82623);
#73562=AXIS2_PLACEMENT_3D('',#118208,#82624,#82625);
#73563=AXIS2_PLACEMENT_3D('',#118222,#82627,#82628);
#73564=AXIS2_PLACEMENT_3D('',#118240,#82629,#82630);
#73565=AXIS2_PLACEMENT_3D('',#118242,#82632,#82633);
#73566=AXIS2_PLACEMENT_3D('',#118244,#82634,#82635);
#73567=AXIS2_PLACEMENT_3D('',#118245,#82636,#82637);
#73568=AXIS2_PLACEMENT_3D('',#118259,#82639,#82640);
#73569=AXIS2_PLACEMENT_3D('',#118277,#82641,#82642);
#73570=AXIS2_PLACEMENT_3D('',#118279,#82644,#82645);
#73571=AXIS2_PLACEMENT_3D('',#118281,#82646,#82647);
#73572=AXIS2_PLACEMENT_3D('',#118282,#82648,#82649);
#73573=AXIS2_PLACEMENT_3D('',#118296,#82651,#82652);
#73574=AXIS2_PLACEMENT_3D('',#118314,#82653,#82654);
#73575=AXIS2_PLACEMENT_3D('',#118316,#82656,#82657);
#73576=AXIS2_PLACEMENT_3D('',#118318,#82658,#82659);
#73577=AXIS2_PLACEMENT_3D('',#118319,#82660,#82661);
#73578=AXIS2_PLACEMENT_3D('',#118333,#82663,#82664);
#73579=AXIS2_PLACEMENT_3D('',#118351,#82665,#82666);
#73580=AXIS2_PLACEMENT_3D('',#118353,#82668,#82669);
#73581=AXIS2_PLACEMENT_3D('',#118355,#82670,#82671);
#73582=AXIS2_PLACEMENT_3D('',#118356,#82672,#82673);
#73583=AXIS2_PLACEMENT_3D('',#118398,#82677,#82678);
#73584=AXIS2_PLACEMENT_3D('',#118416,#82679,#82680);
#73585=AXIS2_PLACEMENT_3D('',#118418,#82682,#82683);
#73586=AXIS2_PLACEMENT_3D('',#118420,#82684,#82685);
#73587=AXIS2_PLACEMENT_3D('',#118421,#82686,#82687);
#73588=AXIS2_PLACEMENT_3D('',#118435,#82689,#82690);
#73589=AXIS2_PLACEMENT_3D('',#118453,#82691,#82692);
#73590=AXIS2_PLACEMENT_3D('',#118455,#82694,#82695);
#73591=AXIS2_PLACEMENT_3D('',#118457,#82696,#82697);
#73592=AXIS2_PLACEMENT_3D('',#118458,#82698,#82699);
#73593=AXIS2_PLACEMENT_3D('',#118472,#82701,#82702);
#73594=AXIS2_PLACEMENT_3D('',#118490,#82703,#82704);
#73595=AXIS2_PLACEMENT_3D('',#118492,#82706,#82707);
#73596=AXIS2_PLACEMENT_3D('',#118494,#82708,#82709);
#73597=AXIS2_PLACEMENT_3D('',#118495,#82710,#82711);
#73598=AXIS2_PLACEMENT_3D('',#118509,#82713,#82714);
#73599=AXIS2_PLACEMENT_3D('',#118527,#82715,#82716);
#73600=AXIS2_PLACEMENT_3D('',#118529,#82718,#82719);
#73601=AXIS2_PLACEMENT_3D('',#118531,#82720,#82721);
#73602=AXIS2_PLACEMENT_3D('',#118532,#82722,#82723);
#73603=AXIS2_PLACEMENT_3D('',#118546,#82725,#82726);
#73604=AXIS2_PLACEMENT_3D('',#118564,#82727,#82728);
#73605=AXIS2_PLACEMENT_3D('',#118566,#82730,#82731);
#73606=AXIS2_PLACEMENT_3D('',#118568,#82732,#82733);
#73607=AXIS2_PLACEMENT_3D('',#118569,#82734,#82735);
#73608=AXIS2_PLACEMENT_3D('',#118583,#82737,#82738);
#73609=AXIS2_PLACEMENT_3D('',#118601,#82739,#82740);
#73610=AXIS2_PLACEMENT_3D('',#118603,#82742,#82743);
#73611=AXIS2_PLACEMENT_3D('',#118605,#82744,#82745);
#73612=AXIS2_PLACEMENT_3D('',#118606,#82746,#82747);
#73613=AXIS2_PLACEMENT_3D('',#118620,#82749,#82750);
#73614=AXIS2_PLACEMENT_3D('',#118638,#82751,#82752);
#73615=AXIS2_PLACEMENT_3D('',#118640,#82754,#82755);
#73616=AXIS2_PLACEMENT_3D('',#118642,#82756,#82757);
#73617=AXIS2_PLACEMENT_3D('',#118643,#82758,#82759);
#73618=AXIS2_PLACEMENT_3D('',#118651,#82760,#82761);
#73619=AXIS2_PLACEMENT_3D('',#118685,#82762,#82763);
#73620=AXIS2_PLACEMENT_3D('',#118719,#82764,#82765);
#73621=AXIS2_PLACEMENT_3D('',#118753,#82766,#82767);
#73622=AXIS2_PLACEMENT_3D('',#118787,#82768,#82769);
#73623=AXIS2_PLACEMENT_3D('',#118821,#82770,#82771);
#73624=AXIS2_PLACEMENT_3D('',#118855,#82772,#82773);
#73625=AXIS2_PLACEMENT_3D('',#118889,#82774,#82775);
#73626=AXIS2_PLACEMENT_3D('',#118923,#82776,#82777);
#73627=AXIS2_PLACEMENT_3D('',#118957,#82778,#82779);
#73628=AXIS2_PLACEMENT_3D('',#118991,#82780,#82781);
#73629=AXIS2_PLACEMENT_3D('',#119025,#82782,#82783);
#73630=AXIS2_PLACEMENT_3D('',#119059,#82784,#82785);
#73631=AXIS2_PLACEMENT_3D('',#119093,#82786,#82787);
#73632=AXIS2_PLACEMENT_3D('',#119127,#82788,#82789);
#73633=AXIS2_PLACEMENT_3D('',#119161,#82790,#82791);
#73634=AXIS2_PLACEMENT_3D('',#119195,#82792,#82793);
#73635=AXIS2_PLACEMENT_3D('',#119229,#82794,#82795);
#73636=AXIS2_PLACEMENT_3D('',#119263,#82796,#82797);
#73637=AXIS2_PLACEMENT_3D('',#119297,#82798,#82799);
#73638=AXIS2_PLACEMENT_3D('',#119331,#82800,#82801);
#73639=AXIS2_PLACEMENT_3D('',#119365,#82802,#82803);
#73640=AXIS2_PLACEMENT_3D('',#119399,#82804,#82805);
#73641=AXIS2_PLACEMENT_3D('',#119433,#82806,#82807);
#73642=AXIS2_PLACEMENT_3D('',#119467,#82808,#82809);
#73643=AXIS2_PLACEMENT_3D('',#119501,#82810,#82811);
#73644=AXIS2_PLACEMENT_3D('',#119535,#82812,#82813);
#73645=AXIS2_PLACEMENT_3D('',#119569,#82814,#82815);
#73646=AXIS2_PLACEMENT_3D('',#119603,#82816,#82817);
#73647=AXIS2_PLACEMENT_3D('',#119637,#82818,#82819);
#73648=AXIS2_PLACEMENT_3D('',#119675,#82820,#82821);
#73649=AXIS2_PLACEMENT_3D('',#119713,#82822,#82823);
#73650=AXIS2_PLACEMENT_3D('',#119751,#82824,#82825);
#73651=AXIS2_PLACEMENT_3D('',#119789,#82826,#82827);
#73652=AXIS2_PLACEMENT_3D('',#119827,#82828,#82829);
#73653=AXIS2_PLACEMENT_3D('',#119865,#82830,#82831);
#73654=AXIS2_PLACEMENT_3D('',#119903,#82832,#82833);
#73655=AXIS2_PLACEMENT_3D('',#119941,#82834,#82835);
#73656=AXIS2_PLACEMENT_3D('',#119979,#82836,#82837);
#73657=AXIS2_PLACEMENT_3D('',#120017,#82838,#82839);
#73658=AXIS2_PLACEMENT_3D('',#120055,#82840,#82841);
#73659=AXIS2_PLACEMENT_3D('',#120093,#82842,#82843);
#73660=AXIS2_PLACEMENT_3D('',#120131,#82844,#82845);
#73661=AXIS2_PLACEMENT_3D('',#120169,#82846,#82847);
#73662=AXIS2_PLACEMENT_3D('',#120207,#82848,#82849);
#73663=AXIS2_PLACEMENT_3D('',#120245,#82850,#82851);
#73664=AXIS2_PLACEMENT_3D('',#120283,#82852,#82853);
#73665=AXIS2_PLACEMENT_3D('',#120321,#82854,#82855);
#73666=AXIS2_PLACEMENT_3D('',#120359,#82856,#82857);
#73667=AXIS2_PLACEMENT_3D('',#120397,#82858,#82859);
#73668=AXIS2_PLACEMENT_3D('',#120435,#82860,#82861);
#73669=AXIS2_PLACEMENT_3D('',#120473,#82862,#82863);
#73670=AXIS2_PLACEMENT_3D('',#120511,#82864,#82865);
#73671=AXIS2_PLACEMENT_3D('',#120549,#82866,#82867);
#73672=AXIS2_PLACEMENT_3D('',#120587,#82868,#82869);
#73673=AXIS2_PLACEMENT_3D('',#120625,#82870,#82871);
#73674=AXIS2_PLACEMENT_3D('',#120663,#82872,#82873);
#73675=AXIS2_PLACEMENT_3D('',#120701,#82874,#82875);
#73676=AXIS2_PLACEMENT_3D('',#120740,#82876,#82877);
#73677=AXIS2_PLACEMENT_3D('',#120778,#82880,#82881);
#73678=AXIS2_PLACEMENT_3D('',#120780,#82882,#82883);
#73679=AXIS2_PLACEMENT_3D('',#120782,#82884,#82885);
#73680=AXIS2_PLACEMENT_3D('',#120783,#82886,#82887);
#73681=AXIS2_PLACEMENT_3D('',#120821,#82890,#82891);
#73682=AXIS2_PLACEMENT_3D('',#120823,#82892,#82893);
#73683=AXIS2_PLACEMENT_3D('',#120825,#82894,#82895);
#73684=AXIS2_PLACEMENT_3D('',#120826,#82896,#82897);
#73685=AXIS2_PLACEMENT_3D('',#120864,#82900,#82901);
#73686=AXIS2_PLACEMENT_3D('',#120866,#82902,#82903);
#73687=AXIS2_PLACEMENT_3D('',#120868,#82904,#82905);
#73688=AXIS2_PLACEMENT_3D('',#120869,#82906,#82907);
#73689=AXIS2_PLACEMENT_3D('',#120907,#82910,#82911);
#73690=AXIS2_PLACEMENT_3D('',#120909,#82912,#82913);
#73691=AXIS2_PLACEMENT_3D('',#120911,#82914,#82915);
#73692=AXIS2_PLACEMENT_3D('',#120912,#82916,#82917);
#73693=AXIS2_PLACEMENT_3D('',#120950,#82920,#82921);
#73694=AXIS2_PLACEMENT_3D('',#120952,#82922,#82923);
#73695=AXIS2_PLACEMENT_3D('',#120954,#82924,#82925);
#73696=AXIS2_PLACEMENT_3D('',#120955,#82926,#82927);
#73697=AXIS2_PLACEMENT_3D('',#120993,#82930,#82931);
#73698=AXIS2_PLACEMENT_3D('',#120995,#82932,#82933);
#73699=AXIS2_PLACEMENT_3D('',#120997,#82934,#82935);
#73700=AXIS2_PLACEMENT_3D('',#120998,#82936,#82937);
#73701=AXIS2_PLACEMENT_3D('',#121064,#82942,#82943);
#73702=AXIS2_PLACEMENT_3D('',#121066,#82944,#82945);
#73703=AXIS2_PLACEMENT_3D('',#121068,#82946,#82947);
#73704=AXIS2_PLACEMENT_3D('',#121069,#82948,#82949);
#73705=AXIS2_PLACEMENT_3D('',#121107,#82952,#82953);
#73706=AXIS2_PLACEMENT_3D('',#121109,#82954,#82955);
#73707=AXIS2_PLACEMENT_3D('',#121111,#82956,#82957);
#73708=AXIS2_PLACEMENT_3D('',#121112,#82958,#82959);
#73709=AXIS2_PLACEMENT_3D('',#121150,#82962,#82963);
#73710=AXIS2_PLACEMENT_3D('',#121152,#82964,#82965);
#73711=AXIS2_PLACEMENT_3D('',#121154,#82966,#82967);
#73712=AXIS2_PLACEMENT_3D('',#121155,#82968,#82969);
#73713=AXIS2_PLACEMENT_3D('',#121193,#82972,#82973);
#73714=AXIS2_PLACEMENT_3D('',#121195,#82974,#82975);
#73715=AXIS2_PLACEMENT_3D('',#121197,#82976,#82977);
#73716=AXIS2_PLACEMENT_3D('',#121198,#82978,#82979);
#73717=AXIS2_PLACEMENT_3D('',#121236,#82982,#82983);
#73718=AXIS2_PLACEMENT_3D('',#121238,#82984,#82985);
#73719=AXIS2_PLACEMENT_3D('',#121240,#82986,#82987);
#73720=AXIS2_PLACEMENT_3D('',#121241,#82988,#82989);
#73721=AXIS2_PLACEMENT_3D('',#121279,#82992,#82993);
#73722=AXIS2_PLACEMENT_3D('',#121281,#82994,#82995);
#73723=AXIS2_PLACEMENT_3D('',#121283,#82996,#82997);
#73724=AXIS2_PLACEMENT_3D('',#121284,#82998,#82999);
#73725=AXIS2_PLACEMENT_3D('',#121322,#83002,#83003);
#73726=AXIS2_PLACEMENT_3D('',#121324,#83004,#83005);
#73727=AXIS2_PLACEMENT_3D('',#121326,#83006,#83007);
#73728=AXIS2_PLACEMENT_3D('',#121327,#83008,#83009);
#73729=AXIS2_PLACEMENT_3D('',#121365,#83012,#83013);
#73730=AXIS2_PLACEMENT_3D('',#121367,#83014,#83015);
#73731=AXIS2_PLACEMENT_3D('',#121369,#83016,#83017);
#73732=AXIS2_PLACEMENT_3D('',#121370,#83018,#83019);
#73733=AXIS2_PLACEMENT_3D('',#121408,#83022,#83023);
#73734=AXIS2_PLACEMENT_3D('',#121410,#83024,#83025);
#73735=AXIS2_PLACEMENT_3D('',#121412,#83026,#83027);
#73736=AXIS2_PLACEMENT_3D('',#121413,#83028,#83029);
#73737=AXIS2_PLACEMENT_3D('',#121451,#83032,#83033);
#73738=AXIS2_PLACEMENT_3D('',#121453,#83034,#83035);
#73739=AXIS2_PLACEMENT_3D('',#121455,#83036,#83037);
#73740=AXIS2_PLACEMENT_3D('',#121456,#83038,#83039);
#73741=AXIS2_PLACEMENT_3D('',#121494,#83042,#83043);
#73742=AXIS2_PLACEMENT_3D('',#121496,#83044,#83045);
#73743=AXIS2_PLACEMENT_3D('',#121498,#83046,#83047);
#73744=AXIS2_PLACEMENT_3D('',#121499,#83048,#83049);
#73745=AXIS2_PLACEMENT_3D('',#121537,#83052,#83053);
#73746=AXIS2_PLACEMENT_3D('',#121539,#83054,#83055);
#73747=AXIS2_PLACEMENT_3D('',#121541,#83056,#83057);
#73748=AXIS2_PLACEMENT_3D('',#121542,#83058,#83059);
#73749=AXIS2_PLACEMENT_3D('',#121580,#83062,#83063);
#73750=AXIS2_PLACEMENT_3D('',#121582,#83064,#83065);
#73751=AXIS2_PLACEMENT_3D('',#121584,#83066,#83067);
#73752=AXIS2_PLACEMENT_3D('',#121585,#83068,#83069);
#73753=AXIS2_PLACEMENT_3D('',#121623,#83072,#83073);
#73754=AXIS2_PLACEMENT_3D('',#121625,#83074,#83075);
#73755=AXIS2_PLACEMENT_3D('',#121627,#83076,#83077);
#73756=AXIS2_PLACEMENT_3D('',#121628,#83078,#83079);
#73757=AXIS2_PLACEMENT_3D('',#121673,#83082,#83083);
#73758=AXIS2_PLACEMENT_3D('',#121675,#83085,#83086);
#73759=AXIS2_PLACEMENT_3D('',#121677,#83087,#83088);
#73760=AXIS2_PLACEMENT_3D('',#121678,#83089,#83090);
#73761=AXIS2_PLACEMENT_3D('',#121709,#83092,#83093);
#73762=AXIS2_PLACEMENT_3D('',#121711,#83094,#83095);
#73763=AXIS2_PLACEMENT_3D('',#121713,#83096,#83097);
#73764=AXIS2_PLACEMENT_3D('',#121714,#83098,#83099);
#73765=AXIS2_PLACEMENT_3D('',#121752,#83102,#83103);
#73766=AXIS2_PLACEMENT_3D('',#121754,#83104,#83105);
#73767=AXIS2_PLACEMENT_3D('',#121756,#83106,#83107);
#73768=AXIS2_PLACEMENT_3D('',#121757,#83108,#83109);
#73769=AXIS2_PLACEMENT_3D('',#121795,#83112,#83113);
#73770=AXIS2_PLACEMENT_3D('',#121797,#83114,#83115);
#73771=AXIS2_PLACEMENT_3D('',#121799,#83116,#83117);
#73772=AXIS2_PLACEMENT_3D('',#121800,#83118,#83119);
#73773=AXIS2_PLACEMENT_3D('',#121838,#83122,#83123);
#73774=AXIS2_PLACEMENT_3D('',#121840,#83124,#83125);
#73775=AXIS2_PLACEMENT_3D('',#121842,#83126,#83127);
#73776=AXIS2_PLACEMENT_3D('',#121843,#83128,#83129);
#73777=AXIS2_PLACEMENT_3D('',#121881,#83132,#83133);
#73778=AXIS2_PLACEMENT_3D('',#121883,#83134,#83135);
#73779=AXIS2_PLACEMENT_3D('',#121885,#83136,#83137);
#73780=AXIS2_PLACEMENT_3D('',#121886,#83138,#83139);
#73781=AXIS2_PLACEMENT_3D('',#121924,#83142,#83143);
#73782=AXIS2_PLACEMENT_3D('',#121926,#83144,#83145);
#73783=AXIS2_PLACEMENT_3D('',#121928,#83146,#83147);
#73784=AXIS2_PLACEMENT_3D('',#121929,#83148,#83149);
#73785=AXIS2_PLACEMENT_3D('',#121937,#83151,#83152);
#73786=AXIS2_PLACEMENT_3D('',#121940,#83153,#83154);
#73787=AXIS2_PLACEMENT_3D('',#121941,#83155,#83156);
#73788=AXIS2_PLACEMENT_3D('',#121978,#83158,#83159);
#73789=AXIS2_PLACEMENT_3D('',#122013,#83162,#83163);
#73790=AXIS2_PLACEMENT_3D('',#122015,#83165,#83166);
#73791=AXIS2_PLACEMENT_3D('',#122017,#83167,#83168);
#73792=AXIS2_PLACEMENT_3D('',#122018,#83169,#83170);
#73793=AXIS2_PLACEMENT_3D('',#122052,#83172,#83173);
#73794=AXIS2_PLACEMENT_3D('',#122054,#83175,#83176);
#73795=AXIS2_PLACEMENT_3D('',#122056,#83177,#83178);
#73796=AXIS2_PLACEMENT_3D('',#122057,#83179,#83180);
#73797=AXIS2_PLACEMENT_3D('',#122091,#83182,#83183);
#73798=AXIS2_PLACEMENT_3D('',#122093,#83185,#83186);
#73799=AXIS2_PLACEMENT_3D('',#122095,#83187,#83188);
#73800=AXIS2_PLACEMENT_3D('',#122096,#83189,#83190);
#73801=AXIS2_PLACEMENT_3D('',#122130,#83192,#83193);
#73802=AXIS2_PLACEMENT_3D('',#122132,#83195,#83196);
#73803=AXIS2_PLACEMENT_3D('',#122134,#83197,#83198);
#73804=AXIS2_PLACEMENT_3D('',#122135,#83199,#83200);
#73805=AXIS2_PLACEMENT_3D('',#122169,#83202,#83203);
#73806=AXIS2_PLACEMENT_3D('',#122171,#83205,#83206);
#73807=AXIS2_PLACEMENT_3D('',#122173,#83207,#83208);
#73808=AXIS2_PLACEMENT_3D('',#122174,#83209,#83210);
#73809=AXIS2_PLACEMENT_3D('',#122208,#83212,#83213);
#73810=AXIS2_PLACEMENT_3D('',#122210,#83215,#83216);
#73811=AXIS2_PLACEMENT_3D('',#122212,#83217,#83218);
#73812=AXIS2_PLACEMENT_3D('',#122213,#83219,#83220);
#73813=AXIS2_PLACEMENT_3D('',#122247,#83222,#83223);
#73814=AXIS2_PLACEMENT_3D('',#122249,#83225,#83226);
#73815=AXIS2_PLACEMENT_3D('',#122251,#83227,#83228);
#73816=AXIS2_PLACEMENT_3D('',#122252,#83229,#83230);
#73817=AXIS2_PLACEMENT_3D('',#122286,#83232,#83233);
#73818=AXIS2_PLACEMENT_3D('',#122288,#83235,#83236);
#73819=AXIS2_PLACEMENT_3D('',#122290,#83237,#83238);
#73820=AXIS2_PLACEMENT_3D('',#122291,#83239,#83240);
#73821=AXIS2_PLACEMENT_3D('',#122325,#83242,#83243);
#73822=AXIS2_PLACEMENT_3D('',#122327,#83245,#83246);
#73823=AXIS2_PLACEMENT_3D('',#122329,#83247,#83248);
#73824=AXIS2_PLACEMENT_3D('',#122330,#83249,#83250);
#73825=AXIS2_PLACEMENT_3D('',#122364,#83252,#83253);
#73826=AXIS2_PLACEMENT_3D('',#122366,#83255,#83256);
#73827=AXIS2_PLACEMENT_3D('',#122368,#83257,#83258);
#73828=AXIS2_PLACEMENT_3D('',#122369,#83259,#83260);
#73829=AXIS2_PLACEMENT_3D('',#122403,#83262,#83263);
#73830=AXIS2_PLACEMENT_3D('',#122405,#83265,#83266);
#73831=AXIS2_PLACEMENT_3D('',#122407,#83267,#83268);
#73832=AXIS2_PLACEMENT_3D('',#122408,#83269,#83270);
#73833=AXIS2_PLACEMENT_3D('',#122442,#83272,#83273);
#73834=AXIS2_PLACEMENT_3D('',#122444,#83275,#83276);
#73835=AXIS2_PLACEMENT_3D('',#122446,#83277,#83278);
#73836=AXIS2_PLACEMENT_3D('',#122447,#83279,#83280);
#73837=AXIS2_PLACEMENT_3D('',#122481,#83282,#83283);
#73838=AXIS2_PLACEMENT_3D('',#122483,#83285,#83286);
#73839=AXIS2_PLACEMENT_3D('',#122485,#83287,#83288);
#73840=AXIS2_PLACEMENT_3D('',#122486,#83289,#83290);
#73841=AXIS2_PLACEMENT_3D('',#122544,#83294,#83295);
#73842=AXIS2_PLACEMENT_3D('',#122546,#83297,#83298);
#73843=AXIS2_PLACEMENT_3D('',#122548,#83299,#83300);
#73844=AXIS2_PLACEMENT_3D('',#122549,#83301,#83302);
#73845=AXIS2_PLACEMENT_3D('',#122583,#83304,#83305);
#73846=AXIS2_PLACEMENT_3D('',#122585,#83307,#83308);
#73847=AXIS2_PLACEMENT_3D('',#122587,#83309,#83310);
#73848=AXIS2_PLACEMENT_3D('',#122588,#83311,#83312);
#73849=AXIS2_PLACEMENT_3D('',#122622,#83314,#83315);
#73850=AXIS2_PLACEMENT_3D('',#122624,#83317,#83318);
#73851=AXIS2_PLACEMENT_3D('',#122626,#83319,#83320);
#73852=AXIS2_PLACEMENT_3D('',#122627,#83321,#83322);
#73853=AXIS2_PLACEMENT_3D('',#122661,#83324,#83325);
#73854=AXIS2_PLACEMENT_3D('',#122663,#83327,#83328);
#73855=AXIS2_PLACEMENT_3D('',#122665,#83329,#83330);
#73856=AXIS2_PLACEMENT_3D('',#122666,#83331,#83332);
#73857=AXIS2_PLACEMENT_3D('',#122700,#83334,#83335);
#73858=AXIS2_PLACEMENT_3D('',#122702,#83337,#83338);
#73859=AXIS2_PLACEMENT_3D('',#122704,#83339,#83340);
#73860=AXIS2_PLACEMENT_3D('',#122705,#83341,#83342);
#73861=AXIS2_PLACEMENT_3D('',#122739,#83344,#83345);
#73862=AXIS2_PLACEMENT_3D('',#122741,#83347,#83348);
#73863=AXIS2_PLACEMENT_3D('',#122743,#83349,#83350);
#73864=AXIS2_PLACEMENT_3D('',#122744,#83351,#83352);
#73865=AXIS2_PLACEMENT_3D('',#122778,#83354,#83355);
#73866=AXIS2_PLACEMENT_3D('',#122780,#83357,#83358);
#73867=AXIS2_PLACEMENT_3D('',#122782,#83359,#83360);
#73868=AXIS2_PLACEMENT_3D('',#122783,#83361,#83362);
#73869=AXIS2_PLACEMENT_3D('',#122817,#83364,#83365);
#73870=AXIS2_PLACEMENT_3D('',#122819,#83367,#83368);
#73871=AXIS2_PLACEMENT_3D('',#122821,#83369,#83370);
#73872=AXIS2_PLACEMENT_3D('',#122822,#83371,#83372);
#73873=AXIS2_PLACEMENT_3D('',#122856,#83374,#83375);
#73874=AXIS2_PLACEMENT_3D('',#122858,#83377,#83378);
#73875=AXIS2_PLACEMENT_3D('',#122860,#83379,#83380);
#73876=AXIS2_PLACEMENT_3D('',#122861,#83381,#83382);
#73877=AXIS2_PLACEMENT_3D('',#122895,#83384,#83385);
#73878=AXIS2_PLACEMENT_3D('',#122897,#83387,#83388);
#73879=AXIS2_PLACEMENT_3D('',#122899,#83389,#83390);
#73880=AXIS2_PLACEMENT_3D('',#122900,#83391,#83392);
#73881=AXIS2_PLACEMENT_3D('',#122934,#83394,#83395);
#73882=AXIS2_PLACEMENT_3D('',#122936,#83397,#83398);
#73883=AXIS2_PLACEMENT_3D('',#122938,#83399,#83400);
#73884=AXIS2_PLACEMENT_3D('',#122939,#83401,#83402);
#73885=AXIS2_PLACEMENT_3D('',#122973,#83404,#83405);
#73886=AXIS2_PLACEMENT_3D('',#122975,#83407,#83408);
#73887=AXIS2_PLACEMENT_3D('',#122977,#83409,#83410);
#73888=AXIS2_PLACEMENT_3D('',#122978,#83411,#83412);
#73889=AXIS2_PLACEMENT_3D('',#123012,#83414,#83415);
#73890=AXIS2_PLACEMENT_3D('',#123014,#83417,#83418);
#73891=AXIS2_PLACEMENT_3D('',#123016,#83419,#83420);
#73892=AXIS2_PLACEMENT_3D('',#123017,#83421,#83422);
#73893=AXIS2_PLACEMENT_3D('',#123051,#83424,#83425);
#73894=AXIS2_PLACEMENT_3D('',#123053,#83427,#83428);
#73895=AXIS2_PLACEMENT_3D('',#123055,#83429,#83430);
#73896=AXIS2_PLACEMENT_3D('',#123056,#83431,#83432);
#73897=AXIS2_PLACEMENT_3D('',#123057,#83433,#83434);
#73898=AXIS2_PLACEMENT_3D('',#123067,#83435,#83436);
#73899=AXIS2_PLACEMENT_3D('',#123068,#83437,#83438);
#73900=AXIS2_PLACEMENT_3D('',#123087,#83440,#83441);
#73901=AXIS2_PLACEMENT_3D('',#123105,#83442,#83443);
#73902=AXIS2_PLACEMENT_3D('',#123118,#83444,#83445);
#73903=AXIS2_PLACEMENT_3D('',#123130,#83446,#83447);
#73904=AXIS2_PLACEMENT_3D('',#123143,#83448,#83449);
#73905=AXIS2_PLACEMENT_3D('',#123155,#83450,#83451);
#73906=AXIS2_PLACEMENT_3D('',#123168,#83452,#83453);
#73907=AXIS2_PLACEMENT_3D('',#123180,#83454,#83455);
#73908=AXIS2_PLACEMENT_3D('',#123193,#83456,#83457);
#73909=AXIS2_PLACEMENT_3D('',#123205,#83458,#83459);
#73910=AXIS2_PLACEMENT_3D('',#123218,#83460,#83461);
#73911=AXIS2_PLACEMENT_3D('',#123230,#83462,#83463);
#73912=AXIS2_PLACEMENT_3D('',#123243,#83464,#83465);
#73913=AXIS2_PLACEMENT_3D('',#123255,#83466,#83467);
#73914=AXIS2_PLACEMENT_3D('',#123268,#83468,#83469);
#73915=AXIS2_PLACEMENT_3D('',#123280,#83470,#83471);
#73916=AXIS2_PLACEMENT_3D('',#123293,#83472,#83473);
#73917=AXIS2_PLACEMENT_3D('',#123305,#83474,#83475);
#73918=AXIS2_PLACEMENT_3D('',#123318,#83476,#83477);
#73919=AXIS2_PLACEMENT_3D('',#123330,#83478,#83479);
#73920=AXIS2_PLACEMENT_3D('',#123343,#83480,#83481);
#73921=AXIS2_PLACEMENT_3D('',#123355,#83482,#83483);
#73922=AXIS2_PLACEMENT_3D('',#123368,#83484,#83485);
#73923=AXIS2_PLACEMENT_3D('',#123380,#83486,#83487);
#73924=AXIS2_PLACEMENT_3D('',#123393,#83488,#83489);
#73925=AXIS2_PLACEMENT_3D('',#123405,#83490,#83491);
#73926=AXIS2_PLACEMENT_3D('',#123418,#83492,#83493);
#73927=AXIS2_PLACEMENT_3D('',#123430,#83494,#83495);
#73928=AXIS2_PLACEMENT_3D('',#123443,#83496,#83497);
#73929=AXIS2_PLACEMENT_3D('',#123455,#83498,#83499);
#73930=AXIS2_PLACEMENT_3D('',#123468,#83500,#83501);
#73931=AXIS2_PLACEMENT_3D('',#123480,#83502,#83503);
#73932=AXIS2_PLACEMENT_3D('',#123493,#83504,#83505);
#73933=AXIS2_PLACEMENT_3D('',#123505,#83506,#83507);
#73934=AXIS2_PLACEMENT_3D('',#123518,#83508,#83509);
#73935=AXIS2_PLACEMENT_3D('',#123530,#83510,#83511);
#73936=AXIS2_PLACEMENT_3D('',#123543,#83512,#83513);
#73937=AXIS2_PLACEMENT_3D('',#123555,#83514,#83515);
#73938=AXIS2_PLACEMENT_3D('',#123568,#83516,#83517);
#73939=AXIS2_PLACEMENT_3D('',#123580,#83518,#83519);
#73940=AXIS2_PLACEMENT_3D('',#123593,#83520,#83521);
#73941=AXIS2_PLACEMENT_3D('',#123605,#83522,#83523);
#73942=AXIS2_PLACEMENT_3D('',#123618,#83524,#83525);
#73943=AXIS2_PLACEMENT_3D('',#123630,#83526,#83527);
#73944=AXIS2_PLACEMENT_3D('',#123643,#83528,#83529);
#73945=AXIS2_PLACEMENT_3D('',#123655,#83530,#83531);
#73946=AXIS2_PLACEMENT_3D('',#123668,#83532,#83533);
#73947=AXIS2_PLACEMENT_3D('',#123680,#83534,#83535);
#73948=AXIS2_PLACEMENT_3D('',#123693,#83536,#83537);
#73949=AXIS2_PLACEMENT_3D('',#123705,#83538,#83539);
#73950=AXIS2_PLACEMENT_3D('',#123718,#83540,#83541);
#73951=AXIS2_PLACEMENT_3D('',#123730,#83542,#83543);
#73952=AXIS2_PLACEMENT_3D('',#123743,#83544,#83545);
#73953=AXIS2_PLACEMENT_3D('',#123755,#83546,#83547);
#73954=AXIS2_PLACEMENT_3D('',#123768,#83548,#83549);
#73955=AXIS2_PLACEMENT_3D('',#123780,#83550,#83551);
#73956=AXIS2_PLACEMENT_3D('',#123793,#83552,#83553);
#73957=AXIS2_PLACEMENT_3D('',#123804,#83554,#83555);
#73958=AXIS2_PLACEMENT_3D('',#123826,#83556,#83557);
#73959=AXIS2_PLACEMENT_3D('',#123872,#83558,#83559);
#73960=AXIS2_PLACEMENT_3D('',#123913,#83560,#83561);
#73961=AXIS2_PLACEMENT_3D('',#123954,#83562,#83563);
#73962=AXIS2_PLACEMENT_3D('',#124000,#83564,#83565);
#73963=AXIS2_PLACEMENT_3D('',#124046,#83566,#83567);
#73964=AXIS2_PLACEMENT_3D('',#124087,#83568,#83569);
#73965=AXIS2_PLACEMENT_3D('',#124128,#83570,#83571);
#73966=AXIS2_PLACEMENT_3D('',#124169,#83572,#83573);
#73967=AXIS2_PLACEMENT_3D('',#124210,#83574,#83575);
#73968=AXIS2_PLACEMENT_3D('',#124256,#83576,#83577);
#73969=AXIS2_PLACEMENT_3D('',#124297,#83578,#83579);
#73970=AXIS2_PLACEMENT_3D('',#124338,#83580,#83581);
#73971=AXIS2_PLACEMENT_3D('',#124379,#83582,#83583);
#73972=AXIS2_PLACEMENT_3D('',#124429,#83584,#83585);
#73973=AXIS2_PLACEMENT_3D('',#124479,#83586,#83587);
#73974=AXIS2_PLACEMENT_3D('',#124529,#83588,#83589);
#73975=AXIS2_PLACEMENT_3D('',#124570,#83590,#83591);
#73976=AXIS2_PLACEMENT_3D('',#124611,#83592,#83593);
#73977=AXIS2_PLACEMENT_3D('',#124657,#83594,#83595);
#73978=AXIS2_PLACEMENT_3D('',#124698,#83596,#83597);
#73979=AXIS2_PLACEMENT_3D('',#124739,#83598,#83599);
#73980=AXIS2_PLACEMENT_3D('',#124785,#83600,#83601);
#73981=AXIS2_PLACEMENT_3D('',#124835,#83602,#83603);
#73982=AXIS2_PLACEMENT_3D('',#124876,#83604,#83605);
#73983=AXIS2_PLACEMENT_3D('',#124917,#83606,#83607);
#73984=AXIS2_PLACEMENT_3D('',#124958,#83608,#83609);
#73985=AXIS2_PLACEMENT_3D('',#125004,#83610,#83611);
#73986=AXIS2_PLACEMENT_3D('',#125050,#83612,#83613);
#73987=AXIS2_PLACEMENT_3D('',#125091,#83614,#83615);
#73988=AXIS2_PLACEMENT_3D('',#125099,#83617,#83618);
#73989=AXIS2_PLACEMENT_3D('',#125101,#83619,#83620);
#73990=AXIS2_PLACEMENT_3D('',#125103,#83621,#83622);
#73991=AXIS2_PLACEMENT_3D('',#125104,#83623,#83624);
#73992=AXIS2_PLACEMENT_3D('',#125124,#83626,#83627);
#73993=AXIS2_PLACEMENT_3D('',#125132,#83629,#83630);
#73994=AXIS2_PLACEMENT_3D('',#125134,#83631,#83632);
#73995=AXIS2_PLACEMENT_3D('',#125136,#83633,#83634);
#73996=AXIS2_PLACEMENT_3D('',#125137,#83635,#83636);
#73997=AXIS2_PLACEMENT_3D('',#125157,#83638,#83639);
#73998=AXIS2_PLACEMENT_3D('',#125165,#83641,#83642);
#73999=AXIS2_PLACEMENT_3D('',#125167,#83643,#83644);
#74000=AXIS2_PLACEMENT_3D('',#125169,#83645,#83646);
#74001=AXIS2_PLACEMENT_3D('',#125170,#83647,#83648);
#74002=AXIS2_PLACEMENT_3D('',#125190,#83650,#83651);
#74003=AXIS2_PLACEMENT_3D('',#125198,#83653,#83654);
#74004=AXIS2_PLACEMENT_3D('',#125200,#83655,#83656);
#74005=AXIS2_PLACEMENT_3D('',#125202,#83657,#83658);
#74006=AXIS2_PLACEMENT_3D('',#125203,#83659,#83660);
#74007=AXIS2_PLACEMENT_3D('',#125223,#83662,#83663);
#74008=AXIS2_PLACEMENT_3D('',#125231,#83665,#83666);
#74009=AXIS2_PLACEMENT_3D('',#125233,#83667,#83668);
#74010=AXIS2_PLACEMENT_3D('',#125235,#83669,#83670);
#74011=AXIS2_PLACEMENT_3D('',#125236,#83671,#83672);
#74012=AXIS2_PLACEMENT_3D('',#125256,#83674,#83675);
#74013=AXIS2_PLACEMENT_3D('',#125264,#83677,#83678);
#74014=AXIS2_PLACEMENT_3D('',#125266,#83679,#83680);
#74015=AXIS2_PLACEMENT_3D('',#125268,#83681,#83682);
#74016=AXIS2_PLACEMENT_3D('',#125269,#83683,#83684);
#74017=AXIS2_PLACEMENT_3D('',#125289,#83686,#83687);
#74018=AXIS2_PLACEMENT_3D('',#125297,#83689,#83690);
#74019=AXIS2_PLACEMENT_3D('',#125299,#83691,#83692);
#74020=AXIS2_PLACEMENT_3D('',#125301,#83693,#83694);
#74021=AXIS2_PLACEMENT_3D('',#125302,#83695,#83696);
#74022=AXIS2_PLACEMENT_3D('',#125322,#83698,#83699);
#74023=AXIS2_PLACEMENT_3D('',#125330,#83701,#83702);
#74024=AXIS2_PLACEMENT_3D('',#125332,#83703,#83704);
#74025=AXIS2_PLACEMENT_3D('',#125334,#83705,#83706);
#74026=AXIS2_PLACEMENT_3D('',#125335,#83707,#83708);
#74027=AXIS2_PLACEMENT_3D('',#125355,#83710,#83711);
#74028=AXIS2_PLACEMENT_3D('',#125363,#83713,#83714);
#74029=AXIS2_PLACEMENT_3D('',#125365,#83715,#83716);
#74030=AXIS2_PLACEMENT_3D('',#125367,#83717,#83718);
#74031=AXIS2_PLACEMENT_3D('',#125368,#83719,#83720);
#74032=AXIS2_PLACEMENT_3D('',#125388,#83722,#83723);
#74033=AXIS2_PLACEMENT_3D('',#125396,#83725,#83726);
#74034=AXIS2_PLACEMENT_3D('',#125398,#83727,#83728);
#74035=AXIS2_PLACEMENT_3D('',#125400,#83729,#83730);
#74036=AXIS2_PLACEMENT_3D('',#125401,#83731,#83732);
#74037=AXIS2_PLACEMENT_3D('',#125421,#83734,#83735);
#74038=AXIS2_PLACEMENT_3D('',#125429,#83737,#83738);
#74039=AXIS2_PLACEMENT_3D('',#125431,#83739,#83740);
#74040=AXIS2_PLACEMENT_3D('',#125433,#83741,#83742);
#74041=AXIS2_PLACEMENT_3D('',#125434,#83743,#83744);
#74042=AXIS2_PLACEMENT_3D('',#125454,#83746,#83747);
#74043=AXIS2_PLACEMENT_3D('',#125462,#83749,#83750);
#74044=AXIS2_PLACEMENT_3D('',#125464,#83751,#83752);
#74045=AXIS2_PLACEMENT_3D('',#125466,#83753,#83754);
#74046=AXIS2_PLACEMENT_3D('',#125467,#83755,#83756);
#74047=AXIS2_PLACEMENT_3D('',#125487,#83758,#83759);
#74048=AXIS2_PLACEMENT_3D('',#125495,#83761,#83762);
#74049=AXIS2_PLACEMENT_3D('',#125497,#83763,#83764);
#74050=AXIS2_PLACEMENT_3D('',#125499,#83765,#83766);
#74051=AXIS2_PLACEMENT_3D('',#125500,#83767,#83768);
#74052=AXIS2_PLACEMENT_3D('',#125520,#83770,#83771);
#74053=AXIS2_PLACEMENT_3D('',#125528,#83773,#83774);
#74054=AXIS2_PLACEMENT_3D('',#125530,#83775,#83776);
#74055=AXIS2_PLACEMENT_3D('',#125532,#83777,#83778);
#74056=AXIS2_PLACEMENT_3D('',#125533,#83779,#83780);
#74057=AXIS2_PLACEMENT_3D('',#125577,#83784,#83785);
#74058=AXIS2_PLACEMENT_3D('',#125585,#83787,#83788);
#74059=AXIS2_PLACEMENT_3D('',#125587,#83789,#83790);
#74060=AXIS2_PLACEMENT_3D('',#125589,#83791,#83792);
#74061=AXIS2_PLACEMENT_3D('',#125590,#83793,#83794);
#74062=AXIS2_PLACEMENT_3D('',#125610,#83796,#83797);
#74063=AXIS2_PLACEMENT_3D('',#125618,#83799,#83800);
#74064=AXIS2_PLACEMENT_3D('',#125620,#83801,#83802);
#74065=AXIS2_PLACEMENT_3D('',#125622,#83803,#83804);
#74066=AXIS2_PLACEMENT_3D('',#125623,#83805,#83806);
#74067=AXIS2_PLACEMENT_3D('',#125643,#83808,#83809);
#74068=AXIS2_PLACEMENT_3D('',#125651,#83811,#83812);
#74069=AXIS2_PLACEMENT_3D('',#125653,#83813,#83814);
#74070=AXIS2_PLACEMENT_3D('',#125655,#83815,#83816);
#74071=AXIS2_PLACEMENT_3D('',#125656,#83817,#83818);
#74072=AXIS2_PLACEMENT_3D('',#125676,#83820,#83821);
#74073=AXIS2_PLACEMENT_3D('',#125684,#83823,#83824);
#74074=AXIS2_PLACEMENT_3D('',#125686,#83825,#83826);
#74075=AXIS2_PLACEMENT_3D('',#125688,#83827,#83828);
#74076=AXIS2_PLACEMENT_3D('',#125689,#83829,#83830);
#74077=AXIS2_PLACEMENT_3D('',#125709,#83832,#83833);
#74078=AXIS2_PLACEMENT_3D('',#125717,#83835,#83836);
#74079=AXIS2_PLACEMENT_3D('',#125719,#83837,#83838);
#74080=AXIS2_PLACEMENT_3D('',#125721,#83839,#83840);
#74081=AXIS2_PLACEMENT_3D('',#125722,#83841,#83842);
#74082=AXIS2_PLACEMENT_3D('',#125742,#83844,#83845);
#74083=AXIS2_PLACEMENT_3D('',#125750,#83847,#83848);
#74084=AXIS2_PLACEMENT_3D('',#125752,#83849,#83850);
#74085=AXIS2_PLACEMENT_3D('',#125754,#83851,#83852);
#74086=AXIS2_PLACEMENT_3D('',#125755,#83853,#83854);
#74087=AXIS2_PLACEMENT_3D('',#125775,#83856,#83857);
#74088=AXIS2_PLACEMENT_3D('',#125790,#83859,#83860);
#74089=AXIS2_PLACEMENT_3D('',#125792,#83862,#83863);
#74090=AXIS2_PLACEMENT_3D('',#125794,#83864,#83865);
#74091=AXIS2_PLACEMENT_3D('',#125795,#83866,#83867);
#74092=AXIS2_PLACEMENT_3D('',#125809,#83869,#83870);
#74093=AXIS2_PLACEMENT_3D('',#125816,#83871,#83872);
#74094=AXIS2_PLACEMENT_3D('',#125818,#83873,#83874);
#74095=AXIS2_PLACEMENT_3D('',#125820,#83875,#83876);
#74096=AXIS2_PLACEMENT_3D('',#125821,#83877,#83878);
#74097=AXIS2_PLACEMENT_3D('',#125841,#83880,#83881);
#74098=AXIS2_PLACEMENT_3D('',#125849,#83883,#83884);
#74099=AXIS2_PLACEMENT_3D('',#125851,#83885,#83886);
#74100=AXIS2_PLACEMENT_3D('',#125853,#83887,#83888);
#74101=AXIS2_PLACEMENT_3D('',#125854,#83889,#83890);
#74102=AXIS2_PLACEMENT_3D('',#125874,#83892,#83893);
#74103=AXIS2_PLACEMENT_3D('',#125882,#83895,#83896);
#74104=AXIS2_PLACEMENT_3D('',#125884,#83897,#83898);
#74105=AXIS2_PLACEMENT_3D('',#125886,#83899,#83900);
#74106=AXIS2_PLACEMENT_3D('',#125887,#83901,#83902);
#74107=AXIS2_PLACEMENT_3D('',#125907,#83904,#83905);
#74108=AXIS2_PLACEMENT_3D('',#125915,#83907,#83908);
#74109=AXIS2_PLACEMENT_3D('',#125917,#83909,#83910);
#74110=AXIS2_PLACEMENT_3D('',#125919,#83911,#83912);
#74111=AXIS2_PLACEMENT_3D('',#125920,#83913,#83914);
#74112=AXIS2_PLACEMENT_3D('',#125940,#83916,#83917);
#74113=AXIS2_PLACEMENT_3D('',#125948,#83919,#83920);
#74114=AXIS2_PLACEMENT_3D('',#125950,#83921,#83922);
#74115=AXIS2_PLACEMENT_3D('',#125952,#83923,#83924);
#74116=AXIS2_PLACEMENT_3D('',#125953,#83925,#83926);
#74117=AXIS2_PLACEMENT_3D('',#125973,#83928,#83929);
#74118=AXIS2_PLACEMENT_3D('',#125981,#83931,#83932);
#74119=AXIS2_PLACEMENT_3D('',#125983,#83933,#83934);
#74120=AXIS2_PLACEMENT_3D('',#125985,#83935,#83936);
#74121=AXIS2_PLACEMENT_3D('',#125986,#83937,#83938);
#74122=AXIS2_PLACEMENT_3D('',#126006,#83940,#83941);
#74123=AXIS2_PLACEMENT_3D('',#126014,#83943,#83944);
#74124=AXIS2_PLACEMENT_3D('',#126016,#83945,#83946);
#74125=AXIS2_PLACEMENT_3D('',#126018,#83947,#83948);
#74126=AXIS2_PLACEMENT_3D('',#126019,#83949,#83950);
#74127=AXIS2_PLACEMENT_3D('',#126040,#83953,#83954);
#74128=AXIS2_PLACEMENT_3D('',#126066,#83956,#83957);
#74129=AXIS2_PLACEMENT_3D('',#126068,#83958,#83959);
#74130=AXIS2_PLACEMENT_3D('',#126069,#83960,#83961);
#74131=AXIS2_PLACEMENT_3D('',#126083,#83963,#83964);
#74132=AXIS2_PLACEMENT_3D('',#126109,#83966,#83967);
#74133=AXIS2_PLACEMENT_3D('',#126111,#83968,#83969);
#74134=AXIS2_PLACEMENT_3D('',#126112,#83970,#83971);
#74135=AXIS2_PLACEMENT_3D('',#126126,#83973,#83974);
#74136=AXIS2_PLACEMENT_3D('',#126152,#83976,#83977);
#74137=AXIS2_PLACEMENT_3D('',#126154,#83978,#83979);
#74138=AXIS2_PLACEMENT_3D('',#126155,#83980,#83981);
#74139=AXIS2_PLACEMENT_3D('',#126169,#83983,#83984);
#74140=AXIS2_PLACEMENT_3D('',#126195,#83986,#83987);
#74141=AXIS2_PLACEMENT_3D('',#126197,#83988,#83989);
#74142=AXIS2_PLACEMENT_3D('',#126198,#83990,#83991);
#74143=AXIS2_PLACEMENT_3D('',#126212,#83993,#83994);
#74144=AXIS2_PLACEMENT_3D('',#126238,#83996,#83997);
#74145=AXIS2_PLACEMENT_3D('',#126240,#83998,#83999);
#74146=AXIS2_PLACEMENT_3D('',#126241,#84000,#84001);
#74147=AXIS2_PLACEMENT_3D('',#126255,#84003,#84004);
#74148=AXIS2_PLACEMENT_3D('',#126281,#84006,#84007);
#74149=AXIS2_PLACEMENT_3D('',#126283,#84008,#84009);
#74150=AXIS2_PLACEMENT_3D('',#126284,#84010,#84011);
#74151=AXIS2_PLACEMENT_3D('',#126298,#84013,#84014);
#74152=AXIS2_PLACEMENT_3D('',#126324,#84016,#84017);
#74153=AXIS2_PLACEMENT_3D('',#126326,#84018,#84019);
#74154=AXIS2_PLACEMENT_3D('',#126327,#84020,#84021);
#74155=AXIS2_PLACEMENT_3D('',#126341,#84023,#84024);
#74156=AXIS2_PLACEMENT_3D('',#126367,#84026,#84027);
#74157=AXIS2_PLACEMENT_3D('',#126369,#84028,#84029);
#74158=AXIS2_PLACEMENT_3D('',#126370,#84030,#84031);
#74159=AXIS2_PLACEMENT_3D('',#126384,#84033,#84034);
#74160=AXIS2_PLACEMENT_3D('',#126410,#84036,#84037);
#74161=AXIS2_PLACEMENT_3D('',#126412,#84038,#84039);
#74162=AXIS2_PLACEMENT_3D('',#126413,#84040,#84041);
#74163=AXIS2_PLACEMENT_3D('',#126427,#84043,#84044);
#74164=AXIS2_PLACEMENT_3D('',#126453,#84046,#84047);
#74165=AXIS2_PLACEMENT_3D('',#126455,#84048,#84049);
#74166=AXIS2_PLACEMENT_3D('',#126456,#84050,#84051);
#74167=AXIS2_PLACEMENT_3D('',#126470,#84053,#84054);
#74168=AXIS2_PLACEMENT_3D('',#126496,#84056,#84057);
#74169=AXIS2_PLACEMENT_3D('',#126498,#84058,#84059);
#74170=AXIS2_PLACEMENT_3D('',#126499,#84060,#84061);
#74171=AXIS2_PLACEMENT_3D('',#126513,#84063,#84064);
#74172=AXIS2_PLACEMENT_3D('',#126539,#84066,#84067);
#74173=AXIS2_PLACEMENT_3D('',#126541,#84068,#84069);
#74174=AXIS2_PLACEMENT_3D('',#126542,#84070,#84071);
#74175=AXIS2_PLACEMENT_3D('',#126556,#84073,#84074);
#74176=AXIS2_PLACEMENT_3D('',#126582,#84076,#84077);
#74177=AXIS2_PLACEMENT_3D('',#126584,#84078,#84079);
#74178=AXIS2_PLACEMENT_3D('',#126585,#84080,#84081);
#74179=AXIS2_PLACEMENT_3D('',#126599,#84083,#84084);
#74180=AXIS2_PLACEMENT_3D('',#126625,#84086,#84087);
#74181=AXIS2_PLACEMENT_3D('',#126627,#84088,#84089);
#74182=AXIS2_PLACEMENT_3D('',#126628,#84090,#84091);
#74183=AXIS2_PLACEMENT_3D('',#126642,#84093,#84094);
#74184=AXIS2_PLACEMENT_3D('',#126668,#84096,#84097);
#74185=AXIS2_PLACEMENT_3D('',#126670,#84098,#84099);
#74186=AXIS2_PLACEMENT_3D('',#126671,#84100,#84101);
#74187=AXIS2_PLACEMENT_3D('',#126685,#84103,#84104);
#74188=AXIS2_PLACEMENT_3D('',#126711,#84106,#84107);
#74189=AXIS2_PLACEMENT_3D('',#126713,#84108,#84109);
#74190=AXIS2_PLACEMENT_3D('',#126714,#84110,#84111);
#74191=AXIS2_PLACEMENT_3D('',#126728,#84113,#84114);
#74192=AXIS2_PLACEMENT_3D('',#126754,#84116,#84117);
#74193=AXIS2_PLACEMENT_3D('',#126756,#84118,#84119);
#74194=AXIS2_PLACEMENT_3D('',#126757,#84120,#84121);
#74195=AXIS2_PLACEMENT_3D('',#126771,#84123,#84124);
#74196=AXIS2_PLACEMENT_3D('',#126797,#84126,#84127);
#74197=AXIS2_PLACEMENT_3D('',#126799,#84128,#84129);
#74198=AXIS2_PLACEMENT_3D('',#126800,#84130,#84131);
#74199=AXIS2_PLACEMENT_3D('',#126814,#84133,#84134);
#74200=AXIS2_PLACEMENT_3D('',#126840,#84136,#84137);
#74201=AXIS2_PLACEMENT_3D('',#126842,#84138,#84139);
#74202=AXIS2_PLACEMENT_3D('',#126843,#84140,#84141);
#74203=AXIS2_PLACEMENT_3D('',#126857,#84143,#84144);
#74204=AXIS2_PLACEMENT_3D('',#126883,#84146,#84147);
#74205=AXIS2_PLACEMENT_3D('',#126885,#84148,#84149);
#74206=AXIS2_PLACEMENT_3D('',#126886,#84150,#84151);
#74207=AXIS2_PLACEMENT_3D('',#126900,#84153,#84154);
#74208=AXIS2_PLACEMENT_3D('',#126926,#84156,#84157);
#74209=AXIS2_PLACEMENT_3D('',#126928,#84158,#84159);
#74210=AXIS2_PLACEMENT_3D('',#126929,#84160,#84161);
#74211=AXIS2_PLACEMENT_3D('',#126971,#84165,#84166);
#74212=AXIS2_PLACEMENT_3D('',#126997,#84168,#84169);
#74213=AXIS2_PLACEMENT_3D('',#126999,#84170,#84171);
#74214=AXIS2_PLACEMENT_3D('',#127000,#84172,#84173);
#74215=AXIS2_PLACEMENT_3D('',#127014,#84175,#84176);
#74216=AXIS2_PLACEMENT_3D('',#127040,#84178,#84179);
#74217=AXIS2_PLACEMENT_3D('',#127042,#84180,#84181);
#74218=AXIS2_PLACEMENT_3D('',#127043,#84182,#84183);
#74219=AXIS2_PLACEMENT_3D('',#127057,#84185,#84186);
#74220=AXIS2_PLACEMENT_3D('',#127083,#84188,#84189);
#74221=AXIS2_PLACEMENT_3D('',#127085,#84190,#84191);
#74222=AXIS2_PLACEMENT_3D('',#127086,#84192,#84193);
#74223=AXIS2_PLACEMENT_3D('',#127100,#84195,#84196);
#74224=AXIS2_PLACEMENT_3D('',#127126,#84198,#84199);
#74225=AXIS2_PLACEMENT_3D('',#127128,#84200,#84201);
#74226=AXIS2_PLACEMENT_3D('',#127129,#84202,#84203);
#74227=AXIS2_PLACEMENT_3D('',#127143,#84205,#84206);
#74228=AXIS2_PLACEMENT_3D('',#127169,#84208,#84209);
#74229=AXIS2_PLACEMENT_3D('',#127171,#84210,#84211);
#74230=AXIS2_PLACEMENT_3D('',#127172,#84212,#84213);
#74231=AXIS2_PLACEMENT_3D('',#127186,#84215,#84216);
#74232=AXIS2_PLACEMENT_3D('',#127212,#84218,#84219);
#74233=AXIS2_PLACEMENT_3D('',#127214,#84220,#84221);
#74234=AXIS2_PLACEMENT_3D('',#127215,#84222,#84223);
#74235=AXIS2_PLACEMENT_3D('',#127229,#84225,#84226);
#74236=AXIS2_PLACEMENT_3D('',#127255,#84228,#84229);
#74237=AXIS2_PLACEMENT_3D('',#127257,#84230,#84231);
#74238=AXIS2_PLACEMENT_3D('',#127258,#84232,#84233);
#74239=AXIS2_PLACEMENT_3D('',#127270,#84234,#84235);
#74240=AXIS2_PLACEMENT_3D('',#127283,#84236,#84237);
#74241=AXIS2_PLACEMENT_3D('',#127295,#84238,#84239);
#74242=AXIS2_PLACEMENT_3D('',#127308,#84240,#84241);
#74243=AXIS2_PLACEMENT_3D('',#127320,#84242,#84243);
#74244=AXIS2_PLACEMENT_3D('',#127333,#84244,#84245);
#74245=AXIS2_PLACEMENT_3D('',#127345,#84246,#84247);
#74246=AXIS2_PLACEMENT_3D('',#127358,#84248,#84249);
#74247=AXIS2_PLACEMENT_3D('',#127370,#84250,#84251);
#74248=AXIS2_PLACEMENT_3D('',#127383,#84252,#84253);
#74249=AXIS2_PLACEMENT_3D('',#127395,#84254,#84255);
#74250=AXIS2_PLACEMENT_3D('',#127408,#84256,#84257);
#74251=AXIS2_PLACEMENT_3D('',#127420,#84258,#84259);
#74252=AXIS2_PLACEMENT_3D('',#127433,#84260,#84261);
#74253=AXIS2_PLACEMENT_3D('',#127445,#84262,#84263);
#74254=AXIS2_PLACEMENT_3D('',#127458,#84264,#84265);
#74255=AXIS2_PLACEMENT_3D('',#127470,#84266,#84267);
#74256=AXIS2_PLACEMENT_3D('',#127483,#84268,#84269);
#74257=AXIS2_PLACEMENT_3D('',#127495,#84270,#84271);
#74258=AXIS2_PLACEMENT_3D('',#127508,#84272,#84273);
#74259=AXIS2_PLACEMENT_3D('',#127520,#84274,#84275);
#74260=AXIS2_PLACEMENT_3D('',#127533,#84276,#84277);
#74261=AXIS2_PLACEMENT_3D('',#127545,#84278,#84279);
#74262=AXIS2_PLACEMENT_3D('',#127558,#84280,#84281);
#74263=AXIS2_PLACEMENT_3D('',#127570,#84282,#84283);
#74264=AXIS2_PLACEMENT_3D('',#127583,#84284,#84285);
#74265=AXIS2_PLACEMENT_3D('',#127595,#84286,#84287);
#74266=AXIS2_PLACEMENT_3D('',#127608,#84288,#84289);
#74267=AXIS2_PLACEMENT_3D('',#127620,#84290,#84291);
#74268=AXIS2_PLACEMENT_3D('',#127633,#84292,#84293);
#74269=AXIS2_PLACEMENT_3D('',#127645,#84294,#84295);
#74270=AXIS2_PLACEMENT_3D('',#127658,#84296,#84297);
#74271=AXIS2_PLACEMENT_3D('',#127670,#84298,#84299);
#74272=AXIS2_PLACEMENT_3D('',#127683,#84300,#84301);
#74273=AXIS2_PLACEMENT_3D('',#127695,#84302,#84303);
#74274=AXIS2_PLACEMENT_3D('',#127708,#84304,#84305);
#74275=AXIS2_PLACEMENT_3D('',#127720,#84306,#84307);
#74276=AXIS2_PLACEMENT_3D('',#127733,#84308,#84309);
#74277=AXIS2_PLACEMENT_3D('',#127745,#84310,#84311);
#74278=AXIS2_PLACEMENT_3D('',#127758,#84312,#84313);
#74279=AXIS2_PLACEMENT_3D('',#127770,#84314,#84315);
#74280=AXIS2_PLACEMENT_3D('',#127783,#84316,#84317);
#74281=AXIS2_PLACEMENT_3D('',#127795,#84318,#84319);
#74282=AXIS2_PLACEMENT_3D('',#127808,#84320,#84321);
#74283=AXIS2_PLACEMENT_3D('',#127820,#84322,#84323);
#74284=AXIS2_PLACEMENT_3D('',#127833,#84324,#84325);
#74285=AXIS2_PLACEMENT_3D('',#127845,#84326,#84327);
#74286=AXIS2_PLACEMENT_3D('',#127858,#84328,#84329);
#74287=AXIS2_PLACEMENT_3D('',#127870,#84330,#84331);
#74288=AXIS2_PLACEMENT_3D('',#127883,#84332,#84333);
#74289=AXIS2_PLACEMENT_3D('',#127895,#84334,#84335);
#74290=AXIS2_PLACEMENT_3D('',#127908,#84336,#84337);
#74291=AXIS2_PLACEMENT_3D('',#127920,#84338,#84339);
#74292=AXIS2_PLACEMENT_3D('',#127933,#84340,#84341);
#74293=AXIS2_PLACEMENT_3D('',#127945,#84342,#84343);
#74294=AXIS2_PLACEMENT_3D('',#127958,#84344,#84345);
#74295=AXIS2_PLACEMENT_3D('',#127970,#84346,#84347);
#74296=AXIS2_PLACEMENT_3D('',#127983,#84348,#84349);
#74297=AXIS2_PLACEMENT_3D('',#127995,#84350,#84351);
#74298=AXIS2_PLACEMENT_3D('',#128008,#84352,#84353);
#74299=AXIS2_PLACEMENT_3D('',#128020,#84354,#84355);
#74300=AXIS2_PLACEMENT_3D('',#128033,#84356,#84357);
#74301=AXIS2_PLACEMENT_3D('',#128045,#84358,#84359);
#74302=AXIS2_PLACEMENT_3D('',#128058,#84360,#84361);
#74303=AXIS2_PLACEMENT_3D('',#128070,#84362,#84363);
#74304=AXIS2_PLACEMENT_3D('',#128083,#84364,#84365);
#74305=AXIS2_PLACEMENT_3D('',#128095,#84366,#84367);
#74306=AXIS2_PLACEMENT_3D('',#128108,#84368,#84369);
#74307=AXIS2_PLACEMENT_3D('',#128120,#84370,#84371);
#74308=AXIS2_PLACEMENT_3D('',#128133,#84372,#84373);
#74309=AXIS2_PLACEMENT_3D('',#128145,#84374,#84375);
#74310=AXIS2_PLACEMENT_3D('',#128158,#84376,#84377);
#74311=AXIS2_PLACEMENT_3D('',#128170,#84378,#84379);
#74312=AXIS2_PLACEMENT_3D('',#128183,#84380,#84381);
#74313=AXIS2_PLACEMENT_3D('',#128195,#84382,#84383);
#74314=AXIS2_PLACEMENT_3D('',#128208,#84384,#84385);
#74315=AXIS2_PLACEMENT_3D('',#128220,#84386,#84387);
#74316=AXIS2_PLACEMENT_3D('',#128233,#84388,#84389);
#74317=AXIS2_PLACEMENT_3D('',#128245,#84390,#84391);
#74318=AXIS2_PLACEMENT_3D('',#128258,#84392,#84393);
#74319=AXIS2_PLACEMENT_3D('',#128270,#84394,#84395);
#74320=AXIS2_PLACEMENT_3D('',#128283,#84396,#84397);
#74321=AXIS2_PLACEMENT_3D('',#128295,#84398,#84399);
#74322=AXIS2_PLACEMENT_3D('',#128308,#84400,#84401);
#74323=AXIS2_PLACEMENT_3D('',#128320,#84402,#84403);
#74324=AXIS2_PLACEMENT_3D('',#128333,#84404,#84405);
#74325=AXIS2_PLACEMENT_3D('',#128345,#84406,#84407);
#74326=AXIS2_PLACEMENT_3D('',#128358,#84408,#84409);
#74327=AXIS2_PLACEMENT_3D('',#128370,#84410,#84411);
#74328=AXIS2_PLACEMENT_3D('',#128383,#84412,#84413);
#74329=AXIS2_PLACEMENT_3D('',#128395,#84414,#84415);
#74330=AXIS2_PLACEMENT_3D('',#128408,#84416,#84417);
#74331=AXIS2_PLACEMENT_3D('',#128420,#84418,#84419);
#74332=AXIS2_PLACEMENT_3D('',#128433,#84420,#84421);
#74333=AXIS2_PLACEMENT_3D('',#128445,#84422,#84423);
#74334=AXIS2_PLACEMENT_3D('',#128458,#84424,#84425);
#74335=AXIS2_PLACEMENT_3D('',#128470,#84426,#84427);
#74336=AXIS2_PLACEMENT_3D('',#128483,#84428,#84429);
#74337=AXIS2_PLACEMENT_3D('',#128495,#84430,#84431);
#74338=AXIS2_PLACEMENT_3D('',#128508,#84432,#84433);
#74339=AXIS2_PLACEMENT_3D('',#128520,#84434,#84435);
#74340=AXIS2_PLACEMENT_3D('',#128533,#84436,#84437);
#74341=AXIS2_PLACEMENT_3D('',#128545,#84438,#84439);
#74342=AXIS2_PLACEMENT_3D('',#128558,#84440,#84441);
#74343=AXIS2_PLACEMENT_3D('',#128570,#84442,#84443);
#74344=AXIS2_PLACEMENT_3D('',#128583,#84444,#84445);
#74345=AXIS2_PLACEMENT_3D('',#128595,#84446,#84447);
#74346=AXIS2_PLACEMENT_3D('',#128608,#84448,#84449);
#74347=AXIS2_PLACEMENT_3D('',#128620,#84450,#84451);
#74348=AXIS2_PLACEMENT_3D('',#128633,#84452,#84453);
#74349=AXIS2_PLACEMENT_3D('',#128645,#84454,#84455);
#74350=AXIS2_PLACEMENT_3D('',#128658,#84456,#84457);
#74351=AXIS2_PLACEMENT_3D('',#128670,#84458,#84459);
#74352=AXIS2_PLACEMENT_3D('',#128683,#84460,#84461);
#74353=AXIS2_PLACEMENT_3D('',#128695,#84462,#84463);
#74354=AXIS2_PLACEMENT_3D('',#128708,#84464,#84465);
#74355=AXIS2_PLACEMENT_3D('',#128721,#84466,#84467);
#74356=AXIS2_PLACEMENT_3D('',#128741,#84469,#84470);
#74357=AXIS2_PLACEMENT_3D('',#128749,#84472,#84473);
#74358=AXIS2_PLACEMENT_3D('',#128751,#84474,#84475);
#74359=AXIS2_PLACEMENT_3D('',#128753,#84476,#84477);
#74360=AXIS2_PLACEMENT_3D('',#128754,#84478,#84479);
#74361=AXIS2_PLACEMENT_3D('',#128778,#84481,#84482);
#74362=AXIS2_PLACEMENT_3D('',#128786,#84484,#84485);
#74363=AXIS2_PLACEMENT_3D('',#128788,#84486,#84487);
#74364=AXIS2_PLACEMENT_3D('',#128790,#84488,#84489);
#74365=AXIS2_PLACEMENT_3D('',#128791,#84490,#84491);
#74366=AXIS2_PLACEMENT_3D('',#128815,#84493,#84494);
#74367=AXIS2_PLACEMENT_3D('',#128823,#84496,#84497);
#74368=AXIS2_PLACEMENT_3D('',#128825,#84498,#84499);
#74369=AXIS2_PLACEMENT_3D('',#128827,#84500,#84501);
#74370=AXIS2_PLACEMENT_3D('',#128828,#84502,#84503);
#74371=AXIS2_PLACEMENT_3D('',#128852,#84505,#84506);
#74372=AXIS2_PLACEMENT_3D('',#128860,#84508,#84509);
#74373=AXIS2_PLACEMENT_3D('',#128862,#84510,#84511);
#74374=AXIS2_PLACEMENT_3D('',#128864,#84512,#84513);
#74375=AXIS2_PLACEMENT_3D('',#128865,#84514,#84515);
#74376=AXIS2_PLACEMENT_3D('',#128889,#84517,#84518);
#74377=AXIS2_PLACEMENT_3D('',#128897,#84520,#84521);
#74378=AXIS2_PLACEMENT_3D('',#128899,#84522,#84523);
#74379=AXIS2_PLACEMENT_3D('',#128901,#84524,#84525);
#74380=AXIS2_PLACEMENT_3D('',#128902,#84526,#84527);
#74381=AXIS2_PLACEMENT_3D('',#128926,#84529,#84530);
#74382=AXIS2_PLACEMENT_3D('',#128934,#84532,#84533);
#74383=AXIS2_PLACEMENT_3D('',#128936,#84534,#84535);
#74384=AXIS2_PLACEMENT_3D('',#128938,#84536,#84537);
#74385=AXIS2_PLACEMENT_3D('',#128939,#84538,#84539);
#74386=AXIS2_PLACEMENT_3D('',#128991,#84543,#84544);
#74387=AXIS2_PLACEMENT_3D('',#128999,#84546,#84547);
#74388=AXIS2_PLACEMENT_3D('',#129001,#84548,#84549);
#74389=AXIS2_PLACEMENT_3D('',#129003,#84550,#84551);
#74390=AXIS2_PLACEMENT_3D('',#129004,#84552,#84553);
#74391=AXIS2_PLACEMENT_3D('',#129028,#84555,#84556);
#74392=AXIS2_PLACEMENT_3D('',#129036,#84558,#84559);
#74393=AXIS2_PLACEMENT_3D('',#129038,#84560,#84561);
#74394=AXIS2_PLACEMENT_3D('',#129040,#84562,#84563);
#74395=AXIS2_PLACEMENT_3D('',#129041,#84564,#84565);
#74396=AXIS2_PLACEMENT_3D('',#129065,#84567,#84568);
#74397=AXIS2_PLACEMENT_3D('',#129073,#84570,#84571);
#74398=AXIS2_PLACEMENT_3D('',#129075,#84572,#84573);
#74399=AXIS2_PLACEMENT_3D('',#129077,#84574,#84575);
#74400=AXIS2_PLACEMENT_3D('',#129078,#84576,#84577);
#74401=AXIS2_PLACEMENT_3D('',#129102,#84579,#84580);
#74402=AXIS2_PLACEMENT_3D('',#129110,#84582,#84583);
#74403=AXIS2_PLACEMENT_3D('',#129112,#84584,#84585);
#74404=AXIS2_PLACEMENT_3D('',#129114,#84586,#84587);
#74405=AXIS2_PLACEMENT_3D('',#129115,#84588,#84589);
#74406=AXIS2_PLACEMENT_3D('',#129139,#84591,#84592);
#74407=AXIS2_PLACEMENT_3D('',#129147,#84594,#84595);
#74408=AXIS2_PLACEMENT_3D('',#129149,#84596,#84597);
#74409=AXIS2_PLACEMENT_3D('',#129151,#84598,#84599);
#74410=AXIS2_PLACEMENT_3D('',#129152,#84600,#84601);
#74411=AXIS2_PLACEMENT_3D('',#129176,#84603,#84604);
#74412=AXIS2_PLACEMENT_3D('',#129184,#84606,#84607);
#74413=AXIS2_PLACEMENT_3D('',#129186,#84608,#84609);
#74414=AXIS2_PLACEMENT_3D('',#129188,#84610,#84611);
#74415=AXIS2_PLACEMENT_3D('',#129189,#84612,#84613);
#74416=AXIS2_PLACEMENT_3D('',#129213,#84615,#84616);
#74417=AXIS2_PLACEMENT_3D('',#129221,#84618,#84619);
#74418=AXIS2_PLACEMENT_3D('',#129223,#84620,#84621);
#74419=AXIS2_PLACEMENT_3D('',#129225,#84622,#84623);
#74420=AXIS2_PLACEMENT_3D('',#129226,#84624,#84625);
#74421=AXIS2_PLACEMENT_3D('',#129250,#84627,#84628);
#74422=AXIS2_PLACEMENT_3D('',#129258,#84630,#84631);
#74423=AXIS2_PLACEMENT_3D('',#129260,#84632,#84633);
#74424=AXIS2_PLACEMENT_3D('',#129262,#84634,#84635);
#74425=AXIS2_PLACEMENT_3D('',#129263,#84636,#84637);
#74426=AXIS2_PLACEMENT_3D('',#129287,#84639,#84640);
#74427=AXIS2_PLACEMENT_3D('',#129295,#84642,#84643);
#74428=AXIS2_PLACEMENT_3D('',#129297,#84644,#84645);
#74429=AXIS2_PLACEMENT_3D('',#129299,#84646,#84647);
#74430=AXIS2_PLACEMENT_3D('',#129300,#84648,#84649);
#74431=AXIS2_PLACEMENT_3D('',#129324,#84651,#84652);
#74432=AXIS2_PLACEMENT_3D('',#129332,#84654,#84655);
#74433=AXIS2_PLACEMENT_3D('',#129334,#84656,#84657);
#74434=AXIS2_PLACEMENT_3D('',#129336,#84658,#84659);
#74435=AXIS2_PLACEMENT_3D('',#129337,#84660,#84661);
#74436=AXIS2_PLACEMENT_3D('',#129361,#84663,#84664);
#74437=AXIS2_PLACEMENT_3D('',#129369,#84666,#84667);
#74438=AXIS2_PLACEMENT_3D('',#129371,#84668,#84669);
#74439=AXIS2_PLACEMENT_3D('',#129373,#84670,#84671);
#74440=AXIS2_PLACEMENT_3D('',#129374,#84672,#84673);
#74441=AXIS2_PLACEMENT_3D('',#129398,#84675,#84676);
#74442=AXIS2_PLACEMENT_3D('',#129406,#84678,#84679);
#74443=AXIS2_PLACEMENT_3D('',#129408,#84680,#84681);
#74444=AXIS2_PLACEMENT_3D('',#129410,#84682,#84683);
#74445=AXIS2_PLACEMENT_3D('',#129411,#84684,#84685);
#74446=AXIS2_PLACEMENT_3D('',#129435,#84687,#84688);
#74447=AXIS2_PLACEMENT_3D('',#129443,#84690,#84691);
#74448=AXIS2_PLACEMENT_3D('',#129445,#84692,#84693);
#74449=AXIS2_PLACEMENT_3D('',#129447,#84694,#84695);
#74450=AXIS2_PLACEMENT_3D('',#129448,#84696,#84697);
#74451=AXIS2_PLACEMENT_3D('',#129472,#84699,#84700);
#74452=AXIS2_PLACEMENT_3D('',#129491,#84702,#84703);
#74453=AXIS2_PLACEMENT_3D('',#129493,#84705,#84706);
#74454=AXIS2_PLACEMENT_3D('',#129495,#84707,#84708);
#74455=AXIS2_PLACEMENT_3D('',#129496,#84709,#84710);
#74456=AXIS2_PLACEMENT_3D('',#129510,#84712,#84713);
#74457=AXIS2_PLACEMENT_3D('',#129517,#84714,#84715);
#74458=AXIS2_PLACEMENT_3D('',#129519,#84716,#84717);
#74459=AXIS2_PLACEMENT_3D('',#129521,#84718,#84719);
#74460=AXIS2_PLACEMENT_3D('',#129522,#84720,#84721);
#74461=AXIS2_PLACEMENT_3D('',#129546,#84723,#84724);
#74462=AXIS2_PLACEMENT_3D('',#129554,#84726,#84727);
#74463=AXIS2_PLACEMENT_3D('',#129556,#84728,#84729);
#74464=AXIS2_PLACEMENT_3D('',#129558,#84730,#84731);
#74465=AXIS2_PLACEMENT_3D('',#129559,#84732,#84733);
#74466=AXIS2_PLACEMENT_3D('',#129583,#84735,#84736);
#74467=AXIS2_PLACEMENT_3D('',#129591,#84738,#84739);
#74468=AXIS2_PLACEMENT_3D('',#129593,#84740,#84741);
#74469=AXIS2_PLACEMENT_3D('',#129595,#84742,#84743);
#74470=AXIS2_PLACEMENT_3D('',#129596,#84744,#84745);
#74471=AXIS2_PLACEMENT_3D('',#129620,#84747,#84748);
#74472=AXIS2_PLACEMENT_3D('',#129628,#84750,#84751);
#74473=AXIS2_PLACEMENT_3D('',#129630,#84752,#84753);
#74474=AXIS2_PLACEMENT_3D('',#129632,#84754,#84755);
#74475=AXIS2_PLACEMENT_3D('',#129633,#84756,#84757);
#74476=AXIS2_PLACEMENT_3D('',#129657,#84759,#84760);
#74477=AXIS2_PLACEMENT_3D('',#129665,#84762,#84763);
#74478=AXIS2_PLACEMENT_3D('',#129667,#84764,#84765);
#74479=AXIS2_PLACEMENT_3D('',#129669,#84766,#84767);
#74480=AXIS2_PLACEMENT_3D('',#129670,#84768,#84769);
#74481=AXIS2_PLACEMENT_3D('',#129694,#84771,#84772);
#74482=AXIS2_PLACEMENT_3D('',#129702,#84774,#84775);
#74483=AXIS2_PLACEMENT_3D('',#129704,#84776,#84777);
#74484=AXIS2_PLACEMENT_3D('',#129706,#84778,#84779);
#74485=AXIS2_PLACEMENT_3D('',#129707,#84780,#84781);
#74486=AXIS2_PLACEMENT_3D('',#129731,#84783,#84784);
#74487=AXIS2_PLACEMENT_3D('',#129739,#84786,#84787);
#74488=AXIS2_PLACEMENT_3D('',#129741,#84788,#84789);
#74489=AXIS2_PLACEMENT_3D('',#129743,#84790,#84791);
#74490=AXIS2_PLACEMENT_3D('',#129744,#84792,#84793);
#74491=AXIS2_PLACEMENT_3D('',#129756,#84795,#84796);
#74492=AXIS2_PLACEMENT_3D('',#129759,#84797,#84798);
#74493=AXIS2_PLACEMENT_3D('',#129760,#84799,#84800);
#74494=AXIS2_PLACEMENT_3D('',#129761,#84801,#84802);
#74495=AXIS2_PLACEMENT_3D('',#129787,#84804,#84805);
#74496=AXIS2_PLACEMENT_3D('',#129802,#84808,#84809);
#74497=AXIS2_PLACEMENT_3D('',#129816,#84810,#84811);
#74498=AXIS2_PLACEMENT_3D('',#129818,#84813,#84814);
#74499=AXIS2_PLACEMENT_3D('',#129820,#84815,#84816);
#74500=AXIS2_PLACEMENT_3D('',#129821,#84817,#84818);
#74501=AXIS2_PLACEMENT_3D('',#129835,#84820,#84821);
#74502=AXIS2_PLACEMENT_3D('',#129849,#84822,#84823);
#74503=AXIS2_PLACEMENT_3D('',#129851,#84825,#84826);
#74504=AXIS2_PLACEMENT_3D('',#129853,#84827,#84828);
#74505=AXIS2_PLACEMENT_3D('',#129854,#84829,#84830);
#74506=AXIS2_PLACEMENT_3D('',#129868,#84832,#84833);
#74507=AXIS2_PLACEMENT_3D('',#129882,#84834,#84835);
#74508=AXIS2_PLACEMENT_3D('',#129884,#84837,#84838);
#74509=AXIS2_PLACEMENT_3D('',#129886,#84839,#84840);
#74510=AXIS2_PLACEMENT_3D('',#129887,#84841,#84842);
#74511=AXIS2_PLACEMENT_3D('',#129901,#84844,#84845);
#74512=AXIS2_PLACEMENT_3D('',#129915,#84846,#84847);
#74513=AXIS2_PLACEMENT_3D('',#129917,#84849,#84850);
#74514=AXIS2_PLACEMENT_3D('',#129919,#84851,#84852);
#74515=AXIS2_PLACEMENT_3D('',#129920,#84853,#84854);
#74516=AXIS2_PLACEMENT_3D('',#129934,#84856,#84857);
#74517=AXIS2_PLACEMENT_3D('',#129948,#84858,#84859);
#74518=AXIS2_PLACEMENT_3D('',#129950,#84861,#84862);
#74519=AXIS2_PLACEMENT_3D('',#129952,#84863,#84864);
#74520=AXIS2_PLACEMENT_3D('',#129953,#84865,#84866);
#74521=AXIS2_PLACEMENT_3D('',#129967,#84868,#84869);
#74522=AXIS2_PLACEMENT_3D('',#129981,#84870,#84871);
#74523=AXIS2_PLACEMENT_3D('',#129983,#84873,#84874);
#74524=AXIS2_PLACEMENT_3D('',#129985,#84875,#84876);
#74525=AXIS2_PLACEMENT_3D('',#129986,#84877,#84878);
#74526=AXIS2_PLACEMENT_3D('',#130000,#84880,#84881);
#74527=AXIS2_PLACEMENT_3D('',#130014,#84882,#84883);
#74528=AXIS2_PLACEMENT_3D('',#130016,#84885,#84886);
#74529=AXIS2_PLACEMENT_3D('',#130018,#84887,#84888);
#74530=AXIS2_PLACEMENT_3D('',#130019,#84889,#84890);
#74531=AXIS2_PLACEMENT_3D('',#130033,#84892,#84893);
#74532=AXIS2_PLACEMENT_3D('',#130047,#84894,#84895);
#74533=AXIS2_PLACEMENT_3D('',#130049,#84897,#84898);
#74534=AXIS2_PLACEMENT_3D('',#130051,#84899,#84900);
#74535=AXIS2_PLACEMENT_3D('',#130052,#84901,#84902);
#74536=AXIS2_PLACEMENT_3D('',#130066,#84904,#84905);
#74537=AXIS2_PLACEMENT_3D('',#130080,#84906,#84907);
#74538=AXIS2_PLACEMENT_3D('',#130082,#84909,#84910);
#74539=AXIS2_PLACEMENT_3D('',#130084,#84911,#84912);
#74540=AXIS2_PLACEMENT_3D('',#130085,#84913,#84914);
#74541=AXIS2_PLACEMENT_3D('',#130099,#84916,#84917);
#74542=AXIS2_PLACEMENT_3D('',#130113,#84918,#84919);
#74543=AXIS2_PLACEMENT_3D('',#130115,#84921,#84922);
#74544=AXIS2_PLACEMENT_3D('',#130117,#84923,#84924);
#74545=AXIS2_PLACEMENT_3D('',#130118,#84925,#84926);
#74546=AXIS2_PLACEMENT_3D('',#130132,#84928,#84929);
#74547=AXIS2_PLACEMENT_3D('',#130146,#84930,#84931);
#74548=AXIS2_PLACEMENT_3D('',#130148,#84933,#84934);
#74549=AXIS2_PLACEMENT_3D('',#130150,#84935,#84936);
#74550=AXIS2_PLACEMENT_3D('',#130151,#84937,#84938);
#74551=AXIS2_PLACEMENT_3D('',#130165,#84940,#84941);
#74552=AXIS2_PLACEMENT_3D('',#130179,#84942,#84943);
#74553=AXIS2_PLACEMENT_3D('',#130181,#84945,#84946);
#74554=AXIS2_PLACEMENT_3D('',#130183,#84947,#84948);
#74555=AXIS2_PLACEMENT_3D('',#130184,#84949,#84950);
#74556=AXIS2_PLACEMENT_3D('',#130198,#84952,#84953);
#74557=AXIS2_PLACEMENT_3D('',#130212,#84954,#84955);
#74558=AXIS2_PLACEMENT_3D('',#130214,#84957,#84958);
#74559=AXIS2_PLACEMENT_3D('',#130216,#84959,#84960);
#74560=AXIS2_PLACEMENT_3D('',#130217,#84961,#84962);
#74561=AXIS2_PLACEMENT_3D('',#130255,#84966,#84967);
#74562=AXIS2_PLACEMENT_3D('',#130269,#84968,#84969);
#74563=AXIS2_PLACEMENT_3D('',#130271,#84971,#84972);
#74564=AXIS2_PLACEMENT_3D('',#130273,#84973,#84974);
#74565=AXIS2_PLACEMENT_3D('',#130274,#84975,#84976);
#74566=AXIS2_PLACEMENT_3D('',#130288,#84978,#84979);
#74567=AXIS2_PLACEMENT_3D('',#130302,#84980,#84981);
#74568=AXIS2_PLACEMENT_3D('',#130304,#84983,#84984);
#74569=AXIS2_PLACEMENT_3D('',#130306,#84985,#84986);
#74570=AXIS2_PLACEMENT_3D('',#130307,#84987,#84988);
#74571=AXIS2_PLACEMENT_3D('',#130321,#84990,#84991);
#74572=AXIS2_PLACEMENT_3D('',#130335,#84992,#84993);
#74573=AXIS2_PLACEMENT_3D('',#130337,#84995,#84996);
#74574=AXIS2_PLACEMENT_3D('',#130339,#84997,#84998);
#74575=AXIS2_PLACEMENT_3D('',#130340,#84999,#85000);
#74576=AXIS2_PLACEMENT_3D('',#130354,#85002,#85003);
#74577=AXIS2_PLACEMENT_3D('',#130368,#85004,#85005);
#74578=AXIS2_PLACEMENT_3D('',#130370,#85007,#85008);
#74579=AXIS2_PLACEMENT_3D('',#130372,#85009,#85010);
#74580=AXIS2_PLACEMENT_3D('',#130373,#85011,#85012);
#74581=AXIS2_PLACEMENT_3D('',#130387,#85014,#85015);
#74582=AXIS2_PLACEMENT_3D('',#130401,#85016,#85017);
#74583=AXIS2_PLACEMENT_3D('',#130403,#85019,#85020);
#74584=AXIS2_PLACEMENT_3D('',#130405,#85021,#85022);
#74585=AXIS2_PLACEMENT_3D('',#130406,#85023,#85024);
#74586=AXIS2_PLACEMENT_3D('',#130420,#85026,#85027);
#74587=AXIS2_PLACEMENT_3D('',#130434,#85028,#85029);
#74588=AXIS2_PLACEMENT_3D('',#130436,#85031,#85032);
#74589=AXIS2_PLACEMENT_3D('',#130438,#85033,#85034);
#74590=AXIS2_PLACEMENT_3D('',#130439,#85035,#85036);
#74591=AXIS2_PLACEMENT_3D('',#130453,#85038,#85039);
#74592=AXIS2_PLACEMENT_3D('',#130467,#85040,#85041);
#74593=AXIS2_PLACEMENT_3D('',#130469,#85043,#85044);
#74594=AXIS2_PLACEMENT_3D('',#130471,#85045,#85046);
#74595=AXIS2_PLACEMENT_3D('',#130472,#85047,#85048);
#74596=AXIS2_PLACEMENT_3D('',#130486,#85050,#85051);
#74597=AXIS2_PLACEMENT_3D('',#130500,#85052,#85053);
#74598=AXIS2_PLACEMENT_3D('',#130502,#85055,#85056);
#74599=AXIS2_PLACEMENT_3D('',#130504,#85057,#85058);
#74600=AXIS2_PLACEMENT_3D('',#130505,#85059,#85060);
#74601=AXIS2_PLACEMENT_3D('',#130519,#85062,#85063);
#74602=AXIS2_PLACEMENT_3D('',#130533,#85064,#85065);
#74603=AXIS2_PLACEMENT_3D('',#130535,#85067,#85068);
#74604=AXIS2_PLACEMENT_3D('',#130537,#85069,#85070);
#74605=AXIS2_PLACEMENT_3D('',#130538,#85071,#85072);
#74606=AXIS2_PLACEMENT_3D('',#130552,#85074,#85075);
#74607=AXIS2_PLACEMENT_3D('',#130566,#85076,#85077);
#74608=AXIS2_PLACEMENT_3D('',#130568,#85079,#85080);
#74609=AXIS2_PLACEMENT_3D('',#130570,#85081,#85082);
#74610=AXIS2_PLACEMENT_3D('',#130571,#85083,#85084);
#74611=AXIS2_PLACEMENT_3D('',#130585,#85086,#85087);
#74612=AXIS2_PLACEMENT_3D('',#130599,#85088,#85089);
#74613=AXIS2_PLACEMENT_3D('',#130601,#85091,#85092);
#74614=AXIS2_PLACEMENT_3D('',#130603,#85093,#85094);
#74615=AXIS2_PLACEMENT_3D('',#130604,#85095,#85096);
#74616=AXIS2_PLACEMENT_3D('',#130618,#85098,#85099);
#74617=AXIS2_PLACEMENT_3D('',#130632,#85100,#85101);
#74618=AXIS2_PLACEMENT_3D('',#130634,#85103,#85104);
#74619=AXIS2_PLACEMENT_3D('',#130636,#85105,#85106);
#74620=AXIS2_PLACEMENT_3D('',#130637,#85107,#85108);
#74621=AXIS2_PLACEMENT_3D('',#130651,#85110,#85111);
#74622=AXIS2_PLACEMENT_3D('',#130665,#85112,#85113);
#74623=AXIS2_PLACEMENT_3D('',#130667,#85115,#85116);
#74624=AXIS2_PLACEMENT_3D('',#130669,#85117,#85118);
#74625=AXIS2_PLACEMENT_3D('',#130670,#85119,#85120);
#74626=AXIS2_PLACEMENT_3D('',#130684,#85122,#85123);
#74627=AXIS2_PLACEMENT_3D('',#130698,#85124,#85125);
#74628=AXIS2_PLACEMENT_3D('',#130700,#85127,#85128);
#74629=AXIS2_PLACEMENT_3D('',#130702,#85129,#85130);
#74630=AXIS2_PLACEMENT_3D('',#130703,#85131,#85132);
#74631=AXIS2_PLACEMENT_3D('',#130704,#85133,#85134);
#74632=AXIS2_PLACEMENT_3D('',#130706,#85135,#85136);
#74633=AXIS2_PLACEMENT_3D('',#130708,#85137,#85138);
#74634=AXIS2_PLACEMENT_3D('',#130709,#85139,#85140);
#74635=AXIS2_PLACEMENT_3D('',#130728,#85142,#85143);
#74636=AXIS2_PLACEMENT_3D('',#130776,#85144,#85145);
#74637=AXIS2_PLACEMENT_3D('',#130814,#85146,#85147);
#74638=AXIS2_PLACEMENT_3D('',#130852,#85148,#85149);
#74639=AXIS2_PLACEMENT_3D('',#130890,#85150,#85151);
#74640=AXIS2_PLACEMENT_3D('',#130928,#85152,#85153);
#74641=AXIS2_PLACEMENT_3D('',#130966,#85154,#85155);
#74642=AXIS2_PLACEMENT_3D('',#131004,#85156,#85157);
#74643=AXIS2_PLACEMENT_3D('',#131042,#85158,#85159);
#74644=AXIS2_PLACEMENT_3D('',#131080,#85160,#85161);
#74645=AXIS2_PLACEMENT_3D('',#131118,#85162,#85163);
#74646=AXIS2_PLACEMENT_3D('',#131156,#85164,#85165);
#74647=AXIS2_PLACEMENT_3D('',#131194,#85166,#85167);
#74648=AXIS2_PLACEMENT_3D('',#131232,#85168,#85169);
#74649=AXIS2_PLACEMENT_3D('',#131270,#85170,#85171);
#74650=AXIS2_PLACEMENT_3D('',#131308,#85172,#85173);
#74651=AXIS2_PLACEMENT_3D('',#131346,#85174,#85175);
#74652=AXIS2_PLACEMENT_3D('',#131384,#85176,#85177);
#74653=AXIS2_PLACEMENT_3D('',#131422,#85178,#85179);
#74654=AXIS2_PLACEMENT_3D('',#131460,#85180,#85181);
#74655=AXIS2_PLACEMENT_3D('',#131498,#85182,#85183);
#74656=AXIS2_PLACEMENT_3D('',#131536,#85184,#85185);
#74657=AXIS2_PLACEMENT_3D('',#131574,#85186,#85187);
#74658=AXIS2_PLACEMENT_3D('',#131612,#85188,#85189);
#74659=AXIS2_PLACEMENT_3D('',#131650,#85190,#85191);
#74660=AXIS2_PLACEMENT_3D('',#131688,#85192,#85193);
#74661=AXIS2_PLACEMENT_3D('',#131726,#85194,#85195);
#74662=AXIS2_PLACEMENT_3D('',#131764,#85196,#85197);
#74663=AXIS2_PLACEMENT_3D('',#131802,#85198,#85199);
#74664=AXIS2_PLACEMENT_3D('',#131836,#85200,#85201);
#74665=AXIS2_PLACEMENT_3D('',#131848,#85202,#85203);
#74666=AXIS2_PLACEMENT_3D('',#131864,#85204,#85205);
#74667=AXIS2_PLACEMENT_3D('',#131876,#85206,#85207);
#74668=AXIS2_PLACEMENT_3D('',#131892,#85208,#85209);
#74669=AXIS2_PLACEMENT_3D('',#131904,#85210,#85211);
#74670=AXIS2_PLACEMENT_3D('',#131920,#85212,#85213);
#74671=AXIS2_PLACEMENT_3D('',#131932,#85214,#85215);
#74672=AXIS2_PLACEMENT_3D('',#131948,#85216,#85217);
#74673=AXIS2_PLACEMENT_3D('',#131960,#85218,#85219);
#74674=AXIS2_PLACEMENT_3D('',#131976,#85220,#85221);
#74675=AXIS2_PLACEMENT_3D('',#131988,#85222,#85223);
#74676=AXIS2_PLACEMENT_3D('',#132004,#85224,#85225);
#74677=AXIS2_PLACEMENT_3D('',#132016,#85226,#85227);
#74678=AXIS2_PLACEMENT_3D('',#132032,#85228,#85229);
#74679=AXIS2_PLACEMENT_3D('',#132044,#85230,#85231);
#74680=AXIS2_PLACEMENT_3D('',#132060,#85232,#85233);
#74681=AXIS2_PLACEMENT_3D('',#132072,#85234,#85235);
#74682=AXIS2_PLACEMENT_3D('',#132088,#85236,#85237);
#74683=AXIS2_PLACEMENT_3D('',#132100,#85238,#85239);
#74684=AXIS2_PLACEMENT_3D('',#132116,#85240,#85241);
#74685=AXIS2_PLACEMENT_3D('',#132128,#85242,#85243);
#74686=AXIS2_PLACEMENT_3D('',#132144,#85244,#85245);
#74687=AXIS2_PLACEMENT_3D('',#132156,#85246,#85247);
#74688=AXIS2_PLACEMENT_3D('',#132172,#85248,#85249);
#74689=AXIS2_PLACEMENT_3D('',#132184,#85250,#85251);
#74690=AXIS2_PLACEMENT_3D('',#132200,#85252,#85253);
#74691=AXIS2_PLACEMENT_3D('',#132212,#85254,#85255);
#74692=AXIS2_PLACEMENT_3D('',#132228,#85256,#85257);
#74693=AXIS2_PLACEMENT_3D('',#132240,#85258,#85259);
#74694=AXIS2_PLACEMENT_3D('',#132256,#85260,#85261);
#74695=AXIS2_PLACEMENT_3D('',#132268,#85262,#85263);
#74696=AXIS2_PLACEMENT_3D('',#132284,#85264,#85265);
#74697=AXIS2_PLACEMENT_3D('',#132296,#85266,#85267);
#74698=AXIS2_PLACEMENT_3D('',#132312,#85268,#85269);
#74699=AXIS2_PLACEMENT_3D('',#132324,#85270,#85271);
#74700=AXIS2_PLACEMENT_3D('',#132340,#85272,#85273);
#74701=AXIS2_PLACEMENT_3D('',#132352,#85274,#85275);
#74702=AXIS2_PLACEMENT_3D('',#132368,#85276,#85277);
#74703=AXIS2_PLACEMENT_3D('',#132380,#85278,#85279);
#74704=AXIS2_PLACEMENT_3D('',#132396,#85280,#85281);
#74705=AXIS2_PLACEMENT_3D('',#132408,#85282,#85283);
#74706=AXIS2_PLACEMENT_3D('',#132424,#85284,#85285);
#74707=AXIS2_PLACEMENT_3D('',#132436,#85286,#85287);
#74708=AXIS2_PLACEMENT_3D('',#132452,#85288,#85289);
#74709=AXIS2_PLACEMENT_3D('',#132464,#85290,#85291);
#74710=AXIS2_PLACEMENT_3D('',#132480,#85292,#85293);
#74711=AXIS2_PLACEMENT_3D('',#132492,#85294,#85295);
#74712=AXIS2_PLACEMENT_3D('',#132508,#85296,#85297);
#74713=AXIS2_PLACEMENT_3D('',#132520,#85298,#85299);
#74714=AXIS2_PLACEMENT_3D('',#132536,#85300,#85301);
#74715=AXIS2_PLACEMENT_3D('',#132548,#85302,#85303);
#74716=AXIS2_PLACEMENT_3D('',#132564,#85304,#85305);
#74717=AXIS2_PLACEMENT_3D('',#132576,#85306,#85307);
#74718=AXIS2_PLACEMENT_3D('',#132592,#85308,#85309);
#74719=AXIS2_PLACEMENT_3D('',#132604,#85310,#85311);
#74720=AXIS2_PLACEMENT_3D('',#132620,#85312,#85313);
#74721=AXIS2_PLACEMENT_3D('',#132636,#85314,#85315);
#74722=AXIS2_PLACEMENT_3D('',#132645,#85316,#85317);
#74723=AXIS2_PLACEMENT_3D('',#132653,#85319,#85320);
#74724=AXIS2_PLACEMENT_3D('',#132655,#85321,#85322);
#74725=AXIS2_PLACEMENT_3D('',#132657,#85323,#85324);
#74726=AXIS2_PLACEMENT_3D('',#132684,#85326,#85327);
#74727=AXIS2_PLACEMENT_3D('',#132692,#85329,#85330);
#74728=AXIS2_PLACEMENT_3D('',#132694,#85331,#85332);
#74729=AXIS2_PLACEMENT_3D('',#132696,#85333,#85334);
#74730=AXIS2_PLACEMENT_3D('',#132723,#85336,#85337);
#74731=AXIS2_PLACEMENT_3D('',#132731,#85339,#85340);
#74732=AXIS2_PLACEMENT_3D('',#132733,#85341,#85342);
#74733=AXIS2_PLACEMENT_3D('',#132735,#85343,#85344);
#74734=AXIS2_PLACEMENT_3D('',#132762,#85346,#85347);
#74735=AXIS2_PLACEMENT_3D('',#132770,#85349,#85350);
#74736=AXIS2_PLACEMENT_3D('',#132772,#85351,#85352);
#74737=AXIS2_PLACEMENT_3D('',#132774,#85353,#85354);
#74738=AXIS2_PLACEMENT_3D('',#132801,#85356,#85357);
#74739=AXIS2_PLACEMENT_3D('',#132809,#85359,#85360);
#74740=AXIS2_PLACEMENT_3D('',#132811,#85361,#85362);
#74741=AXIS2_PLACEMENT_3D('',#132813,#85363,#85364);
#74742=AXIS2_PLACEMENT_3D('',#132840,#85366,#85367);
#74743=AXIS2_PLACEMENT_3D('',#132848,#85369,#85370);
#74744=AXIS2_PLACEMENT_3D('',#132850,#85371,#85372);
#74745=AXIS2_PLACEMENT_3D('',#132852,#85373,#85374);
#74746=AXIS2_PLACEMENT_3D('',#132879,#85376,#85377);
#74747=AXIS2_PLACEMENT_3D('',#132887,#85379,#85380);
#74748=AXIS2_PLACEMENT_3D('',#132889,#85381,#85382);
#74749=AXIS2_PLACEMENT_3D('',#132891,#85383,#85384);
#74750=AXIS2_PLACEMENT_3D('',#132918,#85386,#85387);
#74751=AXIS2_PLACEMENT_3D('',#132926,#85389,#85390);
#74752=AXIS2_PLACEMENT_3D('',#132928,#85391,#85392);
#74753=AXIS2_PLACEMENT_3D('',#132930,#85393,#85394);
#74754=AXIS2_PLACEMENT_3D('',#132957,#85396,#85397);
#74755=AXIS2_PLACEMENT_3D('',#132965,#85399,#85400);
#74756=AXIS2_PLACEMENT_3D('',#132967,#85401,#85402);
#74757=AXIS2_PLACEMENT_3D('',#132969,#85403,#85404);
#74758=AXIS2_PLACEMENT_3D('',#132994,#85406,#85407);
#74759=AXIS2_PLACEMENT_3D('',#133002,#85409,#85410);
#74760=AXIS2_PLACEMENT_3D('',#133004,#85411,#85412);
#74761=AXIS2_PLACEMENT_3D('',#133006,#85413,#85414);
#74762=AXIS2_PLACEMENT_3D('',#133033,#85416,#85417);
#74763=AXIS2_PLACEMENT_3D('',#133041,#85419,#85420);
#74764=AXIS2_PLACEMENT_3D('',#133043,#85421,#85422);
#74765=AXIS2_PLACEMENT_3D('',#133045,#85423,#85424);
#74766=AXIS2_PLACEMENT_3D('',#133072,#85426,#85427);
#74767=AXIS2_PLACEMENT_3D('',#133080,#85429,#85430);
#74768=AXIS2_PLACEMENT_3D('',#133082,#85431,#85432);
#74769=AXIS2_PLACEMENT_3D('',#133084,#85433,#85434);
#74770=AXIS2_PLACEMENT_3D('',#133111,#85436,#85437);
#74771=AXIS2_PLACEMENT_3D('',#133119,#85439,#85440);
#74772=AXIS2_PLACEMENT_3D('',#133121,#85441,#85442);
#74773=AXIS2_PLACEMENT_3D('',#133123,#85443,#85444);
#74774=AXIS2_PLACEMENT_3D('',#133150,#85446,#85447);
#74775=AXIS2_PLACEMENT_3D('',#133158,#85449,#85450);
#74776=AXIS2_PLACEMENT_3D('',#133160,#85451,#85452);
#74777=AXIS2_PLACEMENT_3D('',#133162,#85453,#85454);
#74778=AXIS2_PLACEMENT_3D('',#133213,#85458,#85459);
#74779=AXIS2_PLACEMENT_3D('',#133221,#85461,#85462);
#74780=AXIS2_PLACEMENT_3D('',#133223,#85463,#85464);
#74781=AXIS2_PLACEMENT_3D('',#133225,#85465,#85466);
#74782=AXIS2_PLACEMENT_3D('',#133252,#85468,#85469);
#74783=AXIS2_PLACEMENT_3D('',#133260,#85471,#85472);
#74784=AXIS2_PLACEMENT_3D('',#133262,#85473,#85474);
#74785=AXIS2_PLACEMENT_3D('',#133264,#85475,#85476);
#74786=AXIS2_PLACEMENT_3D('',#133291,#85478,#85479);
#74787=AXIS2_PLACEMENT_3D('',#133299,#85481,#85482);
#74788=AXIS2_PLACEMENT_3D('',#133301,#85483,#85484);
#74789=AXIS2_PLACEMENT_3D('',#133303,#85485,#85486);
#74790=AXIS2_PLACEMENT_3D('',#133330,#85488,#85489);
#74791=AXIS2_PLACEMENT_3D('',#133338,#85491,#85492);
#74792=AXIS2_PLACEMENT_3D('',#133340,#85493,#85494);
#74793=AXIS2_PLACEMENT_3D('',#133342,#85495,#85496);
#74794=AXIS2_PLACEMENT_3D('',#133369,#85498,#85499);
#74795=AXIS2_PLACEMENT_3D('',#133377,#85501,#85502);
#74796=AXIS2_PLACEMENT_3D('',#133379,#85503,#85504);
#74797=AXIS2_PLACEMENT_3D('',#133381,#85505,#85506);
#74798=AXIS2_PLACEMENT_3D('',#133408,#85508,#85509);
#74799=AXIS2_PLACEMENT_3D('',#133435,#85512,#85513);
#74800=AXIS2_PLACEMENT_3D('',#133437,#85514,#85515);
#74801=AXIS2_PLACEMENT_3D('',#133438,#85516,#85517);
#74802=AXIS2_PLACEMENT_3D('',#133448,#85519,#85520);
#74803=AXIS2_PLACEMENT_3D('',#133455,#85521,#85522);
#74804=AXIS2_PLACEMENT_3D('',#133465,#85523,#85524);
#74805=AXIS2_PLACEMENT_3D('',#133466,#85525,#85526);
#74806=AXIS2_PLACEMENT_3D('',#133486,#85528,#85529);
#74807=AXIS2_PLACEMENT_3D('',#133494,#85531,#85532);
#74808=AXIS2_PLACEMENT_3D('',#133496,#85533,#85534);
#74809=AXIS2_PLACEMENT_3D('',#133498,#85535,#85536);
#74810=AXIS2_PLACEMENT_3D('',#133525,#85538,#85539);
#74811=AXIS2_PLACEMENT_3D('',#133533,#85541,#85542);
#74812=AXIS2_PLACEMENT_3D('',#133535,#85543,#85544);
#74813=AXIS2_PLACEMENT_3D('',#133537,#85545,#85546);
#74814=AXIS2_PLACEMENT_3D('',#133564,#85548,#85549);
#74815=AXIS2_PLACEMENT_3D('',#133572,#85551,#85552);
#74816=AXIS2_PLACEMENT_3D('',#133574,#85553,#85554);
#74817=AXIS2_PLACEMENT_3D('',#133576,#85555,#85556);
#74818=AXIS2_PLACEMENT_3D('',#133603,#85558,#85559);
#74819=AXIS2_PLACEMENT_3D('',#133611,#85561,#85562);
#74820=AXIS2_PLACEMENT_3D('',#133613,#85563,#85564);
#74821=AXIS2_PLACEMENT_3D('',#133615,#85565,#85566);
#74822=AXIS2_PLACEMENT_3D('',#133642,#85568,#85569);
#74823=AXIS2_PLACEMENT_3D('',#133650,#85571,#85572);
#74824=AXIS2_PLACEMENT_3D('',#133652,#85573,#85574);
#74825=AXIS2_PLACEMENT_3D('',#133654,#85575,#85576);
#74826=AXIS2_PLACEMENT_3D('',#133681,#85578,#85579);
#74827=AXIS2_PLACEMENT_3D('',#133689,#85581,#85582);
#74828=AXIS2_PLACEMENT_3D('',#133691,#85583,#85584);
#74829=AXIS2_PLACEMENT_3D('',#133693,#85585,#85586);
#74830=AXIS2_PLACEMENT_3D('',#133720,#85588,#85589);
#74831=AXIS2_PLACEMENT_3D('',#133728,#85591,#85592);
#74832=AXIS2_PLACEMENT_3D('',#133730,#85593,#85594);
#74833=AXIS2_PLACEMENT_3D('',#133732,#85595,#85596);
#74834=AXIS2_PLACEMENT_3D('',#133760,#85599,#85600);
#74835=AXIS2_PLACEMENT_3D('',#133774,#85601,#85602);
#74836=AXIS2_PLACEMENT_3D('',#133776,#85604,#85605);
#74837=AXIS2_PLACEMENT_3D('',#133778,#85606,#85607);
#74838=AXIS2_PLACEMENT_3D('',#133779,#85608,#85609);
#74839=AXIS2_PLACEMENT_3D('',#133789,#85611,#85612);
#74840=AXIS2_PLACEMENT_3D('',#133803,#85613,#85614);
#74841=AXIS2_PLACEMENT_3D('',#133805,#85616,#85617);
#74842=AXIS2_PLACEMENT_3D('',#133807,#85618,#85619);
#74843=AXIS2_PLACEMENT_3D('',#133808,#85620,#85621);
#74844=AXIS2_PLACEMENT_3D('',#133818,#85623,#85624);
#74845=AXIS2_PLACEMENT_3D('',#133832,#85625,#85626);
#74846=AXIS2_PLACEMENT_3D('',#133834,#85628,#85629);
#74847=AXIS2_PLACEMENT_3D('',#133836,#85630,#85631);
#74848=AXIS2_PLACEMENT_3D('',#133837,#85632,#85633);
#74849=AXIS2_PLACEMENT_3D('',#133847,#85635,#85636);
#74850=AXIS2_PLACEMENT_3D('',#133861,#85637,#85638);
#74851=AXIS2_PLACEMENT_3D('',#133863,#85640,#85641);
#74852=AXIS2_PLACEMENT_3D('',#133865,#85642,#85643);
#74853=AXIS2_PLACEMENT_3D('',#133866,#85644,#85645);
#74854=AXIS2_PLACEMENT_3D('',#133876,#85647,#85648);
#74855=AXIS2_PLACEMENT_3D('',#133890,#85649,#85650);
#74856=AXIS2_PLACEMENT_3D('',#133892,#85652,#85653);
#74857=AXIS2_PLACEMENT_3D('',#133894,#85654,#85655);
#74858=AXIS2_PLACEMENT_3D('',#133895,#85656,#85657);
#74859=AXIS2_PLACEMENT_3D('',#133905,#85659,#85660);
#74860=AXIS2_PLACEMENT_3D('',#133919,#85661,#85662);
#74861=AXIS2_PLACEMENT_3D('',#133921,#85664,#85665);
#74862=AXIS2_PLACEMENT_3D('',#133923,#85666,#85667);
#74863=AXIS2_PLACEMENT_3D('',#133924,#85668,#85669);
#74864=AXIS2_PLACEMENT_3D('',#133934,#85671,#85672);
#74865=AXIS2_PLACEMENT_3D('',#133948,#85673,#85674);
#74866=AXIS2_PLACEMENT_3D('',#133950,#85676,#85677);
#74867=AXIS2_PLACEMENT_3D('',#133952,#85678,#85679);
#74868=AXIS2_PLACEMENT_3D('',#133953,#85680,#85681);
#74869=AXIS2_PLACEMENT_3D('',#133963,#85683,#85684);
#74870=AXIS2_PLACEMENT_3D('',#133977,#85685,#85686);
#74871=AXIS2_PLACEMENT_3D('',#133979,#85688,#85689);
#74872=AXIS2_PLACEMENT_3D('',#133981,#85690,#85691);
#74873=AXIS2_PLACEMENT_3D('',#133982,#85692,#85693);
#74874=AXIS2_PLACEMENT_3D('',#133992,#85695,#85696);
#74875=AXIS2_PLACEMENT_3D('',#134006,#85697,#85698);
#74876=AXIS2_PLACEMENT_3D('',#134008,#85700,#85701);
#74877=AXIS2_PLACEMENT_3D('',#134010,#85702,#85703);
#74878=AXIS2_PLACEMENT_3D('',#134011,#85704,#85705);
#74879=AXIS2_PLACEMENT_3D('',#134021,#85707,#85708);
#74880=AXIS2_PLACEMENT_3D('',#134035,#85709,#85710);
#74881=AXIS2_PLACEMENT_3D('',#134037,#85712,#85713);
#74882=AXIS2_PLACEMENT_3D('',#134039,#85714,#85715);
#74883=AXIS2_PLACEMENT_3D('',#134040,#85716,#85717);
#74884=AXIS2_PLACEMENT_3D('',#134050,#85719,#85720);
#74885=AXIS2_PLACEMENT_3D('',#134064,#85721,#85722);
#74886=AXIS2_PLACEMENT_3D('',#134066,#85724,#85725);
#74887=AXIS2_PLACEMENT_3D('',#134068,#85726,#85727);
#74888=AXIS2_PLACEMENT_3D('',#134069,#85728,#85729);
#74889=AXIS2_PLACEMENT_3D('',#134079,#85731,#85732);
#74890=AXIS2_PLACEMENT_3D('',#134093,#85733,#85734);
#74891=AXIS2_PLACEMENT_3D('',#134095,#85736,#85737);
#74892=AXIS2_PLACEMENT_3D('',#134097,#85738,#85739);
#74893=AXIS2_PLACEMENT_3D('',#134098,#85740,#85741);
#74894=AXIS2_PLACEMENT_3D('',#134108,#85743,#85744);
#74895=AXIS2_PLACEMENT_3D('',#134122,#85745,#85746);
#74896=AXIS2_PLACEMENT_3D('',#134124,#85748,#85749);
#74897=AXIS2_PLACEMENT_3D('',#134126,#85750,#85751);
#74898=AXIS2_PLACEMENT_3D('',#134127,#85752,#85753);
#74899=AXIS2_PLACEMENT_3D('',#134137,#85755,#85756);
#74900=AXIS2_PLACEMENT_3D('',#134151,#85757,#85758);
#74901=AXIS2_PLACEMENT_3D('',#134153,#85760,#85761);
#74902=AXIS2_PLACEMENT_3D('',#134155,#85762,#85763);
#74903=AXIS2_PLACEMENT_3D('',#134156,#85764,#85765);
#74904=AXIS2_PLACEMENT_3D('',#134166,#85767,#85768);
#74905=AXIS2_PLACEMENT_3D('',#134180,#85769,#85770);
#74906=AXIS2_PLACEMENT_3D('',#134182,#85772,#85773);
#74907=AXIS2_PLACEMENT_3D('',#134184,#85774,#85775);
#74908=AXIS2_PLACEMENT_3D('',#134185,#85776,#85777);
#74909=AXIS2_PLACEMENT_3D('',#134195,#85779,#85780);
#74910=AXIS2_PLACEMENT_3D('',#134209,#85781,#85782);
#74911=AXIS2_PLACEMENT_3D('',#134211,#85784,#85785);
#74912=AXIS2_PLACEMENT_3D('',#134213,#85786,#85787);
#74913=AXIS2_PLACEMENT_3D('',#134214,#85788,#85789);
#74914=AXIS2_PLACEMENT_3D('',#134224,#85791,#85792);
#74915=AXIS2_PLACEMENT_3D('',#134238,#85793,#85794);
#74916=AXIS2_PLACEMENT_3D('',#134240,#85796,#85797);
#74917=AXIS2_PLACEMENT_3D('',#134242,#85798,#85799);
#74918=AXIS2_PLACEMENT_3D('',#134243,#85800,#85801);
#74919=AXIS2_PLACEMENT_3D('',#134253,#85803,#85804);
#74920=AXIS2_PLACEMENT_3D('',#134267,#85805,#85806);
#74921=AXIS2_PLACEMENT_3D('',#134269,#85808,#85809);
#74922=AXIS2_PLACEMENT_3D('',#134271,#85810,#85811);
#74923=AXIS2_PLACEMENT_3D('',#134272,#85812,#85813);
#74924=AXIS2_PLACEMENT_3D('',#134282,#85815,#85816);
#74925=AXIS2_PLACEMENT_3D('',#134296,#85817,#85818);
#74926=AXIS2_PLACEMENT_3D('',#134298,#85820,#85821);
#74927=AXIS2_PLACEMENT_3D('',#134300,#85822,#85823);
#74928=AXIS2_PLACEMENT_3D('',#134301,#85824,#85825);
#74929=AXIS2_PLACEMENT_3D('',#134311,#85827,#85828);
#74930=AXIS2_PLACEMENT_3D('',#134325,#85829,#85830);
#74931=AXIS2_PLACEMENT_3D('',#134327,#85832,#85833);
#74932=AXIS2_PLACEMENT_3D('',#134329,#85834,#85835);
#74933=AXIS2_PLACEMENT_3D('',#134330,#85836,#85837);
#74934=AXIS2_PLACEMENT_3D('',#134340,#85839,#85840);
#74935=AXIS2_PLACEMENT_3D('',#134354,#85841,#85842);
#74936=AXIS2_PLACEMENT_3D('',#134356,#85844,#85845);
#74937=AXIS2_PLACEMENT_3D('',#134358,#85846,#85847);
#74938=AXIS2_PLACEMENT_3D('',#134359,#85848,#85849);
#74939=AXIS2_PLACEMENT_3D('',#134369,#85851,#85852);
#74940=AXIS2_PLACEMENT_3D('',#134383,#85853,#85854);
#74941=AXIS2_PLACEMENT_3D('',#134385,#85856,#85857);
#74942=AXIS2_PLACEMENT_3D('',#134387,#85858,#85859);
#74943=AXIS2_PLACEMENT_3D('',#134388,#85860,#85861);
#74944=AXIS2_PLACEMENT_3D('',#134398,#85863,#85864);
#74945=AXIS2_PLACEMENT_3D('',#134412,#85865,#85866);
#74946=AXIS2_PLACEMENT_3D('',#134414,#85868,#85869);
#74947=AXIS2_PLACEMENT_3D('',#134416,#85870,#85871);
#74948=AXIS2_PLACEMENT_3D('',#134417,#85872,#85873);
#74949=AXIS2_PLACEMENT_3D('',#134427,#85875,#85876);
#74950=AXIS2_PLACEMENT_3D('',#134441,#85877,#85878);
#74951=AXIS2_PLACEMENT_3D('',#134443,#85880,#85881);
#74952=AXIS2_PLACEMENT_3D('',#134445,#85882,#85883);
#74953=AXIS2_PLACEMENT_3D('',#134446,#85884,#85885);
#74954=AXIS2_PLACEMENT_3D('',#134456,#85887,#85888);
#74955=AXIS2_PLACEMENT_3D('',#134470,#85889,#85890);
#74956=AXIS2_PLACEMENT_3D('',#134472,#85892,#85893);
#74957=AXIS2_PLACEMENT_3D('',#134474,#85894,#85895);
#74958=AXIS2_PLACEMENT_3D('',#134475,#85896,#85897);
#74959=AXIS2_PLACEMENT_3D('',#134485,#85899,#85900);
#74960=AXIS2_PLACEMENT_3D('',#134499,#85901,#85902);
#74961=AXIS2_PLACEMENT_3D('',#134501,#85904,#85905);
#74962=AXIS2_PLACEMENT_3D('',#134503,#85906,#85907);
#74963=AXIS2_PLACEMENT_3D('',#134504,#85908,#85909);
#74964=AXIS2_PLACEMENT_3D('',#134514,#85911,#85912);
#74965=AXIS2_PLACEMENT_3D('',#134528,#85913,#85914);
#74966=AXIS2_PLACEMENT_3D('',#134530,#85916,#85917);
#74967=AXIS2_PLACEMENT_3D('',#134532,#85918,#85919);
#74968=AXIS2_PLACEMENT_3D('',#134533,#85920,#85921);
#74969=AXIS2_PLACEMENT_3D('',#134543,#85923,#85924);
#74970=AXIS2_PLACEMENT_3D('',#134557,#85925,#85926);
#74971=AXIS2_PLACEMENT_3D('',#134559,#85928,#85929);
#74972=AXIS2_PLACEMENT_3D('',#134561,#85930,#85931);
#74973=AXIS2_PLACEMENT_3D('',#134562,#85932,#85933);
#74974=AXIS2_PLACEMENT_3D('',#134572,#85935,#85936);
#74975=AXIS2_PLACEMENT_3D('',#134586,#85937,#85938);
#74976=AXIS2_PLACEMENT_3D('',#134588,#85940,#85941);
#74977=AXIS2_PLACEMENT_3D('',#134590,#85942,#85943);
#74978=AXIS2_PLACEMENT_3D('',#134591,#85944,#85945);
#74979=AXIS2_PLACEMENT_3D('',#134603,#85946,#85947);
#74980=AXIS2_PLACEMENT_3D('',#134649,#85948,#85949);
#74981=AXIS2_PLACEMENT_3D('',#134695,#85950,#85951);
#74982=AXIS2_PLACEMENT_3D('',#134741,#85952,#85953);
#74983=AXIS2_PLACEMENT_3D('',#134787,#85954,#85955);
#74984=AXIS2_PLACEMENT_3D('',#134833,#85956,#85957);
#74985=AXIS2_PLACEMENT_3D('',#134883,#85958,#85959);
#74986=AXIS2_PLACEMENT_3D('',#134929,#85960,#85961);
#74987=AXIS2_PLACEMENT_3D('',#134975,#85962,#85963);
#74988=AXIS2_PLACEMENT_3D('',#135021,#85964,#85965);
#74989=AXIS2_PLACEMENT_3D('',#135067,#85966,#85967);
#74990=AXIS2_PLACEMENT_3D('',#135113,#85968,#85969);
#74991=AXIS2_PLACEMENT_3D('',#135159,#85970,#85971);
#74992=AXIS2_PLACEMENT_3D('',#135209,#85972,#85973);
#74993=AXIS2_PLACEMENT_3D('',#135259,#85974,#85975);
#74994=AXIS2_PLACEMENT_3D('',#135309,#85976,#85977);
#74995=AXIS2_PLACEMENT_3D('',#135355,#85978,#85979);
#74996=AXIS2_PLACEMENT_3D('',#135401,#85980,#85981);
#74997=AXIS2_PLACEMENT_3D('',#135447,#85982,#85983);
#74998=AXIS2_PLACEMENT_3D('',#135493,#85984,#85985);
#74999=AXIS2_PLACEMENT_3D('',#135539,#85986,#85987);
#75000=AXIS2_PLACEMENT_3D('',#135585,#85988,#85989);
#75001=AXIS2_PLACEMENT_3D('',#135631,#85990,#85991);
#75002=AXIS2_PLACEMENT_3D('',#135677,#85992,#85993);
#75003=AXIS2_PLACEMENT_3D('',#135723,#85994,#85995);
#75004=AXIS2_PLACEMENT_3D('',#135769,#85996,#85997);
#75005=AXIS2_PLACEMENT_3D('',#135815,#85998,#85999);
#75006=AXIS2_PLACEMENT_3D('',#135861,#86000,#86001);
#75007=AXIS2_PLACEMENT_3D('',#135907,#86002,#86003);
#75008=AXIS2_PLACEMENT_3D('',#135957,#86004,#86005);
#75009=AXIS2_PLACEMENT_3D('',#136007,#86006,#86007);
#75010=AXIS2_PLACEMENT_3D('',#136053,#86008,#86009);
#75011=AXIS2_PLACEMENT_3D('',#136103,#86010,#86011);
#75012=AXIS2_PLACEMENT_3D('',#136152,#86012,#86013);
#75013=AXIS2_PLACEMENT_3D('',#136202,#86014,#86015);
#75014=AXIS2_PLACEMENT_3D('',#136248,#86016,#86017);
#75015=AXIS2_PLACEMENT_3D('',#136298,#86018,#86019);
#75016=AXIS2_PLACEMENT_3D('',#136344,#86020,#86021);
#75017=AXIS2_PLACEMENT_3D('',#136390,#86022,#86023);
#75018=AXIS2_PLACEMENT_3D('',#136440,#86024,#86025);
#75019=AXIS2_PLACEMENT_3D('',#136481,#86026,#86027);
#75020=AXIS2_PLACEMENT_3D('',#136522,#86028,#86029);
#75021=AXIS2_PLACEMENT_3D('',#136568,#86030,#86031);
#75022=AXIS2_PLACEMENT_3D('',#136618,#86032,#86033);
#75023=AXIS2_PLACEMENT_3D('',#136664,#86034,#86035);
#75024=AXIS2_PLACEMENT_3D('',#136708,#86036,#86037);
#75025=AXIS2_PLACEMENT_3D('',#136758,#86038,#86039);
#75026=AXIS2_PLACEMENT_3D('',#136799,#86040,#86041);
#75027=AXIS2_PLACEMENT_3D('',#136849,#86042,#86043);
#75028=AXIS2_PLACEMENT_3D('',#136898,#86044,#86045);
#75029=AXIS2_PLACEMENT_3D('',#136947,#86046,#86047);
#75030=AXIS2_PLACEMENT_3D('',#136997,#86048,#86049);
#75031=AXIS2_PLACEMENT_3D('',#137047,#86050,#86051);
#75032=AXIS2_PLACEMENT_3D('',#137088,#86052,#86053);
#75033=AXIS2_PLACEMENT_3D('',#137129,#86054,#86055);
#75034=AXIS2_PLACEMENT_3D('',#137179,#86056,#86057);
#75035=AXIS2_PLACEMENT_3D('',#137220,#86058,#86059);
#75036=AXIS2_PLACEMENT_3D('',#137266,#86060,#86061);
#75037=AXIS2_PLACEMENT_3D('',#137320,#86062,#86063);
#75038=AXIS2_PLACEMENT_3D('',#137354,#86066,#86067);
#75039=AXIS2_PLACEMENT_3D('',#137356,#86068,#86069);
#75040=AXIS2_PLACEMENT_3D('',#137358,#86070,#86071);
#75041=AXIS2_PLACEMENT_3D('',#137359,#86072,#86073);
#75042=AXIS2_PLACEMENT_3D('',#137397,#86076,#86077);
#75043=AXIS2_PLACEMENT_3D('',#137399,#86078,#86079);
#75044=AXIS2_PLACEMENT_3D('',#137401,#86080,#86081);
#75045=AXIS2_PLACEMENT_3D('',#137402,#86082,#86083);
#75046=AXIS2_PLACEMENT_3D('',#137440,#86086,#86087);
#75047=AXIS2_PLACEMENT_3D('',#137442,#86088,#86089);
#75048=AXIS2_PLACEMENT_3D('',#137444,#86090,#86091);
#75049=AXIS2_PLACEMENT_3D('',#137445,#86092,#86093);
#75050=AXIS2_PLACEMENT_3D('',#137483,#86096,#86097);
#75051=AXIS2_PLACEMENT_3D('',#137485,#86098,#86099);
#75052=AXIS2_PLACEMENT_3D('',#137487,#86100,#86101);
#75053=AXIS2_PLACEMENT_3D('',#137488,#86102,#86103);
#75054=AXIS2_PLACEMENT_3D('',#137526,#86106,#86107);
#75055=AXIS2_PLACEMENT_3D('',#137528,#86108,#86109);
#75056=AXIS2_PLACEMENT_3D('',#137530,#86110,#86111);
#75057=AXIS2_PLACEMENT_3D('',#137531,#86112,#86113);
#75058=AXIS2_PLACEMENT_3D('',#137569,#86116,#86117);
#75059=AXIS2_PLACEMENT_3D('',#137571,#86118,#86119);
#75060=AXIS2_PLACEMENT_3D('',#137573,#86120,#86121);
#75061=AXIS2_PLACEMENT_3D('',#137574,#86122,#86123);
#75062=AXIS2_PLACEMENT_3D('',#137640,#86128,#86129);
#75063=AXIS2_PLACEMENT_3D('',#137642,#86130,#86131);
#75064=AXIS2_PLACEMENT_3D('',#137644,#86132,#86133);
#75065=AXIS2_PLACEMENT_3D('',#137645,#86134,#86135);
#75066=AXIS2_PLACEMENT_3D('',#137683,#86138,#86139);
#75067=AXIS2_PLACEMENT_3D('',#137685,#86140,#86141);
#75068=AXIS2_PLACEMENT_3D('',#137687,#86142,#86143);
#75069=AXIS2_PLACEMENT_3D('',#137688,#86144,#86145);
#75070=AXIS2_PLACEMENT_3D('',#137726,#86148,#86149);
#75071=AXIS2_PLACEMENT_3D('',#137728,#86150,#86151);
#75072=AXIS2_PLACEMENT_3D('',#137730,#86152,#86153);
#75073=AXIS2_PLACEMENT_3D('',#137731,#86154,#86155);
#75074=AXIS2_PLACEMENT_3D('',#137769,#86158,#86159);
#75075=AXIS2_PLACEMENT_3D('',#137771,#86160,#86161);
#75076=AXIS2_PLACEMENT_3D('',#137773,#86162,#86163);
#75077=AXIS2_PLACEMENT_3D('',#137774,#86164,#86165);
#75078=AXIS2_PLACEMENT_3D('',#137812,#86168,#86169);
#75079=AXIS2_PLACEMENT_3D('',#137814,#86170,#86171);
#75080=AXIS2_PLACEMENT_3D('',#137816,#86172,#86173);
#75081=AXIS2_PLACEMENT_3D('',#137817,#86174,#86175);
#75082=AXIS2_PLACEMENT_3D('',#137855,#86178,#86179);
#75083=AXIS2_PLACEMENT_3D('',#137857,#86180,#86181);
#75084=AXIS2_PLACEMENT_3D('',#137859,#86182,#86183);
#75085=AXIS2_PLACEMENT_3D('',#137860,#86184,#86185);
#75086=AXIS2_PLACEMENT_3D('',#137898,#86188,#86189);
#75087=AXIS2_PLACEMENT_3D('',#137900,#86190,#86191);
#75088=AXIS2_PLACEMENT_3D('',#137902,#86192,#86193);
#75089=AXIS2_PLACEMENT_3D('',#137903,#86194,#86195);
#75090=AXIS2_PLACEMENT_3D('',#137941,#86198,#86199);
#75091=AXIS2_PLACEMENT_3D('',#137943,#86200,#86201);
#75092=AXIS2_PLACEMENT_3D('',#137945,#86202,#86203);
#75093=AXIS2_PLACEMENT_3D('',#137946,#86204,#86205);
#75094=AXIS2_PLACEMENT_3D('',#137984,#86208,#86209);
#75095=AXIS2_PLACEMENT_3D('',#137986,#86210,#86211);
#75096=AXIS2_PLACEMENT_3D('',#137988,#86212,#86213);
#75097=AXIS2_PLACEMENT_3D('',#137989,#86214,#86215);
#75098=AXIS2_PLACEMENT_3D('',#138027,#86218,#86219);
#75099=AXIS2_PLACEMENT_3D('',#138029,#86220,#86221);
#75100=AXIS2_PLACEMENT_3D('',#138031,#86222,#86223);
#75101=AXIS2_PLACEMENT_3D('',#138032,#86224,#86225);
#75102=AXIS2_PLACEMENT_3D('',#138070,#86228,#86229);
#75103=AXIS2_PLACEMENT_3D('',#138072,#86230,#86231);
#75104=AXIS2_PLACEMENT_3D('',#138074,#86232,#86233);
#75105=AXIS2_PLACEMENT_3D('',#138075,#86234,#86235);
#75106=AXIS2_PLACEMENT_3D('',#138113,#86238,#86239);
#75107=AXIS2_PLACEMENT_3D('',#138115,#86240,#86241);
#75108=AXIS2_PLACEMENT_3D('',#138117,#86242,#86243);
#75109=AXIS2_PLACEMENT_3D('',#138118,#86244,#86245);
#75110=AXIS2_PLACEMENT_3D('',#138167,#86248,#86249);
#75111=AXIS2_PLACEMENT_3D('',#138169,#86251,#86252);
#75112=AXIS2_PLACEMENT_3D('',#138171,#86253,#86254);
#75113=AXIS2_PLACEMENT_3D('',#138172,#86255,#86256);
#75114=AXIS2_PLACEMENT_3D('',#138199,#86258,#86259);
#75115=AXIS2_PLACEMENT_3D('',#138201,#86260,#86261);
#75116=AXIS2_PLACEMENT_3D('',#138203,#86262,#86263);
#75117=AXIS2_PLACEMENT_3D('',#138204,#86264,#86265);
#75118=AXIS2_PLACEMENT_3D('',#138242,#86268,#86269);
#75119=AXIS2_PLACEMENT_3D('',#138244,#86270,#86271);
#75120=AXIS2_PLACEMENT_3D('',#138246,#86272,#86273);
#75121=AXIS2_PLACEMENT_3D('',#138247,#86274,#86275);
#75122=AXIS2_PLACEMENT_3D('',#138285,#86278,#86279);
#75123=AXIS2_PLACEMENT_3D('',#138287,#86280,#86281);
#75124=AXIS2_PLACEMENT_3D('',#138289,#86282,#86283);
#75125=AXIS2_PLACEMENT_3D('',#138290,#86284,#86285);
#75126=AXIS2_PLACEMENT_3D('',#138328,#86288,#86289);
#75127=AXIS2_PLACEMENT_3D('',#138330,#86290,#86291);
#75128=AXIS2_PLACEMENT_3D('',#138332,#86292,#86293);
#75129=AXIS2_PLACEMENT_3D('',#138333,#86294,#86295);
#75130=AXIS2_PLACEMENT_3D('',#138371,#86298,#86299);
#75131=AXIS2_PLACEMENT_3D('',#138373,#86300,#86301);
#75132=AXIS2_PLACEMENT_3D('',#138375,#86302,#86303);
#75133=AXIS2_PLACEMENT_3D('',#138376,#86304,#86305);
#75134=AXIS2_PLACEMENT_3D('',#138414,#86308,#86309);
#75135=AXIS2_PLACEMENT_3D('',#138416,#86310,#86311);
#75136=AXIS2_PLACEMENT_3D('',#138418,#86312,#86313);
#75137=AXIS2_PLACEMENT_3D('',#138419,#86314,#86315);
#75138=AXIS2_PLACEMENT_3D('',#138457,#86318,#86319);
#75139=AXIS2_PLACEMENT_3D('',#138459,#86320,#86321);
#75140=AXIS2_PLACEMENT_3D('',#138461,#86322,#86323);
#75141=AXIS2_PLACEMENT_3D('',#138462,#86324,#86325);
#75142=AXIS2_PLACEMENT_3D('',#138500,#86328,#86329);
#75143=AXIS2_PLACEMENT_3D('',#138502,#86330,#86331);
#75144=AXIS2_PLACEMENT_3D('',#138504,#86332,#86333);
#75145=AXIS2_PLACEMENT_3D('',#138505,#86334,#86335);
#75146=AXIS2_PLACEMENT_3D('',#138517,#86337,#86338);
#75147=AXIS2_PLACEMENT_3D('',#138520,#86339,#86340);
#75148=AXIS2_PLACEMENT_3D('',#138521,#86341,#86342);
#75149=AXIS2_PLACEMENT_3D('',#138558,#86344,#86345);
#75150=AXIS2_PLACEMENT_3D('',#138597,#86348,#86349);
#75151=AXIS2_PLACEMENT_3D('',#138599,#86351,#86352);
#75152=AXIS2_PLACEMENT_3D('',#138601,#86353,#86354);
#75153=AXIS2_PLACEMENT_3D('',#138602,#86355,#86356);
#75154=AXIS2_PLACEMENT_3D('',#138640,#86358,#86359);
#75155=AXIS2_PLACEMENT_3D('',#138642,#86361,#86362);
#75156=AXIS2_PLACEMENT_3D('',#138644,#86363,#86364);
#75157=AXIS2_PLACEMENT_3D('',#138645,#86365,#86366);
#75158=AXIS2_PLACEMENT_3D('',#138683,#86368,#86369);
#75159=AXIS2_PLACEMENT_3D('',#138685,#86371,#86372);
#75160=AXIS2_PLACEMENT_3D('',#138687,#86373,#86374);
#75161=AXIS2_PLACEMENT_3D('',#138688,#86375,#86376);
#75162=AXIS2_PLACEMENT_3D('',#138726,#86378,#86379);
#75163=AXIS2_PLACEMENT_3D('',#138728,#86381,#86382);
#75164=AXIS2_PLACEMENT_3D('',#138730,#86383,#86384);
#75165=AXIS2_PLACEMENT_3D('',#138731,#86385,#86386);
#75166=AXIS2_PLACEMENT_3D('',#138769,#86388,#86389);
#75167=AXIS2_PLACEMENT_3D('',#138771,#86391,#86392);
#75168=AXIS2_PLACEMENT_3D('',#138773,#86393,#86394);
#75169=AXIS2_PLACEMENT_3D('',#138774,#86395,#86396);
#75170=AXIS2_PLACEMENT_3D('',#138812,#86398,#86399);
#75171=AXIS2_PLACEMENT_3D('',#138814,#86401,#86402);
#75172=AXIS2_PLACEMENT_3D('',#138816,#86403,#86404);
#75173=AXIS2_PLACEMENT_3D('',#138817,#86405,#86406);
#75174=AXIS2_PLACEMENT_3D('',#138855,#86408,#86409);
#75175=AXIS2_PLACEMENT_3D('',#138857,#86411,#86412);
#75176=AXIS2_PLACEMENT_3D('',#138859,#86413,#86414);
#75177=AXIS2_PLACEMENT_3D('',#138860,#86415,#86416);
#75178=AXIS2_PLACEMENT_3D('',#138898,#86418,#86419);
#75179=AXIS2_PLACEMENT_3D('',#138900,#86421,#86422);
#75180=AXIS2_PLACEMENT_3D('',#138902,#86423,#86424);
#75181=AXIS2_PLACEMENT_3D('',#138903,#86425,#86426);
#75182=AXIS2_PLACEMENT_3D('',#138941,#86428,#86429);
#75183=AXIS2_PLACEMENT_3D('',#138943,#86431,#86432);
#75184=AXIS2_PLACEMENT_3D('',#138945,#86433,#86434);
#75185=AXIS2_PLACEMENT_3D('',#138946,#86435,#86436);
#75186=AXIS2_PLACEMENT_3D('',#138984,#86438,#86439);
#75187=AXIS2_PLACEMENT_3D('',#138986,#86441,#86442);
#75188=AXIS2_PLACEMENT_3D('',#138988,#86443,#86444);
#75189=AXIS2_PLACEMENT_3D('',#138989,#86445,#86446);
#75190=AXIS2_PLACEMENT_3D('',#139027,#86448,#86449);
#75191=AXIS2_PLACEMENT_3D('',#139029,#86451,#86452);
#75192=AXIS2_PLACEMENT_3D('',#139031,#86453,#86454);
#75193=AXIS2_PLACEMENT_3D('',#139032,#86455,#86456);
#75194=AXIS2_PLACEMENT_3D('',#139070,#86458,#86459);
#75195=AXIS2_PLACEMENT_3D('',#139072,#86461,#86462);
#75196=AXIS2_PLACEMENT_3D('',#139074,#86463,#86464);
#75197=AXIS2_PLACEMENT_3D('',#139075,#86465,#86466);
#75198=AXIS2_PLACEMENT_3D('',#139113,#86468,#86469);
#75199=AXIS2_PLACEMENT_3D('',#139115,#86471,#86472);
#75200=AXIS2_PLACEMENT_3D('',#139117,#86473,#86474);
#75201=AXIS2_PLACEMENT_3D('',#139118,#86475,#86476);
#75202=AXIS2_PLACEMENT_3D('',#139184,#86480,#86481);
#75203=AXIS2_PLACEMENT_3D('',#139186,#86483,#86484);
#75204=AXIS2_PLACEMENT_3D('',#139188,#86485,#86486);
#75205=AXIS2_PLACEMENT_3D('',#139189,#86487,#86488);
#75206=AXIS2_PLACEMENT_3D('',#139227,#86490,#86491);
#75207=AXIS2_PLACEMENT_3D('',#139229,#86493,#86494);
#75208=AXIS2_PLACEMENT_3D('',#139231,#86495,#86496);
#75209=AXIS2_PLACEMENT_3D('',#139232,#86497,#86498);
#75210=AXIS2_PLACEMENT_3D('',#139270,#86500,#86501);
#75211=AXIS2_PLACEMENT_3D('',#139272,#86503,#86504);
#75212=AXIS2_PLACEMENT_3D('',#139274,#86505,#86506);
#75213=AXIS2_PLACEMENT_3D('',#139275,#86507,#86508);
#75214=AXIS2_PLACEMENT_3D('',#139313,#86510,#86511);
#75215=AXIS2_PLACEMENT_3D('',#139315,#86513,#86514);
#75216=AXIS2_PLACEMENT_3D('',#139317,#86515,#86516);
#75217=AXIS2_PLACEMENT_3D('',#139318,#86517,#86518);
#75218=AXIS2_PLACEMENT_3D('',#139356,#86520,#86521);
#75219=AXIS2_PLACEMENT_3D('',#139358,#86523,#86524);
#75220=AXIS2_PLACEMENT_3D('',#139360,#86525,#86526);
#75221=AXIS2_PLACEMENT_3D('',#139361,#86527,#86528);
#75222=AXIS2_PLACEMENT_3D('',#139399,#86530,#86531);
#75223=AXIS2_PLACEMENT_3D('',#139401,#86533,#86534);
#75224=AXIS2_PLACEMENT_3D('',#139403,#86535,#86536);
#75225=AXIS2_PLACEMENT_3D('',#139404,#86537,#86538);
#75226=AXIS2_PLACEMENT_3D('',#139442,#86540,#86541);
#75227=AXIS2_PLACEMENT_3D('',#139444,#86543,#86544);
#75228=AXIS2_PLACEMENT_3D('',#139446,#86545,#86546);
#75229=AXIS2_PLACEMENT_3D('',#139447,#86547,#86548);
#75230=AXIS2_PLACEMENT_3D('',#139485,#86550,#86551);
#75231=AXIS2_PLACEMENT_3D('',#139487,#86553,#86554);
#75232=AXIS2_PLACEMENT_3D('',#139489,#86555,#86556);
#75233=AXIS2_PLACEMENT_3D('',#139490,#86557,#86558);
#75234=AXIS2_PLACEMENT_3D('',#139528,#86560,#86561);
#75235=AXIS2_PLACEMENT_3D('',#139530,#86563,#86564);
#75236=AXIS2_PLACEMENT_3D('',#139532,#86565,#86566);
#75237=AXIS2_PLACEMENT_3D('',#139533,#86567,#86568);
#75238=AXIS2_PLACEMENT_3D('',#139571,#86570,#86571);
#75239=AXIS2_PLACEMENT_3D('',#139573,#86573,#86574);
#75240=AXIS2_PLACEMENT_3D('',#139575,#86575,#86576);
#75241=AXIS2_PLACEMENT_3D('',#139576,#86577,#86578);
#75242=AXIS2_PLACEMENT_3D('',#139614,#86580,#86581);
#75243=AXIS2_PLACEMENT_3D('',#139616,#86583,#86584);
#75244=AXIS2_PLACEMENT_3D('',#139618,#86585,#86586);
#75245=AXIS2_PLACEMENT_3D('',#139619,#86587,#86588);
#75246=AXIS2_PLACEMENT_3D('',#139657,#86590,#86591);
#75247=AXIS2_PLACEMENT_3D('',#139659,#86593,#86594);
#75248=AXIS2_PLACEMENT_3D('',#139661,#86595,#86596);
#75249=AXIS2_PLACEMENT_3D('',#139662,#86597,#86598);
#75250=AXIS2_PLACEMENT_3D('',#139700,#86600,#86601);
#75251=AXIS2_PLACEMENT_3D('',#139702,#86603,#86604);
#75252=AXIS2_PLACEMENT_3D('',#139704,#86605,#86606);
#75253=AXIS2_PLACEMENT_3D('',#139705,#86607,#86608);
#75254=AXIS2_PLACEMENT_3D('',#139743,#86610,#86611);
#75255=AXIS2_PLACEMENT_3D('',#139745,#86613,#86614);
#75256=AXIS2_PLACEMENT_3D('',#139747,#86615,#86616);
#75257=AXIS2_PLACEMENT_3D('',#139748,#86617,#86618);
#75258=AXIS2_PLACEMENT_3D('',#139749,#86619,#86620);
#75259=AXIS2_PLACEMENT_3D('',#139759,#86621,#86622);
#75260=AXIS2_PLACEMENT_3D('',#139760,#86623,#86624);
#75261=AXIS2_PLACEMENT_3D('',#139783,#86626,#86627);
#75262=AXIS2_PLACEMENT_3D('',#139797,#86628,#86629);
#75263=AXIS2_PLACEMENT_3D('',#139814,#86630,#86631);
#75264=AXIS2_PLACEMENT_3D('',#139822,#86632,#86633);
#75265=AXIS2_PLACEMENT_3D('',#139839,#86634,#86635);
#75266=AXIS2_PLACEMENT_3D('',#139847,#86636,#86637);
#75267=AXIS2_PLACEMENT_3D('',#139864,#86638,#86639);
#75268=AXIS2_PLACEMENT_3D('',#139872,#86640,#86641);
#75269=AXIS2_PLACEMENT_3D('',#139889,#86642,#86643);
#75270=AXIS2_PLACEMENT_3D('',#139897,#86644,#86645);
#75271=AXIS2_PLACEMENT_3D('',#139914,#86646,#86647);
#75272=AXIS2_PLACEMENT_3D('',#139922,#86648,#86649);
#75273=AXIS2_PLACEMENT_3D('',#139939,#86650,#86651);
#75274=AXIS2_PLACEMENT_3D('',#139947,#86652,#86653);
#75275=AXIS2_PLACEMENT_3D('',#139964,#86654,#86655);
#75276=AXIS2_PLACEMENT_3D('',#139972,#86656,#86657);
#75277=AXIS2_PLACEMENT_3D('',#139989,#86658,#86659);
#75278=AXIS2_PLACEMENT_3D('',#139997,#86660,#86661);
#75279=AXIS2_PLACEMENT_3D('',#140014,#86662,#86663);
#75280=AXIS2_PLACEMENT_3D('',#140022,#86664,#86665);
#75281=AXIS2_PLACEMENT_3D('',#140039,#86666,#86667);
#75282=AXIS2_PLACEMENT_3D('',#140047,#86668,#86669);
#75283=AXIS2_PLACEMENT_3D('',#140064,#86670,#86671);
#75284=AXIS2_PLACEMENT_3D('',#140072,#86672,#86673);
#75285=AXIS2_PLACEMENT_3D('',#140089,#86674,#86675);
#75286=AXIS2_PLACEMENT_3D('',#140097,#86676,#86677);
#75287=AXIS2_PLACEMENT_3D('',#140114,#86678,#86679);
#75288=AXIS2_PLACEMENT_3D('',#140122,#86680,#86681);
#75289=AXIS2_PLACEMENT_3D('',#140139,#86682,#86683);
#75290=AXIS2_PLACEMENT_3D('',#140147,#86684,#86685);
#75291=AXIS2_PLACEMENT_3D('',#140164,#86686,#86687);
#75292=AXIS2_PLACEMENT_3D('',#140172,#86688,#86689);
#75293=AXIS2_PLACEMENT_3D('',#140189,#86690,#86691);
#75294=AXIS2_PLACEMENT_3D('',#140197,#86692,#86693);
#75295=AXIS2_PLACEMENT_3D('',#140214,#86694,#86695);
#75296=AXIS2_PLACEMENT_3D('',#140222,#86696,#86697);
#75297=AXIS2_PLACEMENT_3D('',#140239,#86698,#86699);
#75298=AXIS2_PLACEMENT_3D('',#140247,#86700,#86701);
#75299=AXIS2_PLACEMENT_3D('',#140264,#86702,#86703);
#75300=AXIS2_PLACEMENT_3D('',#140272,#86704,#86705);
#75301=AXIS2_PLACEMENT_3D('',#140289,#86706,#86707);
#75302=AXIS2_PLACEMENT_3D('',#140297,#86708,#86709);
#75303=AXIS2_PLACEMENT_3D('',#140314,#86710,#86711);
#75304=AXIS2_PLACEMENT_3D('',#140322,#86712,#86713);
#75305=AXIS2_PLACEMENT_3D('',#140339,#86714,#86715);
#75306=AXIS2_PLACEMENT_3D('',#140347,#86716,#86717);
#75307=AXIS2_PLACEMENT_3D('',#140364,#86718,#86719);
#75308=AXIS2_PLACEMENT_3D('',#140372,#86720,#86721);
#75309=AXIS2_PLACEMENT_3D('',#140389,#86722,#86723);
#75310=AXIS2_PLACEMENT_3D('',#140397,#86724,#86725);
#75311=AXIS2_PLACEMENT_3D('',#140414,#86726,#86727);
#75312=AXIS2_PLACEMENT_3D('',#140422,#86728,#86729);
#75313=AXIS2_PLACEMENT_3D('',#140439,#86730,#86731);
#75314=AXIS2_PLACEMENT_3D('',#140447,#86732,#86733);
#75315=AXIS2_PLACEMENT_3D('',#140464,#86734,#86735);
#75316=AXIS2_PLACEMENT_3D('',#140472,#86736,#86737);
#75317=AXIS2_PLACEMENT_3D('',#140489,#86738,#86739);
#75318=AXIS2_PLACEMENT_3D('',#140496,#86740,#86741);
#75319=AXIS2_PLACEMENT_3D('',#140514,#86742,#86743);
#75320=AXIS2_PLACEMENT_3D('',#140526,#86744,#86745);
#75321=AXIS2_PLACEMENT_3D('',#140543,#86746,#86747);
#75322=AXIS2_PLACEMENT_3D('',#140555,#86748,#86749);
#75323=AXIS2_PLACEMENT_3D('',#140572,#86750,#86751);
#75324=AXIS2_PLACEMENT_3D('',#140584,#86752,#86753);
#75325=AXIS2_PLACEMENT_3D('',#140601,#86754,#86755);
#75326=AXIS2_PLACEMENT_3D('',#140613,#86756,#86757);
#75327=AXIS2_PLACEMENT_3D('',#140630,#86758,#86759);
#75328=AXIS2_PLACEMENT_3D('',#140647,#86760,#86761);
#75329=AXIS2_PLACEMENT_3D('',#140664,#86762,#86763);
#75330=AXIS2_PLACEMENT_3D('',#140676,#86764,#86765);
#75331=AXIS2_PLACEMENT_3D('',#140693,#86766,#86767);
#75332=AXIS2_PLACEMENT_3D('',#140705,#86768,#86769);
#75333=AXIS2_PLACEMENT_3D('',#140722,#86770,#86771);
#75334=AXIS2_PLACEMENT_3D('',#140734,#86772,#86773);
#75335=AXIS2_PLACEMENT_3D('',#140751,#86774,#86775);
#75336=AXIS2_PLACEMENT_3D('',#140763,#86776,#86777);
#75337=AXIS2_PLACEMENT_3D('',#140780,#86778,#86779);
#75338=AXIS2_PLACEMENT_3D('',#140792,#86780,#86781);
#75339=AXIS2_PLACEMENT_3D('',#140809,#86782,#86783);
#75340=AXIS2_PLACEMENT_3D('',#140821,#86784,#86785);
#75341=AXIS2_PLACEMENT_3D('',#140838,#86786,#86787);
#75342=AXIS2_PLACEMENT_3D('',#140850,#86788,#86789);
#75343=AXIS2_PLACEMENT_3D('',#140867,#86790,#86791);
#75344=AXIS2_PLACEMENT_3D('',#140879,#86792,#86793);
#75345=AXIS2_PLACEMENT_3D('',#140896,#86794,#86795);
#75346=AXIS2_PLACEMENT_3D('',#140913,#86796,#86797);
#75347=AXIS2_PLACEMENT_3D('',#140930,#86798,#86799);
#75348=AXIS2_PLACEMENT_3D('',#140942,#86800,#86801);
#75349=AXIS2_PLACEMENT_3D('',#140959,#86802,#86803);
#75350=AXIS2_PLACEMENT_3D('',#140971,#86804,#86805);
#75351=AXIS2_PLACEMENT_3D('',#140988,#86806,#86807);
#75352=AXIS2_PLACEMENT_3D('',#141000,#86808,#86809);
#75353=AXIS2_PLACEMENT_3D('',#141017,#86810,#86811);
#75354=AXIS2_PLACEMENT_3D('',#141034,#86812,#86813);
#75355=AXIS2_PLACEMENT_3D('',#141051,#86814,#86815);
#75356=AXIS2_PLACEMENT_3D('',#141063,#86816,#86817);
#75357=AXIS2_PLACEMENT_3D('',#141080,#86818,#86819);
#75358=AXIS2_PLACEMENT_3D('',#141092,#86820,#86821);
#75359=AXIS2_PLACEMENT_3D('',#141109,#86822,#86823);
#75360=AXIS2_PLACEMENT_3D('',#141121,#86824,#86825);
#75361=AXIS2_PLACEMENT_3D('',#141138,#86826,#86827);
#75362=AXIS2_PLACEMENT_3D('',#141150,#86828,#86829);
#75363=AXIS2_PLACEMENT_3D('',#141167,#86830,#86831);
#75364=AXIS2_PLACEMENT_3D('',#141179,#86832,#86833);
#75365=AXIS2_PLACEMENT_3D('',#141196,#86834,#86835);
#75366=AXIS2_PLACEMENT_3D('',#141213,#86836,#86837);
#75367=AXIS2_PLACEMENT_3D('',#141230,#86838,#86839);
#75368=AXIS2_PLACEMENT_3D('',#141247,#86840,#86841);
#75369=AXIS2_PLACEMENT_3D('',#141264,#86842,#86843);
#75370=AXIS2_PLACEMENT_3D('',#141276,#86844,#86845);
#75371=AXIS2_PLACEMENT_3D('',#141293,#86846,#86847);
#75372=AXIS2_PLACEMENT_3D('',#141305,#86848,#86849);
#75373=AXIS2_PLACEMENT_3D('',#141322,#86850,#86851);
#75374=AXIS2_PLACEMENT_3D('',#141334,#86852,#86853);
#75375=AXIS2_PLACEMENT_3D('',#141351,#86854,#86855);
#75376=AXIS2_PLACEMENT_3D('',#141367,#86856,#86857);
#75377=AXIS2_PLACEMENT_3D('',#141376,#86858,#86859);
#75378=AXIS2_PLACEMENT_3D('',#141384,#86861,#86862);
#75379=AXIS2_PLACEMENT_3D('',#141386,#86863,#86864);
#75380=AXIS2_PLACEMENT_3D('',#141388,#86865,#86866);
#75381=AXIS2_PLACEMENT_3D('',#141389,#86867,#86868);
#75382=AXIS2_PLACEMENT_3D('',#141409,#86870,#86871);
#75383=AXIS2_PLACEMENT_3D('',#141417,#86873,#86874);
#75384=AXIS2_PLACEMENT_3D('',#141419,#86875,#86876);
#75385=AXIS2_PLACEMENT_3D('',#141421,#86877,#86878);
#75386=AXIS2_PLACEMENT_3D('',#141422,#86879,#86880);
#75387=AXIS2_PLACEMENT_3D('',#141442,#86882,#86883);
#75388=AXIS2_PLACEMENT_3D('',#141450,#86885,#86886);
#75389=AXIS2_PLACEMENT_3D('',#141452,#86887,#86888);
#75390=AXIS2_PLACEMENT_3D('',#141454,#86889,#86890);
#75391=AXIS2_PLACEMENT_3D('',#141455,#86891,#86892);
#75392=AXIS2_PLACEMENT_3D('',#141475,#86894,#86895);
#75393=AXIS2_PLACEMENT_3D('',#141483,#86897,#86898);
#75394=AXIS2_PLACEMENT_3D('',#141485,#86899,#86900);
#75395=AXIS2_PLACEMENT_3D('',#141487,#86901,#86902);
#75396=AXIS2_PLACEMENT_3D('',#141488,#86903,#86904);
#75397=AXIS2_PLACEMENT_3D('',#141508,#86906,#86907);
#75398=AXIS2_PLACEMENT_3D('',#141516,#86909,#86910);
#75399=AXIS2_PLACEMENT_3D('',#141518,#86911,#86912);
#75400=AXIS2_PLACEMENT_3D('',#141520,#86913,#86914);
#75401=AXIS2_PLACEMENT_3D('',#141521,#86915,#86916);
#75402=AXIS2_PLACEMENT_3D('',#141541,#86918,#86919);
#75403=AXIS2_PLACEMENT_3D('',#141549,#86921,#86922);
#75404=AXIS2_PLACEMENT_3D('',#141551,#86923,#86924);
#75405=AXIS2_PLACEMENT_3D('',#141553,#86925,#86926);
#75406=AXIS2_PLACEMENT_3D('',#141554,#86927,#86928);
#75407=AXIS2_PLACEMENT_3D('',#141574,#86930,#86931);
#75408=AXIS2_PLACEMENT_3D('',#141582,#86933,#86934);
#75409=AXIS2_PLACEMENT_3D('',#141584,#86935,#86936);
#75410=AXIS2_PLACEMENT_3D('',#141586,#86937,#86938);
#75411=AXIS2_PLACEMENT_3D('',#141587,#86939,#86940);
#75412=AXIS2_PLACEMENT_3D('',#141607,#86942,#86943);
#75413=AXIS2_PLACEMENT_3D('',#141615,#86945,#86946);
#75414=AXIS2_PLACEMENT_3D('',#141617,#86947,#86948);
#75415=AXIS2_PLACEMENT_3D('',#141619,#86949,#86950);
#75416=AXIS2_PLACEMENT_3D('',#141620,#86951,#86952);
#75417=AXIS2_PLACEMENT_3D('',#141640,#86954,#86955);
#75418=AXIS2_PLACEMENT_3D('',#141648,#86957,#86958);
#75419=AXIS2_PLACEMENT_3D('',#141650,#86959,#86960);
#75420=AXIS2_PLACEMENT_3D('',#141652,#86961,#86962);
#75421=AXIS2_PLACEMENT_3D('',#141653,#86963,#86964);
#75422=AXIS2_PLACEMENT_3D('',#141673,#86966,#86967);
#75423=AXIS2_PLACEMENT_3D('',#141681,#86969,#86970);
#75424=AXIS2_PLACEMENT_3D('',#141683,#86971,#86972);
#75425=AXIS2_PLACEMENT_3D('',#141685,#86973,#86974);
#75426=AXIS2_PLACEMENT_3D('',#141686,#86975,#86976);
#75427=AXIS2_PLACEMENT_3D('',#141706,#86978,#86979);
#75428=AXIS2_PLACEMENT_3D('',#141714,#86981,#86982);
#75429=AXIS2_PLACEMENT_3D('',#141716,#86983,#86984);
#75430=AXIS2_PLACEMENT_3D('',#141718,#86985,#86986);
#75431=AXIS2_PLACEMENT_3D('',#141719,#86987,#86988);
#75432=AXIS2_PLACEMENT_3D('',#141739,#86990,#86991);
#75433=AXIS2_PLACEMENT_3D('',#141747,#86993,#86994);
#75434=AXIS2_PLACEMENT_3D('',#141749,#86995,#86996);
#75435=AXIS2_PLACEMENT_3D('',#141751,#86997,#86998);
#75436=AXIS2_PLACEMENT_3D('',#141752,#86999,#87000);
#75437=AXIS2_PLACEMENT_3D('',#141772,#87002,#87003);
#75438=AXIS2_PLACEMENT_3D('',#141780,#87005,#87006);
#75439=AXIS2_PLACEMENT_3D('',#141782,#87007,#87008);
#75440=AXIS2_PLACEMENT_3D('',#141784,#87009,#87010);
#75441=AXIS2_PLACEMENT_3D('',#141785,#87011,#87012);
#75442=AXIS2_PLACEMENT_3D('',#141805,#87014,#87015);
#75443=AXIS2_PLACEMENT_3D('',#141813,#87017,#87018);
#75444=AXIS2_PLACEMENT_3D('',#141815,#87019,#87020);
#75445=AXIS2_PLACEMENT_3D('',#141817,#87021,#87022);
#75446=AXIS2_PLACEMENT_3D('',#141818,#87023,#87024);
#75447=AXIS2_PLACEMENT_3D('',#141862,#87028,#87029);
#75448=AXIS2_PLACEMENT_3D('',#141870,#87031,#87032);
#75449=AXIS2_PLACEMENT_3D('',#141872,#87033,#87034);
#75450=AXIS2_PLACEMENT_3D('',#141874,#87035,#87036);
#75451=AXIS2_PLACEMENT_3D('',#141875,#87037,#87038);
#75452=AXIS2_PLACEMENT_3D('',#141895,#87040,#87041);
#75453=AXIS2_PLACEMENT_3D('',#141903,#87043,#87044);
#75454=AXIS2_PLACEMENT_3D('',#141905,#87045,#87046);
#75455=AXIS2_PLACEMENT_3D('',#141907,#87047,#87048);
#75456=AXIS2_PLACEMENT_3D('',#141908,#87049,#87050);
#75457=AXIS2_PLACEMENT_3D('',#141928,#87052,#87053);
#75458=AXIS2_PLACEMENT_3D('',#141936,#87055,#87056);
#75459=AXIS2_PLACEMENT_3D('',#141938,#87057,#87058);
#75460=AXIS2_PLACEMENT_3D('',#141940,#87059,#87060);
#75461=AXIS2_PLACEMENT_3D('',#141941,#87061,#87062);
#75462=AXIS2_PLACEMENT_3D('',#141961,#87064,#87065);
#75463=AXIS2_PLACEMENT_3D('',#141969,#87067,#87068);
#75464=AXIS2_PLACEMENT_3D('',#141971,#87069,#87070);
#75465=AXIS2_PLACEMENT_3D('',#141973,#87071,#87072);
#75466=AXIS2_PLACEMENT_3D('',#141974,#87073,#87074);
#75467=AXIS2_PLACEMENT_3D('',#141994,#87076,#87077);
#75468=AXIS2_PLACEMENT_3D('',#142013,#87079,#87080);
#75469=AXIS2_PLACEMENT_3D('',#142015,#87082,#87083);
#75470=AXIS2_PLACEMENT_3D('',#142017,#87084,#87085);
#75471=AXIS2_PLACEMENT_3D('',#142018,#87086,#87087);
#75472=AXIS2_PLACEMENT_3D('',#142028,#87089,#87090);
#75473=AXIS2_PLACEMENT_3D('',#142035,#87091,#87092);
#75474=AXIS2_PLACEMENT_3D('',#142037,#87093,#87094);
#75475=AXIS2_PLACEMENT_3D('',#142039,#87095,#87096);
#75476=AXIS2_PLACEMENT_3D('',#142040,#87097,#87098);
#75477=AXIS2_PLACEMENT_3D('',#142060,#87100,#87101);
#75478=AXIS2_PLACEMENT_3D('',#142068,#87103,#87104);
#75479=AXIS2_PLACEMENT_3D('',#142070,#87105,#87106);
#75480=AXIS2_PLACEMENT_3D('',#142072,#87107,#87108);
#75481=AXIS2_PLACEMENT_3D('',#142073,#87109,#87110);
#75482=AXIS2_PLACEMENT_3D('',#142093,#87112,#87113);
#75483=AXIS2_PLACEMENT_3D('',#142101,#87115,#87116);
#75484=AXIS2_PLACEMENT_3D('',#142103,#87117,#87118);
#75485=AXIS2_PLACEMENT_3D('',#142105,#87119,#87120);
#75486=AXIS2_PLACEMENT_3D('',#142106,#87121,#87122);
#75487=AXIS2_PLACEMENT_3D('',#142126,#87124,#87125);
#75488=AXIS2_PLACEMENT_3D('',#142134,#87127,#87128);
#75489=AXIS2_PLACEMENT_3D('',#142136,#87129,#87130);
#75490=AXIS2_PLACEMENT_3D('',#142138,#87131,#87132);
#75491=AXIS2_PLACEMENT_3D('',#142139,#87133,#87134);
#75492=AXIS2_PLACEMENT_3D('',#142159,#87136,#87137);
#75493=AXIS2_PLACEMENT_3D('',#142167,#87139,#87140);
#75494=AXIS2_PLACEMENT_3D('',#142169,#87141,#87142);
#75495=AXIS2_PLACEMENT_3D('',#142171,#87143,#87144);
#75496=AXIS2_PLACEMENT_3D('',#142172,#87145,#87146);
#75497=AXIS2_PLACEMENT_3D('',#142192,#87148,#87149);
#75498=AXIS2_PLACEMENT_3D('',#142200,#87151,#87152);
#75499=AXIS2_PLACEMENT_3D('',#142202,#87153,#87154);
#75500=AXIS2_PLACEMENT_3D('',#142204,#87155,#87156);
#75501=AXIS2_PLACEMENT_3D('',#142205,#87157,#87158);
#75502=AXIS2_PLACEMENT_3D('',#142225,#87160,#87161);
#75503=AXIS2_PLACEMENT_3D('',#142233,#87163,#87164);
#75504=AXIS2_PLACEMENT_3D('',#142235,#87165,#87166);
#75505=AXIS2_PLACEMENT_3D('',#142237,#87167,#87168);
#75506=AXIS2_PLACEMENT_3D('',#142238,#87169,#87170);
#75507=AXIS2_PLACEMENT_3D('',#142258,#87172,#87173);
#75508=AXIS2_PLACEMENT_3D('',#142266,#87175,#87176);
#75509=AXIS2_PLACEMENT_3D('',#142268,#87177,#87178);
#75510=AXIS2_PLACEMENT_3D('',#142270,#87179,#87180);
#75511=AXIS2_PLACEMENT_3D('',#142271,#87181,#87182);
#75512=AXIS2_PLACEMENT_3D('',#142291,#87184,#87185);
#75513=AXIS2_PLACEMENT_3D('',#142299,#87187,#87188);
#75514=AXIS2_PLACEMENT_3D('',#142301,#87189,#87190);
#75515=AXIS2_PLACEMENT_3D('',#142303,#87191,#87192);
#75516=AXIS2_PLACEMENT_3D('',#142304,#87193,#87194);
#75517=AXIS2_PLACEMENT_3D('',#142329,#87197,#87198);
#75518=AXIS2_PLACEMENT_3D('',#142351,#87199,#87200);
#75519=AXIS2_PLACEMENT_3D('',#142353,#87202,#87203);
#75520=AXIS2_PLACEMENT_3D('',#142355,#87204,#87205);
#75521=AXIS2_PLACEMENT_3D('',#142356,#87206,#87207);
#75522=AXIS2_PLACEMENT_3D('',#142370,#87209,#87210);
#75523=AXIS2_PLACEMENT_3D('',#142392,#87211,#87212);
#75524=AXIS2_PLACEMENT_3D('',#142394,#87214,#87215);
#75525=AXIS2_PLACEMENT_3D('',#142396,#87216,#87217);
#75526=AXIS2_PLACEMENT_3D('',#142397,#87218,#87219);
#75527=AXIS2_PLACEMENT_3D('',#142411,#87221,#87222);
#75528=AXIS2_PLACEMENT_3D('',#142433,#87223,#87224);
#75529=AXIS2_PLACEMENT_3D('',#142435,#87226,#87227);
#75530=AXIS2_PLACEMENT_3D('',#142437,#87228,#87229);
#75531=AXIS2_PLACEMENT_3D('',#142438,#87230,#87231);
#75532=AXIS2_PLACEMENT_3D('',#142452,#87233,#87234);
#75533=AXIS2_PLACEMENT_3D('',#142474,#87235,#87236);
#75534=AXIS2_PLACEMENT_3D('',#142476,#87238,#87239);
#75535=AXIS2_PLACEMENT_3D('',#142478,#87240,#87241);
#75536=AXIS2_PLACEMENT_3D('',#142479,#87242,#87243);
#75537=AXIS2_PLACEMENT_3D('',#142493,#87245,#87246);
#75538=AXIS2_PLACEMENT_3D('',#142515,#87247,#87248);
#75539=AXIS2_PLACEMENT_3D('',#142517,#87250,#87251);
#75540=AXIS2_PLACEMENT_3D('',#142519,#87252,#87253);
#75541=AXIS2_PLACEMENT_3D('',#142520,#87254,#87255);
#75542=AXIS2_PLACEMENT_3D('',#142534,#87257,#87258);
#75543=AXIS2_PLACEMENT_3D('',#142556,#87259,#87260);
#75544=AXIS2_PLACEMENT_3D('',#142558,#87262,#87263);
#75545=AXIS2_PLACEMENT_3D('',#142560,#87264,#87265);
#75546=AXIS2_PLACEMENT_3D('',#142561,#87266,#87267);
#75547=AXIS2_PLACEMENT_3D('',#142575,#87269,#87270);
#75548=AXIS2_PLACEMENT_3D('',#142597,#87271,#87272);
#75549=AXIS2_PLACEMENT_3D('',#142599,#87274,#87275);
#75550=AXIS2_PLACEMENT_3D('',#142601,#87276,#87277);
#75551=AXIS2_PLACEMENT_3D('',#142602,#87278,#87279);
#75552=AXIS2_PLACEMENT_3D('',#142616,#87281,#87282);
#75553=AXIS2_PLACEMENT_3D('',#142638,#87283,#87284);
#75554=AXIS2_PLACEMENT_3D('',#142640,#87286,#87287);
#75555=AXIS2_PLACEMENT_3D('',#142642,#87288,#87289);
#75556=AXIS2_PLACEMENT_3D('',#142643,#87290,#87291);
#75557=AXIS2_PLACEMENT_3D('',#142657,#87293,#87294);
#75558=AXIS2_PLACEMENT_3D('',#142679,#87295,#87296);
#75559=AXIS2_PLACEMENT_3D('',#142681,#87298,#87299);
#75560=AXIS2_PLACEMENT_3D('',#142683,#87300,#87301);
#75561=AXIS2_PLACEMENT_3D('',#142684,#87302,#87303);
#75562=AXIS2_PLACEMENT_3D('',#142698,#87305,#87306);
#75563=AXIS2_PLACEMENT_3D('',#142720,#87307,#87308);
#75564=AXIS2_PLACEMENT_3D('',#142722,#87310,#87311);
#75565=AXIS2_PLACEMENT_3D('',#142724,#87312,#87313);
#75566=AXIS2_PLACEMENT_3D('',#142725,#87314,#87315);
#75567=AXIS2_PLACEMENT_3D('',#142739,#87317,#87318);
#75568=AXIS2_PLACEMENT_3D('',#142761,#87319,#87320);
#75569=AXIS2_PLACEMENT_3D('',#142763,#87322,#87323);
#75570=AXIS2_PLACEMENT_3D('',#142765,#87324,#87325);
#75571=AXIS2_PLACEMENT_3D('',#142766,#87326,#87327);
#75572=AXIS2_PLACEMENT_3D('',#142780,#87329,#87330);
#75573=AXIS2_PLACEMENT_3D('',#142802,#87331,#87332);
#75574=AXIS2_PLACEMENT_3D('',#142804,#87334,#87335);
#75575=AXIS2_PLACEMENT_3D('',#142806,#87336,#87337);
#75576=AXIS2_PLACEMENT_3D('',#142807,#87338,#87339);
#75577=AXIS2_PLACEMENT_3D('',#142821,#87341,#87342);
#75578=AXIS2_PLACEMENT_3D('',#142843,#87343,#87344);
#75579=AXIS2_PLACEMENT_3D('',#142845,#87346,#87347);
#75580=AXIS2_PLACEMENT_3D('',#142847,#87348,#87349);
#75581=AXIS2_PLACEMENT_3D('',#142848,#87350,#87351);
#75582=AXIS2_PLACEMENT_3D('',#142862,#87353,#87354);
#75583=AXIS2_PLACEMENT_3D('',#142884,#87355,#87356);
#75584=AXIS2_PLACEMENT_3D('',#142886,#87358,#87359);
#75585=AXIS2_PLACEMENT_3D('',#142888,#87360,#87361);
#75586=AXIS2_PLACEMENT_3D('',#142889,#87362,#87363);
#75587=AXIS2_PLACEMENT_3D('',#142903,#87365,#87366);
#75588=AXIS2_PLACEMENT_3D('',#142925,#87367,#87368);
#75589=AXIS2_PLACEMENT_3D('',#142927,#87370,#87371);
#75590=AXIS2_PLACEMENT_3D('',#142929,#87372,#87373);
#75591=AXIS2_PLACEMENT_3D('',#142930,#87374,#87375);
#75592=AXIS2_PLACEMENT_3D('',#142944,#87377,#87378);
#75593=AXIS2_PLACEMENT_3D('',#142966,#87379,#87380);
#75594=AXIS2_PLACEMENT_3D('',#142968,#87382,#87383);
#75595=AXIS2_PLACEMENT_3D('',#142970,#87384,#87385);
#75596=AXIS2_PLACEMENT_3D('',#142971,#87386,#87387);
#75597=AXIS2_PLACEMENT_3D('',#142985,#87389,#87390);
#75598=AXIS2_PLACEMENT_3D('',#143007,#87391,#87392);
#75599=AXIS2_PLACEMENT_3D('',#143009,#87394,#87395);
#75600=AXIS2_PLACEMENT_3D('',#143011,#87396,#87397);
#75601=AXIS2_PLACEMENT_3D('',#143012,#87398,#87399);
#75602=AXIS2_PLACEMENT_3D('',#143026,#87401,#87402);
#75603=AXIS2_PLACEMENT_3D('',#143048,#87403,#87404);
#75604=AXIS2_PLACEMENT_3D('',#143050,#87406,#87407);
#75605=AXIS2_PLACEMENT_3D('',#143052,#87408,#87409);
#75606=AXIS2_PLACEMENT_3D('',#143053,#87410,#87411);
#75607=AXIS2_PLACEMENT_3D('',#143067,#87413,#87414);
#75608=AXIS2_PLACEMENT_3D('',#143089,#87415,#87416);
#75609=AXIS2_PLACEMENT_3D('',#143091,#87418,#87419);
#75610=AXIS2_PLACEMENT_3D('',#143093,#87420,#87421);
#75611=AXIS2_PLACEMENT_3D('',#143094,#87422,#87423);
#75612=AXIS2_PLACEMENT_3D('',#143108,#87425,#87426);
#75613=AXIS2_PLACEMENT_3D('',#143130,#87427,#87428);
#75614=AXIS2_PLACEMENT_3D('',#143132,#87430,#87431);
#75615=AXIS2_PLACEMENT_3D('',#143134,#87432,#87433);
#75616=AXIS2_PLACEMENT_3D('',#143135,#87434,#87435);
#75617=AXIS2_PLACEMENT_3D('',#143149,#87437,#87438);
#75618=AXIS2_PLACEMENT_3D('',#143171,#87439,#87440);
#75619=AXIS2_PLACEMENT_3D('',#143173,#87442,#87443);
#75620=AXIS2_PLACEMENT_3D('',#143175,#87444,#87445);
#75621=AXIS2_PLACEMENT_3D('',#143176,#87446,#87447);
#75622=AXIS2_PLACEMENT_3D('',#143222,#87451,#87452);
#75623=AXIS2_PLACEMENT_3D('',#143244,#87453,#87454);
#75624=AXIS2_PLACEMENT_3D('',#143246,#87456,#87457);
#75625=AXIS2_PLACEMENT_3D('',#143248,#87458,#87459);
#75626=AXIS2_PLACEMENT_3D('',#143249,#87460,#87461);
#75627=AXIS2_PLACEMENT_3D('',#143263,#87463,#87464);
#75628=AXIS2_PLACEMENT_3D('',#143285,#87465,#87466);
#75629=AXIS2_PLACEMENT_3D('',#143287,#87468,#87469);
#75630=AXIS2_PLACEMENT_3D('',#143289,#87470,#87471);
#75631=AXIS2_PLACEMENT_3D('',#143290,#87472,#87473);
#75632=AXIS2_PLACEMENT_3D('',#143304,#87475,#87476);
#75633=AXIS2_PLACEMENT_3D('',#143326,#87477,#87478);
#75634=AXIS2_PLACEMENT_3D('',#143328,#87480,#87481);
#75635=AXIS2_PLACEMENT_3D('',#143330,#87482,#87483);
#75636=AXIS2_PLACEMENT_3D('',#143331,#87484,#87485);
#75637=AXIS2_PLACEMENT_3D('',#143345,#87487,#87488);
#75638=AXIS2_PLACEMENT_3D('',#143367,#87489,#87490);
#75639=AXIS2_PLACEMENT_3D('',#143369,#87492,#87493);
#75640=AXIS2_PLACEMENT_3D('',#143371,#87494,#87495);
#75641=AXIS2_PLACEMENT_3D('',#143372,#87496,#87497);
#75642=AXIS2_PLACEMENT_3D('',#143386,#87499,#87500);
#75643=AXIS2_PLACEMENT_3D('',#143408,#87501,#87502);
#75644=AXIS2_PLACEMENT_3D('',#143410,#87504,#87505);
#75645=AXIS2_PLACEMENT_3D('',#143412,#87506,#87507);
#75646=AXIS2_PLACEMENT_3D('',#143413,#87508,#87509);
#75647=AXIS2_PLACEMENT_3D('',#143427,#87511,#87512);
#75648=AXIS2_PLACEMENT_3D('',#143449,#87513,#87514);
#75649=AXIS2_PLACEMENT_3D('',#143451,#87516,#87517);
#75650=AXIS2_PLACEMENT_3D('',#143453,#87518,#87519);
#75651=AXIS2_PLACEMENT_3D('',#143454,#87520,#87521);
#75652=AXIS2_PLACEMENT_3D('',#143468,#87523,#87524);
#75653=AXIS2_PLACEMENT_3D('',#143490,#87525,#87526);
#75654=AXIS2_PLACEMENT_3D('',#143492,#87528,#87529);
#75655=AXIS2_PLACEMENT_3D('',#143494,#87530,#87531);
#75656=AXIS2_PLACEMENT_3D('',#143495,#87532,#87533);
#75657=AXIS2_PLACEMENT_3D('',#143503,#87534,#87535);
#75658=AXIS2_PLACEMENT_3D('',#143520,#87536,#87537);
#75659=AXIS2_PLACEMENT_3D('',#143528,#87538,#87539);
#75660=AXIS2_PLACEMENT_3D('',#143545,#87540,#87541);
#75661=AXIS2_PLACEMENT_3D('',#143553,#87542,#87543);
#75662=AXIS2_PLACEMENT_3D('',#143570,#87544,#87545);
#75663=AXIS2_PLACEMENT_3D('',#143578,#87546,#87547);
#75664=AXIS2_PLACEMENT_3D('',#143595,#87548,#87549);
#75665=AXIS2_PLACEMENT_3D('',#143603,#87550,#87551);
#75666=AXIS2_PLACEMENT_3D('',#143620,#87552,#87553);
#75667=AXIS2_PLACEMENT_3D('',#143628,#87554,#87555);
#75668=AXIS2_PLACEMENT_3D('',#143645,#87556,#87557);
#75669=AXIS2_PLACEMENT_3D('',#143653,#87558,#87559);
#75670=AXIS2_PLACEMENT_3D('',#143670,#87560,#87561);
#75671=AXIS2_PLACEMENT_3D('',#143678,#87562,#87563);
#75672=AXIS2_PLACEMENT_3D('',#143695,#87564,#87565);
#75673=AXIS2_PLACEMENT_3D('',#143703,#87566,#87567);
#75674=AXIS2_PLACEMENT_3D('',#143720,#87568,#87569);
#75675=AXIS2_PLACEMENT_3D('',#143728,#87570,#87571);
#75676=AXIS2_PLACEMENT_3D('',#143745,#87572,#87573);
#75677=AXIS2_PLACEMENT_3D('',#143753,#87574,#87575);
#75678=AXIS2_PLACEMENT_3D('',#143770,#87576,#87577);
#75679=AXIS2_PLACEMENT_3D('',#143778,#87578,#87579);
#75680=AXIS2_PLACEMENT_3D('',#143795,#87580,#87581);
#75681=AXIS2_PLACEMENT_3D('',#143803,#87582,#87583);
#75682=AXIS2_PLACEMENT_3D('',#143820,#87584,#87585);
#75683=AXIS2_PLACEMENT_3D('',#143828,#87586,#87587);
#75684=AXIS2_PLACEMENT_3D('',#143845,#87588,#87589);
#75685=AXIS2_PLACEMENT_3D('',#143853,#87590,#87591);
#75686=AXIS2_PLACEMENT_3D('',#143870,#87592,#87593);
#75687=AXIS2_PLACEMENT_3D('',#143878,#87594,#87595);
#75688=AXIS2_PLACEMENT_3D('',#143895,#87596,#87597);
#75689=AXIS2_PLACEMENT_3D('',#143903,#87598,#87599);
#75690=AXIS2_PLACEMENT_3D('',#143920,#87600,#87601);
#75691=AXIS2_PLACEMENT_3D('',#143928,#87602,#87603);
#75692=AXIS2_PLACEMENT_3D('',#143945,#87604,#87605);
#75693=AXIS2_PLACEMENT_3D('',#143953,#87606,#87607);
#75694=AXIS2_PLACEMENT_3D('',#143970,#87608,#87609);
#75695=AXIS2_PLACEMENT_3D('',#143978,#87610,#87611);
#75696=AXIS2_PLACEMENT_3D('',#143995,#87612,#87613);
#75697=AXIS2_PLACEMENT_3D('',#144003,#87614,#87615);
#75698=AXIS2_PLACEMENT_3D('',#144020,#87616,#87617);
#75699=AXIS2_PLACEMENT_3D('',#144028,#87618,#87619);
#75700=AXIS2_PLACEMENT_3D('',#144045,#87620,#87621);
#75701=AXIS2_PLACEMENT_3D('',#144053,#87622,#87623);
#75702=AXIS2_PLACEMENT_3D('',#144070,#87624,#87625);
#75703=AXIS2_PLACEMENT_3D('',#144078,#87626,#87627);
#75704=AXIS2_PLACEMENT_3D('',#144095,#87628,#87629);
#75705=AXIS2_PLACEMENT_3D('',#144103,#87630,#87631);
#75706=AXIS2_PLACEMENT_3D('',#144120,#87632,#87633);
#75707=AXIS2_PLACEMENT_3D('',#144128,#87634,#87635);
#75708=AXIS2_PLACEMENT_3D('',#144145,#87636,#87637);
#75709=AXIS2_PLACEMENT_3D('',#144153,#87638,#87639);
#75710=AXIS2_PLACEMENT_3D('',#144170,#87640,#87641);
#75711=AXIS2_PLACEMENT_3D('',#144178,#87642,#87643);
#75712=AXIS2_PLACEMENT_3D('',#144195,#87644,#87645);
#75713=AXIS2_PLACEMENT_3D('',#144203,#87646,#87647);
#75714=AXIS2_PLACEMENT_3D('',#144220,#87648,#87649);
#75715=AXIS2_PLACEMENT_3D('',#144228,#87650,#87651);
#75716=AXIS2_PLACEMENT_3D('',#144241,#87652,#87653);
#75717=AXIS2_PLACEMENT_3D('',#144249,#87654,#87655);
#75718=AXIS2_PLACEMENT_3D('',#144262,#87656,#87657);
#75719=AXIS2_PLACEMENT_3D('',#144270,#87658,#87659);
#75720=AXIS2_PLACEMENT_3D('',#144283,#87660,#87661);
#75721=AXIS2_PLACEMENT_3D('',#144291,#87662,#87663);
#75722=AXIS2_PLACEMENT_3D('',#144304,#87664,#87665);
#75723=AXIS2_PLACEMENT_3D('',#144312,#87666,#87667);
#75724=AXIS2_PLACEMENT_3D('',#144325,#87668,#87669);
#75725=AXIS2_PLACEMENT_3D('',#144333,#87670,#87671);
#75726=AXIS2_PLACEMENT_3D('',#144346,#87672,#87673);
#75727=AXIS2_PLACEMENT_3D('',#144354,#87674,#87675);
#75728=AXIS2_PLACEMENT_3D('',#144367,#87676,#87677);
#75729=AXIS2_PLACEMENT_3D('',#144375,#87678,#87679);
#75730=AXIS2_PLACEMENT_3D('',#144388,#87680,#87681);
#75731=AXIS2_PLACEMENT_3D('',#144396,#87682,#87683);
#75732=AXIS2_PLACEMENT_3D('',#144409,#87684,#87685);
#75733=AXIS2_PLACEMENT_3D('',#144417,#87686,#87687);
#75734=AXIS2_PLACEMENT_3D('',#144430,#87688,#87689);
#75735=AXIS2_PLACEMENT_3D('',#144438,#87690,#87691);
#75736=AXIS2_PLACEMENT_3D('',#144451,#87692,#87693);
#75737=AXIS2_PLACEMENT_3D('',#144459,#87694,#87695);
#75738=AXIS2_PLACEMENT_3D('',#144472,#87696,#87697);
#75739=AXIS2_PLACEMENT_3D('',#144480,#87698,#87699);
#75740=AXIS2_PLACEMENT_3D('',#144493,#87700,#87701);
#75741=AXIS2_PLACEMENT_3D('',#144501,#87702,#87703);
#75742=AXIS2_PLACEMENT_3D('',#144514,#87704,#87705);
#75743=AXIS2_PLACEMENT_3D('',#144522,#87706,#87707);
#75744=AXIS2_PLACEMENT_3D('',#144535,#87708,#87709);
#75745=AXIS2_PLACEMENT_3D('',#144543,#87710,#87711);
#75746=AXIS2_PLACEMENT_3D('',#144556,#87712,#87713);
#75747=AXIS2_PLACEMENT_3D('',#144564,#87714,#87715);
#75748=AXIS2_PLACEMENT_3D('',#144577,#87716,#87717);
#75749=AXIS2_PLACEMENT_3D('',#144585,#87718,#87719);
#75750=AXIS2_PLACEMENT_3D('',#144598,#87720,#87721);
#75751=AXIS2_PLACEMENT_3D('',#144606,#87722,#87723);
#75752=AXIS2_PLACEMENT_3D('',#144619,#87724,#87725);
#75753=AXIS2_PLACEMENT_3D('',#144627,#87726,#87727);
#75754=AXIS2_PLACEMENT_3D('',#144640,#87728,#87729);
#75755=AXIS2_PLACEMENT_3D('',#144648,#87730,#87731);
#75756=AXIS2_PLACEMENT_3D('',#144661,#87732,#87733);
#75757=AXIS2_PLACEMENT_3D('',#144669,#87734,#87735);
#75758=AXIS2_PLACEMENT_3D('',#144682,#87736,#87737);
#75759=AXIS2_PLACEMENT_3D('',#144690,#87738,#87739);
#75760=AXIS2_PLACEMENT_3D('',#144703,#87740,#87741);
#75761=AXIS2_PLACEMENT_3D('',#144711,#87742,#87743);
#75762=AXIS2_PLACEMENT_3D('',#144724,#87744,#87745);
#75763=AXIS2_PLACEMENT_3D('',#144732,#87746,#87747);
#75764=AXIS2_PLACEMENT_3D('',#144745,#87748,#87749);
#75765=AXIS2_PLACEMENT_3D('',#144753,#87750,#87751);
#75766=AXIS2_PLACEMENT_3D('',#144766,#87752,#87753);
#75767=AXIS2_PLACEMENT_3D('',#144774,#87754,#87755);
#75768=AXIS2_PLACEMENT_3D('',#144787,#87756,#87757);
#75769=AXIS2_PLACEMENT_3D('',#144795,#87758,#87759);
#75770=AXIS2_PLACEMENT_3D('',#144808,#87760,#87761);
#75771=AXIS2_PLACEMENT_3D('',#144816,#87762,#87763);
#75772=AXIS2_PLACEMENT_3D('',#144829,#87764,#87765);
#75773=AXIS2_PLACEMENT_3D('',#144838,#87766,#87767);
#75774=AXIS2_PLACEMENT_3D('',#144854,#87769,#87770);
#75775=AXIS2_PLACEMENT_3D('',#144862,#87772,#87773);
#75776=AXIS2_PLACEMENT_3D('',#144864,#87774,#87775);
#75777=AXIS2_PLACEMENT_3D('',#144866,#87776,#87777);
#75778=AXIS2_PLACEMENT_3D('',#144867,#87778,#87779);
#75779=AXIS2_PLACEMENT_3D('',#144883,#87781,#87782);
#75780=AXIS2_PLACEMENT_3D('',#144891,#87784,#87785);
#75781=AXIS2_PLACEMENT_3D('',#144893,#87786,#87787);
#75782=AXIS2_PLACEMENT_3D('',#144895,#87788,#87789);
#75783=AXIS2_PLACEMENT_3D('',#144896,#87790,#87791);
#75784=AXIS2_PLACEMENT_3D('',#144912,#87793,#87794);
#75785=AXIS2_PLACEMENT_3D('',#144920,#87796,#87797);
#75786=AXIS2_PLACEMENT_3D('',#144922,#87798,#87799);
#75787=AXIS2_PLACEMENT_3D('',#144924,#87800,#87801);
#75788=AXIS2_PLACEMENT_3D('',#144925,#87802,#87803);
#75789=AXIS2_PLACEMENT_3D('',#144941,#87805,#87806);
#75790=AXIS2_PLACEMENT_3D('',#144949,#87808,#87809);
#75791=AXIS2_PLACEMENT_3D('',#144951,#87810,#87811);
#75792=AXIS2_PLACEMENT_3D('',#144953,#87812,#87813);
#75793=AXIS2_PLACEMENT_3D('',#144954,#87814,#87815);
#75794=AXIS2_PLACEMENT_3D('',#144970,#87817,#87818);
#75795=AXIS2_PLACEMENT_3D('',#144978,#87820,#87821);
#75796=AXIS2_PLACEMENT_3D('',#144980,#87822,#87823);
#75797=AXIS2_PLACEMENT_3D('',#144982,#87824,#87825);
#75798=AXIS2_PLACEMENT_3D('',#144983,#87826,#87827);
#75799=AXIS2_PLACEMENT_3D('',#144999,#87829,#87830);
#75800=AXIS2_PLACEMENT_3D('',#145007,#87832,#87833);
#75801=AXIS2_PLACEMENT_3D('',#145009,#87834,#87835);
#75802=AXIS2_PLACEMENT_3D('',#145011,#87836,#87837);
#75803=AXIS2_PLACEMENT_3D('',#145012,#87838,#87839);
#75804=AXIS2_PLACEMENT_3D('',#145048,#87843,#87844);
#75805=AXIS2_PLACEMENT_3D('',#145056,#87846,#87847);
#75806=AXIS2_PLACEMENT_3D('',#145058,#87848,#87849);
#75807=AXIS2_PLACEMENT_3D('',#145060,#87850,#87851);
#75808=AXIS2_PLACEMENT_3D('',#145061,#87852,#87853);
#75809=AXIS2_PLACEMENT_3D('',#145077,#87855,#87856);
#75810=AXIS2_PLACEMENT_3D('',#145085,#87858,#87859);
#75811=AXIS2_PLACEMENT_3D('',#145087,#87860,#87861);
#75812=AXIS2_PLACEMENT_3D('',#145089,#87862,#87863);
#75813=AXIS2_PLACEMENT_3D('',#145090,#87864,#87865);
#75814=AXIS2_PLACEMENT_3D('',#145106,#87867,#87868);
#75815=AXIS2_PLACEMENT_3D('',#145114,#87870,#87871);
#75816=AXIS2_PLACEMENT_3D('',#145116,#87872,#87873);
#75817=AXIS2_PLACEMENT_3D('',#145118,#87874,#87875);
#75818=AXIS2_PLACEMENT_3D('',#145119,#87876,#87877);
#75819=AXIS2_PLACEMENT_3D('',#145135,#87879,#87880);
#75820=AXIS2_PLACEMENT_3D('',#145143,#87882,#87883);
#75821=AXIS2_PLACEMENT_3D('',#145145,#87884,#87885);
#75822=AXIS2_PLACEMENT_3D('',#145147,#87886,#87887);
#75823=AXIS2_PLACEMENT_3D('',#145148,#87888,#87889);
#75824=AXIS2_PLACEMENT_3D('',#145164,#87891,#87892);
#75825=AXIS2_PLACEMENT_3D('',#145172,#87894,#87895);
#75826=AXIS2_PLACEMENT_3D('',#145174,#87896,#87897);
#75827=AXIS2_PLACEMENT_3D('',#145176,#87898,#87899);
#75828=AXIS2_PLACEMENT_3D('',#145177,#87900,#87901);
#75829=AXIS2_PLACEMENT_3D('',#145193,#87903,#87904);
#75830=AXIS2_PLACEMENT_3D('',#145201,#87906,#87907);
#75831=AXIS2_PLACEMENT_3D('',#145203,#87908,#87909);
#75832=AXIS2_PLACEMENT_3D('',#145205,#87910,#87911);
#75833=AXIS2_PLACEMENT_3D('',#145206,#87912,#87913);
#75834=AXIS2_PLACEMENT_3D('',#145222,#87915,#87916);
#75835=AXIS2_PLACEMENT_3D('',#145230,#87918,#87919);
#75836=AXIS2_PLACEMENT_3D('',#145232,#87920,#87921);
#75837=AXIS2_PLACEMENT_3D('',#145234,#87922,#87923);
#75838=AXIS2_PLACEMENT_3D('',#145235,#87924,#87925);
#75839=AXIS2_PLACEMENT_3D('',#145251,#87927,#87928);
#75840=AXIS2_PLACEMENT_3D('',#145259,#87930,#87931);
#75841=AXIS2_PLACEMENT_3D('',#145261,#87932,#87933);
#75842=AXIS2_PLACEMENT_3D('',#145263,#87934,#87935);
#75843=AXIS2_PLACEMENT_3D('',#145264,#87936,#87937);
#75844=AXIS2_PLACEMENT_3D('',#145280,#87939,#87940);
#75845=AXIS2_PLACEMENT_3D('',#145288,#87942,#87943);
#75846=AXIS2_PLACEMENT_3D('',#145290,#87944,#87945);
#75847=AXIS2_PLACEMENT_3D('',#145292,#87946,#87947);
#75848=AXIS2_PLACEMENT_3D('',#145293,#87948,#87949);
#75849=AXIS2_PLACEMENT_3D('',#145309,#87951,#87952);
#75850=AXIS2_PLACEMENT_3D('',#145317,#87954,#87955);
#75851=AXIS2_PLACEMENT_3D('',#145319,#87956,#87957);
#75852=AXIS2_PLACEMENT_3D('',#145321,#87958,#87959);
#75853=AXIS2_PLACEMENT_3D('',#145322,#87960,#87961);
#75854=AXIS2_PLACEMENT_3D('',#145338,#87963,#87964);
#75855=AXIS2_PLACEMENT_3D('',#145346,#87966,#87967);
#75856=AXIS2_PLACEMENT_3D('',#145348,#87968,#87969);
#75857=AXIS2_PLACEMENT_3D('',#145350,#87970,#87971);
#75858=AXIS2_PLACEMENT_3D('',#145351,#87972,#87973);
#75859=AXIS2_PLACEMENT_3D('',#145367,#87975,#87976);
#75860=AXIS2_PLACEMENT_3D('',#145382,#87978,#87979);
#75861=AXIS2_PLACEMENT_3D('',#145384,#87981,#87982);
#75862=AXIS2_PLACEMENT_3D('',#145386,#87983,#87984);
#75863=AXIS2_PLACEMENT_3D('',#145387,#87985,#87986);
#75864=AXIS2_PLACEMENT_3D('',#145397,#87988,#87989);
#75865=AXIS2_PLACEMENT_3D('',#145404,#87990,#87991);
#75866=AXIS2_PLACEMENT_3D('',#145406,#87992,#87993);
#75867=AXIS2_PLACEMENT_3D('',#145408,#87994,#87995);
#75868=AXIS2_PLACEMENT_3D('',#145409,#87996,#87997);
#75869=AXIS2_PLACEMENT_3D('',#145425,#87999,#88000);
#75870=AXIS2_PLACEMENT_3D('',#145433,#88002,#88003);
#75871=AXIS2_PLACEMENT_3D('',#145435,#88004,#88005);
#75872=AXIS2_PLACEMENT_3D('',#145437,#88006,#88007);
#75873=AXIS2_PLACEMENT_3D('',#145438,#88008,#88009);
#75874=AXIS2_PLACEMENT_3D('',#145454,#88011,#88012);
#75875=AXIS2_PLACEMENT_3D('',#145462,#88014,#88015);
#75876=AXIS2_PLACEMENT_3D('',#145464,#88016,#88017);
#75877=AXIS2_PLACEMENT_3D('',#145466,#88018,#88019);
#75878=AXIS2_PLACEMENT_3D('',#145467,#88020,#88021);
#75879=AXIS2_PLACEMENT_3D('',#145483,#88023,#88024);
#75880=AXIS2_PLACEMENT_3D('',#145491,#88026,#88027);
#75881=AXIS2_PLACEMENT_3D('',#145493,#88028,#88029);
#75882=AXIS2_PLACEMENT_3D('',#145495,#88030,#88031);
#75883=AXIS2_PLACEMENT_3D('',#145496,#88032,#88033);
#75884=AXIS2_PLACEMENT_3D('',#145512,#88035,#88036);
#75885=AXIS2_PLACEMENT_3D('',#145520,#88038,#88039);
#75886=AXIS2_PLACEMENT_3D('',#145522,#88040,#88041);
#75887=AXIS2_PLACEMENT_3D('',#145524,#88042,#88043);
#75888=AXIS2_PLACEMENT_3D('',#145525,#88044,#88045);
#75889=AXIS2_PLACEMENT_3D('',#145541,#88047,#88048);
#75890=AXIS2_PLACEMENT_3D('',#145549,#88050,#88051);
#75891=AXIS2_PLACEMENT_3D('',#145551,#88052,#88053);
#75892=AXIS2_PLACEMENT_3D('',#145553,#88054,#88055);
#75893=AXIS2_PLACEMENT_3D('',#145554,#88056,#88057);
#75894=AXIS2_PLACEMENT_3D('',#145570,#88059,#88060);
#75895=AXIS2_PLACEMENT_3D('',#145578,#88062,#88063);
#75896=AXIS2_PLACEMENT_3D('',#145580,#88064,#88065);
#75897=AXIS2_PLACEMENT_3D('',#145582,#88066,#88067);
#75898=AXIS2_PLACEMENT_3D('',#145583,#88068,#88069);
#75899=AXIS2_PLACEMENT_3D('',#145599,#88071,#88072);
#75900=AXIS2_PLACEMENT_3D('',#145607,#88074,#88075);
#75901=AXIS2_PLACEMENT_3D('',#145609,#88076,#88077);
#75902=AXIS2_PLACEMENT_3D('',#145611,#88078,#88079);
#75903=AXIS2_PLACEMENT_3D('',#145612,#88080,#88081);
#75904=AXIS2_PLACEMENT_3D('',#145628,#88083,#88084);
#75905=AXIS2_PLACEMENT_3D('',#145636,#88086,#88087);
#75906=AXIS2_PLACEMENT_3D('',#145638,#88088,#88089);
#75907=AXIS2_PLACEMENT_3D('',#145640,#88090,#88091);
#75908=AXIS2_PLACEMENT_3D('',#145641,#88092,#88093);
#75909=AXIS2_PLACEMENT_3D('',#145649,#88095,#88096);
#75910=AXIS2_PLACEMENT_3D('',#145652,#88097,#88098);
#75911=AXIS2_PLACEMENT_3D('',#145653,#88099,#88100);
#75912=AXIS2_PLACEMENT_3D('',#145654,#88101,#88102);
#75913=AXIS2_PLACEMENT_3D('',#145676,#88104,#88105);
#75914=AXIS2_PLACEMENT_3D('',#145691,#88108,#88109);
#75915=AXIS2_PLACEMENT_3D('',#145705,#88110,#88111);
#75916=AXIS2_PLACEMENT_3D('',#145707,#88113,#88114);
#75917=AXIS2_PLACEMENT_3D('',#145709,#88115,#88116);
#75918=AXIS2_PLACEMENT_3D('',#145710,#88117,#88118);
#75919=AXIS2_PLACEMENT_3D('',#145724,#88120,#88121);
#75920=AXIS2_PLACEMENT_3D('',#145738,#88122,#88123);
#75921=AXIS2_PLACEMENT_3D('',#145740,#88125,#88126);
#75922=AXIS2_PLACEMENT_3D('',#145742,#88127,#88128);
#75923=AXIS2_PLACEMENT_3D('',#145743,#88129,#88130);
#75924=AXIS2_PLACEMENT_3D('',#145757,#88132,#88133);
#75925=AXIS2_PLACEMENT_3D('',#145771,#88134,#88135);
#75926=AXIS2_PLACEMENT_3D('',#145773,#88137,#88138);
#75927=AXIS2_PLACEMENT_3D('',#145775,#88139,#88140);
#75928=AXIS2_PLACEMENT_3D('',#145776,#88141,#88142);
#75929=AXIS2_PLACEMENT_3D('',#145790,#88144,#88145);
#75930=AXIS2_PLACEMENT_3D('',#145804,#88146,#88147);
#75931=AXIS2_PLACEMENT_3D('',#145806,#88149,#88150);
#75932=AXIS2_PLACEMENT_3D('',#145808,#88151,#88152);
#75933=AXIS2_PLACEMENT_3D('',#145809,#88153,#88154);
#75934=AXIS2_PLACEMENT_3D('',#145823,#88156,#88157);
#75935=AXIS2_PLACEMENT_3D('',#145837,#88158,#88159);
#75936=AXIS2_PLACEMENT_3D('',#145839,#88161,#88162);
#75937=AXIS2_PLACEMENT_3D('',#145841,#88163,#88164);
#75938=AXIS2_PLACEMENT_3D('',#145842,#88165,#88166);
#75939=AXIS2_PLACEMENT_3D('',#145856,#88168,#88169);
#75940=AXIS2_PLACEMENT_3D('',#145870,#88170,#88171);
#75941=AXIS2_PLACEMENT_3D('',#145872,#88173,#88174);
#75942=AXIS2_PLACEMENT_3D('',#145874,#88175,#88176);
#75943=AXIS2_PLACEMENT_3D('',#145875,#88177,#88178);
#75944=AXIS2_PLACEMENT_3D('',#145889,#88180,#88181);
#75945=AXIS2_PLACEMENT_3D('',#145903,#88182,#88183);
#75946=AXIS2_PLACEMENT_3D('',#145905,#88185,#88186);
#75947=AXIS2_PLACEMENT_3D('',#145907,#88187,#88188);
#75948=AXIS2_PLACEMENT_3D('',#145908,#88189,#88190);
#75949=AXIS2_PLACEMENT_3D('',#145922,#88192,#88193);
#75950=AXIS2_PLACEMENT_3D('',#145936,#88194,#88195);
#75951=AXIS2_PLACEMENT_3D('',#145938,#88197,#88198);
#75952=AXIS2_PLACEMENT_3D('',#145940,#88199,#88200);
#75953=AXIS2_PLACEMENT_3D('',#145941,#88201,#88202);
#75954=AXIS2_PLACEMENT_3D('',#145955,#88204,#88205);
#75955=AXIS2_PLACEMENT_3D('',#145969,#88206,#88207);
#75956=AXIS2_PLACEMENT_3D('',#145971,#88209,#88210);
#75957=AXIS2_PLACEMENT_3D('',#145973,#88211,#88212);
#75958=AXIS2_PLACEMENT_3D('',#145974,#88213,#88214);
#75959=AXIS2_PLACEMENT_3D('',#145988,#88216,#88217);
#75960=AXIS2_PLACEMENT_3D('',#146002,#88218,#88219);
#75961=AXIS2_PLACEMENT_3D('',#146004,#88221,#88222);
#75962=AXIS2_PLACEMENT_3D('',#146006,#88223,#88224);
#75963=AXIS2_PLACEMENT_3D('',#146007,#88225,#88226);
#75964=AXIS2_PLACEMENT_3D('',#146021,#88228,#88229);
#75965=AXIS2_PLACEMENT_3D('',#146035,#88230,#88231);
#75966=AXIS2_PLACEMENT_3D('',#146037,#88233,#88234);
#75967=AXIS2_PLACEMENT_3D('',#146039,#88235,#88236);
#75968=AXIS2_PLACEMENT_3D('',#146040,#88237,#88238);
#75969=AXIS2_PLACEMENT_3D('',#146054,#88240,#88241);
#75970=AXIS2_PLACEMENT_3D('',#146068,#88242,#88243);
#75971=AXIS2_PLACEMENT_3D('',#146070,#88245,#88246);
#75972=AXIS2_PLACEMENT_3D('',#146072,#88247,#88248);
#75973=AXIS2_PLACEMENT_3D('',#146073,#88249,#88250);
#75974=AXIS2_PLACEMENT_3D('',#146087,#88252,#88253);
#75975=AXIS2_PLACEMENT_3D('',#146101,#88254,#88255);
#75976=AXIS2_PLACEMENT_3D('',#146103,#88257,#88258);
#75977=AXIS2_PLACEMENT_3D('',#146105,#88259,#88260);
#75978=AXIS2_PLACEMENT_3D('',#146106,#88261,#88262);
#75979=AXIS2_PLACEMENT_3D('',#146144,#88266,#88267);
#75980=AXIS2_PLACEMENT_3D('',#146158,#88268,#88269);
#75981=AXIS2_PLACEMENT_3D('',#146160,#88271,#88272);
#75982=AXIS2_PLACEMENT_3D('',#146162,#88273,#88274);
#75983=AXIS2_PLACEMENT_3D('',#146163,#88275,#88276);
#75984=AXIS2_PLACEMENT_3D('',#146177,#88278,#88279);
#75985=AXIS2_PLACEMENT_3D('',#146191,#88280,#88281);
#75986=AXIS2_PLACEMENT_3D('',#146193,#88283,#88284);
#75987=AXIS2_PLACEMENT_3D('',#146195,#88285,#88286);
#75988=AXIS2_PLACEMENT_3D('',#146196,#88287,#88288);
#75989=AXIS2_PLACEMENT_3D('',#146210,#88290,#88291);
#75990=AXIS2_PLACEMENT_3D('',#146224,#88292,#88293);
#75991=AXIS2_PLACEMENT_3D('',#146226,#88295,#88296);
#75992=AXIS2_PLACEMENT_3D('',#146228,#88297,#88298);
#75993=AXIS2_PLACEMENT_3D('',#146229,#88299,#88300);
#75994=AXIS2_PLACEMENT_3D('',#146243,#88302,#88303);
#75995=AXIS2_PLACEMENT_3D('',#146257,#88304,#88305);
#75996=AXIS2_PLACEMENT_3D('',#146259,#88307,#88308);
#75997=AXIS2_PLACEMENT_3D('',#146261,#88309,#88310);
#75998=AXIS2_PLACEMENT_3D('',#146262,#88311,#88312);
#75999=AXIS2_PLACEMENT_3D('',#146276,#88314,#88315);
#76000=AXIS2_PLACEMENT_3D('',#146290,#88316,#88317);
#76001=AXIS2_PLACEMENT_3D('',#146292,#88319,#88320);
#76002=AXIS2_PLACEMENT_3D('',#146294,#88321,#88322);
#76003=AXIS2_PLACEMENT_3D('',#146295,#88323,#88324);
#76004=AXIS2_PLACEMENT_3D('',#146309,#88326,#88327);
#76005=AXIS2_PLACEMENT_3D('',#146323,#88328,#88329);
#76006=AXIS2_PLACEMENT_3D('',#146325,#88331,#88332);
#76007=AXIS2_PLACEMENT_3D('',#146327,#88333,#88334);
#76008=AXIS2_PLACEMENT_3D('',#146328,#88335,#88336);
#76009=AXIS2_PLACEMENT_3D('',#146342,#88338,#88339);
#76010=AXIS2_PLACEMENT_3D('',#146356,#88340,#88341);
#76011=AXIS2_PLACEMENT_3D('',#146358,#88343,#88344);
#76012=AXIS2_PLACEMENT_3D('',#146360,#88345,#88346);
#76013=AXIS2_PLACEMENT_3D('',#146361,#88347,#88348);
#76014=AXIS2_PLACEMENT_3D('',#146375,#88350,#88351);
#76015=AXIS2_PLACEMENT_3D('',#146389,#88352,#88353);
#76016=AXIS2_PLACEMENT_3D('',#146391,#88355,#88356);
#76017=AXIS2_PLACEMENT_3D('',#146393,#88357,#88358);
#76018=AXIS2_PLACEMENT_3D('',#146394,#88359,#88360);
#76019=AXIS2_PLACEMENT_3D('',#146408,#88362,#88363);
#76020=AXIS2_PLACEMENT_3D('',#146422,#88364,#88365);
#76021=AXIS2_PLACEMENT_3D('',#146424,#88367,#88368);
#76022=AXIS2_PLACEMENT_3D('',#146426,#88369,#88370);
#76023=AXIS2_PLACEMENT_3D('',#146427,#88371,#88372);
#76024=AXIS2_PLACEMENT_3D('',#146441,#88374,#88375);
#76025=AXIS2_PLACEMENT_3D('',#146455,#88376,#88377);
#76026=AXIS2_PLACEMENT_3D('',#146457,#88379,#88380);
#76027=AXIS2_PLACEMENT_3D('',#146459,#88381,#88382);
#76028=AXIS2_PLACEMENT_3D('',#146460,#88383,#88384);
#76029=AXIS2_PLACEMENT_3D('',#146474,#88386,#88387);
#76030=AXIS2_PLACEMENT_3D('',#146488,#88388,#88389);
#76031=AXIS2_PLACEMENT_3D('',#146490,#88391,#88392);
#76032=AXIS2_PLACEMENT_3D('',#146492,#88393,#88394);
#76033=AXIS2_PLACEMENT_3D('',#146493,#88395,#88396);
#76034=AXIS2_PLACEMENT_3D('',#146507,#88398,#88399);
#76035=AXIS2_PLACEMENT_3D('',#146521,#88400,#88401);
#76036=AXIS2_PLACEMENT_3D('',#146523,#88403,#88404);
#76037=AXIS2_PLACEMENT_3D('',#146525,#88405,#88406);
#76038=AXIS2_PLACEMENT_3D('',#146526,#88407,#88408);
#76039=AXIS2_PLACEMENT_3D('',#146540,#88410,#88411);
#76040=AXIS2_PLACEMENT_3D('',#146554,#88412,#88413);
#76041=AXIS2_PLACEMENT_3D('',#146556,#88415,#88416);
#76042=AXIS2_PLACEMENT_3D('',#146558,#88417,#88418);
#76043=AXIS2_PLACEMENT_3D('',#146559,#88419,#88420);
#76044=AXIS2_PLACEMENT_3D('',#146573,#88422,#88423);
#76045=AXIS2_PLACEMENT_3D('',#146587,#88424,#88425);
#76046=AXIS2_PLACEMENT_3D('',#146589,#88427,#88428);
#76047=AXIS2_PLACEMENT_3D('',#146591,#88429,#88430);
#76048=AXIS2_PLACEMENT_3D('',#146592,#88431,#88432);
#76049=AXIS2_PLACEMENT_3D('',#146593,#88433,#88434);
#76050=AXIS2_PLACEMENT_3D('',#146595,#88435,#88436);
#76051=AXIS2_PLACEMENT_3D('',#146597,#88437,#88438);
#76052=AXIS2_PLACEMENT_3D('',#146598,#88439,#88440);
#76053=AXIS2_PLACEMENT_3D('',#146621,#88442,#88443);
#76054=AXIS2_PLACEMENT_3D('',#146680,#88444,#88445);
#76055=AXIS2_PLACEMENT_3D('',#146721,#88446,#88447);
#76056=AXIS2_PLACEMENT_3D('',#146771,#88448,#88449);
#76057=AXIS2_PLACEMENT_3D('',#146812,#88450,#88451);
#76058=AXIS2_PLACEMENT_3D('',#146853,#88452,#88453);
#76059=AXIS2_PLACEMENT_3D('',#146903,#88454,#88455);
#76060=AXIS2_PLACEMENT_3D('',#146953,#88456,#88457);
#76061=AXIS2_PLACEMENT_3D('',#147002,#88458,#88459);
#76062=AXIS2_PLACEMENT_3D('',#147051,#88460,#88461);
#76063=AXIS2_PLACEMENT_3D('',#147101,#88462,#88463);
#76064=AXIS2_PLACEMENT_3D('',#147142,#88464,#88465);
#76065=AXIS2_PLACEMENT_3D('',#147192,#88466,#88467);
#76066=AXIS2_PLACEMENT_3D('',#147236,#88468,#88469);
#76067=AXIS2_PLACEMENT_3D('',#147282,#88470,#88471);
#76068=AXIS2_PLACEMENT_3D('',#147332,#88472,#88473);
#76069=AXIS2_PLACEMENT_3D('',#147378,#88474,#88475);
#76070=AXIS2_PLACEMENT_3D('',#147419,#88476,#88477);
#76071=AXIS2_PLACEMENT_3D('',#147465,#88478,#88479);
#76072=AXIS2_PLACEMENT_3D('',#147515,#88480,#88481);
#76073=AXIS2_PLACEMENT_3D('',#147561,#88482,#88483);
#76074=AXIS2_PLACEMENT_3D('',#147607,#88484,#88485);
#76075=AXIS2_PLACEMENT_3D('',#147657,#88486,#88487);
#76076=AXIS2_PLACEMENT_3D('',#147703,#88488,#88489);
#76077=AXIS2_PLACEMENT_3D('',#147753,#88490,#88491);
#76078=AXIS2_PLACEMENT_3D('',#147802,#88492,#88493);
#76079=AXIS2_PLACEMENT_3D('',#147852,#88494,#88495);
#76080=AXIS2_PLACEMENT_3D('',#147898,#88496,#88497);
#76081=AXIS2_PLACEMENT_3D('',#147948,#88498,#88499);
#76082=AXIS2_PLACEMENT_3D('',#147990,#88500,#88501);
#76083=AXIS2_PLACEMENT_3D('',#148002,#88502,#88503);
#76084=AXIS2_PLACEMENT_3D('',#148015,#88504,#88505);
#76085=AXIS2_PLACEMENT_3D('',#148027,#88506,#88507);
#76086=AXIS2_PLACEMENT_3D('',#148040,#88508,#88509);
#76087=AXIS2_PLACEMENT_3D('',#148052,#88510,#88511);
#76088=AXIS2_PLACEMENT_3D('',#148065,#88512,#88513);
#76089=AXIS2_PLACEMENT_3D('',#148077,#88514,#88515);
#76090=AXIS2_PLACEMENT_3D('',#148090,#88516,#88517);
#76091=AXIS2_PLACEMENT_3D('',#148102,#88518,#88519);
#76092=AXIS2_PLACEMENT_3D('',#148115,#88520,#88521);
#76093=AXIS2_PLACEMENT_3D('',#148127,#88522,#88523);
#76094=AXIS2_PLACEMENT_3D('',#148140,#88524,#88525);
#76095=AXIS2_PLACEMENT_3D('',#148152,#88526,#88527);
#76096=AXIS2_PLACEMENT_3D('',#148165,#88528,#88529);
#76097=AXIS2_PLACEMENT_3D('',#148177,#88530,#88531);
#76098=AXIS2_PLACEMENT_3D('',#148190,#88532,#88533);
#76099=AXIS2_PLACEMENT_3D('',#148202,#88534,#88535);
#76100=AXIS2_PLACEMENT_3D('',#148215,#88536,#88537);
#76101=AXIS2_PLACEMENT_3D('',#148227,#88538,#88539);
#76102=AXIS2_PLACEMENT_3D('',#148240,#88540,#88541);
#76103=AXIS2_PLACEMENT_3D('',#148252,#88542,#88543);
#76104=AXIS2_PLACEMENT_3D('',#148265,#88544,#88545);
#76105=AXIS2_PLACEMENT_3D('',#148277,#88546,#88547);
#76106=AXIS2_PLACEMENT_3D('',#148290,#88548,#88549);
#76107=AXIS2_PLACEMENT_3D('',#148302,#88550,#88551);
#76108=AXIS2_PLACEMENT_3D('',#148315,#88552,#88553);
#76109=AXIS2_PLACEMENT_3D('',#148327,#88554,#88555);
#76110=AXIS2_PLACEMENT_3D('',#148340,#88556,#88557);
#76111=AXIS2_PLACEMENT_3D('',#148352,#88558,#88559);
#76112=AXIS2_PLACEMENT_3D('',#148365,#88560,#88561);
#76113=AXIS2_PLACEMENT_3D('',#148377,#88562,#88563);
#76114=AXIS2_PLACEMENT_3D('',#148390,#88564,#88565);
#76115=AXIS2_PLACEMENT_3D('',#148402,#88566,#88567);
#76116=AXIS2_PLACEMENT_3D('',#148415,#88568,#88569);
#76117=AXIS2_PLACEMENT_3D('',#148427,#88570,#88571);
#76118=AXIS2_PLACEMENT_3D('',#148440,#88572,#88573);
#76119=AXIS2_PLACEMENT_3D('',#148452,#88574,#88575);
#76120=AXIS2_PLACEMENT_3D('',#148465,#88576,#88577);
#76121=AXIS2_PLACEMENT_3D('',#148477,#88578,#88579);
#76122=AXIS2_PLACEMENT_3D('',#148490,#88580,#88581);
#76123=AXIS2_PLACEMENT_3D('',#148502,#88582,#88583);
#76124=AXIS2_PLACEMENT_3D('',#148515,#88584,#88585);
#76125=AXIS2_PLACEMENT_3D('',#148527,#88586,#88587);
#76126=AXIS2_PLACEMENT_3D('',#148540,#88588,#88589);
#76127=AXIS2_PLACEMENT_3D('',#148552,#88590,#88591);
#76128=AXIS2_PLACEMENT_3D('',#148565,#88592,#88593);
#76129=AXIS2_PLACEMENT_3D('',#148577,#88594,#88595);
#76130=AXIS2_PLACEMENT_3D('',#148590,#88596,#88597);
#76131=AXIS2_PLACEMENT_3D('',#148602,#88598,#88599);
#76132=AXIS2_PLACEMENT_3D('',#148615,#88600,#88601);
#76133=AXIS2_PLACEMENT_3D('',#148627,#88602,#88603);
#76134=AXIS2_PLACEMENT_3D('',#148640,#88604,#88605);
#76135=AXIS2_PLACEMENT_3D('',#148652,#88606,#88607);
#76136=AXIS2_PLACEMENT_3D('',#148665,#88608,#88609);
#76137=AXIS2_PLACEMENT_3D('',#148677,#88610,#88611);
#76138=AXIS2_PLACEMENT_3D('',#148690,#88612,#88613);
#76139=AXIS2_PLACEMENT_3D('',#148701,#88614,#88615);
#76140=AXIS2_PLACEMENT_3D('',#148714,#88616,#88617);
#76141=AXIS2_PLACEMENT_3D('',#148722,#88619,#88620);
#76142=AXIS2_PLACEMENT_3D('',#148724,#88621,#88622);
#76143=AXIS2_PLACEMENT_3D('',#148726,#88623,#88624);
#76144=AXIS2_PLACEMENT_3D('',#148757,#88626,#88627);
#76145=AXIS2_PLACEMENT_3D('',#148765,#88629,#88630);
#76146=AXIS2_PLACEMENT_3D('',#148767,#88631,#88632);
#76147=AXIS2_PLACEMENT_3D('',#148769,#88633,#88634);
#76148=AXIS2_PLACEMENT_3D('',#148800,#88636,#88637);
#76149=AXIS2_PLACEMENT_3D('',#148808,#88639,#88640);
#76150=AXIS2_PLACEMENT_3D('',#148810,#88641,#88642);
#76151=AXIS2_PLACEMENT_3D('',#148812,#88643,#88644);
#76152=AXIS2_PLACEMENT_3D('',#148843,#88646,#88647);
#76153=AXIS2_PLACEMENT_3D('',#148851,#88649,#88650);
#76154=AXIS2_PLACEMENT_3D('',#148853,#88651,#88652);
#76155=AXIS2_PLACEMENT_3D('',#148855,#88653,#88654);
#76156=AXIS2_PLACEMENT_3D('',#148886,#88656,#88657);
#76157=AXIS2_PLACEMENT_3D('',#148894,#88659,#88660);
#76158=AXIS2_PLACEMENT_3D('',#148896,#88661,#88662);
#76159=AXIS2_PLACEMENT_3D('',#148898,#88663,#88664);
#76160=AXIS2_PLACEMENT_3D('',#148929,#88666,#88667);
#76161=AXIS2_PLACEMENT_3D('',#148937,#88669,#88670);
#76162=AXIS2_PLACEMENT_3D('',#148939,#88671,#88672);
#76163=AXIS2_PLACEMENT_3D('',#148941,#88673,#88674);
#76164=AXIS2_PLACEMENT_3D('',#148972,#88676,#88677);
#76165=AXIS2_PLACEMENT_3D('',#148980,#88679,#88680);
#76166=AXIS2_PLACEMENT_3D('',#148982,#88681,#88682);
#76167=AXIS2_PLACEMENT_3D('',#148984,#88683,#88684);
#76168=AXIS2_PLACEMENT_3D('',#149015,#88686,#88687);
#76169=AXIS2_PLACEMENT_3D('',#149023,#88689,#88690);
#76170=AXIS2_PLACEMENT_3D('',#149025,#88691,#88692);
#76171=AXIS2_PLACEMENT_3D('',#149027,#88693,#88694);
#76172=AXIS2_PLACEMENT_3D('',#149058,#88696,#88697);
#76173=AXIS2_PLACEMENT_3D('',#149066,#88699,#88700);
#76174=AXIS2_PLACEMENT_3D('',#149068,#88701,#88702);
#76175=AXIS2_PLACEMENT_3D('',#149070,#88703,#88704);
#76176=AXIS2_PLACEMENT_3D('',#149101,#88706,#88707);
#76177=AXIS2_PLACEMENT_3D('',#149109,#88709,#88710);
#76178=AXIS2_PLACEMENT_3D('',#149111,#88711,#88712);
#76179=AXIS2_PLACEMENT_3D('',#149113,#88713,#88714);
#76180=AXIS2_PLACEMENT_3D('',#149144,#88716,#88717);
#76181=AXIS2_PLACEMENT_3D('',#149152,#88719,#88720);
#76182=AXIS2_PLACEMENT_3D('',#149154,#88721,#88722);
#76183=AXIS2_PLACEMENT_3D('',#149156,#88723,#88724);
#76184=AXIS2_PLACEMENT_3D('',#149187,#88726,#88727);
#76185=AXIS2_PLACEMENT_3D('',#149195,#88729,#88730);
#76186=AXIS2_PLACEMENT_3D('',#149197,#88731,#88732);
#76187=AXIS2_PLACEMENT_3D('',#149199,#88733,#88734);
#76188=AXIS2_PLACEMENT_3D('',#149230,#88736,#88737);
#76189=AXIS2_PLACEMENT_3D('',#149238,#88739,#88740);
#76190=AXIS2_PLACEMENT_3D('',#149240,#88741,#88742);
#76191=AXIS2_PLACEMENT_3D('',#149242,#88743,#88744);
#76192=AXIS2_PLACEMENT_3D('',#149273,#88746,#88747);
#76193=AXIS2_PLACEMENT_3D('',#149281,#88749,#88750);
#76194=AXIS2_PLACEMENT_3D('',#149283,#88751,#88752);
#76195=AXIS2_PLACEMENT_3D('',#149285,#88753,#88754);
#76196=AXIS2_PLACEMENT_3D('',#149344,#88758,#88759);
#76197=AXIS2_PLACEMENT_3D('',#149352,#88761,#88762);
#76198=AXIS2_PLACEMENT_3D('',#149354,#88763,#88764);
#76199=AXIS2_PLACEMENT_3D('',#149356,#88765,#88766);
#76200=AXIS2_PLACEMENT_3D('',#149387,#88768,#88769);
#76201=AXIS2_PLACEMENT_3D('',#149395,#88771,#88772);
#76202=AXIS2_PLACEMENT_3D('',#149397,#88773,#88774);
#76203=AXIS2_PLACEMENT_3D('',#149399,#88775,#88776);
#76204=AXIS2_PLACEMENT_3D('',#149430,#88778,#88779);
#76205=AXIS2_PLACEMENT_3D('',#149438,#88781,#88782);
#76206=AXIS2_PLACEMENT_3D('',#149440,#88783,#88784);
#76207=AXIS2_PLACEMENT_3D('',#149442,#88785,#88786);
#76208=AXIS2_PLACEMENT_3D('',#149473,#88788,#88789);
#76209=AXIS2_PLACEMENT_3D('',#149500,#88792,#88793);
#76210=AXIS2_PLACEMENT_3D('',#149502,#88794,#88795);
#76211=AXIS2_PLACEMENT_3D('',#149503,#88796,#88797);
#76212=AXIS2_PLACEMENT_3D('',#149517,#88799,#88800);
#76213=AXIS2_PLACEMENT_3D('',#149524,#88801,#88802);
#76214=AXIS2_PLACEMENT_3D('',#149534,#88803,#88804);
#76215=AXIS2_PLACEMENT_3D('',#149535,#88805,#88806);
#76216=AXIS2_PLACEMENT_3D('',#149559,#88808,#88809);
#76217=AXIS2_PLACEMENT_3D('',#149567,#88811,#88812);
#76218=AXIS2_PLACEMENT_3D('',#149569,#88813,#88814);
#76219=AXIS2_PLACEMENT_3D('',#149571,#88815,#88816);
#76220=AXIS2_PLACEMENT_3D('',#149602,#88818,#88819);
#76221=AXIS2_PLACEMENT_3D('',#149610,#88821,#88822);
#76222=AXIS2_PLACEMENT_3D('',#149612,#88823,#88824);
#76223=AXIS2_PLACEMENT_3D('',#149614,#88825,#88826);
#76224=AXIS2_PLACEMENT_3D('',#149645,#88828,#88829);
#76225=AXIS2_PLACEMENT_3D('',#149653,#88831,#88832);
#76226=AXIS2_PLACEMENT_3D('',#149655,#88833,#88834);
#76227=AXIS2_PLACEMENT_3D('',#149657,#88835,#88836);
#76228=AXIS2_PLACEMENT_3D('',#149688,#88838,#88839);
#76229=AXIS2_PLACEMENT_3D('',#149696,#88841,#88842);
#76230=AXIS2_PLACEMENT_3D('',#149698,#88843,#88844);
#76231=AXIS2_PLACEMENT_3D('',#149700,#88845,#88846);
#76232=AXIS2_PLACEMENT_3D('',#149731,#88848,#88849);
#76233=AXIS2_PLACEMENT_3D('',#149739,#88851,#88852);
#76234=AXIS2_PLACEMENT_3D('',#149741,#88853,#88854);
#76235=AXIS2_PLACEMENT_3D('',#149743,#88855,#88856);
#76236=AXIS2_PLACEMENT_3D('',#149774,#88858,#88859);
#76237=AXIS2_PLACEMENT_3D('',#149782,#88861,#88862);
#76238=AXIS2_PLACEMENT_3D('',#149784,#88863,#88864);
#76239=AXIS2_PLACEMENT_3D('',#149786,#88865,#88866);
#76240=AXIS2_PLACEMENT_3D('',#149817,#88868,#88869);
#76241=AXIS2_PLACEMENT_3D('',#149825,#88871,#88872);
#76242=AXIS2_PLACEMENT_3D('',#149827,#88873,#88874);
#76243=AXIS2_PLACEMENT_3D('',#149829,#88875,#88876);
#76244=AXIS2_PLACEMENT_3D('',#149860,#88878,#88879);
#76245=AXIS2_PLACEMENT_3D('',#149868,#88881,#88882);
#76246=AXIS2_PLACEMENT_3D('',#149870,#88883,#88884);
#76247=AXIS2_PLACEMENT_3D('',#149872,#88885,#88886);
#76248=AXIS2_PLACEMENT_3D('',#149903,#88888,#88889);
#76249=AXIS2_PLACEMENT_3D('',#149911,#88891,#88892);
#76250=AXIS2_PLACEMENT_3D('',#149913,#88893,#88894);
#76251=AXIS2_PLACEMENT_3D('',#149915,#88895,#88896);
#76252=AXIS2_PLACEMENT_3D('',#149947,#88899,#88900);
#76253=AXIS2_PLACEMENT_3D('',#149954,#88901,#88902);
#76254=AXIS2_PLACEMENT_3D('',#149957,#88903,#88904);
#76255=AXIS2_PLACEMENT_3D('',#149959,#88905,#88906);
#76256=AXIS2_PLACEMENT_3D('',#149960,#88907,#88908);
#76257=AXIS2_PLACEMENT_3D('',#149968,#88909,#88910);
#76258=AXIS2_PLACEMENT_3D('',#149970,#88912,#88913);
#76259=AXIS2_PLACEMENT_3D('',#149971,#88914,#88915);
#76260=AXIS2_PLACEMENT_3D('',#149972,#88916,#88917);
#76261=AXIS2_PLACEMENT_3D('',#149986,#88919,#88920);
#76262=AXIS2_PLACEMENT_3D('',#149993,#88921,#88922);
#76263=AXIS2_PLACEMENT_3D('',#149996,#88923,#88924);
#76264=AXIS2_PLACEMENT_3D('',#149998,#88925,#88926);
#76265=AXIS2_PLACEMENT_3D('',#149999,#88927,#88928);
#76266=AXIS2_PLACEMENT_3D('',#150007,#88929,#88930);
#76267=AXIS2_PLACEMENT_3D('',#150009,#88932,#88933);
#76268=AXIS2_PLACEMENT_3D('',#150010,#88934,#88935);
#76269=AXIS2_PLACEMENT_3D('',#150011,#88936,#88937);
#76270=AXIS2_PLACEMENT_3D('',#150025,#88939,#88940);
#76271=AXIS2_PLACEMENT_3D('',#150032,#88941,#88942);
#76272=AXIS2_PLACEMENT_3D('',#150035,#88943,#88944);
#76273=AXIS2_PLACEMENT_3D('',#150037,#88945,#88946);
#76274=AXIS2_PLACEMENT_3D('',#150038,#88947,#88948);
#76275=AXIS2_PLACEMENT_3D('',#150046,#88949,#88950);
#76276=AXIS2_PLACEMENT_3D('',#150048,#88952,#88953);
#76277=AXIS2_PLACEMENT_3D('',#150049,#88954,#88955);
#76278=AXIS2_PLACEMENT_3D('',#150050,#88956,#88957);
#76279=AXIS2_PLACEMENT_3D('',#150064,#88959,#88960);
#76280=AXIS2_PLACEMENT_3D('',#150071,#88961,#88962);
#76281=AXIS2_PLACEMENT_3D('',#150074,#88963,#88964);
#76282=AXIS2_PLACEMENT_3D('',#150076,#88965,#88966);
#76283=AXIS2_PLACEMENT_3D('',#150077,#88967,#88968);
#76284=AXIS2_PLACEMENT_3D('',#150085,#88969,#88970);
#76285=AXIS2_PLACEMENT_3D('',#150087,#88972,#88973);
#76286=AXIS2_PLACEMENT_3D('',#150088,#88974,#88975);
#76287=AXIS2_PLACEMENT_3D('',#150089,#88976,#88977);
#76288=AXIS2_PLACEMENT_3D('',#150103,#88979,#88980);
#76289=AXIS2_PLACEMENT_3D('',#150110,#88981,#88982);
#76290=AXIS2_PLACEMENT_3D('',#150113,#88983,#88984);
#76291=AXIS2_PLACEMENT_3D('',#150115,#88985,#88986);
#76292=AXIS2_PLACEMENT_3D('',#150116,#88987,#88988);
#76293=AXIS2_PLACEMENT_3D('',#150124,#88989,#88990);
#76294=AXIS2_PLACEMENT_3D('',#150126,#88992,#88993);
#76295=AXIS2_PLACEMENT_3D('',#150127,#88994,#88995);
#76296=AXIS2_PLACEMENT_3D('',#150128,#88996,#88997);
#76297=AXIS2_PLACEMENT_3D('',#150142,#88999,#89000);
#76298=AXIS2_PLACEMENT_3D('',#150149,#89001,#89002);
#76299=AXIS2_PLACEMENT_3D('',#150152,#89003,#89004);
#76300=AXIS2_PLACEMENT_3D('',#150154,#89005,#89006);
#76301=AXIS2_PLACEMENT_3D('',#150155,#89007,#89008);
#76302=AXIS2_PLACEMENT_3D('',#150163,#89009,#89010);
#76303=AXIS2_PLACEMENT_3D('',#150165,#89012,#89013);
#76304=AXIS2_PLACEMENT_3D('',#150166,#89014,#89015);
#76305=AXIS2_PLACEMENT_3D('',#150167,#89016,#89017);
#76306=AXIS2_PLACEMENT_3D('',#150181,#89019,#89020);
#76307=AXIS2_PLACEMENT_3D('',#150188,#89021,#89022);
#76308=AXIS2_PLACEMENT_3D('',#150191,#89023,#89024);
#76309=AXIS2_PLACEMENT_3D('',#150193,#89025,#89026);
#76310=AXIS2_PLACEMENT_3D('',#150194,#89027,#89028);
#76311=AXIS2_PLACEMENT_3D('',#150202,#89029,#89030);
#76312=AXIS2_PLACEMENT_3D('',#150204,#89032,#89033);
#76313=AXIS2_PLACEMENT_3D('',#150205,#89034,#89035);
#76314=AXIS2_PLACEMENT_3D('',#150206,#89036,#89037);
#76315=AXIS2_PLACEMENT_3D('',#150220,#89039,#89040);
#76316=AXIS2_PLACEMENT_3D('',#150227,#89041,#89042);
#76317=AXIS2_PLACEMENT_3D('',#150230,#89043,#89044);
#76318=AXIS2_PLACEMENT_3D('',#150232,#89045,#89046);
#76319=AXIS2_PLACEMENT_3D('',#150233,#89047,#89048);
#76320=AXIS2_PLACEMENT_3D('',#150241,#89049,#89050);
#76321=AXIS2_PLACEMENT_3D('',#150243,#89052,#89053);
#76322=AXIS2_PLACEMENT_3D('',#150244,#89054,#89055);
#76323=AXIS2_PLACEMENT_3D('',#150245,#89056,#89057);
#76324=AXIS2_PLACEMENT_3D('',#150259,#89059,#89060);
#76325=AXIS2_PLACEMENT_3D('',#150266,#89061,#89062);
#76326=AXIS2_PLACEMENT_3D('',#150269,#89063,#89064);
#76327=AXIS2_PLACEMENT_3D('',#150271,#89065,#89066);
#76328=AXIS2_PLACEMENT_3D('',#150272,#89067,#89068);
#76329=AXIS2_PLACEMENT_3D('',#150280,#89069,#89070);
#76330=AXIS2_PLACEMENT_3D('',#150282,#89072,#89073);
#76331=AXIS2_PLACEMENT_3D('',#150283,#89074,#89075);
#76332=AXIS2_PLACEMENT_3D('',#150284,#89076,#89077);
#76333=AXIS2_PLACEMENT_3D('',#150298,#89079,#89080);
#76334=AXIS2_PLACEMENT_3D('',#150305,#89081,#89082);
#76335=AXIS2_PLACEMENT_3D('',#150308,#89083,#89084);
#76336=AXIS2_PLACEMENT_3D('',#150310,#89085,#89086);
#76337=AXIS2_PLACEMENT_3D('',#150311,#89087,#89088);
#76338=AXIS2_PLACEMENT_3D('',#150319,#89089,#89090);
#76339=AXIS2_PLACEMENT_3D('',#150321,#89092,#89093);
#76340=AXIS2_PLACEMENT_3D('',#150322,#89094,#89095);
#76341=AXIS2_PLACEMENT_3D('',#150323,#89096,#89097);
#76342=AXIS2_PLACEMENT_3D('',#150337,#89099,#89100);
#76343=AXIS2_PLACEMENT_3D('',#150344,#89101,#89102);
#76344=AXIS2_PLACEMENT_3D('',#150347,#89103,#89104);
#76345=AXIS2_PLACEMENT_3D('',#150349,#89105,#89106);
#76346=AXIS2_PLACEMENT_3D('',#150350,#89107,#89108);
#76347=AXIS2_PLACEMENT_3D('',#150358,#89109,#89110);
#76348=AXIS2_PLACEMENT_3D('',#150360,#89112,#89113);
#76349=AXIS2_PLACEMENT_3D('',#150361,#89114,#89115);
#76350=AXIS2_PLACEMENT_3D('',#150362,#89116,#89117);
#76351=AXIS2_PLACEMENT_3D('',#150376,#89119,#89120);
#76352=AXIS2_PLACEMENT_3D('',#150383,#89121,#89122);
#76353=AXIS2_PLACEMENT_3D('',#150386,#89123,#89124);
#76354=AXIS2_PLACEMENT_3D('',#150388,#89125,#89126);
#76355=AXIS2_PLACEMENT_3D('',#150389,#89127,#89128);
#76356=AXIS2_PLACEMENT_3D('',#150397,#89129,#89130);
#76357=AXIS2_PLACEMENT_3D('',#150399,#89132,#89133);
#76358=AXIS2_PLACEMENT_3D('',#150400,#89134,#89135);
#76359=AXIS2_PLACEMENT_3D('',#150401,#89136,#89137);
#76360=AXIS2_PLACEMENT_3D('',#150415,#89139,#89140);
#76361=AXIS2_PLACEMENT_3D('',#150422,#89141,#89142);
#76362=AXIS2_PLACEMENT_3D('',#150425,#89143,#89144);
#76363=AXIS2_PLACEMENT_3D('',#150427,#89145,#89146);
#76364=AXIS2_PLACEMENT_3D('',#150428,#89147,#89148);
#76365=AXIS2_PLACEMENT_3D('',#150436,#89149,#89150);
#76366=AXIS2_PLACEMENT_3D('',#150438,#89152,#89153);
#76367=AXIS2_PLACEMENT_3D('',#150439,#89154,#89155);
#76368=AXIS2_PLACEMENT_3D('',#150440,#89156,#89157);
#76369=AXIS2_PLACEMENT_3D('',#150454,#89159,#89160);
#76370=AXIS2_PLACEMENT_3D('',#150461,#89161,#89162);
#76371=AXIS2_PLACEMENT_3D('',#150464,#89163,#89164);
#76372=AXIS2_PLACEMENT_3D('',#150466,#89165,#89166);
#76373=AXIS2_PLACEMENT_3D('',#150467,#89167,#89168);
#76374=AXIS2_PLACEMENT_3D('',#150475,#89169,#89170);
#76375=AXIS2_PLACEMENT_3D('',#150477,#89172,#89173);
#76376=AXIS2_PLACEMENT_3D('',#150478,#89174,#89175);
#76377=AXIS2_PLACEMENT_3D('',#150479,#89176,#89177);
#76378=AXIS2_PLACEMENT_3D('',#150493,#89179,#89180);
#76379=AXIS2_PLACEMENT_3D('',#150500,#89181,#89182);
#76380=AXIS2_PLACEMENT_3D('',#150503,#89183,#89184);
#76381=AXIS2_PLACEMENT_3D('',#150505,#89185,#89186);
#76382=AXIS2_PLACEMENT_3D('',#150506,#89187,#89188);
#76383=AXIS2_PLACEMENT_3D('',#150514,#89189,#89190);
#76384=AXIS2_PLACEMENT_3D('',#150516,#89192,#89193);
#76385=AXIS2_PLACEMENT_3D('',#150517,#89194,#89195);
#76386=AXIS2_PLACEMENT_3D('',#150518,#89196,#89197);
#76387=AXIS2_PLACEMENT_3D('',#150532,#89199,#89200);
#76388=AXIS2_PLACEMENT_3D('',#150539,#89201,#89202);
#76389=AXIS2_PLACEMENT_3D('',#150542,#89203,#89204);
#76390=AXIS2_PLACEMENT_3D('',#150544,#89205,#89206);
#76391=AXIS2_PLACEMENT_3D('',#150545,#89207,#89208);
#76392=AXIS2_PLACEMENT_3D('',#150553,#89209,#89210);
#76393=AXIS2_PLACEMENT_3D('',#150555,#89212,#89213);
#76394=AXIS2_PLACEMENT_3D('',#150556,#89214,#89215);
#76395=AXIS2_PLACEMENT_3D('',#150557,#89216,#89217);
#76396=AXIS2_PLACEMENT_3D('',#150571,#89219,#89220);
#76397=AXIS2_PLACEMENT_3D('',#150578,#89221,#89222);
#76398=AXIS2_PLACEMENT_3D('',#150581,#89223,#89224);
#76399=AXIS2_PLACEMENT_3D('',#150583,#89225,#89226);
#76400=AXIS2_PLACEMENT_3D('',#150584,#89227,#89228);
#76401=AXIS2_PLACEMENT_3D('',#150592,#89229,#89230);
#76402=AXIS2_PLACEMENT_3D('',#150594,#89232,#89233);
#76403=AXIS2_PLACEMENT_3D('',#150595,#89234,#89235);
#76404=AXIS2_PLACEMENT_3D('',#150596,#89236,#89237);
#76405=AXIS2_PLACEMENT_3D('',#150610,#89239,#89240);
#76406=AXIS2_PLACEMENT_3D('',#150617,#89241,#89242);
#76407=AXIS2_PLACEMENT_3D('',#150620,#89243,#89244);
#76408=AXIS2_PLACEMENT_3D('',#150622,#89245,#89246);
#76409=AXIS2_PLACEMENT_3D('',#150623,#89247,#89248);
#76410=AXIS2_PLACEMENT_3D('',#150631,#89249,#89250);
#76411=AXIS2_PLACEMENT_3D('',#150633,#89252,#89253);
#76412=AXIS2_PLACEMENT_3D('',#150634,#89254,#89255);
#76413=AXIS2_PLACEMENT_3D('',#150635,#89256,#89257);
#76414=AXIS2_PLACEMENT_3D('',#150649,#89259,#89260);
#76415=AXIS2_PLACEMENT_3D('',#150656,#89261,#89262);
#76416=AXIS2_PLACEMENT_3D('',#150659,#89263,#89264);
#76417=AXIS2_PLACEMENT_3D('',#150661,#89265,#89266);
#76418=AXIS2_PLACEMENT_3D('',#150662,#89267,#89268);
#76419=AXIS2_PLACEMENT_3D('',#150670,#89269,#89270);
#76420=AXIS2_PLACEMENT_3D('',#150672,#89272,#89273);
#76421=AXIS2_PLACEMENT_3D('',#150673,#89274,#89275);
#76422=AXIS2_PLACEMENT_3D('',#150674,#89276,#89277);
#76423=AXIS2_PLACEMENT_3D('',#150688,#89279,#89280);
#76424=AXIS2_PLACEMENT_3D('',#150695,#89281,#89282);
#76425=AXIS2_PLACEMENT_3D('',#150698,#89283,#89284);
#76426=AXIS2_PLACEMENT_3D('',#150700,#89285,#89286);
#76427=AXIS2_PLACEMENT_3D('',#150701,#89287,#89288);
#76428=AXIS2_PLACEMENT_3D('',#150709,#89289,#89290);
#76429=AXIS2_PLACEMENT_3D('',#150711,#89292,#89293);
#76430=AXIS2_PLACEMENT_3D('',#150712,#89294,#89295);
#76431=AXIS2_PLACEMENT_3D('',#150713,#89296,#89297);
#76432=AXIS2_PLACEMENT_3D('',#150727,#89299,#89300);
#76433=AXIS2_PLACEMENT_3D('',#150734,#89301,#89302);
#76434=AXIS2_PLACEMENT_3D('',#150737,#89303,#89304);
#76435=AXIS2_PLACEMENT_3D('',#150739,#89305,#89306);
#76436=AXIS2_PLACEMENT_3D('',#150740,#89307,#89308);
#76437=AXIS2_PLACEMENT_3D('',#150748,#89309,#89310);
#76438=AXIS2_PLACEMENT_3D('',#150750,#89312,#89313);
#76439=AXIS2_PLACEMENT_3D('',#150751,#89314,#89315);
#76440=AXIS2_PLACEMENT_3D('',#150752,#89316,#89317);
#76441=AXIS2_PLACEMENT_3D('',#150790,#89321,#89322);
#76442=AXIS2_PLACEMENT_3D('',#150797,#89323,#89324);
#76443=AXIS2_PLACEMENT_3D('',#150800,#89325,#89326);
#76444=AXIS2_PLACEMENT_3D('',#150802,#89327,#89328);
#76445=AXIS2_PLACEMENT_3D('',#150803,#89329,#89330);
#76446=AXIS2_PLACEMENT_3D('',#150811,#89331,#89332);
#76447=AXIS2_PLACEMENT_3D('',#150813,#89334,#89335);
#76448=AXIS2_PLACEMENT_3D('',#150814,#89336,#89337);
#76449=AXIS2_PLACEMENT_3D('',#150815,#89338,#89339);
#76450=AXIS2_PLACEMENT_3D('',#150829,#89341,#89342);
#76451=AXIS2_PLACEMENT_3D('',#150836,#89343,#89344);
#76452=AXIS2_PLACEMENT_3D('',#150839,#89345,#89346);
#76453=AXIS2_PLACEMENT_3D('',#150841,#89347,#89348);
#76454=AXIS2_PLACEMENT_3D('',#150842,#89349,#89350);
#76455=AXIS2_PLACEMENT_3D('',#150850,#89351,#89352);
#76456=AXIS2_PLACEMENT_3D('',#150852,#89354,#89355);
#76457=AXIS2_PLACEMENT_3D('',#150853,#89356,#89357);
#76458=AXIS2_PLACEMENT_3D('',#150854,#89358,#89359);
#76459=AXIS2_PLACEMENT_3D('',#150868,#89361,#89362);
#76460=AXIS2_PLACEMENT_3D('',#150875,#89363,#89364);
#76461=AXIS2_PLACEMENT_3D('',#150878,#89365,#89366);
#76462=AXIS2_PLACEMENT_3D('',#150880,#89367,#89368);
#76463=AXIS2_PLACEMENT_3D('',#150881,#89369,#89370);
#76464=AXIS2_PLACEMENT_3D('',#150889,#89371,#89372);
#76465=AXIS2_PLACEMENT_3D('',#150891,#89374,#89375);
#76466=AXIS2_PLACEMENT_3D('',#150892,#89376,#89377);
#76467=AXIS2_PLACEMENT_3D('',#150893,#89378,#89379);
#76468=AXIS2_PLACEMENT_3D('',#150907,#89381,#89382);
#76469=AXIS2_PLACEMENT_3D('',#150914,#89383,#89384);
#76470=AXIS2_PLACEMENT_3D('',#150917,#89385,#89386);
#76471=AXIS2_PLACEMENT_3D('',#150919,#89387,#89388);
#76472=AXIS2_PLACEMENT_3D('',#150920,#89389,#89390);
#76473=AXIS2_PLACEMENT_3D('',#150928,#89391,#89392);
#76474=AXIS2_PLACEMENT_3D('',#150930,#89394,#89395);
#76475=AXIS2_PLACEMENT_3D('',#150931,#89396,#89397);
#76476=AXIS2_PLACEMENT_3D('',#150932,#89398,#89399);
#76477=AXIS2_PLACEMENT_3D('',#150946,#89401,#89402);
#76478=AXIS2_PLACEMENT_3D('',#150953,#89403,#89404);
#76479=AXIS2_PLACEMENT_3D('',#150956,#89405,#89406);
#76480=AXIS2_PLACEMENT_3D('',#150958,#89407,#89408);
#76481=AXIS2_PLACEMENT_3D('',#150959,#89409,#89410);
#76482=AXIS2_PLACEMENT_3D('',#150967,#89411,#89412);
#76483=AXIS2_PLACEMENT_3D('',#150969,#89414,#89415);
#76484=AXIS2_PLACEMENT_3D('',#150970,#89416,#89417);
#76485=AXIS2_PLACEMENT_3D('',#150971,#89418,#89419);
#76486=AXIS2_PLACEMENT_3D('',#150985,#89421,#89422);
#76487=AXIS2_PLACEMENT_3D('',#150992,#89423,#89424);
#76488=AXIS2_PLACEMENT_3D('',#150995,#89425,#89426);
#76489=AXIS2_PLACEMENT_3D('',#150997,#89427,#89428);
#76490=AXIS2_PLACEMENT_3D('',#150998,#89429,#89430);
#76491=AXIS2_PLACEMENT_3D('',#151006,#89431,#89432);
#76492=AXIS2_PLACEMENT_3D('',#151008,#89434,#89435);
#76493=AXIS2_PLACEMENT_3D('',#151009,#89436,#89437);
#76494=AXIS2_PLACEMENT_3D('',#151010,#89438,#89439);
#76495=AXIS2_PLACEMENT_3D('',#151024,#89441,#89442);
#76496=AXIS2_PLACEMENT_3D('',#151031,#89443,#89444);
#76497=AXIS2_PLACEMENT_3D('',#151034,#89445,#89446);
#76498=AXIS2_PLACEMENT_3D('',#151036,#89447,#89448);
#76499=AXIS2_PLACEMENT_3D('',#151037,#89449,#89450);
#76500=AXIS2_PLACEMENT_3D('',#151045,#89451,#89452);
#76501=AXIS2_PLACEMENT_3D('',#151047,#89454,#89455);
#76502=AXIS2_PLACEMENT_3D('',#151048,#89456,#89457);
#76503=AXIS2_PLACEMENT_3D('',#151049,#89458,#89459);
#76504=AXIS2_PLACEMENT_3D('',#151061,#89460,#89461);
#76505=AXIS2_PLACEMENT_3D('',#151078,#89462,#89463);
#76506=AXIS2_PLACEMENT_3D('',#151090,#89464,#89465);
#76507=AXIS2_PLACEMENT_3D('',#151107,#89466,#89467);
#76508=AXIS2_PLACEMENT_3D('',#151119,#89468,#89469);
#76509=AXIS2_PLACEMENT_3D('',#151136,#89470,#89471);
#76510=AXIS2_PLACEMENT_3D('',#151148,#89472,#89473);
#76511=AXIS2_PLACEMENT_3D('',#151170,#89474,#89475);
#76512=AXIS2_PLACEMENT_3D('',#151182,#89476,#89477);
#76513=AXIS2_PLACEMENT_3D('',#151204,#89478,#89479);
#76514=AXIS2_PLACEMENT_3D('',#151216,#89480,#89481);
#76515=AXIS2_PLACEMENT_3D('',#151233,#89482,#89483);
#76516=AXIS2_PLACEMENT_3D('',#151245,#89484,#89485);
#76517=AXIS2_PLACEMENT_3D('',#151262,#89486,#89487);
#76518=AXIS2_PLACEMENT_3D('',#151274,#89488,#89489);
#76519=AXIS2_PLACEMENT_3D('',#151291,#89490,#89491);
#76520=AXIS2_PLACEMENT_3D('',#151303,#89492,#89493);
#76521=AXIS2_PLACEMENT_3D('',#151320,#89494,#89495);
#76522=AXIS2_PLACEMENT_3D('',#151332,#89496,#89497);
#76523=AXIS2_PLACEMENT_3D('',#151349,#89498,#89499);
#76524=AXIS2_PLACEMENT_3D('',#151361,#89500,#89501);
#76525=AXIS2_PLACEMENT_3D('',#151383,#89502,#89503);
#76526=AXIS2_PLACEMENT_3D('',#151395,#89504,#89505);
#76527=AXIS2_PLACEMENT_3D('',#151412,#89506,#89507);
#76528=AXIS2_PLACEMENT_3D('',#151424,#89508,#89509);
#76529=AXIS2_PLACEMENT_3D('',#151441,#89510,#89511);
#76530=AXIS2_PLACEMENT_3D('',#151453,#89512,#89513);
#76531=AXIS2_PLACEMENT_3D('',#151470,#89514,#89515);
#76532=AXIS2_PLACEMENT_3D('',#151482,#89516,#89517);
#76533=AXIS2_PLACEMENT_3D('',#151504,#89518,#89519);
#76534=AXIS2_PLACEMENT_3D('',#151516,#89520,#89521);
#76535=AXIS2_PLACEMENT_3D('',#151533,#89522,#89523);
#76536=AXIS2_PLACEMENT_3D('',#151545,#89524,#89525);
#76537=AXIS2_PLACEMENT_3D('',#151562,#89526,#89527);
#76538=AXIS2_PLACEMENT_3D('',#151574,#89528,#89529);
#76539=AXIS2_PLACEMENT_3D('',#151591,#89530,#89531);
#76540=AXIS2_PLACEMENT_3D('',#151603,#89532,#89533);
#76541=AXIS2_PLACEMENT_3D('',#151620,#89534,#89535);
#76542=AXIS2_PLACEMENT_3D('',#151632,#89536,#89537);
#76543=AXIS2_PLACEMENT_3D('',#151649,#89538,#89539);
#76544=AXIS2_PLACEMENT_3D('',#151661,#89540,#89541);
#76545=AXIS2_PLACEMENT_3D('',#151678,#89542,#89543);
#76546=AXIS2_PLACEMENT_3D('',#151690,#89544,#89545);
#76547=AXIS2_PLACEMENT_3D('',#151707,#89546,#89547);
#76548=AXIS2_PLACEMENT_3D('',#151719,#89548,#89549);
#76549=AXIS2_PLACEMENT_3D('',#151736,#89550,#89551);
#76550=AXIS2_PLACEMENT_3D('',#151748,#89552,#89553);
#76551=AXIS2_PLACEMENT_3D('',#151770,#89554,#89555);
#76552=AXIS2_PLACEMENT_3D('',#151782,#89556,#89557);
#76553=AXIS2_PLACEMENT_3D('',#151799,#89558,#89559);
#76554=AXIS2_PLACEMENT_3D('',#151811,#89560,#89561);
#76555=AXIS2_PLACEMENT_3D('',#151828,#89562,#89563);
#76556=AXIS2_PLACEMENT_3D('',#151840,#89564,#89565);
#76557=AXIS2_PLACEMENT_3D('',#151857,#89566,#89567);
#76558=AXIS2_PLACEMENT_3D('',#151869,#89568,#89569);
#76559=AXIS2_PLACEMENT_3D('',#151886,#89570,#89571);
#76560=AXIS2_PLACEMENT_3D('',#151898,#89572,#89573);
#76561=AXIS2_PLACEMENT_3D('',#151920,#89574,#89575);
#76562=AXIS2_PLACEMENT_3D('',#151932,#89576,#89577);
#76563=AXIS2_PLACEMENT_3D('',#151933,#89578,#89579);
#76564=AXIS2_PLACEMENT_3D('',#151940,#89580,#89581);
#76565=AXIS2_PLACEMENT_3D('',#151952,#89582,#89583);
#76566=AXIS2_PLACEMENT_3D('',#151953,#89584,#89585);
#76567=AXIS2_PLACEMENT_3D('',#151960,#89586,#89587);
#76568=AXIS2_PLACEMENT_3D('',#151972,#89588,#89589);
#76569=AXIS2_PLACEMENT_3D('',#151973,#89590,#89591);
#76570=AXIS2_PLACEMENT_3D('',#151980,#89592,#89593);
#76571=AXIS2_PLACEMENT_3D('',#151992,#89594,#89595);
#76572=AXIS2_PLACEMENT_3D('',#151993,#89596,#89597);
#76573=AXIS2_PLACEMENT_3D('',#152000,#89598,#89599);
#76574=AXIS2_PLACEMENT_3D('',#152012,#89600,#89601);
#76575=AXIS2_PLACEMENT_3D('',#152013,#89602,#89603);
#76576=AXIS2_PLACEMENT_3D('',#152020,#89604,#89605);
#76577=AXIS2_PLACEMENT_3D('',#152032,#89606,#89607);
#76578=AXIS2_PLACEMENT_3D('',#152033,#89608,#89609);
#76579=AXIS2_PLACEMENT_3D('',#152040,#89610,#89611);
#76580=AXIS2_PLACEMENT_3D('',#152052,#89612,#89613);
#76581=AXIS2_PLACEMENT_3D('',#152053,#89614,#89615);
#76582=AXIS2_PLACEMENT_3D('',#152060,#89616,#89617);
#76583=AXIS2_PLACEMENT_3D('',#152072,#89618,#89619);
#76584=AXIS2_PLACEMENT_3D('',#152073,#89620,#89621);
#76585=AXIS2_PLACEMENT_3D('',#152080,#89622,#89623);
#76586=AXIS2_PLACEMENT_3D('',#152092,#89624,#89625);
#76587=AXIS2_PLACEMENT_3D('',#152093,#89626,#89627);
#76588=AXIS2_PLACEMENT_3D('',#152100,#89628,#89629);
#76589=AXIS2_PLACEMENT_3D('',#152112,#89630,#89631);
#76590=AXIS2_PLACEMENT_3D('',#152113,#89632,#89633);
#76591=AXIS2_PLACEMENT_3D('',#152120,#89634,#89635);
#76592=AXIS2_PLACEMENT_3D('',#152132,#89636,#89637);
#76593=AXIS2_PLACEMENT_3D('',#152133,#89638,#89639);
#76594=AXIS2_PLACEMENT_3D('',#152140,#89640,#89641);
#76595=AXIS2_PLACEMENT_3D('',#152152,#89642,#89643);
#76596=AXIS2_PLACEMENT_3D('',#152153,#89644,#89645);
#76597=AXIS2_PLACEMENT_3D('',#152160,#89646,#89647);
#76598=AXIS2_PLACEMENT_3D('',#152172,#89648,#89649);
#76599=AXIS2_PLACEMENT_3D('',#152173,#89650,#89651);
#76600=AXIS2_PLACEMENT_3D('',#152180,#89652,#89653);
#76601=AXIS2_PLACEMENT_3D('',#152192,#89654,#89655);
#76602=AXIS2_PLACEMENT_3D('',#152193,#89656,#89657);
#76603=AXIS2_PLACEMENT_3D('',#152200,#89658,#89659);
#76604=AXIS2_PLACEMENT_3D('',#152212,#89660,#89661);
#76605=AXIS2_PLACEMENT_3D('',#152213,#89662,#89663);
#76606=AXIS2_PLACEMENT_3D('',#152220,#89664,#89665);
#76607=AXIS2_PLACEMENT_3D('',#152232,#89666,#89667);
#76608=AXIS2_PLACEMENT_3D('',#152233,#89668,#89669);
#76609=AXIS2_PLACEMENT_3D('',#152240,#89670,#89671);
#76610=AXIS2_PLACEMENT_3D('',#152252,#89672,#89673);
#76611=AXIS2_PLACEMENT_3D('',#152253,#89674,#89675);
#76612=AXIS2_PLACEMENT_3D('',#152260,#89676,#89677);
#76613=AXIS2_PLACEMENT_3D('',#152272,#89678,#89679);
#76614=AXIS2_PLACEMENT_3D('',#152273,#89680,#89681);
#76615=AXIS2_PLACEMENT_3D('',#152280,#89682,#89683);
#76616=AXIS2_PLACEMENT_3D('',#152292,#89684,#89685);
#76617=AXIS2_PLACEMENT_3D('',#152293,#89686,#89687);
#76618=AXIS2_PLACEMENT_3D('',#152300,#89688,#89689);
#76619=AXIS2_PLACEMENT_3D('',#152312,#89690,#89691);
#76620=AXIS2_PLACEMENT_3D('',#152313,#89692,#89693);
#76621=AXIS2_PLACEMENT_3D('',#152320,#89694,#89695);
#76622=AXIS2_PLACEMENT_3D('',#152332,#89696,#89697);
#76623=AXIS2_PLACEMENT_3D('',#152333,#89698,#89699);
#76624=AXIS2_PLACEMENT_3D('',#152340,#89700,#89701);
#76625=AXIS2_PLACEMENT_3D('',#152352,#89702,#89703);
#76626=AXIS2_PLACEMENT_3D('',#152353,#89704,#89705);
#76627=AXIS2_PLACEMENT_3D('',#152360,#89706,#89707);
#76628=AXIS2_PLACEMENT_3D('',#152372,#89708,#89709);
#76629=AXIS2_PLACEMENT_3D('',#152373,#89710,#89711);
#76630=AXIS2_PLACEMENT_3D('',#152380,#89712,#89713);
#76631=AXIS2_PLACEMENT_3D('',#152392,#89714,#89715);
#76632=AXIS2_PLACEMENT_3D('',#152393,#89716,#89717);
#76633=AXIS2_PLACEMENT_3D('',#152400,#89718,#89719);
#76634=AXIS2_PLACEMENT_3D('',#152412,#89720,#89721);
#76635=AXIS2_PLACEMENT_3D('',#152413,#89722,#89723);
#76636=AXIS2_PLACEMENT_3D('',#152420,#89724,#89725);
#76637=AXIS2_PLACEMENT_3D('',#152432,#89726,#89727);
#76638=AXIS2_PLACEMENT_3D('',#152433,#89728,#89729);
#76639=AXIS2_PLACEMENT_3D('',#152440,#89730,#89731);
#76640=AXIS2_PLACEMENT_3D('',#152452,#89732,#89733);
#76641=AXIS2_PLACEMENT_3D('',#152453,#89734,#89735);
#76642=AXIS2_PLACEMENT_3D('',#152460,#89736,#89737);
#76643=AXIS2_PLACEMENT_3D('',#152472,#89738,#89739);
#76644=AXIS2_PLACEMENT_3D('',#152473,#89740,#89741);
#76645=AXIS2_PLACEMENT_3D('',#152480,#89742,#89743);
#76646=AXIS2_PLACEMENT_3D('',#152492,#89744,#89745);
#76647=AXIS2_PLACEMENT_3D('',#152493,#89746,#89747);
#76648=AXIS2_PLACEMENT_3D('',#152500,#89748,#89749);
#76649=AXIS2_PLACEMENT_3D('',#152513,#89750,#89751);
#76650=AXIS2_PLACEMENT_3D('',#152537,#89753,#89754);
#76651=AXIS2_PLACEMENT_3D('',#152545,#89756,#89757);
#76652=AXIS2_PLACEMENT_3D('',#152547,#89758,#89759);
#76653=AXIS2_PLACEMENT_3D('',#152549,#89760,#89761);
#76654=AXIS2_PLACEMENT_3D('',#152550,#89762,#89763);
#76655=AXIS2_PLACEMENT_3D('',#152578,#89765,#89766);
#76656=AXIS2_PLACEMENT_3D('',#152586,#89768,#89769);
#76657=AXIS2_PLACEMENT_3D('',#152588,#89770,#89771);
#76658=AXIS2_PLACEMENT_3D('',#152590,#89772,#89773);
#76659=AXIS2_PLACEMENT_3D('',#152591,#89774,#89775);
#76660=AXIS2_PLACEMENT_3D('',#152619,#89777,#89778);
#76661=AXIS2_PLACEMENT_3D('',#152627,#89780,#89781);
#76662=AXIS2_PLACEMENT_3D('',#152629,#89782,#89783);
#76663=AXIS2_PLACEMENT_3D('',#152631,#89784,#89785);
#76664=AXIS2_PLACEMENT_3D('',#152632,#89786,#89787);
#76665=AXIS2_PLACEMENT_3D('',#152660,#89789,#89790);
#76666=AXIS2_PLACEMENT_3D('',#152668,#89792,#89793);
#76667=AXIS2_PLACEMENT_3D('',#152670,#89794,#89795);
#76668=AXIS2_PLACEMENT_3D('',#152672,#89796,#89797);
#76669=AXIS2_PLACEMENT_3D('',#152673,#89798,#89799);
#76670=AXIS2_PLACEMENT_3D('',#152701,#89801,#89802);
#76671=AXIS2_PLACEMENT_3D('',#152709,#89804,#89805);
#76672=AXIS2_PLACEMENT_3D('',#152711,#89806,#89807);
#76673=AXIS2_PLACEMENT_3D('',#152713,#89808,#89809);
#76674=AXIS2_PLACEMENT_3D('',#152714,#89810,#89811);
#76675=AXIS2_PLACEMENT_3D('',#152742,#89813,#89814);
#76676=AXIS2_PLACEMENT_3D('',#152750,#89816,#89817);
#76677=AXIS2_PLACEMENT_3D('',#152752,#89818,#89819);
#76678=AXIS2_PLACEMENT_3D('',#152754,#89820,#89821);
#76679=AXIS2_PLACEMENT_3D('',#152755,#89822,#89823);
#76680=AXIS2_PLACEMENT_3D('',#152815,#89827,#89828);
#76681=AXIS2_PLACEMENT_3D('',#152823,#89830,#89831);
#76682=AXIS2_PLACEMENT_3D('',#152825,#89832,#89833);
#76683=AXIS2_PLACEMENT_3D('',#152827,#89834,#89835);
#76684=AXIS2_PLACEMENT_3D('',#152828,#89836,#89837);
#76685=AXIS2_PLACEMENT_3D('',#152856,#89839,#89840);
#76686=AXIS2_PLACEMENT_3D('',#152864,#89842,#89843);
#76687=AXIS2_PLACEMENT_3D('',#152866,#89844,#89845);
#76688=AXIS2_PLACEMENT_3D('',#152868,#89846,#89847);
#76689=AXIS2_PLACEMENT_3D('',#152869,#89848,#89849);
#76690=AXIS2_PLACEMENT_3D('',#152897,#89851,#89852);
#76691=AXIS2_PLACEMENT_3D('',#152905,#89854,#89855);
#76692=AXIS2_PLACEMENT_3D('',#152907,#89856,#89857);
#76693=AXIS2_PLACEMENT_3D('',#152909,#89858,#89859);
#76694=AXIS2_PLACEMENT_3D('',#152910,#89860,#89861);
#76695=AXIS2_PLACEMENT_3D('',#152938,#89863,#89864);
#76696=AXIS2_PLACEMENT_3D('',#152946,#89866,#89867);
#76697=AXIS2_PLACEMENT_3D('',#152948,#89868,#89869);
#76698=AXIS2_PLACEMENT_3D('',#152950,#89870,#89871);
#76699=AXIS2_PLACEMENT_3D('',#152951,#89872,#89873);
#76700=AXIS2_PLACEMENT_3D('',#152979,#89875,#89876);
#76701=AXIS2_PLACEMENT_3D('',#152987,#89878,#89879);
#76702=AXIS2_PLACEMENT_3D('',#152989,#89880,#89881);
#76703=AXIS2_PLACEMENT_3D('',#152991,#89882,#89883);
#76704=AXIS2_PLACEMENT_3D('',#152992,#89884,#89885);
#76705=AXIS2_PLACEMENT_3D('',#153020,#89887,#89888);
#76706=AXIS2_PLACEMENT_3D('',#153028,#89890,#89891);
#76707=AXIS2_PLACEMENT_3D('',#153030,#89892,#89893);
#76708=AXIS2_PLACEMENT_3D('',#153032,#89894,#89895);
#76709=AXIS2_PLACEMENT_3D('',#153033,#89896,#89897);
#76710=AXIS2_PLACEMENT_3D('',#153061,#89899,#89900);
#76711=AXIS2_PLACEMENT_3D('',#153069,#89902,#89903);
#76712=AXIS2_PLACEMENT_3D('',#153071,#89904,#89905);
#76713=AXIS2_PLACEMENT_3D('',#153073,#89906,#89907);
#76714=AXIS2_PLACEMENT_3D('',#153074,#89908,#89909);
#76715=AXIS2_PLACEMENT_3D('',#153102,#89911,#89912);
#76716=AXIS2_PLACEMENT_3D('',#153110,#89914,#89915);
#76717=AXIS2_PLACEMENT_3D('',#153112,#89916,#89917);
#76718=AXIS2_PLACEMENT_3D('',#153114,#89918,#89919);
#76719=AXIS2_PLACEMENT_3D('',#153115,#89920,#89921);
#76720=AXIS2_PLACEMENT_3D('',#153143,#89923,#89924);
#76721=AXIS2_PLACEMENT_3D('',#153151,#89926,#89927);
#76722=AXIS2_PLACEMENT_3D('',#153153,#89928,#89929);
#76723=AXIS2_PLACEMENT_3D('',#153155,#89930,#89931);
#76724=AXIS2_PLACEMENT_3D('',#153156,#89932,#89933);
#76725=AXIS2_PLACEMENT_3D('',#153184,#89935,#89936);
#76726=AXIS2_PLACEMENT_3D('',#153192,#89938,#89939);
#76727=AXIS2_PLACEMENT_3D('',#153194,#89940,#89941);
#76728=AXIS2_PLACEMENT_3D('',#153196,#89942,#89943);
#76729=AXIS2_PLACEMENT_3D('',#153197,#89944,#89945);
#76730=AXIS2_PLACEMENT_3D('',#153225,#89947,#89948);
#76731=AXIS2_PLACEMENT_3D('',#153244,#89950,#89951);
#76732=AXIS2_PLACEMENT_3D('',#153246,#89953,#89954);
#76733=AXIS2_PLACEMENT_3D('',#153248,#89955,#89956);
#76734=AXIS2_PLACEMENT_3D('',#153249,#89957,#89958);
#76735=AXIS2_PLACEMENT_3D('',#153267,#89960,#89961);
#76736=AXIS2_PLACEMENT_3D('',#153274,#89962,#89963);
#76737=AXIS2_PLACEMENT_3D('',#153276,#89964,#89965);
#76738=AXIS2_PLACEMENT_3D('',#153278,#89966,#89967);
#76739=AXIS2_PLACEMENT_3D('',#153279,#89968,#89969);
#76740=AXIS2_PLACEMENT_3D('',#153307,#89971,#89972);
#76741=AXIS2_PLACEMENT_3D('',#153315,#89974,#89975);
#76742=AXIS2_PLACEMENT_3D('',#153317,#89976,#89977);
#76743=AXIS2_PLACEMENT_3D('',#153319,#89978,#89979);
#76744=AXIS2_PLACEMENT_3D('',#153320,#89980,#89981);
#76745=AXIS2_PLACEMENT_3D('',#153348,#89983,#89984);
#76746=AXIS2_PLACEMENT_3D('',#153356,#89986,#89987);
#76747=AXIS2_PLACEMENT_3D('',#153358,#89988,#89989);
#76748=AXIS2_PLACEMENT_3D('',#153360,#89990,#89991);
#76749=AXIS2_PLACEMENT_3D('',#153361,#89992,#89993);
#76750=AXIS2_PLACEMENT_3D('',#153389,#89995,#89996);
#76751=AXIS2_PLACEMENT_3D('',#153397,#89998,#89999);
#76752=AXIS2_PLACEMENT_3D('',#153399,#90000,#90001);
#76753=AXIS2_PLACEMENT_3D('',#153401,#90002,#90003);
#76754=AXIS2_PLACEMENT_3D('',#153402,#90004,#90005);
#76755=AXIS2_PLACEMENT_3D('',#153430,#90007,#90008);
#76756=AXIS2_PLACEMENT_3D('',#153438,#90010,#90011);
#76757=AXIS2_PLACEMENT_3D('',#153440,#90012,#90013);
#76758=AXIS2_PLACEMENT_3D('',#153442,#90014,#90015);
#76759=AXIS2_PLACEMENT_3D('',#153443,#90016,#90017);
#76760=AXIS2_PLACEMENT_3D('',#153471,#90019,#90020);
#76761=AXIS2_PLACEMENT_3D('',#153479,#90022,#90023);
#76762=AXIS2_PLACEMENT_3D('',#153481,#90024,#90025);
#76763=AXIS2_PLACEMENT_3D('',#153483,#90026,#90027);
#76764=AXIS2_PLACEMENT_3D('',#153484,#90028,#90029);
#76765=AXIS2_PLACEMENT_3D('',#153512,#90031,#90032);
#76766=AXIS2_PLACEMENT_3D('',#153520,#90034,#90035);
#76767=AXIS2_PLACEMENT_3D('',#153522,#90036,#90037);
#76768=AXIS2_PLACEMENT_3D('',#153524,#90038,#90039);
#76769=AXIS2_PLACEMENT_3D('',#153525,#90040,#90041);
#76770=AXIS2_PLACEMENT_3D('',#153553,#90043,#90044);
#76771=AXIS2_PLACEMENT_3D('',#153561,#90046,#90047);
#76772=AXIS2_PLACEMENT_3D('',#153563,#90048,#90049);
#76773=AXIS2_PLACEMENT_3D('',#153565,#90050,#90051);
#76774=AXIS2_PLACEMENT_3D('',#153566,#90052,#90053);
#76775=AXIS2_PLACEMENT_3D('',#153594,#90055,#90056);
#76776=AXIS2_PLACEMENT_3D('',#153602,#90058,#90059);
#76777=AXIS2_PLACEMENT_3D('',#153604,#90060,#90061);
#76778=AXIS2_PLACEMENT_3D('',#153606,#90062,#90063);
#76779=AXIS2_PLACEMENT_3D('',#153607,#90064,#90065);
#76780=AXIS2_PLACEMENT_3D('',#153635,#90067,#90068);
#76781=AXIS2_PLACEMENT_3D('',#153643,#90070,#90071);
#76782=AXIS2_PLACEMENT_3D('',#153645,#90072,#90073);
#76783=AXIS2_PLACEMENT_3D('',#153647,#90074,#90075);
#76784=AXIS2_PLACEMENT_3D('',#153648,#90076,#90077);
#76785=AXIS2_PLACEMENT_3D('',#153660,#90079,#90080);
#76786=AXIS2_PLACEMENT_3D('',#153663,#90081,#90082);
#76787=AXIS2_PLACEMENT_3D('',#153664,#90083,#90084);
#76788=AXIS2_PLACEMENT_3D('',#153665,#90085,#90086);
#76789=AXIS2_PLACEMENT_3D('',#153729,#90090,#90091);
#76790=AXIS2_PLACEMENT_3D('',#153788,#90094,#90095);
#76791=AXIS2_PLACEMENT_3D('',#153847,#90098,#90099);
#76792=AXIS2_PLACEMENT_3D('',#153906,#90102,#90103);
#76793=AXIS2_PLACEMENT_3D('',#153965,#90106,#90107);
#76794=AXIS2_PLACEMENT_3D('',#154024,#90110,#90111);
#76795=AXIS2_PLACEMENT_3D('',#154083,#90114,#90115);
#76796=AXIS2_PLACEMENT_3D('',#154142,#90118,#90119);
#76797=AXIS2_PLACEMENT_3D('',#154201,#90122,#90123);
#76798=AXIS2_PLACEMENT_3D('',#154260,#90126,#90127);
#76799=AXIS2_PLACEMENT_3D('',#154319,#90130,#90131);
#76800=AXIS2_PLACEMENT_3D('',#154378,#90134,#90135);
#76801=AXIS2_PLACEMENT_3D('',#154437,#90138,#90139);
#76802=AXIS2_PLACEMENT_3D('',#154522,#90144,#90145);
#76803=AXIS2_PLACEMENT_3D('',#154581,#90148,#90149);
#76804=AXIS2_PLACEMENT_3D('',#154640,#90152,#90153);
#76805=AXIS2_PLACEMENT_3D('',#154699,#90156,#90157);
#76806=AXIS2_PLACEMENT_3D('',#154758,#90160,#90161);
#76807=AXIS2_PLACEMENT_3D('',#154817,#90164,#90165);
#76808=AXIS2_PLACEMENT_3D('',#154902,#90170,#90171);
#76809=AXIS2_PLACEMENT_3D('',#154961,#90174,#90175);
#76810=AXIS2_PLACEMENT_3D('',#155020,#90178,#90179);
#76811=AXIS2_PLACEMENT_3D('',#155079,#90182,#90183);
#76812=AXIS2_PLACEMENT_3D('',#155138,#90186,#90187);
#76813=AXIS2_PLACEMENT_3D('',#155197,#90190,#90191);
#76814=AXIS2_PLACEMENT_3D('',#155256,#90194,#90195);
#76815=AXIS2_PLACEMENT_3D('',#155291,#90197,#90198);
#76816=AXIS2_PLACEMENT_3D('',#155333,#90200,#90201);
#76817=AXIS2_PLACEMENT_3D('',#155347,#90202,#90203);
#76818=AXIS2_PLACEMENT_3D('',#155360,#90204,#90205);
#76819=AXIS2_PLACEMENT_3D('',#155368,#90206,#90207);
#76820=AXIS2_PLACEMENT_3D('',#155381,#90208,#90209);
#76821=AXIS2_PLACEMENT_3D('',#155389,#90210,#90211);
#76822=AXIS2_PLACEMENT_3D('',#155402,#90212,#90213);
#76823=AXIS2_PLACEMENT_3D('',#155410,#90214,#90215);
#76824=AXIS2_PLACEMENT_3D('',#155423,#90216,#90217);
#76825=AXIS2_PLACEMENT_3D('',#155431,#90218,#90219);
#76826=AXIS2_PLACEMENT_3D('',#155444,#90220,#90221);
#76827=AXIS2_PLACEMENT_3D('',#155452,#90222,#90223);
#76828=AXIS2_PLACEMENT_3D('',#155465,#90224,#90225);
#76829=AXIS2_PLACEMENT_3D('',#155473,#90226,#90227);
#76830=AXIS2_PLACEMENT_3D('',#155486,#90228,#90229);
#76831=AXIS2_PLACEMENT_3D('',#155494,#90230,#90231);
#76832=AXIS2_PLACEMENT_3D('',#155507,#90232,#90233);
#76833=AXIS2_PLACEMENT_3D('',#155515,#90234,#90235);
#76834=AXIS2_PLACEMENT_3D('',#155528,#90236,#90237);
#76835=AXIS2_PLACEMENT_3D('',#155536,#90238,#90239);
#76836=AXIS2_PLACEMENT_3D('',#155549,#90240,#90241);
#76837=AXIS2_PLACEMENT_3D('',#155557,#90242,#90243);
#76838=AXIS2_PLACEMENT_3D('',#155570,#90244,#90245);
#76839=AXIS2_PLACEMENT_3D('',#155578,#90246,#90247);
#76840=AXIS2_PLACEMENT_3D('',#155591,#90248,#90249);
#76841=AXIS2_PLACEMENT_3D('',#155599,#90250,#90251);
#76842=AXIS2_PLACEMENT_3D('',#155612,#90252,#90253);
#76843=AXIS2_PLACEMENT_3D('',#155620,#90254,#90255);
#76844=AXIS2_PLACEMENT_3D('',#155633,#90256,#90257);
#76845=AXIS2_PLACEMENT_3D('',#155641,#90258,#90259);
#76846=AXIS2_PLACEMENT_3D('',#155654,#90260,#90261);
#76847=AXIS2_PLACEMENT_3D('',#155662,#90262,#90263);
#76848=AXIS2_PLACEMENT_3D('',#155675,#90264,#90265);
#76849=AXIS2_PLACEMENT_3D('',#155683,#90266,#90267);
#76850=AXIS2_PLACEMENT_3D('',#155696,#90268,#90269);
#76851=AXIS2_PLACEMENT_3D('',#155704,#90270,#90271);
#76852=AXIS2_PLACEMENT_3D('',#155717,#90272,#90273);
#76853=AXIS2_PLACEMENT_3D('',#155725,#90274,#90275);
#76854=AXIS2_PLACEMENT_3D('',#155738,#90276,#90277);
#76855=AXIS2_PLACEMENT_3D('',#155746,#90278,#90279);
#76856=AXIS2_PLACEMENT_3D('',#155759,#90280,#90281);
#76857=AXIS2_PLACEMENT_3D('',#155767,#90282,#90283);
#76858=AXIS2_PLACEMENT_3D('',#155780,#90284,#90285);
#76859=AXIS2_PLACEMENT_3D('',#155788,#90286,#90287);
#76860=AXIS2_PLACEMENT_3D('',#155801,#90288,#90289);
#76861=AXIS2_PLACEMENT_3D('',#155809,#90290,#90291);
#76862=AXIS2_PLACEMENT_3D('',#155822,#90292,#90293);
#76863=AXIS2_PLACEMENT_3D('',#155830,#90294,#90295);
#76864=AXIS2_PLACEMENT_3D('',#155843,#90296,#90297);
#76865=AXIS2_PLACEMENT_3D('',#155851,#90298,#90299);
#76866=AXIS2_PLACEMENT_3D('',#155864,#90300,#90301);
#76867=AXIS2_PLACEMENT_3D('',#155872,#90302,#90303);
#76868=AXIS2_PLACEMENT_3D('',#155885,#90304,#90305);
#76869=AXIS2_PLACEMENT_3D('',#155893,#90306,#90307);
#76870=AXIS2_PLACEMENT_3D('',#155906,#90308,#90309);
#76871=AXIS2_PLACEMENT_3D('',#155914,#90310,#90311);
#76872=AXIS2_PLACEMENT_3D('',#155927,#90312,#90313);
#76873=AXIS2_PLACEMENT_3D('',#155934,#90314,#90315);
#76874=AXIS2_PLACEMENT_3D('',#155950,#90316,#90317);
#76875=AXIS2_PLACEMENT_3D('',#155971,#90318,#90319);
#76876=AXIS2_PLACEMENT_3D('',#155997,#90320,#90321);
#76877=AXIS2_PLACEMENT_3D('',#156014,#90322,#90323);
#76878=AXIS2_PLACEMENT_3D('',#156040,#90324,#90325);
#76879=AXIS2_PLACEMENT_3D('',#156057,#90326,#90327);
#76880=AXIS2_PLACEMENT_3D('',#156083,#90328,#90329);
#76881=AXIS2_PLACEMENT_3D('',#156100,#90330,#90331);
#76882=AXIS2_PLACEMENT_3D('',#156126,#90332,#90333);
#76883=AXIS2_PLACEMENT_3D('',#156143,#90334,#90335);
#76884=AXIS2_PLACEMENT_3D('',#156169,#90336,#90337);
#76885=AXIS2_PLACEMENT_3D('',#156186,#90338,#90339);
#76886=AXIS2_PLACEMENT_3D('',#156212,#90340,#90341);
#76887=AXIS2_PLACEMENT_3D('',#156229,#90342,#90343);
#76888=AXIS2_PLACEMENT_3D('',#156255,#90344,#90345);
#76889=AXIS2_PLACEMENT_3D('',#156272,#90346,#90347);
#76890=AXIS2_PLACEMENT_3D('',#156298,#90348,#90349);
#76891=AXIS2_PLACEMENT_3D('',#156315,#90350,#90351);
#76892=AXIS2_PLACEMENT_3D('',#156341,#90352,#90353);
#76893=AXIS2_PLACEMENT_3D('',#156358,#90354,#90355);
#76894=AXIS2_PLACEMENT_3D('',#156384,#90356,#90357);
#76895=AXIS2_PLACEMENT_3D('',#156401,#90358,#90359);
#76896=AXIS2_PLACEMENT_3D('',#156427,#90360,#90361);
#76897=AXIS2_PLACEMENT_3D('',#156444,#90362,#90363);
#76898=AXIS2_PLACEMENT_3D('',#156470,#90364,#90365);
#76899=AXIS2_PLACEMENT_3D('',#156487,#90366,#90367);
#76900=AXIS2_PLACEMENT_3D('',#156513,#90368,#90369);
#76901=AXIS2_PLACEMENT_3D('',#156530,#90370,#90371);
#76902=AXIS2_PLACEMENT_3D('',#156556,#90372,#90373);
#76903=AXIS2_PLACEMENT_3D('',#156573,#90374,#90375);
#76904=AXIS2_PLACEMENT_3D('',#156599,#90376,#90377);
#76905=AXIS2_PLACEMENT_3D('',#156616,#90378,#90379);
#76906=AXIS2_PLACEMENT_3D('',#156642,#90380,#90381);
#76907=AXIS2_PLACEMENT_3D('',#156659,#90382,#90383);
#76908=AXIS2_PLACEMENT_3D('',#156685,#90384,#90385);
#76909=AXIS2_PLACEMENT_3D('',#156702,#90386,#90387);
#76910=AXIS2_PLACEMENT_3D('',#156728,#90388,#90389);
#76911=AXIS2_PLACEMENT_3D('',#156745,#90390,#90391);
#76912=AXIS2_PLACEMENT_3D('',#156771,#90392,#90393);
#76913=AXIS2_PLACEMENT_3D('',#156788,#90394,#90395);
#76914=AXIS2_PLACEMENT_3D('',#156814,#90396,#90397);
#76915=AXIS2_PLACEMENT_3D('',#156831,#90398,#90399);
#76916=AXIS2_PLACEMENT_3D('',#156857,#90400,#90401);
#76917=AXIS2_PLACEMENT_3D('',#156874,#90402,#90403);
#76918=AXIS2_PLACEMENT_3D('',#156900,#90404,#90405);
#76919=AXIS2_PLACEMENT_3D('',#156917,#90406,#90407);
#76920=AXIS2_PLACEMENT_3D('',#156943,#90408,#90409);
#76921=AXIS2_PLACEMENT_3D('',#156960,#90410,#90411);
#76922=AXIS2_PLACEMENT_3D('',#156986,#90412,#90413);
#76923=AXIS2_PLACEMENT_3D('',#157003,#90414,#90415);
#76924=AXIS2_PLACEMENT_3D('',#157029,#90416,#90417);
#76925=AXIS2_PLACEMENT_3D('',#157046,#90418,#90419);
#76926=AXIS2_PLACEMENT_3D('',#157072,#90420,#90421);
#76927=AXIS2_PLACEMENT_3D('',#157089,#90422,#90423);
#76928=AXIS2_PLACEMENT_3D('',#157115,#90424,#90425);
#76929=AXIS2_PLACEMENT_3D('',#157132,#90426,#90427);
#76930=AXIS2_PLACEMENT_3D('',#157158,#90428,#90429);
#76931=AXIS2_PLACEMENT_3D('',#157169,#90430,#90431);
#76932=AXIS2_PLACEMENT_3D('',#157178,#90432,#90433);
#76933=AXIS2_PLACEMENT_3D('',#157186,#90435,#90436);
#76934=AXIS2_PLACEMENT_3D('',#157188,#90437,#90438);
#76935=AXIS2_PLACEMENT_3D('',#157190,#90439,#90440);
#76936=AXIS2_PLACEMENT_3D('',#157191,#90441,#90442);
#76937=AXIS2_PLACEMENT_3D('',#157211,#90444,#90445);
#76938=AXIS2_PLACEMENT_3D('',#157219,#90447,#90448);
#76939=AXIS2_PLACEMENT_3D('',#157221,#90449,#90450);
#76940=AXIS2_PLACEMENT_3D('',#157223,#90451,#90452);
#76941=AXIS2_PLACEMENT_3D('',#157224,#90453,#90454);
#76942=AXIS2_PLACEMENT_3D('',#157244,#90456,#90457);
#76943=AXIS2_PLACEMENT_3D('',#157252,#90459,#90460);
#76944=AXIS2_PLACEMENT_3D('',#157254,#90461,#90462);
#76945=AXIS2_PLACEMENT_3D('',#157256,#90463,#90464);
#76946=AXIS2_PLACEMENT_3D('',#157257,#90465,#90466);
#76947=AXIS2_PLACEMENT_3D('',#157277,#90468,#90469);
#76948=AXIS2_PLACEMENT_3D('',#157285,#90471,#90472);
#76949=AXIS2_PLACEMENT_3D('',#157287,#90473,#90474);
#76950=AXIS2_PLACEMENT_3D('',#157289,#90475,#90476);
#76951=AXIS2_PLACEMENT_3D('',#157290,#90477,#90478);
#76952=AXIS2_PLACEMENT_3D('',#157310,#90480,#90481);
#76953=AXIS2_PLACEMENT_3D('',#157318,#90483,#90484);
#76954=AXIS2_PLACEMENT_3D('',#157320,#90485,#90486);
#76955=AXIS2_PLACEMENT_3D('',#157322,#90487,#90488);
#76956=AXIS2_PLACEMENT_3D('',#157323,#90489,#90490);
#76957=AXIS2_PLACEMENT_3D('',#157343,#90492,#90493);
#76958=AXIS2_PLACEMENT_3D('',#157351,#90495,#90496);
#76959=AXIS2_PLACEMENT_3D('',#157353,#90497,#90498);
#76960=AXIS2_PLACEMENT_3D('',#157355,#90499,#90500);
#76961=AXIS2_PLACEMENT_3D('',#157356,#90501,#90502);
#76962=AXIS2_PLACEMENT_3D('',#157376,#90504,#90505);
#76963=AXIS2_PLACEMENT_3D('',#157384,#90507,#90508);
#76964=AXIS2_PLACEMENT_3D('',#157386,#90509,#90510);
#76965=AXIS2_PLACEMENT_3D('',#157388,#90511,#90512);
#76966=AXIS2_PLACEMENT_3D('',#157389,#90513,#90514);
#76967=AXIS2_PLACEMENT_3D('',#157409,#90516,#90517);
#76968=AXIS2_PLACEMENT_3D('',#157417,#90519,#90520);
#76969=AXIS2_PLACEMENT_3D('',#157419,#90521,#90522);
#76970=AXIS2_PLACEMENT_3D('',#157421,#90523,#90524);
#76971=AXIS2_PLACEMENT_3D('',#157422,#90525,#90526);
#76972=AXIS2_PLACEMENT_3D('',#157442,#90528,#90529);
#76973=AXIS2_PLACEMENT_3D('',#157450,#90531,#90532);
#76974=AXIS2_PLACEMENT_3D('',#157452,#90533,#90534);
#76975=AXIS2_PLACEMENT_3D('',#157454,#90535,#90536);
#76976=AXIS2_PLACEMENT_3D('',#157455,#90537,#90538);
#76977=AXIS2_PLACEMENT_3D('',#157475,#90540,#90541);
#76978=AXIS2_PLACEMENT_3D('',#157483,#90543,#90544);
#76979=AXIS2_PLACEMENT_3D('',#157485,#90545,#90546);
#76980=AXIS2_PLACEMENT_3D('',#157487,#90547,#90548);
#76981=AXIS2_PLACEMENT_3D('',#157488,#90549,#90550);
#76982=AXIS2_PLACEMENT_3D('',#157508,#90552,#90553);
#76983=AXIS2_PLACEMENT_3D('',#157516,#90555,#90556);
#76984=AXIS2_PLACEMENT_3D('',#157518,#90557,#90558);
#76985=AXIS2_PLACEMENT_3D('',#157520,#90559,#90560);
#76986=AXIS2_PLACEMENT_3D('',#157521,#90561,#90562);
#76987=AXIS2_PLACEMENT_3D('',#157541,#90564,#90565);
#76988=AXIS2_PLACEMENT_3D('',#157549,#90567,#90568);
#76989=AXIS2_PLACEMENT_3D('',#157551,#90569,#90570);
#76990=AXIS2_PLACEMENT_3D('',#157553,#90571,#90572);
#76991=AXIS2_PLACEMENT_3D('',#157554,#90573,#90574);
#76992=AXIS2_PLACEMENT_3D('',#157574,#90576,#90577);
#76993=AXIS2_PLACEMENT_3D('',#157582,#90579,#90580);
#76994=AXIS2_PLACEMENT_3D('',#157584,#90581,#90582);
#76995=AXIS2_PLACEMENT_3D('',#157586,#90583,#90584);
#76996=AXIS2_PLACEMENT_3D('',#157587,#90585,#90586);
#76997=AXIS2_PLACEMENT_3D('',#157607,#90588,#90589);
#76998=AXIS2_PLACEMENT_3D('',#157615,#90591,#90592);
#76999=AXIS2_PLACEMENT_3D('',#157617,#90593,#90594);
#77000=AXIS2_PLACEMENT_3D('',#157619,#90595,#90596);
#77001=AXIS2_PLACEMENT_3D('',#157620,#90597,#90598);
#77002=AXIS2_PLACEMENT_3D('',#157664,#90602,#90603);
#77003=AXIS2_PLACEMENT_3D('',#157672,#90605,#90606);
#77004=AXIS2_PLACEMENT_3D('',#157674,#90607,#90608);
#77005=AXIS2_PLACEMENT_3D('',#157676,#90609,#90610);
#77006=AXIS2_PLACEMENT_3D('',#157677,#90611,#90612);
#77007=AXIS2_PLACEMENT_3D('',#157697,#90614,#90615);
#77008=AXIS2_PLACEMENT_3D('',#157705,#90617,#90618);
#77009=AXIS2_PLACEMENT_3D('',#157707,#90619,#90620);
#77010=AXIS2_PLACEMENT_3D('',#157709,#90621,#90622);
#77011=AXIS2_PLACEMENT_3D('',#157710,#90623,#90624);
#77012=AXIS2_PLACEMENT_3D('',#157730,#90626,#90627);
#77013=AXIS2_PLACEMENT_3D('',#157749,#90629,#90630);
#77014=AXIS2_PLACEMENT_3D('',#157751,#90632,#90633);
#77015=AXIS2_PLACEMENT_3D('',#157753,#90634,#90635);
#77016=AXIS2_PLACEMENT_3D('',#157754,#90636,#90637);
#77017=AXIS2_PLACEMENT_3D('',#157764,#90639,#90640);
#77018=AXIS2_PLACEMENT_3D('',#157771,#90641,#90642);
#77019=AXIS2_PLACEMENT_3D('',#157773,#90643,#90644);
#77020=AXIS2_PLACEMENT_3D('',#157775,#90645,#90646);
#77021=AXIS2_PLACEMENT_3D('',#157776,#90647,#90648);
#77022=AXIS2_PLACEMENT_3D('',#157796,#90650,#90651);
#77023=AXIS2_PLACEMENT_3D('',#157804,#90653,#90654);
#77024=AXIS2_PLACEMENT_3D('',#157806,#90655,#90656);
#77025=AXIS2_PLACEMENT_3D('',#157808,#90657,#90658);
#77026=AXIS2_PLACEMENT_3D('',#157809,#90659,#90660);
#77027=AXIS2_PLACEMENT_3D('',#157829,#90662,#90663);
#77028=AXIS2_PLACEMENT_3D('',#157837,#90665,#90666);
#77029=AXIS2_PLACEMENT_3D('',#157839,#90667,#90668);
#77030=AXIS2_PLACEMENT_3D('',#157841,#90669,#90670);
#77031=AXIS2_PLACEMENT_3D('',#157842,#90671,#90672);
#77032=AXIS2_PLACEMENT_3D('',#157862,#90674,#90675);
#77033=AXIS2_PLACEMENT_3D('',#157870,#90677,#90678);
#77034=AXIS2_PLACEMENT_3D('',#157872,#90679,#90680);
#77035=AXIS2_PLACEMENT_3D('',#157874,#90681,#90682);
#77036=AXIS2_PLACEMENT_3D('',#157875,#90683,#90684);
#77037=AXIS2_PLACEMENT_3D('',#157895,#90686,#90687);
#77038=AXIS2_PLACEMENT_3D('',#157903,#90689,#90690);
#77039=AXIS2_PLACEMENT_3D('',#157905,#90691,#90692);
#77040=AXIS2_PLACEMENT_3D('',#157907,#90693,#90694);
#77041=AXIS2_PLACEMENT_3D('',#157908,#90695,#90696);
#77042=AXIS2_PLACEMENT_3D('',#157928,#90698,#90699);
#77043=AXIS2_PLACEMENT_3D('',#157936,#90701,#90702);
#77044=AXIS2_PLACEMENT_3D('',#157938,#90703,#90704);
#77045=AXIS2_PLACEMENT_3D('',#157940,#90705,#90706);
#77046=AXIS2_PLACEMENT_3D('',#157941,#90707,#90708);
#77047=AXIS2_PLACEMENT_3D('',#157961,#90710,#90711);
#77048=AXIS2_PLACEMENT_3D('',#157969,#90713,#90714);
#77049=AXIS2_PLACEMENT_3D('',#157971,#90715,#90716);
#77050=AXIS2_PLACEMENT_3D('',#157973,#90717,#90718);
#77051=AXIS2_PLACEMENT_3D('',#157974,#90719,#90720);
#77052=AXIS2_PLACEMENT_3D('',#157994,#90722,#90723);
#77053=AXIS2_PLACEMENT_3D('',#158002,#90725,#90726);
#77054=AXIS2_PLACEMENT_3D('',#158004,#90727,#90728);
#77055=AXIS2_PLACEMENT_3D('',#158006,#90729,#90730);
#77056=AXIS2_PLACEMENT_3D('',#158007,#90731,#90732);
#77057=AXIS2_PLACEMENT_3D('',#158027,#90734,#90735);
#77058=AXIS2_PLACEMENT_3D('',#158035,#90737,#90738);
#77059=AXIS2_PLACEMENT_3D('',#158037,#90739,#90740);
#77060=AXIS2_PLACEMENT_3D('',#158039,#90741,#90742);
#77061=AXIS2_PLACEMENT_3D('',#158040,#90743,#90744);
#77062=AXIS2_PLACEMENT_3D('',#158060,#90746,#90747);
#77063=AXIS2_PLACEMENT_3D('',#158068,#90749,#90750);
#77064=AXIS2_PLACEMENT_3D('',#158070,#90751,#90752);
#77065=AXIS2_PLACEMENT_3D('',#158072,#90753,#90754);
#77066=AXIS2_PLACEMENT_3D('',#158073,#90755,#90756);
#77067=AXIS2_PLACEMENT_3D('',#158093,#90758,#90759);
#77068=AXIS2_PLACEMENT_3D('',#158101,#90761,#90762);
#77069=AXIS2_PLACEMENT_3D('',#158103,#90763,#90764);
#77070=AXIS2_PLACEMENT_3D('',#158105,#90765,#90766);
#77071=AXIS2_PLACEMENT_3D('',#158106,#90767,#90768);
#77072=AXIS2_PLACEMENT_3D('',#158128,#90770,#90771);
#77073=AXIS2_PLACEMENT_3D('',#158215,#90775,#90776);
#77074=AXIS2_PLACEMENT_3D('',#158301,#90779,#90780);
#77075=AXIS2_PLACEMENT_3D('',#158386,#90783,#90784);
#77076=AXIS2_PLACEMENT_3D('',#158472,#90787,#90788);
#77077=AXIS2_PLACEMENT_3D('',#158556,#90791,#90792);
#77078=AXIS2_PLACEMENT_3D('',#158642,#90795,#90796);
#77079=AXIS2_PLACEMENT_3D('',#158727,#90799,#90800);
#77080=AXIS2_PLACEMENT_3D('',#158813,#90803,#90804);
#77081=AXIS2_PLACEMENT_3D('',#158898,#90807,#90808);
#77082=AXIS2_PLACEMENT_3D('',#158984,#90811,#90812);
#77083=AXIS2_PLACEMENT_3D('',#159070,#90815,#90816);
#77084=AXIS2_PLACEMENT_3D('',#159156,#90819,#90820);
#77085=AXIS2_PLACEMENT_3D('',#159241,#90823,#90824);
#77086=AXIS2_PLACEMENT_3D('',#159326,#90827,#90828);
#77087=AXIS2_PLACEMENT_3D('',#159412,#90831,#90832);
#77088=AXIS2_PLACEMENT_3D('',#159498,#90835,#90836);
#77089=AXIS2_PLACEMENT_3D('',#159583,#90839,#90840);
#77090=AXIS2_PLACEMENT_3D('',#159668,#90843,#90844);
#77091=AXIS2_PLACEMENT_3D('',#159754,#90847,#90848);
#77092=AXIS2_PLACEMENT_3D('',#159839,#90851,#90852);
#77093=AXIS2_PLACEMENT_3D('',#159925,#90855,#90856);
#77094=AXIS2_PLACEMENT_3D('',#160011,#90859,#90860);
#77095=AXIS2_PLACEMENT_3D('',#160097,#90863,#90864);
#77096=AXIS2_PLACEMENT_3D('',#160183,#90867,#90868);
#77097=AXIS2_PLACEMENT_3D('',#160268,#90871,#90872);
#77098=AXIS2_PLACEMENT_3D('',#160354,#90875,#90876);
#77099=AXIS2_PLACEMENT_3D('',#160440,#90879,#90880);
#77100=AXIS2_PLACEMENT_3D('',#160526,#90883,#90884);
#77101=AXIS2_PLACEMENT_3D('',#160608,#90886,#90887);
#77102=AXIS2_PLACEMENT_3D('',#160625,#90888,#90889);
#77103=AXIS2_PLACEMENT_3D('',#160633,#90890,#90891);
#77104=AXIS2_PLACEMENT_3D('',#160650,#90892,#90893);
#77105=AXIS2_PLACEMENT_3D('',#160658,#90894,#90895);
#77106=AXIS2_PLACEMENT_3D('',#160675,#90896,#90897);
#77107=AXIS2_PLACEMENT_3D('',#160683,#90898,#90899);
#77108=AXIS2_PLACEMENT_3D('',#160700,#90900,#90901);
#77109=AXIS2_PLACEMENT_3D('',#160708,#90902,#90903);
#77110=AXIS2_PLACEMENT_3D('',#160725,#90904,#90905);
#77111=AXIS2_PLACEMENT_3D('',#160733,#90906,#90907);
#77112=AXIS2_PLACEMENT_3D('',#160750,#90908,#90909);
#77113=AXIS2_PLACEMENT_3D('',#160758,#90910,#90911);
#77114=AXIS2_PLACEMENT_3D('',#160775,#90912,#90913);
#77115=AXIS2_PLACEMENT_3D('',#160783,#90914,#90915);
#77116=AXIS2_PLACEMENT_3D('',#160800,#90916,#90917);
#77117=AXIS2_PLACEMENT_3D('',#160808,#90918,#90919);
#77118=AXIS2_PLACEMENT_3D('',#160825,#90920,#90921);
#77119=AXIS2_PLACEMENT_3D('',#160833,#90922,#90923);
#77120=AXIS2_PLACEMENT_3D('',#160850,#90924,#90925);
#77121=AXIS2_PLACEMENT_3D('',#160858,#90926,#90927);
#77122=AXIS2_PLACEMENT_3D('',#160875,#90928,#90929);
#77123=AXIS2_PLACEMENT_3D('',#160883,#90930,#90931);
#77124=AXIS2_PLACEMENT_3D('',#160900,#90932,#90933);
#77125=AXIS2_PLACEMENT_3D('',#160908,#90934,#90935);
#77126=AXIS2_PLACEMENT_3D('',#160925,#90936,#90937);
#77127=AXIS2_PLACEMENT_3D('',#160933,#90938,#90939);
#77128=AXIS2_PLACEMENT_3D('',#160950,#90940,#90941);
#77129=AXIS2_PLACEMENT_3D('',#160958,#90942,#90943);
#77130=AXIS2_PLACEMENT_3D('',#160975,#90944,#90945);
#77131=AXIS2_PLACEMENT_3D('',#160983,#90946,#90947);
#77132=AXIS2_PLACEMENT_3D('',#161000,#90948,#90949);
#77133=AXIS2_PLACEMENT_3D('',#161008,#90950,#90951);
#77134=AXIS2_PLACEMENT_3D('',#161025,#90952,#90953);
#77135=AXIS2_PLACEMENT_3D('',#161033,#90954,#90955);
#77136=AXIS2_PLACEMENT_3D('',#161050,#90956,#90957);
#77137=AXIS2_PLACEMENT_3D('',#161058,#90958,#90959);
#77138=AXIS2_PLACEMENT_3D('',#161075,#90960,#90961);
#77139=AXIS2_PLACEMENT_3D('',#161083,#90962,#90963);
#77140=AXIS2_PLACEMENT_3D('',#161100,#90964,#90965);
#77141=AXIS2_PLACEMENT_3D('',#161108,#90966,#90967);
#77142=AXIS2_PLACEMENT_3D('',#161125,#90968,#90969);
#77143=AXIS2_PLACEMENT_3D('',#161133,#90970,#90971);
#77144=AXIS2_PLACEMENT_3D('',#161150,#90972,#90973);
#77145=AXIS2_PLACEMENT_3D('',#161158,#90974,#90975);
#77146=AXIS2_PLACEMENT_3D('',#161175,#90976,#90977);
#77147=AXIS2_PLACEMENT_3D('',#161183,#90978,#90979);
#77148=AXIS2_PLACEMENT_3D('',#161200,#90980,#90981);
#77149=AXIS2_PLACEMENT_3D('',#161208,#90982,#90983);
#77150=AXIS2_PLACEMENT_3D('',#161225,#90984,#90985);
#77151=AXIS2_PLACEMENT_3D('',#161233,#90986,#90987);
#77152=AXIS2_PLACEMENT_3D('',#161250,#90988,#90989);
#77153=AXIS2_PLACEMENT_3D('',#161258,#90990,#90991);
#77154=AXIS2_PLACEMENT_3D('',#161275,#90992,#90993);
#77155=AXIS2_PLACEMENT_3D('',#161283,#90994,#90995);
#77156=AXIS2_PLACEMENT_3D('',#161300,#90996,#90997);
#77157=AXIS2_PLACEMENT_3D('',#161308,#90998,#90999);
#77158=AXIS2_PLACEMENT_3D('',#161325,#91000,#91001);
#77159=AXIS2_PLACEMENT_3D('',#161338,#91002,#91003);
#77160=AXIS2_PLACEMENT_3D('',#161354,#91005,#91006);
#77161=AXIS2_PLACEMENT_3D('',#161362,#91008,#91009);
#77162=AXIS2_PLACEMENT_3D('',#161365,#91010,#91011);
#77163=AXIS2_PLACEMENT_3D('',#161367,#91012,#91013);
#77164=AXIS2_PLACEMENT_3D('',#161368,#91014,#91015);
#77165=AXIS2_PLACEMENT_3D('',#161380,#91016,#91017);
#77166=AXIS2_PLACEMENT_3D('',#161382,#91019,#91020);
#77167=AXIS2_PLACEMENT_3D('',#161383,#91021,#91022);
#77168=AXIS2_PLACEMENT_3D('',#161384,#91023,#91024);
#77169=AXIS2_PLACEMENT_3D('',#161393,#91025,#91026);
#77170=AXIS2_PLACEMENT_3D('',#161401,#91028,#91029);
#77171=AXIS2_PLACEMENT_3D('',#161404,#91030,#91031);
#77172=AXIS2_PLACEMENT_3D('',#161406,#91032,#91033);
#77173=AXIS2_PLACEMENT_3D('',#161407,#91034,#91035);
#77174=AXIS2_PLACEMENT_3D('',#161419,#91036,#91037);
#77175=AXIS2_PLACEMENT_3D('',#161421,#91039,#91040);
#77176=AXIS2_PLACEMENT_3D('',#161422,#91041,#91042);
#77177=AXIS2_PLACEMENT_3D('',#161423,#91043,#91044);
#77178=AXIS2_PLACEMENT_3D('',#161432,#91045,#91046);
#77179=AXIS2_PLACEMENT_3D('',#161440,#91048,#91049);
#77180=AXIS2_PLACEMENT_3D('',#161443,#91050,#91051);
#77181=AXIS2_PLACEMENT_3D('',#161445,#91052,#91053);
#77182=AXIS2_PLACEMENT_3D('',#161446,#91054,#91055);
#77183=AXIS2_PLACEMENT_3D('',#161458,#91056,#91057);
#77184=AXIS2_PLACEMENT_3D('',#161460,#91059,#91060);
#77185=AXIS2_PLACEMENT_3D('',#161461,#91061,#91062);
#77186=AXIS2_PLACEMENT_3D('',#161462,#91063,#91064);
#77187=AXIS2_PLACEMENT_3D('',#161471,#91065,#91066);
#77188=AXIS2_PLACEMENT_3D('',#161479,#91068,#91069);
#77189=AXIS2_PLACEMENT_3D('',#161482,#91070,#91071);
#77190=AXIS2_PLACEMENT_3D('',#161484,#91072,#91073);
#77191=AXIS2_PLACEMENT_3D('',#161485,#91074,#91075);
#77192=AXIS2_PLACEMENT_3D('',#161497,#91076,#91077);
#77193=AXIS2_PLACEMENT_3D('',#161499,#91079,#91080);
#77194=AXIS2_PLACEMENT_3D('',#161500,#91081,#91082);
#77195=AXIS2_PLACEMENT_3D('',#161501,#91083,#91084);
#77196=AXIS2_PLACEMENT_3D('',#161510,#91085,#91086);
#77197=AXIS2_PLACEMENT_3D('',#161518,#91088,#91089);
#77198=AXIS2_PLACEMENT_3D('',#161521,#91090,#91091);
#77199=AXIS2_PLACEMENT_3D('',#161523,#91092,#91093);
#77200=AXIS2_PLACEMENT_3D('',#161524,#91094,#91095);
#77201=AXIS2_PLACEMENT_3D('',#161536,#91096,#91097);
#77202=AXIS2_PLACEMENT_3D('',#161538,#91099,#91100);
#77203=AXIS2_PLACEMENT_3D('',#161539,#91101,#91102);
#77204=AXIS2_PLACEMENT_3D('',#161540,#91103,#91104);
#77205=AXIS2_PLACEMENT_3D('',#161549,#91105,#91106);
#77206=AXIS2_PLACEMENT_3D('',#161557,#91108,#91109);
#77207=AXIS2_PLACEMENT_3D('',#161560,#91110,#91111);
#77208=AXIS2_PLACEMENT_3D('',#161562,#91112,#91113);
#77209=AXIS2_PLACEMENT_3D('',#161563,#91114,#91115);
#77210=AXIS2_PLACEMENT_3D('',#161575,#91116,#91117);
#77211=AXIS2_PLACEMENT_3D('',#161577,#91119,#91120);
#77212=AXIS2_PLACEMENT_3D('',#161578,#91121,#91122);
#77213=AXIS2_PLACEMENT_3D('',#161579,#91123,#91124);
#77214=AXIS2_PLACEMENT_3D('',#161593,#91126,#91127);
#77215=AXIS2_PLACEMENT_3D('',#161595,#91128,#91129);
#77216=AXIS2_PLACEMENT_3D('',#161596,#91130,#91131);
#77217=AXIS2_PLACEMENT_3D('',#161616,#91133,#91134);
#77218=AXIS2_PLACEMENT_3D('',#161624,#91136,#91137);
#77219=AXIS2_PLACEMENT_3D('',#161627,#91138,#91139);
#77220=AXIS2_PLACEMENT_3D('',#161629,#91140,#91141);
#77221=AXIS2_PLACEMENT_3D('',#161630,#91142,#91143);
#77222=AXIS2_PLACEMENT_3D('',#161642,#91144,#91145);
#77223=AXIS2_PLACEMENT_3D('',#161644,#91147,#91148);
#77224=AXIS2_PLACEMENT_3D('',#161645,#91149,#91150);
#77225=AXIS2_PLACEMENT_3D('',#161646,#91151,#91152);
#77226=AXIS2_PLACEMENT_3D('',#161655,#91153,#91154);
#77227=AXIS2_PLACEMENT_3D('',#161663,#91156,#91157);
#77228=AXIS2_PLACEMENT_3D('',#161666,#91158,#91159);
#77229=AXIS2_PLACEMENT_3D('',#161668,#91160,#91161);
#77230=AXIS2_PLACEMENT_3D('',#161669,#91162,#91163);
#77231=AXIS2_PLACEMENT_3D('',#161681,#91164,#91165);
#77232=AXIS2_PLACEMENT_3D('',#161683,#91167,#91168);
#77233=AXIS2_PLACEMENT_3D('',#161684,#91169,#91170);
#77234=AXIS2_PLACEMENT_3D('',#161685,#91171,#91172);
#77235=AXIS2_PLACEMENT_3D('',#161694,#91173,#91174);
#77236=AXIS2_PLACEMENT_3D('',#161702,#91176,#91177);
#77237=AXIS2_PLACEMENT_3D('',#161705,#91178,#91179);
#77238=AXIS2_PLACEMENT_3D('',#161707,#91180,#91181);
#77239=AXIS2_PLACEMENT_3D('',#161708,#91182,#91183);
#77240=AXIS2_PLACEMENT_3D('',#161720,#91184,#91185);
#77241=AXIS2_PLACEMENT_3D('',#161722,#91187,#91188);
#77242=AXIS2_PLACEMENT_3D('',#161723,#91189,#91190);
#77243=AXIS2_PLACEMENT_3D('',#161724,#91191,#91192);
#77244=AXIS2_PLACEMENT_3D('',#161733,#91193,#91194);
#77245=AXIS2_PLACEMENT_3D('',#161741,#91196,#91197);
#77246=AXIS2_PLACEMENT_3D('',#161744,#91198,#91199);
#77247=AXIS2_PLACEMENT_3D('',#161746,#91200,#91201);
#77248=AXIS2_PLACEMENT_3D('',#161747,#91202,#91203);
#77249=AXIS2_PLACEMENT_3D('',#161759,#91204,#91205);
#77250=AXIS2_PLACEMENT_3D('',#161761,#91207,#91208);
#77251=AXIS2_PLACEMENT_3D('',#161762,#91209,#91210);
#77252=AXIS2_PLACEMENT_3D('',#161763,#91211,#91212);
#77253=AXIS2_PLACEMENT_3D('',#161772,#91213,#91214);
#77254=AXIS2_PLACEMENT_3D('',#161780,#91216,#91217);
#77255=AXIS2_PLACEMENT_3D('',#161783,#91218,#91219);
#77256=AXIS2_PLACEMENT_3D('',#161785,#91220,#91221);
#77257=AXIS2_PLACEMENT_3D('',#161786,#91222,#91223);
#77258=AXIS2_PLACEMENT_3D('',#161798,#91224,#91225);
#77259=AXIS2_PLACEMENT_3D('',#161800,#91227,#91228);
#77260=AXIS2_PLACEMENT_3D('',#161801,#91229,#91230);
#77261=AXIS2_PLACEMENT_3D('',#161802,#91231,#91232);
#77262=AXIS2_PLACEMENT_3D('',#161811,#91233,#91234);
#77263=AXIS2_PLACEMENT_3D('',#161819,#91236,#91237);
#77264=AXIS2_PLACEMENT_3D('',#161822,#91238,#91239);
#77265=AXIS2_PLACEMENT_3D('',#161824,#91240,#91241);
#77266=AXIS2_PLACEMENT_3D('',#161825,#91242,#91243);
#77267=AXIS2_PLACEMENT_3D('',#161837,#91244,#91245);
#77268=AXIS2_PLACEMENT_3D('',#161839,#91247,#91248);
#77269=AXIS2_PLACEMENT_3D('',#161840,#91249,#91250);
#77270=AXIS2_PLACEMENT_3D('',#161841,#91251,#91252);
#77271=AXIS2_PLACEMENT_3D('',#161850,#91253,#91254);
#77272=AXIS2_PLACEMENT_3D('',#161858,#91256,#91257);
#77273=AXIS2_PLACEMENT_3D('',#161861,#91258,#91259);
#77274=AXIS2_PLACEMENT_3D('',#161863,#91260,#91261);
#77275=AXIS2_PLACEMENT_3D('',#161864,#91262,#91263);
#77276=AXIS2_PLACEMENT_3D('',#161876,#91264,#91265);
#77277=AXIS2_PLACEMENT_3D('',#161878,#91267,#91268);
#77278=AXIS2_PLACEMENT_3D('',#161879,#91269,#91270);
#77279=AXIS2_PLACEMENT_3D('',#161880,#91271,#91272);
#77280=AXIS2_PLACEMENT_3D('',#161889,#91273,#91274);
#77281=AXIS2_PLACEMENT_3D('',#161897,#91276,#91277);
#77282=AXIS2_PLACEMENT_3D('',#161900,#91278,#91279);
#77283=AXIS2_PLACEMENT_3D('',#161902,#91280,#91281);
#77284=AXIS2_PLACEMENT_3D('',#161903,#91282,#91283);
#77285=AXIS2_PLACEMENT_3D('',#161915,#91284,#91285);
#77286=AXIS2_PLACEMENT_3D('',#161917,#91287,#91288);
#77287=AXIS2_PLACEMENT_3D('',#161918,#91289,#91290);
#77288=AXIS2_PLACEMENT_3D('',#161919,#91291,#91292);
#77289=AXIS2_PLACEMENT_3D('',#161928,#91293,#91294);
#77290=AXIS2_PLACEMENT_3D('',#161936,#91296,#91297);
#77291=AXIS2_PLACEMENT_3D('',#161939,#91298,#91299);
#77292=AXIS2_PLACEMENT_3D('',#161941,#91300,#91301);
#77293=AXIS2_PLACEMENT_3D('',#161942,#91302,#91303);
#77294=AXIS2_PLACEMENT_3D('',#161954,#91304,#91305);
#77295=AXIS2_PLACEMENT_3D('',#161956,#91307,#91308);
#77296=AXIS2_PLACEMENT_3D('',#161957,#91309,#91310);
#77297=AXIS2_PLACEMENT_3D('',#161958,#91311,#91312);
#77298=AXIS2_PLACEMENT_3D('',#161967,#91313,#91314);
#77299=AXIS2_PLACEMENT_3D('',#161975,#91316,#91317);
#77300=AXIS2_PLACEMENT_3D('',#161978,#91318,#91319);
#77301=AXIS2_PLACEMENT_3D('',#161980,#91320,#91321);
#77302=AXIS2_PLACEMENT_3D('',#161981,#91322,#91323);
#77303=AXIS2_PLACEMENT_3D('',#161993,#91324,#91325);
#77304=AXIS2_PLACEMENT_3D('',#161995,#91327,#91328);
#77305=AXIS2_PLACEMENT_3D('',#161996,#91329,#91330);
#77306=AXIS2_PLACEMENT_3D('',#161997,#91331,#91332);
#77307=AXIS2_PLACEMENT_3D('',#162007,#91334,#91335);
#77308=AXIS2_PLACEMENT_3D('',#162014,#91336,#91337);
#77309=AXIS2_PLACEMENT_3D('',#162017,#91338,#91339);
#77310=AXIS2_PLACEMENT_3D('',#162019,#91340,#91341);
#77311=AXIS2_PLACEMENT_3D('',#162020,#91342,#91343);
#77312=AXIS2_PLACEMENT_3D('',#162032,#91344,#91345);
#77313=AXIS2_PLACEMENT_3D('',#162034,#91347,#91348);
#77314=AXIS2_PLACEMENT_3D('',#162035,#91349,#91350);
#77315=AXIS2_PLACEMENT_3D('',#162036,#91351,#91352);
#77316=AXIS2_PLACEMENT_3D('',#162045,#91353,#91354);
#77317=AXIS2_PLACEMENT_3D('',#162053,#91356,#91357);
#77318=AXIS2_PLACEMENT_3D('',#162056,#91358,#91359);
#77319=AXIS2_PLACEMENT_3D('',#162058,#91360,#91361);
#77320=AXIS2_PLACEMENT_3D('',#162059,#91362,#91363);
#77321=AXIS2_PLACEMENT_3D('',#162071,#91364,#91365);
#77322=AXIS2_PLACEMENT_3D('',#162073,#91367,#91368);
#77323=AXIS2_PLACEMENT_3D('',#162074,#91369,#91370);
#77324=AXIS2_PLACEMENT_3D('',#162075,#91371,#91372);
#77325=AXIS2_PLACEMENT_3D('',#162084,#91373,#91374);
#77326=AXIS2_PLACEMENT_3D('',#162092,#91376,#91377);
#77327=AXIS2_PLACEMENT_3D('',#162095,#91378,#91379);
#77328=AXIS2_PLACEMENT_3D('',#162097,#91380,#91381);
#77329=AXIS2_PLACEMENT_3D('',#162098,#91382,#91383);
#77330=AXIS2_PLACEMENT_3D('',#162110,#91384,#91385);
#77331=AXIS2_PLACEMENT_3D('',#162112,#91387,#91388);
#77332=AXIS2_PLACEMENT_3D('',#162113,#91389,#91390);
#77333=AXIS2_PLACEMENT_3D('',#162114,#91391,#91392);
#77334=AXIS2_PLACEMENT_3D('',#162123,#91393,#91394);
#77335=AXIS2_PLACEMENT_3D('',#162131,#91396,#91397);
#77336=AXIS2_PLACEMENT_3D('',#162134,#91398,#91399);
#77337=AXIS2_PLACEMENT_3D('',#162136,#91400,#91401);
#77338=AXIS2_PLACEMENT_3D('',#162137,#91402,#91403);
#77339=AXIS2_PLACEMENT_3D('',#162149,#91404,#91405);
#77340=AXIS2_PLACEMENT_3D('',#162151,#91407,#91408);
#77341=AXIS2_PLACEMENT_3D('',#162152,#91409,#91410);
#77342=AXIS2_PLACEMENT_3D('',#162153,#91411,#91412);
#77343=AXIS2_PLACEMENT_3D('',#162162,#91413,#91414);
#77344=AXIS2_PLACEMENT_3D('',#162170,#91416,#91417);
#77345=AXIS2_PLACEMENT_3D('',#162173,#91418,#91419);
#77346=AXIS2_PLACEMENT_3D('',#162175,#91420,#91421);
#77347=AXIS2_PLACEMENT_3D('',#162176,#91422,#91423);
#77348=AXIS2_PLACEMENT_3D('',#162188,#91424,#91425);
#77349=AXIS2_PLACEMENT_3D('',#162190,#91427,#91428);
#77350=AXIS2_PLACEMENT_3D('',#162191,#91429,#91430);
#77351=AXIS2_PLACEMENT_3D('',#162192,#91431,#91432);
#77352=AXIS2_PLACEMENT_3D('',#162201,#91433,#91434);
#77353=AXIS2_PLACEMENT_3D('',#162209,#91436,#91437);
#77354=AXIS2_PLACEMENT_3D('',#162212,#91438,#91439);
#77355=AXIS2_PLACEMENT_3D('',#162214,#91440,#91441);
#77356=AXIS2_PLACEMENT_3D('',#162215,#91442,#91443);
#77357=AXIS2_PLACEMENT_3D('',#162227,#91444,#91445);
#77358=AXIS2_PLACEMENT_3D('',#162229,#91447,#91448);
#77359=AXIS2_PLACEMENT_3D('',#162230,#91449,#91450);
#77360=AXIS2_PLACEMENT_3D('',#162231,#91451,#91452);
#77361=AXIS2_PLACEMENT_3D('',#162240,#91453,#91454);
#77362=AXIS2_PLACEMENT_3D('',#162248,#91456,#91457);
#77363=AXIS2_PLACEMENT_3D('',#162251,#91458,#91459);
#77364=AXIS2_PLACEMENT_3D('',#162253,#91460,#91461);
#77365=AXIS2_PLACEMENT_3D('',#162254,#91462,#91463);
#77366=AXIS2_PLACEMENT_3D('',#162266,#91464,#91465);
#77367=AXIS2_PLACEMENT_3D('',#162268,#91467,#91468);
#77368=AXIS2_PLACEMENT_3D('',#162269,#91469,#91470);
#77369=AXIS2_PLACEMENT_3D('',#162270,#91471,#91472);
#77370=AXIS2_PLACEMENT_3D('',#162279,#91473,#91474);
#77371=AXIS2_PLACEMENT_3D('',#162287,#91476,#91477);
#77372=AXIS2_PLACEMENT_3D('',#162290,#91478,#91479);
#77373=AXIS2_PLACEMENT_3D('',#162292,#91480,#91481);
#77374=AXIS2_PLACEMENT_3D('',#162293,#91482,#91483);
#77375=AXIS2_PLACEMENT_3D('',#162305,#91484,#91485);
#77376=AXIS2_PLACEMENT_3D('',#162307,#91487,#91488);
#77377=AXIS2_PLACEMENT_3D('',#162308,#91489,#91490);
#77378=AXIS2_PLACEMENT_3D('',#162309,#91491,#91492);
#77379=AXIS2_PLACEMENT_3D('',#162318,#91493,#91494);
#77380=AXIS2_PLACEMENT_3D('',#162326,#91496,#91497);
#77381=AXIS2_PLACEMENT_3D('',#162329,#91498,#91499);
#77382=AXIS2_PLACEMENT_3D('',#162331,#91500,#91501);
#77383=AXIS2_PLACEMENT_3D('',#162332,#91502,#91503);
#77384=AXIS2_PLACEMENT_3D('',#162344,#91504,#91505);
#77385=AXIS2_PLACEMENT_3D('',#162346,#91507,#91508);
#77386=AXIS2_PLACEMENT_3D('',#162347,#91509,#91510);
#77387=AXIS2_PLACEMENT_3D('',#162348,#91511,#91512);
#77388=AXIS2_PLACEMENT_3D('',#162357,#91513,#91514);
#77389=AXIS2_PLACEMENT_3D('',#162365,#91516,#91517);
#77390=AXIS2_PLACEMENT_3D('',#162368,#91518,#91519);
#77391=AXIS2_PLACEMENT_3D('',#162370,#91520,#91521);
#77392=AXIS2_PLACEMENT_3D('',#162371,#91522,#91523);
#77393=AXIS2_PLACEMENT_3D('',#162383,#91524,#91525);
#77394=AXIS2_PLACEMENT_3D('',#162385,#91527,#91528);
#77395=AXIS2_PLACEMENT_3D('',#162386,#91529,#91530);
#77396=AXIS2_PLACEMENT_3D('',#162387,#91531,#91532);
#77397=AXIS2_PLACEMENT_3D('',#162396,#91533,#91534);
#77398=AXIS2_PLACEMENT_3D('',#162404,#91536,#91537);
#77399=AXIS2_PLACEMENT_3D('',#162407,#91538,#91539);
#77400=AXIS2_PLACEMENT_3D('',#162409,#91540,#91541);
#77401=AXIS2_PLACEMENT_3D('',#162410,#91542,#91543);
#77402=AXIS2_PLACEMENT_3D('',#162422,#91544,#91545);
#77403=AXIS2_PLACEMENT_3D('',#162424,#91547,#91548);
#77404=AXIS2_PLACEMENT_3D('',#162425,#91549,#91550);
#77405=AXIS2_PLACEMENT_3D('',#162426,#91551,#91552);
#77406=AXIS2_PLACEMENT_3D('',#162427,#91553,#91554);
#77407=AXIS2_PLACEMENT_3D('',#162430,#91555,#91556);
#77408=AXIS2_PLACEMENT_3D('',#162432,#91557,#91558);
#77409=AXIS2_PLACEMENT_3D('',#162433,#91559,#91560);
#77410=AXIS2_PLACEMENT_3D('',#162434,#91561,#91562);
#77411=AXIS2_PLACEMENT_3D('',#162435,#91563,#91564);
#77412=AXIS2_PLACEMENT_3D('',#162437,#91565,#91566);
#77413=AXIS2_PLACEMENT_3D('',#162438,#91567,#91568);
#77414=AXIS2_PLACEMENT_3D('',#162446,#91570,#91571);
#77415=AXIS2_PLACEMENT_3D('',#162458,#91572,#91573);
#77416=AXIS2_PLACEMENT_3D('',#162459,#91574,#91575);
#77417=AXIS2_PLACEMENT_3D('',#162467,#91576,#91577);
#77418=AXIS2_PLACEMENT_3D('',#162468,#91578,#91579);
#77419=AXIS2_PLACEMENT_3D('',#162479,#91580,#91581);
#77420=AXIS2_PLACEMENT_3D('',#162487,#91582,#91583);
#77421=AXIS2_PLACEMENT_3D('',#162488,#91584,#91585);
#77422=AXIS2_PLACEMENT_3D('',#162499,#91586,#91587);
#77423=AXIS2_PLACEMENT_3D('',#162507,#91588,#91589);
#77424=AXIS2_PLACEMENT_3D('',#162508,#91590,#91591);
#77425=AXIS2_PLACEMENT_3D('',#162519,#91592,#91593);
#77426=AXIS2_PLACEMENT_3D('',#162527,#91594,#91595);
#77427=AXIS2_PLACEMENT_3D('',#162528,#91596,#91597);
#77428=AXIS2_PLACEMENT_3D('',#162539,#91598,#91599);
#77429=AXIS2_PLACEMENT_3D('',#162547,#91600,#91601);
#77430=AXIS2_PLACEMENT_3D('',#162548,#91602,#91603);
#77431=AXIS2_PLACEMENT_3D('',#162559,#91604,#91605);
#77432=AXIS2_PLACEMENT_3D('',#162567,#91606,#91607);
#77433=AXIS2_PLACEMENT_3D('',#162568,#91608,#91609);
#77434=AXIS2_PLACEMENT_3D('',#162579,#91610,#91611);
#77435=AXIS2_PLACEMENT_3D('',#162587,#91612,#91613);
#77436=AXIS2_PLACEMENT_3D('',#162588,#91614,#91615);
#77437=AXIS2_PLACEMENT_3D('',#162599,#91616,#91617);
#77438=AXIS2_PLACEMENT_3D('',#162607,#91618,#91619);
#77439=AXIS2_PLACEMENT_3D('',#162608,#91620,#91621);
#77440=AXIS2_PLACEMENT_3D('',#162619,#91622,#91623);
#77441=AXIS2_PLACEMENT_3D('',#162627,#91624,#91625);
#77442=AXIS2_PLACEMENT_3D('',#162628,#91626,#91627);
#77443=AXIS2_PLACEMENT_3D('',#162639,#91628,#91629);
#77444=AXIS2_PLACEMENT_3D('',#162647,#91630,#91631);
#77445=AXIS2_PLACEMENT_3D('',#162648,#91632,#91633);
#77446=AXIS2_PLACEMENT_3D('',#162659,#91634,#91635);
#77447=AXIS2_PLACEMENT_3D('',#162667,#91636,#91637);
#77448=AXIS2_PLACEMENT_3D('',#162668,#91638,#91639);
#77449=AXIS2_PLACEMENT_3D('',#162679,#91640,#91641);
#77450=AXIS2_PLACEMENT_3D('',#162687,#91642,#91643);
#77451=AXIS2_PLACEMENT_3D('',#162688,#91644,#91645);
#77452=AXIS2_PLACEMENT_3D('',#162699,#91646,#91647);
#77453=AXIS2_PLACEMENT_3D('',#162707,#91648,#91649);
#77454=AXIS2_PLACEMENT_3D('',#162708,#91650,#91651);
#77455=AXIS2_PLACEMENT_3D('',#162719,#91652,#91653);
#77456=AXIS2_PLACEMENT_3D('',#162727,#91654,#91655);
#77457=AXIS2_PLACEMENT_3D('',#162728,#91656,#91657);
#77458=AXIS2_PLACEMENT_3D('',#162739,#91658,#91659);
#77459=AXIS2_PLACEMENT_3D('',#162747,#91660,#91661);
#77460=AXIS2_PLACEMENT_3D('',#162748,#91662,#91663);
#77461=AXIS2_PLACEMENT_3D('',#162759,#91664,#91665);
#77462=AXIS2_PLACEMENT_3D('',#162767,#91666,#91667);
#77463=AXIS2_PLACEMENT_3D('',#162768,#91668,#91669);
#77464=AXIS2_PLACEMENT_3D('',#162779,#91670,#91671);
#77465=AXIS2_PLACEMENT_3D('',#162787,#91672,#91673);
#77466=AXIS2_PLACEMENT_3D('',#162788,#91674,#91675);
#77467=AXIS2_PLACEMENT_3D('',#162799,#91676,#91677);
#77468=AXIS2_PLACEMENT_3D('',#162807,#91678,#91679);
#77469=AXIS2_PLACEMENT_3D('',#162808,#91680,#91681);
#77470=AXIS2_PLACEMENT_3D('',#162819,#91682,#91683);
#77471=AXIS2_PLACEMENT_3D('',#162827,#91684,#91685);
#77472=AXIS2_PLACEMENT_3D('',#162828,#91686,#91687);
#77473=AXIS2_PLACEMENT_3D('',#162839,#91688,#91689);
#77474=AXIS2_PLACEMENT_3D('',#162847,#91690,#91691);
#77475=AXIS2_PLACEMENT_3D('',#162848,#91692,#91693);
#77476=AXIS2_PLACEMENT_3D('',#162859,#91694,#91695);
#77477=AXIS2_PLACEMENT_3D('',#162867,#91696,#91697);
#77478=AXIS2_PLACEMENT_3D('',#162868,#91698,#91699);
#77479=AXIS2_PLACEMENT_3D('',#162879,#91700,#91701);
#77480=AXIS2_PLACEMENT_3D('',#162887,#91702,#91703);
#77481=AXIS2_PLACEMENT_3D('',#162888,#91704,#91705);
#77482=AXIS2_PLACEMENT_3D('',#162899,#91706,#91707);
#77483=AXIS2_PLACEMENT_3D('',#162907,#91708,#91709);
#77484=AXIS2_PLACEMENT_3D('',#162908,#91710,#91711);
#77485=AXIS2_PLACEMENT_3D('',#162919,#91712,#91713);
#77486=AXIS2_PLACEMENT_3D('',#162927,#91714,#91715);
#77487=AXIS2_PLACEMENT_3D('',#162928,#91716,#91717);
#77488=AXIS2_PLACEMENT_3D('',#162939,#91718,#91719);
#77489=AXIS2_PLACEMENT_3D('',#162947,#91720,#91721);
#77490=AXIS2_PLACEMENT_3D('',#162948,#91722,#91723);
#77491=AXIS2_PLACEMENT_3D('',#162959,#91724,#91725);
#77492=AXIS2_PLACEMENT_3D('',#162967,#91726,#91727);
#77493=AXIS2_PLACEMENT_3D('',#162968,#91728,#91729);
#77494=AXIS2_PLACEMENT_3D('',#162979,#91730,#91731);
#77495=AXIS2_PLACEMENT_3D('',#162987,#91732,#91733);
#77496=AXIS2_PLACEMENT_3D('',#162988,#91734,#91735);
#77497=AXIS2_PLACEMENT_3D('',#162999,#91736,#91737);
#77498=AXIS2_PLACEMENT_3D('',#163007,#91738,#91739);
#77499=AXIS2_PLACEMENT_3D('',#163008,#91740,#91741);
#77500=AXIS2_PLACEMENT_3D('',#163019,#91742,#91743);
#77501=AXIS2_PLACEMENT_3D('',#163026,#91744,#91745);
#77502=AXIS2_PLACEMENT_3D('',#163051,#91747,#91748);
#77503=AXIS2_PLACEMENT_3D('',#163110,#91751,#91752);
#77504=AXIS2_PLACEMENT_3D('',#163169,#91755,#91756);
#77505=AXIS2_PLACEMENT_3D('',#163228,#91759,#91760);
#77506=AXIS2_PLACEMENT_3D('',#163287,#91763,#91764);
#77507=AXIS2_PLACEMENT_3D('',#163346,#91767,#91768);
#77508=AXIS2_PLACEMENT_3D('',#163405,#91771,#91772);
#77509=AXIS2_PLACEMENT_3D('',#163464,#91775,#91776);
#77510=AXIS2_PLACEMENT_3D('',#163523,#91779,#91780);
#77511=AXIS2_PLACEMENT_3D('',#163582,#91783,#91784);
#77512=AXIS2_PLACEMENT_3D('',#163641,#91787,#91788);
#77513=AXIS2_PLACEMENT_3D('',#163700,#91791,#91792);
#77514=AXIS2_PLACEMENT_3D('',#163759,#91795,#91796);
#77515=AXIS2_PLACEMENT_3D('',#163818,#91799,#91800);
#77516=AXIS2_PLACEMENT_3D('',#163877,#91803,#91804);
#77517=AXIS2_PLACEMENT_3D('',#163936,#91807,#91808);
#77518=AXIS2_PLACEMENT_3D('',#163995,#91811,#91812);
#77519=AXIS2_PLACEMENT_3D('',#164054,#91815,#91816);
#77520=AXIS2_PLACEMENT_3D('',#164113,#91819,#91820);
#77521=AXIS2_PLACEMENT_3D('',#164172,#91823,#91824);
#77522=AXIS2_PLACEMENT_3D('',#164231,#91827,#91828);
#77523=AXIS2_PLACEMENT_3D('',#164316,#91833,#91834);
#77524=AXIS2_PLACEMENT_3D('',#164375,#91837,#91838);
#77525=AXIS2_PLACEMENT_3D('',#164434,#91841,#91842);
#77526=AXIS2_PLACEMENT_3D('',#164493,#91845,#91846);
#77527=AXIS2_PLACEMENT_3D('',#164552,#91849,#91850);
#77528=AXIS2_PLACEMENT_3D('',#164611,#91853,#91854);
#77529=AXIS2_PLACEMENT_3D('',#164687,#91858,#91859);
#77530=AXIS2_PLACEMENT_3D('',#164688,#91860,#91861);
#77531=AXIS2_PLACEMENT_3D('',#164699,#91862,#91863);
#77532=AXIS2_PLACEMENT_3D('',#164722,#91864,#91865);
#77533=AXIS2_PLACEMENT_3D('',#164737,#91866,#91867);
#77534=AXIS2_PLACEMENT_3D('',#164753,#91868,#91869);
#77535=AXIS2_PLACEMENT_3D('',#164754,#91870,#91871);
#77536=AXIS2_PLACEMENT_3D('',#164765,#91872,#91873);
#77537=AXIS2_PLACEMENT_3D('',#164781,#91874,#91875);
#77538=AXIS2_PLACEMENT_3D('',#164782,#91876,#91877);
#77539=AXIS2_PLACEMENT_3D('',#164793,#91878,#91879);
#77540=AXIS2_PLACEMENT_3D('',#164809,#91880,#91881);
#77541=AXIS2_PLACEMENT_3D('',#164810,#91882,#91883);
#77542=AXIS2_PLACEMENT_3D('',#164821,#91884,#91885);
#77543=AXIS2_PLACEMENT_3D('',#164837,#91886,#91887);
#77544=AXIS2_PLACEMENT_3D('',#164838,#91888,#91889);
#77545=AXIS2_PLACEMENT_3D('',#164849,#91890,#91891);
#77546=AXIS2_PLACEMENT_3D('',#164865,#91892,#91893);
#77547=AXIS2_PLACEMENT_3D('',#164866,#91894,#91895);
#77548=AXIS2_PLACEMENT_3D('',#164877,#91896,#91897);
#77549=AXIS2_PLACEMENT_3D('',#164900,#91898,#91899);
#77550=AXIS2_PLACEMENT_3D('',#164915,#91900,#91901);
#77551=AXIS2_PLACEMENT_3D('',#164931,#91902,#91903);
#77552=AXIS2_PLACEMENT_3D('',#164932,#91904,#91905);
#77553=AXIS2_PLACEMENT_3D('',#164943,#91906,#91907);
#77554=AXIS2_PLACEMENT_3D('',#164959,#91908,#91909);
#77555=AXIS2_PLACEMENT_3D('',#164960,#91910,#91911);
#77556=AXIS2_PLACEMENT_3D('',#164971,#91912,#91913);
#77557=AXIS2_PLACEMENT_3D('',#164987,#91914,#91915);
#77558=AXIS2_PLACEMENT_3D('',#164988,#91916,#91917);
#77559=AXIS2_PLACEMENT_3D('',#164999,#91918,#91919);
#77560=AXIS2_PLACEMENT_3D('',#165015,#91920,#91921);
#77561=AXIS2_PLACEMENT_3D('',#165016,#91922,#91923);
#77562=AXIS2_PLACEMENT_3D('',#165027,#91924,#91925);
#77563=AXIS2_PLACEMENT_3D('',#165050,#91926,#91927);
#77564=AXIS2_PLACEMENT_3D('',#165065,#91928,#91929);
#77565=AXIS2_PLACEMENT_3D('',#165081,#91930,#91931);
#77566=AXIS2_PLACEMENT_3D('',#165082,#91932,#91933);
#77567=AXIS2_PLACEMENT_3D('',#165093,#91934,#91935);
#77568=AXIS2_PLACEMENT_3D('',#165109,#91936,#91937);
#77569=AXIS2_PLACEMENT_3D('',#165110,#91938,#91939);
#77570=AXIS2_PLACEMENT_3D('',#165121,#91940,#91941);
#77571=AXIS2_PLACEMENT_3D('',#165144,#91942,#91943);
#77572=AXIS2_PLACEMENT_3D('',#165159,#91944,#91945);
#77573=AXIS2_PLACEMENT_3D('',#165175,#91946,#91947);
#77574=AXIS2_PLACEMENT_3D('',#165176,#91948,#91949);
#77575=AXIS2_PLACEMENT_3D('',#165187,#91950,#91951);
#77576=AXIS2_PLACEMENT_3D('',#165210,#91952,#91953);
#77577=AXIS2_PLACEMENT_3D('',#165225,#91954,#91955);
#77578=AXIS2_PLACEMENT_3D('',#165241,#91956,#91957);
#77579=AXIS2_PLACEMENT_3D('',#165242,#91958,#91959);
#77580=AXIS2_PLACEMENT_3D('',#165253,#91960,#91961);
#77581=AXIS2_PLACEMENT_3D('',#165269,#91962,#91963);
#77582=AXIS2_PLACEMENT_3D('',#165270,#91964,#91965);
#77583=AXIS2_PLACEMENT_3D('',#165281,#91966,#91967);
#77584=AXIS2_PLACEMENT_3D('',#165304,#91968,#91969);
#77585=AXIS2_PLACEMENT_3D('',#165319,#91970,#91971);
#77586=AXIS2_PLACEMENT_3D('',#165342,#91972,#91973);
#77587=AXIS2_PLACEMENT_3D('',#165357,#91974,#91975);
#77588=AXIS2_PLACEMENT_3D('',#165373,#91976,#91977);
#77589=AXIS2_PLACEMENT_3D('',#165374,#91978,#91979);
#77590=AXIS2_PLACEMENT_3D('',#165385,#91980,#91981);
#77591=AXIS2_PLACEMENT_3D('',#165401,#91982,#91983);
#77592=AXIS2_PLACEMENT_3D('',#165402,#91984,#91985);
#77593=AXIS2_PLACEMENT_3D('',#165413,#91986,#91987);
#77594=AXIS2_PLACEMENT_3D('',#165429,#91988,#91989);
#77595=AXIS2_PLACEMENT_3D('',#165430,#91990,#91991);
#77596=AXIS2_PLACEMENT_3D('',#165441,#91992,#91993);
#77597=AXIS2_PLACEMENT_3D('',#165457,#91994,#91995);
#77598=AXIS2_PLACEMENT_3D('',#165458,#91996,#91997);
#77599=AXIS2_PLACEMENT_3D('',#165469,#91998,#91999);
#77600=AXIS2_PLACEMENT_3D('',#165485,#92000,#92001);
#77601=AXIS2_PLACEMENT_3D('',#165486,#92002,#92003);
#77602=AXIS2_PLACEMENT_3D('',#165497,#92004,#92005);
#77603=AXIS2_PLACEMENT_3D('',#165513,#92006,#92007);
#77604=AXIS2_PLACEMENT_3D('',#165514,#92008,#92009);
#77605=AXIS2_PLACEMENT_3D('',#165525,#92010,#92011);
#77606=AXIS2_PLACEMENT_3D('',#165541,#92012,#92013);
#77607=AXIS2_PLACEMENT_3D('',#165542,#92014,#92015);
#77608=AXIS2_PLACEMENT_3D('',#165558,#92016,#92017);
#77609=AXIS2_PLACEMENT_3D('',#165559,#92018,#92019);
#77610=AXIS2_PLACEMENT_3D('',#165624,#92021,#92022);
#77611=AXIS2_PLACEMENT_3D('',#165710,#92025,#92026);
#77612=AXIS2_PLACEMENT_3D('',#165796,#92029,#92030);
#77613=AXIS2_PLACEMENT_3D('',#165882,#92033,#92034);
#77614=AXIS2_PLACEMENT_3D('',#165967,#92037,#92038);
#77615=AXIS2_PLACEMENT_3D('',#166053,#92041,#92042);
#77616=AXIS2_PLACEMENT_3D('',#166139,#92045,#92046);
#77617=AXIS2_PLACEMENT_3D('',#166225,#92049,#92050);
#77618=AXIS2_PLACEMENT_3D('',#166311,#92053,#92054);
#77619=AXIS2_PLACEMENT_3D('',#166396,#92057,#92058);
#77620=AXIS2_PLACEMENT_3D('',#166482,#92061,#92062);
#77621=AXIS2_PLACEMENT_3D('',#166567,#92065,#92066);
#77622=AXIS2_PLACEMENT_3D('',#166652,#92069,#92070);
#77623=AXIS2_PLACEMENT_3D('',#166738,#92073,#92074);
#77624=AXIS2_PLACEMENT_3D('',#166824,#92077,#92078);
#77625=AXIS2_PLACEMENT_3D('',#166909,#92081,#92082);
#77626=AXIS2_PLACEMENT_3D('',#166994,#92085,#92086);
#77627=AXIS2_PLACEMENT_3D('',#167080,#92089,#92090);
#77628=AXIS2_PLACEMENT_3D('',#167166,#92093,#92094);
#77629=AXIS2_PLACEMENT_3D('',#167252,#92097,#92098);
#77630=AXIS2_PLACEMENT_3D('',#167337,#92101,#92102);
#77631=AXIS2_PLACEMENT_3D('',#167423,#92105,#92106);
#77632=AXIS2_PLACEMENT_3D('',#167508,#92109,#92110);
#77633=AXIS2_PLACEMENT_3D('',#167594,#92113,#92114);
#77634=AXIS2_PLACEMENT_3D('',#167678,#92117,#92118);
#77635=AXIS2_PLACEMENT_3D('',#167764,#92121,#92122);
#77636=AXIS2_PLACEMENT_3D('',#167849,#92125,#92126);
#77637=AXIS2_PLACEMENT_3D('',#167935,#92129,#92130);
#77638=AXIS2_PLACEMENT_3D('',#168021,#92133,#92134);
#77639=AXIS2_PLACEMENT_3D('',#168043,#92136,#92137);
#77640=AXIS2_PLACEMENT_3D('',#168044,#92138,#92139);
#77641=AXIS2_PLACEMENT_3D('',#168045,#92140,#92141);
#77642=AXIS2_PLACEMENT_3D('',#168046,#92142,#92143);
#77643=AXIS2_PLACEMENT_3D('',#168048,#92144,#92145);
#77644=AXIS2_PLACEMENT_3D('',#168051,#92147,#92148);
#77645=AXIS2_PLACEMENT_3D('',#168052,#92149,#92150);
#77646=AXIS2_PLACEMENT_3D('',#168055,#92151,#92152);
#77647=AXIS2_PLACEMENT_3D('',#168064,#92154,#92155);
#77648=AXIS2_PLACEMENT_3D('',#168073,#92157,#92158);
#77649=AXIS2_PLACEMENT_3D('',#168076,#92160,#92161);
#77650=AXIS2_PLACEMENT_3D('',#168078,#92162,#92163);
#77651=AXIS2_PLACEMENT_3D('',#168087,#92165,#92166);
#77652=AXIS2_PLACEMENT_3D('',#168094,#92168,#92169);
#77653=AXIS2_PLACEMENT_3D('',#168097,#92170,#92171);
#77654=AXIS2_PLACEMENT_3D('',#168098,#92172,#92173);
#77655=AXIS2_PLACEMENT_3D('',#168101,#92175,#92176);
#77656=AXIS2_PLACEMENT_3D('',#168102,#92177,#92178);
#77657=AXIS2_PLACEMENT_3D('',#168127,#92180,#92181);
#77658=AXIS2_PLACEMENT_3D('',#168136,#92183,#92184);
#77659=AXIS2_PLACEMENT_3D('',#168139,#92186,#92187);
#77660=AXIS2_PLACEMENT_3D('',#168140,#92188,#92189);
#77661=AXIS2_PLACEMENT_3D('',#168142,#92190,#92191);
#77662=AXIS2_PLACEMENT_3D('',#168150,#92192,#92193);
#77663=AXIS2_PLACEMENT_3D('',#168151,#92194,#92195);
#77664=AXIS2_PLACEMENT_3D('',#168163,#92197,#92198);
#77665=AXIS2_PLACEMENT_3D('',#168172,#92199,#92200);
#77666=AXIS2_PLACEMENT_3D('',#168173,#92201,#92202);
#77667=AXIS2_PLACEMENT_3D('',#168174,#92203,#92204);
#77668=AXIS2_PLACEMENT_3D('',#168175,#92205,#92206);
#77669=AXIS2_PLACEMENT_3D('',#168177,#92208,#92209);
#77670=AXIS2_PLACEMENT_3D('',#168187,#92212,#92213);
#77671=AXIS2_PLACEMENT_3D('',#168188,#92214,#92215);
#77672=AXIS2_PLACEMENT_3D('',#168189,#92216,#92217);
#77673=AXIS2_PLACEMENT_3D('',#168191,#92219,#92220);
#77674=AXIS2_PLACEMENT_3D('',#168192,#92221,#92222);
#77675=AXIS2_PLACEMENT_3D('',#168193,#92223,#92224);
#77676=AXIS2_PLACEMENT_3D('',#168194,#92225,#92226);
#77677=AXIS2_PLACEMENT_3D('',#168195,#92227,#92228);
#77678=AXIS2_PLACEMENT_3D('',#168198,#92229,#92230);
#77679=AXIS2_PLACEMENT_3D('',#168289,#92231,#92232);
#77680=AXIS2_PLACEMENT_3D('',#168382,#92233,#92234);
#77681=AXIS2_PLACEMENT_3D('',#168383,#92235,#92236);
#77682=AXIS2_PLACEMENT_3D('',#168384,#92237,#92238);
#77683=AXIS2_PLACEMENT_3D('',#168387,#92239,#92240);
#77684=AXIS2_PLACEMENT_3D('',#168390,#92242,#92243);
#77685=AXIS2_PLACEMENT_3D('',#168391,#92244,#92245);
#77686=AXIS2_PLACEMENT_3D('',#168392,#92246,#92247);
#77687=AXIS2_PLACEMENT_3D('',#168394,#92248,#92249);
#77688=AXIS2_PLACEMENT_3D('',#168397,#92251,#92252);
#77689=AXIS2_PLACEMENT_3D('',#168398,#92253,#92254);
#77690=AXIS2_PLACEMENT_3D('',#168400,#92255,#92256);
#77691=AXIS2_PLACEMENT_3D('',#168402,#92258,#92259);
#77692=AXIS2_PLACEMENT_3D('',#168429,#92262,#92263);
#77693=AXIS2_PLACEMENT_3D('',#168432,#92265,#92266);
#77694=AXIS2_PLACEMENT_3D('',#168433,#92267,#92268);
#77695=AXIS2_PLACEMENT_3D('',#168436,#92269,#92270);
#77696=AXIS2_PLACEMENT_3D('',#168445,#92271,#92272);
#77697=AXIS2_PLACEMENT_3D('',#168449,#92274,#92275);
#77698=AXIS2_PLACEMENT_3D('',#168458,#92276,#92277);
#77699=AXIS2_PLACEMENT_3D('',#168654,#92280,#92281);
#77700=AXIS2_PLACEMENT_3D('',#168667,#92283,#92284);
#77701=AXIS2_PLACEMENT_3D('',#169690,#92288,#92289);
#77702=AXIS2_PLACEMENT_3D('',#169871,#92290,#92291);
#77703=AXIS2_PLACEMENT_3D('',#169874,#92292,#92293);
#77704=AXIS2_PLACEMENT_3D('',#169877,#92296,#92297);
#77705=AXIS2_PLACEMENT_3D('',#169879,#92298,#92299);
#77706=AXIS2_PLACEMENT_3D('',#169881,#92301,#92302);
#77707=AXIS2_PLACEMENT_3D('',#169886,#92303,#92304);
#77708=AXIS2_PLACEMENT_3D('',#169952,#92305,#92306);
#77709=AXIS2_PLACEMENT_3D('',#169963,#92307,#92308);
#77710=AXIS2_PLACEMENT_3D('',#169965,#92310,#92311);
#77711=AXIS2_PLACEMENT_3D('',#169966,#92312,#92313);
#77712=AXIS2_PLACEMENT_3D('',#169967,#92314,#92315);
#77713=AXIS2_PLACEMENT_3D('',#169969,#92316,#92317);
#77714=AXIS2_PLACEMENT_3D('',#169993,#92320,#92321);
#77715=AXIS2_PLACEMENT_3D('',#170061,#92322,#92323);
#77716=AXIS2_PLACEMENT_3D('',#170064,#92324,#92325);
#77717=AXIS2_PLACEMENT_3D('',#170066,#92326,#92327);
#77718=AXIS2_PLACEMENT_3D('',#170068,#92328,#92329);
#77719=AXIS2_PLACEMENT_3D('',#170070,#92330,#92331);
#77720=AXIS2_PLACEMENT_3D('',#170071,#92332,#92333);
#77721=AXIS2_PLACEMENT_3D('',#170073,#92334,#92335);
#77722=AXIS2_PLACEMENT_3D('',#170074,#92336,#92337);
#77723=AXIS2_PLACEMENT_3D('',#170077,#92338,#92339);
#77724=AXIS2_PLACEMENT_3D('',#170078,#92340,#92341);
#77725=AXIS2_PLACEMENT_3D('',#170083,#92344,#92345);
#77726=AXIS2_PLACEMENT_3D('',#170088,#92348,#92349);
#77727=AXIS2_PLACEMENT_3D('',#170090,#92351,#92352);
#77728=AXIS2_PLACEMENT_3D('',#170092,#92353,#92354);
#77729=AXIS2_PLACEMENT_3D('',#170095,#92356,#92357);
#77730=AXIS2_PLACEMENT_3D('',#170096,#92358,#92359);
#77731=AXIS2_PLACEMENT_3D('',#170099,#92361,#92362);
#77732=AXIS2_PLACEMENT_3D('',#170100,#92363,#92364);
#77733=AXIS2_PLACEMENT_3D('',#170102,#92366,#92367);
#77734=AXIS2_PLACEMENT_3D('',#170103,#92368,#92369);
#77735=AXIS2_PLACEMENT_3D('',#170105,#92371,#92372);
#77736=AXIS2_PLACEMENT_3D('',#170107,#92374,#92375);
#77737=AXIS2_PLACEMENT_3D('',#170109,#92377,#92378);
#77738=AXIS2_PLACEMENT_3D('',#170110,#92379,#92380);
#77739=AXIS2_PLACEMENT_3D('',#170111,#92381,#92382);
#77740=AXIS2_PLACEMENT_3D('',#170112,#92383,#92384);
#77741=AXIS2_PLACEMENT_3D('',#170115,#92385,#92386);
#77742=AXIS2_PLACEMENT_3D('',#170116,#92387,#92388);
#77743=AXIS2_PLACEMENT_3D('',#170147,#92391,#92392);
#77744=AXIS2_PLACEMENT_3D('',#170208,#92393,#92394);
#77745=AXIS2_PLACEMENT_3D('',#170211,#92396,#92397);
#77746=AXIS2_PLACEMENT_3D('',#170212,#92398,#92399);
#77747=AXIS2_PLACEMENT_3D('',#170215,#92401,#92402);
#77748=AXIS2_PLACEMENT_3D('',#170216,#92403,#92404);
#77749=AXIS2_PLACEMENT_3D('',#170217,#92405,#92406);
#77750=AXIS2_PLACEMENT_3D('',#170218,#92407,#92408);
#77751=AXIS2_PLACEMENT_3D('',#170220,#92410,#92411);
#77752=AXIS2_PLACEMENT_3D('',#170221,#92412,#92413);
#77753=AXIS2_PLACEMENT_3D('',#170223,#92414,#92415);
#77754=AXIS2_PLACEMENT_3D('',#170226,#92417,#92418);
#77755=AXIS2_PLACEMENT_3D('',#170227,#92419,#92420);
#77756=AXIS2_PLACEMENT_3D('',#170228,#92421,#92422);
#77757=AXIS2_PLACEMENT_3D('',#170229,#92423,#92424);
#77758=AXIS2_PLACEMENT_3D('',#170230,#92425,#92426);
#77759=AXIS2_PLACEMENT_3D('',#170231,#92427,#92428);
#77760=AXIS2_PLACEMENT_3D('',#170232,#92429,#92430);
#77761=AXIS2_PLACEMENT_3D('',#170233,#92431,#92432);
#77762=AXIS2_PLACEMENT_3D('',#170234,#92433,#92434);
#77763=DIRECTION('axis',(0.,0.,1.));
#77764=DIRECTION('refdir',(1.,0.,0.));
#77765=DIRECTION('axis',(0.,0.,1.));
#77766=DIRECTION('refdir',(1.,0.,0.));
#77767=DIRECTION('center_axis',(0.,1.,0.));
#77768=DIRECTION('ref_axis',(0.,0.,1.));
#77769=DIRECTION('',(8.65956056235494E-17,-0.707106781186547,0.707106781186548));
#77770=DIRECTION('center_axis',(0.186577261580871,-0.979058294102434,-0.0814480338020183));
#77771=DIRECTION('ref_axis',(-0.0274385629108201,0.0776784846658033,-0.996600811902847));
#77772=DIRECTION('center_axis',(-0.139289712626125,0.990111866841247,0.0166393238045287));
#77773=DIRECTION('ref_axis',(0.000407580413638487,0.0168604472915263,-0.999857769482908));
#77774=DIRECTION('center_axis',(0.199724107407254,-0.979058294675158,-0.0394352196411607));
#77775=DIRECTION('ref_axis',(0.187442652303081,0.077678476402867,-0.979199319036383));
#77776=DIRECTION('center_axis',(-0.139610153019225,0.990111867364969,-0.0136928914770513));
#77777=DIRECTION('ref_axis',(0.215337916268728,0.0168604199747552,-0.976394033193217));
#77778=DIRECTION('center_axis',(0.203532073931734,-0.979058294942538,0.00442153652667557));
#77779=DIRECTION('ref_axis',(0.393559261674466,0.0776784739001359,-0.916011551369738));
#77780=DIRECTION('center_axis',(-0.133402545882498,0.990111868926104,-0.043384879436559));
#77781=DIRECTION('ref_axis',(0.420199294087297,0.0168603479300273,-0.907275196352361));
#77782=DIRECTION('center_axis',(0.197823135310267,-0.979058291315529,0.0480715023931239));
#77783=DIRECTION('ref_axis',(0.581273459592952,0.077678521741375,-0.809992106401609));
#77784=DIRECTION('center_axis',(-0.120957256826932,0.990111867075851,-0.0710481012869155));
#77785=DIRECTION('ref_axis',(0.605412613918703,0.01686043573858,-0.795733179284883));
#77786=DIRECTION('center_axis',(0.182864205781083,-0.97905828956084,0.0894737273519817));
#77787=DIRECTION('ref_axis',(0.741807964226493,0.077678545281379,-0.666098331939898));
#77788=DIRECTION('center_axis',(-0.102856105182436,0.990111866931577,-0.0953892687253966));
#77789=DIRECTION('ref_axis',(0.762317512889428,0.0168604392837559,-0.646983566351754));
#77790=DIRECTION('center_axis',(0.159354699494,-0.97905829268383,0.126692301566439));
#77791=DIRECTION('ref_axis',(0.867656361984456,0.07767850292466,-0.491058537947649));
#77792=DIRECTION('center_axis',(-0.0799455264710559,0.990111866694433,-0.115270135890139));
#77793=DIRECTION('ref_axis',(0.88357729515684,0.0168604542072331,-0.467981718197676));
#77794=DIRECTION('center_axis',(0.128393954075586,-0.97905829431996,0.157986862998561));
#77795=DIRECTION('ref_axis',(0.952934112137038,0.0776784814458654,-0.293057385926133));
#77796=DIRECTION('center_axis',(-0.0532967709437696,0.990111866732091,-0.129761109594753));
#77797=DIRECTION('ref_axis',(0.963521984490172,0.0168604521778205,-0.267097567485144));
#77798=DIRECTION('center_axis',(0.0914296854463454,-0.979058293066137,0.181894121393751));
#77799=DIRECTION('ref_axis',(0.993653715773841,0.0776784969359244,-0.0813532067137727));
#77800=DIRECTION('center_axis',(-0.024155886086191,0.990111867373155,-0.138184598469708));
#77801=DIRECTION('ref_axis',(0.998413458662092,0.0168604200989514,-0.0537242198313367));
#77802=DIRECTION('center_axis',(0.0501902985567214,-0.979058289631927,0.197296222553278));
#77803=DIRECTION('ref_axis',(0.987911176146774,0.0776785442102777,0.134154954487968));
#77804=DIRECTION('center_axis',(0.00611445816865162,0.990111867197787,-0.140146722528269));
#77805=DIRECTION('ref_axis',(0.986620226468745,0.016860430695643,0.16216119942674));
#77806=DIRECTION('center_axis',(0.00660393563905987,-0.979058296281141,
0.203472947875497));
#77807=DIRECTION('ref_axis',(0.935975012728166,0.0776784552944495,0.343390205351839));
#77808=DIRECTION('center_axis',(0.036098924614116,0.990111867548585,-0.135555735331111));
#77809=DIRECTION('ref_axis',(0.928693728838714,0.0168604130010006,0.370464147373373));
#77810=DIRECTION('center_axis',(-0.0372910827158735,-0.9790582921264,0.200135543490943));
#77811=DIRECTION('ref_axis',(0.840273696303755,0.0776785094363429,0.536568881385953));
#77812=DIRECTION('center_axis',(0.0643953951618964,0.990111866740033,-0.124626339200465));
#77813=DIRECTION('ref_axis',(0.827342546146425,0.0168604531079493,0.561444597851778));
#77814=DIRECTION('center_axis',(-0.0794425096188056,-0.979058296902983,
0.187439960869863));
#77815=DIRECTION('ref_axis',(0.705282109548452,0.0776784470943857,0.70465821843493));
#77816=DIRECTION('center_axis',(0.0896808834567414,0.990111867832051,-0.107869496710356));
#77817=DIRECTION('ref_axis',(0.68730574403223,0.0168603966824033,0.726172528566053));
#77818=DIRECTION('center_axis',(-0.117879200938036,-0.979058291676625,0.165979985195381));
#77819=DIRECTION('ref_axis',(0.537312326052278,0.0776785149589982,0.839798495227311));
#77820=DIRECTION('center_axis',(0.110772921824695,0.990111866779734,-0.0860688738881277));
#77821=DIRECTION('ref_axis',(0.515131290854236,0.0168604487200701,0.85694543493259));
#77822=DIRECTION('center_axis',(-0.150804071311457,-0.979058298006792,0.136758843150757));
#77823=DIRECTION('ref_axis',(0.344218397227483,0.077678432474775,0.935670751994741));
#77824=DIRECTION('center_axis',(0.126685382972232,0.990111867284263,-0.0602437050989526));
#77825=DIRECTION('ref_axis',(0.318869870343511,0.0168604249104656,0.947648527598155));
#77826=DIRECTION('center_axis',(-0.176677455944571,-0.979058293932153,0.101143134436385));
#77827=DIRECTION('ref_axis',(0.135029217419843,0.0776784870269465,0.987792064706024));
#77828=DIRECTION('center_axis',(0.136674164628418,0.990111867169371,-0.031601633082882));
#77829=DIRECTION('ref_axis',(0.107698451602077,0.0168604294462928,0.994040627661366));
#77830=DIRECTION('center_axis',(-0.194289620685681,-0.979058292355819,0.060798054764296));
#77831=DIRECTION('ref_axis',(-0.0804737766854639,0.0776785068362268,0.993725324645434));
#77832=DIRECTION('center_axis',(0.140272217526581,0.990111866870354,-0.00148191520592742));
#77833=DIRECTION('ref_axis',(-0.108508833586371,0.0168604463599934,0.993952493020802));
#77834=DIRECTION('center_axis',(-0.202817020749949,-0.979058292691228,0.0176100995639517));
#77835=DIRECTION('ref_axis',(-0.29221392042967,0.0776785025208492,0.953193094264347));
#77836=DIRECTION('center_axis',(0.137311299111617,0.990111866871472,0.0287071109059762));
#77837=DIRECTION('ref_axis',(-0.319642362401726,0.0168604469759247,0.947388244325427));
#77838=DIRECTION('center_axis',(-0.2018608999098,-0.979058296179043,-0.0264013213797263));
#77839=DIRECTION('ref_axis',(-0.490290465295145,0.0776784543904377,0.868090615871513));
#77840=DIRECTION('center_axis',(0.12792986861175,0.990111866429095,0.0575538067661467));
#77841=DIRECTION('ref_axis',(-0.515829767335335,0.0168604685026887,0.856525175189056));
#77842=DIRECTION('center_axis',(-0.191466007942769,-0.979058295381442,-0.0691781905461903));
#77843=DIRECTION('ref_axis',(-0.665441568100258,0.0776784663688145,0.742397181639895));
#77844=DIRECTION('center_axis',(0.112566545125586,0.990111867161873,0.0837093986582129));
#77845=DIRECTION('ref_axis',(-0.687897551371201,0.0168604299311094,0.72561193810469));
#77846=DIRECTION('center_axis',(-0.172118434479679,-0.979058289748096,-0.108720328309829));
#77847=DIRECTION('ref_axis',(-0.809477352939237,0.0776785431668268,0.581990084975651));
#77848=DIRECTION('center_axis',(0.0919397456149225,0.990111867405625,0.105950805559984));
#77849=DIRECTION('ref_axis',(-0.827800004343528,0.0168604173753996,0.560769898563378));
#77850=DIRECTION('center_axis',(-0.144722724094128,-0.979058291373611,-0.143178892380688));
#77851=DIRECTION('ref_axis',(-0.915662888444695,0.0776785204361908,0.394369778492169));
#77852=DIRECTION('center_axis',(0.067013950564489,0.990111867470249,0.123238063618005));
#77853=DIRECTION('ref_axis',(-0.928995453990013,0.0168604141435253,0.369706874294756));
#77854=DIRECTION('center_axis',(-0.110559921260368,-0.979058294096825,-0.170942565123831));
#77855=DIRECTION('ref_axis',(-0.979033047708099,0.07767848352851,0.188309173149113));
#77856=DIRECTION('center_axis',(0.0389546925791882,0.990111866893729,0.134762839693577));
#77857=DIRECTION('ref_axis',(-0.986752105339078,0.0168604464197057,0.161356772263904));
#77858=DIRECTION('center_axis',(-0.071227498148321,-0.979058293753717,-0.190713137826399));
#77859=DIRECTION('ref_axis',(-0.996624704500865,0.0776784888229868,-0.0265565576221803));
#77860=DIRECTION('center_axis',(0.00907392544468187,0.990111866858401,0.139986267123585));
#77861=DIRECTION('ref_axis',(-0.998369325900615,0.0168604452007894,-0.0545381929328624));
#77862=DIRECTION('center_axis',(-0.0285645023421519,-0.979058297482466,
-0.20156616615067));
#77863=DIRECTION('ref_axis',(-0.967615298794827,0.0776784396145497,-0.240180543669228));
#77864=DIRECTION('center_axis',(-0.021231159700138,0.990111867542855,0.138664081897897));
#77865=DIRECTION('ref_axis',(-0.963303907751991,0.0168604107174527,-0.267883011518427));
#77866=DIRECTION('center_axis',(0.0154340398695587,-0.979058293642597,-0.202994206968947));
#77867=DIRECTION('ref_axis',(-0.893361276330957,0.0776784901989675,-0.442573928415053));
#77868=DIRECTION('center_axis',(-0.0505434286098618,0.99011186673401,0.130858141423657));
#77869=DIRECTION('ref_axis',(-0.883195468264391,0.0168604534636805,-0.468701920143541));
#77870=DIRECTION('center_axis',(0.058710979286812,-0.979058295945962,-0.194930433874684));
#77871=DIRECTION('ref_axis',(-0.777334668183151,0.0776784608195143,-0.624273073554595));
#77872=DIRECTION('center_axis',(-0.0774924111311011,0.990111867436745,0.11693338350535));
#77873=DIRECTION('ref_axis',(-0.761789790422962,0.0168604166683029,-0.647604849856077));
#77874=DIRECTION('center_axis',(0.0992425885922905,-0.979058291277952,-0.177751992645369));
#77875=DIRECTION('ref_axis',(-0.624960765663839,0.0776785237983946,-0.77678187950117));
#77876=DIRECTION('center_axis',(-0.100817900230145,0.990111867381094,0.0975409712085529));
#77877=DIRECTION('ref_axis',(-0.60476366781866,0.0168604206335193,-0.796226495604474));
#77878=DIRECTION('center_axis',(0.135133781652856,-0.979058291913772,-0.152262017887209));
#77879=DIRECTION('ref_axis',(-0.443364387932586,0.0776785131344228,-0.89296924253324));
#77880=DIRECTION('center_axis',(-0.119429263971459,0.990111867544092,0.0735876392853213));
#77881=DIRECTION('ref_axis',(-0.419459468051624,0.0168604098023566,-0.907617475175057));
#77882=DIRECTION('center_axis',(0.164706260161333,-0.979058291532398,-0.119652453570032));
#77883=DIRECTION('ref_axis',(-0.24103677993988,0.077678519808337,-0.96740235593914));
#77884=DIRECTION('center_axis',(-0.132456237944713,0.990111867284881,0.0461934550686622));
#77885=DIRECTION('ref_axis',(-0.214541811918642,0.016860425481317,-0.976569268916064));
#77886=DIRECTION('',(8.65956056235494E-17,-0.707106781186547,0.707106781186548));
#77887=DIRECTION('center_axis',(0.,-1.,0.));
#77888=DIRECTION('ref_axis',(0.,0.,1.));
#77889=DIRECTION('center_axis',(1.00080200537124E-16,-1.,0.));
#77890=DIRECTION('ref_axis',(1.,1.00080200537124E-16,0.));
#77891=DIRECTION('center_axis',(-1.00080200537124E-16,1.,0.));
#77892=DIRECTION('ref_axis',(1.,1.00080200537124E-16,0.));
#77893=DIRECTION('',(1.00080200537124E-16,-1.,0.));
#77894=DIRECTION('center_axis',(1.00080200537124E-16,-1.,0.));
#77895=DIRECTION('ref_axis',(1.,1.00080200537124E-16,0.));
#77896=DIRECTION('center_axis',(0.,1.,0.));
#77897=DIRECTION('ref_axis',(0.,0.,1.));
#77898=DIRECTION('center_axis',(0.,-1.,0.));
#77899=DIRECTION('ref_axis',(0.,0.,-1.));
#77900=DIRECTION('center_axis',(0.,1.,0.));
#77901=DIRECTION('ref_axis',(0.,0.,-1.));
#77902=DIRECTION('',(0.,-1.,0.));
#77903=DIRECTION('center_axis',(0.,1.,0.));
#77904=DIRECTION('ref_axis',(0.,0.,-1.));
#77905=DIRECTION('center_axis',(-1.41610079671576E-16,-1.,0.));
#77906=DIRECTION('ref_axis',(1.,-1.41610079671576E-16,0.));
#77907=DIRECTION('center_axis',(0.,1.,0.));
#77908=DIRECTION('ref_axis',(0.,0.,-1.));
#77909=DIRECTION('',(-1.41610079671576E-16,-1.,0.));
#77910=DIRECTION('center_axis',(1.41610079671576E-16,1.,0.));
#77911=DIRECTION('ref_axis',(1.,-1.41610079671576E-16,0.));
#77912=DIRECTION('center_axis',(0.,1.,0.));
#77913=DIRECTION('ref_axis',(0.,0.,-1.));
#77914=DIRECTION('center_axis',(1.41610079671576E-16,1.,0.));
#77915=DIRECTION('ref_axis',(-1.,1.41610079671576E-16,0.));
#77916=DIRECTION('',(0.707106781186548,0.707106781186547,-8.65956056235493E-17));
#77917=DIRECTION('center_axis',(0.,1.,0.));
#77918=DIRECTION('ref_axis',(0.,0.,1.));
#77919=DIRECTION('center_axis',(-2.19359866955191E-16,-1.,2.19359867215408E-16));
#77920=DIRECTION('ref_axis',(8.25587254851516E-33,-2.19359867215408E-16,
-1.));
#77921=DIRECTION('center_axis',(-0.132456237432219,-0.990111867233412,0.0461934576413813));
#77922=DIRECTION('ref_axis',(-0.17180492619258,-0.0229646841998517,-0.984863285240933));
#77923=DIRECTION('center_axis',(0.164706267778703,0.979058293558939,-0.119652426502217));
#77924=DIRECTION('ref_axis',(-0.277967410339795,-0.0703182237971854,-0.958013291239217));
#77925=DIRECTION('center_axis',(-0.119429259911198,-0.990111867327141,0.0735876487939799));
#77926=DIRECTION('ref_axis',(-0.379504716404044,-0.0229646761552871,-0.92490474854234));
#77927=DIRECTION('center_axis',(0.135133794647117,0.97905829393374,-0.152261993366125));
#77928=DIRECTION('ref_axis',(-0.477413223582112,-0.0703182187181641,-0.875860697865386));
#77929=DIRECTION('center_axis',(-0.100817898675726,-0.990111867329304,0.0975409733409004));
#77930=DIRECTION('ref_axis',(-0.569459287429209,-0.0229646794472329,-0.821698693840086));
#77931=DIRECTION('center_axis',(0.0992426063939419,0.979058293251314,-0.177751971837055));
#77932=DIRECTION('ref_axis',(-0.654535729064363,-0.0703182292933112,-0.752753828291319));
#77933=DIRECTION('center_axis',(-0.0774924094683679,-0.990111867394032,
0.116933384968924));
#77934=DIRECTION('ref_axis',(-0.732786575137973,-0.0229646753529087,-0.680070922024678));
#77935=DIRECTION('center_axis',(0.0587110024176738,0.979058298035316,-0.194930416413916));
#77936=DIRECTION('ref_axis',(-0.801052866818017,-0.0703181640084746,-0.594449039340728));
#77937=DIRECTION('center_axis',(-0.0505434261743817,-0.990111866679012,
0.130858142780482));
#77938=DIRECTION('ref_axis',(-0.861849579756916,-0.0229647121534493,-0.506643784002663));
#77939=DIRECTION('center_axis',(0.0154340585899416,0.97905829512376,-0.202994198401821));
#77940=DIRECTION('ref_axis',(-0.910113666004715,-0.0703182038275187,-0.408348460462299));
#77941=DIRECTION('center_axis',(-0.0212311576904246,-0.990111867502716,
0.138664082492217));
#77942=DIRECTION('ref_axis',(-0.950613451622889,-0.0229646696475091,-0.309526557086138));
#77943=DIRECTION('center_axis',(-0.0285644827311666,0.979058298926961,-0.201566161913518));
#77944=DIRECTION('ref_axis',(-0.976618566039829,-0.0703181511606769,-0.20315396644824));
#77945=DIRECTION('center_axis',(0.00907392867735618,-0.990111866793656,
0.139986267371983));
#77946=DIRECTION('ref_axis',(-0.994927697509577,-0.0229647039748019,-0.097936199128008));
#77947=DIRECTION('center_axis',(-0.0712274703710536,0.979058295754626,-0.19071313792864));
#77948=DIRECTION('ref_axis',(-0.997457861197093,-0.0703181955432002,0.011539779532913));
#77949=DIRECTION('center_axis',(0.0389546957459753,-0.990111866829932,0.134762839246897));
#77950=DIRECTION('ref_axis',(-0.992720228666671,-0.0229647050205448,0.118233539739415));
#77951=DIRECTION('center_axis',(-0.11055990363582,0.979058295394851,-0.17094256908847));
#77952=DIRECTION('ref_axis',(-0.9716571385588,-0.0703182001743572,0.225693942789707));
#77953=DIRECTION('center_axis',(0.067013960412375,-0.99011186725026,0.123238060030383));
#77954=DIRECTION('ref_axis',(-0.94409426681622,-0.0229646803965615,0.328874807212452));
#77955=DIRECTION('center_axis',(-0.144722697903038,0.979058293473277,-0.143178904496649));
#77956=DIRECTION('ref_axis',(-0.900422803742289,-0.0703182258289589,0.42929491217244));
#77957=DIRECTION('center_axis',(0.0919397473787764,-0.990111867365221,0.105950804406956));
#77958=DIRECTION('ref_axis',(-0.851323506878691,-0.0229646761936634,0.524138254931929));
#77959=DIRECTION('center_axis',(-0.172118405928228,0.979058292352157,-0.10872035006016));
#77960=DIRECTION('ref_axis',(-0.787085695174323,-0.0703182391658995,0.612822530340196));
#77961=DIRECTION('center_axis',(0.112566547260454,-0.990111867101572,0.0837093965006225));
#77962=DIRECTION('ref_axis',(-0.718745802161697,-0.0229646885380385,0.694893585346195));
#77963=DIRECTION('center_axis',(-0.191465991434706,0.979058297226015,-0.0691782101302217));
#77964=DIRECTION('ref_axis',(-0.636945360128415,-0.0703181754281751,0.767695227558004));
#77965=DIRECTION('center_axis',(0.127929874677976,-0.990111866193421,0.0575537973365679));
#77966=DIRECTION('ref_axis',(-0.552560338942516,-0.0229647350323582,0.833156463560492));
#77967=DIRECTION('center_axis',(-0.201860887006352,0.979058298183124,-0.0264013457190201));
#77968=DIRECTION('ref_axis',(-0.457022157547164,-0.0703181629482099,0.886671361593755));
#77969=DIRECTION('center_axis',(0.137311300220315,-0.990111866806451,0.0287071078454626));
#77970=DIRECTION('ref_axis',(-0.360537777972085,-0.022964705770711,0.932461866750494));
#77971=DIRECTION('center_axis',(-0.202817012634927,0.979058294905287,0.017610069931631));
#77972=DIRECTION('ref_axis',(-0.25572908737288,-0.0703182060782421,0.964187732635804));
#77973=DIRECTION('center_axis',(0.140272217935505,-0.990111866807758,-0.00148191832138533));
#77974=DIRECTION('ref_axis',(-0.151656867142916,-0.0229647050615583,0.988166391337932));
#77975=DIRECTION('center_axis',(-0.194289619523623,0.979058294022983,0.0607980316307452));
#77976=DIRECTION('ref_axis',(-0.0424784197587449,-0.0703182187381587,0.996619752949084));
#77977=DIRECTION('center_axis',(0.136674163840837,-0.990111866959273,-0.0316016430716887));
#77978=DIRECTION('ref_axis',(0.064315347849392,-0.0229646960050964,0.99766535409846));
#77979=DIRECTION('center_axis',(-0.176677458323459,0.979058295023467,0.101143119717087));
#77980=DIRECTION('ref_axis',(0.172758496808971,-0.0703182041316549,0.982450941242362));
#77981=DIRECTION('',(2.41706455067744E-16,0.707106781186547,-0.707106781186548));
#77982=DIRECTION('center_axis',(0.,1.,0.));
#77983=DIRECTION('ref_axis',(0.,0.,-1.));
#77984=DIRECTION('center_axis',(0.126685420716261,-0.990111870073335,-0.0602435798888724));
#77985=DIRECTION('ref_axis',(0.277280230621252,-0.0229645520370101,0.960514603249927));
#77986=DIRECTION('center_axis',(-0.150804080106185,0.979058299695095,0.136758821366216));
#77987=DIRECTION('ref_axis',(0.379917397187823,-0.0703181421635682,0.922343824285008));
#77988=DIRECTION('center_axis',(0.110772920956554,-0.990111866747598,-0.0860688753751264));
#77989=DIRECTION('ref_axis',(0.477279840221599,-0.0229647061293327,0.878451237343564));
#77990=DIRECTION('center_axis',(-0.117879212274808,0.979058293114798,0.165979968660709));
#77991=DIRECTION('ref_axis',(0.569311805615098,-0.0703182285970028,0.81910891504992));
#77992=DIRECTION('center_axis',(0.0896809564689254,-0.990111870174351,-0.107869414509709));
#77993=DIRECTION('ref_axis',(0.654962335239065,-0.0229645446167437,0.755312497651625));
#77994=DIRECTION('center_axis',(-0.079442525689017,0.979058298513707,0.18743994564552));
#77995=DIRECTION('ref_axis',(0.732085813543258,-0.0703181579044715,0.677573404346442));
#77996=DIRECTION('center_axis',(0.0643953874484482,-0.990111866540803,-0.124626344768881));
#77997=DIRECTION('ref_axis',(0.802019552937378,-0.0229647181121548,0.596856145505898));
#77998=DIRECTION('center_axis',(-0.0372911082222741,0.979058294286732,0.200135528170063));
#77999=DIRECTION('ref_axis',(0.860628304192011,-0.0703182148874076,0.504355302022922));
#78000=DIRECTION('center_axis',(0.0360989233961526,-0.99011186752518,-0.135555735826411));
#78001=DIRECTION('ref_axis',(0.911575207860454,-0.0229646702411923,0.41049149118451));
#78002=DIRECTION('center_axis',(0.00660391626934577,0.979058297745836,0.203472941456433));
#78003=DIRECTION('ref_axis',(0.948928776319299,-0.0703181684385485,0.307554113385929));
#78004=DIRECTION('center_axis',(0.00611444907722728,-0.990111867003953,
-0.140146724294321));
#78005=DIRECTION('ref_axis',(0.978506622816256,-0.0229646957655209,0.204932700790093));
#78006=DIRECTION('center_axis',(0.0501902716064893,0.979058291601222,0.197296219636775));
#78007=DIRECTION('ref_axis',(0.992858387487948,-0.0703182513499916,0.0963720183554905));
#78008=DIRECTION('center_axis',(-0.0241558955906642,-0.990111867174055,
-0.138184598234822));
#78009=DIRECTION('ref_axis',(0.99968415489381,-0.0229646848998216,-0.0102085112382318));
#78010=DIRECTION('center_axis',(0.0914296553058276,0.979058295267563,0.181894124694642));
#78011=DIRECTION('ref_axis',(0.990363050457822,-0.0703182019202536,-0.119316297154157));
#78012=DIRECTION('center_axis',(-0.0532966435780096,-0.990111869527684,
-0.129761140576499));
#78013=DIRECTION('ref_axis',(0.974117573573207,-0.022964579190007,-0.224872365928926));
#78014=DIRECTION('center_axis',(0.128393931794312,0.979058296012373,0.157986870618246));
#78015=DIRECTION('ref_axis',(0.941559434212215,-0.07031819095881,-0.329425536147783));
#78016=DIRECTION('center_axis',(-0.0799455276086676,-0.990111866671711,
-0.115270135296317));
#78017=DIRECTION('ref_axis',(0.903002322585386,-0.0229647115823865,-0.429021476650454));
#78018=DIRECTION('center_axis',(0.159354683412349,0.979058294034251,0.126692311358236));
#78019=DIRECTION('ref_axis',(0.848729542341873,-0.0703182181081923,-0.52413119746705));
#78020=DIRECTION('center_axis',(-0.102856112067682,-0.990111866747235,-0.0953892632146105));
#78021=DIRECTION('ref_axis',(0.789663694904801,-0.0229647044494264,-0.613109999346649));
#78022=DIRECTION('center_axis',(0.182864183474596,0.979058291793841,0.0894737485070039));
#78023=DIRECTION('ref_axis',(0.716213996241899,-0.0703182473574262,-0.694329068724469));
#78024=DIRECTION('center_axis',(-0.120957257720643,-0.990111867049381,-0.0710481001342749));
#78025=DIRECTION('ref_axis',(0.639401271429582,-0.0229646931575987,-0.768530179604166));
#78026=DIRECTION('center_axis',(0.197823121059548,0.979058293153051,0.0480715236131955));
#78027=DIRECTION('ref_axis',(0.550209090024204,-0.0703182290405912,-0.832060877532006));
#78028=DIRECTION('center_axis',(-0.133402538460898,-0.990111869283228,-0.0433848941068217));
#78029=DIRECTION('ref_axis',(0.459241170939672,-0.0229645894669955,-0.888014737796942));
#78030=DIRECTION('center_axis',(0.20353206298097,0.979058297093515,0.0044215643223696));
#78031=DIRECTION('ref_axis',(0.358477019304043,-0.0703181752952904,-0.930886448958212));
#78032=DIRECTION('center_axis',(-0.139610155127693,-0.990111867183911,-0.0136928830715721));
#78033=DIRECTION('ref_axis',(0.25760743208348,-0.0229646850592621,-0.965976725483324));
#78034=DIRECTION('center_axis',(0.199724103311477,0.979058296518537,-0.0394351946191106));
#78035=DIRECTION('ref_axis',(0.149982958526831,-0.0703181840904617,-0.98618480273109));
#78036=DIRECTION('center_axis',(-0.139289712644573,-0.990111866811864,0.0166393253985151));
#78037=DIRECTION('ref_axis',(0.0439282684083753,-0.0229647047719847,-0.998770709206761));
#78038=DIRECTION('center_axis',(0.186577263105276,0.979058295973938,-0.0814480078132881));
#78039=DIRECTION('ref_axis',(-0.0655241373408622,-0.0703181926540497,-0.995370252322021));
#78040=DIRECTION('center_axis',(-7.60853361304994E-16,1.,9.435877229074E-15));
#78041=DIRECTION('ref_axis',(3.09497666338474E-33,-9.435877229074E-15,1.));
#78042=DIRECTION('center_axis',(-0.176808658942607,0.98271042847198,-0.0549446257183899));
#78043=DIRECTION('ref_axis',(-0.186626169750472,0.0213383782231432,0.982199239655109));
#78044=DIRECTION('center_axis',(-0.135281219501057,-0.990789414020337,0.00594379639156948));
#78045=DIRECTION('ref_axis',(0.057133312143485,-0.00181167293401717,0.998364914490035));
#78046=DIRECTION('center_axis',(3.05467988155942E-15,1.,7.62291531082259E-17));
#78047=DIRECTION('ref_axis',(-1.,3.05467988155942E-15,-2.11360725830771E-35));
#78048=DIRECTION('center_axis',(-0.0132749943721122,-0.990789503434023,
-0.134758800860587));
#78049=DIRECTION('ref_axis',(-0.993807435046363,-0.00179566446072954,0.111101564506143));
#78050=DIRECTION('center_axis',(-1.85512445524357E-14,-1.,-4.76054075061197E-16));
#78051=DIRECTION('ref_axis',(1.,-1.85512445524357E-14,-1.98009382376506E-33));
#78052=DIRECTION('center_axis',(-0.0168422547262398,0.987363722175752,0.157572899278335));
#78053=DIRECTION('ref_axis',(0.999535337253718,0.0126220396434726,0.0277451562679874));
#78054=DIRECTION('center_axis',(-0.0337801347625192,-0.987363722337789,
0.15482823484976));
#78055=DIRECTION('ref_axis',(0.994438499473259,-0.0177432088148472,0.103813531422087));
#78056=DIRECTION('center_axis',(-2.55442508253129E-28,-1.,1.25044650541671E-14));
#78057=DIRECTION('ref_axis',(-2.04281036531029E-14,1.25044650541671E-14,
1.));
#78058=DIRECTION('center_axis',(-0.00706164953990097,-0.987363724136274,
-0.158313010727242));
#78059=DIRECTION('ref_axis',(0.99876285352069,0.000828878792820405,-0.0497199697018763));
#78060=DIRECTION('center_axis',(2.48501675249087E-15,-1.,4.74426298407864E-14));
#78061=DIRECTION('ref_axis',(-5.11224396500914E-33,-4.74426298407864E-14,
-1.));
#78062=DIRECTION('center_axis',(-0.158463153814555,-0.987363722560973,-0.0015192938104477));
#78063=DIRECTION('ref_axis',(-0.0274754674163315,0.00594769935929276,-0.999604783683324));
#78064=DIRECTION('center_axis',(-0.15769850577066,0.987363722272492,0.0156224587664822));
#78065=DIRECTION('ref_axis',(-0.103719826367577,-0.00082873932965462,-0.99460620891356));
#78066=DIRECTION('center_axis',(9.74404812678745E-14,-1.,-8.14357426664195E-15));
#78067=DIRECTION('ref_axis',(1.,9.74404812678745E-14,3.07580761015643E-31));
#78068=DIRECTION('center_axis',(0.0182306309460133,0.990568175243044,-0.135802556275557));
#78069=DIRECTION('ref_axis',(0.998320981674736,-0.010565373254294,0.0569525279156969));
#78070=DIRECTION('center_axis',(6.38404008822679E-15,-1.,-2.3030484033016E-13));
#78071=DIRECTION('ref_axis',(-2.77453764336849E-31,2.3030484033016E-13,
-1.));
#78072=DIRECTION('center_axis',(-0.134616404784531,0.990568175273701,-0.0255560892512512));
#78073=DIRECTION('ref_axis',(0.110917009834759,-0.0105653661152137,-0.9937735103977));
#78074=DIRECTION('center_axis',(-2.22618915808562E-14,-1.,-5.55542708669342E-16));
#78075=DIRECTION('ref_axis',(1.,-2.22618915808562E-14,2.18343570758325E-34));
#78076=DIRECTION('center_axis',(0.0197674306362294,0.987366228452097,0.157216982537903));
#78077=DIRECTION('ref_axis',(0.999508415206963,-0.0233430450078669,0.0209291705575077));
#78078=DIRECTION('center_axis',(0.000293086686366353,-0.987363722527596,
0.158470166077536));
#78079=DIRECTION('ref_axis',(0.995082110070574,0.0159849159468142,0.097755187482131));
#78080=DIRECTION('center_axis',(1.18727964638572E-13,-1.,3.04674604886636E-15));
#78081=DIRECTION('ref_axis',(1.,1.18727964638572E-13,1.30307348022364E-31));
#78082=DIRECTION('center_axis',(0.,1.,1.27213054916354E-15));
#78083=DIRECTION('ref_axis',(0.,1.27213054916354E-15,-1.));
#78084=DIRECTION('center_axis',(-0.0337729883191399,0.987363878725217,0.154828796574441));
#78085=DIRECTION('ref_axis',(0.998165425040037,0.0255338649981846,0.0548981419803683));
#78086=DIRECTION('center_axis',(-0.0168421293105201,-0.98736372378855,0.157572902577489));
#78087=DIRECTION('ref_axis',(0.994871215031476,-0.000828295926089754,0.101146326812457));
#78088=DIRECTION('center_axis',(-0.00706160151274273,0.987363724410389,
-0.158313011159923));
#78089=DIRECTION('ref_axis',(0.99997506488799,0.00696332996270449,-0.00117543102288484));
#78090=DIRECTION('center_axis',(-7.86340814423373E-13,-1.,-1.99922748743582E-14));
#78091=DIRECTION('ref_axis',(1.,-7.86340814423373E-13,4.46218307380314E-31));
#78092=DIRECTION('center_axis',(0.0312919785426607,0.983673454219395,0.177221182545905));
#78093=DIRECTION('ref_axis',(0.987338299412827,-0.00283415220946001,-0.158603436576389));
#78094=DIRECTION('center_axis',(-4.10830010678278E-15,-1.,-7.78005123770473E-14));
#78095=DIRECTION('ref_axis',(-7.54086921167661E-33,7.78005123770473E-14,
-1.));
#78096=DIRECTION('center_axis',(-0.154562215376398,-0.987363722188387,0.0349771594649241));
#78097=DIRECTION('ref_axis',(-0.0341799369672018,-0.0300375664419585,-0.998964201816643));
#78098=DIRECTION('center_axis',(0.,-1.,0.));
#78099=DIRECTION('ref_axis',(0.,0.,-1.));
#78100=DIRECTION('center_axis',(-0.15769850569658,-0.987363722272805,0.0156224594944755));
#78101=DIRECTION('ref_axis',(-0.030668260820034,-0.0109157756374432,-0.999470011366278));
#78102=DIRECTION('center_axis',(-0.158463153814891,0.987363722560907,-0.00151929381848589));
#78103=DIRECTION('ref_axis',(-0.101017486121261,-0.0177430370825393,-0.994726420747347));
#78104=DIRECTION('center_axis',(-1.48410173663198E-14,-1.,-3.79995350315268E-16));
#78105=DIRECTION('ref_axis',(1.,-1.48410173663198E-14,-3.46998329439956E-33));
#78106=DIRECTION('center_axis',(-0.0144017677944871,0.987363722001651,0.157814668391251));
#78107=DIRECTION('ref_axis',(0.999573197091345,0.010204689755033,0.0273731248415481));
#78108=DIRECTION('center_axis',(-0.0361720565029735,-0.987363723272852,
0.154286941421227));
#78109=DIRECTION('ref_axis',(0.994359178185766,-0.0201564605092843,0.104132328589471));
#78110=DIRECTION('center_axis',(1.48412610539896E-13,-1.,3.70361805778659E-15));
#78111=DIRECTION('ref_axis',(1.,1.48412610539896E-13,-1.33068137671809E-31));
#78112=DIRECTION('center_axis',(0.000293086690297423,0.987363722527305,
0.158470166079342));
#78113=DIRECTION('ref_axis',(0.999682616725007,-0.00428129299861851,0.0248261222929015));
#78114=DIRECTION('center_axis',(0.019767304632634,-0.987366232852948,0.157216970742152));
#78115=DIRECTION('ref_axis',(0.994881286324056,0.0350112846596324,0.0947915400691157));
#78116=DIRECTION('center_axis',(4.9720804442767E-15,-1.,9.49634653907226E-14));
#78117=DIRECTION('ref_axis',(-6.2871554490736E-32,-9.49634653907226E-14,
-1.));
#78118=DIRECTION('center_axis',(-0.158467690148794,-0.98736372246051,0.000933138698494708));
#78119=DIRECTION('ref_axis',(-0.0278902213647363,0.00353155478491395,-0.999604753726705));
#78120=DIRECTION('center_axis',(-0.157921387631135,0.98736372262811,0.0131800821931044));
#78121=DIRECTION('ref_axis',(-0.0301712582658057,0.00851653398384107,-0.999508461106538));
#78122=DIRECTION('center_axis',(-6.57328045624156E-15,-1.,-1.24480823416616E-13));
#78123=DIRECTION('ref_axis',(2.84794430263569E-31,1.24480823416616E-13,
-1.));
#78124=DIRECTION('center_axis',(-0.154562215376524,0.987363722188496,0.0349771594612696));
#78125=DIRECTION('ref_axis',(-0.107590663502521,0.0183708777819135,-0.994025532859498));
#78126=DIRECTION('center_axis',(2.96824138671882E-14,-1.,7.45035423054637E-16));
#78127=DIRECTION('ref_axis',(1.,2.96824138671882E-14,7.65123809267896E-33));
#78128=DIRECTION('center_axis',(-0.0021592520811022,-0.987363722029701,
0.158455728991117));
#78129=DIRECTION('ref_axis',(0.995065899253389,0.0135962687787092,0.0982801995233089));
#78130=DIRECTION('center_axis',(-1.64176650023047E-15,-1.,-3.10613620490506E-14));
#78131=DIRECTION('ref_axis',(1.6108732260432E-32,3.10613620490506E-14,-1.));
#78132=DIRECTION('center_axis',(-0.154002427947643,-0.987363722886881,0.0373648352490626));
#78133=DIRECTION('ref_axis',(-0.0344441834552631,-0.0324282855855283,-0.998880375480509));
#78134=DIRECTION('center_axis',(0.,-1.,0.));
#78135=DIRECTION('ref_axis',(0.,0.,-1.));
#78136=DIRECTION('center_axis',(-0.157921391999,-0.987363722490913,0.0131800401359445));
#78137=DIRECTION('ref_axis',(-0.103290603183284,0.00324330582810751,-0.994645933114563));
#78138=DIRECTION('center_axis',(-0.158467690148881,0.9873637224605,0.000933138694840477));
#78139=DIRECTION('ref_axis',(-0.101358811973182,-0.0153275572955993,-0.994731851919267));
#78140=DIRECTION('center_axis',(7.42052235095029E-15,-1.,1.89466780213044E-16));
#78141=DIRECTION('ref_axis',(1.,7.42052235095029E-15,1.87127582003944E-33));
#78142=DIRECTION('center_axis',(-0.0119578465267453,0.987363721826008,0.158018640445792));
#78143=DIRECTION('ref_axis',(0.994954618366562,-0.00399376455237794,0.100246482410856));
#78144=DIRECTION('center_axis',(-0.0385553989335021,-0.987363721912245,
0.153708691571677));
#78145=DIRECTION('ref_axis',(0.994276083765525,-0.0225679920880593,0.104430622831643));
#78146=DIRECTION('center_axis',(-8.90472416013529E-14,-1.,-2.23510626916282E-15));
#78147=DIRECTION('ref_axis',(1.,-8.90472416013529E-14,4.2396213639188E-33));
#78148=DIRECTION('center_axis',(-0.0021592520907733,0.987363722029776,0.158455728990515));
#78149=DIRECTION('ref_axis',(0.999678494100297,-0.00187187841216595,0.0252864490305052));
#78150=DIRECTION('center_axis',(3.31562974260561E-15,-1.,6.33437378569497E-14));
#78151=DIRECTION('ref_axis',(8.73037930690793E-32,-6.33437378569497E-14,
-1.));
#78152=DIRECTION('center_axis',(-0.158434275571817,-0.987363722236215,0.00338531178472703));
#78153=DIRECTION('ref_axis',(-0.0283192539122514,0.00111690203907079,-0.999598305514614));
#78154=DIRECTION('center_axis',(-0.158106451168979,0.9873637206975,0.0107346704253699));
#78155=DIRECTION('ref_axis',(-0.0296886063097194,0.00611302356839794,-0.999540503230479));
#78156=DIRECTION('center_axis',(-1.31341320018242E-14,-1.,-2.48490896391667E-13));
#78157=DIRECTION('ref_axis',(2.71489283531412E-31,2.48490896391667E-13,
-1.));
#78158=DIRECTION('center_axis',(-0.154002427947475,0.987363722886904,0.0373648352491493));
#78159=DIRECTION('ref_axis',(-0.108056979266439,0.0207592358981631,-0.993927936702021));
#78160=DIRECTION('center_axis',(-8.90469496711449E-14,-1.,-2.24670375016886E-15));
#78161=DIRECTION('ref_axis',(1.,-8.90469496711449E-14,4.9175005361357E-33));
#78162=DIRECTION('center_axis',(-0.00461116000528831,-0.987363722279733,
0.158403336862949));
#78163=DIRECTION('ref_axis',(0.995045043403193,0.0112022349341195,0.0987920620860687));
#78164=DIRECTION('center_axis',(-1.48410446953476E-14,-1.,-3.7893356050524E-16));
#78165=DIRECTION('ref_axis',(1.,-1.48410446953476E-14,7.48510576451842E-33));
#78166=DIRECTION('center_axis',(-0.0385554684073366,0.987363720853985,0.153708680943092));
#78167=DIRECTION('ref_axis',(0.998951850321529,0.0342871341096827,0.0303247947023321));
#78168=DIRECTION('center_axis',(-0.0119578595718116,-0.987363721877783,
0.158018639135111));
#78169=DIRECTION('ref_axis',(0.99960551080179,-0.00778744826191416,0.0269847813454248));
#78170=DIRECTION('center_axis',(-1.64083644641347E-15,-1.,-3.1026163518096E-14));
#78171=DIRECTION('ref_axis',(-4.16554257031589E-32,3.1026163518096E-14,
-1.));
#78172=DIRECTION('center_axis',(-0.153405755446833,-0.987363722291718,0.0397436044921545));
#78173=DIRECTION('ref_axis',(-0.0346645641532703,-0.0348178308286464,-0.998792314071575));
#78174=DIRECTION('center_axis',(-8.28907435649917E-15,-1.,-1.58359344641865E-13));
#78175=DIRECTION('ref_axis',(-1.73313891738106E-31,1.58359344641865E-13,
-1.));
#78176=DIRECTION('center_axis',(-0.158106468985132,-0.987363719717749,0.0107344981337491));
#78177=DIRECTION('ref_axis',(-0.102875893860418,0.00565948901390946,-0.994678099008177));
#78178=DIRECTION('center_axis',(-0.158434275572002,0.987363722236204,0.00338531177914169));
#78179=DIRECTION('ref_axis',(-0.101715674405555,-0.0129109249611921,-0.994729726909209));
#78180=DIRECTION('center_axis',(1.0388754068593E-13,-1.,2.64359607576203E-15));
#78181=DIRECTION('ref_axis',(1.,1.0388754068593E-13,5.92047222134529E-32));
#78182=DIRECTION('center_axis',(-0.00951105075573686,0.987363721760132,
0.158184768121028));
#78183=DIRECTION('ref_axis',(0.994989346787542,-0.00640051446526875,0.099775914898743));
#78184=DIRECTION('center_axis',(-1.65804226685395E-15,-1.,-3.16805598989081E-14));
#78185=DIRECTION('ref_axis',(-1.16984757162064E-32,3.16805598989081E-14,
-1.));
#78186=DIRECTION('center_axis',(-0.158362916658971,-0.987363722017152,0.0058367004121401));
#78187=DIRECTION('ref_axis',(-0.0287622556155261,-0.00129577990078118,-0.999585440873543));
#78188=DIRECTION('center_axis',(-0.158253626805769,0.987363722312596,0.00828670403938214));
#78189=DIRECTION('ref_axis',(0.00319663291263429,0.00890473459932685,-0.999955242618257));
#78190=DIRECTION('center_axis',(8.20418223212712E-15,-1.,1.55130817591217E-13));
#78191=DIRECTION('ref_axis',(-9.2586468910808E-32,-1.55130817591217E-13,
-1.));
#78192=DIRECTION('center_axis',(-0.15340575544681,0.987363722291716,0.0397436044922978));
#78193=DIRECTION('ref_axis',(-0.108481104460266,0.0231492387674881,-0.993828940371313));
#78194=DIRECTION('center_axis',(8.90466898519274E-14,-1.,2.25697728440651E-15));
#78195=DIRECTION('ref_axis',(1.,8.90466898519274E-14,5.52639293368189E-33));
#78196=DIRECTION('center_axis',(-0.00706194294935648,-0.987363722357662,
0.158313008732074));
#78197=DIRECTION('ref_axis',(0.995019539373588,0.00880345907900943,0.0992905603419373));
#78198=DIRECTION('center_axis',(1.48410772232726E-14,-1.,3.77656582478035E-16));
#78199=DIRECTION('ref_axis',(1.,1.48410772232726E-14,7.44759712696477E-33));
#78200=DIRECTION('center_axis',(-0.00951107056456808,-0.987363721886882,
0.158184766138841));
#78201=DIRECTION('ref_axis',(0.999632196233728,-0.00537048632003542,0.0265825154870454));
#78202=DIRECTION('center_axis',(-4.92158011612943E-15,-1.,-9.30433417784878E-14));
#78203=DIRECTION('ref_axis',(2.13564600095701E-32,9.30433417784878E-14,
-1.));
#78204=DIRECTION('center_axis',(0.,-1.,0.));
#78205=DIRECTION('ref_axis',(0.,0.,-1.));
#78206=DIRECTION('center_axis',(-0.158253626805765,-0.987363722312595,0.00828670403948867));
#78207=DIRECTION('ref_axis',(0.00319663291261748,-0.00890473459943204,-0.999955242618256));
#78208=DIRECTION('center_axis',(-0.158362916658982,0.987363722017151,0.00583670041201556));
#78209=DIRECTION('ref_axis',(-0.102087694185998,-0.0104936223845458,-0.994720054379641));
#78210=DIRECTION('center_axis',(-4.45233449258842E-14,-1.,-1.12848864220478E-15));
#78211=DIRECTION('ref_axis',(1.,-4.45233449258842E-14,1.38159831301423E-33));
#78212=DIRECTION('center_axis',(-0.00706194293192785,0.987363722357751,
0.158313008732295));
#78213=DIRECTION('ref_axis',(0.999653270055242,0.00295455998075385,0.026165057675858));
#78214=DIRECTION('center_axis',(0.158065644955521,0.987363722085681,0.0113195491917563));
#78215=DIRECTION('ref_axis',(0.0998162412145389,-0.0273822810115699,0.994629040736497));
#78216=DIRECTION('',(-0.60378640685546,0.,0.797146144001571));
#78217=DIRECTION('center_axis',(0.163668137701704,0.986495111192551,0.00633532117995019));
#78218=DIRECTION('ref_axis',(0.132080328024876,-0.0282764738460143,0.990835621067227));
#78219=DIRECTION('center_axis',(-0.154431767589658,0.98736372233359,0.0355486846267493));
#78220=DIRECTION('ref_axis',(0.242224239385166,0.0029545567318824,0.970215794784231));
#78221=DIRECTION('center_axis',(-0.160735572549779,0.986495109335916,0.0314876955875371));
#78222=DIRECTION('ref_axis',(0.137589022940416,-0.00919562022103512,0.990446718069706));
#78223=DIRECTION('',(-0.797146142410778,0.,-0.603786408955697));
#78224=DIRECTION('center_axis',(0.,-1.,0.));
#78225=DIRECTION('ref_axis',(0.,0.,-1.));
#78226=DIRECTION('center_axis',(0.147323595598226,-0.987363722485679,-0.0583835396257596));
#78227=DIRECTION('ref_axis',(0.246739261558621,-0.0204740031818272,0.968865600586179));
#78228=DIRECTION('center_axis',(0.156803524253748,0.987363722273868,-0.022924544032473));
#78229=DIRECTION('ref_axis',(0.311298434824083,-0.0273822732473687,0.94991762568545));
#78230=DIRECTION('',(-0.418307357430237,0.,0.908305540399117));
#78231=DIRECTION('center_axis',(0.161203576074765,0.986495111042672,-0.0289966023805347));
#78232=DIRECTION('ref_axis',(0.341992730746353,-0.0282764781824217,0.939277069292257));
#78233=DIRECTION('center_axis',(-0.14317932188315,0.987363722364015,0.0679158416318081));
#78234=DIRECTION('ref_axis',(0.445128886337906,0.0029545558905593,0.895461638009728));
#78235=DIRECTION('center_axis',(-0.150208740836956,0.986495109342673,0.0653049264540071));
#78236=DIRECTION('ref_axis',(0.347289035836765,-0.00919561888430754,0.937713051088074));
#78237=DIRECTION('',(-0.908305540023097,0.,-0.41830735824672));
#78238=DIRECTION('center_axis',(-1.9858077270038E-14,-1.,-3.9865505118548E-14));
#78239=DIRECTION('ref_axis',(4.90281767980684E-31,3.9865505118548E-14,-1.));
#78240=DIRECTION('center_axis',(0.131328515638144,-0.987363722452359,-0.0886887848902167));
#78241=DIRECTION('ref_axis',(0.449248100299316,-0.0204740050587526,0.893172413084008));
#78242=DIRECTION('center_axis',(0.148209449218898,0.987363722079822,-0.0560966976114605));
#78243=DIRECTION('ref_axis',(0.508224662243416,-0.0273822805924994,0.860789116681385));
#78244=DIRECTION('',(-0.213268722699965,0.,0.976993578237813));
#78245=DIRECTION('center_axis',(0.151201315284718,0.986495110967627,-0.062972678942065));
#78246=DIRECTION('ref_axis',(0.535913937257938,-0.0282764816587319,0.843798964468254));
#78247=DIRECTION('center_axis',(-0.125231968802575,0.987363722355346,0.0971073311672561));
#78248=DIRECTION('ref_axis',(0.627219803047757,0.00295455300416013,0.778836689737508));
#78249=DIRECTION('center_axis',(-0.132658313610852,0.986495109357093,0.0960685746977785));
#78250=DIRECTION('ref_axis',(0.540750198857879,-0.00919562137031807,0.841132963914016));
#78251=DIRECTION('',(-0.976993578046234,0.,-0.213268723577597));
#78252=DIRECTION('center_axis',(9.32123720376161E-15,-1.,1.15548573698919E-14));
#78253=DIRECTION('ref_axis',(-9.28936163875297E-32,-1.15548573698919E-14,
-1.));
#78254=DIRECTION('center_axis',(0.109192661680426,-0.987363722508771,-0.114847037875455));
#78255=DIRECTION('ref_axis',(0.630750596642655,-0.0204740033599842,0.775715476203324));
#78256=DIRECTION('center_axis',(0.132685264177728,0.987363722067609,-0.086645836685236));
#78257=DIRECTION('ref_axis',(0.681386866923425,-0.0273822827640736,0.731411066483757));
#78258=DIRECTION('',(0.00174211966764608,0.,0.99999848250838));
#78259=DIRECTION('center_axis',(0.134129050998668,0.986495110882551,-0.0940042226871755));
#78260=DIRECTION('ref_axis',(0.704776399762923,-0.0282764856453087,0.708865760702803));
#78261=DIRECTION('center_axis',(-0.101428913882394,0.987363722346396,0.121758183391945));
#78262=DIRECTION('ref_axis',(0.77998261856607,0.00295455906396604,0.6257942036449));
#78263=DIRECTION('center_axis',(-0.108904931346361,0.986495109325205,0.122340161868036));
#78264=DIRECTION('ref_axis',(0.708926482606278,-0.00919562280969778,0.705222434966893));
#78265=DIRECTION('',(-0.999998482504938,0.,0.00174212164352577));
#78266=DIRECTION('center_axis',(-3.47617938933741E-14,-1.,-2.78427622754031E-14));
#78267=DIRECTION('ref_axis',(1.,-3.47617938933741E-14,-2.64513424347123E-31));
#78268=DIRECTION('center_axis',(0.0819510840896689,-0.98736372258218,-0.135635169278427));
#78269=DIRECTION('ref_axis',(0.782759894667927,-0.020473998065395,0.621986947373233));
#78270=DIRECTION('center_axis',(0.110956859400106,0.987363722163423,-0.113143517302827));
#78271=DIRECTION('ref_axis',(0.822688179932599,-0.0273822785974938,0.567833047134452));
#78272=DIRECTION('',(0.216671507230176,0.,0.976244568719644));
#78273=DIRECTION('center_axis',(0.110785051961001,0.986495111067726,-0.120640242462761));
#78274=DIRECTION('ref_axis',(0.840684304897729,-0.0282764769411339,0.540786779008529));
#78275=DIRECTION('center_axis',(-0.072883154065608,0.987363722339465,0.140715761950835));
#78276=DIRECTION('ref_axis',(0.896274313951706,0.00295456149316253,0.443490275786045));
#78277=DIRECTION('center_axis',(-0.0800592741231056,0.986495109329499,0.142891258990401));
#78278=DIRECTION('ref_axis',(0.843954154358251,-0.00919562458937126,0.536336485641114));
#78279=DIRECTION('',(-0.976244569049372,0.,0.21667150574454));
#78280=DIRECTION('center_axis',(-1.19803360132752E-13,-1.,-5.9157167556196E-14));
#78281=DIRECTION('ref_axis',(1.,-1.19803360132752E-13,4.85558563358209E-31));
#78282=DIRECTION('center_axis',(0.0508775535853363,-0.987363722440403,-0.150081158543641));
#78283=DIRECTION('ref_axis',(0.898168212197172,-0.0204740061785341,0.439174996635211));
#78284=DIRECTION('center_axis',(0.0840402415547244,0.987363722072807,-0.134350728073787));
#78285=DIRECTION('ref_axis',(0.925521507090383,-0.0273822824049576,0.377703786747554));
#78286=DIRECTION('',(0.421469570788822,0.,0.906842544711642));
#78287=DIRECTION('center_axis',(0.0822608827577467,0.986495110858974,-0.14163524779961));
#78288=DIRECTION('ref_axis',(0.937282744975115,-0.0282764878537391,0.347421208630923));
#78289=DIRECTION('center_axis',(-0.0409294558523139,0.98736372233825,0.153093629697608));
#78290=DIRECTION('ref_axis',(0.970657218166449,0.00295456000537552,0.240449236631237));
#78291=DIRECTION('center_axis',(-0.0474701448626713,0.986495109347408,0.156760915346788));
#78292=DIRECTION('ref_axis',(0.939519464582124,-0.00919561566235212,0.342372043724235));
#78293=DIRECTION('',(-0.906842545090482,0.,0.421469569973702));
#78294=DIRECTION('center_axis',(-4.32398221734478E-14,-1.,-1.06733082637491E-14));
#78295=DIRECTION('ref_axis',(1.,-4.32398221734478E-14,1.34659732169751E-31));
#78296=DIRECTION('center_axis',(0.0174250529774224,-0.987363722464747,-0.157509514281813));
#78297=DIRECTION('ref_axis',(0.971579180580289,-0.0204740052995073,0.235827714592517));
#78298=DIRECTION('center_axis',(0.0531939918666645,0.987363722074045,-0.149275850563239));
#78299=DIRECTION('ref_axis',(0.985078477924935,-0.0273822820278065,0.169913516119356));
#78300=DIRECTION('',(0.606560188090453,0.,0.795037570322104));
#78301=DIRECTION('center_axis',(0.0498902720504715,0.986495110970026,-0.156007553621502));
#78302=DIRECTION('ref_axis',(0.99005488546476,-0.0282764821508358,0.13781061034817));
#78303=DIRECTION('center_axis',(-0.0126613523898977,0.986495109360025,0.163300610422653));
#78304=DIRECTION('ref_axis',(0.99115389070861,-0.00919561936268709,0.132398661313931));
#78305=DIRECTION('',(-0.795037570867346,0.,0.606560187375787));
#78306=DIRECTION('',(0.763288723126606,0.,0.646057524642935));
#78307=DIRECTION('center_axis',(0.0151868509194036,0.986495111011435,-0.163085117376443));
#78308=DIRECTION('ref_axis',(0.996533160031484,-0.0282764803465164,-0.0782438599308505));
#78309=DIRECTION('center_axis',(0.0271357814650671,0.987363722366795,0.156129846980859));
#78310=DIRECTION('ref_axis',(0.981906645777785,0.00295455723886698,-0.189342571993048));
#78311=DIRECTION('center_axis',(0.0227394687727759,0.986495109360623,0.162204549157858));
#78312=DIRECTION('ref_axis',(0.996443062115878,-0.00919562124639705,-0.0837655329537448));
#78313=DIRECTION('',(-0.646057525329045,0.,0.763288722545873));
#78314=DIRECTION('center_axis',(-7.28750092129755E-14,-1.,1.4115163077016E-14));
#78315=DIRECTION('ref_axis',(1.,-7.28750092129755E-14,2.34639488711829E-31));
#78316=DIRECTION('center_axis',(-0.0503219761482737,-0.987363722498344,
-0.150268353989605));
#78317=DIRECTION('ref_axis',(0.980802869726446,-0.0204740025985538,-0.193924072652061));
#78318=DIRECTION('center_axis',(-0.014401744385676,0.987363722089047,-0.157814669980683));
#78319=DIRECTION('ref_axis',(0.96537784684984,-0.0273822807921186,-0.25941438570401));
#78320=DIRECTION('',(0.884326726957381,0.,0.466868546797539));
#78321=DIRECTION('center_axis',(-0.0202266860130407,0.986495110995933,-0.162537002414993));
#78322=DIRECTION('ref_axis',(0.956414651573567,-0.0282764829956247,-0.290639733630504));
#78323=DIRECTION('center_axis',(0.0600646626950177,0.987363722325613,0.146646227809116));
#78324=DIRECTION('ref_axis',(0.918247158172296,0.00295455860910801,-0.395996751365372));
#78325=DIRECTION('center_axis',(0.0570770171919397,0.986495109334282,0.153523983038531));
#78326=DIRECTION('ref_axis',(0.955139663050738,-0.00919562223710471,-0.296012946674627));
#78327=DIRECTION('',(-0.466868545344239,0.,0.884326727724632));
#78328=DIRECTION('center_axis',(-2.72547556736019E-14,-1.,1.17804524909488E-14));
#78329=DIRECTION('ref_axis',(1.,-2.7254755673602E-14,2.30862714510734E-31));
#78330=DIRECTION('center_axis',(-0.0814487304934385,-0.987363722500416,
-0.135937426013325));
#78331=DIRECTION('ref_axis',(0.916184300434874,-0.0204740025869863,-0.400233860205166));
#78332=DIRECTION('center_axis',(-0.04799053510301,0.987363722266212,-0.151029098166998));
#78333=DIRECTION('ref_axis',(0.887041423826419,-0.027382273844073,-0.46087712407444));
#78334=DIRECTION('',(0.9640145970433,0.,0.26584931199355));
#78335=DIRECTION('center_axis',(-0.0546944500572356,0.986495111027636,-0.154388837198514));
#78336=DIRECTION('ref_axis',(0.871575256307171,-0.028276481282656,-0.489445618224703));
#78337=DIRECTION('center_axis',(0.0901849869939468,0.98736372233563,0.130305594417243));
#78338=DIRECTION('ref_axis',(0.811651454559872,0.00295456013056681,-0.584134562310158));
#78339=DIRECTION('center_axis',(0.0887457096272254,0.986495109349921,0.137664803967637));
#78340=DIRECTION('ref_axis',(0.869174995589528,-0.00919562629084827,-0.494419121291909));
#78341=DIRECTION('',(-0.265849312860113,0.,0.964014596804325));
#78342=DIRECTION('center_axis',(-2.40851055933823E-14,-1.,1.7363998897165E-14));
#78343=DIRECTION('ref_axis',(1.,-2.40851055933823E-14,-4.78390718535403E-31));
#78344=DIRECTION('center_axis',(-0.108767033401082,-0.987363722485907,-0.115250214593728));
#78345=DIRECTION('ref_axis',(0.808725971271374,-0.0204740033547571,-0.587829157645146));
#78346=DIRECTION('center_axis',(-0.0793353310092768,0.987363722158247,-0.137181578280253));
#78347=DIRECTION('ref_axis',(0.767227931430855,-0.0273822783229919,-0.640789756524068));
#78348=DIRECTION('',(0.998626215091659,0.,0.0523992607935185));
#78349=DIRECTION('center_axis',(-0.086604758281656,0.986495110914412,-0.139021624163072));
#78350=DIRECTION('ref_axis',(0.745981973061737,-0.0282764839575028,-0.665365565927422));
#78351=DIRECTION('center_axis',(0.116088364954327,0.987363722346356,0.10787201359286));
#78352=DIRECTION('ref_axis',(0.667103830154567,0.00295455740629755,-0.744958891740772));
#78353=DIRECTION('center_axis',(0.116264741557208,0.986495109322745,0.115368579574079));
#78354=DIRECTION('ref_axis',(0.742568672016664,-0.00919561744090605,-0.669706807460764));
#78355=DIRECTION('',(-0.0523992616912084,0.,0.998626215044556));
#78356=DIRECTION('center_axis',(-9.89463135438162E-15,-1.,1.10678119935376E-14));
#78357=DIRECTION('ref_axis',(-2.31592387427123E-31,-1.10678119935376E-14,
-1.));
#78358=DIRECTION('center_axis',(-0.130999510963508,-0.987363722459965,-0.0891740303974366));
#78359=DIRECTION('ref_axis',(0.663452515084082,-0.0204740050005565,-0.747938216263779));
#78360=DIRECTION('center_axis',(-0.106970499870904,0.987363722142363,-0.116919597820675));
#78361=DIRECTION('ref_axis',(0.611539710180093,-0.0273822782045853,-0.790739776230571));
#78362=DIRECTION('',(0.9865431813915,0.,-0.163500921251039));
#78363=DIRECTION('center_axis',(-0.114465528537602,0.986495111025307,-0.117153910305101));
#78364=DIRECTION('ref_axis',(0.58550739818458,-0.028276481381445,-0.810173763628401));
#78365=DIRECTION('center_axis',(0.136563576370328,0.98736372234371,0.0803944613049864));
#78366=DIRECTION('ref_axis',(0.49136317195317,0.00295456025843987,-0.870949771124488));
#78367=DIRECTION('center_axis',(0.138347373964644,0.986495109335736,0.0876778385554841));
#78368=DIRECTION('ref_axis',(0.581240659621152,-0.00919562299664161,-0.813679750344613));
#78369=DIRECTION('',(0.163500920364212,0.,0.986543181538475));
#78370=DIRECTION('center_axis',(2.18521438712326E-14,-1.,-3.88083178875241E-14));
#78371=DIRECTION('ref_axis',(-1.82162563614679E-31,3.88083178875241E-14,
-1.));
#78372=DIRECTION('center_axis',(-0.147106595225137,-0.987363722492263,-0.058928169388586));
#78373=DIRECTION('ref_axis',(0.487156755321014,-0.0204740038282639,-0.873074516242652));
#78374=DIRECTION('center_axis',(-0.129603845053748,0.987363722128369,-0.0911905892737636));
#78375=DIRECTION('ref_axis',(0.427256576207141,-0.027382280323163,-0.903715679189011));
#78376=DIRECTION('',(0.928330484082491,0.,-0.371755984919097));
#78377=DIRECTION('center_axis',(-0.136974018842237,0.986495111137968,-0.0898082059897402));
#78378=DIRECTION('ref_axis',(0.397655150255994,-0.0282764745849969,-0.917099134477799));
#78379=DIRECTION('center_axis',(0.150653229591986,0.987363722340574,0.0491577483136696));
#78380=DIRECTION('ref_axis',(0.292646918554997,0.0029545569875937,-0.956216006796201));
#78381=DIRECTION('center_axis',(0.153961033449543,0.98649510932601,0.0558873818944154));
#78382=DIRECTION('ref_axis',(0.392734481097539,-0.00919562464313007,-0.919605930735807));
#78383=DIRECTION('',(0.371755983092481,0.,0.928330484813971));
#78384=DIRECTION('center_axis',(4.33287056654286E-15,-1.,-1.41995219769621E-14));
#78385=DIRECTION('ref_axis',(1.09233946293455E-31,1.41995219769621E-14,
-1.));
#78386=DIRECTION('center_axis',(-0.156335138791017,-0.987363722512377,-0.0259268942547021));
#78387=DIRECTION('ref_axis',(0.288082088867567,-0.0204740016392568,-0.957386821159857));
#78388=DIRECTION('center_axis',(-0.146177060289827,0.987363722117319,-0.0611976085452475));
#78389=DIRECTION('ref_axis',(0.222995395855195,-0.0273822807870121,-0.974434843448389));
#78390=DIRECTION('',(0.826710085934478,0.,-0.562628148792973));
#78391=DIRECTION('center_axis',(-0.153077751184681,0.986495111055157,-0.0582631783935128));
#78392=DIRECTION('ref_axis',(0.191208989636266,-0.0282764781182431,-0.981141968864602));
#78393=DIRECTION('center_axis',(0.157698503409577,0.987363722348828,0.0156224777754914));
#78394=DIRECTION('ref_axis',(0.0802468205327068,0.0029545583644425,-0.996770644822199));
#78395=DIRECTION('center_axis',(0.162375644751385,0.986495109354807,0.0214836963909733));
#78396=DIRECTION('ref_axis',(0.185864477196135,-0.00919562331167665,-0.982532359074508));
#78397=DIRECTION('',(0.562628148677447,0.,0.826710086013101));
#78398=DIRECTION('center_axis',(5.89546486710796E-15,-1.,-7.39949208706086E-14));
#78399=DIRECTION('ref_axis',(1.17599418447442E-31,7.39949208706086E-14,
-1.));
#78400=DIRECTION('center_axis',(-0.158253626200997,-0.987363722455385,0.00828669857543342));
#78401=DIRECTION('ref_axis',(0.0755370232536191,-0.0204740045161776,-0.996932782717598));
#78402=DIRECTION('center_axis',(-0.155915199182761,0.98736372221274,-0.0283430894929197));
#78403=DIRECTION('ref_axis',(0.00830720070699266,-0.0273822746524882,-0.999590516887425));
#78404=DIRECTION('',(0.686433642056073,0.,-0.72719244705486));
#78405=DIRECTION('center_axis',(-0.162023739702991,0.986495110930413,-0.0239938301038143));
#78406=DIRECTION('ref_axis',(-0.0241778909692891,-0.0282764821330522,-0.99930769543042));
#78407=DIRECTION('center_axis',(0.157369971048538,0.987363722346775,-0.0186432831256345));
#78408=DIRECTION('ref_axis',(-0.135905529982305,0.00295455904762982,-0.990717395376231));
#78409=DIRECTION('center_axis',(0.163197752475911,0.986495109366373,-0.0139245388806963));
#78410=DIRECTION('ref_axis',(-0.0296963431688327,-0.00919561804706838,-0.99951666710022));
#78411=DIRECTION('',(0.727192446437817,0.,0.686433642709755));
#78412=DIRECTION('center_axis',(-1.21789062324421E-14,-1.,-8.8238773580434E-14));
#78413=DIRECTION('ref_axis',(-1.00747679306799E-32,8.8238773580434E-14,
-1.));
#78414=DIRECTION('center_axis',(-0.15277234939578,-0.98736372254509,0.0421128087640363));
#78415=DIRECTION('ref_axis',(-0.140540068186091,-0.020474001593977,-0.989863275656279));
#78416=DIRECTION('center_axis',(-0.158362915039067,0.987363722199346,0.00583671354287932));
#78417=DIRECTION('ref_axis',(-0.206769430856227,-0.0273822763792333,-0.978006448549131));
#78418=DIRECTION('',(0.514060324983116,0.,-0.85775403367064));
#78419=DIRECTION('center_axis',(-0.163393677467838,0.986495111106532,0.0113974526297502));
#78420=DIRECTION('ref_axis',(-0.238434241820558,-0.0282764764144799,-0.970746904815584));
#78421=DIRECTION('center_axis',(0.149682992843389,0.987363722367546,-0.0520373078276564));
#78422=DIRECTION('ref_axis',(-0.34570308938674,0.00295455657717342,-0.938339301417081));
#78423=DIRECTION('center_axis',(0.156388914161816,0.986495109361921,-0.0486816878538454));
#78424=DIRECTION('ref_axis',(-0.243868596486215,-0.00919562266043916,-0.969764687010066));
#78425=DIRECTION('',(0.85775403194092,0.,0.514060327869303));
#78426=DIRECTION('center_axis',(-2.05752654287162E-14,-1.,-5.57051301330842E-14));
#78427=DIRECTION('ref_axis',(4.21927796480682E-31,5.57051301330842E-14,
-1.));
#78428=DIRECTION('center_axis',(-0.140147605924149,-0.987363722434189,0.0739697787926336));
#78429=DIRECTION('ref_axis',(-0.350045664256259,-0.0204740067575522,-0.936508861667996));
#78430=DIRECTION('center_axis',(-0.153405758249488,0.987363722140234,0.0397435974376149));
#78431=DIRECTION('ref_axis',(-0.412177752017299,-0.0273822789533092,-0.910691886172974));
#78432=DIRECTION('',(0.317650120667855,0.,-0.948207994503156));
#78433=DIRECTION('center_axis',(-0.157123509264922,0.986495111084634,0.0462557957708086));
#78434=DIRECTION('ref_axis',(-0.441541669900457,-0.0282764778254351,-0.896795068308978));
#78435=DIRECTION('center_axis',(0.134997006587638,0.987363722345089,-0.0829981205162371));
#78436=DIRECTION('ref_axis',(-0.539335955073032,0.00295455986961746,-0.84208550524364));
#78437=DIRECTION('center_axis',(0.142267503246296,0.986495109321295,-0.081162533260312));
#78438=DIRECTION('ref_axis',(-0.446637828743161,-0.00919562490853365,-0.894667586547169));
#78439=DIRECTION('',(0.948207994217622,0.,0.317650121520194));
#78440=DIRECTION('center_axis',(0.,-1.,0.));
#78441=DIRECTION('ref_axis',(0.,0.,-1.));
#78442=DIRECTION('center_axis',(-0.120969720836266,-0.987363722540217,0.102367993300253));
#78443=DIRECTION('ref_axis',(-0.543183512539008,-0.020473999900492,-0.839364335097614));
#78444=DIRECTION('center_axis',(-0.141275518361541,0.987363722123742,0.0717921175730828));
#78445=DIRECTION('ref_axis',(-0.598313102465493,-0.0273822793619485,-0.800794381970216));
#78446=DIRECTION('',(0.106386947436074,0.,-0.994324804787266));
#78447=DIRECTION('center_axis',(-0.143506420757269,0.98649511106524,0.0789512700709557));
#78448=DIRECTION('ref_axis',(-0.624003101326521,-0.028276478820293,-0.780910091035075));
#78449=DIRECTION('center_axis',(0.113998708813961,0.987363722364336,-0.11007803662671));
#78450=DIRECTION('ref_axis',(-0.7077500725784,0.00295455974303667,-0.706456725739089));
#78451=DIRECTION('center_axis',(0.121493827765142,0.98649510934329,-0.109848300199615));
#78452=DIRECTION('ref_axis',(-0.628522767255286,-0.00919561739573514,-0.777736826736698));
#78453=DIRECTION('',(0.994324804659096,0.,0.106386948633988));
#78454=DIRECTION('center_axis',(-3.15476866325682E-14,-1.,-3.14379578369509E-14));
#78455=DIRECTION('ref_axis',(1.,-3.15476866325682E-14,7.63333428802623E-31));
#78456=DIRECTION('center_axis',(-0.0961354199646547,-0.987363722474464,
0.125979603784065));
#78457=DIRECTION('ref_axis',(-0.710922705002381,-0.0204740044788156,-0.702972063920537));
#78458=DIRECTION('center_axis',(-0.12253939143678,0.987363722160225,0.100483718622524));
#78459=DIRECTION('ref_axis',(-0.756471994289161,-0.0273822782236257,-0.653452624675625));
#78460=DIRECTION('',(-0.109850764109878,0.,-0.993948092017121));
#78461=DIRECTION('center_axis',(-0.123179134229024,0.986495110939119,0.107955069282568));
#78462=DIRECTION('ref_axis',(-0.777286841805984,-0.02827648289046,-0.6285106252647));
#78463=DIRECTION('center_axis',(0.0876699555529006,0.987363722327402,-0.132010828060165));
#78464=DIRECTION('ref_axis',(-0.843070582388619,0.00295455614116526,-0.537794815621091));
#78465=DIRECTION('center_axis',(0.0950392295741619,0.986495109351144,-0.133397691390157));
#78466=DIRECTION('ref_axis',(-0.78101868357015,-0.00919562018639328,-0.62443995426601));
#78467=DIRECTION('',(0.993948092429756,0.,-0.10985076037629));
#78468=DIRECTION('center_axis',(6.26139182359859E-14,-1.,3.98685596779503E-14));
#78469=DIRECTION('ref_axis',(1.,6.26139182359859E-14,3.82708143198835E-31));
#78470=DIRECTION('center_axis',(-0.0668059353666372,-0.98736372243687,0.143700544937714));
#78471=DIRECTION('ref_axis',(-0.845419941715254,-0.0204740056074118,-0.533709600105305));
#78472=DIRECTION('center_axis',(-0.0980734572566049,0.987363722206714,0.124476813310113));
#78473=DIRECTION('ref_axis',(-0.879259097639604,-0.0273822756801386,-0.475556148311181));
#78474=DIRECTION('',(-0.320951972736834,0.,-0.947095471004024));
#78475=DIRECTION('center_axis',(-0.0970921254666728,0.986495110935384,0.131911012705338));
#78476=DIRECTION('ref_axis',(-0.894225513091188,-0.0282764824828937,-0.446722701768331));
#78477=DIRECTION('center_axis',(0.0572418589335363,0.987363722345491,-0.147770935511318));
#78478=DIRECTION('ref_axis',(-0.938970048578615,0.00295456041420517,-0.343986218394039));
#78479=DIRECTION('center_axis',(0.0641407031162536,0.986495109342319,-0.150709553271978));
#78480=DIRECTION('ref_axis',(-0.896995032092022,-0.0091956222124549,-0.441944965956575));
#78481=DIRECTION('',(0.947095471292532,0.,-0.320951971885478));
#78482=DIRECTION('center_axis',(-1.39441202957605E-14,-1.,-5.09526267024949E-15));
#78483=DIRECTION('ref_axis',(1.,-1.39441202957605E-14,-4.33523906590216E-32));
#78484=DIRECTION('center_axis',(-0.0343526833148809,-0.987363722490136,
0.1547022063821));
#78485=DIRECTION('ref_axis',(-0.940386280729254,-0.0204740025468243,-0.339491470048825));
#78486=DIRECTION('center_axis',(-0.0690217183976504,0.987363722198575,0.142649509202135));
#78487=DIRECTION('ref_axis',(-0.960933023633175,-0.027382275329481,-0.275423192721647));
#78488=DIRECTION('',(-0.517045822704402,0.,-0.855957719296887));
#78489=DIRECTION('center_axis',(-0.0664652025269315,0.986495110851481,0.149698941610083));
#78490=DIRECTION('ref_axis',(-0.969351193563916,-0.0282764885549299,-0.244046519604798));
#78491=DIRECTION('center_axis',(0.0241371926176063,0.98736372236658,-0.156621440700023));
#78492=DIRECTION('ref_axis',(-0.990964319395181,0.002954559969109,-0.134093207363515));
#78493=DIRECTION('center_axis',(0.0302430298729286,0.986495109332971,-0.160974402953495));
#78494=DIRECTION('ref_axis',(-0.971028890904806,-0.00919562225302405,-0.238785120054752));
#78495=DIRECTION('',(0.855957719761673,0.,-0.51704582193496));
#78496=DIRECTION('center_axis',(-8.82806721608986E-14,-1.,-1.1871387483534E-14));
#78497=DIRECTION('ref_axis',(1.,-8.82806721608986E-14,1.9887858054574E-31));
#78498=DIRECTION('center_axis',(-0.000293134981233076,-0.987363722491244,
0.158470166214708));
#78499=DIRECTION('ref_axis',(-0.991381202856231,-0.0204740027916695,-0.129399095178518));
#78500=DIRECTION('center_axis',(-0.0367426028752615,0.987363722166916,0.154152071937562));
#78501=DIRECTION('ref_axis',(-0.997674788534383,-0.0273822772005084,-0.0624117554487041));
#78502=DIRECTION('',(-0.688963187756883,0.,-0.724796334093843));
#78503=DIRECTION('center_axis',(-0.0327304188065948,0.986495111201851,0.160487118671852));
#78504=DIRECTION('ref_axis',(-0.99915108956692,-0.0282764714310698,-0.0299589949872197));
#78505=DIRECTION('center_axis',(-0.0100961008866114,0.987363722319459,-0.158148501713896));
#78506=DIRECTION('ref_axis',(-0.996622199995403,0.00295456092772905,0.0820698546729972));
#78507=DIRECTION('center_axis',(-0.00506877082020845,0.986495109324231,
-0.16371226845214));
#78508=DIRECTION('ref_axis',(-0.999658517458994,-0.00919561933260429,-0.0244599480125288));
#78509=DIRECTION('',(0.724796334642181,0.,-0.688963187180026));
#78510=DIRECTION('center_axis',(8.87687165924134E-14,-1.,-7.38389392493213E-15));
#78511=DIRECTION('ref_axis',(1.,8.87687165924134E-14,6.42305605932119E-32));
#78512=DIRECTION('center_axis',(0.0337801256786956,-0.987363722407571,0.154828236386635));
#78513=DIRECTION('ref_axis',(-0.996020241549457,-0.020474008779607,0.0867438377537795));
#78514=DIRECTION('center_axis',(-0.00274544497597346,0.98736372213281,0.158446655843306));
#78515=DIRECTION('ref_axis',(-0.987766389444261,-0.0273822791546761,0.153517981593504));
#78516=DIRECTION('',(-0.828665397705427,0.,-0.559744279690027));
#78517=DIRECTION('center_axis',(0.00253477441076304,0.986495110962286,0.16377109319472));
#78518=DIRECTION('ref_axis',(-0.982231790619155,-0.0282764837612161,0.185529377628423));
#78519=DIRECTION('center_axis',(-0.0438573179899566,0.987363722349411,-0.152280712656075));
#78520=DIRECTION('ref_axis',(-0.95567913422659,0.00295455517364751,0.294395419474627));
#78521=DIRECTION('center_axis',(-0.0401435654911374,0.986495109322325,-0.158795130381233));
#78522=DIRECTION('ref_axis',(-0.981545222756637,-0.00919562080500803,0.191008942831572));
#78523=DIRECTION('',(0.559744278460836,0.,-0.828665398535717));
#78524=DIRECTION('center_axis',(2.83686781064125E-14,-1.,-8.76463754737558E-15));
#78525=DIRECTION('ref_axis',(1.,2.83686781064125E-14,-2.01260476590519E-31));
#78526=DIRECTION('center_axis',(0.0662738583278151,-0.987363722418306,0.143946710120834));
#78527=DIRECTION('ref_axis',(-0.954086480895184,-0.0204740078213297,0.298830724619768));
#78528=DIRECTION('center_axis',(0.0313800915092737,0.987363722164569,0.155332449958781));
#78529=DIRECTION('ref_axis',(-0.931671131181227,-0.0273822773082007,0.362269394529693));
#78530=DIRECTION('',(-0.929620135502299,0.,-0.36851920393473));
#78531=DIRECTION('center_axis',(0.0376814580230275,0.986495110934236,0.159397314356638));
#78532=DIRECTION('ref_axis',(-0.919384425301451,-0.0282764825435261,0.392342604171514));
#78533=DIRECTION('center_axis',(-0.0755678077734676,0.987363722339704,-0.139292448595736));
#78534=DIRECTION('ref_axis',(-0.87004957346559,0.00295455813711103,0.492955383679455));
#78535=DIRECTION('center_axis',(-0.0733412931473506,0.986495109333737,-0.146452907038722));
#78536=DIRECTION('ref_axis',(-0.917535964181013,-0.00919562396521216,0.397546468899309));
#78537=DIRECTION('',(0.3685192037855,0.,-0.929620135561457));
#78538=DIRECTION('center_axis',(2.58212961952919E-14,-1.,-1.46581524198925E-14));
#78539=DIRECTION('ref_axis',(1.,2.58212961952919E-14,-3.82337337017993E-31));
#78540=DIRECTION('center_axis',(0.0956686992681182,-0.987363722428569,0.126334395998662));
#78541=DIRECTION('ref_axis',(-0.86754069645364,-0.0204740068519684,0.496944619691328));
#78542=DIRECTION('center_axis',(0.0640383226550879,0.987363722055881,0.144955074417834));
#78543=DIRECTION('ref_axis',(-0.832011966724281,-0.0273822830093003,0.55408149022034));
#78544=DIRECTION('',(-0.987106868581237,0.,-0.160062581510308));
#78545=DIRECTION('center_axis',(0.071066195202264,0.986495110975005,0.147570294849225));
#78546=DIRECTION('ref_axis',(-0.813547665355053,-0.0282764848871257,0.580810327557776));
#78547=DIRECTION('center_axis',(-0.103744832799726,0.987363722346279,-0.119791024128924));
#78548=DIRECTION('ref_axis',(-0.743737463193152,0.00295455866069842,0.668465299343305));
#78549=DIRECTION('center_axis',(-0.103109658554765,0.98649510935733,-0.127262710668878));
#78550=DIRECTION('ref_axis',(-0.810623745170262,-0.00919562209827842,0.585495161637023));
#78551=DIRECTION('',(0.160062579596475,0.,-0.987106868891572));
#78552=DIRECTION('center_axis',(0.0937021734286871,0.98736372160279,0.127799780740929));
#78553=DIRECTION('ref_axis',(-0.693448832647947,-0.0273823195503969,0.719985364486834));
#78554=DIRECTION('',(-0.998437581939004,0.,0.0558783944990723));
#78555=DIRECTION('center_axis',(0.101127960417461,0.986495110941819,0.128843050684517));
#78556=DIRECTION('ref_axis',(-0.669670322268832,-0.028276482174131,0.742120003791984));
#78557=DIRECTION('center_axis',(-2.20665391377616E-14,-1.,1.98662683520469E-14));
#78558=DIRECTION('ref_axis',(1.,-2.20665391377616E-14,-4.42483838814686E-31));
#78559=DIRECTION('center_axis',(0.120590140483329,-0.987363723519774,0.102814860284774));
#78560=DIRECTION('ref_axis',(-0.740429679278794,-0.0204739556178617,0.671821931157699));
#78561=DIRECTION('center_axis',(-0.127070866310374,0.987363722339884,-0.0946883030910327));
#78562=DIRECTION('ref_axis',(-0.582649014492189,0.00295455734858739,0.812718522307788));
#78563=DIRECTION('center_axis',(-0.128056733023664,0.986495109359135,-0.102121850442573));
#78564=DIRECTION('ref_axis',(-0.665807659368209,-0.00919562209053125,0.746066753890692));
#78565=DIRECTION('',(-0.0558783934411736,0.,-0.99843758199821));
#78566=DIRECTION('center_axis',(3.45599505596096E-14,-1.,-4.82909193868955E-14));
#78567=DIRECTION('ref_axis',(-2.68967614992597E-31,4.82909193868955E-14,
-1.));
#78568=DIRECTION('center_axis',(0.118984666368161,0.987363722173452,0.10466866438932));
#78569=DIRECTION('ref_axis',(-0.5224608308728,-0.0273822777464371,0.852223498308467));
#78570=DIRECTION('center_axis',(0.139872995331646,-0.987363722448005,0.0744877491307953));
#78571=DIRECTION('ref_axis',(-0.57869698151077,-0.0204740057536221,0.815285605587836));
#78572=DIRECTION('center_axis',(0.12646109336356,0.986495110980928,0.104091247835831));
#78573=DIRECTION('ref_axis',(-0.494479938320355,-0.0282764800739962,0.868728974579139));
#78574=DIRECTION('',(-0.963082463535534,0.,0.269206553468387));
#78575=DIRECTION('center_axis',(-0.144455208030673,0.987363722350675,-0.0651580590459365));
#78576=DIRECTION('ref_axis',(-0.394316546242898,0.00295455278274242,0.918969929854577));
#78577=DIRECTION('center_axis',(-0.147016018399682,0.986495109320743,-0.0722058835563958));
#78578=DIRECTION('ref_axis',(-0.489859148114179,-0.00919562510734571,0.871753093190805));
#78579=DIRECTION('',(-0.269206552602653,0.,-0.963082463777529));
#78580=DIRECTION('center_axis',(-1.75281284135584E-14,-1.,4.09434541677049E-14));
#78581=DIRECTION('ref_axis',(-6.97643112798884E-32,-4.09434541677049E-14,
-1.));
#78582=DIRECTION('center_axis',(0.152615505806413,-0.987363722502889,0.0426777093186988));
#78583=DIRECTION('ref_axis',(-0.389905061888299,-0.0204740037428501,0.920627426207051));
#78584=DIRECTION('center_axis',(0.138703539562874,0.987363722143939,0.0766433839727627));
#78585=DIRECTION('ref_axis',(-0.327043125582336,-0.0273822788356535,0.94461262156246));
#78586=DIRECTION('',(-0.882694679781319,0.,0.469946914327305));
#78587=DIRECTION('center_axis',(0.145881043013491,0.986495110952259,0.0744722589733021));
#78588=DIRECTION('ref_axis',(-0.296168221911397,-0.0282764840435662,0.954717143859885));
#78589=DIRECTION('center_axis',(-0.155084980925954,0.9873637223546,-0.0325811060166102));
#78590=DIRECTION('ref_axis',(-0.187546275077728,0.00295455868251791,0.982251324910005));
#78591=DIRECTION('center_axis',(-0.159100996390971,0.986495109339711,-0.0389136505127861));
#78592=DIRECTION('ref_axis',(-0.291005366268943,-0.00919562638014897,0.956677227312407));
#78593=DIRECTION('',(-0.469946915773758,0.,-0.882694679011227));
#78594=DIRECTION('center_axis',(-1.94056290405287E-14,-1.,1.02093246551329E-13));
#78595=DIRECTION('ref_axis',(4.6849201298372E-31,-1.02093246551329E-13,
-1.));
#78596=DIRECTION('center_axis',(0.158221886231727,-0.987363722470914,0.00887210604393224));
#78597=DIRECTION('ref_axis',(-0.182881616600238,-0.0204740036971804,0.982921731106954));
#78598=DIRECTION('center_axis',(0.151936789673059,0.987363722123935,0.0450343444208377));
#78599=DIRECTION('ref_axis',(-0.116333249189989,-0.0273822798023598,0.992832707904874));
#78600=DIRECTION('',(-0.761033074141649,0.,0.648713079922481));
#78601=DIRECTION('center_axis',(0.158479759458568,0.986495110935801,0.0413710278058995));
#78602=DIRECTION('ref_axis',(-0.0840080098883409,-0.0282764847776318,0.996063800508391));
#78603=DIRECTION('center_axis',(2.56722337042868E-15,-1.,8.90382855340933E-14));
#78604=DIRECTION('ref_axis',(0.0288208255552056,8.90752879685742E-14,0.999584593725972));
#78605=DIRECTION('center_axis',(0.156429986789619,-0.987363722430428,-0.0253483502683913));
#78606=DIRECTION('ref_axis',(0.0326931712220302,-0.0204740066028789,0.999255708819856));
#78607=DIRECTION('center_axis',(-0.158463154907314,0.987363722361481,0.00151930948189432));
#78608=DIRECTION('ref_axis',(0.0279934535704983,0.00295455814615585,0.999603740060709));
#78609=DIRECTION('center_axis',(-0.163746588080473,0.986495109318213,-0.0038018657591047));
#78610=DIRECTION('ref_axis',(-0.0785444998839504,-0.0091956206558518,0.996868196954208));
#78611=DIRECTION('',(-0.648713080657652,0.,-0.761033073514981));
#78612=DIRECTION('center_axis',(-0.154562212825867,-0.987363722400022,-0.0349771647613762));
#78613=DIRECTION('ref_axis',(-0.156465939823782,-0.0104932879265436,0.987627612303115));
#78614=DIRECTION('',(0.562296676496711,-6.23377071775851E-15,0.826935576451245));
#78615=DIRECTION('',(0.826935573288472,0.,-0.562296681148009));
#78616=DIRECTION('center_axis',(0.152615509258216,-0.987363722350212,0.0426777005072813));
#78617=DIRECTION('ref_axis',(-0.32231653707131,-0.00890473778974789,0.94659006733393));
#78618=DIRECTION('center_axis',(-0.14342957841421,-0.987363722441753,-0.0673857228341938));
#78619=DIRECTION('ref_axis',(-0.36511859464289,-0.0104932857748454,0.930901876031866));
#78620=DIRECTION('',(0.371383789246354,0.,0.928479445698729));
#78621=DIRECTION('center_axis',(8.67712559411096E-15,-1.,-2.83955679719989E-14));
#78622=DIRECTION('ref_axis',(-3.40757823733139E-32,2.83955679719989E-14,
-1.));
#78623=DIRECTION('center_axis',(0.151936786270519,0.987363722024958,0.0450343580703467));
#78624=DIRECTION('ref_axis',(-0.220871911237121,-0.0104936262509378,0.975246370223733));
#78625=DIRECTION('center_axis',(-0.144455200951618,0.987363721612747,-0.0651580859222701));
#78626=DIRECTION('ref_axis',(-0.295080326269699,0.0198684700496971,0.955265850403149));
#78627=DIRECTION('',(0.928479445093011,0.,-0.371383790760683));
#78628=DIRECTION('center_axis',(0.139872999273741,-0.987363722338544,0.0744877431792839));
#78629=DIRECTION('ref_axis',(-0.518269837796488,-0.00890473716144612,0.855170790477836));
#78630=DIRECTION('center_axis',(-0.125590335269879,-0.987363722391106,-0.096643403255366));
#78631=DIRECTION('ref_axis',(-0.556698710963746,-0.0104932875265685,0.830648202386659));
#78632=DIRECTION('',(0.163105405539061,0.,0.986608649203897));
#78633=DIRECTION('center_axis',(-5.10246344398526E-14,-1.,9.0532294620924E-14));
#78634=DIRECTION('ref_axis',(1.03431144013726E-30,-9.0532294620924E-14,
-1.));
#78635=DIRECTION('center_axis',(0.138703533836429,0.987363721999689,0.0766433961943712));
#78636=DIRECTION('ref_axis',(-0.425357189232499,-0.0104936246872304,0.904964720532879));
#78637=DIRECTION('center_axis',(-0.127070856969211,0.987363721618719,-0.0946883231467527));
#78638=DIRECTION('ref_axis',(-0.493535432378174,0.0198684687691836,0.869498718191152));
#78639=DIRECTION('',(0.98660864901436,0.,-0.163105406685554));
#78640=DIRECTION('center_axis',(0.120590183957813,-0.987363722329175,0.102814820727838));
#78641=DIRECTION('ref_axis',(-0.689989418966707,-0.00890473821475343,0.723764676777827));
#78642=DIRECTION('center_axis',(-0.101878628092225,-0.987363722385251,-0.121382143891048));
#78643=DIRECTION('ref_axis',(-0.722248213566424,-0.0104932876907897,0.691554342704569));
#78644=DIRECTION('',(-0.0527996037021425,0.,0.998605128090627));
#78645=DIRECTION('center_axis',(2.9697203196646E-14,-1.,-3.31915336355735E-14));
#78646=DIRECTION('ref_axis',(-1.45851444347016E-32,3.31915336355735E-14,
-1.));
#78647=DIRECTION('center_axis',(0.118984659539348,0.987363722014647,0.104668673650181));
#78648=DIRECTION('ref_axis',(-0.609953239450716,-0.0104936216088402,0.792367925643831));
#78649=DIRECTION('center_axis',(-0.103744818751068,0.987363721575649,-0.119791042647572));
#78650=DIRECTION('ref_axis',(-0.668913370904801,0.0198684711732498,0.743074791712123));
#78651=DIRECTION('',(0.99860512817674,0.,0.052799602073472));
#78652=DIRECTION('center_axis',(0.0956687012151709,-0.987363722323065,0.126334395348786));
#78653=DIRECTION('ref_axis',(-0.829445861762146,-0.00890473335574096,0.558516130590258));
#78654=DIRECTION('center_axis',(-0.0734031899540221,-0.987363722401994,
-0.140445189981899));
#78655=DIRECTION('ref_axis',(-0.854026193536076,-0.0104932869748259,0.520124169485272));
#78656=DIRECTION('',(-0.266235760272642,0.,0.963907941637607));
#78657=DIRECTION('center_axis',(2.4092065114801E-14,-1.,-1.73543421154282E-14));
#78658=DIRECTION('ref_axis',(1.,2.4092065114801E-14,-3.57346751578377E-31));
#78659=DIRECTION('center_axis',(0.0937021908558792,0.987363722013814,0.127799764787879));
#78660=DIRECTION('ref_axis',(-0.766028551888797,-0.0104936252703983,0.642720889282305));
#78661=DIRECTION('center_axis',(-0.0755677888343809,0.987363721559842,-0.139292464398404));
#78662=DIRECTION('ref_axis',(-0.81301366345872,0.0198684717500299,0.581905513687359));
#78663=DIRECTION('',(0.963907941868057,0.,0.266235759438296));
#78664=DIRECTION('center_axis',(0.0662738630982961,-0.987363722324091,0.14394670857072));
#78665=DIRECTION('ref_axis',(-0.930118336104504,-0.00890473695803777,0.367151993732701));
#78666=DIRECTION('center_axis',(-0.04149549491575,-0.987363722304536,-0.152941177511578));
#78667=DIRECTION('ref_axis',(-0.945870857771692,-0.0104932921380493,0.324373567416256));
#78668=DIRECTION('',(-0.467223032247448,6.23377071131938E-15,0.88413949020361));
#78669=DIRECTION('center_axis',(-5.45189531984744E-14,-1.,2.35390508043942E-14));
#78670=DIRECTION('ref_axis',(1.,-5.45189531984744E-14,-2.16278283367938E-31));
#78671=DIRECTION('center_axis',(0.0640383165993706,0.987363721994225,0.144955077513102));
#78672=DIRECTION('ref_axis',(-0.886285223091077,-0.0104936222903732,0.463020936051089));
#78673=DIRECTION('center_axis',(-0.0438572993335235,0.987363721632358,-0.152280722678445));
#78674=DIRECTION('ref_axis',(-0.919098339570757,0.0198684658176202,0.393526982892318));
#78675=DIRECTION('',(0.884139492153187,0.,0.467223028558209));
#78676=DIRECTION('center_axis',(0.0337801291775882,-0.98736372232979,0.154828236119277));
#78677=DIRECTION('ref_axis',(-0.987299512398125,-0.00890473682484817,0.158620233515478));
#78678=DIRECTION('center_axis',(-0.00764752125946903,-0.987363722329066,
-0.158285802417894));
#78679=DIRECTION('ref_axis',(-0.993487651528559,-0.0104932916296771,0.113455617274087));
#78680=DIRECTION('',(-0.646363471935384,-6.23377071920573E-15,0.763029660070718));
#78681=DIRECTION('center_axis',(1.16609060841453E-13,-1.,-2.25375149943799E-14));
#78682=DIRECTION('ref_axis',(1.,1.16609060841453E-13,-4.9990146629533E-31));
#78683=DIRECTION('center_axis',(0.0313800754377996,0.987363722013489,0.155332454165855));
#78684=DIRECTION('ref_axis',(-0.965100182175857,-0.0104936260553598,0.261670636824878));
#78685=DIRECTION('center_axis',(-0.0100960862249963,0.987363721665325,-0.158148506733817));
#78686=DIRECTION('ref_axis',(-0.98220699998696,0.0198684655322117,0.186747565590591));
#78687=DIRECTION('',(0.76302966112491,0.,0.646363470690915));
#78688=DIRECTION('center_axis',(-0.000293120077939613,-0.987363722326222,
0.158470167270458));
#78689=DIRECTION('ref_axis',(-0.998315660024052,-0.00890474181677815,-0.0573284268397199));
#78690=DIRECTION('center_axis',(0.0265580433165256,-0.987363722271751,-0.156229159496141));
#78691=DIRECTION('ref_axis',(-0.994650066459442,-0.0104932930201555,-0.102767388279653));
#78692=DIRECTION('',(-0.795280674871628,-6.23377070532254E-15,0.606241410805735));
#78693=DIRECTION('center_axis',(1.48409631970856E-14,-1.,3.82112591215294E-16));
#78694=DIRECTION('ref_axis',(-0.999668706672101,-1.48458815383128E-14,-0.0257386266247645));
#78695=DIRECTION('center_axis',(-0.00274545648219705,0.987363722011251,
0.158446656401429));
#78696=DIRECTION('ref_axis',(-0.998788128182702,-0.0104936233898283,0.0480849131167593));
#78697=DIRECTION('center_axis',(0.0241372137388688,0.987363721561804,-0.156621442518411));
#78698=DIRECTION('ref_axis',(-0.999388752406702,0.0198684703996675,-0.0287639609051392));
#78699=DIRECTION('',(0.606241413488844,0.,0.795280672826298));
#78700=DIRECTION('center_axis',(-0.0343526754374226,-0.987363722316263,
0.15470220924106));
#78701=DIRECTION('ref_axis',(-0.96265167765723,-0.00890473481808807,-0.270596476698311));
#78702=DIRECTION('center_axis',(0.0595217799933164,-0.98736372233658,-0.14686741476611));
#78703=DIRECTION('ref_axis',(-0.949303750074943,-0.0104932907929634,-0.314185106174663));
#78704=DIRECTION('',(-0.907011438172325,6.23377072148099E-15,0.421105985500765));
#78705=DIRECTION('center_axis',(5.76473871287922E-14,-1.,1.42541895811654E-14));
#78706=DIRECTION('ref_axis',(1.,5.76473871287922E-14,4.64171933072534E-32));
#78707=DIRECTION('center_axis',(-0.0367426193503058,0.98736372202171,0.154152068940748));
#78708=DIRECTION('ref_axis',(-0.985773851402552,-0.0104936258606393,-0.167749210750086));
#78709=DIRECTION('center_axis',(0.0572418783879038,0.987363721619137,-0.147770932828589));
#78710=DIRECTION('ref_axis',(-0.969840197166203,0.0198684690771466,-0.24293051660331));
#78711=DIRECTION('',(0.421105986980064,0.,0.907011437485518));
#78712=DIRECTION('center_axis',(-0.0668059282074712,-0.987363722329631,
0.143700549002825));
#78713=DIRECTION('ref_axis',(-0.881975171793276,-0.00890473817601859,-0.471211737946157));
#78714=DIRECTION('center_axis',(0.0897023443099469,-0.987363722380802,-0.130638314255909));
#78715=DIRECTION('ref_axis',(-0.859569045297417,-0.0104932880608984,-0.510911878186598));
#78716=DIRECTION('',(-0.9763313539579,0.,0.216280112998708));
#78717=DIRECTION('center_axis',(3.99265454288478E-14,-1.,1.97350640766554E-14));
#78718=DIRECTION('ref_axis',(1.,3.99265454288478E-14,-5.50716463294474E-31));
#78719=DIRECTION('center_axis',(-0.0690217288582187,0.987363722016548,0.142649505400653));
#78720=DIRECTION('ref_axis',(-0.926665886657474,-0.0104936191794018,-0.375739562013153));
#78721=DIRECTION('center_axis',(0.0876699778602928,0.987363721604882,-0.132010818649586));
#78722=DIRECTION('ref_axis',(-0.894942993070415,0.0198684697000682,-0.445737908491016));
#78723=DIRECTION('',(0.216280117331436,0.,0.9763313529981));
#78724=DIRECTION('center_axis',(-0.0961354113898672,-0.987363722329987,
0.125979611459841));
#78725=DIRECTION('ref_axis',(-0.760058487094592,-0.00890474036864194,-0.649793660937414));
#78726=DIRECTION('center_axis',(0.115688529063399,-0.987363722404488,-0.108300710628786));
#78727=DIRECTION('ref_axis',(-0.729641847515942,-0.0104932879451102,-0.683748978252709));
#78728=DIRECTION('',(-0.99999910056149,0.,0.00134122190962044));
#78729=DIRECTION('center_axis',(3.47506295206373E-14,-1.,2.78566962532615E-14));
#78730=DIRECTION('ref_axis',(1.,3.47506295206373E-14,4.63567395073469E-32));
#78731=DIRECTION('center_axis',(-0.0980734723655976,0.987363721986029,0.124476803156453));
#78732=DIRECTION('ref_axis',(-0.824228051317188,-0.0104936262373712,-0.566160757409291));
#78733=DIRECTION('center_axis',(0.113998724386721,0.987363721657003,-0.11007802684384));
#78734=DIRECTION('ref_axis',(-0.778199249123463,0.0198684673062269,-0.627703092768053));
#78735=DIRECTION('',(0.00134122641155386,0.,0.999999100555452));
#78736=DIRECTION('center_axis',(-0.120969711832683,-0.987363722336904,0.10236800590092));
#78737=DIRECTION('ref_axis',(-0.602602313497403,-0.00890473952231705,-0.797991953206057));
#78738=DIRECTION('center_axis',(0.136265247370615,-0.987363722378472,-0.0808990858412706));
#78739=DIRECTION('ref_axis',(-0.565597408134151,-0.010493288525919,-0.824614735987565));
#78740=DIRECTION('',(-0.976908000747675,0.,-0.213660380218656));
#78741=DIRECTION('center_axis',(-1.86332085823107E-14,-1.,-2.31171868766338E-14));
#78742=DIRECTION('ref_axis',(-2.32159898207252E-31,2.31171868766338E-14,
-1.));
#78743=DIRECTION('center_axis',(-0.122539404214814,0.987363722008592,0.10048370452973));
#78744=DIRECTION('ref_axis',(-0.683250231372573,-0.0104936297776743,-0.730108899455016));
#78745=DIRECTION('center_axis',(0.134997021813067,0.987363721562226,-0.0829981050650767));
#78746=DIRECTION('ref_axis',(-0.625067771768455,0.0198684707171492,-0.78031757930203));
#78747=DIRECTION('',(-0.213660376481803,0.,0.976908001564965));
#78748=DIRECTION('center_axis',(-0.140147603738312,-0.987363722333548,0.0739697842774299));
#78749=DIRECTION('ref_axis',(-0.416969124659213,-0.00890473688030596,-0.908877029494102));
#78750=DIRECTION('center_axis',(0.150470353718179,-0.987363722377245,-0.0497147099486297));
#78751=DIRECTION('ref_axis',(-0.37510626190524,-0.0104932884810437,-0.926922425651862));
#78752=DIRECTION('',(-0.908137769272627,0.,-0.418671460718947));
#78753=DIRECTION('center_axis',(3.96841880413548E-14,-1.,7.9746926833596E-14));
#78754=DIRECTION('ref_axis',(2.96482732682133E-31,-7.9746926833596E-14,
-1.));
#78755=DIRECTION('center_axis',(-0.141275524388681,0.987363722030692,0.0717921069923499));
#78756=DIRECTION('ref_axis',(-0.510324391310211,-0.0104936240876129,-0.859917960905208));
#78757=DIRECTION('center_axis',(0.149683006307519,0.987363721553883,-0.052037284537236));
#78758=DIRECTION('ref_axis',(-0.442708819693711,0.0198684723546586,-0.896445282642334));
#78759=DIRECTION('',(-0.41867146160869,0.,0.908137768862436));
#78760=DIRECTION('center_axis',(-0.152772346323565,-0.987363722329941,0.0421128249534124));
#78761=DIRECTION('ref_axis',(-0.211838925404988,-0.00890474194811866,-0.977264025355532));
#78762=DIRECTION('center_axis',(0.157639633326776,-0.987363722396684,-0.0162057304544932));
#78763=DIRECTION('ref_axis',(-0.167075565562151,-0.0104932877122433,-0.985888252442981));
#78764=DIRECTION('',(-0.796904023488092,-6.23377073564162E-15,-0.604105932224218));
#78765=DIRECTION('center_axis',(-1.08065809005894E-14,-1.,-4.32067076774285E-14));
#78766=DIRECTION('ref_axis',(1.3068534013106E-31,4.32067076774285E-14,-1.));
#78767=DIRECTION('center_axis',(-0.153405762942741,0.987363721993324,0.0397435829719167));
#78768=DIRECTION('ref_axis',(-0.313536345948425,-0.0104936267221054,-0.949518216553809));
#78769=DIRECTION('center_axis',(0.157369977170714,0.98736372166309,-0.0186432676562037));
#78770=DIRECTION('ref_axis',(-0.239649298886824,0.0198684648167131,-0.970656199510867));
#78771=DIRECTION('',(-0.604105932750183,0.,0.796904023089375));
#78772=DIRECTION('',(-0.64840793185587,0.,-0.761293080164527));
#78773=DIRECTION('',(-0.761293077687916,0.,0.648407934763649));
#78774=DIRECTION('center_axis',(-0.156335141249768,-0.987363722339936,-0.0259268859958497));
#78775=DIRECTION('ref_axis',(0.218082714256779,-0.00890473458450209,-0.975889663560577));
#78776=DIRECTION('center_axis',(0.149874466705301,-0.987363722477481,0.0514832377110639));
#78777=DIRECTION('ref_axis',(0.26233005865523,-0.0104932834881059,-0.964921152907108));
#78778=DIRECTION('',(-0.469593007892373,0.,-0.882883008636248));
#78779=DIRECTION('center_axis',(2.77807948950603E-15,-1.,-1.45836371277071E-14));
#78780=DIRECTION('ref_axis',(-3.32256348487704E-32,1.45836371277071E-14,
-1.));
#78781=DIRECTION('center_axis',(-0.155915196790434,0.987363722007201,-0.0283431098132548));
#78782=DIRECTION('ref_axis',(0.114134469893609,-0.0104936276209515,-0.993409888495911));
#78783=DIRECTION('center_axis',(0.150653227138706,0.987363721651154,0.0491577696796259));
#78784=DIRECTION('ref_axis',(0.190068147031143,0.0198684676975153,-0.981569836270197));
#78785=DIRECTION('',(-0.882883007870352,0.,0.469593009332337));
#78786=DIRECTION('center_axis',(-0.147106599459758,-0.987363722334265,-0.0589281614647145));
#78787=DIRECTION('ref_axis',(0.422771490401481,-0.00890473699181164,-0.906192569249394));
#78788=DIRECTION('center_axis',(0.135303108094111,-0.98736372235854,0.0824981739819796));
#78789=DIRECTION('ref_axis',(0.463626451505004,-0.0104932900032102,-0.885968624912749));
#78790=DIRECTION('',(-0.268820435286404,0.,-0.963190310152894));
#78791=DIRECTION('center_axis',(2.92409021633132E-14,-1.,-6.82273741811819E-14));
#78792=DIRECTION('ref_axis',(1.48618071870625E-31,6.82273741811819E-14,
-1.));
#78793=DIRECTION('center_axis',(-0.146177057117787,0.98736372202545,-0.0611976176042204));
#78794=DIRECTION('ref_axis',(0.325019829443857,-0.010493622859718,-0.94564898051421));
#78795=DIRECTION('center_axis',(0.136563571725779,0.987363721650438,0.0803944777089522));
#78796=DIRECTION('ref_axis',(0.396632959753101,0.019868466210324,-0.91776224551239));
#78797=DIRECTION('',(-0.963190309714461,0.,0.26882043685732));
#78798=DIRECTION('center_axis',(-0.130999516830709,-0.987363722332075,-0.0891740231943641));
#78799=DIRECTION('ref_axis',(0.607691945400389,-0.00890473868258867,-0.794122915627352));
#78800=DIRECTION('center_axis',(0.114405126201655,-0.98736372230861,0.10965558338575));
#78801=DIRECTION('ref_axis',(0.643244187693094,-0.0104932928074988,-0.765589188667857));
#78802=DIRECTION('',(-0.0554781176097352,0.,-0.998459903284293));
#78803=DIRECTION('center_axis',(-2.59344808506195E-14,-1.,3.62077958619679E-14));
#78804=DIRECTION('ref_axis',(-2.56733982118683E-31,-3.62077958619679E-14,
-1.));
#78805=DIRECTION('center_axis',(-0.129603838858743,0.987363722017638,-0.0911905992773047));
#78806=DIRECTION('ref_axis',(0.520707624190231,-0.0104936248398,-0.853670576948677));
#78807=DIRECTION('center_axis',(0.116088352443771,0.987363721593397,0.107872033948232));
#78808=DIRECTION('ref_axis',(0.584651655468008,0.0198684704736681,-0.811041112175921));
#78809=DIRECTION('',(-0.998459903193811,0.,0.0554781192381759));
#78810=DIRECTION('center_axis',(-0.108767041434347,-0.987363722333227,-0.115250208320386));
#78811=DIRECTION('ref_axis',(0.764197398165907,-0.00890473803429298,-0.644920958162315));
#78812=DIRECTION('center_axis',(0.0881576937942685,-0.987363722413996,0.131685613054932));
#78813=DIRECTION('ref_axis',(0.792784541219236,-0.0104932863050875,-0.60941165245368));
#78814=DIRECTION('',(0.160458295775008,0.,-0.987042620820894));
#78815=DIRECTION('center_axis',(0.,-1.,0.));
#78816=DIRECTION('ref_axis',(0.,0.,-1.));
#78817=DIRECTION('center_axis',(-0.106970493768576,0.987363722044527,-0.116919604229933));
#78818=DIRECTION('ref_axis',(0.692047709918238,-0.0104936191287768,-0.721775485282302));
#78819=DIRECTION('center_axis',(0.0901849707939082,0.987363721562147,0.130305611490251));
#78820=DIRECTION('ref_axis',(0.74533268947275,0.0198684729177045,-0.666396597970935));
#78821=DIRECTION('',(-0.987042621082596,0.,-0.160458294165178));
#78822=DIRECTION('center_axis',(-0.0814487385773337,-0.987363722310449,
-0.135937422549555));
#78823=DIRECTION('ref_axis',(0.884969829016091,-0.00890473544370706,-0.465563215275765));
#78824=DIRECTION('center_axis',(0.0577880997168462,-0.987363722387455,0.147558175796212));
#78825=DIRECTION('ref_axis',(0.905255170761543,-0.0104932883859293,-0.424738704038541));
#78826=DIRECTION('',(0.368891856208119,0.,-0.929472322569816));
#78827=DIRECTION('center_axis',(-1.03308683298469E-13,-1.,5.85911991188191E-14));
#78828=DIRECTION('ref_axis',(1.,-1.03308683298469E-13,-1.34828625307809E-30));
#78829=DIRECTION('center_axis',(-0.0793353189734799,0.987363722004231,-0.137181586349362));
#78830=DIRECTION('ref_axis',(0.831028411874342,-0.0104936257469269,-0.556130976008612));
#78831=DIRECTION('center_axis',(0.0600646425439804,0.987363721585129,0.146646241048408));
#78832=DIRECTION('ref_axis',(0.87116279556875,0.0198684718001344,-0.49059211922448));
#78833=DIRECTION('',(-0.929472323171464,0.,-0.368891854692188));
#78834=DIRECTION('center_axis',(-0.0503219877413936,-0.987363722316605,
-0.150268351301444));
#78835=DIRECTION('ref_axis',(0.964362055625502,-0.0089047387008506,-0.264436251861248));
#78836=DIRECTION('center_axis',(0.0247164004782463,-0.98736372239089,0.156531080791658));
#78837=DIRECTION('ref_axis',(0.975397074152575,-0.0104932879170649,-0.220205446443284));
#78838=DIRECTION('',(0.560076443596158,0.,-0.828440931707674));
#78839=DIRECTION('center_axis',(0.,-1.,0.));
#78840=DIRECTION('ref_axis',(0.,0.,-1.));
#78841=DIRECTION('center_axis',(-0.0479905184903675,0.987363721986371,-0.151029105275263));
#78842=DIRECTION('ref_axis',(0.93115115039746,-0.0104936244188649,-0.36448239869717));
#78843=DIRECTION('center_axis',(0.0271357589007339,0.987363721594987,0.156129855783506));
#78844=DIRECTION('ref_axis',(0.956258297310921,0.0198684704798575,-0.291848098682876));
#78845=DIRECTION('',(-0.828440931287221,0.,-0.560076444218074));
#78846=DIRECTION('center_axis',(-0.0168422317619783,-0.987363722303815,
-0.157572900930427));
#78847=DIRECTION('ref_axis',(0.9986617842021,-0.00890473654938958,-0.0509445428015999));
#78848=DIRECTION('center_axis',(-0.0095110139153878,-0.987363722326397,
0.158184766801555));
#78849=DIRECTION('ref_axis',(0.999930494315556,-0.0104932914060547,-0.00537562771357042));
#78850=DIRECTION('',(0.725072479416806,0.,-0.688672563409031));
#78851=DIRECTION('center_axis',(1.47952784583182E-14,-1.,-1.2247177407368E-15));
#78852=DIRECTION('ref_axis',(1.,1.47952784583182E-14,-9.42445205896519E-33));
#78853=DIRECTION('center_axis',(-0.0144017381581264,0.98736372201421,-0.157814671017212));
#78854=DIRECTION('ref_axis',(0.987734295571055,-0.0104936198849398,-0.155791030853714));
#78855=DIRECTION('center_axis',(-0.00706196206119799,0.987363721631619,
0.158313012407715));
#78856=DIRECTION('ref_axis',(0.99664022404459,0.0198684685501518,-0.0794575847469598));
#78857=DIRECTION('',(-0.688672563156092,0.,-0.725072479657047));
#78858=DIRECTION('center_axis',(0.0174250494756407,-0.987363722319657,-0.157509515578722));
#78859=DIRECTION('ref_axis',(0.986265197685238,-0.00890473293355562,0.164929274436897));
#78860=DIRECTION('center_axis',(-0.0432936989265123,-0.987363722380122,
0.152441908151695));
#78861=DIRECTION('ref_axis',(0.977708276320475,-0.0104932898364058,0.209705549003491));
#78862=DIRECTION('',(0.85616493303156,-6.23377073251911E-15,-0.516702629611138));
#78863=DIRECTION('center_axis',(0.,-1.,0.));
#78864=DIRECTION('ref_axis',(0.,0.,-1.));
#78865=DIRECTION('center_axis',(0.0198604574059867,0.98736372203083,-0.157220999389557));
#78866=DIRECTION('ref_axis',(0.998132083080332,-0.0104936214945499,0.0601849535485897));
#78867=DIRECTION('center_axis',(-0.0409294756228172,0.987363721602464,0.153093629157369));
#78868=DIRECTION('ref_axis',(0.99042036160996,0.0198684691135502,0.136648275669615));
#78869=DIRECTION('',(-0.516702631843025,0.,-0.856164931684597));
#78870=DIRECTION('center_axis',(0.0508775475539415,-0.987363722317753,-0.150081161395184));
#78871=DIRECTION('ref_axis',(0.927751945958094,-0.00890473735616938,0.373091185132519));
#78872=DIRECTION('center_axis',(-0.075052025203131,-0.987363722271263,0.139571033726721));
#78873=DIRECTION('ref_axis',(0.909769504880944,-0.0104932946190869,0.414981130603211));
#78874=DIRECTION('',(0.947224063311177,-6.23377072438015E-15,-0.320572260004298));
#78875=DIRECTION('center_axis',(1.11536613512245E-13,-1.,4.08068196962375E-14));
#78876=DIRECTION('ref_axis',(1.,1.11536613512245E-13,2.49166158235023E-31));
#78877=DIRECTION('center_axis',(0.0531940004054215,0.987363721999169,-0.149275848015733));
#78878=DIRECTION('ref_axis',(0.961858323093725,-0.0104936232507952,0.273346758104787));
#78879=DIRECTION('center_axis',(-0.0728831743619325,0.987363721576898,0.140715756789161));
#78880=DIRECTION('ref_axis',(0.937889543295604,0.019868471341455,0.346364617741648));
#78881=DIRECTION('',(-0.320572261549173,0.,-0.94722406278834));
#78882=DIRECTION('center_axis',(0.0819510725694303,-0.987363722321963,-0.135635178133246));
#78883=DIRECTION('ref_axis',(0.825858045362124,-0.00890473659940747,0.563807763849299));
#78884=DIRECTION('center_axis',(-0.10330099281142,-0.987363722350749,0.120173976674849));
#78885=DIRECTION('ref_axis',(0.799290923600527,-0.0104932893936424,0.600852652758992));
#78886=DIRECTION('',(0.993992051028923,6.23377071783232E-15,-0.109452284084504));
#78887=DIRECTION('center_axis',(0.,-1.,0.));
#78888=DIRECTION('ref_axis',(0.,0.,-1.));
#78889=DIRECTION('center_axis',(0.0840402479765716,0.987363722025755,-0.134350724402526));
#78890=DIRECTION('ref_axis',(0.880609137464754,-0.0104936222499426,0.473727169271151));
#78891=DIRECTION('center_axis',(-0.101428934845169,0.98736372155012,0.121758172386384));
#78892=DIRECTION('ref_axis',(0.841504053053872,0.0198684718986061,0.539885332749762));
#78893=DIRECTION('',(-0.109452286018412,0.,-0.993992050815973));
#78894=DIRECTION('center_axis',(0.109192655757424,-0.987363722338937,-0.114847044966942));
#78895=DIRECTION('ref_axis',(0.685347939677887,-0.00890473688215913,0.728161319516723));
#78896=DIRECTION('center_axis',(-0.126719726918145,-0.987363722313106,0.0951577147150889));
#78897=DIRECTION('ref_axis',(0.651438386396749,-0.0104932911252255,0.758628973589963));
#78898=DIRECTION('',(0.994282074768413,0.,0.106785559858154));
#78899=DIRECTION('center_axis',(0.,-1.,0.));
#78900=DIRECTION('ref_axis',(0.,0.,-1.));
#78901=DIRECTION('center_axis',(0.110956868842276,0.987363722031638,-0.113143509193188));
#78902=DIRECTION('ref_axis',(0.758183647957641,-0.0104936236265723,0.651956624195834));
#78903=DIRECTION('center_axis',(-0.125231991823691,0.987363721532925,0.0971073098408352));
#78904=DIRECTION('ref_axis',(0.705770767641394,0.0198684735905038,0.708161611004198));
#78905=DIRECTION('',(0.106785558236532,0.,-0.994282074942575));
#78906=DIRECTION('center_axis',(0.131328513345731,-0.987363722333514,-0.0886887896078565));
#78907=DIRECTION('ref_axis',(0.512791724826996,-0.00890473470600238,0.858466861706828));
#78908=DIRECTION('center_axis',(-0.14421318479626,-0.987363722360672,0.0656919865508537));
#78909=DIRECTION('ref_axis',(0.473125316803008,-0.0104932893774458,0.880932645256205));
#78910=DIRECTION('',(0.948080573707217,0.,0.318030227744147));
#78911=DIRECTION('center_axis',(1.60245723675726E-14,-1.,2.49962771693286E-14));
#78912=DIRECTION('ref_axis',(2.60545369112877E-31,-2.49962771693286E-14,
-1.));
#78913=DIRECTION('center_axis',(0.132685267518363,0.987363722025376,-0.0866458320508048));
#78914=DIRECTION('ref_axis',(0.600306333746986,-0.0104936211668166,0.799701312727483));
#78915=DIRECTION('center_axis',(-0.143179334653652,0.987363721650584,0.0679158250810903));
#78916=DIRECTION('ref_axis',(0.537036428165803,0.0198684662055829,0.843325037499512));
#78917=DIRECTION('',(0.318030226197875,0.,-0.948080574225908));
#78918=DIRECTION('center_axis',(0.147323593750354,-0.987363722328393,-0.058383546948617));
#78919=DIRECTION('ref_axis',(0.316257941884461,-0.00890473470053631,0.948631445765382));
#78920=DIRECTION('center_axis',(-0.154963396007214,-0.987363722357769,0.0331545723803159));
#78921=DIRECTION('ref_axis',(0.272689429059446,-0.0104932892324504,0.962044887809461));
#78922=DIRECTION('',(0.857547878362251,0.,0.514404156589351));
#78923=DIRECTION('center_axis',(-2.56911651515087E-14,-1.,-6.96417186706459E-14));
#78924=DIRECTION('ref_axis',(5.51927619771536E-31,6.96417186706459E-14,
-1.));
#78925=DIRECTION('center_axis',(0.148209454900643,0.987363721999609,-0.0560966840119264));
#78926=DIRECTION('ref_axis',(0.414359359374223,-0.0104936275490271,0.910052858398811));
#78927=DIRECTION('center_axis',(-0.154431776622887,0.987363721630883,0.0355486649019513));
#78928=DIRECTION('ref_axis',(0.343190859386594,0.0198684674577238,0.939055524468267));
#78929=DIRECTION('',(0.514404155190728,0.,-0.857547879201222));
#78930=DIRECTION('center_axis',(0.156429986048551,-0.987363722317835,-0.0253483592273561));
#78931=DIRECTION('ref_axis',(0.104936288763443,-0.00890473956698211,0.994439078533119));
#78932=DIRECTION('center_axis',(-0.158467691048673,-0.987363722338777,-0.000933114686009084));
#78933=DIRECTION('ref_axis',(0.0595028880774467,-0.0104932912931376,0.998172979572319));
#78934=DIRECTION('',(0.726917198560946,0.,0.686725117085655));
#78935=DIRECTION('center_axis',(-6.07176543710283E-15,-1.,-4.41218250330748E-14));
#78936=DIRECTION('ref_axis',(1.229306260954E-32,4.41218250330748E-14,-1.));
#78937=DIRECTION('center_axis',(0.156803528780516,0.987363722000409,-0.0229245248473604));
#78938=DIRECTION('ref_axis',(0.209037406064962,-0.0104936259099717,0.977851341810653));
#78939=DIRECTION('center_axis',(-0.158463159546821,0.987363721647528,0.00151928956512539));
#78940=DIRECTION('ref_axis',(0.133298067969916,0.0198684676897788,0.990876818311513));
#78941=DIRECTION('center_axis',(1.18502573726487E-15,-1.,-1.47985104495617E-14));
#78942=DIRECTION('ref_axis',(5.2890212177402E-33,1.47985104495617E-14,-1.));
#78943=DIRECTION('center_axis',(0.15822188745822,-0.987363722342132,0.00887209850308879));
#78944=DIRECTION('ref_axis',(-0.111292072300084,-0.00890473567894903,0.993747845444528));
#78945=DIRECTION('center_axis',(0.158065644488417,0.987363722016583,0.0113195617415647));
#78946=DIRECTION('ref_axis',(-0.00605890847863349,-0.01049362580408,0.999926584027813));
#78947=DIRECTION('center_axis',(-0.155084981185087,0.987363721609556,-0.032581127361534));
#78948=DIRECTION('ref_axis',(-0.082827591604534,0.0198684694891143,0.99636581333823));
#78949=DIRECTION('',(0.686725115900101,0.,-0.726917199680949));
#78950=DIRECTION('center_axis',(0.160735571009733,-0.986495108236408,-0.0314877378961024));
#78951=DIRECTION('ref_axis',(0.0338459065175243,-0.026374683548954,0.999078991211255));
#78952=DIRECTION('center_axis',(0.150208716674817,-0.98649510778408,-0.0653050055736983));
#78953=DIRECTION('ref_axis',(0.247827082207865,-0.0263747191535445,0.968445203154989));
#78954=DIRECTION('center_axis',(0.132658271716979,-0.986495107714006,-0.09606864942007));
#78955=DIRECTION('ref_axis',(0.450220114874771,-0.026374724543006,0.89252799511692));
#78956=DIRECTION('center_axis',(0.108904879252692,-0.986495107784954,-0.122340220660702));
#78957=DIRECTION('ref_axis',(0.631561354084168,-0.026374718820451,0.774877171062946));
#78958=DIRECTION('center_axis',(0.0800592132564947,-0.986495107789174,-0.142891303726913));
#78959=DIRECTION('ref_axis',(0.78337148772173,-0.0263747179124343,0.620993950437267));
#78960=DIRECTION('center_axis',(0.0474700634140202,-0.986495107779111,-0.156760949880223));
#78961=DIRECTION('ref_axis',(0.898552041178325,-0.0263747212958625,0.438073741932602));
#78962=DIRECTION('center_axis',(0.0126612724730868,-0.986495107813198,-0.163300625963248));
#78963=DIRECTION('ref_axis',(0.971717298672813,-0.0263747183100887,0.234669694877874));
#78964=DIRECTION('center_axis',(-0.0227395414182952,-0.986495107969959,
-0.162204547431399));
#78965=DIRECTION('ref_axis',(0.999446135984411,-0.0263747114092139,0.0202927539755223));
#78966=DIRECTION('center_axis',(-0.057077088049556,-0.986495107936662,-0.153523965675774));
#78967=DIRECTION('ref_axis',(0.980441982767649,-0.0263747128260375,-0.195033056044317));
#78968=DIRECTION('center_axis',(-0.0887457768143703,-0.986495107851645,
-0.137664771391902));
#78969=DIRECTION('ref_axis',(0.915593452045644,-0.0263747184035609,-0.401239336058012));
#78970=DIRECTION('center_axis',(-0.11626480563914,-0.986495107850101,-0.115368527586643));
#78971=DIRECTION('ref_axis',(0.807932787678787,-0.0263747169054886,-0.588684113002669));
#78972=DIRECTION('center_axis',(-0.138347424378308,-0.986495107799886,-0.0876777762878373));
#78973=DIRECTION('ref_axis',(0.662494084335353,-0.0263747202768151,-0.748602673219233));
#78974=DIRECTION('center_axis',(-0.153961068298618,-0.986495107760049,-0.0558873135321256));
#78975=DIRECTION('ref_axis',(0.48607789980036,-0.0263747196220043,-0.873517400794358));
#78976=DIRECTION('center_axis',(-0.16237566480624,-0.986495107781903,-0.0214836170395995));
#78977=DIRECTION('ref_axis',(0.28693324431429,-0.0263747224425676,-0.957587430641899));
#78978=DIRECTION('center_axis',(-0.163197754870596,-0.986495107694381,0.0139246292679042));
#78979=DIRECTION('ref_axis',(0.0743719117694134,-0.0263747254297085,-0.9968817345093));
#78980=DIRECTION('center_axis',(-0.156388898490704,-0.986495107734565,0.0486817711739611));
#78981=DIRECTION('ref_axis',(-0.14166696604054,-0.026374724445378,-0.989562956381906));
#78982=DIRECTION('center_axis',(-0.14226747115853,-0.986495107737351,0.0811626087581541));
#78983=DIRECTION('ref_axis',(-0.351081656040152,-0.0263747243360462,-0.935973314100515));
#78984=DIRECTION('center_axis',(-0.121493781342904,-0.986495107917773,0.109848364345144));
#78985=DIRECTION('ref_axis',(-0.544080153780647,-0.0263747142436309,-0.838618602649974));
#78986=DIRECTION('center_axis',(-0.0950391693815611,-0.986495107856857,
0.133397745324843));
#78987=DIRECTION('ref_axis',(-0.711638074696993,-0.0263747184469962,-0.702051013010022));
#78988=DIRECTION('center_axis',(-0.0641406289410978,-0.986495107726884,
0.150709595414372));
#78989=DIRECTION('ref_axis',(-0.84592058827809,-0.0263747244747136,-0.532656298410273));
#78990=DIRECTION('center_axis',(-0.0302429488762457,-0.986495107736434,
0.160974427954722));
#78991=DIRECTION('ref_axis',(-0.940648794174339,-0.0263747240848742,-0.338355168348007));
#78992=DIRECTION('center_axis',(0.00506885405486264,-0.986495107766302,
0.163712275262799));
#78993=DIRECTION('ref_axis',(-0.991393307475592,-0.0263747202754443,-0.128232928778058));
#78994=DIRECTION('center_axis',(0.0401436540411063,-0.986495107671852,0.158795118249051));
#78995=DIRECTION('ref_axis',(-0.99578137173735,-0.026374727357795,0.0878853426783058));
#78996=DIRECTION('center_axis',(0.0733413717326372,-0.986495107710258,0.146452878620057));
#78997=DIRECTION('ref_axis',(-0.95360780588139,-0.0263747246785699,0.29989419210817));
#78998=DIRECTION('center_axis',(0.103109727120042,-0.986495107818647,0.127262667043824));
#78999=DIRECTION('ref_axis',(-0.866844599765875,-0.0263747203806475,0.497880320942274));
#79000=DIRECTION('center_axis',(0.128056786609181,-0.986495107867452,0.102121797658064));
#79001=DIRECTION('ref_axis',(-0.739548704901369,-0.0263747148151698,0.672586119019064));
#79002=DIRECTION('center_axis',(0.147016061558686,-0.986495107750468,0.0722058171352182));
#79003=DIRECTION('ref_axis',(-0.577672332535789,-0.0263747217122836,0.815842540124784));
#79004=DIRECTION('center_axis',(0.159101024800094,-0.986495107740196,0.0389135749092782));
#79005=DIRECTION('ref_axis',(-0.388784639613202,-0.0263747238453144,0.92095107250218));
#79006=DIRECTION('center_axis',(0.163746574337308,-0.986495111251671,0.00380195599009181));
#79007=DIRECTION('ref_axis',(-0.181717844385214,-0.0263745487091407,0.982996952290484));
#79008=DIRECTION('center_axis',(-0.159100997357643,0.98649510752794,-0.0389136924904468));
#79009=DIRECTION('ref_axis',(-0.0837188756473344,0.02579266142082,0.996155554357439));
#79010=DIRECTION('center_axis',(0.158479747774604,0.986495108552522,0.0413711293929183));
#79011=DIRECTION('ref_axis',(-0.188882155795407,-0.0108363123862134,0.981939970444196));
#79012=DIRECTION('center_axis',(-0.147016016485829,0.986495108226829,-0.0722059023984579));
#79013=DIRECTION('ref_axis',(-0.295905551411954,0.0257926430848816,0.954868914671686));
#79014=DIRECTION('center_axis',(0.145881036647377,0.98649510866697,0.0744723017156756));
#79015=DIRECTION('ref_axis',(-0.395554272691206,-0.0108362488831137,0.918378676290927));
#79016=DIRECTION('center_axis',(-0.12805672646284,0.986495108187664,-0.102121869985965));
#79017=DIRECTION('ref_axis',(-0.49425603816082,0.0257926470332549,0.868933661507361));
#79018=DIRECTION('center_axis',(0.126461036348405,0.986495108605843,0.104091339613025));
#79019=DIRECTION('ref_axis',(-0.583730693143186,-0.0108363135264812,0.811875022519927));
#79020=DIRECTION('center_axis',(-0.103109645269706,0.986495108091246,-0.127262731246802));
#79021=DIRECTION('ref_axis',(-0.669495658588641,0.0257926510703653,0.742368036947796));
#79022=DIRECTION('center_axis',(0.101127884369277,0.98649510856977,0.128843128535876));
#79023=DIRECTION('ref_axis',(-0.744612526030204,-0.0108363161639954,0.667408990298237));
#79024=DIRECTION('center_axis',(-0.0733412770708288,0.986495108148242,-0.146452923074984));
#79025=DIRECTION('ref_axis',(-0.813430404670402,0.0257926474265038,0.581090110134803));
#79026=DIRECTION('center_axis',(0.0710661069826356,0.986495108527701,0.147570353693592));
#79027=DIRECTION('ref_axis',(-0.870677103550572,-0.0108363157948494,0.491735656234914));
#79028=DIRECTION('center_axis',(-0.0401435546289612,0.986495108250283,-0.15879513978713));
#79029=DIRECTION('ref_axis',(-0.919330050714222,0.0257926418184515,0.392641054249057));
#79030=DIRECTION('center_axis',(0.0376813611744201,0.986495108564832,0.15939735191559));
#79031=DIRECTION('ref_axis',(-0.956029786695043,-0.0108363116963436,0.293069311427605));
#79032=DIRECTION('center_axis',(-0.00506877383917619,0.986495109538723,
-0.163712267066185));
#79033=DIRECTION('ref_axis',(-0.982242845537332,0.0257926261277419,0.18583253974522));
#79034=DIRECTION('center_axis',(0.00253467411141179,0.986495108531174,0.163771109391173));
#79035=DIRECTION('ref_axis',(-0.996679580402424,-0.010836310684072,0.0806993703792479));
#79036=DIRECTION('center_axis',(0.030243052772592,0.986495108131346,-0.160974406015112));
#79037=DIRECTION('ref_axis',(-0.999227055883883,0.0257926494833967,-0.0296652999690604));
#79038=DIRECTION('center_axis',(-0.0327304788680687,0.98649510864271,0.160487122153385));
#79039=DIRECTION('ref_axis',(-0.990725744073173,-0.0108362535714797,-0.13544399447444));
#79040=DIRECTION('center_axis',(0.0641407249324134,0.986495108138678,-0.150709551865841));
#79041=DIRECTION('ref_axis',(-0.969488520532474,0.0257926487542448,-0.24377601979275));
#79042=DIRECTION('center_axis',(-0.066465247725591,0.986495108659402,0.149698935987706));
#79043=DIRECTION('ref_axis',(-0.938446671669539,-0.0108362558229288,-0.345254138269339));
#79044=DIRECTION('center_axis',(0.0950392464485186,0.986495108205489,-0.133397687840304));
#79045=DIRECTION('ref_axis',(-0.894417778304127,0.0257926452473245,-0.446488048333497));
#79046=DIRECTION('center_axis',(-0.0970922211053784,0.986495108544631,0.131910960190357));
#79047=DIRECTION('ref_axis',(-0.842286880175986,-0.0108363168256393,-0.538920574594308));
#79048=DIRECTION('center_axis',(0.121493846397364,0.986495108098352,-0.109848290772291));
#79049=DIRECTION('ref_axis',(-0.77752505341967,0.0257926516741728,-0.628322791584353));
#79050=DIRECTION('center_axis',(-0.123179214736194,0.98649510858114,0.10795499896929));
#79051=DIRECTION('ref_axis',(-0.706742688013733,-0.0108363149944035,-0.707387692299255));
#79052=DIRECTION('center_axis',(0.142267519731351,0.986495108183289,-0.0811625181960835));
#79053=DIRECTION('ref_axis',(-0.624276124919574,0.0257926459277216,-0.78077785526451));
#79054=DIRECTION('center_axis',(-0.143506486862139,0.986495108529785,0.0789511815953027));
#79055=DIRECTION('ref_axis',(-0.538151993297995,-0.0108363146180653,-0.842778147791513));
#79056=DIRECTION('center_axis',(0.156388927828418,0.986495108133772,-0.0486816688376107));
#79057=DIRECTION('ref_axis',(-0.441836737174637,0.025792649754231,-0.896724615978354));
#79058=DIRECTION('center_axis',(-0.157123555131713,0.986495108582043,0.046255693341188));
#79059=DIRECTION('ref_axis',(-0.344397908228475,-0.0108363152052421,-0.938761234329914));
#79060=DIRECTION('center_axis',(0.163197761691791,0.98649510810079,-0.0139245205303402));
#79061=DIRECTION('ref_axis',(-0.238737553542187,0.0257926509570806,-0.97074153083367));
#79062=DIRECTION('center_axis',(-0.163393695748629,0.986495108696646,0.0113973991417967));
#79063=DIRECTION('ref_axis',(-0.134540152524605,-0.0108362549029294,-0.990848890062624));
#79064=DIRECTION('center_axis',(0.162375649064761,0.986495108153596,0.0214837189476841));
#79065=DIRECTION('ref_axis',(-0.0244752698996862,0.0257926484885163,-0.999367650290565));
#79066=DIRECTION('center_axis',(-0.162023738619945,0.986495108586251,-0.0239939337962111));
#79067=DIRECTION('ref_axis',(0.0816085326334352,-0.0108363112271417,-0.996605549733898));
#79068=DIRECTION('center_axis',(0.153961032422443,0.986495108170358,0.0558874051228876));
#79069=DIRECTION('ref_axis',(0.190931452696257,0.0257926471489565,-0.98126444943468));
#79070=DIRECTION('center_axis',(-0.153077727573336,0.986495108555797,-0.0582632827471033));
#79071=DIRECTION('ref_axis',(0.293941306053273,-0.0108363101764777,-0.955762043072153));
#79072=DIRECTION('center_axis',(0.138347370174831,0.986495108190401,0.0876778574220337));
#79073=DIRECTION('ref_axis',(0.397410430852247,0.0257926448954982,-0.917278414070192));
#79074=DIRECTION('center_axis',(-0.136973968593323,0.986495108545223,-0.0898083111084));
#79075=DIRECTION('ref_axis',(0.492529708452136,-0.0108363163076087,-0.870228165793854));
#79076=DIRECTION('center_axis',(0.116264737376085,0.986495108195573,0.115368593425922));
#79077=DIRECTION('ref_axis',(0.585306940258781,0.0257926456565238,-0.810401459225574));
#79078=DIRECTION('center_axis',(-0.114465461008113,0.98649510855171,-0.117153997113845));
#79079=DIRECTION('ref_axis',(0.668087970700035,-0.010836316193007,-0.744003385514659));
#79080=DIRECTION('center_axis',(0.0887457396433074,0.986495110261859,0.137664778082866));
#79081=DIRECTION('ref_axis',(0.745835155355629,0.0257925810343138,-0.665631026770261));
#79082=DIRECTION('center_axis',(-0.0866046781088066,0.986495108574076,-0.139021690714405));
#79083=DIRECTION('ref_axis',(0.812407179532708,-0.0108363136409741,-0.582989836060959));
#79084=DIRECTION('center_axis',(0.0570770025958331,0.986495108207936,0.153523995702587));
#79085=DIRECTION('ref_axis',(0.871488933067144,0.0257926456383099,-0.489736438273146));
#79086=DIRECTION('center_axis',(-0.0546943527508883,0.986495108539707,-0.154388887567706));
#79087=DIRECTION('ref_axis',(0.918739133301432,-0.0108363157338381,-0.394716327508567));
#79088=DIRECTION('center_axis',(0.0227394532199647,0.986495108204772,0.162204558367862));
#79089=DIRECTION('ref_axis',(0.956392864428311,0.0257926451466668,-0.290942310994721));
#79090=DIRECTION('center_axis',(-0.0202265838329727,0.986495108564546,-0.162537029887571));
#79091=DIRECTION('ref_axis',(0.982111865497668,-0.0108363139982903,-0.187986323831341));
#79092=DIRECTION('center_axis',(-0.0126613696931214,0.986495108187824,0.1633006161623));
#79093=DIRECTION('ref_axis',(0.996576927422038,0.0257926468525222,-0.0785440455947577));
#79094=DIRECTION('center_axis',(0.0151869637456814,0.986495108589766,-0.163085121518345));
#79095=DIRECTION('ref_axis',(0.999562138566932,-0.0108363183416792,0.0275337129406814));
#79096=DIRECTION('center_axis',(-0.0474701574982222,0.986495108181291,0.156760918858867));
#79097=DIRECTION('ref_axis',(0.990162161023867,0.0257926453276796,0.137526849464193));
#79098=DIRECTION('center_axis',(0.0498903833976718,0.986495108560806,-0.156007533247715));
#79099=DIRECTION('ref_axis',(0.970273996606324,-0.0108363203371629,0.241766303837284));
#79100=DIRECTION('center_axis',(-0.0800592947092413,0.98649510820446,0.142891255223438));
#79101=DIRECTION('ref_axis',(0.93744851294225,0.0257926448400367,0.347167142821033));
#79102=DIRECTION('center_axis',(0.082260972070614,0.986495108556871,-0.141635211961453));
#79103=DIRECTION('ref_axis',(0.895616922134147,-0.0108363090296816,0.444694168157815));
#79104=DIRECTION('center_axis',(-0.1089049496773,0.986495108205681,0.122340154577497));
#79105=DIRECTION('ref_axis',(0.840900814631357,0.0257926460076625,0.540574286628807));
#79106=DIRECTION('center_axis',(0.110785147588489,0.986495108531122,-0.120640175389326));
#79107=DIRECTION('ref_axis',(0.779081793886847,-0.0108363188476222,0.626828630989272));
#79108=DIRECTION('center_axis',(-0.1326583321652,0.986495108139982,0.0960685615747012));
#79109=DIRECTION('ref_axis',(0.705033525947712,0.025792649733389,0.70870478092748));
#79110=DIRECTION('center_axis',(0.1341291247422,0.986495108557981,-0.0940041418612458));
#79111=DIRECTION('ref_axis',(0.626117669612743,-0.0108363207540363,0.779653280600565));
#79112=DIRECTION('center_axis',(-0.150208754328115,0.986495108142209,0.0653049135570062));
#79113=DIRECTION('ref_axis',(0.536199657697366,0.0257926484359865,0.843697022853515));
#79114=DIRECTION('center_axis',(0.151201369427729,0.986495108577346,-0.0629725863860636));
#79115=DIRECTION('ref_axis',(0.443876975459743,-0.0108363136168601,0.896022212316139));
#79116=DIRECTION('center_axis',(-0.160735582317945,0.986495108181445,0.0314876818929413));
#79117=DIRECTION('ref_axis',(0.342293688451243,0.0257926455307577,0.939238931413604));
#79118=DIRECTION('center_axis',(0.161203610189716,0.986495108559943,-0.0289964971868899));
#79119=DIRECTION('ref_axis',(0.240881089900806,-0.0108363139760407,0.970494139512245));
#79120=DIRECTION('center_axis',(-0.16374658310287,0.986495110327121,-0.00380181835653959));
#79121=DIRECTION('ref_axis',(0.132382437034705,0.0257925790892707,0.990863074914327));
#79122=DIRECTION('center_axis',(0.163668141680259,0.986495109676435,0.00633545447533204));
#79123=DIRECTION('ref_axis',(0.0266218532422533,-0.0108363296107072,0.999586840094704));
#79124=DIRECTION('center_axis',(-0.154431767361342,0.987363722573609,0.0355486789520771));
#79125=DIRECTION('ref_axis',(0.139174517129888,-0.0138817019862933,0.990170567191141));
#79126=DIRECTION('',(-0.727678230552677,0.,-0.68591864880591));
#79127=DIRECTION('center_axis',(8.16091499892112E-15,-1.,5.88200858810152E-14));
#79128=DIRECTION('ref_axis',(1.05765828811544E-31,-5.88200858810152E-14,
-1.));
#79129=DIRECTION('center_axis',(-0.154431767361249,-0.987363722573576,0.0355486789533851));
#79130=DIRECTION('ref_axis',(0.0663140400757799,0.0255405502863858,0.99747186846542));
#79131=DIRECTION('',(-0.513452942861744,0.,0.858117751515848));
#79132=DIRECTION('center_axis',(-0.1431793235287,0.987363722550876,0.0679158354460898));
#79133=DIRECTION('ref_axis',(0.348778095876434,-0.0138817019407607,0.937102522773275));
#79134=DIRECTION('',(-0.858117752273735,0.,-0.513452941595112));
#79135=DIRECTION('center_axis',(1.54610228332736E-14,-1.,4.17679121291167E-14));
#79136=DIRECTION('ref_axis',(2.92220659082831E-31,-4.17679121291167E-14,
-1.));
#79137=DIRECTION('center_axis',(-0.143179323527856,-0.9873637225508,0.0679158354489722));
#79138=DIRECTION('ref_axis',(0.279190622005061,0.0255405499579519,0.959895971911682));
#79139=DIRECTION('',(-0.316978747916834,0.,0.948432640396289));
#79140=DIRECTION('center_axis',(-0.125231975596325,0.987363722629922,0.0971073196140432));
#79141=DIRECTION('ref_axis',(0.542073198201638,-0.0138816980343954,0.840216606745623));
#79142=DIRECTION('',(-0.948432641260561,0.,-0.316978745330844));
#79143=DIRECTION('center_axis',(-8.02613972714816E-15,-1.,-1.24892462308838E-14));
#79144=DIRECTION('ref_axis',(-6.1223084794885E-33,1.24892462308838E-14,
-1.));
#79145=DIRECTION('center_axis',(-0.125231975595508,-0.987363722629879,0.0971073196155321));
#79146=DIRECTION('ref_axis',(0.479012558830294,0.0255405459996456,0.877436407378275));
#79147=DIRECTION('',(-0.105682979626772,0.,0.994399873198507));
#79148=DIRECTION('center_axis',(-0.101428915968318,0.987363722535096,0.121758180124088));
#79149=DIRECTION('ref_axis',(0.710021563218345,-0.0138817014069173,0.704043093944559));
#79150=DIRECTION('',(-0.994399873500629,0.,-0.10568297678403));
#79151=DIRECTION('center_axis',(1.05233118009756E-14,-1.,1.04718718035991E-14));
#79152=DIRECTION('ref_axis',(1.,1.05233118009756E-14,7.09245862821757E-33));
#79153=DIRECTION('center_axis',(-0.1014289159663,-0.987363722535019,0.121758180126395));
#79154=DIRECTION('ref_axis',(0.656436402981568,0.0255405495051092,0.753948890291376));
#79155=DIRECTION('',(0.110554410161169,0.,0.993870073195645));
#79156=DIRECTION('center_axis',(-0.072883153345059,0.987363722527268,0.140715761006283));
#79157=DIRECTION('ref_axis',(0.844770107743317,-0.01388170288603,0.53494930917642));
#79158=DIRECTION('',(-0.993870073195645,0.,0.110554410161163));
#79159=DIRECTION('center_axis',(8.76989783374246E-14,-1.,5.57539098784638E-14));
#79160=DIRECTION('ref_axis',(1.,8.76989783374246E-14,1.1265317878891E-30));
#79161=DIRECTION('center_axis',(-0.0728831533423562,-0.987363722527182,
0.140715761008282));
#79162=DIRECTION('ref_axis',(0.803166008716124,0.025540551261839,0.595207562690741));
#79163=DIRECTION('',(0.321622397477402,0.,0.946868012682279));
#79164=DIRECTION('center_axis',(-0.0409294572073719,0.98736372258034,0.153093627773999));
#79165=DIRECTION('ref_axis',(0.940018140150174,-0.013881702361494,0.340841890805919));
#79166=DIRECTION('',(-0.946868013557757,0.,0.321622394899963));
#79167=DIRECTION('center_axis',(-6.97386197287161E-14,-1.,-2.54269475096828E-14));
#79168=DIRECTION('ref_axis',(1.,-6.9738619728716E-14,-6.95679877401685E-32));
#79169=DIRECTION('center_axis',(-0.040929457207014,-0.987363722580331,0.153093627774153));
#79170=DIRECTION('ref_axis',(0.912340465561708,0.0255405505164363,0.408634990153761));
#79171=DIRECTION('',(0.517651677844017,0.,0.855591456493854));
#79172=DIRECTION('center_axis',(-0.00706194783320453,0.987363722614641,
0.158313006911495));
#79173=DIRECTION('ref_axis',(0.991311969812551,-0.0138816990973224,0.130797083058193));
#79174=DIRECTION('',(-0.855591457767102,0.,0.517651675739552));
#79175=DIRECTION('center_axis',(0.,-1.,0.));
#79176=DIRECTION('ref_axis',(0.,0.,-1.));
#79177=DIRECTION('center_axis',(-0.00706194783100147,-0.987363722614584,
0.158313006911947));
#79178=DIRECTION('ref_axis',(0.97885489623469,0.0255405473561743,0.202955099857384));
#79179=DIRECTION('',(0.689476142154167,0.,0.724308393849061));
#79180=DIRECTION('center_axis',(0.027135771312802,0.987363722645229,0.156129846984537));
#79181=DIRECTION('ref_axis',(0.996253153475163,-0.0138816971664084,-0.0853636496090367));
#79182=DIRECTION('',(-0.724308395215675,0.,0.689476140718513));
#79183=DIRECTION('center_axis',(1.47939110561966E-14,-1.,-1.24112276742186E-15));
#79184=DIRECTION('ref_axis',(1.,1.47939110561966E-14,-1.12478059837392E-32));
#79185=DIRECTION('center_axis',(0.0271357713158418,-0.987363722645153,0.156129846984491));
#79186=DIRECTION('ref_axis',(0.999599159917687,0.0255405449786543,-0.0122147474000547));
#79187=DIRECTION('',(0.829061466833223,0.,0.559157477113867));
#79188=DIRECTION('center_axis',(0.0600646555848615,0.98736372261194,0.146646228793531));
#79189=DIRECTION('ref_axis',(0.954610646786095,-0.0138816987062048,-0.297532874626762));
#79190=DIRECTION('',(-0.559157478446539,0.,0.829061465934407));
#79191=DIRECTION('center_axis',(4.25436987427772E-14,-1.,-1.31770787232342E-14));
#79192=DIRECTION('ref_axis',(1.,4.25436987427772E-14,-1.95686662459851E-31));
#79193=DIRECTION('center_axis',(0.0600646555883885,-0.987363722611848,0.146646228792703));
#79194=DIRECTION('ref_axis',(0.973603277803162,0.0255405469455389,-0.226813442971669));
#79195=DIRECTION('',(0.929880799447459,0.,0.36786097757027));
#79196=DIRECTION('center_axis',(0.0901849880419648,0.987363722479871,0.130305592598951));
#79197=DIRECTION('ref_axis',(0.868331607406681,-0.0138817060745571,-0.495789791963276));
#79198=DIRECTION('',(-0.367860977570298,0.,0.929880799447448));
#79199=DIRECTION('center_axis',(1.2905456100855E-14,-1.,-7.33821453172643E-15));
#79200=DIRECTION('ref_axis',(1.,1.2905456100855E-14,7.8359382974112E-32));
#79201=DIRECTION('center_axis',(0.0901849880425129,-0.987363722479855,0.130305592598688));
#79202=DIRECTION('ref_axis',(0.902082787661463,0.0255405539856764,-0.430806597334615));
#79203=DIRECTION('',(0.987219939393379,0.,0.15936370748741));
#79204=DIRECTION('center_axis',(0.116088358724509,0.98736372258947,0.107872018071949));
#79205=DIRECTION('ref_axis',(0.741450347498087,-0.0138816993904279,-0.670864129773682));
#79206=DIRECTION('',(-0.159363707939627,0.,0.987219939320379));
#79207=DIRECTION('center_axis',(-6.615740706242E-14,-1.,5.96456564476805E-14));
#79208=DIRECTION('ref_axis',(1.,-6.615740706242E-14,3.94765483631823E-31));
#79209=DIRECTION('center_axis',(0.116088358724872,-0.987363722589458,0.107872018071664));
#79210=DIRECTION('ref_axis',(0.788381910992222,0.0255405475942004,-0.614655710824231));
#79211=DIRECTION('',(0.998397772228337,0.,-0.0565852313726192));
#79212=DIRECTION('center_axis',(0.136563571478651,0.987363722650077,0.0803944658516843));
#79213=DIRECTION('ref_axis',(0.579899693448114,-0.0138816977980671,-0.814569606605247));
#79214=DIRECTION('',(0.0565852313726899,0.,0.998397772228333));
#79215=DIRECTION('center_axis',(-8.63143843731526E-15,-1.,1.20788435100477E-14));
#79216=DIRECTION('ref_axis',(5.52127733821679E-32,-1.20788435100477E-14,
-1.));
#79217=DIRECTION('center_axis',(0.136563571478661,-0.987363722650076,0.0803944658516745));
#79218=DIRECTION('ref_axis',(0.637817169827513,0.0255405456164728,-0.769764209614109));
#79219=DIRECTION('',(0.962891634602509,0.,-0.269888310255389));
#79220=DIRECTION('center_axis',(0.150653224778143,0.987363722643224,0.0491577569876829));
#79221=DIRECTION('ref_axis',(0.391233574762388,-0.0138816977976142,-0.920186713903705));
#79222=DIRECTION('',(0.269888310255455,0.,0.96289163460249));
#79223=DIRECTION('center_axis',(-5.83304589634749E-15,-1.,1.36519509804903E-14));
#79224=DIRECTION('ref_axis',(-3.18463081696841E-32,-1.36519509804903E-14,
-1.));
#79225=DIRECTION('center_axis',(0.150653224778077,-0.987363722643228,0.0491577569878172));
#79226=DIRECTION('ref_axis',(0.457428808928521,0.0255405456747179,-0.888879387368653));
#79227=DIRECTION('',(0.882361755339619,0.,-0.470571708365458));
#79228=DIRECTION('center_axis',(0.157698501629331,0.987363722576351,0.0156224813661074));
#79229=DIRECTION('ref_axis',(0.184273806832079,-0.0138817022434584,-0.982776913881496));
#79230=DIRECTION('',(0.470571708365521,0.,0.882361755339586));
#79231=DIRECTION('center_axis',(-1.10476264533498E-14,-1.,5.8346833597847E-14));
#79232=DIRECTION('ref_axis',(-2.5417154544527E-32,-5.8346833597847E-14,
-1.));
#79233=DIRECTION('center_axis',(0.15769850162929,-0.987363722576355,0.015622481366281));
#79234=DIRECTION('ref_axis',(0.255651581918147,0.0255405499347531,-0.966431554209495));
#79235=DIRECTION('',(0.760573620677732,0.,-0.649251698133447));
#79236=DIRECTION('',(0.649251699553084,0.,0.760573619465882));
#79237=DIRECTION('',(0.603221906321608,0.,-0.797573402097716));
#79238=DIRECTION('center_axis',(0.14968299370784,0.987363722548993,-0.0520373018982967));
#79239=DIRECTION('ref_axis',(-0.245414938382434,-0.0138817019099837,-0.96931873311663));
#79240=DIRECTION('',(0.797573400714641,0.,0.603221908150295));
#79241=DIRECTION('center_axis',(1.08544839876594E-14,-1.,4.31946974113953E-14));
#79242=DIRECTION('ref_axis',(8.99397962473849E-34,-4.31946974113953E-14,
-1.));
#79243=DIRECTION('center_axis',(0.149682993707841,-0.987363722548993,-0.0520373018982921));
#79244=DIRECTION('ref_axis',(-0.173770985052446,0.025540549741825,-0.984454836481993));
#79245=DIRECTION('',(0.417664210217885,0.,-0.908601456912254));
#79246=DIRECTION('center_axis',(0.134997008782224,0.987363722631273,-0.08299811354222));
#79247=DIRECTION('ref_axis',(-0.448052147183188,-0.0138816974014571,-0.893899643070624));
#79248=DIRECTION('',(0.908601457413776,0.,0.417664209126856));
#79249=DIRECTION('center_axis',(-3.97725906070439E-14,-1.,-7.97028723859732E-14));
#79250=DIRECTION('ref_axis',(8.44798570949651E-31,7.97028723859732E-14,
-1.));
#79251=DIRECTION('center_axis',(0.134997008782151,-0.987363722631268,-0.0829981135423979));
#79252=DIRECTION('ref_axis',(-0.381337005043723,0.0255405451368106,-0.924083204662003));
#79253=DIRECTION('',(0.212576996304382,0.,-0.977144319249826));
#79254=DIRECTION('center_axis',(0.113998711847197,0.987363722595133,-0.110078031415265));
#79255=DIRECTION('ref_axis',(-0.629738937334439,-0.0138816988167137,-0.776682798343605));
#79256=DIRECTION('',(0.977144319379751,0.,0.212576995707162));
#79257=DIRECTION('center_axis',(-9.32941520012954E-15,-1.,-1.1548255390224E-14));
#79258=DIRECTION('ref_axis',(-1.54567726138217E-31,1.1548255390224E-14,
-1.));
#79259=DIRECTION('center_axis',(0.113998711845088,-0.987363722595039,-0.110078031418294));
#79260=DIRECTION('ref_axis',(-0.571072129830343,0.0255405469171674,-0.820502469828219));
#79261=DIRECTION('',(-0.00245007782715285,0.,-0.999996998554816));
#79262=DIRECTION('center_axis',(0.0876699563048406,0.987363722480806,-0.132010826413413));
#79263=DIRECTION('ref_axis',(-0.781979834526339,-0.0138817066334,-0.623149128712464));
#79264=DIRECTION('',(0.999996998554795,0.,-0.00245007783568496));
#79265=DIRECTION('center_axis',(3.47814965074125E-14,-1.,2.78181452331395E-14));
#79266=DIRECTION('ref_axis',(1.,3.47814965074125E-14,7.96189918324429E-31));
#79267=DIRECTION('center_axis',(0.0876699563044266,-0.98736372248079,-0.13201082641381));
#79268=DIRECTION('ref_axis',(-0.734104558096312,0.025540554789388,-0.678555950414753));
#79269=DIRECTION('',(-0.217362592525063,0.,-0.976090929868106));
#79270=DIRECTION('center_axis',(0.0572418589303205,0.987363722536242,-0.147770934238016));
#79271=DIRECTION('ref_axis',(-0.897656223127401,-0.0138817032674184,-0.440477699089346));
#79272=DIRECTION('',(0.9760909303422,0.,-0.217362590396092));
#79273=DIRECTION('center_axis',(-2.66322689534313E-14,-1.,-1.31271859147942E-14));
#79274=DIRECTION('ref_axis',(1.,-2.66322689534313E-14,3.23564926775337E-31));
#79275=DIRECTION('center_axis',(0.0572418589303068,-0.987363722536242,-0.147770934238022));
#79276=DIRECTION('ref_axis',(-0.86281107255647,0.0255405515494598,-0.504880910017901));
#79277=DIRECTION('',(-0.422111470626519,0.,-0.906543935154561));
#79278=DIRECTION('center_axis',(0.0241371946610542,0.987363722568252,-0.15662143911374));
#79279=DIRECTION('ref_axis',(-0.97135920429933,-0.0138817018667561,-0.237210022082234));
#79280=DIRECTION('',(0.906543934642298,0.,-0.422111471726677));
#79281=DIRECTION('center_axis',(-1.44157891168532E-14,-1.,-3.54756450935383E-15));
#79282=DIRECTION('ref_axis',(1.,-1.44157891168532E-14,-6.23813188579977E-32));
#79283=DIRECTION('center_axis',(0.0241371946612772,-0.987363722568257,-0.156621439113674));
#79284=DIRECTION('ref_axis',(-0.951173500802478,0.0255405500367738,-0.307598198426091));
#79285=DIRECTION('',(-0.607122889070729,0.,-0.79460795211627));
#79286=DIRECTION('center_axis',(-0.0100960958892223,0.987363722611222,-0.158148500211367));
#79287=DIRECTION('ref_axis',(-0.99964250877371,-0.0138816987180042,-0.0228506694279372));
#79288=DIRECTION('',(0.794607951056583,0.,-0.607122890457656));
#79289=DIRECTION('center_axis',(7.42068874433645E-14,-1.,1.82827944841588E-15));
#79290=DIRECTION('ref_axis',(-0.99969663250782,-7.42294062334711E-14,-0.0246301228686554));
#79291=DIRECTION('center_axis',(-0.0100960958892171,-0.987363722611223,
-0.158148500211366));
#79292=DIRECTION('ref_axis',(-0.995060113131406,0.0255405466605858,-0.0959325373957782));
#79293=DIRECTION('',(-0.763745915082458,0.,-0.645516984435622));
#79294=DIRECTION('center_axis',(-0.0438573087936048,0.987363722583665,-0.15228071378579));
#79295=DIRECTION('ref_axis',(-0.981183640694819,-0.0138816999014745,0.192577157629626));
#79296=DIRECTION('',(0.645516984435563,0.,-0.763745915082508));
#79297=DIRECTION('center_axis',(7.28649976714645E-14,-1.,-1.41667519678132E-14));
#79298=DIRECTION('ref_axis',(1.,7.28649976714645E-14,9.36660370336697E-32));
#79299=DIRECTION('center_axis',(-0.0438573087934124,-0.987363722583669,
-0.152280713785819));
#79300=DIRECTION('ref_axis',(-0.992418820392299,0.0255405479708334,0.120218822737984));
#79301=DIRECTION('',(-0.884657030427525,0.,-0.466242360275376));
#79302=DIRECTION('center_axis',(-0.0755677988336853,0.987363722655466,-0.139292451207418));
#79303=DIRECTION('ref_axis',(-0.916845716143399,-0.0138816972143508,0.399000289814364));
#79304=DIRECTION('',(0.466242360275311,0.,-0.884657030427559));
#79305=DIRECTION('center_axis',(1.36232043304539E-14,-1.,-5.89987236371338E-15));
#79306=DIRECTION('ref_axis',(1.,1.36232043304539E-14,-1.37390409739643E-31));
#79307=DIRECTION('center_axis',(-0.0755677988336818,-0.987363722655467,
-0.139292451207416));
#79308=DIRECTION('ref_axis',(-0.943373127031503,0.0255405454300251,0.330748883193792));
#79309=DIRECTION('',(-0.964202566256142,0.,-0.265166761161859));
#79310=DIRECTION('center_axis',(-0.103744835240006,0.987363722371026,-0.119791021811549));
#79311=DIRECTION('ref_axis',(-0.809637102056546,-0.013881708435082,0.586766615567383));
#79312=DIRECTION('',(0.265166763834479,0.,-0.964202565521141));
#79313=DIRECTION('',(-0.998663061429463,0.,-0.0516922599267325));
#79314=DIRECTION('center_axis',(-3.61092096369038E-14,-1.,2.60715685497971E-14));
#79315=DIRECTION('ref_axis',(1.,-3.61092096369038E-14,7.02924335103244E-31));
#79316=DIRECTION('center_axis',(-0.103744831159682,-0.987363722491922,-0.119791024348835));
#79317=DIRECTION('ref_axis',(-0.850216353240246,0.0255405521846307,0.525813496286432));
#79318=DIRECTION('',(0.0516922599267204,0.,-0.998663061429463));
#79319=DIRECTION('center_axis',(-0.127070861066288,0.9873637225882,-0.0946883075392291));
#79320=DIRECTION('ref_axis',(-0.664570762150803,-0.0138817002430436,0.747096379654368));
#79321=DIRECTION('center_axis',(1.97735865367437E-14,-1.,-2.21496282986849E-14));
#79322=DIRECTION('ref_axis',(-5.91610294980431E-32,2.21496282986849E-14,
-1.));
#79323=DIRECTION('center_axis',(-0.12707086106538,-0.987363722588226,-0.0946883075401802));
#79324=DIRECTION('ref_axis',(-0.717304409962752,0.0255405484483746,0.696291651416951));
#79325=DIRECTION('',(-0.986427181731827,0.,0.164199315286653));
#79326=DIRECTION('center_axis',(-0.144455203317022,0.987363722518218,-0.0651580669572451));
#79327=DIRECTION('ref_axis',(-0.488429827499476,-0.0138817019329595,0.872492751809593));
#79328=DIRECTION('',(-0.164199314821143,0.,-0.986427181809315));
#79329=DIRECTION('center_axis',(0.,-1.,0.));
#79330=DIRECTION('ref_axis',(0.,0.,-1.));
#79331=DIRECTION('center_axis',(-0.144455203317624,-0.987363722518189,-0.0651580669563533));
#79332=DIRECTION('ref_axis',(-0.550852108221544,0.0255405504288338,0.834211984540904));
#79333=DIRECTION('',(-0.928067064308992,0.,0.372413109523401));
#79334=DIRECTION('center_axis',(-0.155084978924344,0.987363722546342,-0.0325811097334957));
#79335=DIRECTION('ref_axis',(-0.289450459918619,-0.0138817012506714,0.95709233077237));
#79336=DIRECTION('',(-0.372413110516999,0.,-0.928067063910283));
#79337=DIRECTION('center_axis',(0.,-1.,0.));
#79338=DIRECTION('ref_axis',(0.,0.,-1.));
#79339=DIRECTION('center_axis',(-0.155084978924618,-0.987363722546322,-0.0325811097327927));
#79340=DIRECTION('ref_axis',(-0.358642575991151,0.0255405497773031,0.933125491562365));
#79341=DIRECTION('',(-0.826311561170158,0.,0.563213284534852));
#79342=DIRECTION('center_axis',(-0.158463154019127,0.987363722508337,0.00151930668065768));
#79343=DIRECTION('ref_axis',(-0.0769367093312951,-0.0138817032695296,0.996939336705904));
#79344=DIRECTION('',(-0.563213284534842,0.,-0.826311561170165));
#79345=DIRECTION('center_axis',(-2.33723120489955E-15,-1.,2.95996302335738E-14));
#79346=DIRECTION('ref_axis',(1.47644993132475E-32,-2.95996302335738E-14,
-1.));
#79347=DIRECTION('center_axis',(-0.158463154019238,-0.987363722508318,0.00151930668137857));
#79348=DIRECTION('ref_axis',(-0.149663313270426,0.0255405516534839,0.988407088644226));
#79349=DIRECTION('',(-0.685918647283643,0.,0.727678231987585));
#79350=DIRECTION('',(0.761098361889465,0.,-0.648636480263925));
#79351=DIRECTION('center_axis',(0.152615509638427,-0.987363721954313,0.0426777083069028));
#79352=DIRECTION('ref_axis',(-0.189172281343434,0.0131994979521353,0.981855193613158));
#79353=DIRECTION('center_axis',(-0.15456220255018,-0.987363721855482,-0.0349772255407453));
#79354=DIRECTION('ref_axis',(-0.187954824318923,-0.0053704878227672,0.982162991501812));
#79355=DIRECTION('',(0.469858074213424,0.,0.882741972547161));
#79356=DIRECTION('center_axis',(-2.77370063757617E-15,-1.,1.45844706016369E-14));
#79357=DIRECTION('ref_axis',(-3.54850712574642E-32,-1.45844706016369E-14,
-1.));
#79358=DIRECTION('center_axis',(0.158065641712032,0.987363722473557,0.0113195606506649));
#79359=DIRECTION('ref_axis',(-0.111146690329742,0.0064001555740922,0.993783402576926));
#79360=DIRECTION('',(0.882741973773695,0.,-0.469858071909084));
#79361=DIRECTION('center_axis',(0.139872998404444,-0.987363721993328,0.074487749387615));
#79362=DIRECTION('ref_axis',(-0.395819382646154,0.0131994966388906,0.918233515839025));
#79363=DIRECTION('center_axis',(-0.143429555557831,-0.987363721894278,-0.0673857795054785));
#79364=DIRECTION('ref_axis',(-0.394696555489278,-0.00537048497618321,0.918795835306201));
#79365=DIRECTION('',(0.26910962254562,0.,0.963109552986239));
#79366=DIRECTION('center_axis',(1.75322493495858E-14,-1.,-4.09416903538788E-14));
#79367=DIRECTION('ref_axis',(-3.88570892755786E-32,4.09416903538788E-14,
-1.));
#79368=DIRECTION('center_axis',(0.151936786191382,0.987363722382829,0.0450343504911405));
#79369=DIRECTION('ref_axis',(-0.322182197946835,0.00640016177914806,0.946656045908622));
#79370=DIRECTION('',(0.963109553688447,0.,-0.269109620032506));
#79371=DIRECTION('center_axis',(0.120590181104626,-0.987363721999251,0.102814827242669));
#79372=DIRECTION('ref_axis',(-0.583958407758862,0.0131994968264676,0.811676260150106));
#79373=DIRECTION('center_axis',(-0.125590297867976,-0.987363721894042,-0.0966434569382695));
#79374=DIRECTION('ref_axis',(-0.582982714666456,-0.00537049109331535,0.812466806845391));
#79375=DIRECTION('',(0.055777904388787,0.,0.998443200879247));
#79376=DIRECTION('center_axis',(3.45648110535867E-14,-1.,-4.82874413478829E-14));
#79377=DIRECTION('ref_axis',(-1.4878768112405E-31,4.82874413478829E-14,
-1.));
#79378=DIRECTION('center_axis',(0.138703532219836,0.987363722447253,0.076643393354187));
#79379=DIRECTION('ref_axis',(-0.518152824713272,0.00640015801778179,0.855264104367186));
#79380=DIRECTION('',(0.998443201024793,0.,-0.0557779017834631));
#79381=DIRECTION('center_axis',(0.095668705435196,-0.987363722100653,0.126334393891365));
#79382=DIRECTION('ref_axis',(-0.744792187180435,0.0131994908163985,0.667165924907119));
#79383=DIRECTION('center_axis',(-0.10187858278201,-0.987363721875608,-0.121382186066478));
#79384=DIRECTION('ref_axis',(-0.74400924970769,-0.00537048758462738,0.66814773382277));
#79385=DIRECTION('',(-0.160161927182448,0.,0.987090754227393));
#79386=DIRECTION('center_axis',(-4.41370775386657E-14,-1.,3.9728095186524E-14));
#79387=DIRECTION('ref_axis',(1.,-4.41370775386657E-14,6.86387583734043E-31));
#79388=DIRECTION('center_axis',(0.118984656681779,0.987363722441671,0.104668672870372));
#79389=DIRECTION('ref_axis',(-0.689895198735468,0.00640015752131604,0.723880965867629));
#79390=DIRECTION('',(0.987090754263963,0.,0.160161926957068));
#79391=DIRECTION('center_axis',(0.0662738593681364,-0.987363721996382,0.143946712535936));
#79392=DIRECTION('ref_axis',(-0.870800313020862,0.0131994960636845,0.491459650578187));
#79393=DIRECTION('center_axis',(-0.0734031336639462,-0.987363721877004,
-0.140445223092502));
#79394=DIRECTION('ref_axis',(-0.870246739706229,-0.00537049031533164,0.492586814545874));
#79395=DIRECTION('',(-0.368612762585142,0.,0.929583041615621));
#79396=DIRECTION('center_axis',(-9.03797007523297E-14,-1.,5.129443795653E-14));
#79397=DIRECTION('ref_axis',(1.,-9.03797007523297E-14,3.11692668887943E-32));
#79398=DIRECTION('center_axis',(0.0937021887534254,0.987363722499088,0.127799762580223));
#79399=DIRECTION('ref_axis',(-0.829378843888429,0.00640015560929818,0.558649954191773));
#79400=DIRECTION('',(0.929583040653769,0.,0.368612765010781));
#79401=DIRECTION('center_axis',(0.0337801242911014,-0.987363721967948,0.154828239492928));
#79402=DIRECTION('ref_axis',(-0.956090783052351,0.0131994970506592,0.292773270364546));
#79403=DIRECTION('center_axis',(-0.0414954358906202,-0.987363721863099,
-0.152941196375913));
#79404=DIRECTION('ref_axis',(-0.955792459128537,-0.00537049216965758,0.293993083059585));
#79405=DIRECTION('',(-0.559827676809204,0.,0.828609058771632));
#79406=DIRECTION('center_axis',(-5.67391208751526E-14,-1.,1.7523564833116E-14));
#79407=DIRECTION('ref_axis',(1.,-5.67391208751526E-14,2.39428158731835E-31));
#79408=DIRECTION('center_axis',(0.0640383186167767,0.987363722391337,0.144955073916917));
#79409=DIRECTION('ref_axis',(-0.930081653875991,0.00640016214797504,0.367297093709957));
#79410=DIRECTION('',(0.828609057310836,0.,0.559827678971349));
#79411=DIRECTION('center_axis',(-0.000293130042014416,-0.987363722005209,
0.158470169252131));
#79412=DIRECTION('ref_axis',(-0.996675510595413,0.0131994961838119,0.0803971385054558));
#79413=DIRECTION('center_axis',(-0.00764746068325912,-0.987363721888245,
-0.158285808094381));
#79414=DIRECTION('ref_axis',(-0.996646385061109,-0.00537049081886417,0.0816525625622804));
#79415=DIRECTION('',(-0.72486567039439,0.,0.688890237907094));
#79416=DIRECTION('center_axis',(7.39745501415128E-14,-1.,-6.14579978269866E-15));
#79417=DIRECTION('ref_axis',(1.,7.39745501415128E-14,1.07588057771275E-31));
#79418=DIRECTION('center_axis',(0.0313800724017027,0.987363722539182,0.155332451437662));
#79419=DIRECTION('ref_axis',(-0.987294879630409,0.00640015209656239,0.1587698293402));
#79420=DIRECTION('',(0.688890236015648,0.,0.724865672191962));
#79421=DIRECTION('center_axis',(-0.0343526804446576,-0.98736372198438,0.154702210247363));
#79422=DIRECTION('ref_axis',(-0.990656799336339,0.0131994978913179,-0.13573827457316));
#79423=DIRECTION('center_axis',(0.0265580987606778,-0.987363721867808,-0.156229152623856));
#79424=DIRECTION('ref_axis',(-0.990898233870037,-0.00537048704539685,-0.134505940322863));
#79425=DIRECTION('',(-0.856009751718059,0.,0.516959674407576));
#79426=DIRECTION('center_axis',(-5.8852985332957E-14,-1.,-7.9201817788065E-15));
#79427=DIRECTION('ref_axis',(1.,-5.8852985332957E-14,9.47619536544115E-32));
#79428=DIRECTION('center_axis',(-0.00274545651990735,0.987363722462837,
0.158446653586713));
#79429=DIRECTION('ref_axis',(-0.998343294030884,0.00640015748189069,-0.0571813365336253));
#79430=DIRECTION('',(0.516959673446092,0.,0.856009752298717));
#79431=DIRECTION('center_axis',(-0.0668059398504362,-0.987363721922213,
0.143700546389407));
#79432=DIRECTION('ref_axis',(-0.938316076633506,0.0131995016487155,-0.345526718919579));
#79433=DIRECTION('center_axis',(0.0595218347697124,-0.987363721868324,-0.146867395714565));
#79434=DIRECTION('ref_axis',(-0.9388167823789,-0.00537048681305594,-0.344375096363137));
#79435=DIRECTION('',(-0.947127767923488,0.,0.320856652149012));
#79436=DIRECTION('center_axis',(-2.7887215127273E-14,-1.,-1.01933322424768E-14));
#79437=DIRECTION('ref_axis',(1.,-2.7887215127273E-14,-1.63004429102285E-31));
#79438=DIRECTION('center_axis',(-0.0367426203518148,0.987363722519173,0.154152065515721));
#79439=DIRECTION('ref_axis',(-0.962710285131315,0.00640015325057946,-0.270458767542763));
#79440=DIRECTION('',(0.320856647098721,0.,0.947127769634365));
#79441=DIRECTION('center_axis',(-0.0961354192454943,-0.987363721975525,
0.125979608243283));
#79442=DIRECTION('ref_axis',(-0.842100737714532,0.0131994961709445,-0.539158715817035));
#79443=DIRECTION('center_axis',(0.0897023972641109,-0.987363721874223,-0.130638281723827));
#79444=DIRECTION('ref_axis',(-0.842837302056352,-0.00537048843902798,-0.538141654321886));
#79445=DIRECTION('',(-0.993959142840391,0.,0.109750728307355));
#79446=DIRECTION('center_axis',(5.00879248534494E-14,-1.,3.18998894380968E-14));
#79447=DIRECTION('ref_axis',(1.,5.00879248534494E-14,-3.90471029974449E-31));
#79448=DIRECTION('center_axis',(-0.069021730874996,0.987363722442924,0.142649501473623));
#79449=DIRECTION('ref_axis',(-0.88206201520754,0.0064001582682407,-0.471089842070655));
#79450=DIRECTION('',(0.109750725713721,0.,0.993959143126774));
#79451=DIRECTION('center_axis',(-0.120969721135708,-0.987363721902305,0.102367999099214));
#79452=DIRECTION('ref_axis',(-0.706509702519059,0.0131994996103268,-0.707580252308152));
#79453=DIRECTION('center_axis',(0.115688572607768,-0.98736372188139,-0.108300668883003));
#79454=DIRECTION('ref_axis',(-0.707447686309035,-0.00537048650344094,-0.70674530703126));
#79455=DIRECTION('',(-0.994314092728476,0.,-0.10648701799538));
#79456=DIRECTION('center_axis',(6.30890455641618E-14,-1.,6.28822664835682E-14));
#79457=DIRECTION('ref_axis',(1.,6.30890455641618E-14,-1.84569166322532E-31));
#79458=DIRECTION('center_axis',(-0.0980734667158721,0.987363722423218,0.124476804139958));
#79459=DIRECTION('ref_axis',(-0.760169502183937,0.00640015973960987,-0.649693286024054));
#79460=DIRECTION('',(-0.106487020589929,0.,0.99431409245061));
#79461=DIRECTION('center_axis',(-0.140147609432002,-0.987363721938444,0.0739697787637499));
#79462=DIRECTION('ref_axis',(-0.537883061423971,0.0131994988325246,-0.842916120064));
#79463=DIRECTION('center_axis',(0.136265278239864,-0.987363721884388,-0.0808990398757652));
#79464=DIRECTION('ref_axis',(-0.538978603059603,-0.00537048203791794,-0.842302334893237));
#79465=DIRECTION('',(-0.948176020641203,0.,-0.317745548955471));
#79466=DIRECTION('center_axis',(4.00801918488179E-14,-1.,6.24786615949557E-14));
#79467=DIRECTION('ref_axis',(1.14695319878951E-30,-6.24786615949557E-14,
-1.));
#79468=DIRECTION('center_axis',(-0.122539399999212,0.987363722490082,0.100483704939462));
#79469=DIRECTION('ref_axis',(-0.602732310836473,0.00640015416421709,-0.797917789938537));
#79470=DIRECTION('',(-0.317745554014208,0.,0.948176018945957));
#79471=DIRECTION('center_axis',(-0.152772350424458,-0.987363722024416,0.0421128172398611));
#79472=DIRECTION('ref_axis',(-0.344105606166508,0.0131994945560806,-0.93883816770956));
#79473=DIRECTION('center_axis',(0.150470376064837,-0.987363721904127,-0.0497146517088959));
#79474=DIRECTION('ref_axis',(-0.345307478360847,-0.00537048903212129,-0.938474242180162));
#79475=DIRECTION('',(-0.857702290213478,0.,-0.51414665355573));
#79476=DIRECTION('center_axis',(-2.05696590877686E-14,-1.,-5.57072013831238E-14));
#79477=DIRECTION('ref_axis',(4.64417736689475E-31,5.57072013831238E-14,
-1.));
#79478=DIRECTION('center_axis',(-0.141275521246512,0.987363722413862,0.0717921079058763));
#79479=DIRECTION('ref_axis',(-0.41711202824178,0.00640015907852063,-0.908832544454586));
#79480=DIRECTION('',(-0.514146654526059,0.,0.857702289631817));
#79481=DIRECTION('center_axis',(-0.158253628125781,-0.9873637220816,0.00828670635390313));
#79482=DIRECTION('ref_axis',(-0.134238153215872,0.0131994915295978,-0.990861186869559));
#79483=DIRECTION('center_axis',(0.15763964250658,-0.987363721893091,-0.0162056718410967));
#79484=DIRECTION('ref_axis',(-0.135490161169236,-0.00537048504490039,-0.990764136470794));
#79485=DIRECTION('',(-0.727123357294462,0.,-0.686506826824636));
#79486=DIRECTION('center_axis',(2.02833757196093E-15,-1.,1.47066666659893E-14));
#79487=DIRECTION('ref_axis',(3.92305557744363E-32,-1.47066666659893E-14,
-1.));
#79488=DIRECTION('center_axis',(-0.153405759751366,0.987363722449018,0.0397435839693078));
#79489=DIRECTION('ref_axis',(-0.211988047664614,0.00640015578210116,-0.977251301177599));
#79490=DIRECTION('',(-0.686506828721979,0.,0.727123355503103));
#79491=DIRECTION('center_axis',(-0.156335142838038,-0.987363722080833,-0.0259268862861391));
#79492=DIRECTION('ref_axis',(0.081906124669614,0.0131994936921692,-0.996552637901218));
#79493=DIRECTION('center_axis',(0.157437855226706,-0.987363721871608,0.0180610761988493));
#79494=DIRECTION('ref_axis',(0.0806625276050987,-0.00537048997581514,-0.996727000977588));
#79495=DIRECTION('',(-0.562544940564676,0.,-0.826766708234605));
#79496=DIRECTION('center_axis',(-1.18058243820127E-15,-1.,1.47988655758512E-14));
#79497=DIRECTION('ref_axis',(4.8499339749902E-33,-1.47988655758512E-14,
-1.));
#79498=DIRECTION('center_axis',(-0.158362913987084,0.987363722452981,0.00583669917957237));
#79499=DIRECTION('ref_axis',(0.00304825895565919,0.00640015786115479,-0.999974872732656));
#79500=DIRECTION('',(-0.826766709702496,0.,0.562544938407333));
#79501=DIRECTION('center_axis',(-0.14710660094675,-0.987363722108276,-0.0589281615391628));
#79502=DIRECTION('ref_axis',(0.294220564215013,0.0131994904617581,-0.95564639540185));
#79503=DIRECTION('center_axis',(0.149874448064302,-0.987363721871317,0.0514833036026376));
#79504=DIRECTION('ref_axis',(0.293043523486218,-0.00537049048421785,-0.956084018888895));
#79505=DIRECTION('',(-0.371662549274472,0.,-0.928367895538617));
#79506=DIRECTION('center_axis',(-1.73371989163566E-14,-1.,5.67963440396674E-14));
#79507=DIRECTION('ref_axis',(-2.26462988917793E-31,-5.67963440396674E-14,
-1.));
#79508=DIRECTION('center_axis',(-0.155915195724226,0.987363722398576,-0.0283431020444865));
#79509=DIRECTION('ref_axis',(0.217942029486368,0.00640016067289282,-0.97594073064235));
#79510=DIRECTION('',(-0.928367895516495,0.,0.371662549329729));
#79511=DIRECTION('center_axis',(-0.130999513940044,-0.987363721968695,-0.0891740314643088));
#79512=DIRECTION('ref_axis',(0.492777578093553,0.0131994981102028,-0.870055188926479));
#79513=DIRECTION('center_axis',(0.135303080594625,-0.98736372187151,0.0824982249120781));
#79514=DIRECTION('ref_axis',(0.491722131566428,-0.00537048598229784,-0.870735610393926));
#79515=DIRECTION('',(-0.163401630169058,0.,-0.986559631881466));
#79516=DIRECTION('center_axis',(-2.91413998726486E-14,-1.,5.17414917161749E-14));
#79517=DIRECTION('ref_axis',(3.23235934945798E-31,-5.17414917161749E-14,
-1.));
#79518=DIRECTION('center_axis',(-0.146177052628152,0.987363722526871,-0.061197620238264));
#79519=DIRECTION('ref_axis',(0.422645075236517,0.00640015395770225,-0.90627268435479));
#79520=DIRECTION('',(-0.986559631844411,0.,0.163401630392784));
#79521=DIRECTION('center_axis',(-0.108767037567511,-0.987363721988378,-0.115250214924069));
#79522=DIRECTION('ref_axis',(0.668292860223129,0.0131994973818557,-0.743781168250216));
#79523=DIRECTION('center_axis',(0.114405086728576,-0.987363721852231,0.109655628677866));
#79524=DIRECTION('ref_axis',(0.667408358630309,-0.00537049099330845,-0.744672572784098));
#79525=DIRECTION('',(0.0524997650266615,0.,-0.998620936427905));
#79526=DIRECTION('center_axis',(6.92702175257193E-14,-1.,-7.74677135725862E-14));
#79527=DIRECTION('ref_axis',(1.15000252023255E-30,7.74677135725862E-14,
-1.));
#79528=DIRECTION('center_axis',(-0.129603834006118,0.98736372253409,-0.0911906005821871));
#79529=DIRECTION('ref_axis',(0.60758570602415,0.00640015223266166,-0.794228334854992));
#79530=DIRECTION('',(-0.998620936282989,0.,-0.0524997677831598));
#79531=DIRECTION('center_axis',(-0.0814487376935129,-0.987363722005638,
-0.135937425293063));
#79532=DIRECTION('ref_axis',(0.812559508457631,0.0131994947613375,-0.582728769285624));
#79533=DIRECTION('center_axis',(0.088157642749355,-0.987363721858716,0.131685651390657));
#79534=DIRECTION('ref_axis',(0.811887313110997,-0.0053704882952763,-0.583789472896588));
#79535=DIRECTION('',(0.265946332280708,0.,-0.963987836202532));
#79536=DIRECTION('center_axis',(1.20434266953032E-13,-1.,-8.68078747800019E-14));
#79537=DIRECTION('ref_axis',(1.,1.20434266953032E-13,-1.16030839842935E-30));
#79538=DIRECTION('center_axis',(-0.106970488036622,0.987363722454154,-0.116919606014916));
#79539=DIRECTION('ref_axis',(0.764116305563639,0.00640015641498283,-0.645046749910144));
#79540=DIRECTION('',(-0.96398783550857,0.,-0.265946334796144));
#79541=DIRECTION('center_axis',(-0.0503219807087614,-0.987363721983654,
-0.150268355844243));
#79542=DIRECTION('ref_axis',(0.918831778987382,0.0131994974814984,-0.394428618623343));
#79543=DIRECTION('center_axis',(0.0577880427271561,-0.987363721860299,0.147558201642413));
#79544=DIRECTION('ref_axis',(0.918403318689976,-0.00537048931959254,-0.395609026772275));
#79545=DIRECTION('',(0.466957545975081,0.,-0.884279735296999));
#79546=DIRECTION('center_axis',(-2.72559415313569E-14,-1.,1.17777094957016E-14));
#79547=DIRECTION('ref_axis',(1.,-2.72559415313569E-14,2.44775647909051E-31));
#79548=DIRECTION('center_axis',(-0.0793353163545417,0.987363722508187,-0.137181584236734));
#79549=DIRECTION('ref_axis',(0.884917674707086,0.00640015430844893,-0.465703496890276));
#79550=DIRECTION('',(-0.884279734078536,-3.74026243169963E-15,-0.466957548282489));
#79551=DIRECTION('center_axis',(-0.0168422275713211,-0.987363722000351,
-0.15757290327988));
#79552=DIRECTION('ref_axis',(0.982140496261105,0.013199496140424,-0.187685425394804));
#79553=DIRECTION('center_axis',(0.0247163358735517,-0.987363721874109,0.156531094252524));
#79554=DIRECTION('ref_axis',(0.981975806292579,-0.00537049216555821,-0.188930340787122));
#79555=DIRECTION('',(0.646134340612186,0.,-0.763223698453904));
#79556=DIRECTION('center_axis',(-1.45752860926422E-14,-1.,2.82156572357862E-15));
#79557=DIRECTION('ref_axis',(1.,-1.45752860926422E-14,1.01827328463709E-32));
#79558=DIRECTION('center_axis',(-0.0479905205829132,0.987363722406498,-0.151029101863734));
#79559=DIRECTION('ref_axis',(0.964341276427462,0.00640015954765453,-0.264584467677182));
#79560=DIRECTION('',(-0.763223696767415,0.,-0.646134342604292));
#79561=DIRECTION('',(0.795098614022376,0.,-0.606480167837084));
#79562=DIRECTION('',(-0.606480167148637,0.,-0.795098614547505));
#79563=DIRECTION('center_axis',(0.050877555165117,-0.987363721972948,-0.150081161083423));
#79564=DIRECTION('ref_axis',(0.970173637559078,0.0131994982843853,0.24205141237024));
#79565=DIRECTION('center_axis',(-0.0432937565932917,-0.987363721878708,
0.152441895021893));
#79566=DIRECTION('ref_axis',(0.970546895646585,-0.00537048691830518,0.240852405470729));
#79567=DIRECTION('',(0.906884959783822,0.,-0.421378297635148));
#79568=DIRECTION('center_axis',(1.4412916073023E-14,-1.,3.55922008307402E-15));
#79569=DIRECTION('ref_axis',(1.,1.4412916073023E-14,-5.23604782595645E-32));
#79570=DIRECTION('center_axis',(0.0198604640484954,0.987363722513242,-0.157220995520868));
#79571=DIRECTION('ref_axis',(0.98630857283147,0.00640015256345255,0.164786034621606));
#79572=DIRECTION('',(-0.421378297633106,0.,-0.906884959784771));
#79573=DIRECTION('center_axis',(0.0819510773744515,-0.987363722025524,-0.135635177387983));
#79574=DIRECTION('ref_axis',(0.895457618754654,0.0131994961189737,0.444951038111443));
#79575=DIRECTION('center_axis',(-0.0750520708927661,-0.987363721878045,
0.139571011939592));
#79576=DIRECTION('ref_axis',(0.896079901408113,-0.00537048362115263,0.443860302570642));
#79577=DIRECTION('',(0.976266370926292,0.,-0.21657325088387));
#79578=DIRECTION('center_axis',(-5.32432919859296E-14,-1.,-2.62974336310652E-14));
#79579=DIRECTION('ref_axis',(1.,-5.32432919859296E-14,3.34469867477409E-31));
#79580=DIRECTION('center_axis',(0.0531939969984103,0.987363722423736,-0.14927584642157));
#79581=DIRECTION('ref_axis',(0.927825100680265,0.00640016009637148,0.37296061521077));
#79582=DIRECTION('',(-0.216573248336411,0.,-0.976266371491416));
#79583=DIRECTION('center_axis',(0.109192663323288,-0.987363721947468,-0.114847041139118));
#79584=DIRECTION('ref_axis',(0.778870996263127,0.013199499495899,0.627045249079476));
#79585=DIRECTION('center_axis',(-0.103301042454407,-0.987363721854847,0.120173938076346));
#79586=DIRECTION('ref_axis',(0.779713205798433,-0.00537049049308058,0.626113787210754));
#79587=DIRECTION('',(0.999998652775296,0.,-0.00164147725930846));
#79588=DIRECTION('center_axis',(-5.79316531842594E-14,-1.,-4.64104352224614E-14));
#79589=DIRECTION('ref_axis',(1.,-5.79316531842594E-14,3.76431018964206E-31));
#79590=DIRECTION('center_axis',(0.0840402488511352,0.987363722495072,-0.134350720406385));
#79591=DIRECTION('ref_axis',(0.825957557940463,0.00640015555580381,0.563695973455451));
#79592=DIRECTION('',(-0.00164147464991938,0.,-0.999998652779579));
#79593=DIRECTION('center_axis',(0.131328515370216,-0.987363722033873,-0.0886887899459243));
#79594=DIRECTION('ref_axis',(0.625865231966009,0.0131994945570568,0.779819520632545));
#79595=DIRECTION('center_axis',(-0.126719763793783,-0.987363721877416,0.0951576701292319));
#79596=DIRECTION('ref_axis',(0.626887989061991,-0.00537048743991487,0.779090884964309));
#79597=DIRECTION('',(0.976972108935026,0.,0.213367050790528));
#79598=DIRECTION('center_axis',(-6.52405203017506E-14,-1.,-8.08905692541282E-14));
#79599=DIRECTION('ref_axis',(-3.50266061336804E-31,8.08905692541282E-14,
-1.));
#79600=DIRECTION('center_axis',(0.110956869526365,0.987363722511827,-0.113143504331872));
#79601=DIRECTION('ref_axis',(0.685469157120961,0.00640015346900311,0.728073535208809));
#79602=DIRECTION('',(0.213367053339806,0.,-0.976972108378273));
#79603=DIRECTION('center_axis',(0.147323596858144,-0.987363721972992,-0.0583835451169203));
#79604=DIRECTION('ref_axis',(0.443594705445403,0.0131994963886616,0.896130297778114));
#79605=DIRECTION('center_axis',(-0.14421321305761,-0.987363721863186,0.0656919319861826));
#79606=DIRECTION('ref_axis',(0.444750185379517,-0.00537048885387717,0.895638560164956));
#79607=DIRECTION('',(0.908263435453809,0.,0.418398771290792));
#79608=DIRECTION('center_axis',(3.97081302317317E-14,-1.,7.97350081058221E-14));
#79609=DIRECTION('ref_axis',(-1.76608788499542E-31,-7.97350081058221E-14,
-1.));
#79610=DIRECTION('center_axis',(0.132685266333161,0.987363722430977,-0.0866458292437882));
#79611=DIRECTION('ref_axis',(0.51292898068897,0.00640015831316843,0.858407187028942));
#79612=DIRECTION('',(0.418398773660791,0.,-0.90826343436205));
#79613=DIRECTION('center_axis',(0.156429989965125,-0.987363721958195,-0.0253483490659727));
#79614=DIRECTION('ref_axis',(0.240582182111676,0.013199499044569,0.970539018728952));
#79615=DIRECTION('center_axis',(-0.154963411925007,-0.987363721875536,0.0331545123422059));
#79616=DIRECTION('ref_axis',(0.241816356527403,-0.00537048956491149,0.970307171754205));
#79617=DIRECTION('',(0.797085373092917,0.,0.603866630971877));
#79618=DIRECTION('center_axis',(3.24586596311348E-14,-1.,1.29610383251507E-13));
#79619=DIRECTION('ref_axis',(8.61439714851782E-31,-1.29610383251507E-13,
-1.));
#79620=DIRECTION('center_axis',(0.148209450383187,0.987363722419937,-0.0560966885489541));
#79621=DIRECTION('ref_axis',(0.316404815531485,0.00640015906571002,0.948602672709929));
#79622=DIRECTION('',(0.603866633051783,0.,-0.797085371517194));
#79623=DIRECTION('center_axis',(0.158221889636225,-0.987363721921636,0.00887210645764376));
#79624=DIRECTION('ref_axis',(0.0263203038047064,0.0131995003924017,0.99956641339984));
#79625=DIRECTION('center_axis',(-0.158467693619661,-0.987363721870234,-0.000933173844636907));
#79626=DIRECTION('ref_axis',(0.0275754654179984,-0.00537048891585742,0.999605297883012));
#79627=DIRECTION('',(0.648636483669163,0.,0.761098358987394));
#79628=DIRECTION('center_axis',(4.26377006545449E-16,-1.,1.48397574152667E-14));
#79629=DIRECTION('ref_axis',(0.0287202210588392,1.48458814994488E-14,0.999587489368655));
#79630=DIRECTION('center_axis',(0.156803525494413,0.987363722442391,-0.0229245282880083));
#79631=DIRECTION('ref_axis',(0.105085911959256,0.00640015912441032,0.994442551920861));
#79632=DIRECTION('center_axis',(-0.160735572208841,-0.986495109500315,0.0314876921774008));
#79633=DIRECTION('ref_axis',(0.0338459003609357,0.026374638220109,0.999078992616458));
#79634=DIRECTION('center_axis',(-0.150208729944758,-0.986495109192071,0.0653049537822887));
#79635=DIRECTION('ref_axis',(0.247827073369561,0.0263746665288115,0.968445206849914));
#79636=DIRECTION('center_axis',(-0.132658295477633,-0.986495109084167,0.0960686025399893));
#79637=DIRECTION('ref_axis',(0.450220106754815,0.0263746728872703,0.892528000739345));
#79638=DIRECTION('center_axis',(-0.108904912105237,-0.986495109156878,0.12234018035343));
#79639=DIRECTION('ref_axis',(0.631561347853854,0.026374667624227,0.774877177883525));
#79640=DIRECTION('center_axis',(-0.0800592540170044,-0.986495109155527,
0.142891271456541));
#79641=DIRECTION('ref_axis',(0.783371482987673,0.0263746667580228,0.620993958581802));
#79642=DIRECTION('center_axis',(-0.0474701058253641,-0.986495109083009,
0.156760928831869));
#79643=DIRECTION('ref_axis',(0.898552039413217,0.0263746743925295,0.438073748376956));
#79644=DIRECTION('center_axis',(-0.0126613186995483,-0.986495109111999,
0.163300614533115));
#79645=DIRECTION('ref_axis',(0.971717298236084,0.0263746712037161,0.234669701980597));
#79646=DIRECTION('center_axis',(0.0227394998600456,-0.986495109150332,0.162204546078675));
#79647=DIRECTION('ref_axis',(0.999446136981731,0.0263746700344972,0.0202927586312497));
#79648=DIRECTION('center_axis',(0.0570770466086315,-0.986495109126712,0.153523973435789));
#79649=DIRECTION('ref_axis',(0.980441984811844,0.0263746709087561,-0.195033051436586));
#79650=DIRECTION('center_axis',(0.0887457320211409,-0.986495109141813,0.137664791022663));
#79651=DIRECTION('ref_axis',(0.915593456668965,0.0263746702572848,-0.401239328672796));
#79652=DIRECTION('center_axis',(0.116264768310826,-0.986495109125943,0.115368554295456));
#79653=DIRECTION('ref_axis',(0.807932792175151,0.0263746713744888,-0.588684108871601));
#79654=DIRECTION('center_axis',(0.138347388597019,-0.986495109217853,0.0876778167933158));
#79655=DIRECTION('ref_axis',(0.662494092566996,0.0263746671072638,-0.748602667807706));
#79656=DIRECTION('center_axis',(0.153961044274636,-0.986495109084597,0.0558873563342683));
#79657=DIRECTION('ref_axis',(0.486077907132691,0.0263746711415175,-0.87351739817801));
#79658=DIRECTION('center_axis',(0.162375650580194,-0.98649510910325,0.0214836638873636));
#79659=DIRECTION('ref_axis',(0.2869332520124,0.0263746740827948,-0.95758742966719));
#79660=DIRECTION('center_axis',(0.163197750937941,-0.986495109091353,-0.0139245763898883));
#79661=DIRECTION('ref_axis',(0.0743719212258115,0.0263746732350422,-0.996881735184734));
#79662=DIRECTION('center_axis',(0.156388905548954,-0.986495109083077,-0.0486817211730238));
#79663=DIRECTION('ref_axis',(-0.141666957958585,0.0263746746431137,-0.989562958866302));
#79664=DIRECTION('center_axis',(0.142267491681255,-0.986495109182172,-0.0811625552233208));
#79665=DIRECTION('ref_axis',(-0.35108164507487,0.0263746682502834,-0.935973319794005));
#79666=DIRECTION('center_axis',(0.121493807280624,-0.986495109226014,-0.109848323908989));
#79667=DIRECTION('ref_axis',(-0.544080148475943,0.0263746667314525,-0.838618607585833));
#79668=DIRECTION('center_axis',(0.0950392032811796,-0.986495109159665,-0.133397711538612));
#79669=DIRECTION('ref_axis',(-0.71163807058147,0.0263746711143374,-0.702051018959942));
#79670=DIRECTION('center_axis',(0.0641406724996807,-0.986495109097894,-0.150709567902049));
#79671=DIRECTION('ref_axis',(-0.84592058478901,0.0263746736888512,-0.532656306466023));
#79672=DIRECTION('center_axis',(0.0302430011311341,-0.986495109169532,-0.16097440935495));
#79673=DIRECTION('ref_axis',(-0.940648791899366,0.0263746696350386,-0.338355178916926));
#79674=DIRECTION('center_axis',(-0.00506880138706661,-0.986495109150829,
-0.163712268550626));
#79675=DIRECTION('ref_axis',(-0.991393307574693,0.0263746680911805,-0.12823293874504));
#79676=DIRECTION('center_axis',(-0.0401436004710594,-0.986495109078913,
-0.15879512305044));
#79677=DIRECTION('ref_axis',(-0.995781373991902,0.0263746744667969,0.0878853330059665));
#79678=DIRECTION('center_axis',(-0.0733413264079324,-0.986495109008859,
-0.1464528925707));
#79679=DIRECTION('ref_axis',(-0.953607809106848,0.0263746777387383,0.299894185980015));
#79680=DIRECTION('center_axis',(-0.103109683648256,-0.986495109146731,-0.127262691970334));
#79681=DIRECTION('ref_axis',(-0.8668446051852,0.0263746710119367,0.497880314122105));
#79682=DIRECTION('center_axis',(-0.128056752441364,-0.986495109121959,-0.102121828384661));
#79683=DIRECTION('ref_axis',(-0.739548710327857,0.0263746693552898,0.672586114834972));
#79684=DIRECTION('center_axis',(-0.147016031601871,-0.986495109109258,-0.0722058595652089));
#79685=DIRECTION('ref_axis',(-0.577672341080192,0.0263746706390861,0.815842535725866));
#79686=DIRECTION('center_axis',(-0.159101004976774,-0.986495109093066,-0.0389136216618427));
#79687=DIRECTION('ref_axis',(-0.388784647961224,0.0263746737791896,0.920951070411837));
#79688=DIRECTION('center_axis',(-0.163746589679106,-0.986495109177042,-0.00380183353643957));
#79689=DIRECTION('ref_axis',(-0.181717824059167,0.0263746702342777,0.98299695278736));
#79690=DIRECTION('center_axis',(0.163668143187915,0.98649510955974,0.00633543369766243));
#79691=DIRECTION('ref_axis',(-0.0784216555462039,0.00660859149372386,0.996898375191705));
#79692=DIRECTION('center_axis',(0.158479742656236,0.986495109491893,0.0413711266004603));
#79693=DIRECTION('ref_axis',(-0.290891882249892,0.00660859243598289,0.956733107688414));
#79694=DIRECTION('center_axis',(0.14588100613144,0.986495109481366,0.074472350704314));
#79695=DIRECTION('ref_axis',(-0.489760328703683,0.00660859467570009,0.871832063475801));
#79696=DIRECTION('center_axis',(0.126461037299186,0.986495109425709,0.104091330687878));
#79697=DIRECTION('ref_axis',(-0.665728126384466,0.00660859742232058,0.746165121257177));
#79698=DIRECTION('center_axis',(0.101127890716206,0.98649510939482,0.128843117237175));
#79699=DIRECTION('ref_axis',(-0.810567217647311,0.00660859914361863,0.585608326522818));
#79700=DIRECTION('center_axis',(0.0710661119071067,0.986495109452163,0.147570345142143));
#79701=DIRECTION('ref_axis',(-0.917505087153752,0.0066085959530382,0.397669135722796));
#79702=DIRECTION('center_axis',(0.0376813607638582,0.986495109493467,0.159397346265416));
#79703=DIRECTION('ref_axis',(-0.981541437170374,0.00660859291907783,0.19113538033851));
#79704=DIRECTION('center_axis',(0.00253467983119023,0.986495109399991,0.163771104069227));
#79705=DIRECTION('ref_axis',(-0.999682000665267,0.00660859883572792,-0.0243356521859752));
#79706=DIRECTION('center_axis',(-0.0327305250144651,0.986495109396022,0.160487108111548));
#79707=DIRECTION('ref_axis',(-0.971078545498027,0.0066085995295211,-0.238668776520294));
#79708=DIRECTION('center_axis',(-0.0664652930897966,0.986495109464134,0.149698910543241));
#79709=DIRECTION('ref_axis',(-0.89706853564046,0.00660859391791874,-0.441842017977364));
#79710=DIRECTION('center_axis',(-0.0970922137686021,0.986495109509118,0.131910958377629));
#79711=DIRECTION('ref_axis',(-0.781112598468359,0.00660859175496055,-0.624355215425501));
#79712=DIRECTION('center_axis',(-0.123179205476025,0.986495109422879,0.107955001843537));
#79713=DIRECTION('ref_axis',(-0.628632706297494,0.00660859671899613,-0.777674255085312));
#79714=DIRECTION('center_axis',(-0.143506479071122,0.986495109469043,0.0789511840207048));
#79715=DIRECTION('ref_axis',(-0.446758644581469,0.006608594994134,-0.894630113490448));
#79716=DIRECTION('center_axis',(-0.157123548631729,0.98649510949616,0.0462556959252781));
#79717=DIRECTION('ref_axis',(-0.2439946456178,0.00660859273657448,-0.969754061302084));
#79718=DIRECTION('center_axis',(-0.163393694811817,0.98649510941163,0.0113973506868681));
#79719=DIRECTION('ref_axis',(-0.0298217307358154,0.00660859815402411,-0.999533386539119));
#79720=DIRECTION('center_axis',(-0.162023734603462,0.98649510942972,-0.0239939262396024));
#79721=DIRECTION('ref_axis',(0.185745616396384,0.0066085993854543,-0.982575642077336));
#79722=DIRECTION('center_axis',(-0.153077721679699,0.986495109522431,-0.0582632818649898));
#79723=DIRECTION('ref_axis',(0.392627706962826,0.00660859212269046,-0.919673752063888));
#79724=DIRECTION('center_axis',(-0.136973968951122,0.986495109442921,-0.089808300701981));
#79725=DIRECTION('ref_axis',(0.581150960023441,0.00660859623492829,-0.813768940252475));
#79726=DIRECTION('center_axis',(-0.114465467592361,0.986495109370403,-0.117153983786893));
#79727=DIRECTION('ref_axis',(0.742500239708373,0.00660860100223232,-0.669813198157368));
#79728=DIRECTION('center_axis',(-0.0866046785300646,0.986495109478629,-0.139021684033288));
#79729=DIRECTION('ref_axis',(0.869131036238581,0.00660859401759509,-0.494537731959819));
#79730=DIRECTION('center_axis',(-0.0546943599861106,0.986495109488404,-0.154388878942662));
#79731=DIRECTION('ref_axis',(0.955122228521663,0.00660859705495355,-0.296138236350488));
#79732=DIRECTION('center_axis',(-0.020226587168411,0.986495109469708,-0.162537023978744));
#79733=DIRECTION('ref_axis',(0.996452968940974,0.00660859375025051,-0.0838916394962136));
#79734=DIRECTION('center_axis',(0.0151869523181353,0.986495109436306,-0.163085117461823));
#79735=DIRECTION('ref_axis',(0.99119067534219,0.00660859577406016,0.132277630673472));
#79736=DIRECTION('center_axis',(0.0498903736231824,0.986495109518188,-0.156007530319653));
#79737=DIRECTION('ref_axis',(0.939581407019408,0.0066085913316494,0.342261750863341));
#79738=DIRECTION('center_axis',(0.0822609667229837,0.986495109465284,-0.14163520874019));
#79739=DIRECTION('ref_axis',(0.844038356618601,0.00660859756009447,0.536242089913558));
#79740=DIRECTION('center_axis',(0.110785139185442,0.98649510953755,-0.1206401748762));
#79741=DIRECTION('ref_axis',(0.709029009947545,0.00660859048807991,0.705148345800062));
#79742=DIRECTION('center_axis',(0.134129115877841,0.986495109511418,-0.0940041445037607));
#79743=DIRECTION('ref_axis',(0.540866255489018,0.00660859038340004,0.841082647666942));
#79744=DIRECTION('center_axis',(0.151201360818737,0.986495109387669,-0.0629725943627227));
#79745=DIRECTION('ref_axis',(0.347413197746676,0.00660860031970175,0.93768885907493));
#79746=DIRECTION('center_axis',(0.161203604303846,0.986495109502081,-0.0289964978562238));
#79747=DIRECTION('ref_axis',(0.137715482655985,0.00660859113228861,0.990449782856292));
#79748=DIRECTION('center_axis',(0.156429986790059,0.987363722430518,-0.0253483502621767));
#79749=DIRECTION('ref_axis',(0.105566785065707,0.00880314965778774,0.994373249060429));
#79750=DIRECTION('',(-0.60378640757203,0.,0.797146143458816));
#79751=DIRECTION('',(-0.797146142953525,0.,-0.603786408239137));
#79752=DIRECTION('center_axis',(7.21593417373741E-15,-1.,2.88015808780585E-14));
#79753=DIRECTION('ref_axis',(3.73148717172395E-32,-2.88015808780585E-14,
-1.));
#79754=DIRECTION('center_axis',(-0.154431767592391,-0.987363722333479,0.0355486846179549));
#79755=DIRECTION('ref_axis',(0.170524506140172,0.00880346257917287,0.985314108217409));
#79756=DIRECTION('center_axis',(0.156803524252501,-0.987363722273954,-0.0229245440372688));
#79757=DIRECTION('ref_axis',(0.240230849202258,0.015616035248029,0.970590170223609));
#79758=DIRECTION('center_axis',(0.147323595591869,0.987363722485576,-0.0583835396435483));
#79759=DIRECTION('ref_axis',(0.316859547487647,0.00880314606301053,0.9484316168208));
#79760=DIRECTION('',(-0.418307358246727,0.,0.908305540023094));
#79761=DIRECTION('',(-0.908305540399124,0.,-0.418307357430222));
#79762=DIRECTION('center_axis',(1.98580772700459E-14,-1.,3.98655051185617E-14));
#79763=DIRECTION('ref_axis',(4.90281768277353E-31,-3.98655051185617E-14,
-1.));
#79764=DIRECTION('center_axis',(-0.143179321891756,-0.987363722363956,0.0679158416145226));
#79765=DIRECTION('ref_axis',(0.378351146654384,0.00880346294309428,0.925620283304943));
#79766=DIRECTION('center_axis',(0.148209449214943,-0.987363722079989,-0.0560966976189729));
#79767=DIRECTION('ref_axis',(0.443262580240077,0.0156160420103856,0.896255780562022));
#79768=DIRECTION('center_axis',(0.131328515651695,0.987363722452776,-0.0886887848655015));
#79769=DIRECTION('ref_axis',(0.513336310721137,0.00880314782965812,0.858142375531882));
#79770=DIRECTION('',(-0.213268723577629,0.,0.976993578046227));
#79771=DIRECTION('',(-0.976993578237944,0.,-0.213268722699364));
#79772=DIRECTION('center_axis',(-1.8642474407541E-14,-1.,-2.31097147398058E-14));
#79773=DIRECTION('ref_axis',(-3.71574464986128E-31,2.31097147398058E-14,
-1.));
#79774=DIRECTION('center_axis',(-0.125231968813796,-0.987363722355263,0.0971073311536195));
#79775=DIRECTION('ref_axis',(0.568486505809193,0.00880346607357507,0.822645483606363));
#79776=DIRECTION('center_axis',(0.13268526417301,-0.98736372206775,-0.0866458366908468));
#79777=DIRECTION('ref_axis',(0.625567847037377,0.0156160442834527,0.780013466495264));
#79778=DIRECTION('center_axis',(0.109192661699068,0.987363722509184,-0.114847037854183));
#79779=DIRECTION('ref_axis',(0.685810037120877,0.00880314627001295,0.727727351141903));
#79780=DIRECTION('',(0.00174211876870894,0.,0.999998482509946));
#79781=DIRECTION('',(-0.999998482503372,0.,0.00174212254246539));
#79782=DIRECTION('center_axis',(5.7936323155652E-14,-1.,4.64046037923618E-14));
#79783=DIRECTION('ref_axis',(1.,5.7936323155652E-14,1.59675549687847E-31));
#79784=DIRECTION('center_axis',(-0.101428913894775,-0.987363722346308,0.12175818338235));
#79785=DIRECTION('ref_axis',(0.732040068171316,0.00880346020649426,0.681204695873515));
#79786=DIRECTION('center_axis',(0.110956859394232,-0.987363722163564,-0.113143517307362));
#79787=DIRECTION('ref_axis',(0.778622256538946,0.0156160399944578,0.627298589921173));
#79788=DIRECTION('center_axis',(0.0819510841136594,0.98736372258261,-0.135635169260802));
#79789=DIRECTION('ref_axis',(0.826216048340669,0.00880314079029221,0.563284604952554));
#79790=DIRECTION('',(0.216671506352657,0.,0.976244568914404));
#79791=DIRECTION('',(-0.976244568854602,0.,0.216671506622102));
#79792=DIRECTION('center_axis',(-2.66229689183797E-14,-1.,-1.31460372347046E-14));
#79793=DIRECTION('ref_axis',(1.,-2.66229689183797E-14,-3.13869790383516E-31));
#79794=DIRECTION('center_axis',(-0.0728831540845708,-0.987363722339392,
0.14071576194153));
#79795=DIRECTION('ref_axis',(0.861364251543031,0.00880345782593299,0.507911532940552));
#79796=DIRECTION('center_axis',(0.0840402415482007,-0.987363722072949,-0.134350728076821));
#79797=DIRECTION('ref_axis',(0.895269154764806,0.0156160439371077,0.445251928348957));
#79798=DIRECTION('center_axis',(0.0508775536079316,0.987363722440774,-0.150081158533545));
#79799=DIRECTION('ref_axis',(0.927989115978238,0.00880314919346329,0.372503295542745));
#79800=DIRECTION('',(0.421469569973658,0.,0.906842545090502));
#79801=DIRECTION('',(-0.906842544711597,0.,0.421469570788919));
#79802=DIRECTION('center_axis',(5.76530962313139E-14,-1.,1.42310776850099E-14));
#79803=DIRECTION('ref_axis',(1.,5.76530962313139E-14,-3.49047495775741E-32));
#79804=DIRECTION('center_axis',(-0.0409294558697067,-0.987363722338178,
0.153093629693422));
#79805=DIRECTION('ref_axis',(0.950411999976481,0.00880345909517113,0.310868990747977));
#79806=DIRECTION('center_axis',(0.0531939918611952,-0.987363722074152,-0.149275850564478));
#79807=DIRECTION('ref_axis',(0.97005426217788,0.0156160433238334,0.242385782630575));
#79808=DIRECTION('center_axis',(0.0174250530024264,0.987363722465118,-0.157509514276718));
#79809=DIRECTION('ref_axis',(0.986370443252028,0.00880314841710919,0.16430414862913));
#79810=DIRECTION('',(0.606560187375799,0.,0.795037570867337));
#79811=DIRECTION('',(-0.795037570322038,0.,0.60656018809054));
#79812=DIRECTION('',(0.763288722545863,0.,0.646057525329057));
#79813=DIRECTION('',(-0.646057524642841,0.,0.763288723126685));
#79814=DIRECTION('center_axis',(1.02025012898349E-13,-1.,-1.97612283078631E-14));
#79815=DIRECTION('ref_axis',(1.,1.02025012898349E-13,4.59893401350721E-31));
#79816=DIRECTION('center_axis',(0.0271357814488703,-0.987363722366704,0.156129846984253));
#79817=DIRECTION('ref_axis',(0.993101070891819,0.00880346203509836,-0.116930586459314));
#79818=DIRECTION('center_axis',(-0.0144017443938191,-0.987363722089207,
-0.15781466997894));
#79819=DIRECTION('ref_axis',(0.982172552118582,0.0156160426088595,-0.187331836797992));
#79820=DIRECTION('center_axis',(-0.0503219761172802,0.987363722498807,-0.150268353996944));
#79821=DIRECTION('ref_axis',(0.96419509013843,0.00880314564673555,-0.265047793387659));
#79822=DIRECTION('',(0.884326726537715,0.,0.466868547592457));
#79823=DIRECTION('',(-0.466868544549227,0.,0.884326728144347));
#79824=DIRECTION('center_axis',(-8.1764267020795E-14,-1.,3.5341357472854E-14));
#79825=DIRECTION('ref_axis',(1.,-8.1764267020795E-14,3.41816808687732E-32));
#79826=DIRECTION('center_axis',(0.0600646626700829,-0.987363722325553,0.146646227819738));
#79827=DIRECTION('ref_axis',(0.944746300203437,0.00880346065774608,-0.327684188407626));
#79828=DIRECTION('center_axis',(-0.0479905351096277,-0.987363722266364,
-0.1510290981639));
#79829=DIRECTION('ref_axis',(0.918939096098908,0.0156160354520983,-0.394090189040125));
#79830=DIRECTION('center_axis',(-0.0814487305111112,0.987363722500292,-0.135937426003639));
#79831=DIRECTION('ref_axis',(0.884675303833306,0.00880314564771947,-0.466124566413477));
#79832=DIRECTION('',(0.964014596804326,0.,0.265849312860112));
#79833=DIRECTION('',(-0.265849311993547,0.,0.964014597043301));
#79834=DIRECTION('center_axis',(-3.61276583900821E-14,-1.,2.60459983457543E-14));
#79835=DIRECTION('ref_axis',(1.,-3.61276583900821E-14,-3.2333570323359E-31));
#79836=DIRECTION('center_axis',(0.0901849869769349,-0.987363722335554,0.130305594429595));
#79837=DIRECTION('ref_axis',(0.852216242175415,0.00880345886951841,-0.52311564274484));
#79838=DIRECTION('center_axis',(-0.0793353310103516,-0.987363722158274,
-0.137181578279438));
#79839=DIRECTION('ref_axis',(0.812737069336137,0.0156160402722304,-0.582421321221264));
#79840=DIRECTION('center_axis',(-0.108767033422489,0.987363722485668,-0.115250214575575));
#79841=DIRECTION('ref_axis',(0.763789083031293,0.0088031463387518,-0.64540587327414));
#79842=DIRECTION('',(0.998626215044556,0.,0.0523992616912134));
#79843=DIRECTION('',(-0.0523992607935246,0.,0.998626215091659));
#79844=DIRECTION('center_axis',(1.97892627087603E-14,-1.,-2.2135623987073E-14));
#79845=DIRECTION('ref_axis',(2.17927070130815E-31,2.2135623987073E-14,-1.));
#79846=DIRECTION('center_axis',(0.116088364939715,-0.987363722346286,0.107872013609233));
#79847=DIRECTION('ref_axis',(0.719837499788847,0.00880346163078833,-0.694086790654495));
#79848=DIRECTION('center_axis',(-0.106970499871311,-0.987363722142377,-0.116919597820181));
#79849=DIRECTION('ref_axis',(0.668532361216325,0.0156160394805405,-0.743519079323098));
#79850=DIRECTION('center_axis',(-0.130999510954202,0.987363722460183,-0.0891740304086968));
#79851=DIRECTION('ref_axis',(0.607188933706365,0.00880314778993197,-0.794508718248904));
#79852=DIRECTION('',(0.986543181538475,0.,-0.16350092036421));
#79853=DIRECTION('',(0.163500921251019,0.,0.986543181391503));
#79854=DIRECTION('center_axis',(-7.28404795707868E-15,-1.,1.29361059625103E-14));
#79855=DIRECTION('ref_axis',(1.20157592816024E-31,-1.29361059625103E-14,
-1.));
#79856=DIRECTION('center_axis',(0.136563576359677,-0.987363722343636,0.0803944613239859));
#79857=DIRECTION('ref_axis',(0.553799956712619,0.00880345897931285,-0.8326032110526));
#79858=DIRECTION('center_axis',(-0.129603845053638,-0.987363722128365,-0.0911905892739679));
#79859=DIRECTION('ref_axis',(0.493067823026643,0.0156160419141663,-0.869850711979189));
#79860=DIRECTION('center_axis',(-0.14710659521871,0.987363722492469,-0.0589281694011677));
#79861=DIRECTION('ref_axis',(0.422197307061374,0.00880314719321597,-0.906461217322406));
#79862=DIRECTION('',(0.928330484416674,0.,-0.371755984084592));
#79863=DIRECTION('',(0.37175598392696,0.,0.928330484479799));
#79864=DIRECTION('center_axis',(-1.73314822661811E-14,-1.,5.67980879078818E-14));
#79865=DIRECTION('ref_axis',(-2.56612137703982E-31,-5.67980879078818E-14,
-1.));
#79866=DIRECTION('center_axis',(0.150653229585631,-0.987363722340501,0.0491577483346112));
#79867=DIRECTION('ref_axis',(0.361867341872136,0.00880346207617823,-0.932188031430284));
#79868=DIRECTION('center_axis',(-0.146177060289818,-0.987363722117319,-0.0611976085452662));
#79869=DIRECTION('ref_axis',(0.294547980804413,0.0156160421158191,-0.955509092700158));
#79870=DIRECTION('center_axis',(-0.156335138797612,0.987363722512107,-0.0259268942252293));
#79871=DIRECTION('ref_axis',(0.217464201437641,0.00880314485374298,-0.976028598829856));
#79872=DIRECTION('',(0.826710086440232,0.,-0.562628148049833));
#79873=DIRECTION('',(0.562628149420581,0.,0.826710085507351));
#79874=DIRECTION('center_axis',(9.43274378737716E-15,-1.,-1.1839187339302E-13));
#79875=DIRECTION('ref_axis',(-2.44385558762843E-31,1.1839187339302E-13,
-1.));
#79876=DIRECTION('center_axis',(0.157698503408068,-0.98736372234875,0.015622477795658));
#79877=DIRECTION('ref_axis',(0.15301421202466,0.00880346049852462,-0.988184775232711));
#79878=DIRECTION('center_axis',(-0.155915199182802,-0.987363722212749,-0.028343089492366));
#79879=DIRECTION('ref_axis',(0.0822554028362943,0.0156160359799182,-0.996488930256886));
#79880=DIRECTION('center_axis',(-0.158253626201034,0.987363722455138,0.00828669860420722));
#79881=DIRECTION('ref_axis',(0.00256271212569272,0.00880314780058656,-0.999957967664322));
#79882=DIRECTION('',(0.686433642709764,0.,-0.727192446437808));
#79883=DIRECTION('',(0.727192447054856,0.,0.686433642056077));
#79884=DIRECTION('center_axis',(-4.05963541081443E-15,-1.,-2.94129245268148E-14));
#79885=DIRECTION('ref_axis',(-7.93676947716632E-32,2.94129245268148E-14,
-1.));
#79886=DIRECTION('center_axis',(0.157369971051554,-0.987363722346701,-0.0186432831041112));
#79887=DIRECTION('ref_axis',(-0.0629936888030954,0.0088034602491171,-0.997975097013258));
#79888=DIRECTION('center_axis',(-0.158362915039063,-0.987363722199347,0.00583671354289517));
#79889=DIRECTION('ref_axis',(-0.133883348256068,0.0156160378949963,-0.990874052753531));
#79890=DIRECTION('center_axis',(-0.152772349398299,0.9873637225453,0.0421128087499838));
#79891=DIRECTION('ref_axis',(-0.212458609616509,0.00880314423507185,-0.977130412919072));
#79892=DIRECTION('',(0.514060325754162,0.,-0.857754033208544));
#79893=DIRECTION('',(0.857754032403029,0.,0.514060327098234));
#79894=DIRECTION('center_axis',(2.05752654287224E-14,-1.,5.57051301331E-14));
#79895=DIRECTION('ref_axis',(4.21927796756254E-31,-5.57051301331E-14,-1.));
#79896=DIRECTION('center_axis',(0.149682992850515,-0.987363722367468,-0.0520373078086402));
#79897=DIRECTION('ref_axis',(-0.276056079899396,0.0088034623672994,-0.961101212048411));
#79898=DIRECTION('center_axis',(-0.15340575824948,-0.987363722140233,0.0397435974376586));
#79899=DIRECTION('ref_axis',(-0.343761860804829,0.01561604059786,-0.938927005859373));
#79900=DIRECTION('center_axis',(-0.140147605930203,0.987363722434418,0.0739697787781123));
#79901=DIRECTION('ref_axis',(-0.417545600877838,0.00880314941097575,-0.908613325759651));
#79902=DIRECTION('',(0.317650121520213,0.,-0.948207994217616));
#79903=DIRECTION('',(0.948207994503158,0.,0.317650120667848));
#79904=DIRECTION('center_axis',(-4.00864794192018E-14,-1.,-6.24746266568276E-14));
#79905=DIRECTION('ref_axis',(9.85386662136157E-31,6.24746266568276E-14,
-1.));
#79906=DIRECTION('center_axis',(0.134997006595335,-0.987363722344993,-0.0829981205048595));
#79907=DIRECTION('ref_axis',(-0.476210392871911,0.00880345891853127,-0.87928730278098));
#79908=DIRECTION('center_axis',(-0.141275518359591,-0.9873637221238,0.0717921175761243));
#79909=DIRECTION('ref_axis',(-0.537566450769722,0.0156160405828081,-0.843076776031318));
#79910=DIRECTION('center_axis',(-0.120969720854335,0.987363722540651,0.102367993274716));
#79911=DIRECTION('ref_axis',(-0.603108622345235,0.00880314257524947,-0.797610490360823));
#79912=DIRECTION('',(0.106386948329893,0.,-0.994324804691632));
#79913=DIRECTION('',(0.994324804754728,0.,0.106386947740181));
#79914=DIRECTION('center_axis',(-7.36112688092222E-14,-1.,-7.33552349527714E-14));
#79915=DIRECTION('ref_axis',(1.,-7.36112688092222E-14,-8.57751515811246E-32));
#79916=DIRECTION('center_axis',(0.113998708832555,-0.987363722364275,-0.110078036608008));
#79917=DIRECTION('ref_axis',(-0.654097634895031,0.00880345963371462,-0.756358898356596));
#79918=DIRECTION('center_axis',(-0.122539391431094,-0.987363722160386,0.100483718627868));
#79919=DIRECTION('ref_axis',(-0.706235031996309,0.0156160398271936,-0.707805212527633));
#79920=DIRECTION('center_axis',(-0.0961354199797208,0.987363722474785,0.125979603770045));
#79921=DIRECTION('ref_axis',(-0.760470956138659,0.00880314729218524,-0.64931227423121));
#79922=DIRECTION('',(-0.109850763216409,0.,-0.993948092115867));
#79923=DIRECTION('',(0.993948092331009,0.,-0.109850761269768));
#79924=DIRECTION('center_axis',(-6.26139182359717E-14,-1.,-3.986855967794E-14));
#79925=DIRECTION('ref_axis',(1.,-6.26139182359717E-14,3.82708143775318E-31));
#79926=DIRECTION('center_axis',(0.0876699555725528,-0.987363722327332,-0.132010828047633));
#79927=DIRECTION('ref_axis',(-0.80140000250608,0.00880346280796036,-0.598063989072946));
#79928=DIRECTION('center_axis',(-0.0980734572555049,-0.987363722206742,
0.124476813310756));
#79929=DIRECTION('ref_axis',(-0.841880847839118,0.0156160374502623,-0.539437463860307));
#79930=DIRECTION('center_axis',(-0.066805935379289,0.98736372243709,0.143700544930325));
#79931=DIRECTION('ref_axis',(-0.882274512475655,0.00880314880506724,-0.470652939231194));
#79932=DIRECTION('',(-0.320951971885479,0.,-0.947095471292532));
#79933=DIRECTION('',(0.947095471004021,0.,-0.320951972736843));
#79934=DIRECTION('center_axis',(1.39441202957586E-14,-1.,5.09526267024895E-15));
#79935=DIRECTION('ref_axis',(1.,1.39441202957586E-14,-4.33523906184624E-32));
#79936=DIRECTION('center_axis',(0.0572418589532895,-0.987363722345415,-0.147770935504174));
#79937=DIRECTION('ref_axis',(-0.91122979430671,0.00880345858023634,-0.411804275214303));
#79938=DIRECTION('center_axis',(-0.0690217183973883,-0.98736372219858,0.142649509202227));
#79939=DIRECTION('ref_axis',(-0.938161250680476,0.0156160368527398,-0.34584621888154));
#79940=DIRECTION('center_axis',(-0.0343526832863041,0.987363722489873,0.154702206390121));
#79941=DIRECTION('ref_axis',(-0.962823895055901,0.00880314516105514,-0.269986391776803));
#79942=DIRECTION('',(-0.517045821934947,0.,-0.85595771976168));
#79943=DIRECTION('',(0.855957719296903,0.,-0.517045822704376));
#79944=DIRECTION('center_axis',(1.32421008241407E-13,-1.,1.78070812253087E-14));
#79945=DIRECTION('ref_axis',(1.,1.32421008241407E-13,-6.73625595346913E-32));
#79946=DIRECTION('center_axis',(0.0241371926388202,-0.987363722366506,-0.156621440697221));
#79947=DIRECTION('ref_axis',(-0.978451494625342,0.00880345880616111,-0.206289049099757));
#79948=DIRECTION('center_axis',(-0.0367426028754845,-0.987363722166912,
0.154152071937536));
#79949=DIRECTION('ref_axis',(-0.990574275756191,0.0156160384287705,-0.136083590318191));
#79950=DIRECTION('center_axis',(-0.000293134950792496,0.98736372249097,
0.15847016621647));
#79951=DIRECTION('ref_axis',(-0.998352700893353,0.00880314554373982,-0.0566955840209985));
#79952=DIRECTION('',(-0.688963187105363,0.,-0.724796334713153));
#79953=DIRECTION('',(0.724796334022858,0.,-0.68896318783156));
#79954=DIRECTION('center_axis',(-8.87687165924439E-14,-1.,7.38389392493327E-15));
#79955=DIRECTION('ref_axis',(1.,-8.87687165924439E-14,6.42305608760724E-32));
#79956=DIRECTION('center_axis',(-0.0100961008658548,-0.987363722319383,
-0.158148501715697));
#79957=DIRECTION('ref_axis',(-0.999921890126576,0.00880345827309538,0.00887202164842416));
#79958=DIRECTION('center_axis',(-0.00274544497606824,-0.987363722132808,
0.158446655843319));
#79959=DIRECTION('ref_axis',(-0.996669148956917,0.0156160409304335,0.0800421562875077));
#79960=DIRECTION('center_axis',(0.0337801256632999,0.987363722407798,0.154828236388552));
#79961=DIRECTION('ref_axis',(-0.987199644128115,0.00880315153869502,0.159246246914358));
#79962=DIRECTION('',(-0.828665397202258,0.,-0.559744280434935));
#79963=DIRECTION('',(0.559744277715943,0.,-0.828665399038875));
#79964=DIRECTION('center_axis',(2.83686781064228E-14,-1.,-8.76463754737869E-15));
#79965=DIRECTION('ref_axis',(1.,2.83686781064229E-14,-2.01260476470523E-31));
#79966=DIRECTION('center_axis',(-0.0438573179697657,-0.987363722349336,
-0.152280712662379));
#79967=DIRECTION('ref_axis',(-0.974637049721441,0.00880346401316108,0.223618246866515));
#79968=DIRECTION('center_axis',(0.0313800915095481,-0.987363722164575,0.155332449958691));
#79969=DIRECTION('ref_axis',(-0.95616088060051,0.0156160386448679,0.292425220776696));
#79970=DIRECTION('center_axis',(0.0662738583554316,0.987363722418044,0.143946710109916));
#79971=DIRECTION('ref_axis',(-0.929886229135973,0.00880315053968251,0.367741900527878));
#79972=DIRECTION('',(-0.929620135171039,0.,-0.36851920477036));
#79973=DIRECTION('',(0.36851920294983,0.,-0.929620135892732));
#79974=DIRECTION('center_axis',(0.0956686246027889,0.987363724192392,0.126334438754998));
#79975=DIRECTION('ref_axis',(-0.829092352089055,0.0088030580832515,0.559042375742503));
#79976=DIRECTION('',(-0.987106868437356,0.,-0.160062582397625));
#79977=DIRECTION('center_axis',(1.29106480976479E-14,-1.,-7.32907620994719E-15));
#79978=DIRECTION('ref_axis',(1.,1.29106480976479E-14,1.16314341729505E-31));
#79979=DIRECTION('center_axis',(-0.0755678077550528,-0.987363722339629,
-0.139292448606257));
#79980=DIRECTION('ref_axis',(-0.903779263376947,0.00880346100684245,0.427908333833455));
#79981=DIRECTION('center_axis',(0.0640381965992371,-0.987363718774048,0.14495515246103));
#79982=DIRECTION('ref_axis',(-0.87094360115238,0.0156161908311511,0.491134786179566));
#79983=DIRECTION('',(0.160062578709125,0.,-0.987106869035458));
#79984=DIRECTION('center_axis',(-4.41330782755392E-14,-1.,3.97325367041087E-14));
#79985=DIRECTION('ref_axis',(1.,-4.41330782755392E-14,5.27563451808919E-31));
#79986=DIRECTION('center_axis',(0.120590177674939,0.987363722471961,0.102814826725719));
#79987=DIRECTION('ref_axis',(-0.68953106913893,0.00880314808545024,0.724202602367534));
#79988=DIRECTION('center_axis',(-0.103744832782692,-0.987363722346209,-0.119791024144255));
#79989=DIRECTION('ref_axis',(-0.790661764724653,0.00880346052475684,0.612189899365619));
#79990=DIRECTION('center_axis',(0.0937021981459183,-0.98736372205965,0.127799759088729));
#79991=DIRECTION('ref_axis',(-0.745001950293547,0.0156160444667243,0.666879474278542));
#79992=DIRECTION('',(-0.998437581989233,-7.4805248799978E-15,0.0558783936015749));
#79993=DIRECTION('',(-0.0558783943386867,0.,-0.99843758194798));
#79994=DIRECTION('center_axis',(-4.31999381995619E-14,-1.,6.03636492336854E-14));
#79995=DIRECTION('ref_axis',(2.04237656696525E-31,-6.03636492336854E-14,
-1.));
#79996=DIRECTION('center_axis',(-0.127070866296767,-0.987363722339815,-0.0946883031100116));
#79997=DIRECTION('ref_axis',(-0.640573800107769,0.00880346197464888,0.76784614713675));
#79998=DIRECTION('center_axis',(0.118984666370147,-0.987363722173514,0.104668664386479));
#79999=DIRECTION('ref_axis',(-0.584224842185945,0.0156160393644823,0.811441601772657));
#80000=DIRECTION('center_axis',(0.139872995317343,0.987363722448375,0.0744877491527499));
#80001=DIRECTION('ref_axis',(-0.517728064119055,0.00880314880339182,0.855499945175148));
#80002=DIRECTION('',(-0.963082463777524,0.,0.269206552602669));
#80003=DIRECTION('',(-0.269206553468368,0.,-0.963082463535539));
#80004=DIRECTION('center_axis',(-3.5056256827116E-14,-1.,8.18869083354101E-14));
#80005=DIRECTION('ref_axis',(-2.79057244880545E-31,-8.18869083354101E-14,
-1.));
#80006=DIRECTION('center_axis',(-0.144455208023086,-0.987363722350595,-0.0651580590639688));
#80007=DIRECTION('ref_axis',(-0.460533315515677,0.0088034663068353,0.887598763113786));
#80008=DIRECTION('center_axis',(0.138703539564003,-0.987363722143998,0.0766433839699575));
#80009=DIRECTION('ref_axis',(-0.396130032146719,0.0156160402368145,0.918061619347395));
#80010=DIRECTION('center_axis',(0.152615505799362,0.987363722503179,0.0426777093371941));
#80011=DIRECTION('ref_axis',(-0.321716670115856,0.00880314689765988,0.946795061654983));
#80012=DIRECTION('',(-0.88269468020377,0.,0.469946913533821));
#80013=DIRECTION('',(-0.469946916567211,0.,-0.882694678588792));
#80014=DIRECTION('center_axis',(5.54446544015125E-15,-1.,-2.91694990146662E-14));
#80015=DIRECTION('ref_axis',(-1.44957932349112E-31,2.91694990146662E-14,
-1.));
#80016=DIRECTION('center_axis',(-0.15508498092205,-0.987363722354531,-0.0325811060372834));
#80017=DIRECTION('ref_axis',(-0.258958805904553,0.00880346029549782,0.965848246843837));
#80018=DIRECTION('center_axis',(0.151936789673519,-0.987363722123989,0.0450343444180885));
#80019=DIRECTION('ref_axis',(-0.189512623029802,0.015616041182101,0.981754095978297));
#80020=DIRECTION('center_axis',(0.158221886234408,0.987363722470712,0.00887210601856122));
#80021=DIRECTION('ref_axis',(-0.110662161816853,0.00880314662070804,0.99381909347305));
#80022=DIRECTION('',(-0.761033074724776,0.,0.64871307923839));
#80023=DIRECTION('center_axis',(-2.99509393216772E-15,-1.,-1.03877999789806E-13));
#80024=DIRECTION('ref_axis',(0.0288208256144518,-1.03921169296701E-13,0.999584593724264));
#80025=DIRECTION('center_axis',(-0.158463154906743,-0.987363722361537,0.00151930950452709));
#80026=DIRECTION('ref_axis',(-0.0452756706492831,0.00880346115518785,0.998935740034837));
#80027=DIRECTION('center_axis',(0.158065644955419,-0.987363722085724,0.0113195491894476));
#80028=DIRECTION('ref_axis',(0.0259661867516164,0.0156160424447702,0.99954084276929));
#80029=DIRECTION('',(-0.648713081341758,0.,-0.761033072931841));
#80030=DIRECTION('center_axis',(-0.158467695620547,-0.987363721671432,-0.000933044400132078));
#80031=DIRECTION('ref_axis',(-0.150057930269645,0.023149632801892,0.988406147322207));
#80032=DIRECTION('',(0.563196917554046,0.,0.826322716653501));
#80033=DIRECTION('',(0.826322717534269,0.,-0.563196916261782));
#80034=DIRECTION('center_axis',(-0.154562233296029,-0.987363721596047,-0.0349770970000011));
#80035=DIRECTION('ref_axis',(-0.359027761721998,0.0231496363467189,0.933039742267127));
#80036=DIRECTION('',(0.372394728026814,0.,0.928074440192076));
#80037=DIRECTION('center_axis',(2.16154908660597E-14,-1.,-7.10125017377928E-14));
#80038=DIRECTION('ref_axis',(-9.69985311778293E-32,7.10125017377928E-14,
-1.));
#80039=DIRECTION('center_axis',(0.158065646374123,0.987363722077051,0.0113195301352506));
#80040=DIRECTION('ref_axis',(-0.214528637032064,0.0231492483173103,0.976443329740906));
#80041=DIRECTION('center_axis',(-0.155570612698608,0.987363722813212,-0.0301771989590363));
#80042=DIRECTION('ref_axis',(-0.288936904074014,-0.0162697674035493,0.957209883010387));
#80043=DIRECTION('',(0.928074440978588,0.,-0.372394726066685));
#80044=DIRECTION('center_axis',(-0.14342960823569,-0.987363721719631,-0.0673856699403972));
#80045=DIRECTION('ref_axis',(-0.551209858073525,0.0231496287762393,0.834045434643753));
#80046=DIRECTION('',(0.164179775258774,0.,0.986430434139163));
#80047=DIRECTION('center_axis',(1.45502885892669E-14,-1.,-2.58822309381055E-14));
#80048=DIRECTION('ref_axis',(3.34263340561198E-31,2.58822309381055E-14,
-1.));
#80049=DIRECTION('center_axis',(0.151936792278081,0.98736372224679,0.0450343329384399));
#80050=DIRECTION('ref_axis',(-0.419419530467412,0.0231492422746426,0.907497311315359));
#80051=DIRECTION('center_axis',(-0.145446249712898,0.987363722931636,-0.0629147604543809));
#80052=DIRECTION('ref_axis',(-0.487953552939853,-0.0162697625976409,0.872717952719199));
#80053=DIRECTION('',(0.986430434661683,0.,-0.164179772119355));
#80054=DIRECTION('center_axis',(-0.125590380613658,-0.987363721619889,-0.096643352209241));
#80055=DIRECTION('ref_axis',(-0.717617991607929,0.0231496346007728,0.696052090391555));
#80056=DIRECTION('',(-0.0517120410961091,0.,0.998662037330785));
#80057=DIRECTION('center_axis',(4.94350637840417E-14,-1.,-5.53730920682456E-14));
#80058=DIRECTION('ref_axis',(1.10788581713826E-30,5.53730920682456E-14,
-1.));
#80059=DIRECTION('center_axis',(0.138703544670118,0.987363722225615,0.076643373677849));
#80060=DIRECTION('ref_axis',(-0.604698830638238,0.023149243016814,0.796117727960191));
#80061=DIRECTION('center_axis',(-0.128520985285773,0.98736372286041,-0.0927104908864498));
#80062=DIRECTION('ref_axis',(-0.664154030955957,-0.0162697648243992,0.747418703216285));
#80063=DIRECTION('',(0.998662037017743,0.,0.0517120471415683));
#80064=DIRECTION('center_axis',(-0.101878684209459,-0.987363721630791,-0.121382102927672));
#80065=DIRECTION('ref_axis',(-0.850471105103065,0.023149635510488,0.525512125226909));
#80066=DIRECTION('',(-0.265185861602725,0.,0.964197313212405));
#80067=DIRECTION('center_axis',(-1.20365754886992E-14,-1.,8.69028450318463E-15));
#80068=DIRECTION('ref_axis',(1.,-1.20365754886992E-14,7.95976927521444E-32));
#80069=DIRECTION('center_axis',(0.118984673112717,0.987363722197058,0.104668656499597));
#80070=DIRECTION('ref_axis',(-0.761703085973765,0.0231492427474054,0.647512564648954));
#80071=DIRECTION('center_axis',(-0.105586217923025,0.987363722968099,-0.118171185791153));
#80072=DIRECTION('ref_axis',(-0.809299406389199,-0.0162697611307288,0.587170985055324));
#80073=DIRECTION('',(0.964197312368427,0.,0.265185864671369));
#80074=DIRECTION('center_axis',(-0.0734032480289828,-0.987363721695065,
-0.140445164599092));
#80075=DIRECTION('ref_axis',(-0.943557136986267,0.0231496302779127,0.330399793977349));
#80076=DIRECTION('',(-0.46625988377264,0.,0.884647794765987));
#80077=DIRECTION('center_axis',(-1.36233213274569E-14,-1.,5.89960255031437E-15));
#80078=DIRECTION('ref_axis',(1.,-1.36233213274569E-14,-1.3669389075937E-31));
#80079=DIRECTION('center_axis',(0.0937022060756123,0.98736372236211,0.127799750937949));
#80080=DIRECTION('ref_axis',(-0.883090952952439,0.023149238195361,0.468630431773832));
#80081=DIRECTION('center_axis',(-0.0777143651771768,0.987363722808187,-0.138106322547035));
#80082=DIRECTION('ref_axis',(-0.91660284094264,-0.0162697677780348,0.399467804250018));
#80083=DIRECTION('',(0.884647793282078,0.,0.466259886588103));
#80084=DIRECTION('center_axis',(-0.0414955664543414,-0.987363721630556,
-0.152941162453053));
#80085=DIRECTION('ref_axis',(-0.992523484580295,0.023149634910543,0.119838336771237));
#80086=DIRECTION('',(-0.64553211208243,0.,0.763733128959585));
#80087=DIRECTION('center_axis',(1.0201139073888E-13,-1.,-1.9831432186191E-14));
#80088=DIRECTION('ref_axis',(1.,1.0201139073888E-13,1.91380290558237E-31));
#80089=DIRECTION('center_axis',(0.0640383411138823,0.987363722029649,0.144955066441778));
#80090=DIRECTION('ref_axis',(-0.963186466508821,0.023149247304864,0.267835664323237));
#80091=DIRECTION('center_axis',(-0.0462086656340887,0.98736372290792,-0.151583765310571));
#80092=DIRECTION('ref_axis',(-0.981046945841421,-0.016269763912773,0.193085951942246));
#80093=DIRECTION('',(0.763733125487799,0.,0.645532116189921));
#80094=DIRECTION('center_axis',(-0.00764758997613864,-0.987363721700575,
-0.158285803018297));
#80095=DIRECTION('ref_axis',(-0.995080537351366,0.0231496303981934,-0.0963266255868246));
#80096=DIRECTION('',(-0.794619977419008,0.,0.607107149922166));
#80097=DIRECTION('center_axis',(-1.48413703996974E-14,-1.,-3.65949892926735E-16));
#80098=DIRECTION('ref_axis',(-0.999696144378386,1.48458814041184E-14,-0.0246499272816014));
#80099=DIRECTION('center_axis',(0.0313800969967225,0.987363722278217,0.155332448127816));
#80100=DIRECTION('ref_axis',(-0.998244453125112,0.0231492385997883,0.054517195059875));
#80101=DIRECTION('center_axis',(-0.0125422991360817,0.987363723013676,-0.157973318028564));
#80102=DIRECTION('ref_axis',(-0.999618385591608,-0.0162697590345936,-0.0223243841613663));
#80103=DIRECTION('',(0.6071071473932,0.,0.794619979351194));
#80104=DIRECTION('center_axis',(0.0265579739516111,-0.987363721673672,-0.156229175067596));
#80105=DIRECTION('ref_axis',(-0.951108729662977,0.0231496319897582,-0.30798746548783));
#80106=DIRECTION('',(-0.906552294984449,0.,0.422093516247796));
#80107=DIRECTION('center_axis',(-1.44157189798803E-14,-1.,-3.54785011149324E-15));
#80108=DIRECTION('ref_axis',(1.,-1.44157189798803E-14,-6.21375054833169E-32));
#80109=DIRECTION('center_axis',(-0.00274543728995823,0.987363722329316,
0.158446654751954));
#80110=DIRECTION('ref_axis',(-0.986625637587546,0.0231492386145962,-0.16135043850741));
#80111=DIRECTION('center_axis',(0.0217105186266266,0.987363722833723,-0.156976215436906));
#80112=DIRECTION('ref_axis',(-0.971448780790989,-0.01626976712843,-0.236690855288682));
#80113=DIRECTION('',(0.422093512262599,0.,0.906552296839969));
#80114=DIRECTION('center_axis',(0.059521713817587,-0.987363721611479,-0.146867446460227));
#80115=DIRECTION('ref_axis',(-0.862664136105473,0.0231496361748456,-0.505247150038839));
#80116=DIRECTION('',(-0.976095235356397,0.,0.217343257347773));
#80117=DIRECTION('center_axis',(-5.32640183211155E-14,-1.,-2.62554272104013E-14));
#80118=DIRECTION('ref_axis',(1.,-5.32640183211155E-14,-2.10243185391532E-31));
#80119=DIRECTION('center_axis',(-0.0367425905234397,0.987363722095349,0.154152075340054));
#80120=DIRECTION('ref_axis',(-0.928873303691505,0.0231492463964906,-0.369673501999405));
#80121=DIRECTION('center_axis',(0.0549481854235957,0.987363722864592,-0.148639078608649));
#80122=DIRECTION('ref_axis',(-0.897855310311268,-0.0162697666496942,-0.439989927656328));
#80123=DIRECTION('',(0.217343253631377,0.,0.976095236183912));
#80124=DIRECTION('center_axis',(0.0897022905136939,-0.987363721638354,-0.130638356806321));
#80125=DIRECTION('ref_axis',(-0.733882324749335,0.0231496342440029,-0.678882042666382));
#80126=DIRECTION('',(-0.999997046887668,0.,0.00243027075520032));
#80127=DIRECTION('center_axis',(8.11555403438022E-14,-1.,6.49106139899144E-14));
#80128=DIRECTION('ref_axis',(1.,8.11555403438022E-14,-1.83734581581371E-30));
#80129=DIRECTION('center_axis',(-0.0690217128897,0.987363722232311,0.142649511633679));
#80130=DIRECTION('ref_axis',(-0.82768788739491,0.0231492409593687,-0.560711042964873));
#80131=DIRECTION('center_axis',(0.0856165363963591,0.987363722869809,-0.13335174335629));
#80132=DIRECTION('ref_axis',(-0.782279123826205,-0.0162697655685773,-0.62271555878591));
#80133=DIRECTION('',(0.00243026757266593,0.,0.999997046895402));
#80134=DIRECTION('center_axis',(0.115688484628851,-0.987363721599696,-0.108300765431633));
#80135=DIRECTION('ref_axis',(-0.570784992354785,0.0231496363486892,-0.82077316405903));
#80136=DIRECTION('',(-0.977140108330193,0.,-0.212596351550206));
#80137=DIRECTION('center_axis',(-2.79875595292076E-14,-1.,-3.46453208693661E-14));
#80138=DIRECTION('ref_axis',(2.42805112830695E-31,3.46453208693661E-14,
-1.));
#80139=DIRECTION('center_axis',(-0.0980734510975878,0.98736372225289,0.124476817796436));
#80140=DIRECTION('ref_axis',(-0.687800705810551,0.0231492416525541,-0.725530358908171));
#80141=DIRECTION('center_axis',(0.112281552464805,0.98736372285531,-0.111829029171298));
#80142=DIRECTION('ref_axis',(-0.630124435048572,-0.0162697654267482,-0.776323702515695));
#80143=DIRECTION('',(-0.212596357404932,0.,0.97714010705638));
#80144=DIRECTION('center_axis',(0.136265218706276,-0.987363721707863,-0.0808991423077467));
#80145=DIRECTION('ref_axis',(-0.380998386991564,0.0231496287520599,-0.924285845287305));
#80146=DIRECTION('',(-0.908593184668933,0.,-0.417682205478239));
#80147=DIRECTION('center_axis',(-5.96565182927404E-14,-1.,-1.19555491768862E-13));
#80148=DIRECTION('ref_axis',(-1.47827908722308E-30,1.19555491768862E-13,
-1.));
#80149=DIRECTION('center_axis',(-0.122539383910873,0.987363722169366,0.100483727710508));
#80150=DIRECTION('ref_axis',(-0.51575272537891,0.0231492437747636,-0.856424683656936));
#80151=DIRECTION('center_axis',(0.133696406656168,0.987363722782425,-0.0850773164859957));
#80152=DIRECTION('ref_axis',(-0.448505827915095,-0.0162697683111609,-0.893631812865509));
#80153=DIRECTION('',(-0.417682210743198,0.,0.90859318224862));
#80154=DIRECTION('center_axis',(0.150470336690132,-0.987363721658464,-0.0497147757623953));
#80155=DIRECTION('ref_axis',(-0.173396723049576,0.0231496331670833,-0.984579946433959));
#80156=DIRECTION('',(-0.797561452045313,0.,-0.603237706224812));
#80157=DIRECTION('center_axis',(-7.23575228850367E-15,-1.,-2.87966085777709E-14));
#80158=DIRECTION('ref_axis',(1.43902150932921E-33,2.87966085777709E-14,
-1.));
#80159=DIRECTION('center_axis',(-0.141275515075797,0.987363722429278,0.0717921198368483));
#80160=DIRECTION('ref_axis',(-0.319588720183942,0.0231492347253357,-0.947273541730593));
#80161=DIRECTION('center_axis',(0.148859768603231,0.987363722988668,-0.0543474729619374));
#80162=DIRECTION('ref_axis',(-0.245915584978653,-0.016269760627855,-0.969154693510648));
#80163=DIRECTION('',(-0.60323770876311,0.,0.797561450125464));
#80164=DIRECTION('',(-0.649236632677518,0.,-0.760586480809091));
#80165=DIRECTION('',(-0.760586482875992,0.,0.649236630256125));
#80166=DIRECTION('center_axis',(0.15743787146309,-0.987363721659547,0.0180609462592491));
#80167=DIRECTION('ref_axis',(0.256043784428875,0.0231496327469448,-0.966387952614798));
#80168=DIRECTION('',(-0.470554230370041,0.,-0.882371076294355));
#80169=DIRECTION('center_axis',(0.,-1.,0.));
#80170=DIRECTION('ref_axis',(0.,0.,-1.));
#80171=DIRECTION('center_axis',(-0.158362914256764,0.987363722293322,0.00583671887102137));
#80172=DIRECTION('ref_axis',(0.107698968169371,0.0231492392945268,-0.993914002806751));
#80173=DIRECTION('center_axis',(0.157921378608865,0.987363722987877,0.0131801633447803));
#80174=DIRECTION('ref_axis',(0.183750552646889,-0.0162697611016185,-0.982838251837839));
#80175=DIRECTION('',(-0.882371077791938,0.,0.470554227561812));
#80176=DIRECTION('center_axis',(0.149874493682656,-0.987363721587329,0.0514831762480454));
#80177=DIRECTION('ref_axis',(0.457802465965002,0.0231496367329827,-0.888752494497481));
#80178=DIRECTION('',(-0.269869235978793,0.,-0.962896980716121));
#80179=DIRECTION('center_axis',(-3.49998983126278E-14,-1.,8.19110133354615E-14));
#80180=DIRECTION('ref_axis',(9.01557008337089E-31,-8.19110133354614E-14,
-1.));
#80181=DIRECTION('center_axis',(-0.155915201154255,0.987363722160555,-0.0283430804656613));
#80182=DIRECTION('ref_axis',(0.318843156646597,0.023149244932748,-0.947524751084993));
#80183=DIRECTION('center_axis',(0.151395920224427,0.987363722911968,0.0468204444320834));
#80184=DIRECTION('ref_axis',(0.390735738541771,-0.0162697637311714,-0.920359102423803));
#80185=DIRECTION('',(-0.962896981574999,0.,0.269869232914305));
#80186=DIRECTION('center_axis',(0.135303149199466,-0.987363721625002,0.0824981153453359));
#80187=DIRECTION('ref_axis',(0.638154814540316,0.0231496352403355,-0.769559956772216));
#80188=DIRECTION('',(-0.0565654558858671,0.,-0.998398892828124));
#80189=DIRECTION('center_axis',(-3.45267111776215E-14,-1.,4.83146905674551E-14));
#80190=DIRECTION('ref_axis',(9.07026936983547E-31,-4.83146905674551E-14,
-1.));
#80191=DIRECTION('center_axis',(-0.14617706594016,0.987363722148467,-0.06119759454628));
#80192=DIRECTION('ref_axis',(0.515078592760366,0.0231492446704375,-0.856830295771099));
#80193=DIRECTION('center_axis',(0.137791354900117,0.987363722950062,0.0782714578692801));
#80194=DIRECTION('ref_axis',(0.579450554843935,-0.0162697613589407,-0.814844984862998));
#80195=DIRECTION('',(-0.998398893008149,0.,0.0565654527083613));
#80196=DIRECTION('center_axis',(0.114405181244365,-0.987363721617109,0.109655532185364));
#80197=DIRECTION('ref_axis',(0.78866775356503,0.0231496364833883,-0.614383649536163));
#80198=DIRECTION('',(0.159383264798036,0.,-0.987216782121495));
#80199=DIRECTION('center_axis',(7.7185020740154E-14,-1.,-6.95850708510898E-14));
#80200=DIRECTION('ref_axis',(1.,7.7185020740154E-14,-7.07954392306507E-31));
#80201=DIRECTION('center_axis',(-0.129603858059397,0.987363721960499,-0.0911905726072057));
#80202=DIRECTION('ref_axis',(0.687229526331659,0.0231492508551655,-0.726071408556217));
#80203=DIRECTION('center_axis',(0.117743826010255,0.987363722792658,0.10606257751672));
#80204=DIRECTION('ref_axis',(0.741070908158961,-0.0162697697172345,-0.671229620676711));
#80205=DIRECTION('',(-0.987216781687272,0.,-0.159383267487605));
#80206=DIRECTION('center_axis',(0.0881577516901096,-0.987363721641326,0.131685580089599));
#80207=DIRECTION('ref_axis',(0.902303462413274,0.0231496338228235,-0.430479449185309));
#80208=DIRECTION('',(0.367879397950885,0.,-0.929873512131244));
#80209=DIRECTION('center_axis',(7.74336096465508E-14,-1.,-4.40277537714319E-14));
#80210=DIRECTION('ref_axis',(1.,7.74336096465508E-14,3.13411658643789E-31));
#80211=DIRECTION('center_axis',(-0.106970507172761,0.98736372217698,-0.116919590847819));
#80212=DIRECTION('ref_axis',(0.827246372683671,0.0231492422380706,-0.561362228392249));
#80213=DIRECTION('center_axis',(0.092190715571351,0.987363722946451,0.128894338788664));
#80214=DIRECTION('ref_axis',(0.868039608686221,-0.016269762386131,-0.496228306915044));
#80215=DIRECTION('',(-0.929873511942708,0.,-0.36787939842744));
#80216=DIRECTION('center_axis',(0.0577881631569067,-0.987363721669339,0.147558155756379));
#80217=DIRECTION('ref_axis',(0.973748465835437,0.0231496316831997,-0.226446505462252));
#80218=DIRECTION('',(0.55917389836542,0.,-0.829050391343505));
#80219=DIRECTION('center_axis',(0.,-1.,0.));
#80220=DIRECTION('ref_axis',(0.,0.,-1.));
#80221=DIRECTION('center_axis',(-0.0793353368678561,0.987363722342691,-0.137181573564561));
#80222=DIRECTION('ref_axis',(0.928582098048572,0.0231492389550655,-0.370404373515639));
#80223=DIRECTION('center_axis',(0.0623268761099373,0.987363722900334,0.145699139375525));
#80224=DIRECTION('ref_axis',(0.954419742951362,-0.0162697635743861,-0.298023906856295));
#80225=DIRECTION('',(-0.829050388663707,0.,-0.559173902338581));
#80226=DIRECTION('center_axis',(0.024716470913478,-0.987363721605843,0.156531074621758));
#80227=DIRECTION('ref_axis',(0.999662072669057,0.0231496360950727,-0.011825177194063));
#80228=DIRECTION('',(0.724322051650169,0.,-0.689461794078026));
#80229=DIRECTION('center_axis',(4.438180735115E-14,-1.,-3.72248916065518E-15));
#80230=DIRECTION('ref_axis',(1.,4.438180735115E-14,-1.00930208127364E-31));
#80231=DIRECTION('center_axis',(-0.0479905464206515,0.987363722052463,-0.151029095968143));
#80232=DIRECTION('ref_axis',(0.986498355424332,0.0231492477827189,-0.162126824036563));
#80233=DIRECTION('center_axis',(0.0295487005393224,0.987363722907453,0.155691210358106));
#80234=DIRECTION('ref_axis',(0.996172270241457,-0.0162697639762549,-0.0858842405924241));
#80235=DIRECTION('',(-0.689461790264558,0.,-0.724322055280102));
#80236=DIRECTION('center_axis',(-0.00951094462361416,-0.987363721678243,
0.15818477501345));
#80237=DIRECTION('ref_axis',(0.978832592072294,0.0231496322092273,0.203349087102972));
#80238=DIRECTION('',(0.855601711026882,0.,-0.517634728440695));
#80239=DIRECTION('center_axis',(8.82888209575531E-14,-1.,1.18106344614963E-14));
#80240=DIRECTION('ref_axis',(1.,8.82888209575531E-14,1.01618340658559E-31));
#80241=DIRECTION('center_axis',(-0.0144017553818927,0.98736372226706,-0.157814667863467));
#80242=DIRECTION('ref_axis',(0.998287046995834,0.0231492401613689,0.0537315966661112));
#80243=DIRECTION('center_axis',(-0.00461113702491368,0.987363722854809,
0.15840333394733));
#80244=DIRECTION('ref_axis',(0.991344889319113,-0.0162697664504085,0.130271275116678));
#80245=DIRECTION('',(-0.517634729095432,0.,-0.855601710630769));
#80246=DIRECTION('center_axis',(-0.0432936350148198,-0.987363721689003,
0.152441930779051));
#80247=DIRECTION('ref_axis',(0.912233988122506,0.0231496315622569,0.409014969741498));
#80248=DIRECTION('',(0.946874383847733,0.,-0.321603639924949));
#80249=DIRECTION('center_axis',(1.3947623333974E-14,-1.,5.08566584326984E-15));
#80250=DIRECTION('ref_axis',(1.,1.3947623333974E-14,-6.10860190589621E-32));
#80251=DIRECTION('center_axis',(0.0198604347480238,0.987363722186016,-0.157221001277166));
#80252=DIRECTION('ref_axis',(0.963396944726995,0.0231492443313783,0.267077590556711));
#80253=DIRECTION('center_axis',(-0.0385553678039905,0.987363722908173,0.153708692982577));
#80254=DIRECTION('ref_axis',(0.940163323192753,-0.0162697641668067,0.340335452894809));
#80255=DIRECTION('',(-0.321603636911446,0.,-0.946874384871262));
#80256=DIRECTION('center_axis',(-0.0750519575388816,-0.987363721595131,
0.139571074895176));
#80257=DIRECTION('ref_axis',(0.802980336676752,0.0231496378805331,0.595555768317704));
#80258=DIRECTION('',(0.993872262844379,0.,-0.110534723723333));
#80259=DIRECTION('center_axis',(-1.2528267825801E-14,-1.,-7.96509253005815E-15));
#80260=DIRECTION('ref_axis',(1.,-1.2528267825801E-14,1.55839561051282E-31));
#80261=DIRECTION('center_axis',(0.0531939794798619,0.987363722280913,-0.149275853608936));
#80262=DIRECTION('ref_axis',(0.883459473117363,0.023149240803084,0.467935328875084));
#80263=DIRECTION('center_axis',(-0.0706967919103074,0.987363722959237,0.141826803523406));
#80264=DIRECTION('ref_axis',(0.845020764817006,-0.0162697620358347,0.534485922987107));
#80265=DIRECTION('',(-0.110534720558305,0.,-0.993872263196381));
#80266=DIRECTION('center_axis',(-0.103300941109169,-0.987363721578903,0.120174027459422));
#80267=DIRECTION('ref_axis',(0.65618021622441,0.0231496365281075,0.754249042534562));
#80268=DIRECTION('',(0.994397779862904,0.,0.105702674534415));
#80269=DIRECTION('center_axis',(-2.1046208900298E-14,-1.,-2.09441607063673E-14));
#80270=DIRECTION('ref_axis',(1.,-2.1046208900298E-14,3.70559775903116E-32));
#80271=DIRECTION('center_axis',(0.0840402285537729,0.987363722249449,-0.134350734908083));
#80272=DIRECTION('ref_axis',(0.762212418662718,0.0231492422016354,0.646912931870913));
#80273=DIRECTION('center_axis',(-0.0995325095569162,0.987363722892599,0.123313252560172));
#80274=DIRECTION('ref_axis',(0.710365975348149,-0.0162697636185344,0.70364442430781));
#80275=DIRECTION('',(0.105702677699157,0.,-0.994397779526497));
#80276=DIRECTION('center_axis',(-0.126719690076456,-0.987363721725139,0.0951577698772395));
#80277=DIRECTION('ref_axis',(0.478697837936382,0.023149628695089,0.877674469633425));
#80278=DIRECTION('',(0.948426361813909,0.,0.316997533454809));
#80279=DIRECTION('center_axis',(2.40776771854987E-14,-1.,3.74682160055375E-14));
#80280=DIRECTION('ref_axis',(-4.36064925888224E-32,-3.74682160055375E-14,
-1.));
#80281=DIRECTION('center_axis',(0.110956844829281,0.987363721895544,-0.113143533929734));
#80282=DIRECTION('ref_axis',(0.605325158041782,0.023149253813639,0.795641605931693));
#80283=DIRECTION('center_axis',(-0.123714196260695,0.987363722788117,0.0990337142874071));
#80284=DIRECTION('ref_axis',(0.542495262034564,-0.0162697688673487,0.839901294969268));
#80285=DIRECTION('',(0.316997534753807,0.,-0.948426361379738));
#80286=DIRECTION('center_axis',(-0.144213159817898,-0.987363721644968,0.0656920521428219));
#80287=DIRECTION('ref_axis',(0.278832083128177,0.0231496344178445,0.960060812576329));
#80288=DIRECTION('',(0.858107580390881,0.,0.513469941160831));
#80289=DIRECTION('center_axis',(-3.09203911029191E-14,-1.,-8.35364374290109E-14));
#80290=DIRECTION('ref_axis',(-6.00164705136111E-31,8.35364374290109E-14,
-1.));
#80291=DIRECTION('center_axis',(0.132685252824541,0.987363722069219,-0.0866458540526028));
#80292=DIRECTION('ref_axis',(0.420133565785062,0.0231492482371895,0.907166963246999));
#80293=DIRECTION('center_axis',(-0.142111149096565,0.987363722895652,0.0701234626362136));
#80294=DIRECTION('ref_axis',(0.349258074078322,-0.0162697653671039,0.936885314446758));
#80295=DIRECTION('',(0.513469942625881,0.,-0.858107579514232));
#80296=DIRECTION('center_axis',(-0.154963385615948,-0.987363721624743,0.0331546427786408));
#80297=DIRECTION('ref_axis',(0.0659284479281176,0.0231496352727361,0.997555779964473));
#80298=DIRECTION('',(0.727664643914042,0.,0.685933062330028));
#80299=DIRECTION('center_axis',(1.22396248333418E-14,-1.,8.82303721717431E-14));
#80300=DIRECTION('ref_axis',(-1.12955086660186E-31,-8.82303721717431E-14,
-1.));
#80301=DIRECTION('center_axis',(0.148209443903507,0.987363722200597,-0.0560967095291348));
#80302=DIRECTION('ref_axis',(0.215296994344091,0.0231492427667388,0.976274201638928));
#80303=DIRECTION('center_axis',(-0.153863141406208,0.987363722919929,0.0379343166316623));
#80304=DIRECTION('ref_axis',(0.139689965561605,-0.0162697632310827,0.990061618448974));
#80305=DIRECTION('center_axis',(-2.33781757796594E-15,-1.,2.95995842083303E-14));
#80306=DIRECTION('ref_axis',(1.48758021322455E-32,-2.95995842083303E-14,
-1.));
#80307=DIRECTION('center_axis',(0.156803523942189,0.987363722029914,-0.0229245566706625));
#80308=DIRECTION('ref_axis',(0.000393374217064282,0.0231492494663704,0.99973194282561));
#80309=DIRECTION('center_axis',(-0.158420663823298,0.987363722839941,0.00397140950277908));
#80310=DIRECTION('ref_axis',(-0.0764098928436923,-0.0162697670803354,0.996943741118207));
#80311=DIRECTION('',(0.68593306312575,0.,-0.727664643163955));
#80312=DIRECTION('center_axis',(0.163668138515803,-0.986495110831716,0.00633535633501474));
#80313=DIRECTION('ref_axis',(0.0266156894481207,0.0108352085748758,0.999587016387438));
#80314=DIRECTION('center_axis',(-0.160735572549809,-0.986495109335916,0.0314876955873914));
#80315=DIRECTION('ref_axis',(0.137589022940409,0.00919562022088586,0.990446718069709));
#80316=DIRECTION('center_axis',(0.161203584621629,-0.986495110673399,-0.0289965674281651));
#80317=DIRECTION('ref_axis',(0.240875086954021,0.0108352135078831,0.97049564173835));
#80318=DIRECTION('center_axis',(-0.150208740836978,-0.986495109342673,0.0653049264539607));
#80319=DIRECTION('ref_axis',(0.347289035836757,0.0091956188842569,0.937713051088077));
#80320=DIRECTION('center_axis',(0.151201330251114,-0.986495110631542,-0.0629726482717326));
#80321=DIRECTION('ref_axis',(0.443871436852541,0.0108352148540632,0.896024969331507));
#80322=DIRECTION('center_axis',(-0.132658313610887,-0.986495109357092,0.0960685746977337));
#80323=DIRECTION('ref_axis',(0.540750198857872,0.00919562137026215,0.841132963914022));
#80324=DIRECTION('center_axis',(0.134129071901824,-0.98649511055174,-0.0940041963332786));
#80325=DIRECTION('ref_axis',(0.626112849827963,0.0108352185265547,0.779657166528846));
#80326=DIRECTION('center_axis',(-0.108904931346394,-0.986495109325204,0.122340161868011));
#80327=DIRECTION('ref_axis',(0.708926482606273,0.00919562280965737,0.705222434966898));
#80328=DIRECTION('center_axis',(0.11078507982091,-0.986495110702303,-0.120640219866864));
#80329=DIRECTION('ref_axis',(0.779077926113261,0.0108352124652135,0.626833457318524));
#80330=DIRECTION('center_axis',(-0.0800592741231365,-0.986495109329498,
0.142891258990387));
#80331=DIRECTION('ref_axis',(0.843954154358249,0.00919562458933819,0.536336485641118));
#80332=DIRECTION('center_axis',(0.0822609122539169,-0.986495110548935,-0.141635232827848));
#80333=DIRECTION('ref_axis',(0.895614180534253,0.0108352201189312,0.444699716247866));
#80334=DIRECTION('center_axis',(-0.0474701448624736,-0.986495109347409,
0.156760915346842));
#80335=DIRECTION('ref_axis',(0.939519464582128,0.00919561566255652,0.342372043724219));
#80336=DIRECTION('center_axis',(0.0498903044633597,-0.986495110644867,-0.156007545312159));
#80337=DIRECTION('ref_axis',(0.970272512659709,0.0108352150321386,0.241772308778781));
#80338=DIRECTION('center_axis',(-0.0126613523898467,-0.986495109360026,
0.163300610422653));
#80339=DIRECTION('ref_axis',(0.991153890708611,0.00919561936273666,0.132398661313921));
#80340=DIRECTION('center_axis',(0.0151868873866259,-0.986495110617347,-0.163085116364352));
#80341=DIRECTION('ref_axis',(0.999561980115019,0.0108352160970614,0.0275398983417428));
#80342=DIRECTION('center_axis',(0.0227394687730209,-0.986495109360623,0.162204549157824));
#80343=DIRECTION('ref_axis',(0.996443062115871,0.00919562124663718,-0.083765532953806));
#80344=DIRECTION('center_axis',(-0.0202266525106009,-0.986495110648347,
-0.162537008693776));
#80345=DIRECTION('ref_axis',(0.982113040696751,0.0108352162892002,-0.187980247316966));
#80346=DIRECTION('center_axis',(0.0570770171920215,-0.986495109334282,0.153523983038496));
#80347=DIRECTION('ref_axis',(0.955139663050732,0.0091956222371918,-0.296012946674642));
#80348=DIRECTION('center_axis',(-0.0546944187067478,-0.986495110682322,
-0.154388850511314));
#80349=DIRECTION('ref_axis',(0.918741586296566,0.0108352146166071,-0.394710648112616));
#80350=DIRECTION('center_axis',(0.0887457096270632,-0.986495109349921,0.13766480396774));
#80351=DIRECTION('ref_axis',(0.869174995589545,0.00919562629065882,-0.494419121291882));
#80352=DIRECTION('center_axis',(-0.0866047287783385,-0.986495110539464,
-0.139021645203043));
#80353=DIRECTION('ref_axis',(0.812410797887989,0.0108352196224996,-0.582984814116744));
#80354=DIRECTION('center_axis',(0.116264741557142,-0.986495109322745,0.115368579574145));
#80355=DIRECTION('ref_axis',(0.742568672016674,0.00919561744081361,-0.669706807460754));
#80356=DIRECTION('center_axis',(-0.11446550582471,-0.986495110697102,-0.11715393526043));
#80357=DIRECTION('ref_axis',(0.668092580575766,0.0108352145780534,-0.743999262032336));
#80358=DIRECTION('center_axis',(0.138347373964608,-0.986495109335736,0.0876778385555427));
#80359=DIRECTION('ref_axis',(0.581240659621162,0.00919562299657433,-0.813679750344607));
#80360=DIRECTION('center_axis',(-0.136974001509193,-0.986495110784133,-0.0898082363124904));
#80361=DIRECTION('ref_axis',(0.492535098370621,0.0108352090189169,-0.870225128985919));
#80362=DIRECTION('center_axis',(0.153961033449504,-0.98649510932601,0.0558873818945187));
#80363=DIRECTION('ref_axis',(0.392734481097556,0.00919562464302147,-0.919605930735801));
#80364=DIRECTION('center_axis',(-0.153077740706661,-0.986495110692389,-0.0582632120652054));
#80365=DIRECTION('ref_axis',(0.293947223383176,0.0108352127995201,-0.955760235639101));
#80366=DIRECTION('center_axis',(0.162375644751377,-0.986495109354807,0.0214836963910421));
#80367=DIRECTION('ref_axis',(0.185864477196147,0.0091956233116086,-0.982532359074506));
#80368=DIRECTION('center_axis',(-0.162023736642693,-0.986495110541471,-0.0239938667602651));
#80369=DIRECTION('ref_axis',(0.0816147053940807,0.0108352178154801,-0.996605056137249));
#80370=DIRECTION('center_axis',(0.163197752475919,-0.986495109366373,-0.0139245388805864));
#80371=DIRECTION('ref_axis',(-0.0296963431688148,0.0091956180469598,-0.999516667100221));
#80372=DIRECTION('center_axis',(-0.163393682065958,-0.986495110747374,0.0113974177977136));
#80373=DIRECTION('ref_axis',(-0.134534032791039,0.0108352109294644,-0.9908497324141));
#80374=DIRECTION('center_axis',(0.156388914161848,-0.986495109361921,-0.04868168785374));
#80375=DIRECTION('ref_axis',(-0.243868596486197,0.00919562266033067,-0.969764687010071));
#80376=DIRECTION('center_axis',(-0.157123521961374,-0.98649511068723,0.0462557611184147));
#80377=DIRECTION('ref_axis',(-0.344392104001794,0.0108352142003043,-0.938763376381105));
#80378=DIRECTION('center_axis',(0.14226750324635,-0.986495109321295,-0.0811625332602162));
#80379=DIRECTION('ref_axis',(-0.446637828743146,0.00919562490842527,-0.894667586547178));
#80380=DIRECTION('center_axis',(-0.143506439863672,-0.986495110699152,0.0789512399163027));
#80381=DIRECTION('ref_axis',(-0.538146784719012,0.0108352141235931,-0.842781487831505));
#80382=DIRECTION('center_axis',(0.121493827765215,-0.98649510934329,-0.109848300199533));
#80383=DIRECTION('ref_axis',(-0.628522767255273,0.00919561739562644,-0.77773682673671));
#80384=DIRECTION('center_axis',(-0.123179159947951,-0.986495110553911,0.107955043456728));
#80385=DIRECTION('ref_axis',(-0.706738317361023,0.0108352183847782,-0.707392075737539));
#80386=DIRECTION('center_axis',(0.0950392295742507,-0.986495109351144,-0.133397691390092));
#80387=DIRECTION('ref_axis',(-0.78101868357014,0.00919562018628519,-0.624439954266025));
#80388=DIRECTION('center_axis',(-0.0970921547944209,-0.986495110583613,
0.131910993749582));
#80389=DIRECTION('ref_axis',(-0.842283554826315,0.0108352166558452,-0.538925793917091));
#80390=DIRECTION('center_axis',(0.0641407031163179,-0.986495109342318,-0.150709553271953));
#80391=DIRECTION('ref_axis',(-0.896995032092018,0.00919562221238664,-0.441944965956585));
#80392=DIRECTION('center_axis',(-0.0664652338195093,-0.986495110523081,
0.149698929880515));
#80393=DIRECTION('ref_axis',(-0.93844454810202,0.0108352208023414,-0.345259942836929));
#80394=DIRECTION('center_axis',(0.0302430298729998,-0.986495109332971,-0.160974402953483));
#80395=DIRECTION('ref_axis',(-0.971028890904804,0.00919562225295301,-0.238785120054764));
#80396=DIRECTION('center_axis',(-0.0327304542696101,-0.986495110838626,
0.160487113672068));
#80397=DIRECTION('ref_axis',(-0.990724918720199,0.0108352068721514,-0.135450115241342));
#80398=DIRECTION('center_axis',(-0.0050687708200986,-0.986495109324231,
-0.163712268452142));
#80399=DIRECTION('ref_axis',(-0.999658517458995,0.00919561933249602,-0.0244599480125467));
#80400=DIRECTION('center_axis',(0.00253474197814183,-0.986495110653344,
0.163771095557642));
#80401=DIRECTION('ref_axis',(-0.996680091659884,0.0108352157596983,0.0806932028629744));
#80402=DIRECTION('center_axis',(-0.0401435654910706,-0.986495109322325,
-0.158795130381252));
#80403=DIRECTION('ref_axis',(-0.98154522275664,0.00919562080493988,0.191008942831561));
#80404=DIRECTION('center_axis',(0.0376814241786472,-0.986495110573158,0.159397324592106));
#80405=DIRECTION('ref_axis',(-0.956031612134756,0.0108352171239012,0.293063397013166));
#80406=DIRECTION('center_axis',(-0.0733412931472915,-0.986495109333737,
-0.146452907038753));
#80407=DIRECTION('ref_axis',(-0.917535964181018,0.00919562396514639,0.397546468899299));
#80408=DIRECTION('center_axis',(0.0710661668584858,-0.986495110657146,0.14757031062374));
#80409=DIRECTION('ref_axis',(-0.870680155667432,0.0108352167935401,0.491730276273461));
#80410=DIRECTION('center_axis',(-0.103109658554887,-0.98649510935733,-0.127262710668778));
#80411=DIRECTION('ref_axis',(-0.810623745170238,0.00919562209843176,0.585495161637054));
#80412=DIRECTION('center_axis',(0.101127933530792,-0.986495110572645,0.128843074614264));
#80413=DIRECTION('ref_axis',(-0.744616664928424,0.0108352174921367,0.667404390435641));
#80414=DIRECTION('center_axis',(-0.128056733023712,-0.986495109359134,-0.102121850442517));
#80415=DIRECTION('ref_axis',(-0.665807659368194,0.00919562209060315,0.746066753890705));
#80416=DIRECTION('center_axis',(0.126461072293326,-0.986495110609015,0.104091276958878));
#80417=DIRECTION('ref_axis',(-0.583735724868433,0.0108352154539179,0.811871419387573));
#80418=DIRECTION('center_axis',(-0.147016018399577,-0.986495109320743,-0.072205883556608));
#80419=DIRECTION('ref_axis',(-0.489859148114204,0.00919562510711065,0.871753093190793));
#80420=DIRECTION('center_axis',(0.145881029487065,-0.986495110618633,0.0744722898890882));
#80421=DIRECTION('ref_axis',(-0.395559949617682,0.0108352175612732,0.91837624333323));
#80422=DIRECTION('center_axis',(-0.159100996125728,-0.986495109348092,-0.0389136513847887));
#80423=DIRECTION('ref_axis',(-0.291005366413958,0.00919562548096839,0.956677227276939));
#80424=DIRECTION('center_axis',(0.158479752759108,-0.986495110571815,0.0413710621487411));
#80425=DIRECTION('ref_axis',(-0.188888235368966,0.0108352192583513,0.981938813044286));
#80426=DIRECTION('center_axis',(-0.163746588080474,-0.986495109318213,-0.00380186575922749));
#80427=DIRECTION('ref_axis',(-0.078544499883981,0.00919562065573288,0.996868196954207));
#80428=DIRECTION('center_axis',(-0.163785826049748,0.986495107503612,-0.00126730289954508));
#80429=DIRECTION('ref_axis',(-0.0773835475264423,-0.0115671232882696,0.996934294841469));
#80430=DIRECTION('center_axis',(-0.15968413796074,0.986495109554075,-0.0364468779133307));
#80431=DIRECTION('ref_axis',(-0.289885795065082,-0.0115670281141406,0.956991342531421));
#80432=DIRECTION('center_axis',(-0.148115829760526,0.986495109166574,-0.0699221035494464));
#80433=DIRECTION('ref_axis',(-0.488833270659318,-0.0115670686396249,0.872300542484986));
#80434=DIRECTION('center_axis',(-0.129621778541751,0.986495109136216,-0.100127889111863));
#80435=DIRECTION('ref_axis',(-0.66492345234669,-0.0115670683985371,0.746821936908673));
#80436=DIRECTION('center_axis',(-0.105066761514118,0.986495109034855,-0.125651802514903));
#80437=DIRECTION('ref_axis',(-0.809922550492909,-0.0115670734541557,0.586422769863831));
#80438=DIRECTION('center_axis',(-0.0755989299477404,0.986495109165786,-0.14530038328491));
#80439=DIRECTION('ref_axis',(-0.917050572988009,-0.0115670674832961,0.398603122832976));
#80440=DIRECTION('center_axis',(-0.0425961838796048,0.986495109110088,-0.158154876057523));
#80441=DIRECTION('ref_axis',(-0.981298328950922,-0.0115670697713018,0.192145238023309));
#80442=DIRECTION('center_axis',(-0.00760168522970371,0.986495109123514,
-0.163614223272475));
#80443=DIRECTION('ref_axis',(-0.999661665709804,-0.0115670697656513,-0.0232971459054031));
#80444=DIRECTION('center_axis',(0.027748260597412,0.986495109147497,-0.161423150947704));
#80445=DIRECTION('ref_axis',(-0.971281934258545,-0.0115670683292826,-0.237650178020647));
#80446=DIRECTION('center_axis',(0.0618007301690269,0.986495109234294,-0.151684109937044));
#80447=DIRECTION('ref_axis',(-0.897486138513145,-0.0115670653616409,-0.440890954971502));
#80448=DIRECTION('center_axis',(0.0929634596254936,0.986495109112267,-0.134852493013792));
#80449=DIRECTION('ref_axis',(-0.78172489008437,-0.0115670700835441,-0.623516157859813));
#80450=DIRECTION('center_axis',(0.119779323731273,0.986495109049208,-0.111715323158778));
#80451=DIRECTION('ref_axis',(-0.629411051229153,-0.01156707348397,-0.776986442225107));
#80452=DIRECTION('center_axis',(0.140994442093736,0.98649510906358,-0.0833544665408682));
#80453=DIRECTION('ref_axis',(-0.447666654717905,-0.0115670726511384,-0.894125700941407));
#80454=DIRECTION('center_axis',(0.155616817660157,0.98649510916704,-0.0510960433970798));
#80455=DIRECTION('ref_axis',(-0.244989860530128,-0.0115670679347961,-0.969456637079153));
#80456=DIRECTION('center_axis',(0.162962722044672,0.986495109086415,-0.0164484337361611));
#80457=DIRECTION('ref_axis',(-0.0308576148295037,-0.0115670710205182,-0.999456857735761));
#80458=DIRECTION('center_axis',(0.162688670639839,0.986495109142254,0.0189682915375994));
#80459=DIRECTION('ref_axis',(0.184717500858052,-0.0115670691724926,-0.982723586664894));
#80460=DIRECTION('center_axis',(0.154807480106536,0.986495109045727,0.0534980740954653));
#80461=DIRECTION('ref_axis',(0.391655430727299,-0.0115670742698257,-0.920039252627109));
#80462=DIRECTION('center_axis',(0.139687659558307,0.986495109146884,0.0855263549813787));
#80463=DIRECTION('ref_axis',(0.580279987484035,-0.0115670691065026,-0.81433490594338));
#80464=DIRECTION('center_axis',(0.118036205631609,0.986495109050785,0.113555510561892));
#80465=DIRECTION('ref_axis',(0.741771295505608,-0.0115670741590964,-0.670553165647087));
#80466=DIRECTION('center_axis',(0.0908655060555755,0.986495109046781,0.13627494133568));
#80467=DIRECTION('ref_axis',(0.868578204792008,-0.0115670736825183,-0.495417102012755));
#80468=DIRECTION('center_axis',(0.0594460303999144,0.98649510918911,0.152622308381373));
#80469=DIRECTION('ref_axis',(0.954771361534156,-0.0115670668654126,-0.297115886748495));
#80470=DIRECTION('center_axis',(0.0252469304063644,0.986495109178945,0.161833223013932));
#80471=DIRECTION('ref_axis',(0.996320470721413,-0.0115670669916884,-0.0849218616298022));
#80472=DIRECTION('center_axis',(-0.0101326829954701,0.986495109072926,0.16347699688491));
#80473=DIRECTION('ref_axis',(0.991282741819984,-0.0115670719871803,0.131243013587384));
#80474=DIRECTION('center_axis',(-0.0450385103095808,0.986495109124808,0.157476767371973));
#80475=DIRECTION('ref_axis',(0.939893734132406,-0.0115670697918787,0.341271111339756));
#80476=DIRECTION('center_axis',(-0.0778383841323234,0.986495109096431,0.144113100322244));
#80477=DIRECTION('ref_axis',(0.844556339406886,-0.0115670710113924,0.535341752935316));
#80478=DIRECTION('center_axis',(-0.106998623258878,0.98649510911199,0.124010863712931));
#80479=DIRECTION('ref_axis',(0.709728428982206,-0.0115670700803942,0.704380408574944));
#80480=DIRECTION('center_axis',(-0.131155746156512,0.986495109479997,0.0981099853336883));
#80481=DIRECTION('ref_axis',(0.541714399859645,-0.0115670322937331,0.840483023474371));
#80482=DIRECTION('center_axis',(-0.149180131415552,0.986495109199563,0.0676216527170227));
#80483=DIRECTION('ref_axis',(0.348370418284784,-0.0115670670447902,0.937285577945199));
#80484=DIRECTION('center_axis',(-0.160229038678211,0.986495109002492,0.0339713861715604));
#80485=DIRECTION('ref_axis',(0.138737020809764,-0.0115670753660123,0.990261703704787));
#80486=DIRECTION('center_axis',(-0.158467690734171,0.987363722391381,-0.000933112434262052));
#80487=DIRECTION('ref_axis',(0.132986651957032,0.0222802173076005,0.990867368681594));
#80488=DIRECTION('',(-0.726917198560946,0.,-0.686725117085655));
#80489=DIRECTION('center_axis',(-6.0717653292393E-15,-1.,-4.41218244212294E-14));
#80490=DIRECTION('ref_axis',(1.22893474481546E-32,4.41218244212294E-14,
-1.));
#80491=DIRECTION('center_axis',(-0.158463159478122,-0.987363721657774,0.00151929007160298));
#80492=DIRECTION('ref_axis',(0.0598900529342102,-0.00807590308752957,0.998172310449883));
#80493=DIRECTION('center_axis',(0.156803528780472,-0.98736372200041,-0.0229245248475905));
#80494=DIRECTION('ref_axis',(0.136667846576374,-0.00129577614547245,0.990616081373787));
#80495=DIRECTION('center_axis',(0.156429986048559,0.987363722317839,-0.0253483592271716));
#80496=DIRECTION('ref_axis',(0.104936288763291,0.00890473956681993,0.994439078533137));
#80497=DIRECTION('',(-0.514404155191573,0.,0.857547879200715));
#80498=DIRECTION('center_axis',(-0.154963395216921,0.987363722410324,0.0331545745089898));
#80499=DIRECTION('ref_axis',(0.342884692245767,0.0222802151330409,0.939113241221287));
#80500=DIRECTION('',(-0.857547878362246,0.,-0.514404156589359));
#80501=DIRECTION('center_axis',(-2.05529318053831E-14,-1.,-5.5713374170716E-14));
#80502=DIRECTION('ref_axis',(5.90908953540761E-31,5.5713374170716E-14,-1.));
#80503=DIRECTION('center_axis',(-0.154431776448159,-0.987363721641073,0.0355486653779795));
#80504=DIRECTION('ref_axis',(0.273067397311036,-0.00807590271631994,0.961961005613582));
#80505=DIRECTION('center_axis',(0.148209454900557,-0.98736372199961,-0.0560966840121288));
#80506=DIRECTION('ref_axis',(0.346425803548562,-0.00129577417114879,0.93807648068003));
#80507=DIRECTION('center_axis',(0.147323593750353,0.987363722328396,-0.0583835469485666));
#80508=DIRECTION('ref_axis',(0.316257941884345,0.00890473470050748,0.94863144576542));
#80509=DIRECTION('',(-0.318030226197861,0.,0.948080574225913));
#80510=DIRECTION('center_axis',(-0.144213183568975,0.987363722413158,0.0656919884562336));
#80511=DIRECTION('ref_axis',(0.536749825063267,0.0222802148207466,0.843447222606189));
#80512=DIRECTION('',(-0.948080573707219,0.,-0.318030227744142));
#80513=DIRECTION('center_axis',(-4.0061430327584E-14,-1.,-6.24906920732847E-14));
#80514=DIRECTION('ref_axis',(-6.88142309551226E-31,6.24906920732847E-14,
-1.));
#80515=DIRECTION('center_axis',(-0.143179334387656,-0.987363721660589,0.0679158254964088));
#80516=DIRECTION('ref_axis',(0.473476414686258,-0.00807590141090528,0.880769472990662));
#80517=DIRECTION('center_axis',(0.132685267518502,-0.987363722025356,-0.0866458320508252));
#80518=DIRECTION('ref_axis',(0.539985276142485,-0.00129578075687071,0.841673465485015));
#80519=DIRECTION('center_axis',(0.131328513345755,0.987363722333517,-0.088688789607791));
#80520=DIRECTION('ref_axis',(0.512791724826885,0.00890473470595383,0.858466861706895));
#80521=DIRECTION('',(-0.106785558236527,0.,0.994282074942575));
#80522=DIRECTION('center_axis',(-0.126719725305287,0.987363722365704,0.0951577163171387));
#80523=DIRECTION('ref_axis',(0.705517132930511,0.0222802169333673,0.70834254924783));
#80524=DIRECTION('',(-0.994282074768412,0.,-0.106785559858167));
#80525=DIRECTION('center_axis',(-3.15350807326005E-14,-1.,-3.14506026353153E-14));
#80526=DIRECTION('ref_axis',(1.,-3.15350807326005E-14,-6.58499687751044E-31));
#80527=DIRECTION('center_axis',(-0.125231991468926,-0.98736372154303,0.097107310195598));
#80528=DIRECTION('ref_axis',(0.651746198497286,-0.00807590874348845,0.758394140564326));
#80529=DIRECTION('center_axis',(0.110956868842192,-0.987363722031639,-0.113143509193262));
#80530=DIRECTION('ref_axis',(0.708295635388373,-0.00129577826698679,0.705914735537136));
#80531=DIRECTION('center_axis',(0.109192655757456,0.98736372233894,-0.114847044966885));
#80532=DIRECTION('ref_axis',(0.685347939677784,0.00890473688211755,0.72816131951682));
#80533=DIRECTION('',(0.109452286018412,0.,0.993992050815973));
#80534=DIRECTION('center_axis',(-0.103300990893775,0.98736372240331,0.120173977891405));
#80535=DIRECTION('ref_axis',(0.841295244695768,0.0222802153147481,0.540116564509751));
#80536=DIRECTION('',(-0.993992051028922,-7.48052486139887E-15,0.10945228408451));
#80537=DIRECTION('center_axis',(-2.50391719930817E-14,-1.,-1.59574632360699E-14));
#80538=DIRECTION('ref_axis',(1.,-2.50391719930817E-14,-2.12206039582561E-32));
#80539=DIRECTION('center_axis',(-0.101428934423903,-0.987363721560199,0.121758172655575));
#80540=DIRECTION('ref_axis',(0.799541057122385,-0.0080759069910923,0.600557139414636));
#80541=DIRECTION('center_axis',(0.0840402479765299,-0.987363722025756,-0.134350724402548));
#80542=DIRECTION('ref_axis',(0.843486878181686,-0.00129577952144824,0.537148217246176));
#80543=DIRECTION('center_axis',(0.0819510725694751,0.987363722321965,-0.135635178133206));
#80544=DIRECTION('ref_axis',(0.825858045362074,0.00890473659936113,0.563807763849373));
#80545=DIRECTION('',(0.320572261549181,0.,0.947224062788337));
#80546=DIRECTION('center_axis',(-0.0750520230763435,0.987363722323689,0.139571034499487));
#80547=DIRECTION('ref_axis',(0.937735324337171,0.022280220396402,0.346635331824884));
#80548=DIRECTION('',(-0.947224063311177,0.,0.320572260004299));
#80549=DIRECTION('center_axis',(5.57683059679842E-14,-1.,2.04034095930511E-14));
#80550=DIRECTION('ref_axis',(1.,5.57683059679842E-14,-5.27596941019497E-31));
#80551=DIRECTION('center_axis',(-0.0728831738933898,-0.987363721586963,
0.140715756961213));
#80552=DIRECTION('ref_axis',(0.909950264086116,-0.00807590654910975,0.414638754367001));
#80553=DIRECTION('center_axis',(0.053194000405138,-0.987363721999171,-0.149275848015821));
#80554=DIRECTION('ref_axis',(0.939237612569815,-0.00129577834127603,0.343265244516022));
#80555=DIRECTION('center_axis',(0.0508775475537803,0.987363722317756,-0.150081161395219));
#80556=DIRECTION('ref_axis',(0.927751945958066,0.00890473735634552,0.373091185132585));
#80557=DIRECTION('',(0.516702631843025,0.,0.856164931684597));
#80558=DIRECTION('center_axis',(-0.0432936966707817,0.987363722432758,0.152441908451404));
#80559=DIRECTION('ref_axis',(0.99032794366912,0.0222802153308313,0.136945814075875));
#80560=DIRECTION('',(-0.85616493303156,8.72727902552676E-15,0.516702629611138));
#80561=DIRECTION('center_axis',(0.,-1.,0.));
#80562=DIRECTION('ref_axis',(0.,0.,-1.));
#80563=DIRECTION('center_axis',(-0.040929475115219,-0.987363721612732,0.153093629226847));
#80564=DIRECTION('ref_axis',(0.977811208330937,-0.00807590414837374,0.209332321046173));
#80565=DIRECTION('center_axis',(0.0198604574058036,-0.987363722030831,-0.157220999389572));
#80566=DIRECTION('ref_axis',(0.991070639694408,-0.0012957806161101,0.133331571986204));
#80567=DIRECTION('center_axis',(0.0174250494756002,0.98736372231966,-0.157509515578703));
#80568=DIRECTION('ref_axis',(0.986265197685215,0.00890473293361446,0.16492927443703));
#80569=DIRECTION('',(0.688672563156092,0.,0.725072479657047));
#80570=DIRECTION('center_axis',(-0.00951101165175448,0.98736372237897,0.158184766609506));
#80571=DIRECTION('ref_axis',(0.99661392865015,0.0222802169467632,-0.0791471361030735));
#80572=DIRECTION('',(-0.725072479416792,0.,0.688672563409046));
#80573=DIRECTION('center_axis',(-5.91811130109693E-14,-1.,4.89887086351612E-15));
#80574=DIRECTION('ref_axis',(1.,-5.91811130109693E-14,1.32477618157157E-31));
#80575=DIRECTION('center_axis',(-0.00706196155846046,-0.98736372164178,
0.158313012366767));
#80576=DIRECTION('ref_axis',(0.999950786861993,-0.00807590397254324,-0.00576225902811757));
#80577=DIRECTION('center_axis',(-0.0144017381581722,-0.987363722014211,
-0.1578146710172));
#80578=DIRECTION('ref_axis',(0.996562305425301,-0.00129578193788791,-0.0828365399722749));
#80579=DIRECTION('center_axis',(-0.016842231762191,0.987363722303819,-0.15757290093038));
#80580=DIRECTION('ref_axis',(0.998661784202103,0.00890473654962193,-0.0509445428015075));
#80581=DIRECTION('',(0.828440931287242,0.,0.560076444218043));
#80582=DIRECTION('center_axis',(0.0247164028032826,0.987363722445006,0.156531080083181));
#80583=DIRECTION('ref_axis',(0.956299353761225,0.0222802136408306,-0.291539256492126));
#80584=DIRECTION('',(-0.560076443596154,0.,0.828440931707677));
#80585=DIRECTION('center_axis',(1.41860947647529E-14,-1.,-4.37663197613812E-15));
#80586=DIRECTION('ref_axis',(1.,1.41860947647529E-14,8.39717137422895E-32));
#80587=DIRECTION('center_axis',(0.0271357593812573,-0.987363721605125,0.156129855635876));
#80588=DIRECTION('ref_axis',(0.975333777955869,-0.00807590569621869,-0.220587400649986));
#80589=DIRECTION('center_axis',(-0.0479905184904216,-0.987363721986366,
-0.151029105275279));
#80590=DIRECTION('ref_axis',(0.955455825497261,-0.00129577751323549,-0.295131303802195));
#80591=DIRECTION('center_axis',(-0.0503219877413723,0.987363722316606,-0.150268351301443));
#80592=DIRECTION('ref_axis',(0.964362055625514,0.00890473870083696,-0.264436251861207));
#80593=DIRECTION('',(0.929472323171464,0.,0.368891854692188));
#80594=DIRECTION('center_axis',(0.0577881016916056,0.987363722440046,0.147558174670931));
#80595=DIRECTION('ref_axis',(0.871269283997801,0.0222802142335214,-0.490299323694892));
#80596=DIRECTION('',(-0.368891856208104,0.,0.929472322569822));
#80597=DIRECTION('center_axis',(0.,-1.,0.));
#80598=DIRECTION('ref_axis',(0.,0.,-1.));
#80599=DIRECTION('center_axis',(0.0600646429832507,-0.987363721595286,0.146646240800101));
#80600=DIRECTION('ref_axis',(0.905111246041376,-0.00807590689066388,-0.425098120458466));
#80601=DIRECTION('center_axis',(-0.0793353189735047,-0.987363722004232,
-0.13718158634934));
#80602=DIRECTION('ref_axis',(0.869673293108132,-0.00129577632919989,-0.493626057069682));
#80603=DIRECTION('center_axis',(-0.0814487385771656,0.98736372231045,-0.13593742254965));
#80604=DIRECTION('ref_axis',(0.884969829016108,0.00890473544351639,-0.465563215275737));
#80605=DIRECTION('',(0.987042621082438,0.,0.160458294166147));
#80606=DIRECTION('center_axis',(0.0881576954790623,0.987363722466547,0.131685611533014));
#80607=DIRECTION('ref_axis',(0.74549963072673,0.0222802120580983,-0.666133539717793));
#80608=DIRECTION('',(-0.160458295774993,0.,0.987042620820897));
#80609=DIRECTION('center_axis',(-5.51862541569629E-14,-1.,4.96435508966708E-14));
#80610=DIRECTION('ref_axis',(1.,-5.51862541569629E-14,1.09452219029166E-30));
#80611=DIRECTION('center_axis',(0.0901849711692664,-0.987363721572303,0.130305611153511));
#80612=DIRECTION('ref_axis',(0.792566717847699,-0.00807590799570002,-0.609731725818963));
#80613=DIRECTION('center_axis',(-0.10697049376863,-0.987363722044528,-0.116919604229878));
#80614=DIRECTION('ref_axis',(0.743225803750709,-0.0012957826187869,-0.66903940510744));
#80615=DIRECTION('center_axis',(-0.108767041434322,0.987363722333227,-0.115250208320414));
#80616=DIRECTION('ref_axis',(0.764197398165913,0.00890473803425694,-0.644920958162309));
#80617=DIRECTION('',(0.998459903193811,0.,-0.055478119238171));
#80618=DIRECTION('center_axis',(0.114405127522865,0.987363722361241,0.109655581533414));
#80619=DIRECTION('ref_axis',(0.584871244104147,0.0222802183373292,-0.810820090828358));
#80620=DIRECTION('',(0.0554781176097552,0.,0.998459903284292));
#80621=DIRECTION('center_axis',(3.45793073442067E-14,-1.,-4.82770604581073E-14));
#80622=DIRECTION('ref_axis',(2.10113896538771E-31,4.82770604581073E-14,
-1.));
#80623=DIRECTION('center_axis',(0.11608835273895,-0.987363721603576,0.107872033537397));
#80624=DIRECTION('ref_axis',(0.642962649087655,-0.00807590594756614,-0.765854954688753));
#80625=DIRECTION('center_axis',(-0.129603838858782,-0.987363722017638,-0.0911905992772433));
#80626=DIRECTION('ref_axis',(0.582025902704371,-0.00129577722766678,-0.813169213351402));
#80627=DIRECTION('center_axis',(-0.130999516830708,0.987363722332075,-0.0891740231943745));
#80628=DIRECTION('ref_axis',(0.60769194540039,0.00890473868257953,-0.794122915627351));
#80629=DIRECTION('',(0.963190309714462,0.,-0.268820436857317));
#80630=DIRECTION('center_axis',(0.135303108987166,0.987363722411206,0.0824981718869856));
#80631=DIRECTION('ref_axis',(0.396894927700357,0.0222802155771096,-0.917593596511858));
#80632=DIRECTION('',(0.268820435286404,0.,0.963190310152894));
#80633=DIRECTION('center_axis',(0.,-1.,0.));
#80634=DIRECTION('ref_axis',(0.,0.,-1.));
#80635=DIRECTION('center_axis',(0.136563571924955,-0.987363721660594,0.0803944772458867));
#80636=DIRECTION('ref_axis',(0.463294363871762,-0.00807590150730855,-0.886167654690411));
#80637=DIRECTION('center_axis',(-0.146177057117807,-0.987363722025451,-0.0611976176041577));
#80638=DIRECTION('ref_axis',(0.393611115932371,-0.0012957790850932,-0.919276133907019));
#80639=DIRECTION('center_axis',(-0.147106599459718,0.987363722334265,-0.058928161464812));
#80640=DIRECTION('ref_axis',(0.422771490401496,0.00890473699170785,-0.906192569249388));
#80641=DIRECTION('',(0.882883007870352,0.,-0.469593009332337));
#80642=DIRECTION('center_axis',(0.149874467126569,0.987363722530107,0.0514832354754118));
#80643=DIRECTION('ref_axis',(0.190360243209039,0.0222802096345352,-0.981461446040565));
#80644=DIRECTION('',(0.469593007892378,-7.4805248730079E-15,0.882883008636246));
#80645=DIRECTION('center_axis',(5.55615891691316E-15,-1.,-2.91672738458947E-14));
#80646=DIRECTION('ref_axis',(-1.32900262527756E-31,2.91672738458947E-14,
-1.));
#80647=DIRECTION('center_axis',(0.150653224989841,-0.987363721911679,0.0491577710324375));
#80648=DIRECTION('ref_axis',(0.26196294939556,-0.0080759051180692,-0.965044140389704));
#80649=DIRECTION('center_axis',(-0.155915196790453,-0.987363722007203,-0.0283431098131091));
#80650=DIRECTION('ref_axis',(0.186791512180786,-0.00129577424341934,-0.982398723506055));
#80651=DIRECTION('center_axis',(-0.156335141249754,0.987363722339936,-0.0259268859959211));
#80652=DIRECTION('ref_axis',(0.218082714256815,0.0089047345844343,-0.975889663560569));
#80653=DIRECTION('',(0.761293077687916,0.,-0.648407934763649));
#80654=DIRECTION('',(0.648407931855868,0.,0.761293080164529));
#80655=DIRECTION('',(0.604105932750183,0.,-0.796904023089375));
#80656=DIRECTION('center_axis',(0.157639632770391,0.98736372244931,-0.0162057326603608));
#80657=DIRECTION('ref_axis',(-0.239338686253989,0.022280213284518,-0.970680475418256));
#80658=DIRECTION('',(0.796904023488083,-8.72727902989815E-15,0.60410593222423));
#80659=DIRECTION('center_axis',(3.60219357573548E-15,-1.,1.44022356936135E-14));
#80660=DIRECTION('ref_axis',(1.45198767877956E-32,-1.44022356936135E-14,
-1.));
#80661=DIRECTION('center_axis',(0.157369977048825,-0.987363721673261,-0.0186432681464133));
#80662=DIRECTION('ref_axis',(-0.16746038604,-0.00807590017643478,-0.985845727760523));
#80663=DIRECTION('center_axis',(-0.153405762942724,-0.987363721993325,0.039743582971959));
#80664=DIRECTION('ref_axis',(-0.242971131641253,-0.00129577523006141,-0.970032654169705));
#80665=DIRECTION('center_axis',(-0.152772346323586,0.987363722329941,0.0421128249533245));
#80666=DIRECTION('ref_axis',(-0.211838925404961,0.00890474194803155,-0.977264025355538));
#80667=DIRECTION('',(0.418671461608696,0.,-0.908137768862433));
#80668=DIRECTION('center_axis',(0.150470352701532,0.987363722429834,-0.0497147119812497));
#80669=DIRECTION('ref_axis',(-0.442410689753908,0.0222802142789809,-0.896535762612487));
#80670=DIRECTION('',(0.908137769272627,0.,0.418671460718947));
#80671=DIRECTION('center_axis',(3.30701562051688E-14,-1.,6.64557714523879E-14));
#80672=DIRECTION('ref_axis',(5.24569482125142E-31,-6.6455771452388E-14,
-1.));
#80673=DIRECTION('center_axis',(0.1496830060805,-0.987363721564142,-0.0520372849955869));
#80674=DIRECTION('ref_axis',(-0.375472943297379,-0.00807590774965808,-0.926798170350817));
#80675=DIRECTION('center_axis',(-0.141275524388632,-0.987363722030693,0.0717921069924385));
#80676=DIRECTION('ref_axis',(-0.445818949253545,-0.0012957780307353,-0.895122218161163));
#80677=DIRECTION('center_axis',(-0.140147603738348,0.987363722333552,0.0739697842773073));
#80678=DIRECTION('ref_axis',(-0.41696912465906,0.00890473688020523,-0.908877029494173));
#80679=DIRECTION('',(0.21366037648181,0.,-0.976908001564964));
#80680=DIRECTION('center_axis',(0.136265245926737,0.987363722431167,-0.0808990876301783));
#80681=DIRECTION('ref_axis',(-0.624796061376071,0.0222802142679187,-0.780470033852117));
#80682=DIRECTION('',(0.976908000747675,0.,0.213660380218656));
#80683=DIRECTION('center_axis',(4.65830207759487E-14,-1.,5.77929664104324E-14));
#80684=DIRECTION('ref_axis',(1.2425862598362E-30,-5.77929664104324E-14,
-1.));
#80685=DIRECTION('center_axis',(0.134997021497864,-0.987363721572367,-0.0829981054571122));
#80686=DIRECTION('ref_axis',(-0.565928805917978,-0.00807590600271466,-0.824414559778323));
#80687=DIRECTION('center_axis',(-0.122539404214696,-0.987363722008594,0.100483704529859));
#80688=DIRECTION('ref_axis',(-0.627820766522833,-0.00129577208819613,-0.778356862947439));
#80689=DIRECTION('center_axis',(-0.120969711832747,0.987363722336905,0.102368005900832));
#80690=DIRECTION('ref_axis',(-0.602602313497365,0.00890473952221489,-0.797991953206087));
#80691=DIRECTION('',(-0.00134122641154887,0.,-0.999999100555452));
#80692=DIRECTION('center_axis',(0.115688527292004,0.987363722456973,-0.108300712042521));
#80693=DIRECTION('ref_axis',(-0.777966662680144,0.0222802135997342,-0.627910394754115));
#80694=DIRECTION('',(0.99999910056149,0.,-0.00134122190964533));
#80695=DIRECTION('center_axis',(-6.95012580428984E-14,-1.,-5.57133917663028E-14));
#80696=DIRECTION('ref_axis',(1.,-6.95012580428984E-14,1.85482578544888E-31));
#80697=DIRECTION('center_axis',(0.113998724849479,-0.987363721657277,-0.110078026362143));
#80698=DIRECTION('ref_axis',(-0.729922464896629,-0.00807590335540471,-0.683482241923097));
#80699=DIRECTION('center_axis',(-0.0980734700468536,-0.987363722015549,
0.124476804749198));
#80700=DIRECTION('ref_axis',(-0.78046638447579,-0.00129577794930648,-0.625196404070588));
#80701=DIRECTION('center_axis',(-0.0961354113899496,0.987363722329988,0.125979611459777));
#80702=DIRECTION('ref_axis',(-0.760058487094582,0.00890474036853936,-0.649793660937427));
#80703=DIRECTION('',(-0.216280117331432,0.,-0.976331352998101));
#80704=DIRECTION('center_axis',(0.0897023422704652,0.987363722433392,-0.130638315258841));
#80705=DIRECTION('ref_axis',(-0.894760409380084,0.0222802141144841,-0.445990360731033));
#80706=DIRECTION('',(0.976331353957897,0.,-0.216280112998722));
#80707=DIRECTION('center_axis',(0.,-1.,0.));
#80708=DIRECTION('ref_axis',(0.,0.,-1.));
#80709=DIRECTION('center_axis',(0.087669977412081,-0.987363721614985,-0.132010818871684));
#80710=DIRECTION('ref_axis',(-0.859785762310091,-0.00807590481960915,-0.510591052301351));
#80711=DIRECTION('center_axis',(-0.0690217288581476,-0.987363722016549,
0.142649505400682));
#80712=DIRECTION('ref_axis',(-0.896618260249722,-0.00129578297260527,-0.442802457460716));
#80713=DIRECTION('center_axis',(-0.0668059282075274,0.987363722329631,0.143700549002799));
#80714=DIRECTION('ref_axis',(-0.881975171793268,0.00890473817595887,-0.471211737946173));
#80715=DIRECTION('',(-0.421105986980058,0.,-0.907011437485521));
#80716=DIRECTION('center_axis',(0.0595217777845465,0.987363722389193,-0.146867415307565));
#80717=DIRECTION('ref_axis',(-0.969716151761567,0.0222802164264929,-0.243216317233707));
#80718=DIRECTION('',(0.907011438172321,0.,-0.421105985500774));
#80719=DIRECTION('center_axis',(1.44118465794018E-14,-1.,3.56354735319859E-15));
#80720=DIRECTION('ref_axis',(1.,1.44118465794018E-14,-4.86129465338419E-32));
#80721=DIRECTION('center_axis',(0.0572418778963929,-0.987363721629328,-0.147770932950893));
#80722=DIRECTION('ref_axis',(-0.949446432501417,-0.00807590462824617,-0.313825192702509));
#80723=DIRECTION('center_axis',(-0.0367426193502507,-0.987363722021711,
0.154152068940755));
#80724=DIRECTION('ref_axis',(-0.970845262562338,-0.00129577570246486,-0.239703560936405));
#80725=DIRECTION('center_axis',(-0.0343526754374338,0.987363722316262,0.154702209241063));
#80726=DIRECTION('ref_axis',(-0.96265167765723,0.00890473481807808,-0.270596476698312));
#80727=DIRECTION('',(-0.606241413488836,0.,-0.795280672826304));
#80728=DIRECTION('center_axis',(0.0265580410445182,0.987363722324339,-0.156229159550013));
#80729=DIRECTION('ref_axis',(-0.999329045759756,0.0222802188112533,-0.0290697463115691));
#80730=DIRECTION('',(0.795280674871624,0.,-0.60624141080574));
#80731=DIRECTION('center_axis',(-5.93638519600052E-14,-1.,-1.52845037480549E-15));
#80732=DIRECTION('ref_axis',(-0.999668706664393,5.9383525325444E-14,-0.025738626924135));
#80733=DIRECTION('center_axis',(0.0241372132342312,-0.987363721571971,-0.156621442532088));
#80734=DIRECTION('ref_axis',(-0.994712042298421,-0.00807590568879488,-0.102385216969101));
#80735=DIRECTION('center_axis',(-0.00274545648193553,-0.987363722011253,
0.158446656401424));
#80736=DIRECTION('ref_axis',(-0.99967661984729,-0.00129577844027622,-0.0253963912580066));
#80737=DIRECTION('center_axis',(-0.000293120077989504,0.987363722326222,
0.158470167270459));
#80738=DIRECTION('ref_axis',(-0.998315660024052,0.0089047418167306,-0.0573284268397376));
#80739=DIRECTION('',(-0.763029661124908,0.,-0.646363470690918));
#80740=DIRECTION('center_axis',(-0.00764752348920133,0.987363722381642,
-0.158285801982208));
#80741=DIRECTION('ref_axis',(-0.982214424081302,0.0222802177426303,0.18643609367281));
#80742=DIRECTION('',(0.646363471935383,0.,-0.76302966007072));
#80743=DIRECTION('center_axis',(0.,-1.,0.));
#80744=DIRECTION('ref_axis',(0.,0.,-1.));
#80745=DIRECTION('center_axis',(-0.010096086717736,-0.98736372167545,-0.158148506639151));
#80746=DIRECTION('ref_axis',(-0.993466022793342,-0.00807590057927945,0.113842177531057));
#80747=DIRECTION('center_axis',(0.0313800754379938,-0.98736372201349,0.155332454165809));
#80748=DIRECTION('ref_axis',(-0.981764209494793,-0.00129577561140111,0.190098284896603));
#80749=DIRECTION('center_axis',(0.033780129177532,0.98736372232979,0.15482823611929));
#80750=DIRECTION('ref_axis',(-0.987299512398128,0.0089047368247926,0.158620233515461));
#80751=DIRECTION('',(-0.884139492153183,0.,-0.467223028558216));
#80752=DIRECTION('center_axis',(-0.0414954970019995,0.987363722357152,-0.152941176605865));
#80753=DIRECTION('ref_axis',(-0.919172548808744,0.0222802174733878,0.393224385593997));
#80754=DIRECTION('',(0.46722303224745,0.,-0.884139490203609));
#80755=DIRECTION('center_axis',(0.0662738630982185,0.987363722324091,0.143946708570755));
#80756=DIRECTION('ref_axis',(-0.930118336104512,0.00890473695795505,0.367151993732682));
#80757=DIRECTION('',(-0.963907941868057,0.,-0.266235759438296));
#80758=DIRECTION('center_axis',(-5.45189523126693E-14,-1.,2.35390503939764E-14));
#80759=DIRECTION('ref_axis',(1.,-5.45189523126693E-14,-2.16299130535504E-31));
#80760=DIRECTION('center_axis',(-0.0438572997935655,-0.98736372164247,-0.152280722480383));
#80761=DIRECTION('ref_axis',(-0.945766635917038,-0.00807590093282602,0.324746439873159));
#80762=DIRECTION('center_axis',(0.0640383176205965,-0.987363721999432,0.144955077026479));
#80763=DIRECTION('ref_axis',(-0.917945595484297,-0.00129578079888721,0.396704177798899));
#80764=DIRECTION('',(0.266235760272643,0.,-0.963907941637607));
#80765=DIRECTION('center_axis',(-0.0734031917968273,0.987363722454611,-0.140445188648852));
#80766=DIRECTION('ref_axis',(-0.813151184179084,0.0222802126576441,0.581625948348321));
#80767=DIRECTION('center_axis',(4.81841295761272E-14,-1.,-3.47086837216053E-14));
#80768=DIRECTION('ref_axis',(1.,4.81841295761272E-14,5.77589282990628E-31));
#80769=DIRECTION('center_axis',(0.0956687012153076,0.987363722323065,0.126334395348684));
#80770=DIRECTION('ref_axis',(-0.829445861762144,0.00890473335591326,0.558516130590259));
#80771=DIRECTION('center_axis',(-0.0755677892436326,-0.987363721569997,
-0.139292464104397));
#80772=DIRECTION('ref_axis',(-0.853844253208445,-0.00807590692743719,0.520465917222456));
#80773=DIRECTION('center_axis',(0.0937021908559942,-0.98736372201381,0.12779976478782));
#80774=DIRECTION('ref_axis',(-0.811204865945284,-0.00129577686847123,0.584760623186104));
#80775=DIRECTION('',(-0.998605128176721,0.,-0.0527996020738229));
#80776=DIRECTION('center_axis',(-0.101878629601441,0.987363722437774,-0.121382142197087));
#80777=DIRECTION('ref_axis',(-0.669107775438933,0.0222802132234434,0.742831324693487));
#80778=DIRECTION('',(0.0527996037021322,0.,-0.998605128090627));
#80779=DIRECTION('center_axis',(-7.919254080032E-14,-1.,8.85107550859449E-14));
#80780=DIRECTION('ref_axis',(1.42279732145531E-30,-8.85107550859449E-14,
-1.));
#80781=DIRECTION('center_axis',(-0.103744819083784,-0.98736372158572,-0.119791042276414));
#80782=DIRECTION('ref_axis',(-0.721997061657015,-0.00807590627316386,0.691848988361264));
#80783=DIRECTION('center_axis',(0.118984659539436,-0.987363722014648,0.104668673650071));
#80784=DIRECTION('ref_axis',(-0.666533097641615,-0.00129577999390995,0.745474312570514));
#80785=DIRECTION('center_axis',(0.120590183957815,0.987363722329175,0.102814820727838));
#80786=DIRECTION('ref_axis',(-0.689989418966709,0.008904738214755,0.723764676777825));
#80787=DIRECTION('',(-0.986608649014418,0.,0.163105406685201));
#80788=DIRECTION('center_axis',(-0.125590336384488,0.98736372244378,-0.0966434012687544));
#80789=DIRECTION('ref_axis',(-0.49377763077791,0.0222802131608028,0.869302734060387));
#80790=DIRECTION('',(-0.163105405539067,0.,-0.986608649203896));
#80791=DIRECTION('center_axis',(7.28923339660516E-15,-1.,-1.29331847617228E-14));
#80792=DIRECTION('ref_axis',(1.41536446124868E-31,1.29331847617228E-14,
-1.));
#80793=DIRECTION('center_axis',(-0.127070857216169,-0.987363721628838,-0.0946883227098194));
#80794=DIRECTION('ref_axis',(-0.556390090292438,-0.00807590370700494,0.830881969478029));
#80795=DIRECTION('center_axis',(0.138703533836467,-0.98736372199969,0.0766433961942858));
#80796=DIRECTION('ref_axis',(-0.490694984314965,-0.00129577725624227,0.871330450133265));
#80797=DIRECTION('center_axis',(0.13987299927364,0.987363722338545,0.0744877431794555));
#80798=DIRECTION('ref_axis',(-0.518269837796568,0.00890473716125946,0.85517079047779));
#80799=DIRECTION('',(-0.928479445093385,0.,0.371383790759748));
#80800=DIRECTION('center_axis',(-0.143429579074395,0.987363722494363,-0.0673857206581365));
#80801=DIRECTION('ref_axis',(-0.295358993677058,0.0222802112338344,0.955126513631284));
#80802=DIRECTION('',(-0.371383789246356,0.,-0.928479445698729));
#80803=DIRECTION('center_axis',(1.73542509762026E-14,-1.,-5.67911351432082E-14));
#80804=DIRECTION('ref_axis',(-1.36289230963929E-31,5.67911351432082E-14,
-1.));
#80805=DIRECTION('center_axis',(-0.144455201097379,-0.987363721622812,-0.0651580854466019));
#80806=DIRECTION('ref_axis',(-0.364766936905548,-0.00807590495895753,0.931063833203523));
#80807=DIRECTION('center_axis',(0.15193678627059,-0.987363722024951,0.0450343580702607));
#80808=DIRECTION('ref_axis',(-0.291912518475211,-0.00129577560950907,0.95644414500954));
#80809=DIRECTION('center_axis',(0.152615509258198,0.987363722350212,0.042677700507334));
#80810=DIRECTION('ref_axis',(-0.32231653707135,0.00890473778969789,0.946590067333917));
#80811=DIRECTION('',(-0.826935574625762,0.,0.562296679181339));
#80812=DIRECTION('center_axis',(-0.154562213002855,0.987363722452636,-0.0349771624940467));
#80813=DIRECTION('ref_axis',(-0.0831296955738956,0.0222802138641302,0.996289639504477));
#80814=DIRECTION('',(-0.562296676496723,0.,-0.826935576451237));
#80815=DIRECTION('center_axis',(5.92512864267629E-15,-1.,-7.3992551213235E-14));
#80816=DIRECTION('ref_axis',(1.32231659479589E-31,7.3992551213235E-14,-1.));
#80817=DIRECTION('center_axis',(-0.155084981226389,-0.987363721619744,-0.032581126856186));
#80818=DIRECTION('ref_axis',(-0.156087686465311,-0.00807590435685906,0.987710187202058));
#80819=DIRECTION('center_axis',(0.158065644439664,-0.987363722011343,0.0113195628794571));
#80820=DIRECTION('ref_axis',(-0.0794805468680407,-0.00129577465791448,0.996835575026089));
#80821=DIRECTION('center_axis',(0.158221887458208,0.987363722342132,0.00887209850323346));
#80822=DIRECTION('ref_axis',(-0.111292072300149,0.00890473567881247,0.993747845444522));
#80823=DIRECTION('',(-0.686725115900806,0.,0.726917199680283));
#80824=DIRECTION('',(0.760958224664095,0.,-0.648800878787991));
#80825=DIRECTION('center_axis',(0.158340241420988,-0.987363721978348,0.00642249700707894));
#80826=DIRECTION('ref_axis',(-0.182442184061493,-0.0228638555270408,0.982950707607106));
#80827=DIRECTION('',(0.470048751153951,0.,0.882640454283969));
#80828=DIRECTION('center_axis',(1.9393850192807E-14,-1.,-1.02095484779451E-13));
#80829=DIRECTION('ref_axis',(4.24799785959656E-31,1.02095484779451E-13,
-1.));
#80830=DIRECTION('center_axis',(0.151221680423885,0.98736372206301,0.0473802039216277));
#80831=DIRECTION('ref_axis',(-0.116574944043651,-0.0297836931839635,0.992735218495618));
#80832=DIRECTION('center_axis',(-0.155570611822151,0.987363722257103,-0.0301772216726333));
#80833=DIRECTION('ref_axis',(-0.187122270954565,0.000540286809661816,0.982336481966831));
#80834=DIRECTION('',(0.882640455447344,0.,-0.470048748969407));
#80835=DIRECTION('center_axis',(0.153257689134951,-0.987363721885547,0.0403108102788267));
#80836=DIRECTION('ref_axis',(-0.389482131659896,-0.022863859304535,0.920750190364013));
#80837=DIRECTION('',(0.269317664813194,0.,0.963051398119315));
#80838=DIRECTION('center_axis',(1.16822697290887E-14,-1.,-2.72969841571987E-14));
#80839=DIRECTION('ref_axis',(-4.67462342555635E-32,2.72969841571987E-14,
-1.));
#80840=DIRECTION('center_axis',(0.137500857422994,0.987363722012776,0.0787806744133277));
#80841=DIRECTION('ref_axis',(-0.327258211259482,-0.0297836958742307,0.944465454436167));
#80842=DIRECTION('center_axis',(-0.145446246378588,0.987363722270834,-0.0629147785330536));
#80843=DIRECTION('ref_axis',(-0.393920760901921,0.000540287765887657,0.919144244512025));
#80844=DIRECTION('',(0.963051398102499,0.,-0.269317664873326));
#80845=DIRECTION('center_axis',(0.141008974677269,-0.9873637219592,0.0723142421611428));
#80846=DIRECTION('ref_axis',(-0.578310330469618,-0.0228638554140194,0.815496416784113));
#80847=DIRECTION('',(0.055993585129981,0.,0.998431128533306));
#80848=DIRECTION('center_axis',(-5.18315684147911E-14,-1.,7.24423595823463E-14));
#80849=DIRECTION('ref_axis',(5.83498941382284E-31,-7.24423595823463E-14,
-1.));
#80850=DIRECTION('center_axis',(0.117350647804882,0.987363722042521,0.106497445293839));
#80851=DIRECTION('ref_axis',(-0.522639253324542,-0.0297836947345418,0.852033533619613));
#80852=DIRECTION('center_axis',(-0.128520974775072,0.987363722243296,-0.0927105120292627));
#80853=DIRECTION('ref_axis',(-0.582299955948521,0.000540290561766755,0.812973842991556));
#80854=DIRECTION('',(0.998431128681518,0.,-0.0559935824872008));
#80855=DIRECTION('center_axis',(0.122166839683711,-0.987363721945433,0.100936335715917));
#80856=DIRECTION('ref_axis',(-0.740097379992076,-0.0228638568074939,0.672110937405984));
#80857=DIRECTION('',(-0.159948692818663,0.,0.987125329259462));
#80858=DIRECTION('center_axis',(3.30963705216048E-14,-1.,-2.98032211797663E-14));
#80859=DIRECTION('ref_axis',(1.,3.30963705216048E-14,6.25159708608419E-31));
#80860=DIRECTION('center_axis',(0.0917132492495926,0.987363721931247,0.129234517549131));
#80861=DIRECTION('ref_axis',(-0.693582260141972,-0.0297836992689342,0.719761474152521));
#80862=DIRECTION('center_axis',(-0.105586206860168,0.98736372225967,-0.118171201595023));
#80863=DIRECTION('ref_axis',(-0.743451451729584,0.000540289541825534,0.66878968817438));
#80864=DIRECTION('',(0.9871253291959,0.,0.159948693210935));
#80865=DIRECTION('center_axis',(0.0976123117887723,-0.987363722077454,0.124838763661801));
#80866=DIRECTION('ref_axis',(-0.867278299557125,-0.0228638492548932,0.497298296311731));
#80867=DIRECTION('',(-0.368411947167087,0.,0.929662646977147));
#80868=DIRECTION('center_axis',(-3.87294073426819E-14,-1.,2.19916970886201E-14));
#80869=DIRECTION('ref_axis',(1.,-3.87294073426819E-14,-2.80400459788044E-31));
#80870=DIRECTION('center_axis',(0.0617874476087296,0.987363722074324,0.145928721126229));
#80871=DIRECTION('ref_axis',(-0.832094133351182,-0.0297836941084912,0.55383416724485));
#80872=DIRECTION('center_axis',(-0.0777143454300615,0.987363722242749,-0.138106337701498));
#80873=DIRECTION('ref_axis',(-0.869839983855047,0.000540288780145893,0.493333670627787));
#80874=DIRECTION('',(0.929662646609954,0.,0.368411948093674));
#80875=DIRECTION('center_axis',(0.0684935522830534,-0.987363721953246,0.14290386232108));
#80876=DIRECTION('ref_axis',(-0.953906248045583,-0.0228638555599683,0.299232541760637));
#80877=DIRECTION('',(-0.559648669545669,0.,0.8287299721114));
#80878=DIRECTION('center_axis',(-4.25515000991007E-14,-1.,1.31518656770642E-14));
#80879=DIRECTION('ref_axis',(1.,-4.25515000991007E-14,-9.27098447437634E-32));
#80880=DIRECTION('center_axis',(0.0289725294669247,0.987363722077741,0.155799463609725));
#80881=DIRECTION('ref_axis',(-0.931698210467539,-0.0297836942824951,0.362010187931876));
#80882=DIRECTION('center_axis',(-0.0462086544522591,0.987363722215039,-0.151583773232412));
#80883=DIRECTION('ref_axis',(-0.955555764032208,0.000540281349776698,0.294809921679862));
#80884=DIRECTION('',(0.828729971245935,0.,0.559648670827254));
#80885=DIRECTION('center_axis',(0.0361721042068151,-0.987363721965724,0.154286938602218));
#80886=DIRECTION('ref_axis',(-0.995930601319451,-0.0228638548777849,0.0871750049934288));
#80887=DIRECTION('',(-0.724716840964423,0.,0.689046805683437));
#80888=DIRECTION('center_axis',(5.91785760991902E-14,-1.,-4.92942355256591E-15));
#80889=DIRECTION('ref_axis',(1.,5.91785760991902E-14,1.20798325998743E-31));
#80890=DIRECTION('center_axis',(-0.00519711437170142,0.98736372197901,0.158385196662958));
#80891=DIRECTION('ref_axis',(-0.987737113176826,-0.0297836975432815,0.153259018050357));
#80892=DIRECTION('center_axis',(-0.0125422848273878,0.987363722246296,-0.157973323960879));
#80893=DIRECTION('ref_axis',(-0.996590820051855,0.000540287682197817,0.0825011847041714));
#80894=DIRECTION('',(0.68904680421877,0.,0.724716842357));
#80895=DIRECTION('center_axis',(0.00215929339199061,-0.987363721902053,
0.158455729223565));
#80896=DIRECTION('ref_axis',(-0.991386346590728,-0.0228638587196378,-0.128958736648343));
#80897=DIRECTION('',(-0.855898060460215,0.,0.517144573693317));
#80898=DIRECTION('center_axis',(2.94273471123754E-14,-1.,3.95373409499303E-15));
#80899=DIRECTION('ref_axis',(1.,2.94273471123754E-14,2.02742082198128E-32));
#80900=DIRECTION('center_axis',(-0.0391237393995077,0.987363722089514,0.153565013323152));
#80901=DIRECTION('ref_axis',(-0.997590527089144,-0.029783692692005,-0.0626583746328627));
#80902=DIRECTION('center_axis',(0.0217105382769153,0.987363722231686,-0.156976216505932));
#80903=DIRECTION('ref_axis',(-0.991026396674851,0.000540284273519458,-0.133665213075668));
#80904=DIRECTION('',(0.517144572474294,0.,0.855898061196764));
#80905=DIRECTION('center_axis',(-0.0319544928798145,-0.987363721986839,
0.155215304944744));
#80906=DIRECTION('ref_axis',(-0.940485968153084,-0.0228638532295288,-0.33906251329608));
#80907=DIRECTION('',(-0.947058436717489,0.,0.32106123628091));
#80908=DIRECTION('center_axis',(-5.57788322291163E-14,-1.,-2.03746154928163E-14));
#80909=DIRECTION('ref_axis',(1.,-5.57788322291163E-14,4.36823228791738E-31));
#80910=DIRECTION('center_axis',(-0.0712209830271485,0.987363722192202,0.141564302263692));
#80911=DIRECTION('ref_axis',(-0.96079771655334,-0.0297836888147394,-0.27564593185185));
#80912=DIRECTION('center_axis',(0.0549482066376669,0.987363722243729,-0.148639074890527));
#80913=DIRECTION('ref_axis',(-0.939122680647031,0.00054028684886553,-0.343581575152767));
#80914=DIRECTION('',(0.321061238918488,0.,0.947058435823326));
#80915=DIRECTION('center_axis',(-0.0645741168328686,-0.987363722016858,
0.144717185849752));
#80916=DIRECTION('ref_axis',(-0.845609510466505,-0.0228638535199251,-0.533312103754282));
#80917=DIRECTION('',(-0.993935411981185,0.,0.109965434613753));
#80918=DIRECTION('center_axis',(0.,-1.,0.));
#80919=DIRECTION('ref_axis',(0.,0.,-1.));
#80920=DIRECTION('center_axis',(-0.0999880255367153,0.987363721948417,0.122944195997362));
#80921=DIRECTION('ref_axis',(-0.879079071420455,-0.0297836993029511,-0.475744592661212));
#80922=DIRECTION('center_axis',(0.0856165537158678,0.987363722249874,-0.133351736826677));
#80923=DIRECTION('ref_axis',(-0.843306631655252,0.000540284728342988,-0.537432445148862));
#80924=DIRECTION('',(0.109965437515861,0.,0.993935411660106));
#80925=DIRECTION('center_axis',(-0.0941743252867184,-0.9873637219706,0.127452253778252));
#80926=DIRECTION('ref_axis',(-0.711193292549383,-0.0228638558648281,-0.702624611530054));
#80927=DIRECTION('',(-0.994337072346781,0.,-0.106272228530468));
#80928=DIRECTION('center_axis',(4.20684180271517E-14,-1.,4.19124239078833E-14));
#80929=DIRECTION('ref_axis',(1.,4.20684180271517E-14,1.15419787652154E-30));
#80930=DIRECTION('center_axis',(-0.124079726667146,0.987363722011638,0.0985753614527047));
#80931=DIRECTION('ref_axis',(-0.756255667861176,-0.0297836962498653,-0.653597962256265));
#80932=DIRECTION('center_axis',(0.11228156877962,0.98736372228335,-0.111829017840426));
#80933=DIRECTION('ref_axis',(-0.708058500491322,0.000540285967795188,-0.706153572513128));
#80934=DIRECTION('',(-0.106272228164584,0.,0.994337072385886));
#80935=DIRECTION('center_axis',(-0.119371047568695,-0.987363721916357,0.104227796896177));
#80936=DIRECTION('ref_axis',(-0.543522466694485,-0.0228638584411881,-0.839083173574303));
#80937=DIRECTION('',(-0.948244636544391,0.,-0.317540720640354));
#80938=DIRECTION('center_axis',(6.41498992470956E-14,-1.,9.99520022934591E-14));
#80939=DIRECTION('ref_axis',(-1.66109997065748E-30,-9.99520022934592E-14,
-1.));
#80940=DIRECTION('center_axis',(-0.142369599811967,0.987363722034372,0.069597251812215));
#80941=DIRECTION('ref_axis',(-0.598070588946222,-0.0297836950516744,-0.800889818980481));
#80942=DIRECTION('center_axis',(0.133696423493094,0.98736372226897,-0.0850772959861791));
#80943=DIRECTION('ref_axis',(-0.539702340761982,0.000540289765636053,-0.84185574266795));
#80944=DIRECTION('',(-0.317540722300475,0.,0.948244635988463));
#80945=DIRECTION('center_axis',(-0.13898611473656,-0.987363721915582,0.076129761299015));
#80946=DIRECTION('ref_axis',(-0.350437134000453,-0.0228638573645295,-0.936307139319125));
#80947=DIRECTION('',(-0.857813335121565,0.,-0.513961362446262));
#80948=DIRECTION('center_axis',(-2.57271152087778E-14,-1.,-6.96284450963471E-14));
#80949=DIRECTION('ref_axis',(2.11209165460069E-31,6.96284450963471E-14,
-1.));
#80950=DIRECTION('center_axis',(-0.154002428756816,0.987363722073544,0.0373648534063824));
#80951=DIRECTION('ref_axis',(-0.411920395828391,-0.0297836930004011,-0.910732957091067));
#80952=DIRECTION('center_axis',(0.148859778365135,0.987363722268598,-0.0543474593056635));
#80953=DIRECTION('ref_axis',(-0.346110301969915,0.000540287633313102,-0.938193672415012));
#80954=DIRECTION('',(-0.513961362392703,0.,0.857813335153655));
#80955=DIRECTION('center_axis',(-0.152102345152299,-0.987363721974116,0.0444719813882001));
#80956=DIRECTION('ref_axis',(-0.140965751559213,-0.022863855048196,-0.989750423601668));
#80957=DIRECTION('',(-0.727271635232519,0.,-0.686349742176842));
#80958=DIRECTION('center_axis',(-1.42206008573881E-14,-1.,-1.0294359583756E-13));
#80959=DIRECTION('ref_axis',(2.37051675250879E-31,1.0294359583756E-13,-1.));
#80960=DIRECTION('center_axis',(-0.158434276437426,0.987363722091202,0.00338531356859956));
#80961=DIRECTION('ref_axis',(-0.206509259301968,-0.029783693097487,-0.977991235874855));
#80962=DIRECTION('center_axis',(0.157062616400018,0.987363722260677,-0.0210763965876856));
#80963=DIRECTION('ref_axis',(-0.1363345302832,0.000540285074681563,-0.990662709475075));
#80964=DIRECTION('',(-0.686349742131425,0.,0.727271635275381));
#80965=DIRECTION('center_axis',(-0.158106438275909,-0.987363721978957,0.0107347424546262));
#80966=DIRECTION('ref_axis',(0.0750970332009502,-0.0228638543459592,-0.996914078428458));
#80967=DIRECTION('',(-0.562723523285499,0.,-0.826645169550488));
#80968=DIRECTION('center_axis',(1.17738557350016E-15,-1.,-1.47991200996898E-14));
#80969=DIRECTION('ref_axis',(4.53712827619466E-33,1.47991200996898E-14,
-1.));
#80970=DIRECTION('center_axis',(-0.15545791360717,0.987363722140864,-0.030752516922108));
#80971=DIRECTION('ref_axis',(0.00855801734471834,-0.0297836909058287,-0.999519730718285));
#80972=DIRECTION('center_axis',(0.157921382458744,0.987363722227175,0.0131801742028564));
#80973=DIRECTION('ref_axis',(0.0798160940080673,0.000540281567541906,-0.996809459843316));
#80974=DIRECTION('',(-0.826645169515347,0.,0.562723523337121));
#80975=DIRECTION('center_axis',(-0.156717651053432,-0.987363721910341,-0.0235044358292781));
#80976=DIRECTION('ref_axis',(0.287648364605956,-0.0228638592072449,-0.957463138863147));
#80977=DIRECTION('',(-0.37186308447585,0.,-0.928287588198887));
#80978=DIRECTION('center_axis',(-8.66246462967909E-15,-1.,2.84000436037034E-14));
#80979=DIRECTION('ref_axis',(-7.27882089572718E-32,-2.84000436037034E-14,
-1.));
#80980=DIRECTION('center_axis',(-0.145212510328833,0.987363722018922,-0.0634524017271248));
#80981=DIRECTION('ref_axis',(0.223225132689914,-0.0297836965305611,-0.974311793809634));
#80982=DIRECTION('center_axis',(0.151395919725379,0.987363722225758,0.0468204605167725));
#80983=DIRECTION('ref_axis',(0.292234606692641,0.000540284026219369,-0.95634650767615));
#80984=DIRECTION('',(-0.928287587778145,0.,0.371863085526155));
#80985=DIRECTION('center_axis',(-0.148000920052496,-0.987363721900531,-0.0566445790728921));
#80986=DIRECTION('ref_axis',(0.486749578565709,-0.0228638577531011,-0.873242286982685));
#80987=DIRECTION('',(-0.163614740740223,0.,-0.986524311212101));
#80988=DIRECTION('center_axis',(-2.18476663765354E-14,-1.,3.88108388533404E-14));
#80989=DIRECTION('ref_axis',(-2.37202458671487E-31,-3.88108388533404E-14,
-1.));
#80990=DIRECTION('center_axis',(-0.128177133113144,0.987363722071159,-0.0931853147479977));
#80991=DIRECTION('ref_axis',(0.427454489836029,-0.0297836935546327,-0.903546119861772));
#80992=DIRECTION('center_axis',(0.137791350316563,0.987363722237745,0.0782714749239015));
#80993=DIRECTION('ref_axis',(0.490988553554454,0.0005402878828289,-0.871165855832004));
#80994=DIRECTION('',(-0.986524311201882,0.,0.163614740801838));
#80995=DIRECTION('center_axis',(-0.132363832496354,-0.987363721865011,-0.0871360808835846));
#80996=DIRECTION('ref_axis',(0.663090921521998,-0.0228638604900558,-0.74818959741405));
#80997=DIRECTION('',(0.0522840469698041,0.,-0.998632253851466));
#80998=DIRECTION('center_axis',(9.89335438426233E-15,-1.,-1.10689535020008E-14));
#80999=DIRECTION('ref_axis',(-2.42855846616023E-31,1.10689535020008E-14,
-1.));
#81000=DIRECTION('center_axis',(-0.105148334450947,0.987363722064401,-0.118560989002812));
#81001=DIRECTION('ref_axis',(0.611696547757108,-0.0297836942674327,-0.790531634419408));
#81002=DIRECTION('center_axis',(0.117743810833585,0.987363722264892,0.106062599277983));
#81003=DIRECTION('ref_axis',(0.666784422275534,0.000540288842422262,-0.745250456087515));
#81004=DIRECTION('',(-0.99863225400483,0.,-0.0522840440405324));
#81005=DIRECTION('center_axis',(-0.110537553796009,-0.987363721965769,-0.113553202274082));
#81006=DIRECTION('ref_axis',(0.808426872685382,-0.022863855483925,-0.588152391504569));
#81007=DIRECTION('',(0.265738088458527,0.,-0.964045262600469));
#81008=DIRECTION('center_axis',(1.20415510587402E-14,-1.,-8.68338877012913E-15));
#81009=DIRECTION('ref_axis',(1.,1.20415510587402E-14,1.22739341060735E-31));
#81010=DIRECTION('center_axis',(-0.0772029162671188,0.987363722049365,-0.13839288312871));
#81011=DIRECTION('ref_axis',(0.767336357098404,-0.0297836946635119,-0.640552766450307));
#81012=DIRECTION('center_axis',(0.0921907025089084,0.987363722255374,0.128894353425302));
#81013=DIRECTION('ref_axis',(0.811402191745447,0.000540288608632149,-0.584487973630685));
#81014=DIRECTION('',(-0.964045262617061,0.,-0.265738088398336));
#81015=DIRECTION('center_axis',(-0.0835426669511802,-0.987363721945072,
-0.134660697255953));
#81016=DIRECTION('ref_axis',(0.915961679953268,-0.0228638572586547,-0.400613835118612));
#81017=DIRECTION('',(0.466766516185184,0.,-0.884380585137613));
#81018=DIRECTION('center_axis',(4.08800946221569E-14,-1.,-1.76753953209365E-14));
#81019=DIRECTION('ref_axis',(1.,4.08800946221569E-14,-2.74904545746926E-32));
#81020=DIRECTION('center_axis',(-0.045647575810467,0.987363722013861,-0.151753679604688));
#81021=DIRECTION('ref_axis',(0.887096369051805,-0.0297836951534783,-0.460622365412393));
#81022=DIRECTION('center_axis',(0.0623268615180566,0.987363722252623,0.14569915000697));
#81023=DIRECTION('ref_axis',(0.918079696437692,0.000540286067284419,-0.396395483172854));
#81024=DIRECTION('',(-0.884380585166462,0.,-0.466766516130523));
#81025=DIRECTION('center_axis',(-0.0526414158310298,-0.987363721922956,
-0.149471609243201));
#81026=DIRECTION('ref_axis',(0.980667137396743,-0.0228638565726862,-0.1943430206946));
#81027=DIRECTION('',(0.645969457690815,0.,-0.763363255423415));
#81028=DIRECTION('center_axis',(0.,-1.,0.));
#81029=DIRECTION('ref_axis',(0.,0.,-1.));
#81030=DIRECTION('center_axis',(-0.011957812984655,0.987363722205697,-0.158018640611592));
#81031=DIRECTION('ref_axis',(0.965376741456017,-0.0297836876240715,-0.259153774827367));
#81032=DIRECTION('center_axis',(0.0295486796979486,0.987363722245942,0.155691218508769));
#81033=DIRECTION('ref_axis',(0.981828814775111,0.00054029026758487,-0.189767980870663));
#81034=DIRECTION('',(-0.763363255462685,0.,-0.645969457644409));
#81035=DIRECTION('center_axis',(-0.0192787124909096,-0.987363721914727,
-0.157293394303103));
#81036=DIRECTION('ref_axis',(0.999517689362401,-0.0228638579857241,0.021015057688609));
#81037=DIRECTION('',(0.794967585437563,0.,-0.606651908513911));
#81038=DIRECTION('center_axis',(0.,-1.,0.));
#81039=DIRECTION('ref_axis',(0.,0.,-1.));
#81040=DIRECTION('center_axis',(0.0222910985942386,0.987363722043707,-0.156894828835942));
#81041=DIRECTION('ref_axis',(0.998517170574893,-0.0297836953944212,-0.0455674396445725));
#81042=DIRECTION('center_axis',(-0.00461116002007661,0.987363722279684,
0.15840333686282));
#81043=DIRECTION('ref_axis',(0.999668709074289,0.00054028841285584,0.0257328619895947));
#81044=DIRECTION('',(-0.606651908563567,0.,-0.79496758539967));
#81045=DIRECTION('center_axis',(0.0149854418475902,-0.987363721860772,-0.157760315941228));
#81046=DIRECTION('ref_axis',(0.971631905064919,-0.0228638594886714,0.23539049468744));
#81047=DIRECTION('',(0.906793913166479,0.,-0.421574191624944));
#81048=DIRECTION('center_axis',(1.44136844525623E-14,-1.,3.55610651202243E-15));
#81049=DIRECTION('ref_axis',(1.,1.44136844525623E-14,-5.50471133143517E-32));
#81050=DIRECTION('center_axis',(0.0554976904766439,0.987363722124659,-0.148434788994693));
#81051=DIRECTION('ref_axis',(0.984968046763139,-0.0297836901696709,0.170149577300337));
#81052=DIRECTION('center_axis',(-0.0385553889347902,0.987363722263352,0.153708691824324));
#81053=DIRECTION('ref_axis',(0.970765205310708,0.000540288479386633,0.240030465246431));
#81054=DIRECTION('',(-0.421574190582567,0.,-0.906793913651086));
#81055=DIRECTION('center_axis',(0.048548891846868,-0.987363721815495,-0.150850541739481));
#81056=DIRECTION('ref_axis',(0.898313693186332,-0.0228638628925394,0.438759333128726));
#81057=DIRECTION('',(0.976219564475212,0.,-0.216784136725517));
#81058=DIRECTION('center_axis',(1.33122427314128E-14,-1.,6.57148280683985E-15));
#81059=DIRECTION('ref_axis',(1.,1.33122427314128E-14,-8.34320862855221E-32));
#81060=DIRECTION('center_axis',(0.0861092826875015,0.987363721992229,-0.133034100623476));
#81061=DIRECTION('ref_axis',(0.925362911146449,-0.0297836960963146,0.377910590115454));
#81062=DIRECTION('center_axis',(-0.0706968106702072,0.987363722284384,0.141826798870266));
#81063=DIRECTION('ref_axis',(0.896469799427748,0.000540288698301344,0.443104510022292));
#81064=DIRECTION('',(-0.216784133438348,0.,-0.976219565205177));
#81065=DIRECTION('center_axis',(0.0798422585918534,-0.987363721936398,-0.136887159174463));
#81066=DIRECTION('ref_axis',(0.78299133001524,-0.0228638563166837,0.621612275615029));
#81067=DIRECTION('',(0.999998274855759,0.,-0.00185749441591979));
#81068=DIRECTION('center_axis',(-5.79416767742965E-14,-1.,-4.63979194031601E-14));
#81069=DIRECTION('ref_axis',(1.,-5.79416767742965E-14,-8.87442181665929E-32));
#81070=DIRECTION('center_axis',(0.11269449223574,0.987363722076581,-0.111412888602755));
#81071=DIRECTION('ref_axis',(0.822488835150569,-0.0297836931952023,0.568000922246007));
#81072=DIRECTION('center_axis',(-0.0995325279600817,0.987363722252021,0.123313242835106));
#81073=DIRECTION('ref_axis',(0.780256462409246,0.000540288674050379,0.625459479868007));
#81074=DIRECTION('',(-0.00185749160357402,0.,-0.999998274860983));
#81075=DIRECTION('center_axis',(0.107402284445999,-0.987363721972997,-0.116523087100419));
#81076=DIRECTION('ref_axis',(0.631057164088596,-0.022863855066005,0.775399316342218));
#81077=DIRECTION('',(0.977018176875493,0.,0.213156004031993));
#81078=DIRECTION('center_axis',(-9.3225702735687E-15,-1.,-1.15537819071333E-14));
#81079=DIRECTION('ref_axis',(-1.02932978610097E-31,1.15537819071333E-14,
-1.));
#81080=DIRECTION('center_axis',(0.134010238812352,0.987363721952771,-0.084582128520313));
#81081=DIRECTION('ref_axis',(0.681156094834938,-0.0297836985911217,0.731532163180438));
#81082=DIRECTION('center_axis',(-0.123714212040058,0.987363722232974,0.0990337001103841));
#81083=DIRECTION('ref_axis',(0.627559201727512,0.000540284264199704,0.778568658770722));
#81084=DIRECTION('',(0.213156003970963,0.,-0.977018176888808));
#81085=DIRECTION('center_axis',(0.129940297562282,-0.987363721916974,-0.0907105270169139));
#81086=DIRECTION('ref_axis',(0.449615466022523,-0.0228638564463816,0.892929547490589));
#81087=DIRECTION('',(0.908353794958554,0.,0.41820256238382));
#81088=DIRECTION('center_axis',(0.,-1.,0.));
#81089=DIRECTION('ref_axis',(0.,0.,-1.));
#81090=DIRECTION('center_axis',(0.14905980749689,0.987363722127537,-0.053796412663352));
#81091=DIRECTION('ref_axis',(0.507973253116063,-0.0297836902908456,0.860857773335029));
#81092=DIRECTION('center_axis',(-0.142111161646279,0.987363722248888,0.0701234463098179));
#81093=DIRECTION('ref_axis',(0.445517968814157,0.000540286778625937,0.895272834142701));
#81094=DIRECTION('',(0.418202564699209,0.,-0.908353793892558));
#81095=DIRECTION('center_axis',(0.146402447495151,-0.987363721952896,-0.0606564418570101));
#81096=DIRECTION('ref_axis',(0.247150249152909,-0.0228638558610294,0.96870738535371));
#81097=DIRECTION('',(0.797215799077901,0.,0.603694434048041));
#81098=DIRECTION('center_axis',(-2.16577711357467E-14,-1.,-8.64022447059934E-14));
#81099=DIRECTION('ref_axis',(2.81888937165628E-31,8.64022447059934E-14,
-1.));
#81100=DIRECTION('center_axis',(0.157139511605707,0.987363722043768,-0.0204952258879351));
#81101=DIRECTION('ref_axis',(0.311038146206098,-0.0297836945747142,0.949930630700028));
#81102=DIRECTION('center_axis',(-0.153863149848971,0.987363722253108,0.0379342997436371));
#81103=DIRECTION('ref_axis',(0.242644810113474,0.000540287020636909,0.970115046896465));
#81104=DIRECTION('',(0.603694433998265,0.,-0.797215799115594));
#81105=DIRECTION('center_axis',(0.15601898153659,-0.987363721893832,-0.0277661320360645));
#81106=DIRECTION('ref_axis',(0.0331285598677343,-0.0228638586816274,0.999189542823221));
#81107=DIRECTION('',(0.648800877075795,0.,0.760958226123931));
#81108=DIRECTION('center_axis',(3.00707855221535E-15,-1.,1.03877653670037E-13));
#81109=DIRECTION('ref_axis',(0.0289361498648771,1.03921169418994E-13,0.999581261944719));
#81110=DIRECTION('center_axis',(0.157871544748138,0.987363722095124,0.0137642889136518));
#81111=DIRECTION('ref_axis',(0.0995592420306967,-0.0297836924791192,0.994585787646587));
#81112=DIRECTION('center_axis',(-0.158420668071144,0.987363722255966,0.003971385241346));
#81113=DIRECTION('ref_axis',(0.0284258509567777,0.000540289709918792,0.999595757836343));
#81114=DIRECTION('center_axis',(-0.163746583102855,-0.986495110327124,-0.00380181835644106));
#81115=DIRECTION('ref_axis',(0.0270297015237054,-0.00833893471375523,0.999599848641135));
#81116=DIRECTION('center_axis',(0.161203610189502,-0.986495108559966,-0.0289964971872927));
#81117=DIRECTION('ref_axis',(0.137709438928237,-0.00660960175535,0.990450616434109));
#81118=DIRECTION('center_axis',(-0.160735582317879,-0.986495108181465,0.0314876818926446));
#81119=DIRECTION('ref_axis',(0.241282154885155,-0.00833899447686017,0.970419178966023));
#81120=DIRECTION('center_axis',(0.151201369427675,-0.986495108577346,-0.0629725863861876));
#81121=DIRECTION('ref_axis',(0.347407475820122,-0.00660960159429159,0.937690971968407));
#81122=DIRECTION('center_axis',(-0.150208754328077,-0.986495108142209,0.0653049135570864));
#81123=DIRECTION('ref_axis',(0.444252549571252,-0.00833899746620968,0.895862787105649));
#81124=DIRECTION('center_axis',(0.134129124742108,-0.986495108557985,-0.0940041418613364));
#81125=DIRECTION('ref_axis',(0.540861120534035,-0.00660959535685714,0.841085941829898));
#81126=DIRECTION('center_axis',(-0.132658332165123,-0.986495108139988,0.0960685615747535));
#81127=DIRECTION('ref_axis',(0.626450190063033,-0.0083389993819398,0.779416846404604));
#81128=DIRECTION('center_axis',(0.110785147588717,-0.986495108531098,-0.120640175389312));
#81129=DIRECTION('ref_axis',(0.709024704301451,-0.00660959663965462,0.705152665684886));
#81130=DIRECTION('center_axis',(-0.108904949677008,-0.986495108205661,0.122340154577923));
#81131=DIRECTION('ref_axis',(0.779355715649713,-0.00833899514876089,0.626526240187938));
#81132=DIRECTION('center_axis',(0.0822609720701449,-0.986495108556898,-0.141635211961534));
#81133=DIRECTION('ref_axis',(0.844035079541172,-0.00660960678430646,0.536247235519293));
#81134=DIRECTION('center_axis',(-0.0800592947095578,-0.986495108204483,
0.142891255223105));
#81135=DIRECTION('ref_axis',(0.895819434046711,-0.00833899422620221,0.444339963045781));
#81136=DIRECTION('center_axis',(0.0498903833975317,-0.986495108560805,-0.156007533247763));
#81137=DIRECTION('ref_axis',(0.939579312919432,-0.00660959500260434,0.342267480178513));
#81138=DIRECTION('center_axis',(-0.0474701574982248,-0.986495108181289,
0.156760918858883));
#81139=DIRECTION('ref_axis',(0.97039563113366,-0.00833899500264603,0.241376842797838));
#81140=DIRECTION('center_axis',(0.0151869637452026,-0.986495108589794,-0.163085121518218));
#81141=DIRECTION('ref_axis',(0.991189861386224,-0.00660959737962207,0.132283679672277));
#81142=DIRECTION('center_axis',(-0.0126613696933789,-0.986495108187851,
0.163300616162116));
#81143=DIRECTION('ref_axis',(0.999597206674059,-0.00833899686580644,0.027127210337405));
#81144=DIRECTION('center_axis',(-0.0202265838329378,-0.986495108564548,
-0.162537029887563));
#81145=DIRECTION('ref_axis',(0.996453473854886,-0.00660960148140599,-0.0838855625884892));
#81146=DIRECTION('center_axis',(0.0227394532200513,-0.986495108204774,0.162204558367835));
#81147=DIRECTION('ref_axis',(0.982058727938165,-0.00833899493008264,-0.188390859767746));
#81148=DIRECTION('center_axis',(-0.0546943527513138,-0.986495108539734,
-0.154388887567379));
#81149=DIRECTION('ref_axis',(0.955124029393475,-0.00660959983514798,-0.296132405631656));
#81150=DIRECTION('center_axis',(0.0570770025954627,-0.98649510820796,0.153523995702568));
#81151=DIRECTION('ref_axis',(0.918600274496498,-0.00833899512343136,-0.395099983365338));
#81152=DIRECTION('center_axis',(-0.0866046781089558,-0.986495108574079,
-0.139021690714295));
#81153=DIRECTION('ref_axis',(0.869134046575717,-0.00660960205580594,-0.494532427898903));
#81154=DIRECTION('center_axis',(0.0887457396431603,-0.986495110261855,0.137664778082992));
#81155=DIRECTION('ref_axis',(0.812189079529727,-0.00833893655201375,-0.583334690576377));
#81156=DIRECTION('center_axis',(-0.114465461008326,-0.986495108551733,-0.117153997113444));
#81157=DIRECTION('ref_axis',(0.742504322941052,-0.00660959950258174,-0.669808661938815));
#81158=DIRECTION('center_axis',(0.116264737375798,-0.986495108195593,0.11536859342604));
#81159=DIRECTION('ref_axis',(0.66780085302811,-0.00833899486530625,-0.744293276779768));
#81160=DIRECTION('center_axis',(-0.136973968593365,-0.986495108545222,-0.0898083111083468));
#81161=DIRECTION('ref_axis',(0.581155923333125,-0.00660960002778809,-0.813765387542562));
#81162=DIRECTION('center_axis',(0.138347370174825,-0.986495108190397,0.0876778574220828));
#81163=DIRECTION('ref_axis',(0.492186987026872,-0.00833899405968922,-0.870449556826518));
#81164=DIRECTION('center_axis',(-0.153077727573361,-0.986495108555823,-0.0582632827466133));
#81165=DIRECTION('ref_axis',(0.392633313565955,-0.00660960544614752,-0.919671351186969));
#81166=DIRECTION('center_axis',(0.153961032422214,-0.986495108170381,0.0558874051231136));
#81167=DIRECTION('ref_axis',(0.293559004575771,-0.00833899651873737,-0.955904583088471));
#81168=DIRECTION('center_axis',(-0.162023738619957,-0.98649510858625,-0.0239939337961682));
#81169=DIRECTION('ref_axis',(0.185751609571843,-0.0066096046717047,-0.982574502349595));
#81170=DIRECTION('center_axis',(0.162375649064777,-0.986495108153596,0.0214837189475607));
#81171=DIRECTION('ref_axis',(0.0812045315127966,-0.00833899735817754,-0.996662573384216));
#81172=DIRECTION('center_axis',(-0.163393695748669,-0.986495108696664,0.0113973991396275));
#81173=DIRECTION('ref_axis',(-0.0298156589858182,-0.00660965490275117,-0.999533560687838));
#81174=DIRECTION('center_axis',(0.163197761691683,-0.986495108100812,-0.0139245205300664));
#81175=DIRECTION('ref_axis',(-0.134946979285497,-0.00833900044466913,-0.990817729884414));
#81176=DIRECTION('center_axis',(-0.157123555131692,-0.986495108582043,0.0462556933412782));
#81177=DIRECTION('ref_axis',(-0.243988729791768,-0.00660960030427146,-0.969755542865529));
#81178=DIRECTION('center_axis',(0.156388927828435,-0.98649510813377,-0.0486816688376119));
#81179=DIRECTION('ref_axis',(-0.344788517321524,-0.00833899908727815,-0.938643350489123));
#81180=DIRECTION('center_axis',(-0.143506486861752,-0.986495108529812,0.0789511815956736));
#81181=DIRECTION('ref_axis',(-0.446753182602872,-0.0066096015307531,-0.894632833626069));
#81182=DIRECTION('center_axis',(0.142267519731386,-0.986495108183313,-0.0811625181957401));
#81183=DIRECTION('ref_axis',(-0.538508128428602,-0.00833899548032144,-0.842579050754707));
#81184=DIRECTION('center_axis',(-0.123179214736077,-0.986495108581144,0.107954998969391));
#81185=DIRECTION('ref_axis',(-0.628627956656191,-0.00660960084133648,-0.777678085898645));
#81186=DIRECTION('center_axis',(0.121493846397304,-0.986495108098356,-0.109848290772327));
#81187=DIRECTION('ref_axis',(-0.707047696569409,-0.00833900158626248,-0.707116691804428));
#81188=DIRECTION('center_axis',(-0.0970922211053125,-0.986495108544632,
0.131910960190395));
#81189=DIRECTION('ref_axis',(-0.781108784594513,-0.00660959905628847,-0.624359976159265));
#81190=DIRECTION('center_axis',(0.0950392464483762,-0.986495108205492,-0.133397687840383));
#81191=DIRECTION('ref_axis',(-0.842526501061776,-0.00833899471871473,-0.538590341702934));
#81192=DIRECTION('center_axis',(-0.0664652477252153,-0.986495108659401,
0.149698935987874));
#81193=DIRECTION('ref_axis',(-0.897065845627383,-0.00660965417426619,-0.441847463589557));
#81194=DIRECTION('center_axis',(0.0641407249323982,-0.986495108138676,-0.150709551865859));
#81195=DIRECTION('ref_axis',(-0.938609701908453,-0.00833899750784452,-0.344880107579271));
#81196=DIRECTION('center_axis',(-0.0327304788701568,-0.986495108642727,
0.160487122152853));
#81197=DIRECTION('ref_axis',(-0.971077088526604,-0.00660965631685087,-0.238674675200505));
#81198=DIRECTION('center_axis',(0.0302430527726786,-0.986495108131369,-0.160974406014955));
#81199=DIRECTION('ref_axis',(-0.990804557523789,-0.00833899897663459,-0.1350436591853));
#81200=DIRECTION('center_axis',(0.00253467411159349,-0.986495108531176,
0.16377110939116));
#81201=DIRECTION('ref_axis',(-0.999681845517634,-0.00660960532316903,-0.0243417513735121));
#81202=DIRECTION('center_axis',(-0.00506877383906692,-0.98649510953872,
-0.163712267066205));
#81203=DIRECTION('ref_axis',(-0.9966704924382,-0.00833897643643672,0.0811072806533985));
#81204=DIRECTION('center_axis',(0.0376813611748462,-0.986495108564858,0.159397351915329));
#81205=DIRECTION('ref_axis',(-0.981542596263219,-0.00660960394970318,0.19112939296845));
#81206=DIRECTION('center_axis',(-0.0401435546287142,-0.986495108250307,
-0.158795139787041));
#81207=DIRECTION('ref_axis',(-0.955933222817366,-0.00833899125541052,0.293465730092707));
#81208=DIRECTION('center_axis',(0.071066106982771,-0.986495108527701,0.14757035369353));
#81209=DIRECTION('ref_axis',(-0.917507506499398,-0.00660959972608852,0.397663537062072));
#81210=DIRECTION('center_axis',(-0.0733412770709218,-0.986495108148242,
-0.146452923074941));
#81211=DIRECTION('ref_axis',(-0.870497578451788,-0.00833899674706999,0.492102049419454));
#81212=DIRECTION('center_axis',(0.101127884369458,-0.986495108569774,0.128843128535705));
#81213=DIRECTION('ref_axis',(-0.810570785291136,-0.00660959938835658,0.585603377063722));
#81214=DIRECTION('center_axis',(-0.103109645269805,-0.986495108091252,-0.127262731246679));
#81215=DIRECTION('ref_axis',(-0.744358435177321,-0.00833900060649908,0.667728223942387));
#81216=DIRECTION('center_axis',(0.126461036348525,-0.986495108605844,0.104091339612869));
#81217=DIRECTION('ref_axis',(-0.665732675140154,-0.00660960231984546,0.746161053934007));
#81218=DIRECTION('center_axis',(-0.128056726462949,-0.986495108187667,-0.102121869985805));
#81219=DIRECTION('ref_axis',(-0.583413917845377,-0.0083389966343753,0.81213217003111));
#81220=DIRECTION('center_axis',(0.145881036647334,-0.986495108666972,0.0744723017157289));
#81221=DIRECTION('ref_axis',(-0.489765620838123,-0.00660966075859189,0.871829082463819));
#81222=DIRECTION('center_axis',(-0.147016016485838,-0.986495108226831,-0.0722059023984096));
#81223=DIRECTION('ref_axis',(-0.395189612230243,-0.0083389924723117,0.918561718987819));
#81224=DIRECTION('center_axis',(0.158479747416599,-0.986495108589863,0.0413711298739316));
#81225=DIRECTION('ref_axis',(-0.290897714801348,-0.00660960233039995,0.95673132732256));
#81226=DIRECTION('center_axis',(-0.159100997820152,-0.986495108218158,-0.0389136731018442));
#81227=DIRECTION('ref_axis',(-0.188486684529742,-0.00833899442689887,0.982040340783887));
#81228=DIRECTION('center_axis',(0.163668149216442,-0.986495108539713,0.00633543678716717));
#81229=DIRECTION('ref_axis',(-0.0784277380083555,-0.00660960110726281,0.996897889998818));
#81230=DIRECTION('center_axis',(0.157820536375367,0.986495107342785,0.0438187344287677));
#81231=DIRECTION('ref_axis',(-0.0842779456589509,-0.0307566094543304,0.9959674988926));
#81232=DIRECTION('center_axis',(-0.159684149326762,0.986495109228651,-0.0364468369236698));
#81233=DIRECTION('ref_axis',(-0.188062917200979,0.00584413918467036,0.982139595582546));
#81234=DIRECTION('center_axis',(0.144711044901561,0.986495107184974,0.0767210335149689));
#81235=DIRECTION('ref_axis',(-0.296411159314078,-0.0307566142160131,0.954565060808351));
#81236=DIRECTION('center_axis',(-0.148115826717113,0.986495109262762,-0.0699221086392466));
#81237=DIRECTION('ref_axis',(-0.394797092742267,0.0058441465540804,0.918749749122855));
#81238=DIRECTION('center_axis',(0.124835029133822,0.986495107315147,0.106035931383823));
#81239=DIRECTION('ref_axis',(-0.49468450248903,-0.0307566094782253,0.86852822289813));
#81240=DIRECTION('center_axis',(-0.129621774237926,0.986495109274237,-0.100127893323603));
#81241=DIRECTION('ref_axis',(-0.583070994334214,0.00584414688962944,0.81240018556943));
#81242=DIRECTION('center_axis',(0.0991218622187246,0.986495107224221,0.130392713956586));
#81243=DIRECTION('ref_axis',(-0.669826947539466,-0.0307566131833028,0.741879970814319));
#81244=DIRECTION('center_axis',(-0.105066754479679,0.986495109268846,-0.125651806559855));
#81245=DIRECTION('ref_axis',(-0.744081144306829,0.00584414342332145,0.668063692079347));
#81246=DIRECTION('center_axis',(0.0687738742096104,0.986495107341322,0.148652471953324));
#81247=DIRECTION('ref_axis',(-0.813649029250165,-0.0307566072135042,0.580542236459138));
#81248=DIRECTION('center_axis',(-0.0755989235215173,0.986495109243414,-0.145300386101388));
#81249=DIRECTION('ref_axis',(-0.870298887517183,0.0058441482875633,0.492489281423613));
#81250=DIRECTION('center_axis',(0.0352100904666574,0.986495107332255,0.159961410155238));
#81251=DIRECTION('ref_axis',(-0.919425787446233,-0.0307566086054127,0.392058990977081));
#81252=DIRECTION('center_axis',(-0.0425961788887042,0.98649510923347,-0.158154876632134));
#81253=DIRECTION('ref_axis',(-0.955822420196878,0.00584414429733773,0.293886622741517));
#81254=DIRECTION('center_axis',(-8.08933777940142E-8,0.986495107233467,
0.163790730520455));
#81255=DIRECTION('ref_axis',(-0.982211217362213,-0.0307566128273725,0.185243502599218));
#81256=DIRECTION('center_axis',(-0.00760168005488907,0.986495109258893,
-0.163614222696645));
#81257=DIRECTION('ref_axis',(-0.996652759685361,0.00584414497927649,0.0815421521730635));
#81258=DIRECTION('center_axis',(-0.0352102396399392,0.986495107333701,0.1599613773108));
#81259=DIRECTION('ref_axis',(-0.999069542386125,-0.0307566080214822,-0.0302337648894542));
#81260=DIRECTION('center_axis',(0.0277482648205711,0.986495109259409,-0.161423149537834));
#81261=DIRECTION('ref_axis',(-0.990880723998028,0.00584414488177559,-0.134615143203669));
#81262=DIRECTION('center_axis',(-0.068774016277597,0.986495107239889,0.14865240689881));
#81263=DIRECTION('ref_axis',(-0.969212485547708,-0.0307566129481366,-0.244297336494674));
#81264=DIRECTION('center_axis',(0.0618007367032491,0.986495109255772,-0.151684107135118));
#81265=DIRECTION('ref_axis',(-0.938776207478608,0.00584415113812403,-0.344477979222993));
#81266=DIRECTION('center_axis',(-0.0991219940639645,0.98649510717573,0.130392614097306));
#81267=DIRECTION('ref_axis',(-0.894036130325223,-0.0307566161811387,-0.446937834865417));
#81268=DIRECTION('center_axis',(0.0929634643369069,0.986495109244732,-0.134852488796849));
#81269=DIRECTION('ref_axis',(-0.84277555735421,0.00584414483275066,-0.538233412096903));
#81270=DIRECTION('center_axis',(-0.124835129047348,0.986495107325627,0.106035813659025));
#81271=DIRECTION('ref_axis',(-0.777055640426787,-0.0307566088079032,-0.628680016141403));
#81272=DIRECTION('center_axis',(0.119779331592666,0.986495109281869,-0.111715312675426));
#81273=DIRECTION('ref_axis',(-0.70736765939202,0.00584414874542795,-0.706821646790544));
#81274=DIRECTION('center_axis',(-0.144711118947382,0.986495107322158,0.0767208920857999));
#81275=DIRECTION('ref_axis',(-0.623740890245506,-0.0307566091489452,-0.78102582084679));
#81276=DIRECTION('center_axis',(0.14099444508826,0.986495109264767,-0.0833544590945802));
#81277=DIRECTION('ref_axis',(-0.538884035681307,0.00584414404218474,-0.842359686872682));
#81278=DIRECTION('center_axis',(-0.157820578861477,0.986495107231569,0.0438185839114293));
#81279=DIRECTION('ref_axis',(-0.441260710694636,-0.0307566129997595,-0.8968517246201));
#81280=DIRECTION('center_axis',(0.15561681786306,0.986495109242456,-0.0510960413230788));
#81281=DIRECTION('ref_axis',(-0.3452027953793,0.00584414322937402,-0.938509923257198));
#81282=DIRECTION('center_axis',(-0.163550521074303,0.986495107310167,0.00886737331046764));
#81283=DIRECTION('ref_axis',(-0.238147671140176,-0.0307566101542153,-0.970741838833751));
#81284=DIRECTION('center_axis',(0.162962721877935,0.986495109263591,-0.0164484247619832));
#81285=DIRECTION('ref_axis',(-0.135380253335906,0.00584414675128041,-0.99077647981543));
#81286=DIRECTION('center_axis',(-0.161633023909072,0.986495107269765,-0.0264984700468796));
#81287=DIRECTION('ref_axis',(-0.023899110607332,-0.0307566117760031,-0.999241143740708));
#81288=DIRECTION('center_axis',(0.162688669256186,0.98649510925121,0.0189682977384475));
#81289=DIRECTION('ref_axis',(0.0807725185426244,0.00584414601514746,-0.996715428899159));
#81290=DIRECTION('center_axis',(-0.152157746672938,0.986495107328072,-0.060625269856628));
#81291=DIRECTION('ref_axis',(0.191466946290586,-0.0307566085800032,-0.981017043433402));
#81292=DIRECTION('center_axis',(0.15480747712726,0.986495109248499,0.0534980789775261));
#81293=DIRECTION('ref_axis',(0.293148453799504,0.00584414074149075,-0.956049073036502));
#81294=DIRECTION('center_axis',(-0.135567741492699,0.986495107298358,-0.0919173038277894));
#81295=DIRECTION('ref_axis',(0.397880222564963,-0.0307566098130572,-0.916921675741425));
#81296=DIRECTION('center_axis',(0.139687655736703,0.986495109271076,0.0855263597906008));
#81297=DIRECTION('ref_axis',(0.491817096867627,0.00584414618293675,-0.870678924279261));
#81298=DIRECTION('center_axis',(-0.112638738693271,0.98649510727198,-0.118911386645828));
#81299=DIRECTION('ref_axis',(0.585689058392209,-0.0307566118478401,-0.809952071240816));
#81300=DIRECTION('center_axis',(0.118036198596492,0.986495109232562,0.113555516295446));
#81301=DIRECTION('ref_axis',(0.667488917242194,0.00584414393862002,-0.744596797831194));
#81302=DIRECTION('center_axis',(-0.0844428742116338,0.98649510726281,-0.140345303952126));
#81303=DIRECTION('ref_axis',(0.746111727528467,-0.0307566120268138,-0.665110006586217));
#81304=DIRECTION('center_axis',(0.0908654951821626,0.986495109267407,0.136274946988751));
#81305=DIRECTION('ref_axis',(0.811949699492863,0.00584414764719881,-0.583698150957948));
#81306=DIRECTION('center_axis',(-0.0522985590070483,0.986495107345266,-0.155216828693408));
#81307=DIRECTION('ref_axis',(0.871647040461356,-0.030756607696321,-0.489168138719167));
#81308=DIRECTION('center_axis',(0.0594460241246673,0.986495109265874,0.152622310329388));
#81309=DIRECTION('ref_axis',(0.918444615884464,0.00584414837009446,-0.39550642660097));
#81310=DIRECTION('center_axis',(-0.0177088158045688,0.986495107315265,-0.162830590141542));
#81311=DIRECTION('ref_axis',(0.95642510724864,-0.0307566096312886,-0.290353310965133));
#81312=DIRECTION('center_axis',(0.0252469209161744,0.986495109272428,0.161833223924607));
#81313=DIRECTION('ref_axis',(0.981994082020776,0.00584415117907665,-0.188821261443645));
#81314=DIRECTION('center_axis',(0.0177089703130797,0.986495107305418,-0.162830573397388));
#81315=DIRECTION('ref_axis',(0.996481798831909,-0.0307566097856968,-0.0779618852466596));
#81316=DIRECTION('center_axis',(-0.0101326912774383,0.98649510925592,0.163476995267305));
#81317=DIRECTION('ref_axis',(0.999626595924691,0.00584414560012706,0.0266929706518109));
#81318=DIRECTION('center_axis',(0.0522987062482193,0.986495107258488,-0.155216779633607));
#81319=DIRECTION('ref_axis',(0.989944108838892,-0.030756611577791,0.138074951455448));
#81320=DIRECTION('center_axis',(-0.0450385179583478,0.9864951092558,0.157476764363833));
#81321=DIRECTION('ref_axis',(0.97051768183973,0.00584414735009744,0.240959073658137));
#81322=DIRECTION('center_axis',(0.0844430093711828,0.986495107287759,-0.140345222453955));
#81323=DIRECTION('ref_axis',(0.937117733008439,-0.0307566099217808,0.347655555726129));
#81324=DIRECTION('center_axis',(-0.0778383928847949,0.986495109242354,0.144113094595974));
#81325=DIRECTION('ref_axis',(0.896028439172403,0.00584414839521296,0.443958198622125));
#81326=DIRECTION('center_axis',(0.112638853167697,0.98649510728676,-0.118911278087279));
#81327=DIRECTION('ref_axis',(0.840472772307255,-0.0307566098546537,0.540980175200909));
#81328=DIRECTION('center_axis',(-0.106998624069058,0.986495109229354,0.124010862080276));
#81329=DIRECTION('ref_axis',(0.779641903689181,0.00584414075326297,0.626198329629492));
#81330=DIRECTION('center_axis',(0.135567830575905,0.986495107258612,-0.0919171728664588));
#81331=DIRECTION('ref_axis',(0.704528239345761,-0.0307566120938428,0.709009161278521));
#81332=DIRECTION('center_axis',(-0.131155729272352,0.986495109286854,0.0981100098468817));
#81333=DIRECTION('ref_axis',(0.626800178425283,0.00584414786553591,0.779158124042713));
#81334=DIRECTION('center_axis',(0.15215780302399,0.986495107357182,-0.0606251279524845));
#81335=DIRECTION('ref_axis',(0.535640750317832,-0.03075660797491,0.843885666227854));
#81336=DIRECTION('center_axis',(-0.149180133269989,0.986495109263725,0.0676216476899283));
#81337=DIRECTION('ref_axis',(0.444649973888181,0.00584414774400711,0.895685350253305));
#81338=DIRECTION('center_axis',(0.161633050323747,0.986495107231132,-0.0264983103627146));
#81339=DIRECTION('ref_axis',(0.341707291870125,-0.0307566138101899,0.939303016810718));
#81340=DIRECTION('center_axis',(-0.160229039203752,0.986495109251109,0.0339713764732204));
#81341=DIRECTION('ref_axis',(0.241708429149031,0.00584414312165487,0.970331325511797));
#81342=DIRECTION('center_axis',(0.163550512813746,0.986495107277076,0.00886752934879879));
#81343=DIRECTION('ref_axis',(0.131795983805801,-0.0307566099985574,0.990799601127321));
#81344=DIRECTION('center_axis',(-0.163785815013084,0.986495109257399,-0.00126736408796769));
#81345=DIRECTION('ref_axis',(0.0274648691190149,0.0058441448589071,0.999605685725698));
#81346=DIRECTION('center_axis',(0.158221889598354,0.987363721928435,0.00887210637637829));
#81347=DIRECTION('ref_axis',(0.100091036882028,-0.0249769803935397,0.994664734866126));
#81348=DIRECTION('',(-0.603866633051807,0.,0.797085371517176));
#81349=DIRECTION('center_axis',(-0.154963408409918,0.987363721744034,0.0331545326878635));
#81350=DIRECTION('ref_axis',(0.170048762550982,-0.00640051209031499,0.985414862786157));
#81351=DIRECTION('',(-0.797085373092917,0.,-0.603866630971877));
#81352=DIRECTION('center_axis',(1.08195532252148E-14,-1.,4.32034611348363E-14));
#81353=DIRECTION('ref_axis',(9.57160757280875E-32,-4.32034611348363E-14,
-1.));
#81354=DIRECTION('center_axis',(0.148209450383285,-0.987363722419923,-0.0560966885489519));
#81355=DIRECTION('ref_axis',(0.246286329386107,-0.0180858580271892,0.96902835133805));
#81356=DIRECTION('center_axis',(0.156429989972518,0.987363721957276,-0.0253483490561554));
#81357=DIRECTION('ref_axis',(0.31157448071377,-0.0249769791829524,0.949893411640927));
#81358=DIRECTION('',(-0.418398773660791,0.,0.90826343436205));
#81359=DIRECTION('center_axis',(-0.144213205978919,0.987363721743852,0.0656919493196141));
#81360=DIRECTION('ref_axis',(0.377908184227036,-0.00640051097435485,0.925820953399464));
#81361=DIRECTION('',(-0.908263435453809,0.,-0.418398771290792));
#81362=DIRECTION('center_axis',(4.63261519963882E-14,-1.,9.30241762321944E-14));
#81363=DIRECTION('ref_axis',(-6.86840611318753E-31,-9.30241762321944E-14,
-1.));
#81364=DIRECTION('center_axis',(0.132685266333269,-0.987363722430966,-0.0866458292437413));
#81365=DIRECTION('ref_axis',(0.448840743760145,-0.0180858571215153,0.893428726039755));
#81366=DIRECTION('center_axis',(0.14732359669216,0.987363721989446,-0.0583835452574898));
#81367=DIRECTION('ref_axis',(0.508489047823086,-0.0249769762377366,0.860706128072753));
#81368=DIRECTION('',(-0.213367053339806,0.,0.976972108378273));
#81369=DIRECTION('center_axis',(-0.126719752544101,0.98736372175126,0.0951576864192368));
#81370=DIRECTION('ref_axis',(0.568097038624291,-0.00640051356442193,0.822936685372831));
#81371=DIRECTION('',(-0.976972108935031,0.,-0.213367050790503));
#81372=DIRECTION('center_axis',(3.72802973617033E-14,-1.,4.62231824842334E-14));
#81373=DIRECTION('ref_axis',(8.09500923725542E-31,-4.62231824842334E-14,
-1.));
#81374=DIRECTION('center_axis',(0.110956869526437,-0.987363722511827,-0.113143504331802));
#81375=DIRECTION('ref_axis',(0.63040786220677,-0.0180858524826944,0.776053367499854));
#81376=DIRECTION('center_axis',(0.131328515273723,0.98736372204213,-0.0886887899968879));
#81377=DIRECTION('ref_axis',(0.681627231977705,-0.0249769746314516,0.73127318244598));
#81378=DIRECTION('',(0.00164147464992936,0.,0.999998652779579));
#81379=DIRECTION('center_axis',(-0.103301029362936,0.987363721740793,0.120173950266803));
#81380=DIRECTION('ref_axis',(0.731722307361928,-0.00640050828832963,0.681572812253091));
#81381=DIRECTION('',(-0.999998652775296,0.,0.00164147725929106));
#81382=DIRECTION('center_axis',(6.95179839064118E-14,-1.,5.56925223301725E-14));
#81383=DIRECTION('ref_axis',(1.,6.95179839064117E-14,-7.46092427407147E-31));
#81384=DIRECTION('center_axis',(0.0840402488509648,-0.987363722495071,-0.134350720406496));
#81385=DIRECTION('ref_axis',(0.782497810464355,-0.0180858547525612,0.62239061567183));
#81386=DIRECTION('center_axis',(0.109192663208195,0.987363721956499,-0.114847041170904));
#81387=DIRECTION('ref_axis',(0.822893282784237,-0.0249769792256637,0.567646717296367));
#81388=DIRECTION('',(0.216573248336246,0.,0.976266371491452));
#81389=DIRECTION('center_axis',(-0.0750520550117979,0.987363721760651,0.139571021309803));
#81390=DIRECTION('ref_axis',(0.861133053975587,-0.00640051588460806,0.508339351956043));
#81391=DIRECTION('',(-0.976266370926293,0.,0.216573250883864));
#81392=DIRECTION('center_axis',(1.06486584100908E-13,-1.,5.25948673199192E-14));
#81393=DIRECTION('ref_axis',(1.,1.06486584100907E-13,1.33787268438141E-30));
#81394=DIRECTION('center_axis',(0.0531939969983551,-0.987363722423737,-0.149275846421587));
#81395=DIRECTION('ref_axis',(0.897999032444012,-0.0180858587656301,0.439625567321019));
#81396=DIRECTION('center_axis',(0.0819510774520538,0.987363722019657,-0.135635177383809));
#81397=DIRECTION('ref_axis',(0.925681760845532,-0.0249769763290022,0.377477718933682));
#81398=DIRECTION('',(0.421378297633106,0.,0.906884959784771));
#81399=DIRECTION('center_axis',(-0.04329373942725,0.987363721763552,0.152441900642943));
#81400=DIRECTION('ref_axis',(0.950278176164913,-0.00640051196046937,0.311336508221136));
#81401=DIRECTION('',(-0.906884959783822,0.,0.421378297635148));
#81402=DIRECTION('center_axis',(-4.32387482710148E-14,-1.,-1.06776602599891E-14));
#81403=DIRECTION('ref_axis',(1.,-4.32387482710148E-14,1.46181404460457E-31));
#81404=DIRECTION('center_axis',(0.0198604640486852,-0.987363722513244,-0.157220995520829));
#81405=DIRECTION('ref_axis',(0.971510815298322,-0.0180858514112591,0.236304121286785));
#81406=DIRECTION('center_axis',(0.0508775551859789,0.987363721971355,-0.150081161086825));
#81407=DIRECTION('ref_axis',(0.985186386900731,-0.0249769784355612,0.169658284836645));
#81408=DIRECTION('',(0.606480167148637,0.,0.795098614547505));
#81409=DIRECTION('',(-0.795098614022376,0.,0.606480167837084));
#81410=DIRECTION('',(0.763223696767892,0.,0.646134342603729));
#81411=DIRECTION('center_axis',(0.0247163556944388,0.987363721746886,0.156531091925291));
#81412=DIRECTION('ref_axis',(0.993175921563928,-0.0064005089879201,-0.116450085059387));
#81413=DIRECTION('',(-0.646134340612186,0.,0.763223698453904));
#81414=DIRECTION('center_axis',(5.83011444394288E-14,-1.,-1.12862629103633E-14));
#81415=DIRECTION('ref_axis',(1.,5.83011444394288E-14,1.62924502720985E-31));
#81416=DIRECTION('center_axis',(-0.0479905205830286,-0.987363722406496,
-0.151029101863708));
#81417=DIRECTION('ref_axis',(0.98094086059819,-0.0180858583824029,-0.19346299319367));
#81418=DIRECTION('center_axis',(-0.0168422276470354,0.987363722007276,-0.157572903228392));
#81419=DIRECTION('ref_axis',(0.965368612718929,-0.0249769765126249,-0.259691340289618));
#81420=DIRECTION('',(0.884279734078537,0.,0.466957548282488));
#81421=DIRECTION('center_axis',(0.0577880595905376,0.987363721746732,0.147558195798141));
#81422=DIRECTION('ref_axis',(0.944922693933094,-0.00640050965701902,-0.327231013148746));
#81423=DIRECTION('',(-0.466957545975081,0.,0.884279735296999));
#81424=DIRECTION('center_axis',(9.53957954715973E-14,-1.,-4.12219832883748E-14));
#81425=DIRECTION('ref_axis',(1.,9.53957954715972E-14,-5.76930804743858E-31));
#81426=DIRECTION('center_axis',(-0.079335316354445,-0.987363722508174,-0.137181584236888));
#81427=DIRECTION('ref_axis',(0.916418183908204,-0.0180858529151483,-0.399813224051833));
#81428=DIRECTION('center_axis',(-0.0503219807862601,0.987363721992186,-0.150268355762234));
#81429=DIRECTION('ref_axis',(0.886972870654081,-0.0249769774602344,-0.461145614009946));
#81430=DIRECTION('',(0.96398783550857,0.,0.265946334796144));
#81431=DIRECTION('center_axis',(0.0881576574204831,0.987363721749088,0.131685642390972));
#81432=DIRECTION('ref_axis',(0.852485931692217,-0.00640051001953579,-0.522710981076868));
#81433=DIRECTION('',(-0.265946332280708,0.,0.963987836202532));
#81434=DIRECTION('center_axis',(-1.20434267092608E-14,-1.,8.68078748888327E-15));
#81435=DIRECTION('ref_axis',(1.,-1.20434267092608E-14,1.38984695640427E-31));
#81436=DIRECTION('center_axis',(-0.106970488036425,-0.987363722454144,-0.116919606015178));
#81437=DIRECTION('ref_axis',(0.80904481124605,-0.0180858550211184,-0.587468633412881));
#81438=DIRECTION('center_axis',(-0.0814487377651023,0.98736372201617,-0.135937425173668));
#81439=DIRECTION('ref_axis',(0.767103261833128,-0.0249769747251451,-0.641037234814449));
#81440=DIRECTION('',(0.998620936282989,0.,0.0524997677831598));
#81441=DIRECTION('center_axis',(0.11440510064347,0.987363721729216,0.109655615267929));
#81442=DIRECTION('ref_axis',(0.720187874107375,-0.006400509403508,-0.693749565382261));
#81443=DIRECTION('',(-0.0524997650266615,0.,0.998620936427905));
#81444=DIRECTION('center_axis',(3.95829814884668E-14,-1.,-4.42672649531729E-14));
#81445=DIRECTION('ref_axis',(1.02946627009731E-30,4.42672649531729E-14,
-1.));
#81446=DIRECTION('center_axis',(-0.129603834006006,-0.987363722534076,-0.0911906005824955));
#81447=DIRECTION('ref_axis',(0.663841403133051,-0.0180858512043145,-0.747654661907861));
#81448=DIRECTION('center_axis',(-0.10876703762367,0.987363722001739,-0.115250214756607));
#81449=DIRECTION('ref_axis',(0.611364755852421,-0.0249769779150519,-0.790954667396141));
#81450=DIRECTION('',(0.986559631844411,0.,-0.163401630392784));
#81451=DIRECTION('center_axis',(0.135303090156659,0.987363721761573,0.0824982105454026));
#81452=DIRECTION('ref_axis',(0.554214631875562,-0.00640051217383139,-0.832349190700002));
#81453=DIRECTION('',(0.163401630169058,0.,0.986559631881466));
#81454=DIRECTION('center_axis',(0.,-1.,0.));
#81455=DIRECTION('ref_axis',(0.,0.,-1.));
#81456=DIRECTION('center_axis',(-0.14617705262823,-0.987363722526724,-0.0611976202404424));
#81457=DIRECTION('ref_axis',(0.487597508052115,-0.0180858528629753,-0.872881190121305));
#81458=DIRECTION('center_axis',(-0.130999513960469,0.987363721983204,-0.0891740312736589));
#81459=DIRECTION('ref_axis',(0.427039517577206,-0.0249769778724014,-0.903887936087096));
#81460=DIRECTION('',(0.928367895516495,0.,-0.371662549329729));
#81461=DIRECTION('center_axis',(0.149874454652235,0.987363721755551,0.0514832866445296));
#81462=DIRECTION('ref_axis',(0.362326932246914,-0.00640050910465206,-0.932029091633808));
#81463=DIRECTION('',(0.371662549274472,0.,0.928367895538617));
#81464=DIRECTION('center_axis',(-8.66859946722313E-15,-1.,2.8398172054035E-14));
#81465=DIRECTION('ref_axis',(-5.66160437743644E-32,-2.8398172054035E-14,
-1.));
#81466=DIRECTION('center_axis',(-0.155915195724191,-0.987363722398575,-0.0283431020447134));
#81467=DIRECTION('ref_axis',(0.288554093317215,-0.0180858593659295,-0.957292764477449));
#81468=DIRECTION('center_axis',(-0.147106600945047,0.987363722109429,-0.0589281615240848));
#81469=DIRECTION('ref_axis',(0.222746379323286,-0.0249769709087309,-0.974556412642486));
#81470=DIRECTION('',(0.826766709702495,0.,-0.562544938407333));
#81471=DIRECTION('center_axis',(0.157437857984951,0.987363721756996,0.0180610584209056));
#81472=DIRECTION('ref_axis',(0.153497224345565,-0.00640050896740749,-0.988128349761895));
#81473=DIRECTION('',(0.562544940564669,0.,0.82676670823461));
#81474=DIRECTION('center_axis',(5.90291219470682E-15,-1.,-7.39943279675939E-14));
#81475=DIRECTION('ref_axis',(1.21247827875496E-31,7.39943279675939E-14,
-1.));
#81476=DIRECTION('center_axis',(-0.158362913987082,-0.987363722452981,0.00583669917960967));
#81477=DIRECTION('ref_axis',(0.0760182140121149,-0.0180858566325272,-0.996942391980738));
#81478=DIRECTION('center_axis',(-0.156335142857511,0.987363722076235,-0.025926886343826));
#81479=DIRECTION('ref_axis',(0.00803787335697108,-0.0249769739436616,-0.999655712415287));
#81480=DIRECTION('',(0.686506828721979,0.,-0.727123355503103));
#81481=DIRECTION('center_axis',(0.157639641237614,0.987363721764162,-0.0162056920401103));
#81482=DIRECTION('ref_axis',(-0.0625098404813812,-0.00640051662167854,-0.998023823979151));
#81483=DIRECTION('',(0.727123357294462,0.,0.686506826824636));
#81484=DIRECTION('center_axis',(2.02833757503951E-15,-1.,1.47066666834218E-14));
#81485=DIRECTION('ref_axis',(3.92305911876007E-32,-1.47066666834218E-14,
-1.));
#81486=DIRECTION('center_axis',(-0.15340575975138,-0.987363722449015,0.0397435839693258));
#81487=DIRECTION('ref_axis',(-0.140072193470226,-0.0180858549598506,-0.989976101967523));
#81488=DIRECTION('center_axis',(-0.158253628115571,0.987363722083096,0.00828670637064815));
#81489=DIRECTION('ref_axis',(-0.207046477588685,-0.0249769721149615,-0.978012222307107));
#81490=DIRECTION('',(0.514146654526065,0.,-0.857702289631814));
#81491=DIRECTION('center_axis',(0.150470370386449,0.987363721772875,-0.0497146715022924));
#81492=DIRECTION('ref_axis',(-0.275594018979377,-0.00640051236263403,-0.961252812814761));
#81493=DIRECTION('',(0.857702290213478,0.,0.51414665355573));
#81494=DIRECTION('center_axis',(1.02848295574032E-14,-1.,2.78536007243207E-14));
#81495=DIRECTION('ref_axis',(-1.81250816775491E-31,-2.78536007243207E-14,
-1.));
#81496=DIRECTION('center_axis',(-0.141275521246826,-0.987363722413841,0.071792107905542));
#81497=DIRECTION('ref_axis',(-0.349612983833228,-0.0180858580766434,-0.936719628956743));
#81498=DIRECTION('center_axis',(-0.152772350370556,0.987363722030341,0.0421128172965009));
#81499=DIRECTION('ref_axis',(-0.412449562440443,-0.0249769746789723,-0.910637968228084));
#81500=DIRECTION('',(0.317745554014209,0.,-0.948176018945957));
#81501=DIRECTION('center_axis',(0.136265268983339,0.987363721760609,-0.0808990569780495));
#81502=DIRECTION('ref_axis',(-0.475791723949279,-0.00640051838988543,-0.87953468879045));
#81503=DIRECTION('',(0.948176020641203,0.,0.317745548955471));
#81504=DIRECTION('center_axis',(-4.00801918993373E-14,-1.,-6.2478661667528E-14));
#81505=DIRECTION('ref_axis',(1.14695610830292E-30,6.2478661667528E-14,-1.));
#81506=DIRECTION('center_axis',(-0.122539399999297,-0.987363722490077,0.100483704939411));
#81507=DIRECTION('ref_axis',(-0.542806256612586,-0.0180858529120981,-0.83966318825269));
#81508=DIRECTION('center_axis',(-0.140147609257795,0.987363721954357,0.0739697788814082));
#81509=DIRECTION('ref_axis',(-0.598566966055042,-0.0249769790975152,-0.800683294232385));
#81510=DIRECTION('',(0.106487020589929,0.,-0.99431409245061));
#81511=DIRECTION('center_axis',(0.115688560696546,0.987363721765323,-0.108300682664935));
#81512=DIRECTION('ref_axis',(-0.653741935995577,-0.00640051286148278,-0.756690501166669));
#81513=DIRECTION('',(0.994314092728476,0.,0.10648701799538));
#81514=DIRECTION('center_axis',(-4.20593637613534E-14,-1.,-4.19215110370194E-14));
#81515=DIRECTION('ref_axis',(1.,-4.20593637613534E-14,-8.90057686802853E-31));
#81516=DIRECTION('center_axis',(-0.0980734667160037,-0.987363722423222,
0.124476804139819));
#81517=DIRECTION('ref_axis',(-0.710618513547246,-0.0180858582164273,-0.703345029083506));
#81518=DIRECTION('center_axis',(-0.120969720893936,0.987363721921982,0.102367999195127));
#81519=DIRECTION('ref_axis',(-0.756696041964833,-0.0249769798023517,-0.653289561033014));
#81520=DIRECTION('',(-0.109750725713721,0.,-0.993959143126774));
#81521=DIRECTION('center_axis',(0.0897023821862004,0.987363721754206,-0.130638292984115));
#81522=DIRECTION('ref_axis',(-0.801123903692137,-0.00640051127421329,-0.598464305024535));
#81523=DIRECTION('',(0.993959142840391,0.,-0.109750728307355));
#81524=DIRECTION('center_axis',(-1.25219812285885E-14,-1.,-7.97497236843094E-15));
#81525=DIRECTION('ref_axis',(1.,-1.25219812285885E-14,2.06168302278434E-31));
#81526=DIRECTION('center_axis',(-0.0690217308745455,-0.987363722442943,
0.142649501473708));
#81527=DIRECTION('ref_axis',(-0.845203037920175,-0.0180858574324823,-0.53413923882396));
#81528=DIRECTION('center_axis',(-0.0961354190219717,0.987363721992652,0.125979608279625));
#81529=DIRECTION('ref_axis',(-0.879442854871605,-0.0249769765036889,-0.47534873057579));
#81530=DIRECTION('',(-0.320856647098721,0.,-0.947127769634365));
#81531=DIRECTION('center_axis',(0.05952181604836,0.987363721737319,-0.146867404182599));
#81532=DIRECTION('ref_axis',(-0.911046207097607,-0.00640051453204226,-0.412254583900276));
#81533=DIRECTION('',(0.947127767923488,0.,-0.320856652149012));
#81534=DIRECTION('center_axis',(2.78872151609101E-14,-1.,1.01933322533513E-14));
#81535=DIRECTION('ref_axis',(1.,2.78872151609101E-14,-1.63004772219339E-31));
#81536=DIRECTION('center_axis',(-0.0367426203520342,-0.987363722519182,
0.154152065515615));
#81537=DIRECTION('ref_axis',(-0.940266807613487,-0.0180858519364689,-0.339957692161941));
#81538=DIRECTION('center_axis',(-0.0668059397156617,0.987363721932429,0.143700546381871));
#81539=DIRECTION('ref_axis',(-0.961067894383304,-0.0249769815637861,-0.275181127219154));
#81540=DIRECTION('',(-0.516959673446092,0.,-0.856009752298717));
#81541=DIRECTION('center_axis',(0.0265580802596591,0.98736372174745,-0.156229156529586));
#81542=DIRECTION('ref_axis',(-0.978369002212705,-0.00640051292843176,-0.20676829772373));
#81543=DIRECTION('',(0.856009751718059,0.,-0.516959674407576));
#81544=DIRECTION('center_axis',(-7.35662317542014E-14,-1.,-9.90022723198433E-15));
#81545=DIRECTION('ref_axis',(1.,-7.35662317542014E-14,-1.38171261729452E-31));
#81546=DIRECTION('center_axis',(-0.00274545652003569,-0.987363722462837,
0.158446653586706));
#81547=DIRECTION('ref_axis',(-0.991364746987655,-0.018085856216804,-0.129880099457186));
#81548=DIRECTION('center_axis',(-0.034352680445948,0.987363721984285,0.154702210247681));
#81549=DIRECTION('ref_axis',(-0.997754469338468,-0.02497697794916,-0.0621463553850053));
#81550=DIRECTION('',(-0.688890236015648,0.,-0.724865672191962));
#81551=DIRECTION('center_axis',(-0.00764747800342432,0.987363721777915,
-0.15828580794579));
#81552=DIRECTION('ref_axis',(-0.999944350655294,-0.00640050754420234,0.00838624443593926));
#81553=DIRECTION('',(0.72486567039439,0.,-0.688890237907094));
#81554=DIRECTION('center_axis',(-4.43847301375668E-14,-1.,3.68747987600371E-15));
#81555=DIRECTION('ref_axis',(1.,-4.43847301375668E-14,-8.92032631172152E-32));
#81556=DIRECTION('center_axis',(0.0313800724015774,-0.987363722539182,0.155332451437688));
#81557=DIRECTION('ref_axis',(-0.996107572444681,-0.0180858510767603,0.0862705402161922));
#81558=DIRECTION('center_axis',(-0.000293129977269768,0.987363722010763,
0.158470169217646));
#81559=DIRECTION('ref_axis',(-0.987787153673095,-0.0249769763228967,0.153794309687225));
#81560=DIRECTION('',(-0.828609057310836,0.,-0.559827678971349));
#81561=DIRECTION('center_axis',(-0.0414954703147962,0.987363721637735,-0.152941188490987));
#81562=DIRECTION('ref_axis',(-0.974763412214174,-0.00640052409804163,0.22314865784909));
#81563=DIRECTION('',(0.559827676809204,0.,-0.828609058771632));
#81564=DIRECTION('center_axis',(0.0337800681979452,0.987363721247363,0.154828256326492));
#81565=DIRECTION('ref_axis',(-0.931631996025623,-0.0249770413045674,0.36254375099977));
#81566=DIRECTION('',(-0.929583040653769,0.,-0.368612765010781));
#81567=DIRECTION('center_axis',(-2.83695604196629E-14,-1.,8.76178241451945E-15));
#81568=DIRECTION('ref_axis',(1.,-2.83695604196629E-14,-1.9346427804638E-31));
#81569=DIRECTION('center_axis',(0.0640383594408077,-0.987363723068623,0.144955051268308));
#81570=DIRECTION('ref_axis',(-0.95427351150155,-0.0180859060603392,0.298387273938547));
#81571=DIRECTION('',(0.368612762585142,0.,-0.929583041615621));
#81572=DIRECTION('center_axis',(-0.0734031508739946,0.987363721755664,-0.140445214950786));
#81573=DIRECTION('ref_axis',(-0.904003620306502,-0.00640050963073223,0.427476885865428));
#81574=DIRECTION('center_axis',(-5.16455433471228E-14,-1.,2.93111074408959E-14));
#81575=DIRECTION('ref_axis',(1.,-5.16455433471228E-14,2.52306462361569E-31));
#81576=DIRECTION('center_axis',(0.0662738594893761,0.987363722011568,0.143946712375955));
#81577=DIRECTION('ref_axis',(-0.831914785709354,-0.0249769763266405,0.554340996113167));
#81578=DIRECTION('center_axis',(0.0937021887535035,-0.987363722499099,0.12779976258008));
#81579=DIRECTION('ref_axis',(-0.867818688045048,-0.0180858544134419,0.49655173602547));
#81580=DIRECTION('',(-0.987090754263963,0.,-0.160161926957068));
#81581=DIRECTION('center_axis',(-0.101878596556153,0.987363721764728,-0.121382175407489));
#81582=DIRECTION('ref_axis',(-0.79097362430467,-0.00640051099472303,0.611816769231884));
#81583=DIRECTION('',(0.160161927182448,0.,-0.987090754227393));
#81584=DIRECTION('center_axis',(-5.51713469867962E-14,-1.,4.96601190447716E-14));
#81585=DIRECTION('ref_axis',(1.,-5.51713469867962E-14,3.54595632905444E-31));
#81586=DIRECTION('center_axis',(0.118984656681206,-0.987363722441525,0.104668672872408));
#81587=DIRECTION('ref_axis',(-0.740785623688482,-0.018085856711078,0.671497998153005));
#81588=DIRECTION('center_axis',(0.0956687054159054,0.987363722097152,0.126334393933332));
#81589=DIRECTION('ref_axis',(-0.693298151125857,-0.0249769713557858,0.720217900740714));
#81590=DIRECTION('',(-0.998443201024793,0.,0.0557779017834631));
#81591=DIRECTION('center_axis',(-0.125590310399083,0.987363721769394,-0.0966434419272879));
#81592=DIRECTION('ref_axis',(-0.640958581238794,-0.00640050978831664,0.767548780606681));
#81593=DIRECTION('',(-0.0557779043887846,0.,-0.998443200879247));
#81594=DIRECTION('center_axis',(-6.04884194119145E-14,-1.,8.45030224620041E-14));
#81595=DIRECTION('ref_axis',(-1.33009085890558E-30,-8.45030224620041E-14,
-1.));
#81596=DIRECTION('center_axis',(0.1387035322197,-0.987363722447262,0.0766433933543153));
#81597=DIRECTION('ref_axis',(-0.579114246483947,-0.0180858566454766,0.815045760254434));
#81598=DIRECTION('center_axis',(0.120590181118975,0.987363722004324,0.102814827177119));
#81599=DIRECTION('ref_axis',(-0.522263667215958,-0.0249769772189026,0.852418214560872));
#81600=DIRECTION('',(-0.963109553688447,0.,0.269109620032506));
#81601=DIRECTION('center_axis',(-0.1434295647149,0.987363721767691,-0.0673857618696123));
#81602=DIRECTION('ref_axis',(-0.460973024805055,-0.00640051594299878,0.887391065876675));
#81603=DIRECTION('',(-0.26910962254562,0.,-0.963109552986239));
#81604=DIRECTION('center_axis',(3.50644987367232E-14,-1.,-8.18833808057458E-14));
#81605=DIRECTION('ref_axis',(-1.55431794060648E-31,8.18833808057458E-14,
-1.));
#81606=DIRECTION('center_axis',(0.151936786191621,-0.987363722382686,0.0450343504934522));
#81607=DIRECTION('ref_axis',(-0.390364131367923,-0.0180858605302077,0.920482887722661));
#81608=DIRECTION('center_axis',(0.139872998404293,0.987363721998246,0.0744877493227145));
#81609=DIRECTION('ref_axis',(-0.326808714331911,-0.0249769771506971,0.944760400762615));
#81610=DIRECTION('',(-0.882741973773198,0.,0.469858071910016));
#81611=DIRECTION('center_axis',(-0.154562207340053,0.987363721737865,-0.0349772076947687));
#81612=DIRECTION('ref_axis',(-0.259432884589524,-0.00640051184677438,0.965739929712787));
#81613=DIRECTION('',(-0.469858074213424,0.,-0.882741972547161));
#81614=DIRECTION('center_axis',(1.10948025608841E-14,-1.,-5.83378824764552E-14));
#81615=DIRECTION('ref_axis',(7.37852326003163E-32,5.83378824764552E-14,
-1.));
#81616=DIRECTION('center_axis',(0.158065641712028,-0.987363722473558,0.0113195606506427));
#81617=DIRECTION('ref_axis',(-0.183361024325124,-0.0180858544734437,0.982879258417028));
#81618=DIRECTION('center_axis',(0.152615509613344,0.987363721963071,0.0426777081939762));
#81619=DIRECTION('ref_axis',(-0.11607254932281,-0.0249769782048113,0.992926640720985));
#81620=DIRECTION('',(-0.761098361889465,0.,0.648636480263925));
#81621=DIRECTION('center_axis',(8.52754015441823E-16,-1.,2.96795148658844E-14));
#81622=DIRECTION('ref_axis',(0.0287202214020975,2.96917630343014E-14,0.999587489358793));
#81623=DIRECTION('center_axis',(0.156803525494539,-0.987363722442378,-0.0229245282877005));
#81624=DIRECTION('ref_axis',(0.0322158416459406,-0.0180858578001288,0.999317287599227));
#81625=DIRECTION('center_axis',(-0.158467694455886,0.98736372175334,-0.000933155522557501));
#81626=DIRECTION('ref_axis',(-0.0457619486551963,-0.00640051033716772,0.998931868308697));
#81627=DIRECTION('',(-0.648636483669163,0.,-0.761098358987394));
#81628=DIRECTION('center_axis',(-0.154002425234077,-0.987363721934798,-0.0373648715919747));
#81629=DIRECTION('ref_axis',(-0.156828000124788,-0.0129106125839618,0.987541540624781));
#81630=DIRECTION('',(0.562308454249505,0.,0.826927567734643));
#81631=DIRECTION('',(0.826927567205404,0.,-0.562308455027801));
#81632=DIRECTION('center_axis',(0.153257640420856,-0.987363719698522,0.0403110490527193));
#81633=DIRECTION('ref_axis',(-0.22011157129971,0.00565948153778567,0.97545828534525));
#81634=DIRECTION('center_axis',(-0.142369591901464,-0.987363721987792,-0.0695972686549175));
#81635=DIRECTION('ref_axis',(-0.365453688647701,-0.0129106102549393,0.930739983881983));
#81636=DIRECTION('',(0.371397010878143,0.,0.928474157050578));
#81637=DIRECTION('center_axis',(-1.73534424515167E-14,-1.,5.67913830243607E-14));
#81638=DIRECTION('ref_axis',(-1.40584472586084E-31,-5.67913830243607E-14,
-1.));
#81639=DIRECTION('center_axis',(0.151221679661691,0.987363722237908,0.0473802027095796));
#81640=DIRECTION('ref_axis',(-0.22122754271641,-0.0129109223179644,0.975136750629653));
#81641=DIRECTION('center_axis',(-0.145446249487498,0.987363722234589,-0.0629147719146933));
#81642=DIRECTION('ref_axis',(-0.294783644363712,0.0174544460973992,0.955404597710876));
#81643=DIRECTION('',(0.928474157301366,0.,-0.371397010251184));
#81644=DIRECTION('center_axis',(0.141008876239464,-0.987363719704729,0.0723144648913742));
#81645=DIRECTION('ref_axis',(-0.424660181785132,0.00565948540464467,0.905335131446457));
#81646=DIRECTION('center_axis',(-0.124079714504303,-0.98736372202158,-0.098575376662847));
#81647=DIRECTION('ref_axis',(-0.55699116933223,-0.0129106097786204,0.830418059438172));
#81648=DIRECTION('',(0.163119455793019,0.,0.98660632632362));
#81649=DIRECTION('center_axis',(-1.45780985909293E-14,-1.,2.58665774076789E-14));
#81650=DIRECTION('ref_axis',(-2.79864733334849E-31,-2.58665774076789E-14,
-1.));
#81651=DIRECTION('center_axis',(0.137500856816951,0.987363722241852,0.0787806726000697));
#81652=DIRECTION('ref_axis',(-0.425680940306143,-0.0129109245961234,0.904781213933043));
#81653=DIRECTION('center_axis',(-0.128520982733433,0.987363722311966,-0.0927105002655624));
#81654=DIRECTION('ref_axis',(-0.493275513135145,0.0174544420981305,0.869697999648328));
#81655=DIRECTION('',(0.98660632651026,0.,-0.163119454664154));
#81656=DIRECTION('center_axis',(0.122166697612528,-0.98736371968855,0.10093652974637));
#81657=DIRECTION('ref_axis',(-0.609352153792431,0.00565948107801637,0.792879513509116));
#81658=DIRECTION('center_axis',(-0.0999880073936607,-0.987363722004062,
-0.122944210305859));
#81659=DIRECTION('ref_axis',(-0.722484361105512,-0.0129106101685073,0.691266709818314));
#81660=DIRECTION('',(-0.052785381049886,0.,0.998605879988406));
#81661=DIRECTION('center_axis',(2.9696730449051E-14,-1.,-3.31919564300345E-14));
#81662=DIRECTION('ref_axis',(-2.71405253502507E-32,3.31919564300345E-14,
-1.));
#81663=DIRECTION('center_axis',(0.11735064596239,0.987363722220979,0.106497445669567));
#81664=DIRECTION('ref_axis',(-0.610229972424937,-0.0129109267773616,0.79211911271223));
#81665=DIRECTION('center_axis',(-0.105586214396424,0.9873637222575,-0.118171194879493));
#81666=DIRECTION('ref_axis',(-0.668702368113783,0.0174544451919355,0.743325288969816));
#81667=DIRECTION('',(0.998605879960773,0.,0.0527853815726573));
#81668=DIRECTION('center_axis',(0.0976121372020436,-0.987363719722958,0.124838918794155));
#81669=DIRECTION('ref_axis',(-0.765551498855408,0.00565948133520904,0.643349728274797));
#81670=DIRECTION('center_axis',(-0.0712209754792646,-0.987363722077632,
-0.141564306860121));
#81671=DIRECTION('ref_axis',(-0.854194986236279,-0.0129106066366808,0.519792498719515));
#81672=DIRECTION('',(-0.266222032663715,0.,0.963911733160459));
#81673=DIRECTION('center_axis',(9.63672715364679E-14,-1.,-6.94187404808866E-14));
#81674=DIRECTION('ref_axis',(1.,9.63672715364678E-14,-1.77223350769445E-30));
#81675=DIRECTION('center_axis',(0.0917132479702667,0.987363722209605,0.129234516330349));
#81676=DIRECTION('ref_axis',(-0.766245330217187,-0.0129109294373159,0.642418400905063));
#81677=DIRECTION('center_axis',(-0.0777143582214746,0.987363722327266,-0.138106329899358));
#81678=DIRECTION('ref_axis',(-0.812861441870596,0.0174544398692866,0.582195515998624));
#81679=DIRECTION('',(0.96391173298069,0.,0.266222033314604));
#81680=DIRECTION('center_axis',(0.068493335254789,-0.98736371970251,0.142903981893081));
#81681=DIRECTION('ref_axis',(-0.885954504802779,0.00565948925795247,0.463737625819819));
#81682=DIRECTION('center_axis',(-0.03912372399873,-0.98736372203281,-0.153565017611393));
#81683=DIRECTION('ref_axis',(-0.945964404768215,-0.012910609960063,0.324013365560705));
#81684=DIRECTION('',(-0.467210440327732,0.,0.884146144282022));
#81685=DIRECTION('center_axis',(-1.36296544362407E-14,-1.,5.8849567649498E-15));
#81686=DIRECTION('ref_axis',(1.,-1.36296544362407E-14,-9.90844762885813E-32));
#81687=DIRECTION('center_axis',(0.061787444507619,0.987363722220606,0.145928721449507));
#81688=DIRECTION('ref_axis',(-0.886431907160726,-0.012910926851988,0.462678918835968));
#81689=DIRECTION('center_axis',(-0.0462086621742918,0.987363722352972,-0.151583769979986));
#81690=DIRECTION('ref_axis',(-0.919012019491634,0.0174544387401066,0.393842926302068));
#81691=DIRECTION('',(0.884146145154076,0.,0.467210438677464));
#81692=DIRECTION('center_axis',(0.0361718722602125,-0.987363719711651,0.154287007406209));
#81693=DIRECTION('ref_axis',(-0.964931262274253,0.00565948410852384,0.262441668424515));
#81694=DIRECTION('center_axis',(-0.00519709259350015,-0.987363721985343,
-0.15838519733809));
#81695=DIRECTION('ref_axis',(-0.993501578246324,-0.0129106113742557,0.113083730642412));
#81696=DIRECTION('',(-0.64635260602278,0.,0.763038864467309));
#81697=DIRECTION('center_axis',(-8.74565546649098E-14,-1.,1.69043816072292E-14));
#81698=DIRECTION('ref_axis',(1.,-8.74565546649098E-14,4.47822014116462E-31));
#81699=DIRECTION('center_axis',(0.0289725258709897,0.987363722235357,0.155799463279547));
#81700=DIRECTION('ref_axis',(-0.965169912231812,-0.0129109281183902,0.261305086933948));
#81701=DIRECTION('center_axis',(-0.0125422923522538,0.987363722231902,-0.157973323453408));
#81702=DIRECTION('ref_axis',(-0.982190616805527,0.0174544457418185,0.187074676487826));
#81703=DIRECTION('',(0.763038865448696,0.,0.646352604864224));
#81704=DIRECTION('center_axis',(0.00215905541530509,-0.987363719712137,
0.15845574611205));
#81705=DIRECTION('ref_axis',(-0.998788906524019,0.00565947699061602,0.0488742317049259));
#81706=DIRECTION('center_axis',(0.0289725475431906,-0.987363722006681,-0.155799460698588));
#81707=DIRECTION('ref_axis',(-0.994583722670036,-0.0129106105555476,-0.103133577145834));
#81708=DIRECTION('',(-0.795272041985628,0.,0.606252735446208));
#81709=DIRECTION('center_axis',(0.,-1.,0.));
#81710=DIRECTION('ref_axis',(0.,0.,-1.));
#81711=DIRECTION('center_axis',(-0.00519711222669223,0.987363722216384,
0.158385195253569));
#81712=DIRECTION('ref_axis',(-0.998777645603758,-0.0129109255541131,0.0477129190424396));
#81713=DIRECTION('center_axis',(0.0217105317550711,0.987363722287536,-0.156976217056641));
#81714=DIRECTION('ref_axis',(-0.99944307160964,0.0174544431624296,-0.028440974409791));
#81715=DIRECTION('',(0.606252735341353,0.,0.795272042065561));
#81716=DIRECTION('center_axis',(-0.0319547269489774,-0.987363719689367,
0.155215271371064));
#81717=DIRECTION('ref_axis',(-0.985944291779663,0.00565948020654221,-0.166978512961669));
#81718=DIRECTION('center_axis',(0.061787468866819,-0.987363721901482,-0.145928713294833));
#81719=DIRECTION('ref_axis',(-0.949160236890853,-0.0129106152611583,-0.314528473621829));
#81720=DIRECTION('',(-0.907005440776329,0.,0.421118902926641));
#81721=DIRECTION('center_axis',(-4.32356925031948E-14,-1.,-1.06900264805193E-14));
#81722=DIRECTION('ref_axis',(1.,-4.32356925031948E-14,1.79016941821345E-31));
#81723=DIRECTION('center_axis',(-0.0391237430712795,0.987363722200939,0.15356501167128));
#81724=DIRECTION('ref_axis',(-0.985683646016057,-0.0129109264441407,-0.168110255352985));
#81725=DIRECTION('center_axis',(0.0549482001638952,0.987363722238535,-0.148639077318224));
#81726=DIRECTION('ref_axis',(-0.969962679413179,0.0174544454904423,-0.242626756311474));
#81727=DIRECTION('',(0.421118902314201,0.,0.907005441060682));
#81728=DIRECTION('center_axis',(-0.064574338796006,-0.987363719700537,0.144717102611194));
#81729=DIRECTION('ref_axis',(-0.926998018391755,0.00565948096684053,-0.375023524826038));
#81730=DIRECTION('center_axis',(0.0917132688626462,-0.987363721970692,-0.129234503329062));
#81731=DIRECTION('ref_axis',(-0.859355073458652,-0.0129106117045736,-0.511216366938979));
#81732=DIRECTION('',(-0.9763282731838,0.,0.216294019755377));
#81733=DIRECTION('center_axis',(-1.33089421047624E-14,-1.,-6.57816514610932E-15));
#81734=DIRECTION('ref_axis',(1.,-1.33089421047624E-14,-6.18048586043692E-32));
#81735=DIRECTION('center_axis',(-0.0712209911166728,0.987363722215975,0.141564298028046));
#81736=DIRECTION('ref_axis',(-0.926500175100293,-0.0129109281555154,-0.37607277683088));
#81737=DIRECTION('center_axis',(0.0856165460212759,0.987363722297612,-0.133351741413418));
#81738=DIRECTION('ref_axis',(-0.895127910167366,0.0174544412333558,-0.445467582345378));
#81739=DIRECTION('',(0.216294019096123,0.,0.97632827332985));
#81740=DIRECTION('center_axis',(-0.0941745270390424,-0.987363719687872,
0.127452122387594));
#81741=DIRECTION('ref_axis',(-0.82470634699939,0.00565948217092306,-0.565532856234258));
#81742=DIRECTION('center_axis',(0.117350661423251,-0.987363721986634,-0.106497430805754));
#81743=DIRECTION('ref_axis',(-0.729367422684911,-0.0129106116023004,-0.684000350024783));
#81744=DIRECTION('',(-0.999999081357214,0.,0.00135546476455657));
#81745=DIRECTION('center_axis',(1.15836753776633E-14,-1.,9.28540044415546E-15));
#81746=DIRECTION('ref_axis',(1.,1.15836753776633E-14,-1.75050267875677E-31));
#81747=DIRECTION('center_axis',(-0.0999880263442184,0.987363722188352,0.122944193413724));
#81748=DIRECTION('ref_axis',(-0.823994584277942,-0.0129109315438825,-0.566450556471869));
#81749=DIRECTION('center_axis',(0.112281563017468,0.987363722285881,-0.111829023603552));
#81750=DIRECTION('ref_axis',(-0.778437954930438,0.0174544436516842,-0.627478838464317));
#81751=DIRECTION('',(0.00135546408934942,0.,0.999999081358129));
#81752=DIRECTION('center_axis',(-0.119371216758459,-0.987363719705103,0.10422762407207));
#81753=DIRECTION('ref_axis',(-0.683852325090944,0.00565948098279108,-0.729598497629152));
#81754=DIRECTION('center_axis',(0.137500865949824,-0.987363722045799,-0.0787806591170389));
#81755=DIRECTION('ref_axis',(-0.565275361749489,-0.0129106086395355,-0.82480123762246));
#81756=DIRECTION('',(-0.976911043828257,0.,-0.213646466028307));
#81757=DIRECTION('center_axis',(-2.7950306566047E-14,-1.,-3.4675382181889E-14));
#81758=DIRECTION('ref_axis',(-5.33496938660793E-31,3.4675382181889E-14,
-1.));
#81759=DIRECTION('center_axis',(-0.12407972669933,0.987363722202763,0.0985753594978235));
#81760=DIRECTION('ref_axis',(-0.682959926175101,-0.0129109281602422,-0.730341733144794));
#81761=DIRECTION('center_axis',(0.133696416719564,0.987363722290334,-0.0850773063826399));
#81762=DIRECTION('ref_axis',(-0.625349106696063,0.0174544434909131,-0.780149881213128));
#81763=DIRECTION('',(-0.213646469431568,0.,0.976911043083978));
#81764=DIRECTION('center_axis',(-0.138986243896786,-0.987363719681023,0.0761295544786478));
#81765=DIRECTION('ref_axis',(-0.511022127211816,0.00565948406729928,-0.859548925739543));
#81766=DIRECTION('center_axis',(0.151221685925258,-0.987363722020143,-0.0473801872564035));
#81767=DIRECTION('ref_axis',(-0.374751652353903,-0.0129106109021625,-0.92703533653478));
#81768=DIRECTION('',(-0.908143731209353,0.,-0.418658528475361));
#81769=DIRECTION('center_axis',(6.61422058830698E-15,-1.,1.32910602459398E-14));
#81770=DIRECTION('ref_axis',(-5.61309428634172E-32,-1.32910602459398E-14,
-1.));
#81771=DIRECTION('center_axis',(-0.142369597806779,0.987363722223232,0.0695972532347455));
#81772=DIRECTION('ref_axis',(-0.509990818251875,-0.0129109231207067,-0.860082945629637));
#81773=DIRECTION('center_axis',(0.148859773252513,0.987363722335809,-0.0543474720882764));
#81774=DIRECTION('ref_axis',(-0.443019628618916,0.017454439684933,-0.896341983393416));
#81775=DIRECTION('',(-0.418658529088568,0.,0.908143730926662));
#81776=DIRECTION('center_axis',(-0.152102425325803,-0.987363719696516,0.0444717577465602));
#81777=DIRECTION('ref_axis',(-0.314297103910649,0.00565948000699346,-0.94930780085251));
#81778=DIRECTION('center_axis',(0.157871546545998,-0.987363722028207,-0.0137642730931085));
#81779=DIRECTION('ref_axis',(-0.166704973938361,-0.0129106104254692,-0.985922292983911));
#81780=DIRECTION('',(-0.796912626680255,0.,-0.604094583188408));
#81781=DIRECTION('center_axis',(-1.08071961368061E-14,-1.,-4.32065536369259E-14));
#81782=DIRECTION('ref_axis',(1.29028034373309E-31,4.32065536369259E-14,
-1.));
#81783=DIRECTION('center_axis',(-0.154002427753715,0.987363722237364,0.0373648532117916));
#81784=DIRECTION('ref_axis',(-0.313175106282416,-0.0129109227870478,-0.949607635225088));
#81785=DIRECTION('center_axis',(0.157062615356744,0.987363722285769,-0.0210764031867505));
#81786=DIRECTION('ref_axis',(-0.239975045778217,0.0174544441542665,-0.970622130276766));
#81787=DIRECTION('',(-0.60409458190082,0.,0.796912627656303));
#81788=DIRECTION('',(-0.648418775400067,0.,-0.761283844376509));
#81789=DIRECTION('',(-0.761283846233458,0.,0.648418773219895));
#81790=DIRECTION('center_axis',(-0.156717628096624,-0.987363719703207,-0.0235046816106097));
#81791=DIRECTION('ref_axis',(0.113355675865131,0.00565948486422126,-0.993538354055962));
#81792=DIRECTION('center_axis',(0.14905980269933,-0.987363721901566,0.0537964301038988));
#81793=DIRECTION('ref_axis',(0.262680691146538,-0.0129106143644342,-0.964796439947573));
#81794=DIRECTION('',(-0.469605582630858,0.,-0.882876320195492));
#81795=DIRECTION('center_axis',(2.22229744853242E-14,-1.,-1.16669413356185E-13));
#81796=DIRECTION('ref_axis',(4.36736143566875E-31,1.16669413356185E-13,
-1.));
#81797=DIRECTION('center_axis',(-0.155457912814063,0.987363722264946,-0.0307525169474946));
#81798=DIRECTION('ref_axis',(0.114499868445593,-0.0129109209841225,-0.99333936207385));
#81799=DIRECTION('center_axis',(0.151395920500974,0.987363722202361,0.0468204585022689));
#81800=DIRECTION('ref_axis',(0.189758203180646,0.0174544474591918,-0.981675693184642));
#81801=DIRECTION('',(-0.8828763217045,0.,0.469605579793865));
#81802=DIRECTION('center_axis',(-0.148000847497835,-0.987363719703838,-0.0566448069334213));
#81803=DIRECTION('ref_axis',(0.324286860420664,0.00565947861214943,-0.945941859978903));
#81804=DIRECTION('center_axis',(0.134010224920062,-0.987363721885144,0.0845821513204255));
#81805=DIRECTION('ref_axis',(0.463942076602047,-0.0129106150950262,-0.885771452224584));
#81806=DIRECTION('',(-0.268834151573639,0.,-0.963186481917018));
#81807=DIRECTION('center_axis',(-1.75439583158224E-14,-1.,4.09366742645534E-14));
#81808=DIRECTION('ref_axis',(4.91190218677542E-32,-4.09366742645534E-14,
-1.));
#81809=DIRECTION('center_axis',(-0.145212510191229,0.987363722233914,-0.0634523986965965));
#81810=DIRECTION('ref_axis',(0.325361525070664,-0.0129109237299263,-0.945501552643956));
#81811=DIRECTION('center_axis',(0.137791354159373,0.987363722222338,0.0782714683532711));
#81812=DIRECTION('ref_axis',(0.396353016518055,0.0174544459680833,-0.917932257093619));
#81813=DIRECTION('',(-0.963186482098545,0.,0.268834150923259));
#81814=DIRECTION('center_axis',(-0.132363709699744,-0.987363719708208,-0.0871362918564599));
#81815=DIRECTION('ref_axis',(0.520054751302658,0.00565948078914774,-0.854114176164245));
#81816=DIRECTION('center_axis',(0.1126944776794,-0.987363721924488,0.111412904674414));
#81817=DIRECTION('ref_axis',(0.643510048271339,-0.0129106152021611,-0.765328774964669));
#81818=DIRECTION('',(-0.0554923374905852,0.,-0.998459113073656));
#81819=DIRECTION('center_axis',(4.32232752686131E-14,-1.,-6.03469417671824E-14));
#81820=DIRECTION('ref_axis',(9.26499412064615E-31,6.03469417671824E-14,
-1.));
#81821=DIRECTION('center_axis',(-0.128177131858304,0.987363722255328,-0.0931853145226321));
#81822=DIRECTION('ref_axis',(0.521009637840492,-0.0129109244303183,-0.85345314183479));
#81823=DIRECTION('center_axis',(0.117743818984395,0.987363722290477,0.106062589991308));
#81824=DIRECTION('ref_axis',(0.584414805440217,0.0174544421071706,-0.811267328094137));
#81825=DIRECTION('',(-0.998459113111129,0.,0.0554923368163326));
#81826=DIRECTION('center_axis',(-0.110537393066309,-0.987363719709225,-0.113553378356029));
#81827=DIRECTION('ref_axis',(0.691505459935205,0.00565948043168418,-0.722349063238157));
#81828=DIRECTION('center_axis',(0.0861092664287607,-0.987363721999118,0.133034111096177));
#81829=DIRECTION('ref_axis',(0.792988204586121,-0.0129106098602343,-0.609100175291649));
#81830=DIRECTION('',(0.160444237331189,0.,-0.987044906124951));
#81831=DIRECTION('center_axis',(0.,-1.,0.));
#81832=DIRECTION('ref_axis',(0.,0.,-1.));
#81833=DIRECTION('center_axis',(-0.105148331973208,0.987363722223282,-0.118560989877104));
#81834=DIRECTION('ref_axis',(0.692295920183945,-0.0129109267763575,-0.721498209884432));
#81835=DIRECTION('center_axis',(0.0921907102839049,0.987363722266113,0.128894347782028));
#81836=DIRECTION('ref_axis',(0.74515000645914,0.0174544447381545,-0.666668441005592));
#81837=DIRECTION('',(-0.987044905635345,0.,-0.160444240343221));
#81838=DIRECTION('center_axis',(-0.0835424717653903,-0.987363719700328,
-0.134660834806788));
#81839=DIRECTION('ref_axis',(0.83062214417687,0.00565947854203068,-0.556807708195255));
#81840=DIRECTION('center_axis',(0.0554976762857084,-0.987363721959145,0.148434795401454));
#81841=DIRECTION('ref_axis',(0.905387113396104,-0.0129106122046947,-0.424390729150356));
#81842=DIRECTION('',(0.36887861981684,0.,-0.929477575760719));
#81843=DIRECTION('center_axis',(9.03943676094093E-14,-1.,-5.12685863601807E-14));
#81844=DIRECTION('ref_axis',(1.,9.03943676094093E-14,7.83102586053432E-31));
#81845=DIRECTION('center_axis',(-0.0772029158233061,0.987363722218407,-0.138392882170259));
#81846=DIRECTION('ref_axis',(0.831211213975916,-0.012910924975103,-0.555806824154734));
#81847=DIRECTION('center_axis',(0.0623268682590145,0.987363722274991,0.145699146971756));
#81848=DIRECTION('ref_axis',(0.871042822047256,0.0174544443199294,-0.490896877697786));
#81849=DIRECTION('',(-0.929477575511641,0.,-0.368878620444452));
#81850=DIRECTION('center_axis',(-0.0526411923994217,-0.987363719715787,
-0.149471702511788));
#81851=DIRECTION('ref_axis',(0.930899857264182,0.00565948303979362,-0.365230647669728));
#81852=DIRECTION('center_axis',(0.0222910793373077,-0.987363722001288,0.15689483183885));
#81853=DIRECTION('ref_axis',(0.97545112806071,-0.012910610669765,-0.219837241834094));
#81854=DIRECTION('',(0.56006464518858,0.,-0.828448908026192));
#81855=DIRECTION('center_axis',(2.8372065137431E-14,-1.,-8.75366807693456E-15));
#81856=DIRECTION('ref_axis',(1.,2.8372065137431E-14,-1.7135964172008E-31));
#81857=DIRECTION('center_axis',(-0.045647571293492,0.987363722194643,-0.151753679787165));
#81858=DIRECTION('ref_axis',(0.931259995085496,-0.0129109298287278,-0.36412652944316));
#81859=DIRECTION('center_axis',(0.0295486889639333,0.987363722256726,0.15569121668179));
#81860=DIRECTION('ref_axis',(0.956206642880283,0.0174544463351347,-0.292171522251491));
#81861=DIRECTION('',(-0.82844890631414,0.,-0.560064647721052));
#81862=DIRECTION('center_axis',(-0.0192784774288681,-0.987363719716235,
-0.157293436913768));
#81863=DIRECTION('ref_axis',(0.987649729086615,0.00565947836576162,-0.156575805729248));
#81864=DIRECTION('center_axis',(-0.0119578245152855,-0.98736372200228,0.158018641010057));
#81865=DIRECTION('ref_axis',(0.999904131400371,-0.0129106106213219,-0.00500441223858307));
#81866=DIRECTION('',(0.725062671623472,0.,-0.688682889447845));
#81867=DIRECTION('center_axis',(-1.47952609495248E-14,-1.,1.2249284241146E-15));
#81868=DIRECTION('ref_axis',(1.,-1.47952609495248E-14,-9.44752033172559E-33));
#81869=DIRECTION('center_axis',(-0.0119578035856478,0.987363722219315,-0.158018641237758));
#81870=DIRECTION('ref_axis',(0.9877640942684,-0.0129109272861874,-0.155420082456347));
#81871=DIRECTION('center_axis',(-0.0046111468982762,0.987363722325162,0.158403336961328));
#81872=DIRECTION('ref_axis',(0.996659303735564,0.0174544409252697,-0.0797845521973175));
#81873=DIRECTION('',(-0.688682888958241,0.,-0.725062672088511));
#81874=DIRECTION('center_axis',(0.0149856872273682,-0.987363719693288,-0.157760306198226));
#81875=DIRECTION('ref_axis',(0.998218197100463,0.00565948357705208,0.0594003469951372));
#81876=DIRECTION('center_axis',(-0.0456475956634642,-0.987363721979248,
0.151753673858105));
#81877=DIRECTION('ref_axis',(0.977602729074026,-0.0129106122427607,0.210062419767398));
#81878=DIRECTION('',(0.856157573483628,0.,-0.516714824024457));
#81879=DIRECTION('center_axis',(1.32414114458036E-13,-1.,1.78582813416022E-14));
#81880=DIRECTION('ref_axis',(1.,1.32414114458036E-13,5.55548786246673E-32));
#81881=DIRECTION('center_axis',(0.0222911022848482,0.987363722208355,-0.156894827275438));
#81882=DIRECTION('ref_axis',(0.998081442094801,-0.012910929320345,0.0605536361422535));
#81883=DIRECTION('center_axis',(-0.0385553754235707,0.987363722312957,0.15370869489476));
#81884=DIRECTION('ref_axis',(0.990509283694734,0.0174544407656422,0.136333053263337));
#81885=DIRECTION('',(-0.516714824718151,0.,-0.856157573064965));
#81886=DIRECTION('center_axis',(0.0485491287704313,-0.987363719723607,-0.150850479181189));
#81887=DIRECTION('ref_axis',(0.962111091449422,0.00565947937755026,0.272599005873419));
#81888=DIRECTION('center_axis',(-0.0772029342179146,-0.987363721959937,
0.138392873752822));
#81889=DIRECTION('ref_axis',(0.90958970992946,-0.0129106121656763,0.415306965609714));
#81890=DIRECTION('',(0.947219498157893,0.,-0.32058574876234));
#81891=DIRECTION('center_axis',(5.57685970606299E-14,-1.,2.04026155986365E-14));
#81892=DIRECTION('ref_axis',(1.,5.57685970606299E-14,-5.33515460699669E-31));
#81893=DIRECTION('center_axis',(0.0554976970957135,0.9873637222177,-0.148434785901016));
#81894=DIRECTION('ref_axis',(0.961729611179224,-0.0129109277223155,0.273695931512342));
#81895=DIRECTION('center_axis',(-0.0706968022411019,0.987363722240037,0.14182680338068));
#81896=DIRECTION('ref_axis',(0.938044149622633,0.01745444496317,0.346075881433219));
#81897=DIRECTION('',(-0.320585748995687,0.,-0.947219498078916));
#81898=DIRECTION('center_axis',(0.0798424772113265,-0.987363719686393,-0.136887047889156));
#81899=DIRECTION('ref_axis',(0.881016739713925,0.00565948623402568,0.473051238830861));
#81900=DIRECTION('center_axis',(-0.105148351657736,-0.987363721915906,0.118560974979252));
#81901=DIRECTION('ref_axis',(0.799045286445946,-0.0129106147625576,0.60113222026021));
#81902=DIRECTION('',(0.993990492096634,0.,-0.109466440617618));
#81903=DIRECTION('center_axis',(1.00157598129628E-13,-1.,6.38284273780134E-14));
#81904=DIRECTION('ref_axis',(1.,1.00157598129628E-13,-3.97615990582066E-31));
#81905=DIRECTION('center_axis',(0.0861092789791971,0.987363722241669,-0.133034101172438));
#81906=DIRECTION('ref_axis',(0.880408371952486,-0.0129109227373763,0.474040511633807));
#81907=DIRECTION('center_axis',(-0.0995325171218021,0.98736372227733,0.123313251380591));
#81908=DIRECTION('ref_axis',(0.841717114861623,0.0174544407701366,0.539636582383391));
#81909=DIRECTION('',(-0.109466440259225,0.,-0.993990492136104));
#81910=DIRECTION('center_axis',(0.107402471327209,-0.987363719708752,-0.116522934033203));
#81911=DIRECTION('ref_axis',(0.758727025472456,0.00565948363991874,0.651384119443089));
#81912=DIRECTION('center_axis',(-0.128177146079023,-0.987363721938031,0.0931852983239097));
#81913=DIRECTION('ref_axis',(0.651138393509337,-0.0129106139935096,0.75884920013425));
#81914=DIRECTION('',(0.994283595393051,0.,0.106771400347975));
#81915=DIRECTION('center_axis',(5.25592149427991E-14,-1.,5.24169231671855E-14));
#81916=DIRECTION('ref_axis',(1.,5.25592149427991E-14,1.52343460007419E-31));
#81917=DIRECTION('center_axis',(0.112694496580979,0.987363722214069,-0.111412882989084));
#81918=DIRECTION('ref_axis',(0.757920215591527,-0.012910930245521,0.652219483516008));
#81919=DIRECTION('center_axis',(-0.12371420854767,0.987363722261302,0.0990337041906916));
#81920=DIRECTION('ref_axis',(0.706032321934242,0.0174544443873073,0.707964478455857));
#81921=DIRECTION('',(0.106771401019337,0.,-0.994283595320957));
#81922=DIRECTION('center_axis',(0.129940445222184,-0.987363719718547,-0.0907103394273005));
#81923=DIRECTION('ref_axis',(0.600960079687005,0.00565947968915366,0.799259002396743));
#81924=DIRECTION('center_axis',(-0.145212520372231,-0.987363721945181,0.0634523798899918));
#81925=DIRECTION('ref_axis',(0.472784992661812,-0.0129106143584673,0.8810832348596));
#81926=DIRECTION('',(0.948085102432835,0.,0.318016726831972));
#81927=DIRECTION('center_axis',(0.,-1.,0.));
#81928=DIRECTION('ref_axis',(0.,0.,-1.));
#81929=DIRECTION('center_axis',(0.134010234072352,0.987363722256383,-0.0845821324860878));
#81930=DIRECTION('ref_axis',(0.599992554262842,-0.0129109228150569,0.799901395736508));
#81931=DIRECTION('center_axis',(-0.142111155988232,0.987363722341574,0.0701234564712802));
#81932=DIRECTION('ref_axis',(0.537334244319765,0.0174544408201278,0.843188740660692));
#81933=DIRECTION('',(0.318016724021307,0.,-0.948085103375618));
#81934=DIRECTION('center_axis',(0.14640255189611,-0.987363719719664,-0.0606562262233358));
#81935=DIRECTION('ref_axis',(0.415092905252734,0.00565948058615717,0.909761424928722));
#81936=DIRECTION('center_axis',(-0.155457917085905,-0.987363722019786,0.0307525032240912));
#81937=DIRECTION('ref_axis',(0.272324693801645,-0.0129106103601986,0.962118795828232));
#81938=DIRECTION('',(0.857555204217401,0.,0.514391943676854));
#81939=DIRECTION('center_axis',(2.56921567550482E-14,-1.,6.96413525208238E-14));
#81940=DIRECTION('ref_axis',(5.42541743807951E-31,-6.96413525208238E-14,
-1.));
#81941=DIRECTION('center_axis',(0.149059810145022,0.987363722194985,-0.0537964040879616));
#81942=DIRECTION('ref_axis',(0.414009904232867,-0.0129109291564851,0.910180810117094));
#81943=DIRECTION('center_axis',(-0.153863147665941,0.987363722279557,0.03793430790968));
#81944=DIRECTION('ref_axis',(0.343511013224812,0.0174544443899348,0.938986435559269));
#81945=DIRECTION('',(0.514391942141765,0.,-0.857555205138202));
#81946=DIRECTION('center_axis',(0.156019037498486,-0.987363719708581,-0.027765895290473));
#81947=DIRECTION('ref_axis',(0.209816451605885,0.00565948196952231,0.97772441255159));
#81948=DIRECTION('center_axis',(-0.158434276356287,-0.987363722051535,-0.0033853289351005));
#81949=DIRECTION('ref_axis',(0.0591307919551479,-0.0129106090674337,0.998166752409769));
#81950=DIRECTION('',(0.72692697915402,0.,0.686714763914401));
#81951=DIRECTION('center_axis',(0.,-1.,0.));
#81952=DIRECTION('ref_axis',(0.,0.,-1.));
#81953=DIRECTION('center_axis',(0.157139511089208,0.987363722227819,-0.0204952209812866));
#81954=DIRECTION('ref_axis',(0.208668612810206,-0.0129109291001378,0.977901180047164));
#81955=DIRECTION('center_axis',(-0.158420667613503,0.987363722279252,0.00397139770759942));
#81956=DIRECTION('ref_axis',(0.133625589541009,0.0174544430089088,0.990878168211949));
#81957=DIRECTION('center_axis',(-2.36962999805567E-15,-1.,2.95970545814484E-14));
#81958=DIRECTION('ref_axis',(2.10725079438871E-32,-2.95970545814484E-14,
-1.));
#81959=DIRECTION('center_axis',(0.157871543355326,0.987363722242725,0.0137642943007882));
#81960=DIRECTION('ref_axis',(-0.00642978887167585,-0.0129109278822441,0.999895977467799));
#81961=DIRECTION('center_axis',(-0.155570614016615,0.98736372228924,-0.0301772093081879));
#81962=DIRECTION('ref_axis',(-0.082508018693808,0.0174544402047945,0.996437539120421));
#81963=DIRECTION('center_axis',(0.158340246542571,-0.987363720697896,0.00642256758979644));
#81964=DIRECTION('ref_axis',(-0.00527076112834019,0.0056593145872632,0.999970095170616));
#81965=DIRECTION('',(0.686714765840337,0.,-0.726926977334623));
#81966=DIRECTION('center_axis',(0.161203604208133,-0.986495109513923,-0.0289964979854629));
#81967=DIRECTION('ref_axis',(0.0334320569963806,-0.0239054702440692,0.999155056063573));
#81968=DIRECTION('center_axis',(0.151201360906316,-0.986495109379104,-0.0629725942866305));
#81969=DIRECTION('ref_axis',(0.247439236341897,-0.0239054792976647,0.968608461855505));
#81970=DIRECTION('center_axis',(0.13412911587782,-0.986495109511419,-0.0940041445037833));
#81971=DIRECTION('ref_axis',(0.449876430650253,-0.0239054694228749,0.892770813634194));
#81972=DIRECTION('center_axis',(0.110785139185501,-0.986495109537552,-0.120640174876129));
#81973=DIRECTION('ref_axis',(0.631277905258259,-0.0239054693349842,0.7751881931948));
#81974=DIRECTION('center_axis',(0.0822609672332386,-0.986495109427629,-0.141635208706104));
#81975=DIRECTION('ref_axis',(0.783161525338651,-0.0239054762326219,0.621358635117699));
#81976=DIRECTION('center_axis',(0.0498903701130608,-0.986495109459145,-0.156007531815523));
#81977=DIRECTION('ref_axis',(0.898425384303044,-0.0239054739893283,0.43847503595219));
#81978=DIRECTION('center_axis',(0.0151869524931169,-0.986495109422531,-0.163085117528855));
#81979=DIRECTION('ref_axis',(0.971679868827215,-0.0239054752549652,0.235088835908386));
#81980=DIRECTION('center_axis',(-0.0202265870975381,-0.986495109463458,
-0.162537024025499));
#81981=DIRECTION('ref_axis',(0.999499684133882,-0.0239054723659645,0.0207101377887582));
#81982=DIRECTION('center_axis',(-0.054694359581535,-0.986495109445661,-0.154388879359104));
#81983=DIRECTION('ref_axis',(0.980584004496004,-0.023905475956201,-0.194636939828719));
#81984=DIRECTION('center_axis',(-0.0866046785300437,-0.98649510947863,-0.1390216840333));
#81985=DIRECTION('ref_axis',(0.915817306663047,-0.0239054728221509,-0.400883011844594));
#81986=DIRECTION('center_axis',(-0.114465467498151,-0.986495109349503,-0.117153984054926));
#81987=DIRECTION('ref_axis',(0.808228009920007,-0.0239054802132403,-0.588384238399126));
#81988=DIRECTION('center_axis',(-0.136973968945314,-0.986495109439412,-0.0898083007493744));
#81989=DIRECTION('ref_axis',(0.662846868214859,-0.0239054750836998,-0.748373274214663));
#81990=DIRECTION('center_axis',(-0.153077721692645,-0.986495109512432,-0.0582632820002848));
#81991=DIRECTION('ref_axis',(0.486471746056184,-0.0239054710243431,-0.87336920528729));
#81992=DIRECTION('center_axis',(-0.162023734697267,-0.986495109407243,-0.0239939265302789));
#81993=DIRECTION('ref_axis',(0.287349742887533,-0.023905478144174,-0.957527364296795));
#81994=DIRECTION('center_axis',(-0.16339369481978,-0.986495109410467,0.01139735067332));
#81995=DIRECTION('ref_axis',(0.0747915872978661,-0.0239054772206403,-0.996912607317371));
#81996=DIRECTION('center_axis',(-0.157123548484063,-0.986495109484464,0.0462556966763247));
#81997=DIRECTION('ref_axis',(-0.141263742161791,-0.0239054720233515,-0.989683324886192));
#81998=DIRECTION('center_axis',(-0.143506479156584,-0.986495109461388,0.0789511839610127));
#81999=DIRECTION('ref_axis',(-0.350713731644889,-0.0239054740284668,-0.936177550866924));
#82000=DIRECTION('center_axis',(-0.123179205476089,-0.98649510942288,0.107955001843448));
#82001=DIRECTION('ref_axis',(-0.54376474062529,-0.0239054759324562,-0.838897154049979));
#82002=DIRECTION('center_axis',(-0.0970922114149732,-0.986495109447443,
0.131910960571241));
#82003=DIRECTION('ref_axis',(-0.711389914873902,-0.0239054735609438,-0.702390857962666));
#82004=DIRECTION('center_axis',(-0.0664652930898098,-0.986495109464134,
0.149698910543234));
#82005=DIRECTION('ref_axis',(-0.845751284614566,-0.0239054729384704,-0.533041548977562));
#82006=DIRECTION('center_axis',(-0.0327305254113617,-0.986495109365823,
0.160487108216234));
#82007=DIRECTION('ref_axis',(-0.940566265756416,-0.0239054786927108,-0.338767808106827));
#82008=DIRECTION('center_axis',(0.00253467972596253,-0.986495109391286,
0.163771104123291));
#82009=DIRECTION('ref_axis',(-0.991401414099233,-0.0239054778873439,-0.128653660068495));
#82010=DIRECTION('center_axis',(0.0376813603758679,-0.986495109487736,0.159397346392603));
#82011=DIRECTION('ref_axis',(-0.995879734001976,-0.0239054713375422,0.0874761901564217));
#82012=DIRECTION('center_axis',(0.0710661117949504,-0.986495109438756,0.14757034528578));
#82013=DIRECTION('ref_axis',(-0.953791823912064,-0.0239054744511443,0.299515750720665));
#82014=DIRECTION('center_axis',(0.10112789063694,-0.986495109381306,0.12884311740286));
#82015=DIRECTION('ref_axis',(-0.867105668209388,-0.0239054779846499,0.497550287188617));
#82016=DIRECTION('center_axis',(0.126461037271181,-0.986495109416645,0.104091330807796));
#82017=DIRECTION('ref_axis',(-0.739874616419024,-0.023905476675434,0.672319923967542));
#82018=DIRECTION('center_axis',(0.14588100612832,-0.986495109464053,0.0744723509397584));
#82019=DIRECTION('ref_axis',(-0.578047850450362,-0.0239054740051813,0.815652628820813));
#82020=DIRECTION('center_axis',(0.158479742656197,-0.986495109491895,0.0413711266005706));
#82021=DIRECTION('ref_axis',(-0.389192206378908,-0.023905471580982,0.920846325356413));
#82022=DIRECTION('center_axis',(0.163668143341035,-0.986495109532137,0.00633543404000669));
#82023=DIRECTION('ref_axis',(-0.182138368827764,-0.0239054700782205,0.982982269983086));
#82024=DIRECTION('center_axis',(-0.15968414742932,0.986495108980163,-0.0364468519626609));
#82025=DIRECTION('ref_axis',(-0.0834110839114267,0.0233052156986855,0.996242670237507));
#82026=DIRECTION('center_axis',(0.157820544757278,0.986495109280205,0.0438186606225335));
#82027=DIRECTION('ref_axis',(-0.189267235091296,-0.0133324946527578,0.981835097308723));
#82028=DIRECTION('center_axis',(-0.148115819742677,0.98649510925013,-0.0699221235913883));
#82029=DIRECTION('ref_axis',(-0.295623702609842,0.02330522464751,0.955020153169229));
#82030=DIRECTION('center_axis',(0.144711069366068,0.986495109279994,0.0767209604318213));
#82031=DIRECTION('ref_axis',(-0.395907796897688,-0.0133324986804576,0.918193476798085));
#82032=DIRECTION('center_axis',(-0.129621765649933,0.986495109247231,-0.100127904707367));
#82033=DIRECTION('ref_axis',(-0.49401328476561,0.0233052232947627,0.869141956783973));
#82034=DIRECTION('center_axis',(0.124835066434606,0.986495109301351,0.106035868991504));
#82035=DIRECTION('ref_axis',(-0.584036148783592,-0.0133324983230549,0.811618149995733));
#82036=DIRECTION('center_axis',(-0.105066742164848,0.986495109264697,-0.125651816889763));
#82037=DIRECTION('ref_axis',(-0.669303358386494,0.0233052215977236,0.742623647010275));
#82038=DIRECTION('center_axis',(0.0991219123680177,0.986495109264719,0.130392660396576));
#82039=DIRECTION('ref_axis',(-0.744855620159144,-0.0133325009867863,0.667092459509755));
#82040=DIRECTION('center_axis',(-0.0755989173091877,0.986495109354151,-0.145300388581793));
#82041=DIRECTION('ref_axis',(-0.813297549159958,0.0233052174831723,0.581381082740458));
#82042=DIRECTION('center_axis',(0.0687739335327272,0.986495109263157,0.148652431753765));
#82043=DIRECTION('ref_axis',(-0.870846468817089,-0.0133324967428771,0.491374269044899));
#82044=DIRECTION('center_axis',(-0.0425961641668376,0.986495109300106,-0.15815488018156));
#82045=DIRECTION('ref_axis',(-0.919262851645652,0.0233052217291667,0.392953783827639));
#82046=DIRECTION('center_axis',(0.0352101565309262,0.986495109262151,0.159961383711587));
#82047=DIRECTION('ref_axis',(-0.956117505325965,-0.0133324987105083,0.292679962565576));
#82048=DIRECTION('center_axis',(-0.00760166424791377,0.986495109286655,
-0.163614223263664));
#82049=DIRECTION('ref_axis',(-0.982244445249597,0.0233052224913856,0.186152400953997));
#82050=DIRECTION('center_axis',(-4.18661250280414E-9,0.986495109267288,
0.163790718270974));
#82051=DIRECTION('ref_axis',(-0.996681549668706,-0.0133324966986084,0.0803002682546456));
#82052=DIRECTION('center_axis',(0.0277482857855902,0.986495109197101,-0.161423146314772));
#82053=DIRECTION('ref_axis',(-0.999297379399636,0.0233052282832678,-0.0293532597795325));
#82054=DIRECTION('center_axis',(-0.0352101726580663,0.986495109258677,0.159961380183158));
#82055=DIRECTION('ref_axis',(-0.990641872508763,-0.0133325022384921,-0.135834181325586));
#82056=DIRECTION('center_axis',(0.0618007488839688,0.986495109226498,-0.151684102362711));
#82057=DIRECTION('ref_axis',(-0.969624278718342,0.0233052258209236,-0.243486395039581));
#82058=DIRECTION('center_axis',(-0.0687739426532382,0.986495109277808,0.148652427436938));
#82059=DIRECTION('ref_axis',(-0.938280882830305,-0.0133324980118305,-0.345617171755035));
#82060=DIRECTION('center_axis',(0.0929634778324112,0.986495109264974,-0.134852479345355));
#82061=DIRECTION('ref_axis',(-0.89461262460464,0.0233052233982638,-0.446234376152661));
#82062=DIRECTION('center_axis',(-0.0991219242755312,0.986495109247182,0.130392651477402));
#82063=DIRECTION('ref_axis',(-0.84204692162246,-0.0133324984111526,-0.539239488791627));
#82064=DIRECTION('center_axis',(0.119779342921852,0.98649510919913,-0.111715301259079));
#82065=DIRECTION('ref_axis',(-0.777769877304456,0.0233052267413185,-0.62811693526313));
#82066=DIRECTION('center_axis',(-0.124835075987954,0.986495109277209,0.106035857969037));
#82067=DIRECTION('ref_axis',(-0.706439782054066,-0.0133325009604519,-0.70764756676579));
#82068=DIRECTION('center_axis',(0.140994452051711,0.986495109320719,-0.0833544466536714));
#82069=DIRECTION('ref_axis',(-0.624559478487569,0.023305220786728,-0.780629441230228));
#82070=DIRECTION('center_axis',(-0.144711073722138,0.986495109289194,0.0767209520971159));
#82071=DIRECTION('ref_axis',(-0.537800303819866,-0.0133324954651747,-0.842966830768525));
#82072=DIRECTION('center_axis',(0.155616822593003,0.986495109297831,-0.0510960258485798));
#82073=DIRECTION('ref_axis',(-0.442145367329196,0.0233052210821708,-0.896640586199198));
#82074=DIRECTION('center_axis',(-0.157820545741181,0.986495109287339,0.043818656918217));
#82075=DIRECTION('ref_axis',(-0.344013881227021,-0.0133324941993633,-0.938869902660398));
#82076=DIRECTION('center_axis',(0.162962722649269,0.986495109321916,-0.0164484136219705));
#82077=DIRECTION('ref_axis',(-0.239057033921903,0.0233052199010562,-0.97072581157494));
#82078=DIRECTION('center_axis',(-0.163550504854886,0.986495109300725,0.00886745101273296));
#82079=DIRECTION('ref_axis',(-0.134141752519128,-0.0133324921844451,-0.990872461461741));
#82080=DIRECTION('center_axis',(0.162688667483949,0.986495109300975,0.0189683103505219));
#82081=DIRECTION('ref_axis',(-0.0247906600931756,0.0233052211894522,-0.999420977285076));
#82082=DIRECTION('center_axis',(-0.161633024216997,0.986495109294657,-0.02649839278503));
#82083=DIRECTION('ref_axis',(0.0820026983652642,-0.0133324956280381,-0.996542925327928));
#82084=DIRECTION('center_axis',(0.154807469423538,0.986495109257914,0.053498101096184));
#82085=DIRECTION('ref_axis',(0.190634902087668,0.0233052257812496,-0.981384328669105));
#82086=DIRECTION('center_axis',(-0.152157762777711,0.986495109280064,-0.0606251976738774));
#82087=DIRECTION('ref_axis',(0.294312792599874,-0.0133324957669015,-0.955616149229746));
#82088=DIRECTION('center_axis',(0.139687648469914,0.986495109284146,0.0855263715084811));
#82089=DIRECTION('ref_axis',(0.397146585108484,0.0233052216819088,-0.917459239737127));
#82090=DIRECTION('center_axis',(-0.135567769450184,0.986495109256001,-0.091917241583357));
#82091=DIRECTION('ref_axis',(0.49286114707,-0.0133325031596082,-0.870005824157714));
#82092=DIRECTION('center_axis',(0.118036188482416,0.986495109330827,0.113555525954939));
#82093=DIRECTION('ref_axis',(0.585088132697792,0.0233052199382875,-0.810634778244703));
#82094=DIRECTION('center_axis',(-0.112638782506801,0.986495109231987,-0.118911328883146));
#82095=DIRECTION('ref_axis',(0.668363861819259,-0.0133325005712271,-0.743714994230024));
#82096=DIRECTION('center_axis',(0.0908654815662987,0.98649510920376,0.136274956528284));
#82097=DIRECTION('ref_axis',(0.745671613248655,0.0233052263820281,-0.665905933010384));
#82098=DIRECTION('center_axis',(-0.0844429344226583,0.986495109307055,-0.140345253355262));
#82099=DIRECTION('ref_axis',(0.81261462650057,-0.0133324944657728,-0.582648876587486));
#82100=DIRECTION('center_axis',(0.0594460085246961,0.986495109207123,0.152622316785285));
#82101=DIRECTION('ref_axis',(0.871388316849539,0.0233052276412447,-0.490040067364615));
#82102=DIRECTION('center_axis',(-0.052298619937897,0.986495109270013,-0.155216795930522));
#82103=DIRECTION('ref_axis',(0.918868433255501,-0.0133324996967874,-0.39433874628093));
#82104=DIRECTION('center_axis',(0.025246910107844,0.986495109231267,0.16183322586168));
#82105=DIRECTION('ref_axis',(0.956359871910885,0.0233052243661917,-0.291260470911925));
#82106=DIRECTION('center_axis',(-0.0177088862318153,0.986495109292059,-0.162830570505903));
#82107=DIRECTION('ref_axis',(0.982156973931475,-0.0133324976255219,-0.18758977334821));
#82108=DIRECTION('center_axis',(-0.0101327025401918,0.986495109345222,0.163476994030323));
#82109=DIRECTION('ref_axis',(0.99661310121068,0.0233052186751277,-0.0788618619976393));
#82110=DIRECTION('center_axis',(0.0177088989246918,0.986495109263363,-0.16283056929932));
#82111=DIRECTION('ref_axis',(0.999520945806007,-0.0133324994616411,0.0279306883762481));
#82112=DIRECTION('center_axis',(-0.045038534560328,0.986495109243709,0.157476759691396));
#82113=DIRECTION('ref_axis',(0.99026580966141,0.023305226422398,0.137224242162354));
#82114=DIRECTION('center_axis',(0.0522986285573802,0.986495109283445,-0.155216792940907));
#82115=DIRECTION('ref_axis',(0.970148429509415,-0.0133324940184864,0.242145141028396));
#82116=DIRECTION('center_axis',(-0.0778384024322311,0.98649510932681,0.144113088861088));
#82117=DIRECTION('ref_axis',(0.937614789438134,0.0233052212853708,0.346893893413713));
#82118=DIRECTION('center_axis',(0.0844429366349048,0.986495109286383,-0.140345252169504));
#82119=DIRECTION('ref_axis',(0.895412851334178,-0.0133324926260604,0.445037156095953));
#82120=DIRECTION('center_axis',(-0.106998637769303,0.986495109310485,0.124010849614086));
#82121=DIRECTION('ref_axis',(0.841121944973973,0.0233052212986492,0.540343169054095));
#82122=DIRECTION('center_axis',(0.112638793408809,0.986495109254256,-0.118911318371472));
#82123=DIRECTION('ref_axis',(0.778808761715822,-0.0133324991579478,0.627119731104731));
#82124=DIRECTION('center_axis',(-0.131155737577945,0.98649510924389,0.0981099991757735));
#82125=DIRECTION('ref_axis',(0.705299172575773,0.0233052234911864,0.70852660057471));
#82126=DIRECTION('center_axis',(0.135567778586344,0.986495109306674,-0.0919172275646806));
#82127=DIRECTION('ref_axis',(0.625788442491835,-0.0133324983270567,0.779878881450192));
#82128=DIRECTION('center_axis',(-0.149180137288326,0.986495109329306,0.0676216378683425));
#82129=DIRECTION('ref_axis',(0.536497393132868,0.0233052200227967,0.843580117049546));
#82130=DIRECTION('center_axis',(0.152157765743977,0.986495109271346,-0.0606251903709633));
#82131=DIRECTION('ref_axis',(0.443506950190524,-0.0133324967788789,0.896171763481946));
#82132=DIRECTION('center_axis',(-0.1602290428339,0.986495109287375,0.0339713582981541));
#82133=DIRECTION('ref_axis',(0.342609592811973,0.0233052236259752,0.939188763489511));
#82134=DIRECTION('center_axis',(0.161633025665583,0.98649510926358,-0.0264983851059975));
#82135=DIRECTION('ref_axis',(0.240487563639497,-0.0133324965701397,0.970560650485041));
#82136=DIRECTION('center_axis',(-0.163785814321667,0.986495109358156,-0.00126737501506783));
#82137=DIRECTION('ref_axis',(0.13270175267014,0.0233052181179322,0.990881986740474));
#82138=DIRECTION('center_axis',(0.163550504525506,0.986495109354549,0.00886745109988042));
#82139=DIRECTION('ref_axis',(0.0262232508807231,-0.0133324930323418,0.999567199213134));
#82140=DIRECTION('center_axis',(-0.154963399779559,0.987363722743152,0.0331545432715526));
#82141=DIRECTION('ref_axis',(0.138670756052496,-0.0114882900478161,0.990271902361976));
#82142=DIRECTION('',(-0.72766464391209,0.,-0.685933062332099));
#82143=DIRECTION('center_axis',(1.22396249182026E-14,-1.,8.82303726500718E-14));
#82144=DIRECTION('ref_axis',(-1.12949232739023E-31,-8.82303726500718E-14,
-1.));
#82145=DIRECTION('center_axis',(-0.153863150617874,-0.987363722405381,0.0379342926615524));
#82146=DIRECTION('ref_axis',(0.0666568490087253,0.0279320151284881,0.997384914168592));
#82147=DIRECTION('center_axis',(0.148209443903646,-0.987363722200592,-0.0560967095288448));
#82148=DIRECTION('ref_axis',(0.142449801462467,-0.0348178353517325,0.989189452230827));
#82149=DIRECTION('',(-0.513469942625881,0.,0.858107579514232));
#82150=DIRECTION('center_axis',(-0.144213195008524,0.987363722762328,0.065691958094963));
#82151=DIRECTION('ref_axis',(0.34830789812865,-0.0114882892894636,0.937309781934662));
#82152=DIRECTION('',(-0.858107580390448,0.,-0.513469941161556));
#82153=DIRECTION('center_axis',(5.15339854808296E-15,-1.,1.39227396462689E-14));
#82154=DIRECTION('ref_axis',(-6.63359757292675E-32,-1.39227396462689E-14,
-1.));
#82155=DIRECTION('center_axis',(-0.142111163603627,-0.98736372241876,0.070123439951227));
#82156=DIRECTION('ref_axis',(0.279506722704434,0.0279320160327722,0.959737357011475));
#82157=DIRECTION('center_axis',(0.132685252824785,-0.987363722069216,-0.0866458540522629));
#82158=DIRECTION('ref_axis',(0.351765899733318,-0.0348178403340402,0.935440254521518));
#82159=DIRECTION('',(-0.316997534753803,0.,0.948426361379739));
#82160=DIRECTION('center_axis',(-0.126719744698157,0.98736372284324,0.0951576855370697));
#82161=DIRECTION('ref_axis',(0.541658548276654,-0.0114882834278289,0.840520098761897));
#82162=DIRECTION('',(-0.94842636181411,0.,-0.316997533454207));
#82163=DIRECTION('center_axis',(4.8155354648782E-14,-1.,7.49364324094566E-14));
#82164=DIRECTION('ref_axis',(-1.74406787356792E-31,-7.49364324094566E-14,
-1.));
#82165=DIRECTION('center_axis',(-0.123714216968241,-0.987363722393222,0.0990336923563706));
#82166=DIRECTION('ref_axis',(0.479287174540691,0.0279320157356044,0.877213546873136));
#82167=DIRECTION('center_axis',(0.110956844829601,-0.987363721895533,-0.11314353392952));
#82168=DIRECTION('ref_axis',(0.5446338136483,-0.0348178455852978,0.837950909456937));
#82169=DIRECTION('',(-0.105702677699157,0.,0.994397779526497));
#82170=DIRECTION('center_axis',(-0.103301012505807,0.987363722695783,0.120173956910803));
#82171=DIRECTION('ref_axis',(0.709681848697047,-0.0114882913682037,0.704428628600074));
#82172=DIRECTION('',(-0.994397779862904,0.,-0.105702674534415));
#82173=DIRECTION('center_axis',(6.31386270573628E-14,-1.,6.28324824480148E-14));
#82174=DIRECTION('ref_axis',(1.,6.31386270573628E-14,3.33481401827685E-31));
#82175=DIRECTION('center_axis',(-0.0995325333667008,-0.98736372246363,0.123313236776796));
#82176=DIRECTION('ref_axis',(0.656656687002873,0.0279320125704962,0.75367220864788));
#82177=DIRECTION('center_axis',(0.0840402285537813,-0.987363722249468,-0.134350734907943));
#82178=DIRECTION('ref_axis',(0.712035251163724,-0.034817834568617,0.701279915223704));
#82179=DIRECTION('',(0.110534720558305,0.,0.993872263196381));
#82180=DIRECTION('center_axis',(-0.0750520425157905,0.987363722713108,0.139571021291385));
#82181=DIRECTION('ref_axis',(0.844521214338555,-0.0114882926440067,0.535398858482401));
#82182=DIRECTION('',(-0.993872263160416,0.,0.110534720881691));
#82183=DIRECTION('center_axis',(8.76978752697669E-14,-1.,5.57556479960677E-14));
#82184=DIRECTION('ref_axis',(1.,8.76978752697669E-14,1.18806915830677E-30));
#82185=DIRECTION('center_axis',(-0.0706968179443026,-0.987363722496075,
0.141826793770582));
#82186=DIRECTION('ref_axis',(0.803321666208873,0.0279320113621636,0.594889992637852));
#82187=DIRECTION('center_axis',(0.0531939794800717,-0.987363722280923,-0.149275853608792));
#82188=DIRECTION('ref_axis',(0.846142716066501,-0.0348178326291315,0.531817847179478));
#82189=DIRECTION('',(0.321603636911446,0.,0.946874384871262));
#82190=DIRECTION('center_axis',(-0.0432937294344491,0.987363722805861,0.15244189672989));
#82191=DIRECTION('ref_axis',(0.939871705575629,-0.0114882864976855,0.34133443472891));
#82192=DIRECTION('',(-0.946874383847733,0.,0.321603639924949));
#82193=DIRECTION('center_axis',(8.36857404655723E-14,-1.,3.05139952084908E-14));
#82194=DIRECTION('ref_axis',(1.,8.36857404655723E-14,-4.34665991130318E-31));
#82195=DIRECTION('center_axis',(-0.0385553939103757,-0.987363722414026,
0.153708689608408));
#82196=DIRECTION('ref_axis',(0.912424215593072,0.0279320150912321,0.408291382877855));
#82197=DIRECTION('center_axis',(0.0198604347482932,-0.987363722186018,-0.15722100127712));
#82198=DIRECTION('ref_axis',(0.940685486343554,-0.0348178358371948,0.337488568828939));
#82199=DIRECTION('',(0.517634729095432,0.,0.855601710630769));
#82200=DIRECTION('center_axis',(-0.00951104415543458,0.987363722795096,
0.158184762057801));
#82201=DIRECTION('ref_axis',(0.991274841117851,-0.0114882867674769,0.131309590791865));
#82202=DIRECTION('',(-0.855601711026882,0.,0.517634728440695));
#82203=DIRECTION('center_axis',(7.35740178671048E-14,-1.,9.84219542303022E-15));
#82204=DIRECTION('ref_axis',(1.,7.35740178671048E-14,-2.13993793218284E-31));
#82205=DIRECTION('center_axis',(-0.00461116285625835,-0.987363722349456,
0.158403336345352));
#82206=DIRECTION('ref_axis',(0.978862822739999,0.0279320178453563,0.202601521802199));
#82207=DIRECTION('center_axis',(-0.0144017553816479,-0.98736372226706,-0.157814667863491));
#82208=DIRECTION('ref_axis',(0.991242848386679,-0.0348178325842814,0.127378703307875));
#82209=DIRECTION('',(0.689461790264558,0.,0.724322055280102));
#82210=DIRECTION('center_axis',(0.0247163709221402,0.987363722722755,0.156531083365262));
#82211=DIRECTION('ref_axis',(0.99632706671758,-0.0114882911099796,-0.0848551429986193));
#82212=DIRECTION('',(-0.724322051650169,0.,0.689461794078026));
#82213=DIRECTION('center_axis',(7.39696793198838E-14,-1.,-6.20414865005964E-15));
#82214=DIRECTION('ref_axis',(1.,7.39696793198838E-14,7.83902087019578E-32));
#82215=DIRECTION('center_axis',(0.0295486732720129,-0.987363722463355,0.155691218349561));
#82216=DIRECTION('ref_axis',(0.999530892382157,0.0279320124645528,-0.0125617615567688));
#82217=DIRECTION('center_axis',(-0.04799054642031,-0.987363722052468,-0.151029095968217));
#82218=DIRECTION('ref_axis',(0.995450796857855,-0.0348178397390494,-0.08868725427573));
#82219=DIRECTION('',(0.829050388663707,0.,0.559173902338581));
#82220=DIRECTION('center_axis',(0.0577880672762993,0.987363722787464,0.147558185824273));
#82221=DIRECTION('ref_axis',(0.954792146314158,-0.0114882864052091,-0.297052144601374));
#82222=DIRECTION('',(-0.559173898367332,0.,0.829050391342216));
#82223=DIRECTION('center_axis',(-2.83626402819203E-14,-1.,8.78415744494621E-15));
#82224=DIRECTION('ref_axis',(1.,-2.83626402819203E-14,2.53190229195437E-31));
#82225=DIRECTION('center_axis',(0.0623268522204319,-0.987363722435415,0.145699152745555));
#82226=DIRECTION('ref_axis',(0.973462008503631,0.0279320135103828,-0.227137668873598));
#82227=DIRECTION('center_axis',(-0.0793353368674458,-0.987363722342688,
-0.13718157356482));
#82228=DIRECTION('ref_axis',(0.953112573469767,-0.0348178311350821,-0.300606288904418));
#82229=DIRECTION('',(0.929873511942708,0.,0.36787939842744));
#82230=DIRECTION('center_axis',(0.0881576644780861,0.987363722759926,0.13168563008707));
#82231=DIRECTION('ref_axis',(0.868612205916541,-0.0114882885629135,-0.495359319038914));
#82232=DIRECTION('',(-0.367879397953789,0.,0.929873512130095));
#82233=DIRECTION('center_axis',(5.16224067063556E-14,-1.,-2.93518360182265E-14));
#82234=DIRECTION('ref_axis',(1.,5.16224067063556E-14,-4.26445836114867E-31));
#82235=DIRECTION('center_axis',(0.0921906971087603,-0.987363722419199,0.128894356032774));
#82236=DIRECTION('ref_axis',(0.901875122927973,0.027932014716579,-0.431092873053506));
#82237=DIRECTION('center_axis',(-0.10697050717258,-0.987363722176988,-0.116919590847921));
#82238=DIRECTION('ref_axis',(0.866207865215385,-0.0348178347625664,-0.498469309608377));
#82239=DIRECTION('',(0.987216781687272,0.,0.159383267487605));
#82240=DIRECTION('center_axis',(0.114405106934006,0.98736372273398,0.109655599657815));
#82241=DIRECTION('ref_axis',(0.741816923184193,-0.0114882907434627,-0.6705040429806));
#82242=DIRECTION('',(-0.159383264798036,0.,0.987216782121495));
#82243=DIRECTION('center_axis',(-6.61585895537706E-14,-1.,5.96443467821074E-14));
#82244=DIRECTION('ref_axis',(1.,-6.61585895537706E-14,4.65285739771408E-31));
#82245=DIRECTION('center_axis',(0.117743809112344,-0.987363722349516,0.106062600401007));
#82246=DIRECTION('ref_axis',(0.788117558174073,0.0279320182998367,-0.614890654386155));
#82247=DIRECTION('center_axis',(-0.129603858059164,-0.987363721960494,-0.0911905726075923));
#82248=DIRECTION('ref_axis',(0.738800236790062,-0.0348178427955682,-0.673024463108149));
#82249=DIRECTION('',(0.998398893008149,0.,-0.0565654527083613));
#82250=DIRECTION('center_axis',(0.135303091130996,0.987363722741908,0.0824981972144672));
#82251=DIRECTION('ref_axis',(0.580335108423646,-0.0114882902169116,-0.814296740211335));
#82252=DIRECTION('',(0.0565654558858671,0.,0.998398892828124));
#82253=DIRECTION('center_axis',(4.31583891944395E-14,-1.,-6.03933635467864E-14));
#82254=DIRECTION('ref_axis',(-1.07838066469352E-30,6.03933635467864E-14,
-1.));
#82255=DIRECTION('center_axis',(0.13779134444909,-0.987363722465363,0.0782714823818561));
#82256=DIRECTION('ref_axis',(0.637508495489619,0.0279320123949856,-0.769936829137384));
#82257=DIRECTION('center_axis',(-0.146177065940087,-0.987363722148474,-0.0611975945463366));
#82258=DIRECTION('ref_axis',(0.57684713562104,-0.0348178369452184,-0.816109735486753));
#82259=DIRECTION('',(0.962896981574999,0.,-0.269869232914305));
#82260=DIRECTION('center_axis',(0.149874454570686,0.987363722704243,0.0514832686875784));
#82261=DIRECTION('ref_axis',(0.391717465649994,-0.0114882915735154,-0.920013829385987));
#82262=DIRECTION('',(0.269869235978793,0.,0.962896980716121));
#82263=DIRECTION('center_axis',(5.83331641438036E-15,-1.,-1.36518356314104E-14));
#82264=DIRECTION('ref_axis',(-3.1174917420091E-32,1.36518356314104E-14,
-1.));
#82265=DIRECTION('center_axis',(0.151395914356882,-0.98736372247739,0.0468204725695329));
#82266=DIRECTION('ref_axis',(0.457090239152709,0.0279320119247548,-0.88898161734715));
#82267=DIRECTION('center_axis',(-0.155915201154234,-0.987363722160554,-0.0283430804658039));
#82268=DIRECTION('ref_axis',(0.38792129719992,-0.0348178363740269,-0.921034627714378));
#82269=DIRECTION('',(0.882371077791938,0.,-0.470554227561812));
#82270=DIRECTION('center_axis',(0.15743785313733,0.987363722776465,0.0180610449450756));
#82271=DIRECTION('ref_axis',(0.184783553077732,-0.0114882878011365,-0.9827120930137));
#82272=DIRECTION('',(0.470554230370041,0.,0.882371076294355));
#82273=DIRECTION('center_axis',(8.28658681025308E-15,-1.,-4.37599616907709E-14));
#82274=DIRECTION('ref_axis',(1.06847413692382E-31,4.37599616907709E-14,
-1.));
#82275=DIRECTION('center_axis',(0.15792137988059,-0.987363722452379,0.0131801882229025));
#82276=DIRECTION('ref_axis',(0.25529895511123,0.0279320135506513,-0.966458610669966));
#82277=DIRECTION('center_axis',(-0.158362914256743,-0.987363722293327,0.00583671887090705));
#82278=DIRECTION('ref_axis',(0.180856695325737,-0.0348178310148215,-0.982892961822027));
#82279=DIRECTION('',(0.760586482875992,0.,-0.649236630256125));
#82280=DIRECTION('',(0.649236632676749,0.,0.760586480809747));
#82281=DIRECTION('',(0.60323770876311,0.,-0.797561450125464));
#82282=DIRECTION('center_axis',(0.150470361495174,0.987363722775319,-0.0497146785041838));
#82283=DIRECTION('ref_axis',(-0.244925087799148,-0.0114882879430562,-0.969473940138009));
#82284=DIRECTION('',(0.797561452045313,0.,0.603237706224812));
#82285=DIRECTION('center_axis',(1.80893808345559E-14,-1.,7.19915218327124E-14));
#82286=DIRECTION('ref_axis',(9.00090843414257E-33,-7.19915218327125E-14,
-1.));
#82287=DIRECTION('center_axis',(0.148859780283991,-0.987363722466057,-0.0543474504624917));
#82288=DIRECTION('ref_axis',(-0.174102381956169,0.0279320124232198,-0.984331327998442));
#82289=DIRECTION('center_axis',(-0.141275515076049,-0.987363722429259,0.0717921198366065));
#82290=DIRECTION('ref_axis',(-0.248564947590659,-0.0348178268732931,-0.967989248783825));
#82291=DIRECTION('',(0.417682210743198,0.,-0.90859318224862));
#82292=DIRECTION('center_axis',(0.136265263839099,0.987363722824759,-0.0808990526551015));
#82293=DIRECTION('ref_axis',(-0.447607114670165,-0.0114882833099783,-0.89415652446495));
#82294=DIRECTION('',(0.908593184668933,0.,0.417682205478239));
#82295=DIRECTION('center_axis',(-6.62850207133685E-15,-1.,-1.32839436008182E-14));
#82296=DIRECTION('ref_axis',(-1.03424838227994E-31,1.32839436008182E-14,
-1.));
#82297=DIRECTION('center_axis',(0.13369642391556,-0.987363722333989,-0.0850772945677055));
#82298=DIRECTION('ref_axis',(-0.381634103862487,0.0279320177142337,-0.923891342721366));
#82299=DIRECTION('center_axis',(-0.122539383911072,-0.987363722169357,0.10048372771035));
#82300=DIRECTION('ref_axis',(-0.450842714588386,-0.0348178357828447,-0.891924080297182));
#82301=DIRECTION('',(0.212596357404932,0.,-0.97714010705638));
#82302=DIRECTION('center_axis',(0.115688547978383,0.987363722716593,-0.108300687578074));
#82303=DIRECTION('ref_axis',(-0.629359530672324,-0.0114882911178694,-0.777029343280615));
#82304=DIRECTION('',(0.977140108330193,0.,0.212596351550206));
#82305=DIRECTION('center_axis',(-9.32918656287232E-15,-1.,-1.15484403507104E-14));
#82306=DIRECTION('ref_axis',(-1.52838407231594E-31,1.15484403507104E-14,
-1.));
#82307=DIRECTION('center_axis',(0.112281573151259,-0.987363722364002,-0.111829012739007));
#82308=DIRECTION('ref_axis',(-0.571321039142443,0.0279320163939665,-0.820251225353164));
#82309=DIRECTION('center_axis',(-0.0980734510977039,-0.987363722252895,
0.124476817796301));
#82310=DIRECTION('ref_axis',(-0.632039572503668,-0.0348178343586433,-0.774153535934542));
#82311=DIRECTION('',(-0.00243026757266593,0.,-0.999997046895402));
#82312=DIRECTION('center_axis',(0.0897023691207246,0.98736372275528,-0.130638294389373));
#82313=DIRECTION('ref_axis',(-0.781683795070389,-0.0114882888628608,-0.623569133090596));
#82314=DIRECTION('',(0.999997046887668,0.,-0.00243027075520032));
#82315=DIRECTION('center_axis',(-6.95618921132794E-14,-1.,-5.56376694227202E-14));
#82316=DIRECTION('ref_axis',(1.,-6.95618921132794E-14,2.8891161799313E-32));
#82317=DIRECTION('center_axis',(0.0856165603819998,-0.987363722387814,-0.133351731525449));
#82318=DIRECTION('ref_axis',(-0.734293637815565,0.0279320161221314,-0.678257072162861));
#82319=DIRECTION('center_axis',(-0.0690217128897348,-0.987363722232314,
0.142649511633647));
#82320=DIRECTION('ref_axis',(-0.783682965940413,-0.0348178332220065,-0.620184430137167));
#82321=DIRECTION('',(-0.217343253631377,0.,-0.976095236183912));
#82322=DIRECTION('center_axis',(0.0595218040036869,0.987363722728397,-0.146867402401171));
#82323=DIRECTION('ref_axis',(-0.897457392777709,-0.0114882912460929,-0.440951524901414));
#82324=DIRECTION('',(0.976095235356397,0.,-0.217343257347773));
#82325=DIRECTION('center_axis',(-1.06528037232494E-13,-1.,-5.25108546845533E-14));
#82326=DIRECTION('ref_axis',(1.,-1.06528037232494E-13,-8.41003740475711E-31));
#82327=DIRECTION('center_axis',(0.0549482133195925,-0.98736372243382,-0.14863907115767));
#82328=DIRECTION('ref_axis',(-0.862931481368871,0.0279320151382408,-0.504548373293229));
#82329=DIRECTION('center_axis',(-0.0367425905234866,-0.987363722095364,
0.154152075339946));
#82330=DIRECTION('ref_axis',(-0.898682215257586,-0.0348178378225455,-0.437216186970566));
#82331=DIRECTION('',(-0.422093512262599,0.,-0.906552296839969));
#82332=DIRECTION('center_axis',(0.0265580714999559,0.987363722790579,-0.156229151426141));
#82333=DIRECTION('ref_axis',(-0.971266881255812,-0.0114882866172744,-0.237715512001651));
#82334=DIRECTION('',(0.906552294984449,0.,-0.422093516247796));
#82335=DIRECTION('center_axis',(1.44157190590594E-14,-1.,3.54785012783786E-15));
#82336=DIRECTION('ref_axis',(1.,1.44157190590594E-14,-6.21377867058364E-32));
#82337=DIRECTION('center_axis',(0.0217105441157315,-0.987363722315354,-0.156976215172135));
#82338=DIRECTION('ref_axis',(-0.951219608639794,0.0279320193667842,-0.307247552363319));
#82339=DIRECTION('center_axis',(-0.00274543728998556,-0.987363722329321,
0.158446654751922));
#82340=DIRECTION('ref_axis',(-0.97166008011877,-0.0348178304814863,-0.233804207370502));
#82341=DIRECTION('',(-0.6071071473932,0.,-0.794619979351194));
#82342=DIRECTION('center_axis',(-0.0076474896256404,0.987363722817488,-0.158285800899564));
#82343=DIRECTION('ref_axis',(-0.999661009578761,-0.0114882853853447,-0.0233641868439042));
#82344=DIRECTION('',(0.794619977419008,0.,-0.607107149922166));
#82345=DIRECTION('center_axis',(-7.42068524027303E-14,-1.,-1.82974945934095E-15));
#82346=DIRECTION('ref_axis',(-0.99969614439276,7.42294074245818E-14,-0.0246499266986752));
#82347=DIRECTION('center_axis',(-0.0125422745102943,-0.987363722475656,
-0.157973323346459));
#82348=DIRECTION('ref_axis',(-0.995029764692228,0.0279320112165366,-0.0955801764275887));
#82349=DIRECTION('center_axis',(0.0313800969965281,-0.987363722278222,0.155332448127826));
#82350=DIRECTION('ref_axis',(-0.999204200729344,-0.0348178311476597,-0.0194598016178513));
#82351=DIRECTION('',(-0.763733125487799,0.,-0.645532116189921));
#82352=DIRECTION('center_axis',(-0.0414954679937745,0.987363722747479,-0.152941181956391));
#82353=DIRECTION('ref_axis',(-0.981312099500299,-0.0114882890458985,0.192079625648099));
#82354=DIRECTION('',(0.64553211208243,0.,-0.763733128959585));
#82355=DIRECTION('',(-0.884647793282078,0.,-0.466259886588103));
#82356=DIRECTION('center_axis',(0.,-1.,0.));
#82357=DIRECTION('ref_axis',(0.,0.,-1.));
#82358=DIRECTION('center_axis',(-0.0462086416140792,-0.987363722411243,
-0.151583775867986));
#82359=DIRECTION('ref_axis',(-0.992313434186013,0.0279320148958749,0.120556421968377));
#82360=DIRECTION('center_axis',(0.0640383411135482,-0.987363722029644,0.144955066441962));
#82361=DIRECTION('ref_axis',(-0.980026643477236,-0.0348178399924535,0.19579452518649));
#82362=DIRECTION('',(0.46625988377264,0.,-0.884647794765987));
#82363=DIRECTION('center_axis',(-0.0734031560636246,0.98736372281198,-0.140445204812293));
#82364=DIRECTION('ref_axis',(-0.917078127633942,-0.0114882850235305,0.398542001704515));
#82365=DIRECTION('center_axis',(0.,-1.,0.));
#82366=DIRECTION('ref_axis',(0.,0.,-1.));
#82367=DIRECTION('center_axis',(-0.077714340139779,-0.98736372241589,-0.138106339440582));
#82368=DIRECTION('ref_axis',(-0.943197630236814,0.0279320146514098,0.331055936169662));
#82369=DIRECTION('center_axis',(0.093702206075612,-0.98736372236211,0.12779975093795));
#82370=DIRECTION('ref_axis',(-0.915024129431169,-0.0348178301339077,0.401893718865446));
#82371=DIRECTION('',(-0.964197312368427,0.,-0.265185864671369));
#82372=DIRECTION('center_axis',(-0.101878603038959,0.987363722747707,-0.121382161970443));
#82373=DIRECTION('ref_axis',(-0.809962599989905,-0.0114882903200018,0.586369001400241));
#82374=DIRECTION('',(0.265185861599813,0.,-0.964197313213206));
#82375=DIRECTION('center_axis',(-3.61097266571981E-14,-1.,2.60708536588153E-14));
#82376=DIRECTION('ref_axis',(1.,-3.61097266571981E-14,7.16384221097358E-31));
#82377=DIRECTION('center_axis',(-0.105586200624493,-0.987363722469058,-0.118171205417098));
#82378=DIRECTION('ref_axis',(-0.849978954034902,0.027932012352796,0.526075641313735));
#82379=DIRECTION('center_axis',(0.118984673112858,-0.987363722197065,0.104668656499369));
#82380=DIRECTION('ref_axis',(-0.807236104611648,-0.0348178350983758,0.589200805982541));
#82381=DIRECTION('',(-0.998662037017743,0.,-0.0517120471415683));
#82382=DIRECTION('center_axis',(-0.125590314053738,0.987363722735068,-0.0966434273121139));
#82383=DIRECTION('ref_axis',(-0.664974122526173,-0.0114882892188372,0.746778036354425));
#82384=DIRECTION('',(0.0517120410961091,0.,-0.998662037330785));
#82385=DIRECTION('center_axis',(5.93220768500817E-14,-1.,-6.64477108557578E-14));
#82386=DIRECTION('ref_axis',(-4.62814580839856E-31,6.64477108557578E-14,
-1.));
#82387=DIRECTION('center_axis',(-0.12852097045819,-0.987363722436845,-0.0927105159523013));
#82388=DIRECTION('ref_axis',(-0.71701620639877,0.0279320129697168,0.696496634889915));
#82389=DIRECTION('center_axis',(0.138703544670002,-0.98736372222561,0.0766433736781297));
#82390=DIRECTION('ref_axis',(-0.661702615127607,-0.0348178349574889,0.748957520492423));
#82391=DIRECTION('',(-0.986430434661682,0.,0.164179772119362));
#82392=DIRECTION('center_axis',(-0.143429559359027,0.987363722836541,-0.0673857576082798));
#82393=DIRECTION('ref_axis',(-0.488892194469872,-0.0114882833766482,0.872268560439668));
#82394=DIRECTION('',(-0.164179775258991,0.,-0.986430434139127));
#82395=DIRECTION('center_axis',(1.45502886631244E-14,-1.,-2.58822310819358E-14));
#82396=DIRECTION('ref_axis',(3.34261249505911E-31,2.58822310819358E-14,
-1.));
#82397=DIRECTION('center_axis',(-0.145446240355865,-0.987363722521506,-0.0629147885223953));
#82398=DIRECTION('ref_axis',(-0.550526577599503,0.0279320098890628,0.834350220339238));
#82399=DIRECTION('center_axis',(0.151936792278092,-0.987363722246792,0.0450343329383656));
#82400=DIRECTION('ref_axis',(-0.485228646736117,-0.0348178338663002,0.873693812975401));
#82401=DIRECTION('',(-0.928074440978592,0.,0.372394726066675));
#82402=DIRECTION('center_axis',(-0.154562204409905,0.987363722712876,-0.0349771931195304));
#82403=DIRECTION('ref_axis',(-0.289950209006206,-0.0114882910818072,0.956972776762891));
#82404=DIRECTION('',(-0.372394728026814,0.,-0.928074440192076));
#82405=DIRECTION('center_axis',(8.64619638763411E-15,-1.,-2.84050008514506E-14));
#82406=DIRECTION('ref_axis',(-1.15512849116693E-31,2.84050008514506E-14,
-1.));
#82407=DIRECTION('center_axis',(-0.155570610176543,-0.987363722363232,-0.0301772266837314));
#82408=DIRECTION('ref_axis',(-0.358294937629885,0.0279320170368305,0.933190516504026));
#82409=DIRECTION('center_axis',(0.158065646374136,-0.987363722077046,0.0113195301354719));
#82410=DIRECTION('ref_axis',(-0.286065929346506,-0.0348178405079036,0.957577152008905));
#82411=DIRECTION('',(-0.826322717534286,0.,0.563196916261757));
#82412=DIRECTION('center_axis',(-0.158467688071278,0.987363722788458,-0.000933144502251157));
#82413=DIRECTION('ref_axis',(-0.0774504756911478,-0.0114882872480132,0.99693000911364));
#82414=DIRECTION('',(-0.563196917553715,0.,-0.826322716653726));
#82415=DIRECTION('center_axis',(-9.3512703384342E-15,-1.,1.18398337479732E-13));
#82416=DIRECTION('ref_axis',(2.38006789847537E-31,-1.18398337479732E-13,
-1.));
#82417=DIRECTION('center_axis',(-0.158420667211256,-0.987363722412121,0.00397138071973608));
#82418=DIRECTION('ref_axis',(-0.149309823991232,0.0279320148995181,0.988395861486358));
#82419=DIRECTION('center_axis',(0.15680352394228,-0.987363722029905,-0.0229245566704076));
#82420=DIRECTION('ref_axis',(-0.073527080722506,-0.0348178407589832,0.996685249396874));
#82421=DIRECTION('',(-0.68593306312575,0.,0.727664643163955));
#82422=DIRECTION('',(0.761154167860895,0.,-0.648570992835779));
#82423=DIRECTION('center_axis',(0.153257689897193,-0.987363722734368,0.0403107865900156));
#82424=DIRECTION('ref_axis',(-0.18881520529075,0.0107821800906864,0.98195344229933));
#82425=DIRECTION('center_axis',(-0.154002417765247,-0.987363721883716,-0.0373649037252043));
#82426=DIRECTION('ref_axis',(-0.188347474697552,-0.00778744783873706,0.982071578058959));
#82427=DIRECTION('',(0.46978211759282,0.,0.882782397870509));
#82428=DIRECTION('center_axis',(1.1099822106242E-14,-1.,-5.83369275286436E-14));
#82429=DIRECTION('ref_axis',(8.44183654759075E-32,5.83369275286436E-14,
-1.));
#82430=DIRECTION('center_axis',(0.157871543102446,0.98736372238965,0.0137642866617665));
#82431=DIRECTION('ref_axis',(-0.111617347157657,0.0039934990218299,0.9937432363438));
#82432=DIRECTION('center_axis',(-0.145446222113249,0.98736372086277,-0.0629148567272404));
#82433=DIRECTION('ref_axis',(-0.191537738360655,0.0342871344957478,0.980886174431955));
#82434=DIRECTION('',(0.88278239777599,0.,-0.469782117770433));
#82435=DIRECTION('center_axis',(0.141008981378088,-0.987363722661823,0.072314219501428));
#82436=DIRECTION('ref_axis',(-0.395491774985701,0.0107821839268003,0.918406228435124));
#82437=DIRECTION('center_axis',(-0.14236957508107,-0.987363721868668,-0.0695973047530321));
#82438=DIRECTION('ref_axis',(-0.395060375331871,-0.00778745240990678,0.918622150520879));
#82439=DIRECTION('',(0.269026752423883,0.,0.96313270450144));
#82440=DIRECTION('center_axis',(1.75357720831305E-14,-1.,-4.09401817359017E-14));
#82441=DIRECTION('ref_axis',(-1.24101159417695E-32,4.09401817359017E-14,
-1.));
#82442=DIRECTION('center_axis',(0.151221679088276,0.98736372240244,0.0473802011110068));
#82443=DIRECTION('ref_axis',(-0.322633218628695,0.0039934985935031,0.946515640761563));
#82444=DIRECTION('center_axis',(-0.128520934758922,0.987363720788093,-0.0927105829999236));
#82445=DIRECTION('ref_axis',(-0.397921226436083,0.0342871368088993,0.916778648203072));
#82446=DIRECTION('',(0.963132705018708,0.,-0.269026750572033));
#82447=DIRECTION('center_axis',(0.122166850775448,-0.987363722682965,0.100936315076614));
#82448=DIRECTION('ref_axis',(-0.583675588839591,0.010782182662631,0.811915359831175));
#82449=DIRECTION('center_axis',(-0.124079693435435,-0.987363721896849,-0.0985754044321944));
#82450=DIRECTION('ref_axis',(-0.583300690181401,-0.0077874473065718,0.812218973244499));
#82451=DIRECTION('',(0.0556919954647298,0.,0.998447996463089));
#82452=DIRECTION('center_axis',(-4.32112072582799E-14,-1.,6.03555839612015E-14));
#82453=DIRECTION('ref_axis',(5.52801095037507E-31,-6.03555839612015E-14,
-1.));
#82454=DIRECTION('center_axis',(0.137500857919074,0.987363722378521,0.0787806689635775));
#82455=DIRECTION('ref_axis',(-0.518563117419946,0.00399349906777367,0.855030025915408));
#82456=DIRECTION('center_axis',(-0.10558615361227,0.987363720860938,-0.118171260859017));
#82457=DIRECTION('ref_axis',(-0.585698356105705,0.0342871345631837,0.809803573750154));
#82458=DIRECTION('',(0.998447996527099,0.,-0.05569199431715));
#82459=DIRECTION('center_axis',(0.0976123324921318,-0.987363722657208,0.124838742888357));
#82460=DIRECTION('ref_axis',(-0.744567380952206,0.0107821840596194,0.66746023082194));
#82461=DIRECTION('center_axis',(-0.0999879825042087,-0.987363721894786,
-0.122944231425527));
#82462=DIRECTION('ref_axis',(-0.744266513551164,-0.00778744565864629,0.66783733984894));
#82463=DIRECTION('',(-0.160246858747463,0.,0.987076969775696));
#82464=DIRECTION('center_axis',(-5.51756196524937E-14,-1.,4.96553716611219E-14));
#82465=DIRECTION('ref_axis',(1.,-5.51756196524937E-14,5.66722537932442E-31));
#82466=DIRECTION('center_axis',(0.117350647949358,0.987363722424568,0.10649744159259));
#82467=DIRECTION('ref_axis',(-0.690245581144517,0.0039934975576326,0.723564157271299));
#82468=DIRECTION('center_axis',(-0.0777142754592605,0.98736372070586,-0.138106388062694));
#82469=DIRECTION('ref_axis',(-0.746088886902966,0.0342871399768338,0.664962980076412));
#82470=DIRECTION('',(0.987076969591517,0.,0.160246859881955));
#82471=DIRECTION('center_axis',(0.0684935700481875,-0.987363722645525,0.142903849023131));
#82472=DIRECTION('ref_axis',(-0.870644028746578,0.0107821851182117,0.491795404301427));
#82473=DIRECTION('center_axis',(-0.0712209419243646,-0.987363721889244,
-0.141564325055521));
#82474=DIRECTION('ref_axis',(-0.870431263362817,-0.0077874473242738,0.492228373242321));
#82475=DIRECTION('',(-0.368692746674862,0.,0.929551321094939));
#82476=DIRECTION('center_axis',(-9.03841140943282E-14,-1.,5.12866612338516E-14));
#82477=DIRECTION('ref_axis',(1.,-9.03841140943282E-14,2.57510117333047E-31));
#82478=DIRECTION('center_axis',(0.0917132551111147,0.987363722365359,0.129234510072762));
#82479=DIRECTION('ref_axis',(-0.829652928099899,0.00399349968643042,0.558265233428985));
#82480=DIRECTION('center_axis',(-0.0462085670591155,0.987363720688045,-0.151583809819533));
#82481=DIRECTION('ref_axis',(-0.871593127806196,0.0342871408666792,0.489029458757037));
#82482=DIRECTION('',(0.929551320671185,0.,0.368692747743234));
#82483=DIRECTION('center_axis',(0.036172125985831,-0.987363722634944,0.154286929213499));
#82484=DIRECTION('ref_axis',(-0.956010329767849,0.0107821842182488,0.293134770848927));
#82485=DIRECTION('center_axis',(-0.0391236905722506,-0.98736372188221,-0.153565027095745));
#82486=DIRECTION('ref_axis',(-0.955895614537263,-0.00778744719550599,0.293603354501621));
#82487=DIRECTION('',(-0.559898972904418,0.,0.828560884993117));
#82488=DIRECTION('center_axis',(8.51109427279946E-14,-1.,-2.62780241083103E-14));
#82489=DIRECTION('ref_axis',(1.,8.51109427279946E-14,-1.61762959713368E-31));
#82490=DIRECTION('center_axis',(0.0617874444496923,0.987363722445373,0.145928719953246));
#82491=DIRECTION('ref_axis',(-0.930266626826431,0.00399349312500233,0.366862447009278));
#82492=DIRECTION('center_axis',(-0.0125422004180125,0.987363720749498,-0.157973340017808));
#82493=DIRECTION('ref_axis',(-0.956342642361099,0.0342871387732709,0.290229465279688));
#82494=DIRECTION('',(0.82856088525082,0.,0.55989897252306));
#82495=DIRECTION('center_axis',(0.00215930871990054,-0.987363722594613,
0.15845572469924));
#82496=DIRECTION('ref_axis',(-0.996674650224871,0.0107821882209069,0.0807674811808595));
#82497=DIRECTION('center_axis',(-0.00519705505445424,-0.987363721855407,
-0.158385199379862));
#82498=DIRECTION('ref_axis',(-0.99666334859478,-0.00778745117250021,0.0812497702893763));
#82499=DIRECTION('',(-0.724924943069254,0.,0.6888278645032));
#82500=DIRECTION('center_axis',(0.,-1.,0.));
#82501=DIRECTION('ref_axis',(0.,0.,-1.));
#82502=DIRECTION('center_axis',(0.0289725338065441,0.987363722367401,0.155799460967034));
#82503=DIRECTION('ref_axis',(-0.987382091802038,0.00399349993332521,0.158305580277241));
#82504=DIRECTION('center_axis',(0.0217106310419858,0.987363720643665,-0.156976213664544));
#82505=DIRECTION('ref_axis',(-0.996374638587734,0.0342871422369901,0.0778586633354473));
#82506=DIRECTION('',(0.688827863670013,0.,0.724924943860953));
#82507=DIRECTION('center_axis',(-0.0319544657509305,-0.987363722688464,
0.15521530606661));
#82508=DIRECTION('ref_axis',(-0.99073557192863,0.0107821823962816,-0.13537640510083));
#82509=DIRECTION('center_axis',(0.0289725837152514,-0.987363721882134,-0.155799454761312));
#82510=DIRECTION('ref_axis',(-0.990828212218113,-0.00778744957994967,-0.134902963279899));
#82511=DIRECTION('',(-0.856054231466657,0.,0.516886015276125));
#82512=DIRECTION('center_axis',(-1.47130759122275E-14,-1.,-1.9813114182039E-15));
#82513=DIRECTION('ref_axis',(1.,-1.47130759122275E-14,-5.10197245919429E-32));
#82514=DIRECTION('center_axis',(-0.00519711077038148,0.987363722453804,
0.158385193821289));
#82515=DIRECTION('ref_axis',(-0.998328667570516,0.00399349550016951,-0.057653477783817));
#82516=DIRECTION('center_axis',(0.0549482872906021,0.987363720830978,-0.148639054459575));
#82517=DIRECTION('ref_axis',(-0.989817264642019,0.0342871350541035,-0.138152723412795));
#82518=DIRECTION('',(0.516886016398843,0.,0.85605423078876));
#82519=DIRECTION('center_axis',(-0.0645740904836284,-0.987363722683157,
0.144717193061053));
#82520=DIRECTION('ref_axis',(-0.938470799614058,0.0107821821538341,-0.34519024148975));
#82521=DIRECTION('center_axis',(0.061787500539433,-0.987363721862154,-0.145928700150466));
#82522=DIRECTION('ref_axis',(-0.938663049981464,-0.00778745220173615,-0.344747783441317));
#82523=DIRECTION('',(-0.947155372266923,0.,0.320775156123267));
#82524=DIRECTION('center_axis',(-6.97158450332253E-14,-1.,-2.54893293604934E-14));
#82525=DIRECTION('ref_axis',(1.,-6.97158450332253E-14,5.10773051084881E-31));
#82526=DIRECTION('center_axis',(-0.0391237406597983,0.987363722421879,0.15356501086509));
#82527=DIRECTION('ref_axis',(-0.96259450430855,0.00399349509328662,-0.270916725714593));
#82528=DIRECTION('center_axis',(0.0856166299241214,0.987363720838917,-0.133351698345259));
#82529=DIRECTION('ref_axis',(-0.936977134491496,0.0342871348173222,-0.347704244762878));
#82530=DIRECTION('',(0.320775152455668,0.,0.947155373509037));
#82531=DIRECTION('center_axis',(-0.0941743021688814,-0.987363722710651,
0.127452265126865));
#82532=DIRECTION('ref_axis',(-0.842324175661386,0.0107821814342959,-0.538863366411083));
#82533=DIRECTION('center_axis',(0.0917132966142065,-0.98736372187387,-0.129234484374461));
#82534=DIRECTION('ref_axis',(-0.842607046355374,-0.00778744790203565,-0.538472581555872));
#82535=DIRECTION('',(-0.993968582433906,0.,0.10966520475671));
#82536=DIRECTION('center_axis',(0.,-1.,0.));
#82537=DIRECTION('ref_axis',(0.,0.,-1.));
#82538=DIRECTION('center_axis',(-0.0712209816399244,0.987363722372652,0.141564301703027));
#82539=DIRECTION('ref_axis',(-0.881850493045238,0.00399350132227135,-0.471512205423211));
#82540=DIRECTION('center_axis',(0.112281636624268,0.987363720745417,-0.111828963299954));
#82541=DIRECTION('ref_axis',(-0.840324996204307,0.0342871383705696,-0.540997498050211));
#82542=DIRECTION('',(0.109665200774071,0.,0.993968582873313));
#82543=DIRECTION('center_axis',(-0.11937103403139,-0.987363722603769,0.104227805888375));
#82544=DIRECTION('ref_axis',(-0.706791409383475,0.0107821886588213,-0.707339839136356));
#82545=DIRECTION('center_axis',(0.117350683385862,-0.987363721880914,-0.106497407585072));
#82546=DIRECTION('ref_axis',(-0.707151675129846,-0.00778744623160996,-0.707018998360188));
#82547=DIRECTION('',(-0.994304926390161,0.,-0.106572573189616));
#82548=DIRECTION('center_axis',(7.3597573916883E-14,-1.,7.33689771798346E-14));
#82549=DIRECTION('ref_axis',(1.,7.3597573916883E-14,9.18989021195146E-31));
#82550=DIRECTION('center_axis',(-0.0999880192034275,0.987363722417957,0.122944197377228));
#82551=DIRECTION('ref_axis',(-0.759872130882321,0.00399349582696179,-0.650060302356205));
#82552=DIRECTION('center_axis',(0.133696477668497,0.987363720680591,-0.0850772292850251));
#82553=DIRECTION('ref_axis',(-0.704380193370113,0.0342871409978466,-0.708994312494872));
#82554=DIRECTION('',(-0.106572574332393,0.,0.994304926267675));
#82555=DIRECTION('center_axis',(-0.138986101728336,-0.987363722614939,0.0761297759771471));
#82556=DIRECTION('ref_axis',(-0.538209861740386,0.0107821861776475,-0.842741887642133));
#82557=DIRECTION('center_axis',(0.137500887126174,-0.987363721858741,-0.0787806245010161));
#82558=DIRECTION('ref_axis',(-0.538630675840616,-0.00778745178170863,-0.842505994422728));
#82559=DIRECTION('',(-0.94814867668019,0.,-0.317827133690004));
#82560=DIRECTION('center_axis',(6.41197054336129E-14,-1.,9.99713762191257E-14));
#82561=DIRECTION('ref_axis',(-4.18067723980065E-31,-9.99713762191257E-14,
-1.));
#82562=DIRECTION('center_axis',(-0.124079723161249,0.987363722414627,0.0985753618292045));
#82563=DIRECTION('ref_axis',(-0.602362992892309,0.00399349586706796,-0.798212300572085));
#82564=DIRECTION('center_axis',(0.148859815873385,0.987363720773916,-0.054347383723873));
#82565=DIRECTION('ref_axis',(-0.535499356440476,0.0342871370330924,-0.8438393398544));
#82566=DIRECTION('',(-0.317827133913437,0.,0.948148676605294));
#82567=DIRECTION('center_axis',(-0.152102334827415,-0.987363722642613,0.0444720018592623));
#82568=DIRECTION('ref_axis',(-0.344462219111818,0.0107821847411895,-0.938738261762441));
#82569=DIRECTION('center_axis',(0.151221697237912,-0.987363721876949,-0.0473801541342403));
#82570=DIRECTION('ref_axis',(-0.344923905103641,-0.00778744840236856,-0.938598346117995));
#82571=DIRECTION('',(-0.85765804862894,0.,-0.514220450412077));
#82572=DIRECTION('center_axis',(1.5423649336475E-14,-1.,4.17817283315104E-14));
#82573=DIRECTION('ref_axis',(-3.87248343031339E-31,-4.17817283315104E-14,
-1.));
#82574=DIRECTION('center_axis',(-0.142369594341165,0.987363722348721,0.0695972585437816));
#82575=DIRECTION('ref_axis',(-0.416688032452796,0.00399350289763168,-0.909040777713092));
#82576=DIRECTION('center_axis',(0.157062637484616,0.987363720750114,-0.021076310228941));
#82577=DIRECTION('ref_axis',(-0.341579164027156,0.0342871386853031,-0.939227377594629));
#82578=DIRECTION('',(-0.514220451397814,0.,0.857658048037928));
#82579=DIRECTION('center_axis',(-0.158106432739376,-0.987363722622455,0.0107347648114259));
#82580=DIRECTION('ref_axis',(-0.134607907972329,0.0107821854895616,-0.990840277535881));
#82581=DIRECTION('center_axis',(0.157871551018963,-0.98736372185081,-0.0137642345149945));
#82582=DIRECTION('ref_axis',(-0.135088876457087,-0.00778745163005778,-0.990802882037932));
#82583=DIRECTION('',(-0.727064283330936,0.,-0.686569390451156));
#82584=DIRECTION('center_axis',(1.21624329307288E-14,-1.,8.82410470081755E-14));
#82585=DIRECTION('ref_axis',(1.75892719290299E-32,-8.82410470081755E-14,
-1.));
#82586=DIRECTION('center_axis',(-0.154002425721275,0.987363722322915,0.0373648593279877));
#82587=DIRECTION('ref_axis',(-0.211529202855841,0.00399350306266881,-0.977363519000203));
#82588=DIRECTION('center_axis',(0.157921384382321,0.987363720665047,0.0131802681780967));
#82589=DIRECTION('ref_axis',(-0.131687111262305,0.0342871405833779,-0.990698186491731));
#82590=DIRECTION('',(-0.686569391286805,0.,0.72706428254183));
#82591=DIRECTION('center_axis',(-0.156717649183816,-0.987363722713147,-0.0235044145711971));
#82592=DIRECTION('ref_axis',(0.0815405202994448,0.0107821826469929,-0.996611703767652));
#82593=DIRECTION('center_axis',(0.157139505704567,-0.987363721919153,0.0204952771360236));
#82594=DIRECTION('ref_axis',(0.0810627569208432,-0.00778744642864526,-0.996678576632664));
#82595=DIRECTION('',(-0.562473799699905,0.,-0.826815109109135));
#82596=DIRECTION('center_axis',(7.09113469916638E-15,-1.,-8.8792583730072E-14));
#82597=DIRECTION('ref_axis',(1.79109581697142E-31,8.8792583730072E-14,-1.));
#82598=DIRECTION('center_axis',(-0.158434274586989,0.987363722374258,0.00338531761353594));
#82599=DIRECTION('ref_axis',(0.00352049925138151,0.00399350036430735,-0.999985828919521));
#82600=DIRECTION('center_axis',(0.151395902272578,0.987363720784873,0.0468205473368705));
#82601=DIRECTION('ref_axis',(0.0843624842551672,0.034287137723654,-0.995845049913397));
#82602=DIRECTION('',(-0.826815108418627,0.,0.562473800714926));
#82603=DIRECTION('center_axis',(-0.148000923743781,-0.98736372267634,-0.0566445559052908));
#82604=DIRECTION('ref_axis',(0.293876205497284,0.0107821818853998,-0.955782674249909));
#82605=DIRECTION('center_axis',(0.149059792165184,-0.987363721865846,0.0537964599476181));
#82606=DIRECTION('ref_axis',(0.293423987027018,-0.00778744878999118,-0.955950688832071));
#82607=DIRECTION('',(-0.371582668334801,0.,-0.928399871064828));
#82608=DIRECTION('center_axis',(0.,-1.,0.));
#82609=DIRECTION('ref_axis',(0.,0.,-1.));
#82610=DIRECTION('center_axis',(-0.155457912687852,0.987363722342951,-0.0307525150810125));
#82611=DIRECTION('ref_axis',(0.218405587602123,0.00399350060691493,-0.975849912259603));
#82612=DIRECTION('center_axis',(0.137791315732748,0.987363720667919,0.0782715556089313));
#82613=DIRECTION('ref_axis',(0.296467386930115,0.0342871404434376,-0.954427304977724));
#82614=DIRECTION('',(-0.928399871491895,0.,0.371582667267774));
#82615=DIRECTION('center_axis',(-0.132363838760895,-0.987363722668939,-0.0871360622579147));
#82616=DIRECTION('ref_axis',(0.492470564867695,0.0107821829897946,-0.870262309461273));
#82617=DIRECTION('center_axis',(0.134010209521018,-0.987363721882876,0.0845821757448213));
#82618=DIRECTION('ref_axis',(0.492065037535445,-0.00778744648125535,-0.870523609394107));
#82619=DIRECTION('',(-0.163316741957422,0.,-0.986573687970854));
#82620=DIRECTION('center_axis',(-4.37187777539197E-14,-1.,7.76084762604717E-14));
#82621=DIRECTION('ref_axis',(-3.72167831404108E-31,-7.76084762604717E-14,
-1.));
#82622=DIRECTION('center_axis',(-0.145212512392347,0.987363722361678,-0.0634523916711932));
#82623=DIRECTION('ref_axis',(0.423078269486658,0.00399350308370285,-0.906084339242929));
#82624=DIRECTION('center_axis',(0.117743765163003,0.98736372094914,0.106062662227139));
#82625=DIRECTION('ref_axis',(0.494709800043066,0.0342871317601711,-0.868381601795553));
#82626=DIRECTION('',(-0.986573688235236,0.,0.16331674036033));
#82627=DIRECTION('center_axis',(-0.110537568239643,-0.987363722654522,-0.113553182225208));
#82628=DIRECTION('ref_axis',(0.668037549826968,0.0107821826083705,-0.744049444969473));
#82629=DIRECTION('center_axis',(0.112694458303171,-0.987363721903264,0.111412924461612));
#82630=DIRECTION('ref_axis',(0.667697674265223,-0.00778744546243803,-0.74439181314277));
#82631=DIRECTION('',(0.0525856941427118,0.,-0.99861641523236));
#82632=DIRECTION('center_axis',(-2.96900927039073E-14,-1.,3.31978941985153E-14));
#82633=DIRECTION('ref_axis',(-2.03427355717816E-31,-3.31978941985153E-14,
-1.));
#82634=DIRECTION('center_axis',(-0.128177133532957,0.987363722358752,-0.0931853111232876));
#82635=DIRECTION('ref_axis',(0.607968284882378,0.00399349903820969,-0.793951268367657));
#82636=DIRECTION('center_axis',(0.0921906441866638,0.987363720942169,0.128894405199308));
#82637=DIRECTION('ref_axis',(0.669820133955363,0.0342871320156405,-0.741731339991888));
#82638=DIRECTION('',(-0.998616415322888,0.,-0.0525856924235507));
#82639=DIRECTION('center_axis',(-0.0835426829196343,-0.987363722641279,
-0.134660682244467));
#82640=DIRECTION('ref_axis',(0.812367839804286,0.0107821836697777,-0.5830456563315));
#82641=DIRECTION('center_axis',(0.086109234869091,-0.987363721866257,0.133034132509938));
#82642=DIRECTION('ref_axis',(0.812109509998393,-0.00778745053491031,-0.583453082419088));
#82643=DIRECTION('',(0.266029277211529,0.,-0.963964949397182));
#82644=DIRECTION('center_axis',(-2.40883471761575E-14,-1.,1.73595023882834E-14));
#82645=DIRECTION('ref_axis',(1.,-2.40883471761575E-14,-4.21994572424516E-31));
#82646=DIRECTION('center_axis',(-0.105148334878442,0.98736372239929,-0.118560985834753));
#82647=DIRECTION('ref_axis',(0.76443037844203,0.00399349783751838,-0.644693918452777));
#82648=DIRECTION('center_axis',(0.0623267879409281,0.987363720822469,0.145699191173377));
#82649=DIRECTION('ref_axis',(0.813610424532457,0.0342871357841829,-0.580398543598993));
#82650=DIRECTION('',(-0.96396494909142,0.,-0.266029278319467));
#82651=DIRECTION('center_axis',(-0.0526414310432203,-0.987363722597889,
-0.149471599427316));
#82652=DIRECTION('ref_axis',(0.918712712274094,0.0107821884151984,-0.394779301279786));
#82653=DIRECTION('center_axis',(0.0554976459794082,-0.987363721875457,0.148434807289226));
#82654=DIRECTION('ref_axis',(0.918548006720365,-0.00778744714791775,-0.395232735254764));
#82655=DIRECTION('',(0.467033631299099,0.,-0.884239553082522));
#82656=DIRECTION('center_axis',(4.08854323012095E-14,-1.,-1.76630464062346E-14));
#82657=DIRECTION('ref_axis',(1.,4.08854323012095E-14,6.6808424631127E-32));
#82658=DIRECTION('center_axis',(-0.0772029153070789,0.987363722443365,-0.138392880853279));
#82659=DIRECTION('ref_axis',(0.885148556303636,0.00399349489836831,-0.46529139823565));
#82660=DIRECTION('center_axis',(0.0295485949190189,0.987363720562215,0.155691245276839));
#82661=DIRECTION('ref_axis',(0.919357195679558,0.0342871443428298,-0.391926955547883));
#82662=DIRECTION('',(-0.884239552545753,0.,-0.467033632315368));
#82663=DIRECTION('center_axis',(-0.0192787361679484,-0.98736372270696,-0.157293386428101));
#82664=DIRECTION('ref_axis',(0.982099599572674,0.0107821803329207,-0.18805350596695));
#82665=DIRECTION('center_axis',(0.0222910451404309,-0.987363721898582,0.156894837343769));
#82666=DIRECTION('ref_axis',(0.982036219967827,-0.00778744788706836,-0.188531743551871));
#82667=DIRECTION('',(0.6462000100523,0.,-0.763168098788469));
#82668=DIRECTION('center_axis',(-5.83021152723025E-14,-1.,1.12812464120419E-14));
#82669=DIRECTION('ref_axis',(1.,-5.83021152723025E-14,1.73804291370917E-31));
#82670=DIRECTION('center_axis',(-0.0456475817544446,0.987363722372612,-0.151753675482572));
#82671=DIRECTION('ref_axis',(0.964478171007239,0.00399350098066409,-0.264132371360362));
#82672=DIRECTION('center_axis',(-0.00461124735747092,0.987363720695088,
0.158403344197525));
#82673=DIRECTION('ref_axis',(0.98211584554125,0.0342871412890047,-0.185129300433572));
#82674=DIRECTION('',(-0.763168097828485,0.,-0.646200011186051));
#82675=DIRECTION('',(0.795150795057726,0.,-0.606411752128096));
#82676=DIRECTION('',(-0.606411752600396,0.,-0.795150794697532));
#82677=DIRECTION('center_axis',(0.0485488734866696,-0.987363722705137,-0.150850541825439));
#82678=DIRECTION('ref_axis',(0.970291073781123,0.0107821822196579,0.241700179328144));
#82679=DIRECTION('center_axis',(-0.0456476284023987,-0.9873637218804,0.151753664653351));
#82680=DIRECTION('ref_axis',(0.97043435862057,-0.00778744848726708,0.241239530870754));
#82681=DIRECTION('',(0.906921212507855,0.,-0.421300266203668));
#82682=DIRECTION('center_axis',(1.15300878293867E-13,-1.,2.84836816942017E-14));
#82683=DIRECTION('ref_axis',(1.,1.15300878293867E-13,1.16424979269799E-32));
#82684=DIRECTION('center_axis',(0.0222910902114904,0.987363722384019,-0.156894827885296));
#82685=DIRECTION('ref_axis',(0.986242984785856,0.00399350219507649,0.165253825677056));
#82686=DIRECTION('center_axis',(-0.070696892983569,0.987363720655471,0.141826769179359));
#82687=DIRECTION('ref_axis',(0.969077975887884,0.0342871413349356,0.244360939161972));
#82688=DIRECTION('',(-0.421300264062887,0.,-0.906921213502331));
#82689=DIRECTION('center_axis',(0.0798422345229059,-0.987363722715342,-0.136887167594668));
#82690=DIRECTION('ref_axis',(0.895647813564768,0.0107821814158304,0.444633263061331));
#82691=DIRECTION('center_axis',(-0.0772029647371953,-0.987363721887239,
0.138392857246199));
#82692=DIRECTION('ref_axis',(0.895886775400287,-0.00778744934797183,0.444214184032353));
#82693=DIRECTION('',(0.976285002225685,0.,-0.216489247837379));
#82694=DIRECTION('center_axis',(-5.32410291125588E-14,-1.,-2.6302014804238E-14));
#82695=DIRECTION('ref_axis',(1.,-5.32410291125588E-14,3.94046262851656E-31));
#82696=DIRECTION('center_axis',(0.0554976885389505,0.987363722365366,-0.148434788118024));
#82697=DIRECTION('ref_axis',(0.927660483796157,0.00399350089771891,0.373403372713291));
#82698=DIRECTION('center_axis',(-0.0995325946957576,0.98736372090704,0.123313199738447));
#82699=DIRECTION('ref_axis',(0.893891093343772,0.0342871332184858,0.446971034560779));
#82700=DIRECTION('',(-0.216489246715314,0.,-0.976285002474501));
#82701=DIRECTION('center_axis',(0.107402265541574,-0.987363722643892,-0.11652309884024));
#82702=DIRECTION('ref_axis',(0.779125057181291,0.0107821857526969,0.626775789052708));
#82703=DIRECTION('center_axis',(-0.105148378018556,-0.987363721868306,0.118560951996997));
#82704=DIRECTION('ref_axis',(0.779448521139954,-0.0077874521372006,0.626417878482047));
#82705=DIRECTION('',(0.999998790317524,0.,-0.00155543032291784));
#82706=DIRECTION('center_axis',(8.10987235823951E-14,-1.,6.49815876441424E-14));
#82707=DIRECTION('ref_axis',(1.,8.10987235823951E-14,1.85268858048969E-30));
#82708=DIRECTION('center_axis',(0.0861092731979058,0.987363722354393,-0.133034104077886));
#82709=DIRECTION('ref_axis',(0.825701610179814,0.00399350320383623,0.564092991339747));
#82710=DIRECTION('center_axis',(-0.123714279183475,0.987363720576037,0.0990336327535193));
#82711=DIRECTION('ref_axis',(0.776906855088247,0.0342871442005448,0.628681262850628));
#82712=DIRECTION('',(-0.00155543204838868,0.,-0.99999879031484));
#82713=DIRECTION('center_axis',(0.129940280794788,-0.987363722678062,-0.0907105427516035));
#82714=DIRECTION('ref_axis',(0.626171278679668,0.0107821836502577,0.779610976239048));
#82715=DIRECTION('center_axis',(-0.128177166241555,-0.987363721875366,0.0931852712541492));
#82716=DIRECTION('ref_axis',(0.626564120888356,-0.00778745019988622,0.779330968225173));
#82717=DIRECTION('',(0.976953746694739,0.,0.213451111074907));
#82718=DIRECTION('center_axis',(-5.591447997912E-14,-1.,-6.93395850183567E-14));
#82719=DIRECTION('ref_axis',(4.73600965494586E-31,6.93395850183567E-14,
-1.));
#82720=DIRECTION('center_axis',(0.11269449106455,0.987363722439772,-0.11141288656874));
#82721=DIRECTION('ref_axis',(0.685133845045221,0.00399349595334245,0.728406250909218));
#82722=DIRECTION('center_axis',(-0.142111207537177,0.987363720768343,0.0701233741545532));
#82723=DIRECTION('ref_axis',(0.623595318461725,0.0342871373290877,0.780995051845014));
#82724=DIRECTION('',(0.213451112797233,0.,-0.976953746318434));
#82725=DIRECTION('center_axis',(0.146402435956436,-0.987363722636331,-0.0606564585823214));
#82726=DIRECTION('ref_axis',(0.443938426367657,0.0107821865755688,0.895992420753021));
#82727=DIRECTION('center_axis',(-0.145212533291427,-0.987363721887346,0.0634523512239978));
#82728=DIRECTION('ref_axis',(0.44438227874412,-0.00778744832990127,0.895803408112903));
#82729=DIRECTION('',(0.908227431050156,0.,0.418476921093665));
#82730=DIRECTION('center_axis',(6.6168782348743E-15,-1.,1.32897374105932E-14));
#82731=DIRECTION('ref_axis',(-6.49065371568284E-32,-1.32897374105932E-14,
-1.));
#82732=DIRECTION('center_axis',(0.134010233686802,0.987363722422075,-0.0845821311627522));
#82733=DIRECTION('ref_axis',(0.512529985759116,0.00399349595654121,0.858660040812314));
#82734=DIRECTION('center_axis',(-0.153863177968342,0.987363720847149,0.0379342222848389));
#82735=DIRECTION('ref_axis',(0.441125156119624,0.0342871345160342,0.896790381887047));
#82736=DIRECTION('',(0.418476923230167,0.,-0.908227430065737));
#82737=DIRECTION('center_axis',(0.156018974614436,-0.987363722571497,-0.0277661468341567));
#82738=DIRECTION('ref_axis',(0.24094750808905,0.0107821881505182,0.970478254658168));
#82739=DIRECTION('center_axis',(-0.155457924575797,-0.987363721898907,0.0307524692427131));
#82740=DIRECTION('ref_axis',(0.241421615051718,-0.00778744735097303,0.970389076324325));
#82741=DIRECTION('',(0.797033410730777,0.,0.603935213560912));
#82742=DIRECTION('center_axis',(1.08158357943823E-14,-1.,4.32043918942849E-14));
#82743=DIRECTION('ref_axis',(1.05750130502512E-31,-4.32043918942849E-14,
-1.));
#82744=DIRECTION('center_axis',(0.14905980619695,0.987363722366931,-0.053796411871477));
#82745=DIRECTION('ref_axis',(0.315960793488531,0.00399349875883481,0.948763842558179));
#82746=DIRECTION('center_axis',(-0.15842068050042,0.9873637206152,0.00397129735636706));
#82747=DIRECTION('ref_axis',(0.238028470805658,0.0342871433874741,0.970652790076991));
#82748=DIRECTION('',(0.603935214477023,0.,-0.797033410036613));
#82749=DIRECTION('center_axis',(0.158340237993581,-0.987363722683899,0.00642247303839128));
#82750=DIRECTION('ref_axis',(0.0266901526908901,0.0107821833814529,0.999585604273524));
#82751=DIRECTION('center_axis',(-0.158434276660815,-0.987363721875677,-0.00338536597356439));
#82752=DIRECTION('ref_axis',(0.0271723456231515,-0.00778744857226169,0.999600429810867));
#82753=DIRECTION('',(0.648570992291408,0.,0.761154168324748));
#82754=DIRECTION('center_axis',(-2.55060083723739E-15,-1.,-8.90387643367751E-14));
#82755=DIRECTION('ref_axis',(0.0286342148928776,-8.90752890494927E-14,0.999589956801022));
#82756=DIRECTION('center_axis',(0.157139508999401,0.987363722409248,-0.0204952282636888));
#82757=DIRECTION('ref_axis',(0.1046176245841,0.0039934975627731,0.994504502052955));
#82758=DIRECTION('center_axis',(-0.155570604572091,0.987363720558139,-0.0301773146363916));
#82759=DIRECTION('ref_axis',(0.0238018383267625,0.0342871450113978,0.999128552379139));
#82760=DIRECTION('center_axis',(-0.160229038939383,-0.986495109024279,0.0339713843070435));
#82761=DIRECTION('ref_axis',(0.0342169345737296,0.0288443415490679,0.998998100773459));
#82762=DIRECTION('center_axis',(-0.149180144518476,-0.986495109463456,0.0676216199608588));
#82763=DIRECTION('ref_axis',(0.248172015499022,0.0288443005917729,0.968286454024079));
#82764=DIRECTION('center_axis',(-0.131155746156479,-0.986495109479995,0.0981099853337623));
#82765=DIRECTION('ref_axis',(0.450522855937786,0.0288443007497549,0.892298807906813));
#82766=DIRECTION('center_axis',(-0.106998655483312,-0.98649510960293,0.12401083200377));
#82767=DIRECTION('ref_axis',(0.631807747640335,0.0288442944302163,0.774588262692168));
#82768=DIRECTION('center_axis',(-0.077838417858667,-0.986495109440658,0.144113079749635));
#82769=DIRECTION('ref_axis',(0.783550014359944,0.0288443009343881,0.620658828423585));
#82770=DIRECTION('center_axis',(-0.0450385499786022,-0.986495109516865,
0.157476753570594));
#82771=DIRECTION('ref_axis',(0.898654352338061,0.0288442972480577,0.437708077992771));
#82772=DIRECTION('center_axis',(-0.0101327280341518,-0.986495109574413,
0.163476991067101));
#82773=DIRECTION('ref_axis',(0.971738610638713,0.0288442962006352,0.234290587029514));
#82774=DIRECTION('center_axis',(0.0252468906766347,-0.986495109565086,0.161833226858181));
#82775=DIRECTION('ref_axis',(0.999385452589112,0.0288442963429899,0.0199179246341851));
#82776=DIRECTION('center_axis',(0.0594459960109537,-0.986495109493425,0.152622319808805));
#82777=DIRECTION('ref_axis',(0.980302140845566,0.0288442999651713,-0.195386076814905));
#82778=DIRECTION('center_axis',(0.0908654655990513,-0.986495109564504,0.136274964563505));
#82779=DIRECTION('ref_axis',(0.915380991535049,0.0288442965137984,-0.40155403981897));
#82780=DIRECTION('center_axis',(0.118036175066675,-0.986495109414409,0.113555539173929));
#82781=DIRECTION('ref_axis',(0.807657643449368,0.0288443020225124,-0.588945784617437));
#82782=DIRECTION('center_axis',(0.139687636476012,-0.986495109540251,0.0855263881437399));
#82783=DIRECTION('ref_axis',(0.66216912185642,0.0288442980024015,-0.748799078880741));
#82784=DIRECTION('center_axis',(0.15480746285218,-0.986495109521674,0.0534981152480289));
#82785=DIRECTION('ref_axis',(0.485718306482793,0.028844298557354,-0.87363936105708));
#82786=DIRECTION('center_axis',(0.162688663862699,-0.986495109497723,0.0189683311771181));
#82787=DIRECTION('ref_axis',(0.286555844169295,0.0288442979926773,-0.957629236524101));
#82788=DIRECTION('center_axis',(0.162962723698444,-0.986495109521754,-0.0164483912419118));
#82789=DIRECTION('ref_axis',(0.0739943517728547,0.0288442980844734,-0.996841432913846));
#82790=DIRECTION('center_axis',(0.155616827733293,-0.986495109507004,-0.0510960061549885));
#82791=DIRECTION('ref_axis',(-0.14202703735263,0.028844298707668,-0.989442432429951));
#82792=DIRECTION('center_axis',(0.140994460789364,-0.986495109453923,-0.0833544302974347));
#82793=DIRECTION('ref_axis',(-0.351407401293269,0.028844301034906,-0.935778202681661));
#82794=DIRECTION('center_axis',(0.119779354035356,-0.986495109626686,-0.111715285567845));
#82795=DIRECTION('ref_axis',(-0.544356342929197,0.0288442941149483,-0.838358025314818));
#82796=DIRECTION('center_axis',(0.0929634932824821,-0.986495109537122,-0.134852466703655));
#82797=DIRECTION('ref_axis',(-0.711851787185283,0.0288442970362033,-0.70173715849284));
#82798=DIRECTION('center_axis',(0.0618007632488235,-0.986495109509818,-0.151684094667419));
#82799=DIRECTION('ref_axis',(-0.846061833762455,0.0288442983264773,-0.532303841715017));
#82800=DIRECTION('center_axis',(0.0277482946305678,-0.986495109406112,-0.161423143517025));
#82801=DIRECTION('ref_axis',(-0.940710969996221,0.0288443027818726,-0.3379805869067));
#82802=DIRECTION('center_axis',(-0.00760164176617008,-0.986495109582979,
-0.16361422252153));
#82803=DIRECTION('ref_axis',(-0.991373505862717,0.0288442953495626,-0.127853738698767));
#82804=DIRECTION('center_axis',(-0.0425961448445734,-0.986495109496576,
-0.158154884160174));
#82805=DIRECTION('ref_axis',(-0.995680518590945,0.0288442992254162,0.0882514096242231));
#82806=DIRECTION('center_axis',(-0.0755988954940555,-0.986495109515445,
-0.145300398836991));
#82807=DIRECTION('ref_axis',(-0.953430617566002,0.0288442993207796,0.300230018293316));
#82808=DIRECTION('center_axis',(-0.105066729765575,-0.986495109402435,-0.125651826176323));
#82809=DIRECTION('ref_axis',(-0.866599358686841,0.0288443032152825,0.498170209562536));
#82810=DIRECTION('center_axis',(-0.129621749359243,-0.986495109613201,-0.100127922191002));
#82811=DIRECTION('ref_axis',(-0.73924687943124,0.0288442934410548,0.672816511381119));
#82812=DIRECTION('center_axis',(-0.148115811053804,-0.986495109518648,-0.069922138208617));
#82813=DIRECTION('ref_axis',(-0.577328035667357,0.0288442983711295,0.816002662792192));
#82814=DIRECTION('center_axis',(-0.159684137960783,-0.98649510955407,-0.0364468779132737));
#82815=DIRECTION('ref_axis',(-0.38841397670723,0.0288442969363252,0.921033435458629));
#82816=DIRECTION('center_axis',(-0.163785812747736,-0.986495109585999,-0.00126740106956708));
#82817=DIRECTION('ref_axis',(-0.181338109777202,0.0288442964058661,0.982997709309275));
#82818=DIRECTION('center_axis',(0.163550499649484,0.986495109843996,0.00886748658227992));
#82819=DIRECTION('ref_axis',(-0.0789203331419368,0.00412339327425965,0.996872398376378));
#82820=DIRECTION('center_axis',(0.157820545689508,0.986495109373187,0.043818655171623));
#82821=DIRECTION('ref_axis',(-0.291373304723066,0.00412343120499991,0.956600540774391));
#82822=DIRECTION('center_axis',(0.14471107203118,0.986495109447332,0.0767209532532179));
#82823=DIRECTION('ref_axis',(-0.490202001414802,0.00412342961885999,0.871599102303978));
#82824=DIRECTION('center_axis',(0.124835069886123,0.986495109370258,0.106035864286994));
#82825=DIRECTION('ref_axis',(-0.666109393625256,0.00412342810459183,0.745842659724462));
#82826=DIRECTION('center_axis',(0.0991219177812932,0.986495109435623,0.130392654988527));
#82827=DIRECTION('ref_axis',(-0.81087025092018,0.00412342693382052,0.585211443431318));
#82828=DIRECTION('center_axis',(0.0687739385131564,0.986495109397187,0.148652428560119));
#82829=DIRECTION('ref_axis',(-0.917715716882505,0.00412342974764044,0.397216389785147));
#82830=DIRECTION('center_axis',(0.035210162910571,0.986495109405196,0.159961381425146));
#82831=DIRECTION('ref_axis',(-0.981649815310068,0.00412342834487012,0.190647941086164));
#82832=DIRECTION('center_axis',(-2.83305944967152E-9,0.986495109461485,
0.163790717101347));
#82833=DIRECTION('ref_axis',(-0.999683059979575,0.00412342514179896,-0.0248349945635702));
#82834=DIRECTION('center_axis',(-0.035210167842371,0.986495109484084,0.159961379853065));
#82835=DIRECTION('ref_axis',(-0.970972235526654,0.00412342273155899,-0.239156675050788));
#82836=DIRECTION('center_axis',(-0.068773934373553,0.98649510939345,0.1486524305001));
#82837=DIRECTION('ref_axis',(-0.896859828128692,0.00412343157330405,-0.442295654512945));
#82838=DIRECTION('center_axis',(-0.099121918885696,0.986495109403051,0.130392654395409));
#82839=DIRECTION('ref_axis',(-0.780811251037479,0.00412342870837165,-0.624753381414598));
#82840=DIRECTION('center_axis',(-0.124835073263289,0.986495109420972,0.106035859839273));
#82841=DIRECTION('ref_axis',(-0.628252808807675,0.00412342311877974,-0.77799833265056));
#82842=DIRECTION('center_axis',(-0.144711074072459,0.986495109433479,0.0767209495810921));
#82843=DIRECTION('ref_axis',(-0.446317964038295,0.00412342285807861,-0.894864946436413));
#82844=DIRECTION('center_axis',(-0.157820545244122,0.986495109411327,0.0438186559171042));
#82845=DIRECTION('ref_axis',(-0.243513790037603,0.00412342517897462,-0.969888669604051));
#82846=DIRECTION('center_axis',(-0.16355050422689,0.986495109393709,0.00886745225109193));
#82847=DIRECTION('ref_axis',(-0.0293231770748078,0.00412342975117166,-0.999561478155959));
#82848=DIRECTION('center_axis',(-0.161633023231499,0.986495109438459,-0.02649839344278));
#82849=DIRECTION('ref_axis',(0.18623855536835,0.00412342416576182,-0.98249590221408));
#82850=DIRECTION('center_axis',(-0.152157762655465,0.9864951094082,-0.0606251958956625));
#82851=DIRECTION('ref_axis',(0.393091977801218,0.00412342637242704,-0.919489909864854));
#82852=DIRECTION('center_axis',(-0.135567773032974,0.986495109404893,-0.0919172347011641));
#82853=DIRECTION('ref_axis',(0.581564857222371,0.00412342533892671,-0.813489590718528));
#82854=DIRECTION('center_axis',(-0.112638786693034,0.986495109457597,-0.118911323046059));
#82855=DIRECTION('ref_axis',(0.742844406071995,0.00412342655905149,-0.669451406541922));
#82856=DIRECTION('center_axis',(-0.0844429339025283,0.986495109396176,-0.140345253041778));
#82857=DIRECTION('ref_axis',(0.869389381988438,0.00412342564311634,-0.494110412607068));
#82858=DIRECTION('center_axis',(-0.0522986278065988,0.986495109418806,-0.155216792333578));
#82859=DIRECTION('ref_axis',(0.955282674023109,0.00412342940239734,-0.295665368349459));
#82860=DIRECTION('center_axis',(-0.0177088933836277,0.98649510941386,-0.162830568990174));
#82861=DIRECTION('ref_axis',(0.996508010535055,0.00412343038860525,-0.0833953371676001));
#82862=DIRECTION('center_axis',(0.0177088922524152,0.986495109402834,-0.162830569180003));
#82863=DIRECTION('ref_axis',(0.991137739773237,0.00412342739576669,0.132774162184182));
#82864=DIRECTION('center_axis',(0.0522986293653706,0.986495109470237,-0.155216791481493));
#82865=DIRECTION('ref_axis',(0.939422969947577,0.004123425151586,0.342735292755054));
#82866=DIRECTION('center_axis',(0.0844429357467301,0.986495109349537,-0.140345252259984));
#82867=DIRECTION('ref_axis',(0.843781825182108,0.00412342914002899,0.536670503031867));
#82868=DIRECTION('center_axis',(0.112638790080962,0.986495109475539,-0.118911319687998));
#82869=DIRECTION('ref_axis',(0.708686382684141,0.00412342432368572,0.705511593363223));
#82870=DIRECTION('center_axis',(0.135567776406498,0.986495109430993,-0.0919172294454673));
#82871=DIRECTION('ref_axis',(0.540453551221462,0.00412342487770254,0.841363747935094));
#82872=DIRECTION('center_axis',(0.152157764571979,0.98649510943652,-0.0606251906247457));
#82873=DIRECTION('ref_axis',(0.34694970956876,0.00412342481747551,0.937874669877552));
#82874=DIRECTION('center_axis',(0.161633024106174,0.986495109430748,-0.0264983883945512));
#82875=DIRECTION('ref_axis',(0.137222889143665,0.00412342727951331,0.990531612843596));
#82876=DIRECTION('center_axis',(0.156018981440023,0.987363721870147,-0.0277661334209345));
#82877=DIRECTION('ref_axis',(0.106060021918456,0.0112019472137412,0.9942966298491));
#82878=DIRECTION('',(-0.603694433998265,0.,0.797215799115594));
#82879=DIRECTION('',(-0.797215799077898,0.,-0.603694434048045));
#82880=DIRECTION('center_axis',(1.08288855678234E-14,-1.,4.32011223528413E-14));
#82881=DIRECTION('ref_axis',(7.04722324508856E-32,-4.32011223528413E-14,
-1.));
#82882=DIRECTION('center_axis',(-0.15386314984286,-0.98736372225306,0.0379342997696712));
#82883=DIRECTION('ref_axis',(0.171011654648654,0.0112022366990284,0.985205320665326));
#82884=DIRECTION('center_axis',(0.157139511605135,-0.987363722043811,-0.0204952258902551));
#82885=DIRECTION('ref_axis',(0.239893891223624,0.0180313431330044,0.970631645691819));
#82886=DIRECTION('center_axis',(0.146402446990452,0.987363721922409,-0.0606564435714413));
#82887=DIRECTION('ref_axis',(0.317324780468734,0.0112019451391554,0.948250758041126));
#82888=DIRECTION('',(-0.418202564699196,0.,0.908353793892564));
#82889=DIRECTION('',(-0.908353794958524,0.,-0.418202562383886));
#82890=DIRECTION('center_axis',(6.62089218032808E-15,-1.,1.32877379472513E-14));
#82891=DIRECTION('ref_axis',(-7.81841420998606E-32,-1.32877379472513E-14,
-1.));
#82892=DIRECTION('center_axis',(-0.142111161632101,-0.98736372224877,0.07012344634021));
#82893=DIRECTION('ref_axis',(0.378803518223432,0.0112022371766569,0.925409317255769));
#82894=DIRECTION('center_axis',(0.149059807495583,-0.987363722127591,-0.0537964126659872));
#82895=DIRECTION('ref_axis',(0.442942417495199,0.0180313388269867,0.89636872190166));
#82896=DIRECTION('center_axis',(0.129940297717711,0.987363721920756,-0.0907105267531021));
#82897=DIRECTION('ref_axis',(0.513751786447825,0.0112019434459527,0.85786573447405));
#82898=DIRECTION('',(-0.213156003970963,0.,0.977018176888808));
#82899=DIRECTION('',(-0.977018176875493,0.,-0.213156004031993));
#82900=DIRECTION('center_axis',(-1.86451405470691E-14,-1.,-2.3107563814193E-14));
#82901=DIRECTION('ref_axis',(-4.11731915750795E-31,2.3107563814193E-14,
-1.));
#82902=DIRECTION('center_axis',(-0.123714212024382,-0.987363722232937,0.0990337001303415));
#82903=DIRECTION('ref_axis',(0.568882952848608,0.0112022393150633,0.822342201150213));
#82904=DIRECTION('center_axis',(0.134010238811121,-0.987363721952807,-0.0845821285218517));
#82905=DIRECTION('ref_axis',(0.625279446823254,0.0180313468374548,0.780192594114833));
#82906=DIRECTION('center_axis',(0.107402283594654,0.987363721950959,-0.116523088071864));
#82907=DIRECTION('ref_axis',(0.686156328941859,0.0112019438535314,0.727367863399898));
#82908=DIRECTION('',(0.00185749160357402,0.,0.999998274860983));
#82909=DIRECTION('',(-0.999998274855759,0.,0.00185749441591979));
#82910=DIRECTION('center_axis',(4.63533414192115E-14,-1.,3.71183355223613E-14));
#82911=DIRECTION('ref_axis',(1.,4.63533414192115E-14,8.01737682443457E-31));
#82912=DIRECTION('center_axis',(-0.0995325279449254,-0.987363722252009,
0.123313242847437));
#82913=DIRECTION('ref_axis',(0.732362049748505,0.0112022347792573,0.680823279584444));
#82914=DIRECTION('center_axis',(0.112694492230308,-0.987363722076729,-0.111412888606934));
#82915=DIRECTION('ref_axis',(0.778379106755819,0.0180313415424152,0.627535526395275));
#82916=DIRECTION('center_axis',(0.0798422598236929,0.987363721944083,-0.136887158400539));
#82917=DIRECTION('ref_axis',(0.82647696532404,0.0112019420910649,0.562859078528679));
#82918=DIRECTION('',(0.216784133438348,0.,0.976219565205177));
#82919=DIRECTION('',(-0.976219564475212,0.,0.216784136725517));
#82920=DIRECTION('center_axis',(3.99367281940478E-14,-1.,1.97144484204352E-14));
#82921=DIRECTION('ref_axis',(1.,3.99367281940478E-14,3.89081776988677E-31));
#82922=DIRECTION('center_axis',(-0.0706968106498305,-0.987363722284355,
0.141826798880623));
#82923=DIRECTION('ref_axis',(0.8615967118823,0.0112022347444393,0.507469817831898));
#82924=DIRECTION('center_axis',(0.0861092826808786,-0.987363721992386,-0.133034100626598));
#82925=DIRECTION('ref_axis',(0.895082624554255,0.0180313447346119,0.445535594344748));
#82926=DIRECTION('center_axis',(0.0485488928772202,0.987363721828466,-0.150850541322981));
#82927=DIRECTION('ref_axis',(0.928152457786751,0.0112019490099345,0.372031626938884));
#82928=DIRECTION('',(0.421574190582567,0.,0.906793913651086));
#82929=DIRECTION('',(-0.906793913166479,0.,0.421574191624944));
#82930=DIRECTION('center_axis',(-1.29723160072588E-13,-1.,-3.20049586081121E-14));
#82931=DIRECTION('ref_axis',(1.,-1.29723160072588E-13,-7.57499294018975E-31));
#82932=DIRECTION('center_axis',(-0.0385553889118671,-0.987363722263305,
0.153708691830376));
#82933=DIRECTION('ref_axis',(0.950544069762331,0.0112022349597061,0.310387630828893));
#82934=DIRECTION('center_axis',(0.0554976904691863,-0.987363722124819,-0.14843478899641));
#82935=DIRECTION('ref_axis',(0.96993307281497,0.0180313384327736,0.242702915297762));
#82936=DIRECTION('center_axis',(0.01498544227234,0.987363721863414,-0.157760315884345));
#82937=DIRECTION('ref_axis',(0.986428571397858,0.0112019464713099,0.163808393940099));
#82938=DIRECTION('',(0.606651908563567,0.,0.79496758539967));
#82939=DIRECTION('',(-0.794967585437568,0.,0.606651908513905));
#82940=DIRECTION('',(0.763363255463762,0.,0.645969457643136));
#82941=DIRECTION('',(-0.645969457690815,0.,0.763363255423415));
#82942=DIRECTION('center_axis',(2.91493521777504E-14,-1.,-5.64942831183301E-15));
#82943=DIRECTION('ref_axis',(1.,2.91493521777504E-14,3.3884035720465E-32));
#82944=DIRECTION('center_axis',(0.0295486797280843,-0.987363722245854,0.155691218503611));
#82945=DIRECTION('ref_axis',(0.993018816372276,0.0112022332241641,-0.117422912165366));
#82946=DIRECTION('center_axis',(-0.0119578129886334,-0.987363722205775,
-0.158018640610806));
#82947=DIRECTION('ref_axis',(0.982195724128258,0.0180313362869311,-0.186993129327992));
#82948=DIRECTION('center_axis',(-0.0526414173739263,0.9873637218959,-0.149471608878542));
#82949=DIRECTION('ref_axis',(0.964039683787994,0.0112019454545849,-0.265522135612039));
#82950=DIRECTION('',(0.884380585166769,0.,0.466766516129941));
#82951=DIRECTION('',(-0.466766516185183,0.,0.884380585137614));
#82952=DIRECTION('center_axis',(4.08800946220324E-14,-1.,-1.76753953208713E-14));
#82953=DIRECTION('ref_axis',(1.,4.08800946220324E-14,-2.74904565889751E-32));
#82954=DIRECTION('center_axis',(0.0623268615422876,-0.987363722252581,0.145699149996891));
#82955=DIRECTION('ref_axis',(0.944560133027489,0.0112022373139612,-0.328147322058637));
#82956=DIRECTION('center_axis',(-0.0456475758122678,-0.987363722013895,
-0.151753679603923));
#82957=DIRECTION('ref_axis',(0.919034539789773,0.0180313434872257,-0.393764377928535));
#82958=DIRECTION('center_axis',(-0.0835426679191584,0.987363721926463,-0.134660696791869));
#82959=DIRECTION('ref_axis',(0.884421561891373,0.0112019458379472,-0.466554409764892));
#82960=DIRECTION('',(0.964045262617061,0.,0.265738088398336));
#82961=DIRECTION('',(-0.265738088458527,0.,0.964045262600469));
#82962=DIRECTION('center_axis',(0.,-1.,0.));
#82963=DIRECTION('ref_axis',(0.,0.,-1.));
#82964=DIRECTION('center_axis',(0.0921907025317405,-0.987363722255318,0.128894353409397));
#82965=DIRECTION('ref_axis',(0.851934869173167,0.011202235227345,-0.523527925341916));
#82966=DIRECTION('center_axis',(-0.0772029162694352,-0.987363722049419,
-0.138392883127032));
#82967=DIRECTION('ref_axis',(0.812900319838701,0.0180313436171572,-0.582123647220672));
#82968=DIRECTION('center_axis',(-0.110537555212464,0.987363721935053,-0.11355320116232));
#82969=DIRECTION('ref_axis',(0.763448870616057,0.0112019447737031,-0.645771119196542));
#82970=DIRECTION('',(0.99863225400483,0.,0.0522840440405398));
#82971=DIRECTION('',(-0.0522840469698092,0.,0.998632253851466));
#82972=DIRECTION('center_axis',(9.89335438420199E-15,-1.,-1.10689535019281E-14));
#82973=DIRECTION('ref_axis',(-2.42855845865753E-31,1.10689535019281E-14,
-1.));
#82974=DIRECTION('center_axis',(0.117743810847805,-0.987363722264918,0.106062599261951));
#82975=DIRECTION('ref_axis',(0.719474076791775,0.0112022350142792,-0.694428947233126));
#82976=DIRECTION('center_axis',(-0.105148334451143,-0.987363722064409,-0.118560989002571));
#82977=DIRECTION('ref_axis',(0.668755786226334,0.0180313427373918,-0.743263458719641));
#82978=DIRECTION('center_axis',(-0.132363832466933,0.987363721862616,-0.087136080955418));
#82979=DIRECTION('ref_axis',(0.606778157678717,0.0112019480430204,-0.79479228967326));
#82980=DIRECTION('',(0.986524311201882,0.,-0.163614740801838));
#82981=DIRECTION('',(0.163614740740217,0.,0.986524311212102));
#82982=DIRECTION('center_axis',(0.,-1.,0.));
#82983=DIRECTION('ref_axis',(0.,0.,-1.));
#82984=DIRECTION('center_axis',(0.137791350328405,-0.987363722237725,0.0782714749033058));
#82985=DIRECTION('ref_axis',(0.553371476054598,0.0112022361144345,-0.83285924344705));
#82986=DIRECTION('center_axis',(-0.128177133113773,-0.98736372207118,-0.0931853147468999));
#82987=DIRECTION('ref_axis',(0.493340974292365,0.0180313422430586,-0.869649098074145));
#82988=DIRECTION('center_axis',(-0.148000920166892,0.987363721894028,-0.0566445788873566));
#82989=DIRECTION('ref_axis',(0.421735172486176,0.0112019452194524,-0.906649855628597));
#82990=DIRECTION('',(0.928287587778145,0.,-0.371863085526155));
#82991=DIRECTION('',(0.371863084475821,0.,0.928287588198899));
#82992=DIRECTION('center_axis',(-8.66246462963213E-15,-1.,2.84000436035281E-14));
#82993=DIRECTION('ref_axis',(-7.27882073886525E-32,-2.84000436035281E-14,
-1.));
#82994=DIRECTION('center_axis',(0.151395919729731,-0.987363722225806,0.0468204605016794));
#82995=DIRECTION('ref_axis',(0.361393837408662,0.0112022394380031,-0.932345968036874));
#82996=DIRECTION('center_axis',(-0.145212510328798,-0.987363722018919,-0.0634524017272397));
#82997=DIRECTION('ref_axis',(0.294858087543414,0.0180313448874745,-0.955370911642065));
#82998=DIRECTION('center_axis',(-0.156717651463886,0.987363721882632,-0.0235044342565438));
#82999=DIRECTION('ref_axis',(0.216972319801143,0.0112019481712355,-0.976113481515997));
#83000=DIRECTION('',(0.826645169515348,0.,-0.56272352333712));
#83001=DIRECTION('',(0.56272352328549,0.,0.826645169550494));
#83002=DIRECTION('center_axis',(-2.35477114699405E-15,-1.,2.95982401992128E-14));
#83003=DIRECTION('ref_axis',(1.8148513515194E-32,-2.95982401992128E-14,
-1.));
#83004=DIRECTION('center_axis',(0.157921382460364,-0.987363722227189,0.0131801741823417));
#83005=DIRECTION('ref_axis',(0.15251782909657,0.0112022422485203,-0.988237229402068));
#83006=DIRECTION('center_axis',(-0.155457913607194,-0.987363722140868,-0.0307525169218483));
#83007=DIRECTION('ref_axis',(0.0825879624401618,0.0180313393924332,-0.99642064373421));
#83008=DIRECTION('center_axis',(-0.158106438295245,0.987363721977051,0.0107347423451855));
#83009=DIRECTION('ref_axis',(0.00206408220887537,0.0112019414720079,-0.999935125931624));
#83010=DIRECTION('',(0.686349742131425,0.,-0.727271635275381));
#83011=DIRECTION('',(0.727271635232524,0.,0.686349742176837));
#83012=DIRECTION('center_axis',(-4.06302881637799E-15,-1.,-2.94124559535081E-14));
#83013=DIRECTION('ref_axis',(-8.13378641990255E-32,2.94124559535081E-14,
-1.));
#83014=DIRECTION('center_axis',(0.157062616396446,-0.987363722260598,-0.021076396618003));
#83015=DIRECTION('ref_axis',(-0.0634897471633578,0.0112022384316609,-0.997919616932773));
#83016=DIRECTION('center_axis',(-0.158434276437026,-0.987363722091255,0.00338531357163764));
#83017=DIRECTION('ref_axis',(-0.1335438816567,0.0180313416766307,-0.990878853538313));
#83018=DIRECTION('center_axis',(-0.152102345193246,0.98736372197672,0.0444719811903379));
#83019=DIRECTION('ref_axis',(-0.212940667766901,0.0112019422303222,-0.977000915302158));
#83020=DIRECTION('',(0.513961362392701,0.,-0.857813335153656));
#83021=DIRECTION('',(0.857813335121557,0.,0.513961362446274));
#83022=DIRECTION('center_axis',(-1.54362691251806E-14,-1.,-4.17770670576077E-14));
#83023=DIRECTION('ref_axis',(4.33070742457523E-31,4.17770670576077E-14,
-1.));
#83024=DIRECTION('center_axis',(0.148859778356902,-0.987363722268594,-0.0543474593282965));
#83025=DIRECTION('ref_axis',(-0.276528610540624,0.0112022357729868,-0.960940392254462));
#83026=DIRECTION('center_axis',(-0.154002428756523,-0.987363722073559,0.0373648534071712));
#83027=DIRECTION('ref_axis',(-0.343431362720795,0.0180313411743159,-0.939004669762186));
#83028=DIRECTION('center_axis',(-0.13898611326727,0.987363721839146,0.0761297649727565));
#83029=DIRECTION('ref_axis',(-0.417988550412985,0.0112019485432832,-0.908383227538072));
#83030=DIRECTION('',(0.317540722300475,0.,-0.948244635988463));
#83031=DIRECTION('',(0.948244636544387,0.,0.317540720640366));
#83032=DIRECTION('center_axis',(4.00936870292431E-14,-1.,6.24700014331448E-14));
#83033=DIRECTION('ref_axis',(8.00121565978192E-31,-6.24700014331447E-14,
-1.));
#83034=DIRECTION('center_axis',(0.13369642348063,-0.987363722268957,-0.0850772960059203));
#83035=DIRECTION('ref_axis',(-0.476637303526556,0.011202233537974,-0.879028663270257));
#83036=DIRECTION('center_axis',(-0.142369599811224,-0.987363722034396,0.0695972518133825));
#83037=DIRECTION('ref_axis',(-0.53726037401082,0.0180313432663028,-0.84322367209286));
#83038=DIRECTION('center_axis',(-0.119371046962671,0.987363721897949,0.104227797764633));
#83039=DIRECTION('ref_axis',(-0.603491752064952,0.0112019468735407,-0.797290550286291));
#83040=DIRECTION('',(0.106272228164614,0.,-0.994337072385883));
#83041=DIRECTION('',(0.994337072346781,0.,0.10627222853047));
#83042=DIRECTION('center_axis',(-3.15513135201966E-14,-1.,-3.14343179307583E-14));
#83043=DIRECTION('ref_axis',(1.,-3.15513135201966E-14,6.49236310791174E-31));
#83044=DIRECTION('center_axis',(0.11228156876534,-0.987363722283361,-0.111829017854669));
#83045=DIRECTION('ref_axis',(-0.654458968400117,0.0112022372151143,-0.756014529332626));
#83046=DIRECTION('center_axis',(-0.12407972666712,-0.987363722011638,0.0985753614527323));
#83047=DIRECTION('ref_axis',(-0.705967689967984,0.0180313446855486,-0.708014471130428));
#83048=DIRECTION('center_axis',(-0.0941743240009238,0.98736372194084,0.127452254958871));
#83049=DIRECTION('ref_axis',(-0.760776350944052,0.0112019449395735,-0.648917452588404));
#83050=DIRECTION('',(-0.109965437515888,0.,-0.993935411660103));
#83051=DIRECTION('',(0.993935411981186,0.,-0.109965434613747));
#83052=DIRECTION('center_axis',(-5.00948140137855E-14,-1.,-3.18890683862576E-14));
#83053=DIRECTION('ref_axis',(1.,-5.00948140137855E-14,-6.10027479870061E-31));
#83054=DIRECTION('center_axis',(0.0856165536929381,-0.987363722249842,-0.133351736841637));
#83055=DIRECTION('ref_axis',(-0.801678856600124,0.0112022390584335,-0.597649998511165));
#83056=DIRECTION('center_axis',(-0.0999880255357913,-0.987363721948436,
0.122944195997963));
#83057=DIRECTION('ref_axis',(-0.841664740409905,0.0180313480723561,-0.539699300756838));
#83058=DIRECTION('center_axis',(-0.0645741169833012,0.987363722015683,0.144717185790647));
#83059=DIRECTION('ref_axis',(-0.882487893320251,0.0112019405356229,-0.470201695734311));
#83060=DIRECTION('',(-0.321061238918488,0.,-0.947058435823326));
#83061=DIRECTION('',(0.947058436717493,0.,-0.321061236280897));
#83062=DIRECTION('center_axis',(5.57788322286723E-14,-1.,2.03746154926628E-14));
#83063=DIRECTION('ref_axis',(1.,5.57788322286723E-14,4.3682323794354E-31));
#83064=DIRECTION('center_axis',(0.0549482066282451,-0.987363722243805,-0.148639074893508));
#83065=DIRECTION('ref_axis',(-0.911413133585882,0.0112022370251814,-0.411340017276212));
#83066=DIRECTION('center_axis',(-0.0712209830205846,-0.987363722192365,
0.141564302265861));
#83067=DIRECTION('ref_axis',(-0.938006483548204,0.0180313375612654,-0.346148389693329));
#83068=DIRECTION('center_axis',(-0.0319544928820863,0.987363721983359,0.155215304966415));
#83069=DIRECTION('ref_axis',(-0.962935282094827,0.0112019407089108,-0.269499831208312));
#83070=DIRECTION('',(-0.517144572474315,0.,-0.855898061196751));
#83071=DIRECTION('',(0.855898060460217,0.,-0.517144573693314));
#83072=DIRECTION('center_axis',(-5.88546942245058E-14,-1.,-7.90746818996684E-15));
#83073=DIRECTION('ref_axis',(1.,-5.88546942245058E-14,8.10968348491405E-32));
#83074=DIRECTION('center_axis',(0.0217105382537213,-0.987363722231665,-0.156976216509269));
#83075=DIRECTION('ref_axis',(-0.978530745503069,0.011202239615509,-0.20579623401026));
#83076=DIRECTION('center_axis',(-0.0391237393982408,-0.987363722089536,
0.153565013323332));
#83077=DIRECTION('ref_axis',(-0.990488084645076,0.0180313411108617,-0.136411967634343));
#83078=DIRECTION('center_axis',(0.00215929493914566,0.987363721875552,0.158455729367619));
#83079=DIRECTION('ref_axis',(-0.99835688760782,0.0112019478522475,-0.0561964530049911));
#83080=DIRECTION('',(-0.68904680421877,0.,-0.724716842357));
#83081=DIRECTION('',(0.724716840964441,0.,-0.689046805683417));
#83082=DIRECTION('center_axis',(0.0361720501024856,0.987363723226731,0.15428694321695));
#83083=DIRECTION('ref_axis',(-0.987096432090511,0.0112018841470787,0.159734628511599));
#83084=DIRECTION('',(-0.828729971245926,0.,-0.559648670827267));
#83085=DIRECTION('center_axis',(1.03562508173011E-13,-1.,-8.62649121691859E-15));
#83086=DIRECTION('ref_axis',(1.,1.03562508173011E-13,-4.16955228716423E-33));
#83087=DIRECTION('center_axis',(-0.0125422848473503,-0.987363722246317,
-0.157973323959163));
#83088=DIRECTION('ref_axis',(-0.999893347505735,0.0112022358467117,0.00937035355842204));
#83089=DIRECTION('center_axis',(-0.00519715123370011,-0.987363721335481,
0.158385199465116));
#83090=DIRECTION('ref_axis',(-0.996655564095281,0.0180313824950653,0.0797029221750023));
#83091=DIRECTION('',(0.559648669545658,0.,-0.828729972111408));
#83092=DIRECTION('center_axis',(2.8367666732571E-14,-1.,-8.76791045131834E-15));
#83093=DIRECTION('ref_axis',(1.,2.8367666732571E-14,-2.10203266835669E-31));
#83094=DIRECTION('center_axis',(0.0684935539383942,0.987363721923308,0.142903861734529));
#83095=DIRECTION('ref_axis',(-0.929680449617988,0.0112019447854592,0.368196656735391));
#83096=DIRECTION('center_axis',(-0.0462086544756258,-0.987363722215038,
-0.151583773225295));
#83097=DIRECTION('ref_axis',(-0.974502047462563,0.0112022423458931,0.224098793521289));
#83098=DIRECTION('center_axis',(0.0289725294676274,-0.987363722077757,0.155799463609492));
#83099=DIRECTION('ref_axis',(-0.956220537480874,0.0180313430440089,0.292091003572205));
#83100=DIRECTION('',(-0.929662646609954,0.,-0.368411948093674));
#83101=DIRECTION('',(0.368411947167104,0.,-0.92966264697714));
#83102=DIRECTION('center_axis',(3.87294073425063E-14,-1.,-2.19916970885083E-14));
#83103=DIRECTION('ref_axis',(1.,3.87294073425063E-14,-2.80400463742889E-31));
#83104=DIRECTION('center_axis',(-0.0777143454502976,-0.987363722242736,
-0.138106337690207));
#83105=DIRECTION('ref_axis',(-0.903544115145585,0.0112022346100321,0.428348621948903));
#83106=DIRECTION('center_axis',(0.0617874476101675,-0.987363722074356,0.145928721125403));
#83107=DIRECTION('ref_axis',(-0.87107370117854,0.0180313424742626,0.490821227947299));
#83108=DIRECTION('center_axis',(0.0976123131343119,0.987363722050419,0.124838762823539));
#83109=DIRECTION('ref_axis',(-0.828793639509073,0.0112019379749413,0.559442239820082));
#83110=DIRECTION('',(-0.987125329195886,0.,-0.159948693211022));
#83111=DIRECTION('',(0.159948692818607,0.,-0.987125329259471));
#83112=DIRECTION('center_axis',(-3.30963705214028E-14,-1.,2.9803221179575E-14));
#83113=DIRECTION('ref_axis',(1.,-3.30963705214028E-14,6.25159702479296E-31));
#83114=DIRECTION('center_axis',(-0.105586206869686,-0.987363722259735,-0.118171201585976));
#83115=DIRECTION('ref_axis',(-0.790337464271335,0.0112022339772626,0.612569345072927));
#83116=DIRECTION('center_axis',(0.0917132492516903,-0.987363721931314,0.129234517547133));
#83117=DIRECTION('ref_axis',(-0.745196427498504,0.0180313474279287,0.66660119633361));
#83118=DIRECTION('center_axis',(0.122166840284463,0.987363721930211,0.100936335137705));
#83119=DIRECTION('ref_axis',(-0.689153359040235,0.0112019447743796,0.724528925686775));
#83120=DIRECTION('',(-0.998431128681538,0.,0.0559935824868428));
#83121=DIRECTION('',(-0.0559935851300269,0.,-0.998431128533304));
#83122=DIRECTION('center_axis',(3.45543789430862E-14,-1.,-4.82949063880597E-14));
#83123=DIRECTION('ref_axis',(-4.06692601993503E-31,4.82949063880597E-14,
-1.));
#83124=DIRECTION('center_axis',(-0.128520974782549,-0.987363722243347,-0.0927105120183547));
#83125=DIRECTION('ref_axis',(-0.640175512069977,0.0112022330864055,0.768147006581306));
#83126=DIRECTION('center_axis',(0.117350647805832,-0.98736372204255,0.10649744529252));
#83127=DIRECTION('ref_axis',(-0.584474595140577,0.0180313435221755,0.811211635940981));
#83128=DIRECTION('center_axis',(0.141008974823679,0.987363721952356,0.0723142419691046));
#83129=DIRECTION('ref_axis',(-0.517289037097874,0.0112019432813125,0.85573744137152));
#83130=DIRECTION('',(-0.963051398102499,0.,0.269317664873326));
#83131=DIRECTION('',(-0.269317664813245,0.,-0.963051398119301));
#83132=DIRECTION('center_axis',(2.92056743225914E-14,-1.,-6.82424603926603E-14));
#83133=DIRECTION('ref_axis',(-2.92163954713156E-31,6.82424603926603E-14,
-1.));
#83134=DIRECTION('center_axis',(-0.145446246385829,-0.987363722270873,-0.062914778515692));
#83135=DIRECTION('ref_axis',(-0.460079663912597,0.0112022359509466,0.887806968188339));
#83136=DIRECTION('center_axis',(0.137500857423055,-0.98736372201278,0.0787806744131776));
#83137=DIRECTION('ref_axis',(-0.396423382729331,0.0180313439371385,0.917890719127966));
#83138=DIRECTION('center_axis',(0.153257689760006,0.987363721863816,0.0403108084346932));
#83139=DIRECTION('ref_axis',(-0.321236848885251,0.0112019484669408,0.946932628685282));
#83140=DIRECTION('',(-0.882640455447384,0.,0.470048748969333));
#83141=DIRECTION('',(-0.470048751153994,0.,-0.882640454283946));
#83142=DIRECTION('center_axis',(2.77055002754196E-15,-1.,-1.45850692541728E-14));
#83143=DIRECTION('ref_axis',(-3.71033610358611E-32,1.45850692541728E-14,
-1.));
#83144=DIRECTION('center_axis',(-0.155570611822742,-0.987363722257185,-0.0301772216669084));
#83145=DIRECTION('ref_axis',(-0.258471001547092,0.0112022365512323,0.965954062704585));
#83146=DIRECTION('center_axis',(0.151221680424715,-0.987363722063087,0.0473802039173925));
#83147=DIRECTION('ref_axis',(-0.189835852008218,0.0180313416813938,0.981650253404685));
#83148=DIRECTION('center_axis',(0.158340241637008,0.987363721953189,0.00642249554924032));
#83149=DIRECTION('ref_axis',(-0.110163989544152,0.0112019445036678,0.993850296496939));
#83150=DIRECTION('',(-0.760958224664093,8.72727899869762E-15,0.648800878787993));
#83151=DIRECTION('center_axis',(-3.00707855217943E-15,-1.,-1.03877653669684E-13));
#83152=DIRECTION('ref_axis',(0.0289361497150056,-1.0392116941864E-13,0.999581261949058));
#83153=DIRECTION('center_axis',(-0.158420668070115,-0.987363722255939,0.0039713852891132));
#83154=DIRECTION('ref_axis',(-0.0447765240641304,0.0112022340570488,0.998934218477306));
#83155=DIRECTION('center_axis',(0.157871544748071,-0.987363722095171,0.0137642889111219));
#83156=DIRECTION('ref_axis',(0.0256281921958917,0.0180313407672832,0.999508912674071));
#83157=DIRECTION('',(-0.64880087707579,0.,-0.760958226123935));
#83158=DIRECTION('center_axis',(-0.15843427510874,-0.987363722233975,-0.00338533411013414));
#83159=DIRECTION('ref_axis',(-0.150493176847073,0.0207595602057009,0.98839306168272));
#83160=DIRECTION('',(0.563147788029111,0.,0.826356199733456));
#83161=DIRECTION('',(0.826356198741165,0.,-0.563147789485187));
#83162=DIRECTION('center_axis',(-0.154002421975287,-0.987363722280647,-0.0373648758843351));
#83163=DIRECTION('ref_axis',(-0.359450020738448,0.0207595567062281,0.932933397084963));
#83164=DIRECTION('',(0.372339549379017,0.,0.928096579009012));
#83165=DIRECTION('center_axis',(-4.32394255814854E-15,-1.,1.42022434872714E-14));
#83166=DIRECTION('ref_axis',(9.72412122363789E-32,-1.42022434872714E-14,
-1.));
#83167=DIRECTION('center_axis',(0.157871536511912,0.98736372308643,0.0137643122702139));
#83168=DIRECTION('ref_axis',(-0.214962170603115,0.0207592293548863,0.976401720403128));
#83169=DIRECTION('center_axis',(-0.156018989066482,0.987363721752651,-0.0277660947457013));
#83170=DIRECTION('ref_axis',(-0.288435909505167,-0.0186562580954878,0.957317434366366));
#83171=DIRECTION('',(0.92809657835293,0.,-0.372339551014372));
#83172=DIRECTION('center_axis',(-0.142369586171416,-0.987363722340502,-0.0695972753725918));
#83173=DIRECTION('ref_axis',(-0.551599383034971,0.0207595554529733,0.833850802897517));
#83174=DIRECTION('',(0.164121129029902,0.,0.986440193324436));
#83175=DIRECTION('center_axis',(-1.45518274130907E-14,-1.,2.58813661411197E-14));
#83176=DIRECTION('ref_axis',(3.468830684141E-31,-2.58813661411197E-14,-1.));
#83177=DIRECTION('center_axis',(0.151221665785298,0.98736372318903,0.0473802271777533));
#83178=DIRECTION('ref_axis',(-0.41983398324885,0.0207592259088541,0.907363477912281));
#83179=DIRECTION('center_axis',(-0.146402463399386,0.987363721717716,-0.0606564072982545));
#83180=DIRECTION('ref_axis',(-0.487487389798135,-0.0186562610013775,0.872930689524231));
#83181=DIRECTION('',(0.986440193500669,0.,-0.164121127970665));
#83182=DIRECTION('center_axis',(-0.124079706088548,-0.987363722361159,-0.0985753838546666));
#83183=DIRECTION('ref_axis',(-0.717956569952352,0.0207595533658661,0.695778272588548));
#83184=DIRECTION('',(-0.0517714178151324,0.,0.998658960955846));
#83185=DIRECTION('center_axis',(-2.96630136708453E-14,-1.,3.32220921542847E-14));
#83186=DIRECTION('ref_axis',(7.94211428211299E-31,-3.32220921542847E-14,
-1.));
#83187=DIRECTION('center_axis',(0.137500844342313,0.987363722957583,0.0787806854025349));
#83188=DIRECTION('ref_axis',(-0.60507482268427,0.020759234097064,0.795897928853507));
#83189=DIRECTION('center_axis',(-0.12994032206456,0.987363721679227,-0.0907104945058956));
#83190=DIRECTION('ref_axis',(-0.66374449884885,-0.0186562630185771,0.747726677401623));
#83191=DIRECTION('',(0.998658961195707,0.,0.0517714131882863));
#83192=DIRECTION('center_axis',(-0.0999879970011825,-0.987363722364416,
-0.122944215863846));
#83193=DIRECTION('ref_axis',(-0.850742905726827,0.0207595522304107,0.525171923608515));
#83194=DIRECTION('',(-0.265243185223135,0.,0.964181545505143));
#83195=DIRECTION('center_axis',(9.62967379208464E-14,-1.,-6.95165520896173E-14));
#83196=DIRECTION('ref_axis',(1.,9.62967379208465E-14,1.36148196072087E-30));
#83197=DIRECTION('center_axis',(0.117350631393154,0.987363722976472,0.106497454719203));
#83198=DIRECTION('ref_axis',(-0.762023036778937,0.0207592324872928,0.647217077714073));
#83199=DIRECTION('center_axis',(-0.107402310027922,0.987363721799827,-0.116523064988271));
#83200=DIRECTION('ref_axis',(-0.808965654938278,-0.0186562575082339,0.587559795413258));
#83201=DIRECTION('',(0.964181545972515,0.,0.265243183524199));
#83202=DIRECTION('center_axis',(-0.0712209641401703,-0.987363722346009,
-0.141564310692975));
#83203=DIRECTION('ref_axis',(-0.943749448360311,0.0207595554677546,0.330009120444254));
#83204=DIRECTION('',(-0.466312478831761,0.,0.884620072169843));
#83205=DIRECTION('center_axis',(-1.08989377379274E-13,-1.,4.71903415295343E-14));
#83206=DIRECTION('ref_axis',(1.,-1.08989377379274E-13,-4.28536810502175E-31));
#83207=DIRECTION('center_axis',(0.0917132337655013,0.987363722983199,0.129234520500645));
#83208=DIRECTION('ref_axis',(-0.883339902800466,0.0207592324290681,0.468273072458175));
#83209=DIRECTION('center_axis',(-0.0798422878900739,0.98736372183659,-0.136887142805579));
#83210=DIRECTION('ref_axis',(-0.916360475668615,-0.0186562562932369,0.399919270270277));
#83211=DIRECTION('',(0.8846200741774,0.,0.466312475023317));
#83212=DIRECTION('center_axis',(-0.0391237163265227,-0.987363722297884,
-0.153565017861715));
#83213=DIRECTION('ref_axis',(-0.992627316897588,0.0207595568304632,0.119415453559823));
#83214=DIRECTION('',(-0.645577518758643,0.,0.763694747443921));
#83215=DIRECTION('center_axis',(-4.3719673062391E-14,-1.,8.49658617979204E-15));
#83216=DIRECTION('ref_axis',(1.,-4.3719673062391E-14,3.94366309046456E-32));
#83217=DIRECTION('center_axis',(0.0617874283049422,0.987363722959405,0.145928723311089));
#83218=DIRECTION('ref_axis',(-0.963352775381175,0.0207592332646177,0.267433140054953));
#83219=DIRECTION('center_axis',(-0.0485489300449553,0.987363721841696,-0.150850529274524));
#83220=DIRECTION('ref_axis',(-0.980907298568706,-0.018656256121526,0.193578965081882));
#83221=DIRECTION('',(0.763694749779609,0.,0.645577515995608));
#83222=DIRECTION('center_axis',(-0.00519708773014777,-0.987363722309297,
-0.158385195478159));
#83223=DIRECTION('ref_axis',(-0.995091034656455,0.0207595581066054,-0.0967619423821432));
#83224=DIRECTION('',(-0.794656070501521,0.,0.607059906117248));
#83225=DIRECTION('center_axis',(2.96826975295269E-14,-1.,7.33664433365271E-16));
#83226=DIRECTION('ref_axis',(-0.999694677174641,-2.9691763102419E-14,-0.0247093591315182));
#83227=DIRECTION('center_axis',(0.028972516634715,0.987363722781084,0.155799461538642));
#83228=DIRECTION('ref_axis',(-0.998320342515947,0.0207592391582244,0.0540883324610285));
#83229=DIRECTION('center_axis',(-0.0149854786283017,0.987363721847577,-0.157760312530055));
#83230=DIRECTION('ref_axis',(-0.999587986357288,-0.0186562564288687,-0.0218128775323698));
#83231=DIRECTION('',(0.607059907517467,0.,0.794656069431855));
#83232=DIRECTION('center_axis',(0.0289725563100853,-0.987363722322521,-0.155799457066687));
#83233=DIRECTION('ref_axis',(-0.951025401157534,0.0207595545961579,-0.308414862232871));
#83234=DIRECTION('',(-0.906577388181206,0.,0.422039618091172));
#83235=DIRECTION('center_axis',(-7.20775410205984E-14,-1.,-1.77435358103594E-14));
#83236=DIRECTION('ref_axis',(1.,-7.20775410205984E-14,-5.0910909284395E-31));
#83237=DIRECTION('center_axis',(-0.00519712986190833,0.987363722957772,
0.158385190053129));
#83238=DIRECTION('ref_axis',(-0.986607560385699,0.0207592326909068,-0.161785586650553));
#83239=DIRECTION('center_axis',(0.0192786812815472,0.987363721912878,-0.157293398139886));
#83240=DIRECTION('ref_axis',(-0.971529050833944,-0.0186562524121231,-0.236184774343376));
#83241=DIRECTION('',(0.422039619688627,0.,0.906577387437542));
#83242=DIRECTION('center_axis',(0.0617874731942246,-0.987363722350534,-0.145928708424253));
#83243=DIRECTION('ref_axis',(-0.862490877748826,0.0207595528997825,-0.505646642195377));
#83244=DIRECTION('',(-0.976108155148253,0.,0.217285226034985));
#83245=DIRECTION('center_axis',(7.9893686956293E-14,-1.,3.93878910334263E-14));
#83246=DIRECTION('ref_axis',(1.,7.9893686956293E-14,7.57869122091651E-31));
#83247=DIRECTION('center_axis',(-0.0391237546114933,0.987363722897334,0.153565004253628));
#83248=DIRECTION('ref_axis',(-0.928762104735744,0.0207592363557858,-0.370094591844781));
#83249=DIRECTION('center_axis',(0.0526413843344021,0.987363721816876,-0.149471621036518));
#83250=DIRECTION('ref_axis',(-0.898042496937889,-0.0186562558923963,-0.439512932471434));
#83251=DIRECTION('',(0.21728522775494,0.,0.976108154765385));
#83252=DIRECTION('center_axis',(0.0917132761324331,-0.987363722364209,-0.129234495163442));
#83253=DIRECTION('ref_axis',(-0.733627238879286,0.0207595515989269,-0.679234948594201));
#83254=DIRECTION('',(-0.999997189610847,0.,0.00237081640126621));
#83255=DIRECTION('center_axis',(-3.47792923060787E-14,-1.,-2.782090251181E-14));
#83256=DIRECTION('ref_axis',(1.,-3.47792923060787E-14,-7.51127384914101E-31));
#83257=DIRECTION('center_axis',(-0.0712210092506948,0.98736372322825,0.141564281844537));
#83258=DIRECTION('ref_axis',(-0.82748876612426,0.020759224011969,-0.561098384025984));
#83259=DIRECTION('center_axis',(0.0835426338265499,0.987363721708827,-0.134660719538468));
#83260=DIRECTION('ref_axis',(-0.782564473587812,-0.0186562616054858,-0.622289955391487));
#83261=DIRECTION('',(0.00237082103812565,0.,0.999997189599853));
#83262=DIRECTION('center_axis',(0.117350665271771,-0.987363722334509,-0.106497423339791));
#83263=DIRECTION('ref_axis',(-0.570460005892413,0.0207595544146053,-0.821062983319633));
#83264=DIRECTION('',(-0.977127466912818,0.,-0.212654446002285));
#83265=DIRECTION('center_axis',(-1.86570000645977E-14,-1.,-2.30979900170607E-14));
#83266=DIRECTION('ref_axis',(4.88212395773465E-31,2.30979900170607E-14,
-1.));
#83267=DIRECTION('center_axis',(-0.0999880321934036,0.987363722991602,0.122944182205804));
#83268=DIRECTION('ref_axis',(-0.687522971709477,0.0207592324695274,-0.725865839972543));
#83269=DIRECTION('center_axis',(0.110537530221466,0.987363721825394,-0.113553226443133));
#83270=DIRECTION('ref_axis',(-0.630494605257325,-0.0186562572179942,-0.775969391669559));
#83271=DIRECTION('',(-0.212654444280544,0.,0.977127467287525));
#83272=DIRECTION('center_axis',(0.137500868251949,-0.987363722272268,-0.0787806522606443));
#83273=DIRECTION('ref_axis',(-0.380618696773504,0.0207595585214019,-0.924499025633038));
#83274=DIRECTION('',(-0.908568350643389,0.,-0.417736223242793));
#83275=DIRECTION('center_axis',(-3.31385617699243E-14,-1.,-6.64216885082524E-14));
#83276=DIRECTION('ref_axis',(-6.03805196582697E-31,6.64216885082524E-14,
-1.));
#83277=DIRECTION('center_axis',(-0.12407973107399,0.987363722900487,0.0985753470026679));
#83278=DIRECTION('ref_axis',(-0.515409366918908,0.0207592357297002,-0.85669261618399));
#83279=DIRECTION('center_axis',(0.132363809458612,0.987363721692603,-0.087136117832598));
#83280=DIRECTION('ref_axis',(-0.448943511408003,-0.0186562616387398,-0.893365360569974));
#83281=DIRECTION('',(-0.41773622273295,0.,0.908568350877801));
#83282=DIRECTION('center_axis',(0.151221686204625,-0.987363722346416,-0.0473801795654959));
#83283=DIRECTION('ref_axis',(-0.172980080774042,0.0207595558008577,-0.984706520999205));
#83284=DIRECTION('',(-0.797525585226132,0.,-0.603285124058033));
#83285=DIRECTION('center_axis',(-1.08510605719282E-14,-1.,-4.31955584310798E-14));
#83286=DIRECTION('ref_axis',(1.02420910079709E-32,4.31955584310798E-14,
-1.));
#83287=DIRECTION('center_axis',(-0.142369603550258,0.987363723128988,0.069597228635955));
#83288=DIRECTION('ref_axis',(-0.319195796297111,0.0207592278209998,-0.947461396620743));
#83289=DIRECTION('center_axis',(0.148000906130631,0.987363721679453,-0.0566446193014943));
#83290=DIRECTION('ref_axis',(-0.246400316544395,-0.0186562636632086,-0.968988559185789));
#83291=DIRECTION('',(-0.603285121269556,0.,0.797525587335464));
#83292=DIRECTION('',(-0.649191412957101,3.74026243672172E-15,-0.76062507803961));
#83293=DIRECTION('',(-0.760625076895703,0.,0.64919141429736));
#83294=DIRECTION('center_axis',(0.15713950675887,-0.987363722295113,0.0204952509405883));
#83295=DIRECTION('ref_axis',(0.256475066635952,0.02075955649749,-0.966327884834186));
#83296=DIRECTION('',(-0.470501770976394,0.,-0.882399050038064));
#83297=DIRECTION('center_axis',(2.76306279419956E-15,-1.,-1.45864897414642E-14));
#83298=DIRECTION('ref_axis',(-4.09279871659108E-32,1.45864897414642E-14,
-1.));
#83299=DIRECTION('center_axis',(-0.158434270677379,0.987363723095254,0.00338529029850841));
#83300=DIRECTION('ref_axis',(0.108134457296577,0.0207592293236594,-0.993919510595834));
#83301=DIRECTION('center_axis',(0.158106442288904,0.987363721720486,0.010734707122974));
#83302=DIRECTION('ref_axis',(0.18324086639066,-0.0186562600823441,-0.982891005576987));
#83303=DIRECTION('',(-0.882399049845416,0.,0.470501771337694));
#83304=DIRECTION('center_axis',(0.149059797579392,-0.98736372234962,0.0537964360668407));
#83305=DIRECTION('ref_axis',(0.458210753203742,0.0207595523637838,-0.888601117844286));
#83306=DIRECTION('',(-0.26981198698136,0.,-0.9629130239441));
#83307=DIRECTION('center_axis',(0.,-1.,0.));
#83308=DIRECTION('ref_axis',(0.,0.,-1.));
#83309=DIRECTION('center_axis',(-0.155457905398942,0.987363722888109,-0.0307525344241237));
#83310=DIRECTION('ref_axis',(0.319269649296509,0.0207592364372728,-0.94743651245908));
#83311=DIRECTION('center_axis',(0.152102355397201,0.987363721802279,0.0444719501638507));
#83312=DIRECTION('ref_axis',(0.390249308908463,-0.0186562566933496,-0.920520190426402));
#83313=DIRECTION('',(-0.962913022721775,0.,0.26981199134363));
#83314=DIRECTION('center_axis',(0.134010221269008,-0.987363722314795,0.084582152089576));
#83315=DIRECTION('ref_axis',(0.63852101350025,0.0207595566138072,-0.769324350406128));
#83316=DIRECTION('',(-0.0565060964350291,0.,-0.998402254136916));
#83317=DIRECTION('center_axis',(-4.31619796904112E-14,-1.,6.039079790533E-14));
#83318=DIRECTION('ref_axis',(-9.67732215104448E-31,-6.039079790533E-14,
-1.));
#83319=DIRECTION('center_axis',(-0.145212496255427,0.987363723096625,-0.0634524171646621));
#83320=DIRECTION('ref_axis',(0.515476145884545,0.0207592294934855,-0.856652436764673));
#83321=DIRECTION('center_axis',(0.138986131034853,0.987363721861035,0.076129732251514));
#83322=DIRECTION('ref_axis',(0.57901012730644,-0.0186562549495507,-0.815106874359331));
#83323=DIRECTION('',(-0.998402253875163,0.,0.0565061010599261));
#83324=DIRECTION('center_axis',(0.112694472634348,-0.987363722352503,0.111412905984339));
#83325=DIRECTION('ref_axis',(0.788974741981374,0.0207595546116365,-0.614074830462665));
#83326=DIRECTION('',(0.15944195467659,0.,-0.987207305022055));
#83327=DIRECTION('center_axis',(9.92432034065362E-14,-1.,-8.9460620704829E-14));
#83328=DIRECTION('ref_axis',(1.,9.92432034065362E-14,1.52267170892412E-30));
#83329=DIRECTION('center_axis',(-0.128177111838365,0.987363723176768,-0.0931853322969094));
#83330=DIRECTION('ref_axis',(0.687579553211328,0.0207592255307392,-0.725812243325417));
#83331=DIRECTION('center_axis',(0.11937107285857,0.987363721788263,0.104227769145382));
#83332=DIRECTION('ref_axis',(0.740697075790419,-0.0186562581167305,-0.671580066670091));
#83333=DIRECTION('',(-0.987207304850248,0.,-0.159441955740358));
#83334=DIRECTION('center_axis',(0.0861092603822379,-0.987363722265456,0.133034113033189));
#83335=DIRECTION('ref_axis',(0.902536886948628,0.0207595581119766,-0.430111855735313));
#83336=DIRECTION('',(0.367934678144182,0.,-0.929851640111979));
#83337=DIRECTION('center_axis',(3.87181138908445E-14,-1.,-2.20115753669646E-14));
#83338=DIRECTION('ref_axis',(1.,3.87181138908445E-14,-5.29240579877378E-31));
#83339=DIRECTION('center_axis',(-0.105148313695901,0.987363723085993,-0.118560998902152));
#83340=DIRECTION('ref_axis',(0.827532501342244,0.0207592292772026,-0.561033879210574));
#83341=DIRECTION('center_axis',(0.0941743549645455,0.987363721723206,0.127452233765876));
#83342=DIRECTION('ref_axis',(0.867749851718935,-0.0186562587549658,-0.496650922531142));
#83343=DIRECTION('',(-0.929851640370812,0.,-0.367934677490054));
#83344=DIRECTION('center_axis',(0.0554976663461317,-0.987363722373159,0.148434796363768));
#83345=DIRECTION('ref_axis',(0.973897411717727,0.0207595527340627,-0.226037325280125));
#83346=DIRECTION('',(0.559223188237572,0.,-0.829017144417053));
#83347=DIRECTION('center_axis',(2.83631625789902E-14,-1.,-8.78247130185755E-15));
#83348=DIRECTION('ref_axis',(1.,2.83631625789902E-14,-2.50109950454817E-31));
#83349=DIRECTION('center_axis',(-0.0772028993467409,0.987363722956136,-0.138392886098437));
#83350=DIRECTION('ref_axis',(0.928790951318559,0.0207592346313163,-0.370022192478082));
#83351=DIRECTION('center_axis',(0.0645741468664167,0.987363721787944,0.144717174010324));
#83352=DIRECTION('ref_axis',(0.95422761013519,-0.0186562576921633,-0.298498931496591));
#83353=DIRECTION('',(-0.829017145402445,0.,-0.559223186776784));
#83354=DIRECTION('center_axis',(0.0222910694351928,-0.987363722348557,0.156894831060289));
#83355=DIRECTION('ref_axis',(0.999719574720903,0.0207595537623816,-0.0113935441124832));
#83356=DIRECTION('',(0.724363041874931,0.,-0.689418728760466));
#83357=DIRECTION('center_axis',(-1.47940096643841E-14,-1.,1.23995022967283E-15));
#83358=DIRECTION('ref_axis',(1.,-1.47940096643841E-14,-1.11149104892168E-32));
#83359=DIRECTION('center_axis',(-0.0456475581498243,0.987363722973727,-0.151753678671785));
#83360=DIRECTION('ref_axis',(0.986620168387057,0.0207592337038213,-0.161708681114913));
#83361=DIRECTION('center_axis',(0.0319545266572246,0.987363721747205,0.155215299515288));
#83362=DIRECTION('ref_axis',(0.996086745484081,-0.0186562596592667,-0.0863894637467843));
#83363=DIRECTION('',(-0.689418728599904,0.,-0.724363042027747));
#83364=DIRECTION('center_axis',(-0.0119578282286655,-0.987363722267693,
0.158018639070651));
#83365=DIRECTION('ref_axis',(0.978795961913238,0.0207595597848566,0.203782986581015));
#83366=DIRECTION('',(0.855632484051998,0.,-0.517583860099026));
#83367=DIRECTION('center_axis',(1.32432179419927E-13,-1.,1.77238250181088E-14));
#83368=DIRECTION('ref_axis',(1.,1.32432179419927E-13,-2.65043621295196E-31));
#83369=DIRECTION('center_axis',(-0.0119577902703965,0.987363722876856,-0.158018638136787));
#83370=DIRECTION('ref_axis',(0.998316123369291,0.0207592357518346,0.0541661513485184));
#83371=DIRECTION('center_axis',(-0.00215925399566002,0.987363721770524,
0.158455730580002));
#83372=DIRECTION('ref_axis',(0.991369971740769,-0.0186562595974695,0.129759481767379));
#83373=DIRECTION('',(-0.517583861605946,0.,-0.855632483140441));
#83374=DIRECTION('center_axis',(-0.0456476012493495,-0.987363722312714,
0.151753670008215));
#83375=DIRECTION('ref_axis',(0.912104937720815,0.0207595555807828,0.409430853059947));
#83376=DIRECTION('',(0.946893502365912,0.,-0.321547345156537));
#83377=DIRECTION('center_axis',(-9.76312478759136E-14,-1.,-3.56054655558263E-14));
#83378=DIRECTION('ref_axis',(1.,-9.76312478759136E-14,-8.59526417176721E-31));
#83379=DIRECTION('center_axis',(0.0222911163562628,0.987363723032372,-0.156894820090549));
#83380=DIRECTION('ref_axis',(0.963331926327018,0.0207592312244037,0.267508231720164));
#83381=DIRECTION('center_axis',(-0.0361720677920674,0.987363721674074,0.154286949005961));
#83382=DIRECTION('ref_axis',(0.940297840452972,-0.0186562617608721,0.339841014500292));
#83383=DIRECTION('',(-0.32154734682426,0.,-0.946893501799584));
#83384=DIRECTION('center_axis',(-0.0772029402015664,-0.987363722356275,
0.138392867587147));
#83385=DIRECTION('ref_axis',(0.802764900110338,0.0207595540381597,0.595934187697749));
#83386=DIRECTION('',(0.993878832740327,0.,-0.110475634556792));
#83387=DIRECTION('center_axis',(7.51667665024089E-14,-1.,4.77950244623643E-14));
#83388=DIRECTION('ref_axis',(1.,7.51667665024089E-14,2.19098282777113E-31));
#83389=DIRECTION('center_axis',(0.0554977124760272,0.987363723067266,-0.148434774499359));
#83390=DIRECTION('ref_axis',(0.883303398270499,0.0207592297355248,0.46834192742544));
#83391=DIRECTION('center_axis',(-0.0684935226579129,0.98736372182022,0.142903877439465));
#83392=DIRECTION('ref_axis',(0.845258426819615,-0.0186562564228737,0.534031961577875));
#83393=DIRECTION('',(-0.110475636307964,0.,-0.993878832545673));
#83394=DIRECTION('center_axis',(-0.105148352850834,-0.987363722301292,0.118560970711675));
#83395=DIRECTION('ref_axis',(0.655888469378332,0.0207595557135769,0.754572300434573));
#83396=DIRECTION('',(0.99439149393359,0.,0.105761792687731));
#83397=DIRECTION('center_axis',(2.10449639732453E-14,-1.,2.09454121104238E-14));
#83398=DIRECTION('ref_axis',(1.,2.10449639732453E-14,6.31337018212632E-32));
#83399=DIRECTION('center_axis',(0.0861092934140696,0.987363722975823,-0.133034086380344));
#83400=DIRECTION('ref_axis',(0.76197258528134,0.0207592328245021,0.647276473797873));
#83401=DIRECTION('center_axis',(-0.0976122906414578,0.987363721776479,0.124838782577484));
#83402=DIRECTION('ref_axis',(0.710695667994112,-0.0186562580397901,0.703252167810633));
#83403=DIRECTION('',(0.105761793778192,0.,-0.994391493817611));
#83404=DIRECTION('center_axis',(-0.128177146779924,-0.987363722313685,0.0931852933794923));
#83405=DIRECTION('ref_axis',(0.478343420119804,0.0207595560447544,0.87792745330176));
#83406=DIRECTION('',(0.948407514082987,0.,0.317053918491681));
#83407=DIRECTION('center_axis',(3.21005998968575E-14,-1.,4.99595303694677E-14));
#83408=DIRECTION('ref_axis',(-1.62345145347269E-32,-4.99595303694677E-14,
-1.));
#83409=DIRECTION('center_axis',(0.112694502133346,0.987363722956734,-0.111412870791198));
#83410=DIRECTION('ref_axis',(0.605012781775338,0.0207592327885922,0.7959450911605));
#83411=DIRECTION('center_axis',(-0.122166815496786,0.987363721684866,0.100936367539084));
#83412=DIRECTION('ref_axis',(0.542901569720667,-0.0186562621546152,0.839589083705388));
#83413=DIRECTION('',(0.317053919406767,0.,-0.948407513777072));
#83414=DIRECTION('center_axis',(-0.145212520777593,-0.987363722355149,0.0634523725829109));
#83415=DIRECTION('ref_axis',(0.278431566842413,0.0207595529164433,0.960231692639015));
#83416=DIRECTION('',(0.858077052116883,0.,0.51352095636926));
#83417=DIRECTION('center_axis',(2.06102834792613E-14,-1.,5.56921844170132E-14));
#83418=DIRECTION('ref_axis',(1.55831017715474E-31,-5.56921844170132E-14,
-1.));
#83419=DIRECTION('center_axis',(0.134010239663865,0.987363722853647,-0.0845821166548784));
#83420=DIRECTION('ref_axis',(0.419763252540507,0.0207592367336559,0.907396201175016));
#83421=DIRECTION('center_axis',(-0.141008959833401,0.987363721776961,0.0723142735941615));
#83422=DIRECTION('ref_axis',(0.349721999250997,-0.0186562580065864,0.936667746469941));
#83423=DIRECTION('',(0.513520954857275,0.,-0.858077053021739));
#83424=DIRECTION('center_axis',(-0.155457916612102,-0.987363722303317,0.0307524965159346));
#83425=DIRECTION('ref_axis',(0.0655005617138484,0.020759557685025,0.997636565679051));
#83426=DIRECTION('',(0.727623861282843,0.,0.685976323565068));
#83427=DIRECTION('center_axis',(-6.11718982189012E-15,-1.,-4.41155503170608E-14));
#83428=DIRECTION('ref_axis',(-2.5998598857542E-32,4.41155503170608E-14,
-1.));
#83429=DIRECTION('center_axis',(0.149059810412648,0.987363723002602,-0.0537963885236487));
#83430=DIRECTION('ref_axis',(0.214886058244713,0.0207592318881922,0.976418473946218));
#83431=DIRECTION('center_axis',(-0.153257680116604,0.987363721845255,0.0403108455525592));
#83432=DIRECTION('ref_axis',(0.140189813985162,-0.0186562558720133,0.989948867453084));
#83433=DIRECTION('center_axis',(-7.01873189011981E-15,-1.,8.87983364791519E-14));
#83434=DIRECTION('ref_axis',(1.3690381083063E-31,-8.87983364791519E-14,
-1.));
#83435=DIRECTION('center_axis',(0.157139508177808,0.987363722970567,-0.0204952075212232));
#83436=DIRECTION('ref_axis',(-3.89661523431908E-5,0.0207592334146242,0.999784503135389));
#83437=DIRECTION('center_axis',(-0.158340241192816,0.987363721799664,0.00642253010240786));
#83438=DIRECTION('ref_axis',(-0.0758974889019666,-0.018656256436268,0.996941079138662));
#83439=DIRECTION('',(0.68597632228297,0.,-0.727623862491556));
#83440=DIRECTION('center_axis',(0.163550506959679,-0.986495108643176,0.00886748534365151));
#83441=DIRECTION('ref_axis',(0.0262170039174905,0.0133314937162301,0.999567376408856));
#83442=DIRECTION('center_axis',(-0.160229039203745,-0.98649510925111,0.0339713764732357));
#83443=DIRECTION('ref_axis',(0.138731003294514,0.0115680715646117,0.990262535111358));
#83444=DIRECTION('center_axis',(0.161633050324773,-0.98649510723104,-0.0264983103598656));
#83445=DIRECTION('ref_axis',(0.240481465453549,0.0133315360443304,0.970562174680227));
#83446=DIRECTION('center_axis',(-0.149180133269807,-0.986495109263739,0.0676216476901187));
#83447=DIRECTION('ref_axis',(0.348364721933479,0.0115680673112049,0.937287682801227));
#83448=DIRECTION('center_axis',(0.152157803025431,-0.986495107357098,-0.0606251279502263));
#83449=DIRECTION('ref_axis',(0.443501319199322,0.013331529601327,0.896174564572634));
#83450=DIRECTION('center_axis',(-0.131155729272303,-0.986495109286855,0.0981100098469422));
#83451=DIRECTION('ref_axis',(0.541709293051917,0.0115680673377809,0.840486300685062));
#83452=DIRECTION('center_axis',(0.135567830578251,-0.986495107258517,-0.0919171728640135));
#83453=DIRECTION('ref_axis',(0.625783546599744,0.0133315341903691,0.779882826456114));
#83454=DIRECTION('center_axis',(-0.106998624069017,-0.986495109229355,0.124010862080306));
#83455=DIRECTION('ref_axis',(0.709724143246153,0.0115680739444168,0.704384710338556));
#83456=DIRECTION('center_axis',(0.112638853169902,-0.986495107286684,-0.11891127808582));
#83457=DIRECTION('ref_axis',(0.778804829717616,0.0133315319382028,0.627124634713624));
#83458=DIRECTION('center_axis',(-0.0778383928847543,-0.986495109242355,
0.144113094595991));
#83459=DIRECTION('ref_axis',(0.844553077683583,0.0115680663400262,0.535346877095908));
#83460=DIRECTION('center_axis',(0.0844430093730047,-0.986495107287699,-0.140345222453287));
#83461=DIRECTION('ref_axis',(0.895410064196242,0.0133315316262661,0.445042792549863));
#83462=DIRECTION('center_axis',(-0.0450385179583259,-0.986495109255801,
0.157476764363836));
#83463=DIRECTION('ref_axis',(0.939891649508408,0.0115680677193456,0.341276818717012));
#83464=DIRECTION('center_axis',(0.0522987062510939,-0.986495107258399,-0.1552167796332));
#83465=DIRECTION('ref_axis',(0.970146919221119,0.0133315332775466,0.242151244775328));
#83466=DIRECTION('center_axis',(-0.0101326912773838,-0.986495109255921,
0.163476995267303));
#83467=DIRECTION('ref_axis',(0.991281933042656,0.0115680694691132,0.131249034251579));
#83468=DIRECTION('center_axis',(0.0177089702822737,-0.986495107305781,-0.162830573398542));
#83469=DIRECTION('ref_axis',(0.999520783098335,0.0133315315275395,0.0279369723059262));
#83470=DIRECTION('center_axis',(0.0252469209161869,-0.986495109272429,0.1618332239246));
#83471=DIRECTION('ref_axis',(0.996320974931463,0.0115680629516839,-0.0849158102544182));
#83472=DIRECTION('center_axis',(-0.0177088158145139,-0.986495107315351,
-0.162830590139942));
#83473=DIRECTION('ref_axis',(0.98215816532745,0.0133315318177788,-0.187583604134287));
#83474=DIRECTION('center_axis',(0.0594460241247487,-0.986495109265875,0.152622310329353));
#83475=DIRECTION('ref_axis',(0.954773155677358,0.0115680663260198,-0.297110082359009));
#83476=DIRECTION('center_axis',(-0.0522985590052692,-0.986495107345191,
-0.155216828694483));
#83477=DIRECTION('ref_axis',(0.918870923356613,0.0133315297702083,-0.394332976713528));
#83478=DIRECTION('center_axis',(0.0908654951821714,-0.986495109267404,0.136274946988765));
#83479=DIRECTION('ref_axis',(0.868581205501574,0.0115680676184969,-0.495411817845524));
#83480=DIRECTION('center_axis',(-0.0844428741895767,-0.98649510726196,-0.140345303971376));
#83481=DIRECTION('ref_axis',(0.812618298321134,0.0133315342674835,-0.58264377747277));
#83482=DIRECTION('center_axis',(0.118036198596521,-0.986495109232563,0.113555516295406));
#83483=DIRECTION('ref_axis',(0.741775361464524,0.0115680711949706,-0.670548650623505));
#83484=DIRECTION('center_axis',(-0.11263873867622,-0.986495107271142,-0.118911386668935));
#83485=DIRECTION('ref_axis',(0.668368546867031,0.0133315334872308,-0.743710801167854));
#83486=DIRECTION('center_axis',(0.139687655736812,-0.986495109271077,0.0855263597904134));
#83487=DIRECTION('ref_axis',(0.580284927671301,0.0115680688497371,-0.814331371433399));
#83488=DIRECTION('center_axis',(-0.135567741482167,-0.986495107297552,-0.0919173038519721));
#83489=DIRECTION('ref_axis',(0.492866620788169,0.0133315323142876,-0.87000273813305));
#83490=DIRECTION('center_axis',(0.154807477127269,-0.986495109248506,0.0534980789773647));
#83491=DIRECTION('ref_axis',(0.391661014295995,0.0115680743258794,-0.920036863140289));
#83492=DIRECTION('center_axis',(-0.152157746667951,-0.98649510732727,-0.0606252698822009));
#83493=DIRECTION('ref_axis',(0.294318802411539,0.0133315306675126,-0.9556143117582));
#83494=DIRECTION('center_axis',(0.162688669256179,-0.986495109251213,0.0189682977383472));
#83495=DIRECTION('ref_axis',(0.184723468394355,0.0115680686706918,-0.982722453193978));
#83496=DIRECTION('center_axis',(-0.161633023909734,-0.98649510726897,-0.0264984700724086));
#83497=DIRECTION('ref_axis',(0.0820089640255199,0.0133315336497295,-0.996542422594245));
#83498=DIRECTION('center_axis',(0.16296272187791,-0.986495109263594,-0.0164484247620746));
#83499=DIRECTION('ref_axis',(-0.0308515416615133,0.011568068114073,-0.999457033682397));
#83500=DIRECTION('center_axis',(-0.163550521080517,-0.986495107309364,0.00886737328516426));
#83501=DIRECTION('ref_axis',(-0.134135522765056,0.0133315319656148,-0.990873317729363));
#83502=DIRECTION('center_axis',(0.155616817863015,-0.986495109242457,-0.0510960413232052));
#83503=DIRECTION('ref_axis',(-0.24498396980316,0.0115680715744787,-0.969458113721027));
#83504=DIRECTION('center_axis',(-0.157820578872764,-0.986495107230776,0.0438185838886268));
#83505=DIRECTION('ref_axis',(-0.34400798034835,0.0133315346117581,-0.938872078422585));
#83506=DIRECTION('center_axis',(0.140994445088194,-0.986495109264766,-0.0833544590946969));
#83507=DIRECTION('ref_axis',(-0.447661218276787,0.0115680704375784,-0.89412840990391));
#83508=DIRECTION('center_axis',(-0.144711118948954,-0.986495107322079,0.076720892083849));
#83509=DIRECTION('ref_axis',(-0.537795012205508,0.013331531453837,-0.842970221962777));
#83510=DIRECTION('center_axis',(0.119779331592619,-0.98649510928187,-0.111715312675464));
#83511=DIRECTION('ref_axis',(-0.629406325552992,0.0115680658336281,-0.776990255541696));
#83512=DIRECTION('center_axis',(-0.12483512904919,-0.986495107325552,0.106035813657553));
#83513=DIRECTION('ref_axis',(-0.706435342852236,0.0133315307102021,-0.707652016642479));
#83514=DIRECTION('center_axis',(0.0929634643369165,-0.986495109244733,-0.134852488796836));
#83515=DIRECTION('ref_axis',(-0.781721093297915,0.0115680696470281,-0.623520899455467));
#83516=DIRECTION('center_axis',(-0.099121994066111,-0.986495107175654,0.130392614096246));
#83517=DIRECTION('ref_axis',(-0.842043541607428,0.0133315380501615,-0.539244790545479));
#83518=DIRECTION('center_axis',(0.0618007367032678,-0.986495109255773,-0.151684107135105));
#83519=DIRECTION('ref_axis',(-0.897483449175347,0.0115680643638219,-0.440896403186959));
#83520=DIRECTION('center_axis',(-0.0687740162808509,-0.986495107239798,
0.148652406897909));
#83521=DIRECTION('ref_axis',(-0.9382787215921,0.0133315348704548,-0.345623076176191));
#83522=DIRECTION('center_axis',(0.0277482648204804,-0.986495109259417,-0.1614231495378));
#83523=DIRECTION('ref_axis',(-0.971280479329197,0.0115680697816831,-0.237656075528424));
#83524=DIRECTION('center_axis',(-0.035210239642401,-0.986495107333624,0.159961377310733));
#83525=DIRECTION('ref_axis',(-0.990641031576325,0.0133315299978489,-0.135840409544843));
#83526=DIRECTION('center_axis',(-0.00760168005493634,-0.986495109258894,
-0.163614222696638));
#83527=DIRECTION('ref_axis',(-0.999661512623984,0.0115680702645302,-0.0233032171316153));
#83528=DIRECTION('center_axis',(-8.08991190322417E-8,-0.986495107233334,
0.163790730521253));
#83529=DIRECTION('ref_axis',(-0.996682067559661,0.0133315344477418,0.080293999740133));
#83530=DIRECTION('center_axis',(-0.0425961788913145,-0.986495109233485,
-0.158154876631335));
#83531=DIRECTION('ref_axis',(-0.981299484699764,0.0115680705614484,0.192139275192408));
#83532=DIRECTION('center_axis',(0.0352100904617006,-0.986495107332138,0.159961410157052));
#83533=DIRECTION('ref_axis',(-0.956119357377107,0.0133315306025481,0.292673956375658));
#83534=DIRECTION('center_axis',(-0.0755989235215392,-0.986495109243415,
-0.145300386101373));
#83535=DIRECTION('ref_axis',(-0.917052983559382,0.0115680662317178,0.398597547895737));
#83536=DIRECTION('center_axis',(0.0687738742027003,-0.986495107341154,0.148652471957637));
#83537=DIRECTION('ref_axis',(-0.870849568622735,0.0133315291853619,0.491368801572887));
#83538=DIRECTION('center_axis',(-0.105066754479705,-0.986495109268846,-0.125651806559833));
#83539=DIRECTION('ref_axis',(-0.809926103476048,0.0115680712214746,0.586417843040541));
#83540=DIRECTION('center_axis',(0.0991218622055378,-0.986495107223832,0.130392713969553));
#83541=DIRECTION('ref_axis',(-0.744859823054238,0.0133315350752992,0.66708778595635));
#83542=DIRECTION('center_axis',(-0.129621774237956,-0.986495109274238,-0.100127893323553));
#83543=DIRECTION('ref_axis',(-0.664927980385921,0.0115680680390169,0.746817889918115));
#83544=DIRECTION('center_axis',(0.124835029130842,-0.986495107315024,0.106035931388474));
#83545=DIRECTION('ref_axis',(-0.584041259269706,0.0133315314906892,0.81161448837411));
#83546=DIRECTION('center_axis',(-0.148115826717122,-0.986495109262762,-0.0699221086392219));
#83547=DIRECTION('ref_axis',(-0.488838562437753,0.011568068288881,0.872297563718858));
#83548=DIRECTION('center_axis',(0.144711044899141,-0.986495107184836,0.076721033521315));
#83549=DIRECTION('ref_axis',(-0.395913577600531,0.0133315358117855,0.918190998226648));
#83550=DIRECTION('center_axis',(-0.159684149326762,-0.986495109228651,-0.036446836923669));
#83551=DIRECTION('ref_axis',(-0.28989159657348,0.0115680757083828,0.956989572493078));
#83552=DIRECTION('center_axis',(0.157820536374888,-0.986495107342756,0.0438187344311385));
#83553=DIRECTION('ref_axis',(-0.189273412709158,0.0133315291307049,0.981833919546715));
#83554=DIRECTION('center_axis',(-0.163785816964949,-0.986495108921018,-0.00126737367530744));
#83555=DIRECTION('ref_axis',(-0.0773896270365963,0.0115680610235149,0.996933812041348));
#83556=DIRECTION('center_axis',(-0.163785817306842,0.986495108821648,0.00126740683861602));
#83557=DIRECTION('ref_axis',(-0.0768446779811248,-0.0140392001935921,0.996944229294649));
#83558=DIRECTION('center_axis',(-0.160229061654718,0.986495107964944,-0.033971307930117));
#83559=DIRECTION('ref_axis',(-0.289361608418837,-0.0140392242780245,0.957116899733222));
#83560=DIRECTION('center_axis',(-0.149180170698907,0.986495107847839,-0.0676215857735171));
#83561=DIRECTION('ref_axis',(-0.488348336529291,-0.0140392289373408,0.872535845830943));
#83562=DIRECTION('center_axis',(-0.131155774091502,0.986495108033152,-0.0981099625375499));
#83563=DIRECTION('ref_axis',(-0.664500439371671,-0.0140392219614871,0.74715598526785));
#83564=DIRECTION('center_axis',(-0.106998686998783,0.986495107899956,-0.124010818358685));
#83565=DIRECTION('ref_axis',(-0.809581238604204,-0.0140392262583843,0.586839942596061));
#83566=DIRECTION('center_axis',(-0.0778384296784011,0.986495108808148,-0.144113077695263));
#83567=DIRECTION('ref_axis',(-0.916806922417426,-0.0140391983509365,0.399083910872326));
#83568=DIRECTION('center_axis',(-0.0450385871440512,0.986495107907963,-0.157476753020009));
#83569=DIRECTION('ref_axis',(-0.981163728413274,-0.0140392260617028,0.192667169434109));
#83570=DIRECTION('center_axis',(-0.0101327645796777,0.986495107901833,-0.163476998895024));
#83571=DIRECTION('ref_axis',(-0.999642411894656,-0.0140392275555301,-0.0227584804211519));
#83572=DIRECTION('center_axis',(0.0252468556544985,0.98649510787844,-0.161833242603198));
#83573=DIRECTION('ref_axis',(-0.971378926912717,-0.0140392284255323,-0.237119970510952));
#83574=DIRECTION('center_axis',(0.0594459620639049,0.986495107877398,-0.152622343476498));
#83575=DIRECTION('ref_axis',(-0.897694843465258,-0.0140392277430696,-0.440393991898465));
#83576=DIRECTION('center_axis',(0.0908654418332143,0.986495107903131,-0.136274992436783));
#83577=DIRECTION('ref_axis',(-0.782035544919108,-0.0140392268974693,-0.623075682875841));
#83578=DIRECTION('center_axis',(0.118036168365079,0.986495108253068,-0.113555556228917));
#83579=DIRECTION('ref_axis',(-0.629809135699137,-0.0140392025394138,-0.776623044585958));
#83580=DIRECTION('center_axis',(0.139687633297808,0.986495108711818,-0.0855264028900755));
#83581=DIRECTION('ref_axis',(-0.448133544647552,-0.0140392045032719,-0.893856379346557));
#83582=DIRECTION('center_axis',(0.154807463347207,0.986495108715876,-0.0534981286743339));
#83583=DIRECTION('ref_axis',(-0.245503734126674,-0.0140392015699084,-0.969293978805779));
#83584=DIRECTION('center_axis',(0.162688669059064,0.986495107942603,-0.0189683674864747));
#83585=DIRECTION('ref_axis',(-0.0313944450013707,-0.0140392248625478,-0.999408469540015));
#83586=DIRECTION('center_axis',(0.162962736978838,0.986495107917882,0.016448355858674));
#83587=DIRECTION('ref_axis',(0.184182820785979,-0.0140392266767644,-0.982791732078388));
#83588=DIRECTION('center_axis',(0.155616834415035,0.986495108793173,0.0510959995869567));
#83589=DIRECTION('ref_axis',(0.391147904392901,-0.0140391977490532,-0.920220744069381));
#83590=DIRECTION('center_axis',(0.140994474738935,0.986495108267932,0.0833544207377945));
#83591=DIRECTION('ref_axis',(0.579823339829956,-0.0140392019901395,-0.814621258865686));
#83592=DIRECTION('center_axis',(0.11977938301305,0.986495107934913,0.111715269437521));
#83593=DIRECTION('ref_axis',(0.741386879346129,-0.0140392247113993,-0.670930991461053));
#83594=DIRECTION('center_axis',(0.0929635116883181,0.98649510817471,0.134852463981731));
#83595=DIRECTION('ref_axis',(0.868283999279012,-0.0140392076646582,-0.495868729851151));
#83596=DIRECTION('center_axis',(0.0618007963427444,0.986495108013688,0.151684090914192));
#83597=DIRECTION('ref_axis',(0.954581119976345,-0.0140392215243303,-0.29762020368869));
#83598=DIRECTION('center_axis',(0.0277483051069888,0.986495108865338,0.16142314502095));
#83599=DIRECTION('ref_axis',(0.996243090992236,-0.0140391952154022,-0.0854552786429238));
#83600=DIRECTION('center_axis',(-0.00760161067101913,0.986495107971953,
0.163614233679749));
#83601=DIRECTION('ref_axis',(0.991321840591628,-0.0140392237424351,0.130705426676691));
#83602=DIRECTION('center_axis',(-0.0425961330144984,0.986495108686194,0.158154892401169));
#83603=DIRECTION('ref_axis',(0.940047482190855,-0.014039202231463,0.340754504045564));
#83604=DIRECTION('center_axis',(-0.0755988870791609,0.986495108778708,0.145300408217175));
#83605=DIRECTION('ref_axis',(0.844817547664969,-0.0140392009180133,0.534870275856615));
#83606=DIRECTION('center_axis',(-0.105066704035494,0.986495107904468,0.125651859451703));
#83607=DIRECTION('ref_axis',(0.710084888071399,-0.0140392256505157,0.703976101778862));
#83608=DIRECTION('center_axis',(-0.129621748001392,0.986495108655268,0.100127933386719));
#83609=DIRECTION('ref_axis',(0.542149443931951,-0.0140392038569982,0.840164794072769));
#83610=DIRECTION('center_axis',(-0.14811581037353,0.986495108721487,0.0699221508963698));
#83611=DIRECTION('ref_axis',(0.34886369311992,-0.0140392012981556,0.937068313651486));
#83612=DIRECTION('center_axis',(-0.159684140679065,0.986495108775018,0.0364468870900323));
#83613=DIRECTION('ref_axis',(0.139265465867208,-0.0140391994767074,0.990155558937505));
#83614=DIRECTION('center_axis',(-0.158434276191237,0.98736372208211,-0.00338532774206208));
#83615=DIRECTION('ref_axis',(0.13269176373348,0.0246892551673806,0.990849805226089));
#83616=DIRECTION('',(-0.72692697915403,0.,-0.68671476391439));
#83617=DIRECTION('center_axis',(-2.02413120793788E-15,-1.,-1.47072459452993E-14));
#83618=DIRECTION('ref_axis',(4.03217368274812E-32,1.47072459452993E-14,
-1.));
#83619=DIRECTION('center_axis',(-0.158420667353366,-0.987363722313518,0.00397139956531338));
#83620=DIRECTION('ref_axis',(0.0602919305233937,-0.0056588840615867,0.998164745993836));
#83621=DIRECTION('center_axis',(0.157139511088837,-0.98736372222782,-0.0204952209840727));
#83622=DIRECTION('ref_axis',(0.136228832793141,0.00111690644803579,0.990676767485644));
#83623=DIRECTION('center_axis',(0.156019001054146,0.987363720691631,-0.0277660651163378));
#83624=DIRECTION('ref_axis',(0.137583909697684,0.00611303106107622,0.990471250791029));
#83625=DIRECTION('',(-0.514391942141765,0.,0.857555205138202));
#83626=DIRECTION('center_axis',(-0.155457916667695,0.987363722050394,0.0307525043554571));
#83627=DIRECTION('ref_axis',(0.342592924413078,0.0246892566060478,0.939159479934231));
#83628=DIRECTION('',(-0.857555204217411,0.,-0.514391943676838));
#83629=DIRECTION('center_axis',(-2.05537251143393E-14,-1.,-5.57130813142657E-14));
#83630=DIRECTION('ref_axis',(5.84912470819078E-31,5.57130813142657E-14,
-1.));
#83631=DIRECTION('center_axis',(-0.153863147012197,-0.987363722313836,0.0379343096690717));
#83632=DIRECTION('ref_axis',(0.273458254901472,-0.00565888572755253,0.961867225680636));
#83633=DIRECTION('center_axis',(0.149059810143834,-0.987363722194988,-0.0537964040911902));
#83634=DIRECTION('ref_axis',(0.346010097831234,0.00111690617069978,0.938230123540822));
#83635=DIRECTION('center_axis',(0.146402480579443,0.98736372069204,-0.0606563825277796));
#83636=DIRECTION('ref_axis',(0.347289315232596,0.00611303022144713,0.93773810970163));
#83637=DIRECTION('',(-0.318016724021307,0.,0.948085103375618));
#83638=DIRECTION('center_axis',(-0.145212519477854,0.987363721982425,0.0634523813572531));
#83639=DIRECTION('ref_axis',(0.536474817340266,0.0246892601642735,0.843555102404264));
#83640=DIRECTION('',(-0.948085102432839,0.,-0.318016726831959));
#83641=DIRECTION('center_axis',(1.60249280290899E-14,-1.,2.49960485478454E-14));
#83642=DIRECTION('ref_axis',(2.56887509140615E-31,-2.49960485478454E-14,
-1.));
#83643=DIRECTION('center_axis',(-0.142111154973303,-0.987363722375813,0.0701234580460158));
#83644=DIRECTION('ref_axis',(0.473837973053062,-0.00565888198529935,0.880593863451048));
#83645=DIRECTION('center_axis',(0.134010234071191,-0.987363722256383,-0.0845821324879288));
#83646=DIRECTION('ref_axis',(0.539612318646171,0.0011168997964084,0.841912880350543));
#83647=DIRECTION('center_axis',(0.129940342043695,0.987363720690238,-0.0907104766512528));
#83648=DIRECTION('ref_axis',(0.540755859363086,0.00611303116878817,0.841157376127928));
#83649=DIRECTION('',(-0.106771401019337,0.,0.994283595320957));
#83650=DIRECTION('center_axis',(-0.128177144889255,0.987363721975308,0.0931852995654673));
#83651=DIRECTION('ref_axis',(0.705271747402913,0.0246892600517126,0.708507023785467));
#83652=DIRECTION('',(-0.994283595393053,0.,-0.106771400347955));
#83653=DIRECTION('center_axis',(3.15355285472734E-14,-1.,3.1450153513418E-14));
#83654=DIRECTION('ref_axis',(1.,3.15355285472734E-14,-6.7257412422847E-31));
#83655=DIRECTION('center_axis',(-0.1237142072212,-0.987363722295486,0.0990337055069238));
#83656=DIRECTION('ref_axis',(0.652061557236837,-0.00565888625187118,0.758144908695072));
#83657=DIRECTION('center_axis',(0.112694496579076,-0.987363722214071,-0.111412882990986));
#83658=DIRECTION('ref_axis',(0.707982863381585,0.0011169071748736,0.706228729008085));
#83659=DIRECTION('center_axis',(0.107402339291569,0.987363720693659,-0.116523047388375));
#83660=DIRECTION('ref_axis',(0.708937258694998,0.00611302945419982,0.705245059610426));
#83661=DIRECTION('',(0.109466440259237,0.,0.993990492136102));
#83662=DIRECTION('center_axis',(-0.105148350645483,0.987363721946392,0.118560975623103));
#83663=DIRECTION('ref_axis',(0.841090951872643,0.0246892610870285,0.540329946481729));
#83664=DIRECTION('',(-0.993990492096633,0.,0.10946644061763));
#83665=DIRECTION('center_axis',(7.51181976136774E-14,-1.,4.78713199577313E-14));
#83666=DIRECTION('ref_axis',(1.,7.51181976136774E-14,-2.23611908406028E-31));
#83667=DIRECTION('center_axis',(-0.0995325155372356,-0.987363722311601,
0.123313252385175));
#83668=DIRECTION('ref_axis',(0.799795464104186,-0.00565888214353483,0.600245943469221));
#83669=DIRECTION('center_axis',(0.086109278976296,-0.987363722241673,-0.13303410117429));
#83670=DIRECTION('ref_axis',(0.843248919199685,0.00111689985599072,0.53752210447876));
#83671=DIRECTION('center_axis',(0.079842323792572,0.987363720671974,-0.136887130265043));
#83672=DIRECTION('ref_axis',(0.843969540097002,0.00611302695943941,0.536356268062421));
#83673=DIRECTION('',(0.320585748995715,0.,0.947219498078907));
#83674=DIRECTION('center_axis',(-0.0772029325999934,0.987363721997434,0.138392874387865));
#83675=DIRECTION('ref_axis',(0.937581679979158,0.0246892581637656,0.34688763872295));
#83676=DIRECTION('',(-0.947219498157887,0.,0.320585748762358));
#83677=DIRECTION('center_axis',(5.57685963377941E-14,-1.,2.04026153647313E-14));
#83678=DIRECTION('ref_axis',(1.,5.57685963377941E-14,-5.33500706981931E-31));
#83679=DIRECTION('center_axis',(-0.0706968004725781,-0.98736372227437,0.141826804023219));
#83680=DIRECTION('ref_axis',(0.910131825527501,-0.00565888663633035,0.414280143337833));
#83681=DIRECTION('center_axis',(0.0554976970913057,-0.987363722217709,-0.148434785902608));
#83682=DIRECTION('ref_axis',(0.939085591280658,0.00111690456700952,0.343681545581436));
#83683=DIRECTION('center_axis',(0.0485489640099731,0.987363720692829,-0.150850525863092));
#83684=DIRECTION('ref_axis',(0.939538744720995,0.00611303092727423,0.342388051808148));
#83685=DIRECTION('',(0.516714824718151,0.,0.856157573064965));
#83686=DIRECTION('center_axis',(-0.0456475944673371,0.987363722009869,0.151753674018667));
#83687=DIRECTION('ref_axis',(0.990232129493659,0.0246892586075882,0.137225253608296));
#83688=DIRECTION('',(-0.85615757348362,0.,0.516714824024471));
#83689=DIRECTION('center_axis',(1.02988754365913E-13,-1.,1.38897742489236E-14));
#83690=DIRECTION('ref_axis',(1.,1.02988754365913E-13,-5.56147776580004E-32));
#83691=DIRECTION('center_axis',(-0.0385553735729892,-0.987363722347117,
0.153708695139513));
#83692=DIRECTION('ref_axis',(0.977911433889352,-0.00565888193743767,0.208943065268242));
#83693=DIRECTION('center_axis',(0.0222911022856109,-0.987363722208346,-0.156894827275387));
#83694=DIRECTION('ref_axis',(0.991011665082042,0.00111690628612727,0.133770819656857));
#83695=DIRECTION('center_axis',(0.014985513516289,0.987363720678149,-0.157760316535104));
#83696=DIRECTION('ref_axis',(0.991176161185229,0.00611302969020073,0.132410152050812));
#83697=DIRECTION('',(0.688682888958241,0.,0.725062672088511));
#83698=DIRECTION('center_axis',(-0.0119578233143749,0.987363722032868,0.158018640909809));
#83699=DIRECTION('ref_axis',(0.996580425785282,0.0246892569760022,-0.0788536335979417));
#83700=DIRECTION('',(-0.72506267162346,0.,0.688682889447858));
#83701=DIRECTION('center_axis',(1.4795260760968E-14,-1.,-1.22492840130852E-15));
#83702=DIRECTION('ref_axis',(1.,1.4795260760968E-14,-9.44775112401041E-33));
#83703=DIRECTION('center_axis',(-0.00461114502435709,-0.987363722359484,
0.158403336801938));
#83704=DIRECTION('ref_axis',(0.999964990721314,-0.00565888236509894,-0.00616395831436079));
#83705=DIRECTION('center_axis',(-0.011957803590877,-0.987363722219323,-0.158018641237308));
#83706=DIRECTION('ref_axis',(0.996599135032951,0.00111690409048127,-0.0823948819819873));
#83707=DIRECTION('center_axis',(-0.0192786475907753,0.987363720691356,-0.157293409936951));
#83708=DIRECTION('ref_axis',(0.996467281998849,0.00611303320384331,-0.0837590993915001));
#83709=DIRECTION('',(0.82844890631414,0.,0.560064647721052));
#83710=DIRECTION('center_axis',(0.0222910820964577,0.987363722053383,0.156894831118995));
#83711=DIRECTION('ref_axis',(0.956329728706116,0.0246892557043555,-0.291245413089463));
#83712=DIRECTION('',(-0.560064645188563,0.,0.828448908026203));
#83713=DIRECTION('center_axis',(-5.67441295577895E-14,-1.,1.75073359026152E-14));
#83714=DIRECTION('ref_axis',(1.,-5.67441295577895E-14,3.268951088727E-31));
#83715=DIRECTION('center_axis',(0.0295486907568079,-0.987363722291013,0.155691216124079));
#83716=DIRECTION('ref_axis',(0.975261296101418,-0.00565888786648576,-0.220982762483178));
#83717=DIRECTION('center_axis',(-0.0456475712957085,-0.987363722194644,
-0.151753679786494));
#83718=DIRECTION('ref_axis',(0.955586737475137,0.00111690638869429,-0.294707888733477));
#83719=DIRECTION('center_axis',(-0.05264135563157,0.987363720687697,-0.149471638604182));
#83720=DIRECTION('ref_axis',(0.955164700011649,0.00611303150036867,-0.296011869183537));
#83721=DIRECTION('',(0.929477575511641,0.,0.368878620444452));
#83722=DIRECTION('center_axis',(0.0554976773333573,0.987363721989729,0.148434794806314));
#83723=DIRECTION('ref_axis',(0.871362116748079,0.02468925852975,-0.49001887923789));
#83724=DIRECTION('',(-0.368878619816821,0.,0.929477575760727));
#83725=DIRECTION('center_axis',(-1.29134809254887E-14,-1.,7.3240836658601E-15));
#83726=DIRECTION('ref_axis',(1.,-1.29134809254887E-14,1.36982976880086E-31));
#83727=DIRECTION('center_axis',(0.0623268698928645,-0.987363722309312,0.14569914604025));
#83728=DIRECTION('ref_axis',(0.904955466281401,-0.00565888615062404,-0.425468660485055));
#83729=DIRECTION('center_axis',(-0.0772029158270658,-0.987363722218414,
-0.138392882168117));
#83730=DIRECTION('ref_axis',(0.869892165667375,0.00111690173774196,-0.493240684292194));
#83731=DIRECTION('center_axis',(-0.0835426144518167,0.987363720671955,-0.134660739161004));
#83732=DIRECTION('ref_axis',(0.869199678216931,0.00611303202809246,-0.494423452343238));
#83733=DIRECTION('',(0.9870449056352,0.,0.16044424034411));
#83734=DIRECTION('center_axis',(0.0861092673242092,0.987363722029707,0.133034110289549));
#83735=DIRECTION('ref_axis',(0.745650580592605,0.0246892563347975,-0.665879607949925));
#83736=DIRECTION('',(-0.160444237331189,0.,0.987044906124951));
#83737=DIRECTION('center_axis',(-6.62226565463095E-14,-1.,5.95732040164543E-14));
#83738=DIRECTION('ref_axis',(1.,-6.62226565463095E-14,8.3663892018305E-31));
#83739=DIRECTION('center_axis',(0.0921907116689665,-0.987363722300279,0.12889434652966));
#83740=DIRECTION('ref_axis',(0.792334927588738,-0.00565888580197279,-0.610060111410695));
#83741=DIRECTION('center_axis',(-0.105148331973004,-0.987363722223273,-0.118560989877356));
#83742=DIRECTION('ref_axis',(0.743522402554116,0.00111690374376028,-0.668710093707417));
#83743=DIRECTION('center_axis',(-0.110537512083763,0.987363720682677,-0.113553254035247));
#83744=DIRECTION('ref_axis',(0.742591847367116,0.00611303133035507,-0.669716342246363));
#83745=DIRECTION('',(0.998459113111179,0.,-0.0554923368154404));
#83746=DIRECTION('center_axis',(0.112694478378786,0.987363721955025,0.11141290369636));
#83747=DIRECTION('ref_axis',(0.585073252754729,0.0246892615105305,-0.810604545556627));
#83748=DIRECTION('',(0.05549233749058,0.,0.998459113073656));
#83749=DIRECTION('center_axis',(5.18679296940795E-14,-1.,-7.2416329169589E-14));
#83750=DIRECTION('ref_axis',(-1.06516527527658E-30,7.2416329169589E-14,
-1.));
#83751=DIRECTION('center_axis',(0.117743820074337,-0.987363722324764,0.106062588462134));
#83752=DIRECTION('ref_axis',(0.642665685848445,-0.00565888336345777,-0.766125833836731));
#83753=DIRECTION('center_axis',(-0.128177131859556,-0.987363722255328,-0.0931853145209106));
#83754=DIRECTION('ref_axis',(0.58238635873767,0.00111690127847762,-0.8129113615197));
#83755=DIRECTION('center_axis',(-0.132363799105279,0.987363720680554,-0.0871361450275937));
#83756=DIRECTION('ref_axis',(0.581261245462771,0.00611303055727861,-0.813694042856696));
#83757=DIRECTION('',(0.96318648209878,0.,-0.268834150922416));
#83758=DIRECTION('center_axis',(0.134010225449165,0.987363721917216,0.0845821501077273));
#83759=DIRECTION('ref_axis',(0.397138547751906,0.0246892614356591,-0.917426517089662));
#83760=DIRECTION('',(0.268834151573656,0.,0.963186481917013));
#83761=DIRECTION('center_axis',(2.92399301853973E-14,-1.,-6.82277895542969E-14));
#83762=DIRECTION('ref_axis',(1.3646765082506E-31,6.82277895542969E-14,-1.));
#83763=DIRECTION('center_axis',(0.13779135489011,-0.987363722256491,0.0782714666360208));
#83764=DIRECTION('ref_axis',(0.462946110105927,-0.00565888732432013,-0.886368363679595));
#83765=DIRECTION('center_axis',(-0.145212510191132,-0.987363722233906,-0.0634523986969547));
#83766=DIRECTION('ref_axis',(0.394018574864488,0.00111690088530794,-0.919101798058393));
#83767=DIRECTION('center_axis',(-0.148000903291999,0.987363720676903,-0.0566446441935525));
#83768=DIRECTION('ref_axis',(0.39275151165799,0.00611303235841334,-0.919624315101416));
#83769=DIRECTION('',(0.882876321704911,0.,-0.469605579793092));
#83770=DIRECTION('center_axis',(0.149059803058461,0.987363721938806,0.0537964284253243));
#83771=DIRECTION('ref_axis',(0.190634087994129,0.0246892603839579,-0.981350643203712));
#83772=DIRECTION('',(0.469605582630874,0.,0.882876320195483));
#83773=DIRECTION('center_axis',(-2.77787178218631E-15,-1.,1.4583676481692E-14));
#83774=DIRECTION('ref_axis',(-3.33324710125482E-32,-1.4583676481692E-14,
-1.));
#83775=DIRECTION('center_axis',(0.15139592084631,-0.987363722236557,0.0468204566644608));
#83776=DIRECTION('ref_axis',(0.261579691361806,-0.00565888879861934,-0.965165292602582));
#83777=DIRECTION('center_axis',(-0.155457912814124,-0.987363722264939,-0.0307525169473966));
#83778=DIRECTION('ref_axis',(0.187226921022217,0.00111689821087627,-0.982316055342132));
#83779=DIRECTION('center_axis',(-0.156717647683712,0.987363720680356,-0.0235045099656937));
#83780=DIRECTION('ref_axis',(0.185877157397317,0.00611302709239814,-0.982553974729969));
#83781=DIRECTION('',(0.761283846234037,0.,-0.648418773219215));
#83782=DIRECTION('',(0.648418775400083,0.,0.761283844376496));
#83783=DIRECTION('',(0.604094581901541,0.,-0.796912627655757));
#83784=DIRECTION('center_axis',(0.15787154625285,0.987363722058788,-0.013764274261669));
#83785=DIRECTION('ref_axis',(-0.239043629497269,0.0246892569315091,-0.970694897374526));
#83786=DIRECTION('',(0.796912626680266,0.,0.604094583188394));
#83787=DIRECTION('center_axis',(-1.44095946369905E-14,-1.,-5.76087374528612E-14));
#83788=DIRECTION('ref_axis',(2.29372654111249E-31,5.76087374528612E-14,
-1.));
#83789=DIRECTION('center_axis',(0.157062614897765,-0.987363722320007,-0.0210764050031671));
#83790=DIRECTION('ref_axis',(-0.16785909061338,-0.00565888540722353,-0.98579475689131));
#83791=DIRECTION('center_axis',(-0.154002427753442,-0.987363722237362,0.0373648532129905));
#83792=DIRECTION('ref_axis',(-0.242541254906398,0.00111690004499825,-0.970140449730202));
#83793=DIRECTION('center_axis',(-0.152102370896309,0.987363720676094,0.0444719221574905));
#83794=DIRECTION('ref_axis',(-0.243866167031853,0.00611303266598791,-0.969789628429185));
#83795=DIRECTION('',(0.418658529089389,0.,-0.908143730926283));
#83796=DIRECTION('center_axis',(0.151221685386099,0.987363722050727,-0.0473801883398824));
#83797=DIRECTION('ref_axis',(-0.442125629794732,0.024689257286697,-0.896613276754947));
#83798=DIRECTION('',(0.90814373120936,0.,0.418658528475346));
#83799=DIRECTION('center_axis',(-3.96853229838742E-14,-1.,-7.97463604750937E-14));
#83800=DIRECTION('ref_axis',(2.74015092108731E-31,7.97463604750937E-14,
-1.));
#83801=DIRECTION('center_axis',(0.148859772414883,-0.987363722370017,-0.0543474737610927));
#83802=DIRECTION('ref_axis',(-0.375851371087144,-0.00565888102545851,-0.926662680762236));
#83803=DIRECTION('center_axis',(-0.14236959780652,-0.987363722223227,0.0695972532353474));
#83804=DIRECTION('ref_axis',(-0.445422293864881,0.0011169001223638,-0.895319905208336));
#83805=DIRECTION('center_axis',(-0.138986155548796,0.987363720659471,0.0761297030813302));
#83806=DIRECTION('ref_axis',(-0.446640814676025,0.00611302818007946,-0.894692468701959));
#83807=DIRECTION('',(0.213646469431561,0.,-0.97691104308398));
#83808=DIRECTION('center_axis',(0.137500865192042,0.987363722076415,-0.078780660055933));
#83809=DIRECTION('ref_axis',(-0.624534330014507,0.0246892551508924,-0.780607014645286));
#83810=DIRECTION('',(0.976911043828262,0.,0.213646466028285));
#83811=DIRECTION('center_axis',(-6.52173811143766E-14,-1.,-8.09092240879132E-14));
#83812=DIRECTION('ref_axis',(8.66477572707589E-31,8.09092240879132E-14,
-1.));
#83813=DIRECTION('center_axis',(0.133696415542447,-0.987363722324532,-0.085077307835553));
#83814=DIRECTION('ref_axis',(-0.566269257745158,-0.00565888451119376,-0.824200888593817));
#83815=DIRECTION('center_axis',(-0.124079726700196,-0.987363722202752,0.0985753594968428));
#83816=DIRECTION('ref_axis',(-0.627475881044624,0.00111690481182892,-0.778635197785789));
#83817=DIRECTION('center_axis',(-0.119371098919121,0.987363720680323,0.104227749794143));
#83818=DIRECTION('ref_axis',(-0.628531034292203,0.00611303077633138,-0.777760483559239));
#83819=DIRECTION('',(-0.00135546408935191,0.,-0.999999081358129));
#83820=DIRECTION('center_axis',(0.117350660482125,0.98736372201723,-0.106497431559126));
#83821=DIRECTION('ref_axis',(-0.777740498287201,0.0246892582809723,-0.62810043611632));
#83822=DIRECTION('',(0.999999081357214,0.,-0.00135546476457403));
#83823=DIRECTION('center_axis',(1.15836752250586E-14,-1.,9.2854003310176E-15));
#83824=DIRECTION('ref_axis',(1.,1.15836752250587E-14,-1.75048848759714E-31));
#83825=DIRECTION('center_axis',(0.112281561555748,-0.987363722320076,-0.11182902476927));
#83826=DIRECTION('ref_axis',(-0.730209026605619,-0.00565888518529751,-0.683200376523707));
#83827=DIRECTION('center_axis',(-0.0999880263435284,-0.987363722188348,
0.122944193414313));
#83828=DIRECTION('ref_axis',(-0.780189394960913,0.00111690884324557,-0.625542373069291));
#83829=DIRECTION('center_axis',(-0.0941743838306357,0.987363720670641,0.127452220590891));
#83830=DIRECTION('ref_axis',(-0.781031841493226,0.00611303067508159,-0.624461282570558));
#83831=DIRECTION('',(-0.216294019096128,0.,-0.976328273329849));
#83832=DIRECTION('center_axis',(0.0917132677724629,0.987363722001367,-0.129234503868373));
#83833=DIRECTION('ref_axis',(-0.894580384647363,0.0246892584665362,-0.446224580139361));
#83834=DIRECTION('',(0.976328273183796,0.,-0.216294019755396));
#83835=DIRECTION('center_axis',(-3.99268257941694E-14,-1.,-1.97344952052439E-14));
#83836=DIRECTION('ref_axis',(1.,-3.99268257941694E-14,-5.56233456522579E-31));
#83837=DIRECTION('center_axis',(0.0856165443422947,-0.987363722331818,-0.133351742238116));
#83838=DIRECTION('ref_axis',(-0.860005031066307,-0.0056588828079528,-0.510254175471408));
#83839=DIRECTION('center_axis',(-0.0712209911176648,-0.987363722215966,
0.141564298027612));
#83840=DIRECTION('ref_axis',(-0.89642212049867,0.00111690538718566,-0.443199880869823));
#83841=DIRECTION('center_axis',(-0.0645741780897509,0.987363720681666,0.144717167625991));
#83842=DIRECTION('ref_axis',(-0.897012468634678,0.00611303148819058,-0.441962964466419));
#83843=DIRECTION('',(-0.421118902314207,0.,-0.907005441060679));
#83844=DIRECTION('center_axis',(0.0617874672746259,0.98736372193773,-0.145928713723719));
#83845=DIRECTION('ref_axis',(-0.969590686425388,0.024689261332682,-0.243483759565174));
#83846=DIRECTION('',(0.907005440776321,0.,-0.421118902926657));
#83847=DIRECTION('center_axis',(-5.76475892601268E-14,-1.,-1.42533684862447E-14));
#83848=DIRECTION('ref_axis',(1.,-5.76475892601268E-14,4.35334671275454E-32));
#83849=DIRECTION('center_axis',(0.054948198358191,-0.987363722272578,-0.148639077759611));
#83850=DIRECTION('ref_axis',(-0.949588155632919,-0.00565888675938369,-0.313449057555315));
#83851=DIRECTION('center_axis',(-0.0391237430721977,-0.987363722200919,
0.153565011671174));
#83852=DIRECTION('ref_axis',(-0.970739142604666,0.00111690367333193,-0.240133857548958));
#83853=DIRECTION('center_axis',(-0.0319545557613576,0.987363720672074,0.155215300362732));
#83854=DIRECTION('ref_axis',(-0.971049788381102,0.00611303238509471,-0.238798951672898));
#83855=DIRECTION('',(-0.60625273534136,0.,-0.795272042065556));
#83856=DIRECTION('center_axis',(0.0289725463399352,0.987363722037242,-0.155799460728673));
#83857=DIRECTION('ref_axis',(-0.999264006069101,0.0246892567636708,-0.0293579082222947));
#83858=DIRECTION('',(0.795272041985617,0.,-0.606252735446222));
#83859=DIRECTION('center_axis',(0.00215939850788328,0.987363721656155,0.158455729323336));
#83860=DIRECTION('ref_axis',(-0.999681899289745,0.00611320332131533,-0.0244689390370909));
#83861=DIRECTION('',(-0.763038865448691,0.,-0.64635260486423));
#83862=DIRECTION('center_axis',(-1.48409683524321E-14,-1.,-3.8190125160023E-16));
#83863=DIRECTION('ref_axis',(-0.999669073108583,1.48458812538651E-14,-0.0257243905705709));
#83864=DIRECTION('center_axis',(0.0217105298845489,-0.987363722321747,-0.15697621710016));
#83865=DIRECTION('ref_axis',(-0.994769594219394,-0.00565888470389273,-0.101987408244792));
#83866=DIRECTION('center_axis',(-0.00519733342331163,-0.98736372042386,
0.158385199169749));
#83867=DIRECTION('ref_axis',(-0.999665480855963,0.00111712080139465,-0.0258394741845179));
#83868=DIRECTION('',(0.64635260602278,0.,-0.763038864467309));
#83869=DIRECTION('center_axis',(-0.00519709416112407,0.987363722020954,
-0.158385197064655));
#83870=DIRECTION('ref_axis',(-0.982212851051216,0.0246892572281748,0.186140688210189));
#83871=DIRECTION('center_axis',(4.3728276777336E-14,-1.,-8.45219067440875E-15));
#83872=DIRECTION('ref_axis',(1.,4.3728276777336E-14,1.11950809907711E-31));
#83873=DIRECTION('center_axis',(0.0361720401591797,0.987363720696401,0.154286961741046));
#83874=DIRECTION('ref_axis',(-0.981569996660989,0.00611302890590471,0.191005163627955));
#83875=DIRECTION('center_axis',(-0.0125422941873798,-0.987363722266098,
-0.157973323093972));
#83876=DIRECTION('ref_axis',(-0.993436711795227,-0.00565888753205764,0.114243059523927));
#83877=DIRECTION('center_axis',(0.0289725258699401,-0.987363722235349,0.155799463279798));
#83878=DIRECTION('ref_axis',(-0.981848574517903,0.00111690498030995,0.189663199489062));
#83879=DIRECTION('',(-0.88414614515408,0.,-0.467210438677456));
#83880=DIRECTION('center_axis',(-0.0391237251010263,0.987363722063321,-0.153565017134384));
#83881=DIRECTION('ref_axis',(-0.919234514576966,0.0246892565919667,0.392935551737669));
#83882=DIRECTION('',(0.467210440327718,8.7272790084625E-15,-0.88414614428203));
#83883=DIRECTION('center_axis',(9.54075798536309E-14,-1.,-4.1194696781827E-14));
#83884=DIRECTION('ref_axis',(1.,9.54075798536309E-14,-9.10948663397066E-32));
#83885=DIRECTION('center_axis',(-0.0462086638903957,-0.987363722387185,
-0.151583769233998));
#83886=DIRECTION('ref_axis',(-0.945651833071557,-0.0056588799705953,0.325131646700044));
#83887=DIRECTION('center_axis',(0.0617874445083887,-0.987363722220602,0.145928721449209));
#83888=DIRECTION('ref_axis',(-0.918121518951185,0.00111690394803397,0.396297399643676));
#83889=DIRECTION('center_axis',(0.0684934889757973,0.987363720684482,0.142903901430361));
#83890=DIRECTION('ref_axis',(-0.917560972092285,0.00611302340973764,0.397548102042825));
#83891=DIRECTION('',(-0.963911732980681,0.,-0.266222033314638));
#83892=DIRECTION('center_axis',(-0.0712209764537815,0.987363722108156,-0.141564306156951));
#83893=DIRECTION('ref_axis',(-0.813273794121335,0.0246892530481944,0.581357185024329));
#83894=DIRECTION('',(0.266222032663698,0.,-0.963911733160464));
#83895=DIRECTION('center_axis',(2.40918175844038E-14,-1.,-1.73546848866497E-14));
#83896=DIRECTION('ref_axis',(1.,2.40918175844038E-14,-3.61649621631541E-31));
#83897=DIRECTION('center_axis',(-0.077714359735654,-0.987363722361458,-0.138106328802857));
#83898=DIRECTION('ref_axis',(-0.853649325806049,-0.00565888098702445,0.520817439816345));
#83899=DIRECTION('center_axis',(0.0917132479690571,-0.987363722209593,0.129234516331292));
#83900=DIRECTION('ref_axis',(-0.811464122170743,0.00111690621270039,0.584401172954143));
#83901=DIRECTION('center_axis',(0.0976122690732956,0.98736372069769,0.12483880797403));
#83902=DIRECTION('ref_axis',(-0.810647814349427,0.00611302973016654,0.585502136595602));
#83903=DIRECTION('',(-0.998605879960763,-8.72727900573397E-15,-0.0527853815728483));
#83904=DIRECTION('center_axis',(-0.0999880081949315,0.987363722034604,-0.122944209408914));
#83905=DIRECTION('ref_axis',(-0.669285294789748,0.024689256854248,0.742595202498768));
#83906=DIRECTION('',(0.0527853810498718,0.,-0.998605879988407));
#83907=DIRECTION('center_axis',(-8.90901902559685E-14,-1.,9.95758679737192E-14));
#83908=DIRECTION('ref_axis',(-2.44147446982783E-31,-9.95758679737192E-14,
-1.));
#83909=DIRECTION('center_axis',(-0.10558621563704,-0.98736372229164,-0.118171193485749));
#83910=DIRECTION('ref_axis',(-0.721731125798102,-0.00565888635371337,0.69215038760333));
#83911=DIRECTION('center_axis',(0.117350645962308,-0.987363722220967,0.106497445669769));
#83912=DIRECTION('ref_axis',(-0.666863563286744,0.00111690353864807,0.745178998957292));
#83913=DIRECTION('center_axis',(0.122166802887998,0.987363720666353,0.100936392763069));
#83914=DIRECTION('ref_axis',(-0.665829667603348,0.0061130311092627,0.746078738867335));
#83915=DIRECTION('',(-0.986606326510258,0.,0.163119454664165));
#83916=DIRECTION('center_axis',(-0.124079715094384,0.987363722052136,-0.0985753756140405));
#83917=DIRECTION('ref_axis',(-0.494001758384005,0.0246892565635383,0.86911029410763));
#83918=DIRECTION('',(-0.16311945579303,0.,-0.986606326323618));
#83919=DIRECTION('center_axis',(-7.28904920849601E-14,-1.,1.29332885349243E-13));
#83920=DIRECTION('ref_axis',(1.43316139478469E-30,-1.29332885349243E-13,
-1.));
#83921=DIRECTION('center_axis',(-0.128520983646098,-0.987363722346133,-0.0927104986364962));
#83922=DIRECTION('ref_axis',(-0.556065577731079,-0.00565888351541373,0.831119155296014));
#83923=DIRECTION('center_axis',(0.13750085681627,-0.987363722241842,0.0787806726013888));
#83924=DIRECTION('ref_axis',(-0.4910812059078,0.00111690141433312,0.871113082059598));
#83925=DIRECTION('center_axis',(0.141008950102571,0.987363720689102,0.0723143074221373));
#83926=DIRECTION('ref_axis',(-0.489878064606547,0.00611302773077556,0.871769529582966));
#83927=DIRECTION('',(-0.928474157301363,0.,0.371397010251191));
#83928=DIRECTION('center_axis',(-0.142369592250741,0.98736372201826,-0.0695972675081812));
#83929=DIRECTION('ref_axis',(-0.295619249946772,0.024689256796667,0.954986753656686));
#83930=DIRECTION('',(-0.371397010878169,0.,-0.928474157050567));
#83931=DIRECTION('center_axis',(-1.73534422570156E-14,-1.,5.67913822896903E-14));
#83932=DIRECTION('ref_axis',(-1.40571721593363E-31,-5.67913822896903E-14,
-1.));
#83933=DIRECTION('center_axis',(-0.145446250028888,-0.987363722268766,-0.0629147701267425));
#83934=DIRECTION('ref_axis',(-0.364399023979489,-0.0056588873821436,0.931225712873303));
#83935=DIRECTION('center_axis',(0.151221679661245,-0.987363722237896,0.0473802027112372));
#83936=DIRECTION('ref_axis',(-0.292336437731566,0.00111689942938177,0.956314885228753));
#83937=DIRECTION('center_axis',(0.153257678612783,0.98736372068058,0.0403108797971802));
#83938=DIRECTION('ref_axis',(-0.291020309763654,0.00611303139448231,0.956697345116122));
#83939=DIRECTION('',(-0.826927567205339,0.,0.562308455027896));
#83940=DIRECTION('center_axis',(-0.154002425329325,0.987363721965411,-0.0373648703904596));
#83941=DIRECTION('ref_axis',(-0.083413912942098,0.0246892591347644,0.996209094322605));
#83942=DIRECTION('',(-0.562308454249525,-8.72727898606521E-15,-0.826927567734629));
#83943=DIRECTION('center_axis',(-7.1088899461577E-15,-1.,8.87911626056644E-14));
#83944=DIRECTION('ref_axis',(1.8966066488671E-31,-8.87911626056644E-14,
-1.));
#83945=DIRECTION('center_axis',(-0.155570614161056,-0.987363722323422,-0.0301772074451632));
#83946=DIRECTION('ref_axis',(-0.155693573555354,-0.00565888170651582,0.987789192192036));
#83947=DIRECTION('center_axis',(0.157871543355574,-0.987363722242727,0.0137642942978041));
#83948=DIRECTION('ref_axis',(-0.0799223410303271,0.00111690518742693,0.996800467459278));
#83949=DIRECTION('center_axis',(0.15834024654227,0.987363720697898,0.00642256759684789));
#83950=DIRECTION('ref_axis',(-0.0785547654154159,0.00611302663392469,0.996891057104989));
#83951=DIRECTION('',(-0.686714765840337,0.,0.726926977334623));
#83952=DIRECTION('',(0.760873717902008,0.,-0.648899981049449));
#83953=DIRECTION('center_axis',(0.158420670951937,-0.987363721845357,0.00397137241051485));
#83954=DIRECTION('ref_axis',(-0.18204302254892,-0.0252547793770049,0.982966191717636));
#83955=DIRECTION('',(0.470163700157015,0.,0.882579228769103));
#83956=DIRECTION('center_axis',(1.66119026794183E-14,-1.,-8.75125797881804E-14));
#83957=DIRECTION('ref_axis',(5.50379459184303E-31,8.75125797881804E-14,
-1.));
#83958=DIRECTION('center_axis',(0.150470357297638,0.987363722706508,0.0497146925754033));
#83959=DIRECTION('ref_axis',(-0.116797137708958,-0.0321806451053153,0.992634290513682));
#83960=DIRECTION('center_axis',(-0.156018993570792,0.987363721745411,-0.027766069693188));
#83961=DIRECTION('ref_axis',(-0.186683316697925,-0.00187190037319769,0.982418360605936));
#83962=DIRECTION('',(0.882579228239459,0.,-0.470163701151249));
#83963=DIRECTION('center_axis',(0.153863155238695,-0.987363721900371,0.0379342870638276));
#83964=DIRECTION('ref_axis',(-0.389095632825037,-0.025254777427565,0.920851119743886));
#83965=DIRECTION('',(0.269443091726455,0.,0.963016313631752));
#83966=DIRECTION('center_axis',(2.33574289875519E-14,-1.,-5.45970109405145E-14));
#83967=DIRECTION('ref_axis',(-2.57995956160863E-31,5.45970109405145E-14,
-1.));
#83968=DIRECTION('center_axis',(0.136265253013163,0.987363722600581,0.0808990736262259));
#83969=DIRECTION('ref_axis',(-0.327453516387912,-0.0321806493677835,0.944319120007352));
#83970=DIRECTION('center_axis',(-0.146402464080743,0.987363721985126,-0.0606564013008222));
#83971=DIRECTION('ref_axis',(-0.393509674167322,-0.00187188349778186,0.919318569587768));
#83972=DIRECTION('',(0.963016313438966,0.,-0.269443092415491));
#83973=DIRECTION('center_axis',(0.142111166557216,-0.987363722011711,0.0701234396969183));
#83974=DIRECTION('ref_axis',(-0.577954565812851,-0.025254771821771,0.815678071518604));
#83975=DIRECTION('',(0.0561236183417539,0.,0.998423827572354));
#83976=DIRECTION('center_axis',(-5.18221330477079E-14,-1.,7.24491094435913E-14));
#83977=DIRECTION('ref_axis',(-2.76296851101971E-30,-7.24491094435913E-14,
-1.));
#83978=DIRECTION('center_axis',(0.115688539590078,0.987363722702905,0.108300696663393));
#83979=DIRECTION('ref_axis',(-0.52279853179565,-0.0321806458123467,0.851848637486387));
#83980=DIRECTION('center_axis',(-0.129940334586113,0.987363721716063,-0.0907104761681578));
#83981=DIRECTION('ref_axis',(-0.581935951137064,-0.00187190178823612,0.813232466615725));
#83982=DIRECTION('',(0.99842382757567,0.,-0.0561236182827579));
#83983=DIRECTION('center_axis',(0.123714223149916,-0.987363721940037,0.0990336891523768));
#83984=DIRECTION('ref_axis',(-0.739788982046662,-0.0252547764804811,0.672364825304897));
#83985=DIRECTION('',(-0.159820128826896,0.,0.987146152513271));
#83986=DIRECTION('center_axis',(4.41233181953626E-14,-1.,-3.97433751604223E-14));
#83987=DIRECTION('ref_axis',(1.,4.41233181953626E-14,-2.15831669479006E-30));
#83988=DIRECTION('center_axis',(0.0897023546228915,0.987363722634468,0.130638305257357));
#83989=DIRECTION('ref_axis',(-0.693698068926603,-0.0321806495628235,0.719546659335735));
#83990=DIRECTION('center_axis',(-0.107402316178315,0.987363721994519,-0.116523057669561));
#83991=DIRECTION('ref_axis',(-0.743151555138497,-0.00187188370506456,0.669120513918553));
#83992=DIRECTION('',(0.987146152503824,0.,0.159820128885249));
#83993=DIRECTION('center_axis',(0.0995325402727104,-0.987363721842449,0.123313236176365));
#83994=DIRECTION('ref_axis',(-0.867031688858854,-0.0252547794111912,0.497612546698187));
#83995=DIRECTION('',(-0.368290866546792,0.,0.929710620364322));
#83996=DIRECTION('center_axis',(-7.74530857502545E-14,-1.,4.39934820937403E-14));
#83997=DIRECTION('ref_axis',(1.,-7.74530857502545E-14,-1.3738948908618E-30));
#83998=DIRECTION('center_axis',(0.0595217899121446,0.987363722621448,0.146867408831129));
#83999=DIRECTION('ref_axis',(-0.832161056395907,-0.0321806488996472,0.553599478011356));
#84000=DIRECTION('center_axis',(-0.0798422942999397,0.987363721988568,-0.13688713797068));
#84001=DIRECTION('ref_axis',(-0.86961821732428,-0.00187188122784259,0.493721229195595));
#84002=DIRECTION('',(0.929710620732484,0.,0.368290865617407));
#84003=DIRECTION('center_axis',(0.0706968232391802,-0.987363721882445,0.141826795403174));
#84004=DIRECTION('ref_axis',(-0.953732957852313,-0.0252547784065486,0.299592458639924));
#84005=DIRECTION('',(-0.559540732515555,0.,0.828802852707419));
#84006=DIRECTION('center_axis',(8.50995737247474E-14,-1.,-2.63148149472303E-14));
#84007=DIRECTION('ref_axis',(1.,8.50995737247474E-14,-4.61162654382223E-31));
#84008=DIRECTION('center_axis',(0.0265580544804943,0.987363722702226,0.15622915487774));
#84009=DIRECTION('ref_axis',(-0.931713116916154,-0.032180646225258,0.361766601242998));
#84010=DIRECTION('center_axis',(-0.0485489594157441,0.987363721707236,-0.150850520702069));
#84011=DIRECTION('ref_axis',(-0.955422495320087,-0.00187190327627904,0.295236094362568));
#84012=DIRECTION('',(0.828802852674343,0.,0.559540732564549));
#84013=DIRECTION('center_axis',(0.0385554032256785,-0.987363721881548,0.153708690692241));
#84014=DIRECTION('ref_axis',(-0.995838733942716,-0.0252547794232253,0.0875637601731004));
#84015=DIRECTION('',(-0.724627094472956,0.,0.689141185792637));
#84016=DIRECTION('center_axis',(0.,-1.,0.));
#84017=DIRECTION('ref_axis',(0.,0.,-1.));
#84018=DIRECTION('center_axis',(-0.00764751234414346,0.987363722585381,
0.158285801249784));
#84019=DIRECTION('ref_axis',(-0.987699307272752,-0.0321806505023496,0.15301792099676));
#84020=DIRECTION('center_axis',(-0.014985482612071,0.987363722043209,-0.157760310927254));
#84021=DIRECTION('ref_axis',(-0.996552281853689,-0.00187187734051423,0.0829460403360414));
#84022=DIRECTION('',(0.689141185749805,0.,0.724627094513691));
#84023=DIRECTION('center_axis',(0.00461117065540764,-0.98736372194356,0.15840333864836));
#84024=DIRECTION('ref_axis',(-0.991380197761653,-0.0252547757806465,-0.128559323996106));
#84025=DIRECTION('',(-0.855830699792882,0.,0.517256042296294));
#84026=DIRECTION('center_axis',(5.88557235901373E-14,-1.,7.89980289289736E-15));
#84027=DIRECTION('ref_axis',(1.,5.88557235901373E-14,7.28864359769959E-32));
#84028=DIRECTION('center_axis',(-0.041495480880162,0.987363722713628,0.152941178678636));
#84029=DIRECTION('ref_axis',(-0.997501776374992,-0.0321806452263054,-0.0628857074505336));
#84030=DIRECTION('center_axis',(0.0192786467163599,0.987363721692677,-0.157293403758615));
#84031=DIRECTION('ref_axis',(-0.991084390577787,-0.00187190395811225,-0.133222470809653));
#84032=DIRECTION('',(0.51725604351836,0.,0.855830699054277));
#84033=DIRECTION('center_axis',(-0.0295486717052587,-0.987363721972233,
0.15569122176152));
#84034=DIRECTION('ref_axis',(-0.940565825156794,-0.0252547754165295,-0.338671116078387));
#84035=DIRECTION('',(-0.947016612388295,0.,0.321184582227414));
#84036=DIRECTION('center_axis',(1.11562970629401E-13,-1.,4.07347013544332E-14));
#84037=DIRECTION('ref_axis',(1.,1.11562970629401E-13,1.53052459812118E-30));
#84038=DIRECTION('center_axis',(-0.0734031763791204,0.987363722626315,0.14044519549974));
#84039=DIRECTION('ref_axis',(-0.960662170736016,-0.0321806497949105,-0.275848870752705));
#84040=DIRECTION('center_axis',(0.0526413731130204,0.987363721985208,-0.149471623876552));
#84041=DIRECTION('ref_axis',(-0.939274493787547,-0.00187188437303119,-0.343161654864061));
#84042=DIRECTION('',(0.321184582171429,0.,0.947016612407282));
#84043=DIRECTION('center_axis',(-0.0623268523181122,-0.987363721967415,
0.145699155875284));
#84044=DIRECTION('ref_axis',(-0.845771638811263,-0.0252547739760518,-0.532947024922674));
#84045=DIRECTION('',(-0.993921081291667,0.,0.110094887092924));
#84046=DIRECTION('center_axis',(7.51484503470179E-14,-1.,4.78238157380566E-14));
#84047=DIRECTION('ref_axis',(1.,7.51484503470179E-14,1.09517870617567E-30));
#84048=DIRECTION('center_axis',(-0.101878612836726,0.987363722718883,0.121382153981436));
#84049=DIRECTION('ref_axis',(-0.878903069713223,-0.0321806454471711,-0.47591364774219));
#84050=DIRECTION('center_axis',(0.0835426327950051,0.9873637220322,-0.13466071780738));
#84051=DIRECTION('ref_axis',(-0.843545165481614,-0.0018718784691315,-0.537054978436652));
#84052=DIRECTION('',(0.110094884194222,0.,0.993921081612751));
#84053=DIRECTION('center_axis',(-0.0921906923225379,-0.987363721856517,
0.12889436376637));
#84054=DIRECTION('ref_axis',(-0.711430113097762,-0.0252547796932717,-0.70230291917402));
#84055=DIRECTION('',(-0.994350904942001,0.,-0.106142723919367));
#84056=DIRECTION('center_axis',(0.,-1.,0.));
#84057=DIRECTION('ref_axis',(0.,0.,-1.));
#84058=DIRECTION('center_axis',(-0.125590323972974,0.987363722658854,0.0966434152004877));
#84059=DIRECTION('ref_axis',(-0.756047438066,-0.0321806473676782,-0.653725230757415));
#84060=DIRECTION('center_axis',(0.110537521524331,0.98736372195806,-0.113553233755737));
#84061=DIRECTION('ref_axis',(-0.708372604320887,-0.0018718853427728,-0.705836205852964));
#84062=DIRECTION('',(-0.106142721135687,0.,0.994350905239147));
#84063=DIRECTION('center_axis',(-0.117743802252636,-0.987363721835322,0.106062612802972));
#84064=DIRECTION('ref_axis',(-0.543822905209596,-0.0252547813062237,-0.838819911417564));
#84065=DIRECTION('',(-0.948285986047789,0.,-0.317417215452112));
#84066=DIRECTION('center_axis',(-4.81221873529243E-14,-1.,-7.49577349565336E-14));
#84067=DIRECTION('ref_axis',(8.50838497286474E-31,7.49577349565336E-14,
-1.));
#84068=DIRECTION('center_axis',(-0.143429568776544,0.987363722694744,0.0673857396408982));
#84069=DIRECTION('ref_axis',(-0.597839867781445,-0.0321806459674356,-0.800969349298825));
#84070=DIRECTION('center_axis',(0.132363804610462,0.987363721967653,-0.0871361220804899));
#84071=DIRECTION('ref_axis',(-0.54007732666416,-0.00187188474904035,-0.841613318140095));
#84072=DIRECTION('',(-0.317417216373473,0.,0.948285985739384));
#84073=DIRECTION('center_axis',(-0.13779134681076,-0.987363721977672,0.0782714843763365));
#84074=DIRECTION('ref_axis',(-0.350787141703557,-0.0252547743292595,-0.936114617762711));
#84075=DIRECTION('',(-0.857880267877045,0.,-0.513849633635376));
#84076=DIRECTION('center_axis',(-3.08834200477059E-14,-1.,-8.35501124920039E-14));
#84077=DIRECTION('ref_axis',(1.60869207676635E-30,8.35501124920039E-14,
-1.));
#84078=DIRECTION('center_axis',(-0.154562208249242,0.987363722638654,0.0349771782489369));
#84079=DIRECTION('ref_axis',(-0.411677971069692,-0.0321806490103536,-0.910761030109004));
#84080=DIRECTION('center_axis',(0.148000904439035,0.987363722001869,-0.0566446181013166));
#84081=DIRECTION('ref_axis',(-0.346528631681396,-0.00187188022074965,-0.938037527761794));
#84082=DIRECTION('',(-0.513849635801822,0.,0.857880266579396));
#84083=DIRECTION('center_axis',(-0.151395917147904,-0.987363721934246,0.0468204749986269));
#84084=DIRECTION('ref_axis',(-0.141348960074115,-0.0252547755188113,-0.989637644696007));
#84085=DIRECTION('',(-0.727361020504471,0.,-0.686255015173438));
#84086=DIRECTION('center_axis',(-1.22005783802258E-14,-1.,-8.82357797049569E-14));
#84087=DIRECTION('ref_axis',(-4.66197082555383E-32,8.82357797049569E-14,
-1.));
#84088=DIRECTION('center_axis',(-0.158467688440811,0.987363722742502,0.00093313037385869));
#84089=DIRECTION('ref_axis',(-0.206266469571198,-0.0321806438930113,-0.977966538123501));
#84090=DIRECTION('center_axis',(0.156717643448514,0.987363722017604,-0.0235044820297946));
#84091=DIRECTION('ref_axis',(-0.13677664582851,-0.00187188330714621,-0.990600143957584));
#84092=DIRECTION('',(-0.686255015216422,0.,0.727361020463916));
#84093=DIRECTION('center_axis',(-0.157921382952396,-0.987363721842888,0.0131801970760088));
#84094=DIRECTION('ref_axis',(0.0746985365481363,-0.0252547807219919,-0.996886314826446));
#84095=DIRECTION('',(-0.562831181859169,0.,-0.826571872692878));
#84096=DIRECTION('center_axis',(2.35091625679143E-15,-1.,-2.95985466508887E-14));
#84097=DIRECTION('ref_axis',(1.73983611715488E-32,2.95985466508887E-14,
-1.));
#84098=DIRECTION('center_axis',(-0.154963397163266,0.987363722655173,-0.0331545581200833));
#84099=DIRECTION('ref_axis',(0.00878982263912512,-0.0321806476884021,-0.999443417574165));
#84100=DIRECTION('center_axis',(0.158106440926136,0.987363722001472,0.0107347013498738));
#84101=DIRECTION('ref_axis',(0.0793708644578278,-0.00187188233847563,-0.996843398900614));
#84102=DIRECTION('',(-0.826571873636816,0.,0.562831180472905));
#84103=DIRECTION('center_axis',(-0.157062621681397,-0.987363721823588,-0.0210763777067678));
#84104=DIRECTION('ref_axis',(0.287253218042712,-0.0252547811743122,-0.957521688919861));
#84105=DIRECTION('',(-0.371983982078545,0.,-0.928239148644889));
#84106=DIRECTION('center_axis',(0.,-1.,0.));
#84107=DIRECTION('ref_axis',(0.,0.,-1.));
#84108=DIRECTION('center_axis',(-0.144213189672392,0.987363722716302,-0.0656919705011265));
#84109=DIRECTION('ref_axis',(0.223435111451264,-0.0321806456465352,-0.974187434232516));
#84110=DIRECTION('center_axis',(0.152102356220726,0.987363722015024,0.0444719426238749));
#84111=DIRECTION('ref_axis',(0.291807083291674,-0.00187188102446143,-0.956475364137643));
#84112=DIRECTION('',(-0.928239148269088,0.,0.37198398301631));
#84113=DIRECTION('center_axis',(-0.148859783533753,-0.987363721980219,-0.0543474503877802));
#84114=DIRECTION('ref_axis',(0.486376257462539,-0.0252547747120306,-0.87338441280514));
#84115=DIRECTION('',(-0.163743224263631,0.,-0.986502993663856));
#84116=DIRECTION('center_axis',(4.3685222893723E-14,-1.,-7.76273678386911E-14));
#84117=DIRECTION('ref_axis',(-1.1971649917518E-30,7.7627367838691E-14,-1.));
#84118=DIRECTION('center_axis',(-0.126719731067538,0.987363722569715,-0.0951577065268265));
#84119=DIRECTION('ref_axis',(0.42763282427826,-0.03218065124485,-0.903379528927491));
#84120=DIRECTION('center_axis',(0.138986134009488,0.987363722017502,0.0761297247915765));
#84121=DIRECTION('ref_axis',(0.490598724984633,-0.00187187968910189,-0.871383605027018));
#84122=DIRECTION('',(-0.986502993673533,0.,0.163743224205332));
#84123=DIRECTION('center_axis',(-0.133696433187651,-0.987363721844637,-0.0850772856760678));
#84124=DIRECTION('ref_axis',(0.662756881152128,-0.0252547807035617,-0.748408653435487));
#84125=DIRECTION('',(0.05215398216031,0.,-0.998639054986746));
#84126=DIRECTION('center_axis',(5.93514761815451E-14,-1.,-6.64214516128926E-14));
#84127=DIRECTION('ref_axis',(-2.33646575295403E-30,6.64214516128926E-14,
-1.));
#84128=DIRECTION('center_axis',(-0.103301005449085,0.987363722780521,-0.120173962280518));
#84129=DIRECTION('ref_axis',(0.61183490179735,-0.0321806428555542,-0.790330601184106));
#84130=DIRECTION('center_axis',(0.119371077060778,0.987363721991977,0.104227762402829));
#84131=DIRECTION('ref_axis',(0.666450517002388,-0.00187188279882516,-0.745546916325215));
#84132=DIRECTION('',(-0.998639054975845,0.,-0.0521539823690436));
#84133=DIRECTION('center_axis',(-0.112281580436837,-0.987363721918056,-0.111829009361297));
#84134=DIRECTION('ref_axis',(0.808147731523845,-0.0252547770532661,-0.588438136314136));
#84135=DIRECTION('',(0.265612528541422,0.,-0.964079864265317));
#84136=DIRECTION('center_axis',(-4.81616801158825E-14,-1.,3.47398279347916E-14));
#84137=DIRECTION('ref_axis',(1.,-4.81616801158825E-14,1.80701700499117E-30));
#84138=DIRECTION('center_axis',(-0.0750520328090775,0.987363722700972,-0.139571026596869));
#84139=DIRECTION('ref_axis',(0.767428259443635,-0.0321806464379674,-0.640326692089395));
#84140=DIRECTION('center_axis',(0.0941743565718948,0.987363722016492,0.127452230306137));
#84141=DIRECTION('ref_axis',(0.811139823184763,-0.00187187906711774,-0.584849282561371));
#84142=DIRECTION('',(-0.964079864249621,0.,-0.265612528598395));
#84143=DIRECTION('center_axis',(-0.0856165686441856,-0.987363721901408,
-0.133351729822281));
#84144=DIRECTION('ref_axis',(0.915750492197764,-0.0252547777773986,-0.400952905263157));
#84145=DIRECTION('',(0.466651329562723,0.,-0.884441369802059));
#84146=DIRECTION('center_axis',(-5.45037230112074E-14,-1.,2.35742925329346E-14));
#84147=DIRECTION('ref_axis',(1.,-5.45037230112074E-14,7.87519646691859E-31));
#84148=DIRECTION('center_axis',(-0.0432937091944434,0.987363722575924,-0.152441903967382));
#84149=DIRECTION('ref_axis',(0.887137525153124,-0.0321806502956287,-0.460381816769234));
#84150=DIRECTION('center_axis',(0.0645741461488577,0.987363722058241,0.144717172486346));
#84151=DIRECTION('ref_axis',(0.917901132754908,-0.00187187453050333,-0.396804746157349));
#84152=DIRECTION('',(-0.884441369774467,0.,-0.466651329615018));
#84153=DIRECTION('center_axis',(-0.0549482167247938,-0.987363721999776,
-0.14863907278207));
#84154=DIRECTION('ref_axis',(0.980533777242356,-0.0252547735855317,-0.194719562699746));
#84155=DIRECTION('',(0.645870029654509,0.,-0.763447381811009));
#84156=DIRECTION('center_axis',(-5.82972322439759E-14,-1.,1.1306449337716E-14));
#84157=DIRECTION('ref_axis',(1.,-5.82972322439759E-14,1.18982867353277E-31));
#84158=DIRECTION('center_axis',(-0.009511024359043,0.987363722641755,-0.158184764205208));
#84159=DIRECTION('ref_axis',(0.965365224232181,-0.0321806492226432,-0.258910003010234));
#84160=DIRECTION('center_axis',(0.0319545315579717,0.987363721993611,0.155215296938911));
#84161=DIRECTION('ref_axis',(0.981742405061269,-0.00187188183297512,-0.190206062371624));
#84162=DIRECTION('',(-0.7634473805736,0.,-0.645870031117181));
#84163=DIRECTION('',(0.794888567218867,0.,-0.606755441429854));
#84164=DIRECTION('',(-0.606755441382878,0.,-0.794888567254724));
#84165=DIRECTION('center_axis',(0.0125422740500174,-0.987363721949525,-0.157973326671421));
#84166=DIRECTION('ref_axis',(0.971668976639003,-0.0252547754455921,0.234992757663944));
#84167=DIRECTION('',(0.906738999989211,0.,-0.421692288165868));
#84168=DIRECTION('center_axis',(-2.88282949215819E-14,-1.,-7.10845848220289E-15));
#84169=DIRECTION('ref_axis',(1.,-2.88282949215819E-14,-2.26654765156684E-31));
#84170=DIRECTION('center_axis',(0.0577880837148793,0.987363722691916,-0.147558180025793));
#84171=DIRECTION('ref_axis',(0.98485523721207,-0.0321806462577187,0.170365981763946));
#84172=DIRECTION('center_axis',(-0.0361720451932298,0.987363721719128,0.15428695401586));
#84173=DIRECTION('ref_axis',(0.970870728505734,-0.00187190160635395,0.239596587027282));
#84174=DIRECTION('',(-0.421692289376655,0.,-0.906738999426117));
#84175=DIRECTION('center_axis',(0.0462086355117911,-0.987363721864621,-0.151583781288707));
#84176=DIRECTION('ref_axis',(0.89843539973103,-0.0252547783768751,0.438378864316335));
#84177=DIRECTION('',(0.976191322337168,0.,-0.216911277239362));
#84178=DIRECTION('center_axis',(7.98785909856274E-14,-1.,3.94184938248821E-14));
#84179=DIRECTION('ref_axis',(1.,7.98785909856274E-14,1.35351838227383E-30));
#84180=DIRECTION('center_axis',(0.0881576752423758,0.987363722731961,-0.131685623090541));
#84181=DIRECTION('ref_axis',(0.925206219006397,-0.0321806438492019,0.378097683771452));
#84182=DIRECTION('center_axis',(-0.0684935153894493,0.987363722021412,0.142903879533128));
#84183=DIRECTION('ref_axis',(0.896666124993326,-0.00187188095421391,0.442703463224704));
#84184=DIRECTION('',(-0.216911277181653,0.,-0.976191322349991));
#84185=DIRECTION('center_axis',(0.0777143366891166,-0.987363721914026,-0.138106344970288));
#84186=DIRECTION('ref_axis',(0.783191980717488,-0.0252547770838744,0.621266865021998));
#84187=DIRECTION('',(0.999998024453727,0.,-0.00198773455025544));
#84188=DIRECTION('center_axis',(-4.6358175241323E-14,-1.,-3.71122980948279E-14));
#84189=DIRECTION('ref_axis',(1.,-4.6358175241323E-14,6.22213030087365E-31));
#84190=DIRECTION('center_axis',(0.11440511685421,0.987363722685258,-0.10965558974664));
#84191=DIRECTION('ref_axis',(0.822295585228745,-0.0321806472280121,0.568149959480154));
#84192=DIRECTION('center_axis',(-0.0976122826722845,0.987363722002558,0.12483878702055));
#84193=DIRECTION('ref_axis',(0.780534411660532,-0.00187188378597566,0.625110012929596));
#84194=DIRECTION('',(-0.00198773449113936,0.,-0.999998024453845));
#84195=DIRECTION('center_axis',(0.105586197529413,-0.987363721824817,-0.118171213565425));
#84196=DIRECTION('ref_axis',(0.631327377166835,-0.0252547813377562,0.775105114716209));
#84197=DIRECTION('',(0.977045930400975,0.,0.213028753662255));
#84198=DIRECTION('center_axis',(5.59444497098018E-14,-1.,6.93154057869814E-14));
#84199=DIRECTION('ref_axis',(2.356099361098E-30,-6.93154057869814E-14,-1.));
#84200=DIRECTION('center_axis',(0.135303100940913,0.987363722605909,-0.0824981827531636));
#84201=DIRECTION('ref_axis',(0.680935325332856,-0.0321806500350066,0.731636172203891));
#84202=DIRECTION('center_axis',(-0.122166801575977,0.987363721726155,0.100936383984035));
#84203=DIRECTION('ref_axis',(0.627905778710353,-0.00187189998213551,0.778287112223119));
#84204=DIRECTION('',(0.213028754318377,0.,-0.977045930257918));
#84205=DIRECTION('center_axis',(0.128520970701227,-0.987363721876118,-0.0927105215871122));
#84206=DIRECTION('ref_axis',(0.449942604776546,-0.0252547776970041,0.89270031287682));
#84207=DIRECTION('',(0.908408255110064,0.,0.418084252331859));
#84208=DIRECTION('center_axis',(2.64904908668139E-14,-1.,5.31475021130798E-14));
#84209=DIRECTION('ref_axis',(-1.34265684866501E-30,-5.31475021130798E-14,
-1.));
#84210=DIRECTION('center_axis',(0.149874459411184,0.987363722638236,-0.051483255862173));
#84211=DIRECTION('ref_axis',(0.507735286740845,-0.0321806480468414,0.860911891246414));
#84212=DIRECTION('center_axis',(-0.141008954760601,0.987363721981079,0.072314280698864));
#84213=DIRECTION('ref_axis',(0.44591696457479,-0.00187188353848564,0.895072375149867));
#84214=DIRECTION('',(0.418084253477456,0.,-0.908408254582816));
#84215=DIRECTION('center_axis',(0.145446242924412,-0.987363721883228,-0.0629147926013606));
#84216=DIRECTION('ref_axis',(0.24751901900161,-0.0252547786965402,0.968553835047629));
#84217=DIRECTION('',(0.797294417685632,0.,0.603590599270175));
#84218=DIRECTION('center_axis',(-2.16690239643906E-14,-1.,-8.63994232246378E-14));
#84219=DIRECTION('ref_axis',(2.20896652263452E-31,8.63994232246378E-14,
-1.));
#84220=DIRECTION('center_axis',(0.157437855437323,0.987363722701675,-0.0180610289846971));
#84221=DIRECTION('ref_axis',(0.310794110370792,-0.032180646490395,0.949932327563542));
#84222=DIRECTION('center_axis',(-0.153257677595432,0.987363722047016,0.0403108501959122));
#84223=DIRECTION('ref_axis',(0.243077569452302,-0.00187187794105808,0.970005047049826));
#84224=DIRECTION('',(0.603590599317295,0.,-0.79729441764996));
#84225=DIRECTION('center_axis',(0.155570611632627,-0.98736372193401,-0.0301772332209221));
#84226=DIRECTION('ref_axis',(0.0335217173615916,-0.0252547750561712,0.999118857194674));
#84227=DIRECTION('',(0.648899979430102,0.,0.760873719283045));
#84228=DIRECTION('center_axis',(1.72606145034788E-15,-1.,5.93584349259378E-14));
#84229=DIRECTION('ref_axis',(0.029066335084342,5.93835253667814E-14,0.999577484822845));
#84230=DIRECTION('center_axis',(0.15763963336802,0.987363722676915,0.0162057129797262));
#84231=DIRECTION('ref_axis',(0.0993205454413462,-0.0321806464481439,0.994534984426095));
#84232=DIRECTION('center_axis',(-0.158340239529387,0.987363722011668,0.00642253852005476));
#84233=DIRECTION('ref_axis',(0.0288721401833863,-0.00187188181618428,0.999581360160191));
#84234=DIRECTION('center_axis',(-0.163785815689771,-0.986495109135139,-0.00126737180284747));
#84235=DIRECTION('ref_axis',(0.0274586618280204,-0.00584312233850029,0.999605862233687));
#84236=DIRECTION('center_axis',(0.161633025665585,-0.98649510926358,-0.026498385106));
#84237=DIRECTION('ref_axis',(0.137216842249404,-0.00412443690745434,0.990532446325358));
#84238=DIRECTION('center_axis',(-0.16022904283391,-0.986495109287375,0.0339713582981242));
#84239=DIRECTION('ref_axis',(0.241702398635757,-0.00584313045738827,0.97033283378446));
#84240=DIRECTION('center_axis',(0.152157765743994,-0.986495109271346,-0.0606251903709286));
#84241=DIRECTION('ref_axis',(0.34694398407328,-0.00412443715934191,0.937876783449446));
#84242=DIRECTION('center_axis',(-0.149180137288371,-0.986495109329304,0.0676216378682646));
#84243=DIRECTION('ref_axis',(0.444644406204661,-0.00584312659425322,0.895688120889469));
#84244=DIRECTION('center_axis',(0.135567778586396,-0.986495109306673,-0.0919172275646138));
#84245=DIRECTION('ref_axis',(0.540448409869318,-0.00412443587822252,0.84136704552675));
#84246=DIRECTION('center_axis',(-0.131155737577983,-0.986495109243889,0.0981099991757331));
#84247=DIRECTION('ref_axis',(0.626795335741588,-0.00584312953040013,0.779162027392173));
#84248=DIRECTION('center_axis',(0.11263879340883,-0.986495109254255,-0.118911318371457));
#84249=DIRECTION('ref_axis',(0.708682071585451,-0.00412443451684314,0.705515917930468));
#84250=DIRECTION('center_axis',(-0.106998637769328,-0.986495109310485,0.124010849614069));
#84251=DIRECTION('ref_axis',(0.77963801399506,-0.00584312763501283,0.62620318187732));
#84252=DIRECTION('center_axis',(0.0844429366349232,-0.986495109286381,-0.140345252169501));
#84253=DIRECTION('ref_axis',(0.843778545533548,-0.00412444154263402,0.536675651654937));
#84254=DIRECTION('center_axis',(-0.0778384024322776,-0.986495109326809,
0.14411308886107));
#84255=DIRECTION('ref_axis',(0.896025684448892,-0.00584312812733907,0.443963771789526));
#84256=DIRECTION('center_axis',(0.0522986285574558,-0.986495109283444,-0.155216792940887));
#84257=DIRECTION('ref_axis',(0.939420873422059,-0.00412443980772976,0.342741026979858));
#84258=DIRECTION('center_axis',(-0.0450385345604746,-0.986495109243706,
0.157476759691369));
#84259=DIRECTION('ref_axis',(0.970516188902198,-0.00584313285570177,0.240965111327725));
#84260=DIRECTION('center_axis',(0.0177088989246973,-0.986495109263363,-0.162830569299322));
#84261=DIRECTION('ref_axis',(0.991136924909274,-0.00412443418164394,0.132780213601537));
#84262=DIRECTION('center_axis',(-0.0101327025402808,-0.986495109345221,
0.163476994030326));
#84263=DIRECTION('ref_axis',(0.999626435896561,-0.00584312539720088,0.0266991861735747));
#84264=DIRECTION('center_axis',(-0.017708886231778,-0.986495109292058,-0.16283057050591));
#84265=DIRECTION('ref_axis',(0.996508515296202,-0.00412443589834953,-0.0833892557268596));
#84266=DIRECTION('center_axis',(0.0252469101078213,-0.986495109231266,0.161833225861687));
#84267=DIRECTION('ref_axis',(0.981995261046375,-0.0058431313974677,-0.188815161197225));
#84268=DIRECTION('center_axis',(-0.0522986199379418,-0.986495109270012,
-0.155216795930509));
#84269=DIRECTION('ref_axis',(0.955284475706084,-0.00412443434778573,-0.295659533105672));
#84270=DIRECTION('center_axis',(0.0594460085246589,-0.986495109207122,0.152622316785305));
#84271=DIRECTION('ref_axis',(0.918447080136415,-0.00584313396351778,-0.395500719056714));
#84272=DIRECTION('center_axis',(-0.0844429344225918,-0.986495109307054,
-0.140345253355305));
#84273=DIRECTION('ref_axis',(0.869392394054461,-0.00412443895913273,-0.494105104369026));
#84274=DIRECTION('center_axis',(0.0908654815661706,-0.986495109203758,0.136274956528388));
#84275=DIRECTION('ref_axis',(0.811953333948451,-0.00584313273512341,-0.583693105398577));
#84276=DIRECTION('center_axis',(-0.112638782506712,-0.986495109231985,-0.118911328883243));
#84277=DIRECTION('ref_axis',(0.742848493168704,-0.00412443353133674,-0.669446865139445));
#84278=DIRECTION('center_axis',(0.118036188482337,-0.986495109330825,0.11355552595504));
#84279=DIRECTION('ref_axis',(0.667493552315554,-0.00584312610117444,-0.744592650712138));
#84280=DIRECTION('center_axis',(-0.135567769450099,-0.986495109256,-0.0919172415834949));
#84281=DIRECTION('ref_axis',(0.581569820465018,-0.00412443070425866,-0.81348603736982));
#84282=DIRECTION('center_axis',(0.139687648469892,-0.986495109284145,0.0855263715085294));
#84283=DIRECTION('ref_axis',(0.491822512892929,-0.00584312859394028,-0.870675871757061));
#84284=DIRECTION('center_axis',(-0.152157762777686,-0.986495109280063,-0.0606251976739593));
#84285=DIRECTION('ref_axis',(0.393097587747994,-0.00412443771534683,-0.919487506995196));
#84286=DIRECTION('center_axis',(0.154807469423525,-0.986495109257913,0.0534981010962386));
#84287=DIRECTION('ref_axis',(0.293154401945519,-0.00584313246842049,-0.956047255329422));
#84288=DIRECTION('center_axis',(-0.161633024216978,-0.986495109294656,-0.0264983927851836));
#84289=DIRECTION('ref_axis',(0.186244550464229,-0.00412443791836214,-0.982494761530175));
#84290=DIRECTION('center_axis',(0.162688667483946,-0.986495109300973,0.0189683103506619));
#84291=DIRECTION('ref_axis',(0.0807787151376006,-0.00584312744504146,-0.996714932687566));
#84292=DIRECTION('center_axis',(-0.163550504854883,-0.986495109300725,0.00886745101275484));
#84293=DIRECTION('ref_axis',(-0.0293170730888086,-0.00412444202667359,-0.999561653027703));
#84294=DIRECTION('center_axis',(0.162962722649296,-0.986495109321913,-0.0164484136218403));
#84295=DIRECTION('ref_axis',(-0.135374094935768,-0.00584312658610667,-0.990777327300146));
#84296=DIRECTION('center_axis',(-0.157820545741235,-0.986495109287338,0.0438186569180516));
#84297=DIRECTION('ref_axis',(-0.243507866879218,-0.00412443949873136,-0.969890152422817));
#84298=DIRECTION('center_axis',(0.155616822593042,-0.986495109297829,-0.0510960258484943));
#84299=DIRECTION('ref_axis',(-0.34519696219726,-0.00584312798122105,-0.938512075119536));
#84300=DIRECTION('center_axis',(-0.144711073722153,-0.986495109289193,0.076720952097095));
#84301=DIRECTION('ref_axis',(-0.446312499512019,-0.00412443849907849,-0.894867667192419));
#84302=DIRECTION('center_axis',(0.140994452051794,-0.986495109320717,-0.0833544466535578));
#84303=DIRECTION('ref_axis',(-0.53887880255101,-0.00584312705756995,-0.842363041703148));
#84304=DIRECTION('center_axis',(-0.124835075987998,-0.986495109277208,0.106035857968992));
#84305=DIRECTION('ref_axis',(-0.628248057932132,-0.00412443289639802,-0.778002163723076));
#84306=DIRECTION('center_axis',(0.119779342921941,-0.986495109199128,-0.111715301258998));
#84307=DIRECTION('ref_axis',(-0.7073632684812,-0.00584313333012281,-0.706826049460884));
#84308=DIRECTION('center_axis',(-0.0991219242755701,-0.986495109247181,
0.130392651477376));
#84309=DIRECTION('ref_axis',(-0.780807435100502,-0.00412443550550682,-0.624758143863317));
#84310=DIRECTION('center_axis',(0.0929634778324503,-0.986495109264974,-0.134852479345333));
#84311=DIRECTION('ref_axis',(-0.842772215666208,-0.00584312983766792,-0.538238655556037));
#84312=DIRECTION('center_axis',(-0.0687739426533017,-0.986495109277807,
0.148652427436915));
#84313=DIRECTION('ref_axis',(-0.896857124779159,-0.00412443574213562,-0.442301126793352));
#84314=DIRECTION('center_axis',(0.0618007488840924,-0.986495109226495,-0.151684102362676));
#84315=DIRECTION('ref_axis',(-0.938774069888716,-0.00584313211839086,-0.344483821843091));
#84316=DIRECTION('center_axis',(-0.0352101726582262,-0.986495109258675,
0.159961380183131));
#84317=DIRECTION('ref_axis',(-0.970970771535139,-0.00412443128434196,-0.239162601363671));
#84318=DIRECTION('center_axis',(0.0277482857856159,-0.986495109197101,-0.161423146314771));
#84319=DIRECTION('ref_axis',(-0.990879892697005,-0.00584313456157943,-0.134621305993024));
#84320=DIRECTION('center_axis',(-4.18658415555892E-9,-0.986495109267289,
0.163790718270967));
#84321=DIRECTION('ref_axis',(-0.999682904139737,-0.00412443729868955,-0.0248410987621459));
#84322=DIRECTION('center_axis',(-0.00760166424773501,-0.986495109286652,
-0.163614223263692));
#84323=DIRECTION('ref_axis',(-0.99665327290905,-0.00584312869504784,0.0815359518662326));
#84324=DIRECTION('center_axis',(0.0352101565309749,-0.986495109262151,0.15996138371157));
#84325=DIRECTION('ref_axis',(-0.98165097512954,-0.00412443485408824,0.19064194728432));
#84326=DIRECTION('center_axis',(-0.0425961641670186,-0.986495109300108,
-0.158154880181497));
#84327=DIRECTION('ref_axis',(-0.955824253713504,-0.00584312765218506,0.29388067965122));
#84328=DIRECTION('center_axis',(0.0687739335326133,-0.986495109263156,0.148652431753823));
#84329=DIRECTION('ref_axis',(-0.917718138243298,-0.00412443719897299,0.397210785046234));
#84330=DIRECTION('center_axis',(-0.0755989173093816,-0.986495109354155,
-0.145300388581668));
#84331=DIRECTION('ref_axis',(-0.870301954080379,-0.00584312361802103,0.492483874487539));
#84332=DIRECTION('center_axis',(0.0991219123679854,-0.986495109264719,0.130392660396599));
#84333=DIRECTION('ref_axis',(-0.810873820575113,-0.00412443265964962,0.585206490190561));
#84334=DIRECTION('center_axis',(-0.105066742165034,-0.986495109264701,-0.125651816889575));
#84335=DIRECTION('ref_axis',(-0.744085303337244,-0.00584312785497444,0.668059068656651));
#84336=DIRECTION('center_axis',(0.124835066434611,-0.98649510930135,0.106035868991502));
#84337=DIRECTION('ref_axis',(-0.666113944006964,-0.0041244354640061,0.745838590200045));
#84338=DIRECTION('center_axis',(-0.129621765649896,-0.986495109247229,-0.100127904707433));
#84339=DIRECTION('ref_axis',(-0.583076051165369,-0.00584312925752157,0.812396563506936));
#84340=DIRECTION('center_axis',(0.144711069366066,-0.986495109279995,0.0767209604318137));
#84341=DIRECTION('ref_axis',(-0.490207320958835,-0.00412443533582184,0.871596105723014));
#84342=DIRECTION('center_axis',(-0.148115819742761,-0.986495109250133,-0.0699221235911587));
#84343=DIRECTION('ref_axis',(-0.394802809718104,-0.00584313123430531,0.918747298910897));
#84344=DIRECTION('center_axis',(0.157820544757281,-0.986495109280205,0.0438186606225097));
#84345=DIRECTION('ref_axis',(-0.291379146863202,-0.00412443951164448,0.956598756936254));
#84346=DIRECTION('center_axis',(-0.159684144067683,-0.986495109300543,-0.0364468580193389));
#84347=DIRECTION('ref_axis',(-0.18806902754466,-0.00584312910065061,0.982138431546551));
#84348=DIRECTION('center_axis',(0.163550506209464,-0.986495109038151,0.00886745524006982));
#84349=DIRECTION('ref_axis',(-0.0789264177712791,-0.00412443861087988,0.99687191232572));
#84350=DIRECTION('center_axis',(0.15712354266245,0.986495109435393,0.0462557174979818));
#84351=DIRECTION('ref_axis',(-0.0845282468056531,-0.0332319479630796,0.99586676474644));
#84352=DIRECTION('center_axis',(-0.160229052463087,0.986495108976718,-0.0339713219023825));
#84353=DIRECTION('ref_axis',(-0.18762955624287,0.00334931877564638,0.982234153187438));
#84354=DIRECTION('center_axis',(0.143506481236011,0.986495109925276,0.0789511743850364));
#84355=DIRECTION('ref_axis',(-0.296633918114572,-0.0332319218886669,0.954412886538936));
#84356=DIRECTION('center_axis',(-0.14918015440409,0.986495109054244,-0.067621604121956));
#84357=DIRECTION('ref_axis',(-0.394394189435828,0.00334932227517103,0.918935256358985));
#84358=DIRECTION('center_axis',(0.123179213512155,0.986495110027753,0.107954987146767));
#84359=DIRECTION('ref_axis',(-0.494869342219976,-0.0332319165515335,0.868331718787861));
#84360=DIRECTION('center_axis',(-0.131155762220521,0.986495108970641,-0.0981099689805186));
#84361=DIRECTION('ref_axis',(-0.5827173879895,0.00334931822458211,0.812667968977567));
#84362=DIRECTION('center_axis',(0.0970922175602616,0.986495109914703,0.13191095255364));
#84363=DIRECTION('ref_axis',(-0.669965224461655,-0.0332319210725802,0.741648324634979));
#84364=DIRECTION('center_axis',(-0.10699866856939,0.986495109004646,-0.12401082547217));
#84365=DIRECTION('ref_axis',(-0.743793371796284,0.00334931980664887,0.668401228401585));
#84366=DIRECTION('center_axis',(0.0664652972180845,0.986495109850739,0.149698906162635));
#84367=DIRECTION('ref_axis',(-0.813734276754544,-0.0332319242107122,0.580286279389762));
#84368=DIRECTION('center_axis',(-0.0778384347764584,0.986495109011886,-0.144113073547051));
#84369=DIRECTION('ref_axis',(-0.870090401643211,0.00334932307507521,0.492880791879025));
#84370=DIRECTION('center_axis',(0.0327305405511539,0.986495109972787,0.160487101397616));
#84371=DIRECTION('ref_axis',(-0.919454018071839,-0.0332319192853551,0.391790694366472));
#84372=DIRECTION('center_axis',(-0.0450385678146406,0.986495108996408,-0.157476751729809));
#84373=DIRECTION('ref_axis',(-0.955702972692551,0.0033493195060858,0.294313795200746));
#84374=DIRECTION('center_axis',(-0.00253465994445632,0.986495110068069,
0.16377110035276));
#84375=DIRECTION('ref_axis',(-0.982181112188289,-0.0332319150790252,0.184975411016589));
#84376=DIRECTION('center_axis',(-0.0101327460188246,0.986495108992418,-0.16347699346439));
#84377=DIRECTION('ref_axis',(-0.996627934277689,0.00334931820573886,0.081985015002393));
#84378=DIRECTION('center_axis',(-0.0376813519129768,0.986495109949854,0.159397345533218));
#84379=DIRECTION('ref_axis',(-0.998982508909587,-0.0332319202960521,-0.0304891188154647));
#84380=DIRECTION('center_axis',(0.02524687742827,0.986495109027206,-0.161833232203781));
#84381=DIRECTION('ref_axis',(-0.990951681531433,0.00334932228370334,-0.134177296552975));
#84382=DIRECTION('center_axis',(-0.0710661011878459,0.986495109933046,0.147570347089602));
#84383=DIRECTION('ref_axis',(-0.969072594036823,-0.0332319214002897,-0.244528008389197));
#84384=DIRECTION('center_axis',(0.0594459811191166,0.986495109049416,-0.152622328479048));
#84385=DIRECTION('ref_axis',(-0.93893962948678,0.00334932291028807,-0.344065624867221));
#84386=DIRECTION('center_axis',(-0.101127876712746,0.986495109938007,0.12884312406943));
#84387=DIRECTION('ref_axis',(-0.893849921483746,-0.033231920065598,-0.447133042116387));
#84388=DIRECTION('center_axis',(0.0908654531082973,0.986495109005426,-0.136274976939262));
#84389=DIRECTION('ref_axis',(-0.843023804543385,0.00334931910330392,-0.53786582623805));
#84390=DIRECTION('center_axis',(-0.126461025342994,0.986495109956393,0.104091340184102));
#84391=DIRECTION('ref_axis',(-0.776831821485583,-0.033231919097129,-0.628830629566112));
#84392=DIRECTION('center_axis',(0.118036163879419,0.986495109044257,-0.113555554018244));
#84393=DIRECTION('ref_axis',(-0.707689122394941,0.00334932327296944,-0.706516021104611));
#84394=DIRECTION('center_axis',(-0.145880998923188,0.986495109926482,0.0744723589280713));
#84395=DIRECTION('ref_axis',(-0.62348992709468,-0.0332319204812905,-0.781124798142138));
#84396=DIRECTION('center_axis',(0.13968763128992,0.986495109047707,-0.0855264022952221));
#84397=DIRECTION('ref_axis',(-0.539263682656536,0.00334932285080722,-0.842130312127613));
#84398=DIRECTION('center_axis',(-0.1584797400563,0.986495109801124,0.0413711291863717));
#84399=DIRECTION('ref_axis',(-0.440994335358874,-0.0332319254215281,-0.896894439337296));
#84400=DIRECTION('center_axis',(0.154807460333395,0.986495109016585,-0.0534981318503795));
#84401=DIRECTION('ref_axis',(-0.345622874549849,0.00334932213427141,-0.938367524283071));
#84402=DIRECTION('center_axis',(-0.163668140770195,0.986495109923557,0.00633543950617634));
#84403=DIRECTION('ref_axis',(-0.237878339260044,-0.0332319212560437,-0.970726292587419));
#84404=DIRECTION('center_axis',(0.162688664882239,0.986495109019678,-0.0189683472946007));
#84405=DIRECTION('ref_axis',(-0.135821122852929,0.00334932200186453,-0.990727714676993));
#84406=DIRECTION('center_axis',(-0.161203602974452,0.98649510998187,-0.0289964889238977));
#84407=DIRECTION('ref_axis',(-0.0236394202842747,-0.0332319187916197,-0.999168062631132));
#84408=DIRECTION('center_axis',(0.162962728442386,0.986495108997507,0.0164483756830008));
#84409=DIRECTION('ref_axis',(0.0803314697776428,0.00334932208550028,-0.996762578052031));
#84410=DIRECTION('center_axis',(-0.151201364507919,0.986495110021318,-0.0629725755783483));
#84411=DIRECTION('ref_axis',(0.191704853736926,-0.0332319178461485,-0.980889845339409));
#84412=DIRECTION('center_axis',(0.155616836747566,0.986495109020785,0.0510959880886054));
#84413=DIRECTION('ref_axis',(0.292727855798555,0.00334931856927389,-0.956189931187681));
#84414=DIRECTION('center_axis',(-0.134129119682807,0.986495110072656,-0.0940041331849542));
#84415=DIRECTION('ref_axis',(0.398085224325408,-0.0332319147272993,-0.916746308428535));
#84416=DIRECTION('center_axis',(0.140994470581048,0.986495109053583,0.083354418472747));
#84417=DIRECTION('ref_axis',(0.491436612895278,0.00334932584772274,-0.870906905198473));
#84418=DIRECTION('center_axis',(-0.110785145530079,0.986495110071087,-0.12064016468703));
#84419=DIRECTION('ref_axis',(0.585851568710888,-0.033231915064203,-0.809736734537934));
#84420=DIRECTION('center_axis',(0.11977936442388,0.986495109030295,0.111715279695832));
#84421=DIRECTION('ref_axis',(0.667166337497202,0.00334932295266879,-0.744901241874605));
#84422=DIRECTION('center_axis',(-0.0822609770536327,0.986495109954466,-0.141635199333031));
#84423=DIRECTION('ref_axis',(0.746224147227216,-0.0332319201177854,-0.66486476939322));
#84424=DIRECTION('center_axis',(0.0929635057152089,0.986495109045637,0.134852461728273));
#84425=DIRECTION('ref_axis',(0.811700106743077,0.00334932408193139,-0.584064824091875));
#84426=DIRECTION('center_axis',(-0.0498903763927356,0.986495109833051,-0.156007527442964));
#84427=DIRECTION('ref_axis',(0.871704114499594,-0.0332319238633797,-0.488904465106239));
#84428=DIRECTION('center_axis',(0.0618007766378893,0.986495109035607,0.151684092296388));
#84429=DIRECTION('ref_axis',(0.918279682544927,0.00334932473737517,-0.395918181761071));
#84430=DIRECTION('center_axis',(-0.0151869682934995,0.986495110040763,-0.163085112317817));
#84431=DIRECTION('ref_axis',(0.956424164040124,-0.0332319160599138,-0.29008353658065));
#84432=DIRECTION('center_axis',(0.0277483150289102,0.986495109025233,0.161423142338237));
#84433=DIRECTION('ref_axis',(0.98192151939393,0.0033493226463211,-0.189258848641028));
#84434=DIRECTION('center_axis',(0.0202265769072787,0.986495109950066,-0.162537022340209));
#84435=DIRECTION('ref_axis',(0.996422884216933,-0.0332319196220728,-0.0776986185658488));
#84436=DIRECTION('center_axis',(-0.0076016257944453,0.986495109024876,0.163614226628614));
#84437=DIRECTION('ref_axis',(0.999649797962388,0.00334931933611909,0.0262500189284213));
#84438=DIRECTION('center_axis',(0.0546943469278073,0.986495109914991,-0.154388880842986));
#84439=DIRECTION('ref_axis',(0.989829977359144,-0.0332319208452661,0.138319396174687));
#84440=DIRECTION('center_axis',(-0.0425961353137144,0.986495109055382,0.158154889479096));
#84441=DIRECTION('ref_axis',(0.970635562333554,0.00334932831784015,0.240531468072776));
#84442=DIRECTION('center_axis',(0.0866046692179882,0.986495109923493,-0.139021686677578));
#84443=DIRECTION('ref_axis',(0.936953721048867,-0.0332319209181787,0.347869751551886));
#84444=DIRECTION('center_axis',(-0.0755988798102178,0.986495109009909,0.145300410429456));
#84445=DIRECTION('ref_axis',(0.896235487868925,0.00334931975946973,0.443565927841058));
#84446=DIRECTION('center_axis',(0.114465449777541,0.986495110036967,-0.117153995580081));
#84447=DIRECTION('ref_axis',(0.840266549276586,-0.0332319161818368,0.541154105513118));
#84448=DIRECTION('center_axis',(-0.105066715113567,0.986495109010335,0.125651841506333));
#84449=DIRECTION('ref_axis',(0.779928436803072,0.0033493221170034,0.625859741082036));
#84450=DIRECTION('center_axis',(0.136973958783264,0.986495109992769,-0.0898083101700282));
#84451=DIRECTION('ref_axis',(0.704289448443,-0.0332319188577156,0.709134692693066));
#84452=DIRECTION('center_axis',(-0.129621746388085,0.986495109054189,0.100127931544929));
#84453=DIRECTION('ref_axis',(0.627152799867747,0.00334932424359592,0.778889047069707));
#84454=DIRECTION('center_axis',(0.153077714731913,0.98649511003431,-0.0582632914522498));
#84455=DIRECTION('ref_axis',(0.5353805562444,-0.0332319168564682,0.843956930001456));
#84456=DIRECTION('center_axis',(-0.148115806239736,0.986495109048684,0.0699221550367086));
#84457=DIRECTION('ref_axis',(0.445052195942097,0.00334932140284593,0.895498366795416));
#84458=DIRECTION('center_axis',(0.162023729773525,0.986495109914706,-0.0239939389148083));
#84459=DIRECTION('ref_axis',(0.341437862680118,-0.0332319224161379,0.939316679965261));
#84460=DIRECTION('center_axis',(-0.159684137199492,0.9864951090058,0.0364468960885444));
#84461=DIRECTION('ref_axis',(0.242141441283249,0.0033493185268396,0.970235179984047));
#84462=DIRECTION('center_axis',(0.163393692715904,0.986495109888097,0.0113973394935696));
#84463=DIRECTION('ref_axis',(0.13152991478354,-0.0332319233338571,0.990755025618628));
#84464=DIRECTION('center_axis',(-0.163785816773439,0.986495108928238,0.00126739280443092));
#84465=DIRECTION('ref_axis',(0.0279084234544092,0.00334934443904838,0.99960487283332));
#84466=DIRECTION('center_axis',(0.158340237893585,0.987363722701301,0.00642247282834522));
#84467=DIRECTION('ref_axis',(0.10038315980289,-0.0225682600917394,0.994692864589075));
#84468=DIRECTION('',(-0.603935214477145,0.,0.797033410036521));
#84469=DIRECTION('center_axis',(-0.155457922179175,0.987363721843173,0.0307524831473961));
#84470=DIRECTION('ref_axis',(0.169586056764272,-0.00399376666708634,0.985507290271845));
#84471=DIRECTION('',(-0.797033410730744,0.,-0.603935213560956));
#84472=DIRECTION('center_axis',(-1.44211143998122E-14,-1.,-5.7605855884159E-14));
#84473=DIRECTION('ref_axis',(1.88000594205393E-31,5.7605855884159E-14,-1.));
#84474=DIRECTION('center_axis',(-0.158420672394944,-0.98736372164076,0.00397136571504476));
#84475=DIRECTION('ref_axis',(0.165372899663439,-0.02256800269505,0.985972864388905));
#84476=DIRECTION('center_axis',(0.149059806197162,-0.987363722366908,-0.0537964118713228));
#84477=DIRECTION('ref_axis',(0.245793064245949,-0.0156997426146358,0.969195175210041));
#84478=DIRECTION('center_axis',(0.156018974387301,0.987363722599173,-0.027766147126286));
#84479=DIRECTION('ref_axis',(0.311865820899157,-0.0225682650208507,0.949858085804845));
#84480=DIRECTION('',(-0.418476923230307,0.,0.908227430065672));
#84481=DIRECTION('center_axis',(-0.145212528016864,0.987363721832163,0.0634523641536714));
#84482=DIRECTION('ref_axis',(0.377476166873708,-0.00399376522103734,0.926010687455437));
#84483=DIRECTION('',(-0.908227431050156,0.,-0.418476921093665));
#84484=DIRECTION('center_axis',(2.31590738330052E-14,-1.,4.65140809571269E-14));
#84485=DIRECTION('ref_axis',(-1.25528131886048E-31,-4.65140809571269E-14,
-1.));
#84486=DIRECTION('center_axis',(-0.15386315511425,-0.98736372188743,0.0379342879054026));
#84487=DIRECTION('ref_axis',(0.373461598612057,-0.0225679937784545,0.927371079999232));
#84488=DIRECTION('center_axis',(0.134010233686999,-0.987363722422057,-0.0845821311626506));
#84489=DIRECTION('ref_axis',(0.448394871139783,-0.0156997398795868,0.893697688093267));
#84490=DIRECTION('center_axis',(0.14640243582563,0.987363722649047,-0.0606564586910423));
#84491=DIRECTION('ref_axis',(0.508765982049945,-0.0225682636858441,0.86060899889727));
#84492=DIRECTION('',(-0.213451112797401,0.,0.976953746318397));
#84493=DIRECTION('center_axis',(-0.128177159307217,0.987363721827163,0.0931852813031351));
#84494=DIRECTION('ref_axis',(0.567715906841173,-0.00399376197540127,0.823214855906274));
#84495=DIRECTION('',(-0.976953746694739,0.,-0.213451111074907));
#84496=DIRECTION('center_axis',(-3.72763200032572E-14,-1.,-4.62263900319702E-14));
#84497=DIRECTION('ref_axis',(-1.48754987227568E-31,4.62263900319702E-14,
-1.));
#84498=DIRECTION('center_axis',(-0.142111171391025,-0.987363721797395,0.0701234329184363));
#84499=DIRECTION('ref_axis',(0.564087641138766,-0.0225679966417213,0.825406456627328));
#84500=DIRECTION('center_axis',(0.112694491064729,-0.987363722439752,-0.111412886568739));
#84501=DIRECTION('ref_axis',(0.630030234816697,-0.0156997393169039,0.776411889013943));
#84502=DIRECTION('center_axis',(0.129940280587677,0.987363722695499,-0.0907105428584852));
#84503=DIRECTION('ref_axis',(0.681876811644499,-0.0225682605544513,0.73111879154969));
#84504=DIRECTION('',(0.00155543204822409,0.,0.99999879031484));
#84505=DIRECTION('center_axis',(-0.105148369505461,0.987363721822415,0.118560959929194));
#84506=DIRECTION('ref_axis',(0.731409885236659,-0.00399375923834658,0.68192641074037));
#84507=DIRECTION('',(-0.999998790317524,0.,0.00155543032291784));
#84508=DIRECTION('center_axis',(-3.47565958367976E-14,-1.,-2.78492518591803E-14));
#84509=DIRECTION('ref_axis',(1.,-3.47565958367976E-14,-1.19813090436101E-31));
#84510=DIRECTION('center_axis',(-0.123714231112402,-0.98736372160937,0.0990336825022796));
#84511=DIRECTION('ref_axis',(0.728337575162783,-0.0225680037404996,0.684846743303322));
#84512=DIRECTION('center_axis',(0.0861092731980021,-0.987363722354366,-0.13303410407802));
#84513=DIRECTION('ref_axis',(0.782206083646391,-0.0156997469095425,0.622821933343352));
#84514=DIRECTION('center_axis',(0.107402265374242,0.987363722656843,-0.116523098884737));
#84515=DIRECTION('ref_axis',(0.823103837842111,-0.0225682622741833,0.567442283996806));
#84516=DIRECTION('',(0.216489246715154,0.,0.976285002474536));
#84517=DIRECTION('center_axis',(-0.077202954207757,0.987363721838984,0.138392863464355));
#84518=DIRECTION('ref_axis',(0.86090394918356,-0.0039937628012165,0.508751845341948));
#84519=DIRECTION('',(-0.976285002225685,0.,0.216489247837379));
#84520=DIRECTION('center_axis',(3.9930771852328E-14,-1.,1.97265111112018E-14));
#84521=DIRECTION('ref_axis',(1.,3.9930771852328E-14,-6.35163460405498E-32));
#84522=DIRECTION('center_axis',(-0.0995325366648503,-0.987363721950605,
0.12331323822246));
#84523=DIRECTION('ref_axis',(0.858531254097983,-0.0225679922629129,0.512264357009314));
#84524=DIRECTION('center_axis',(0.0554976885393332,-0.987363722365339,-0.148434788118059));
#84525=DIRECTION('ref_axis',(0.89780684558997,-0.0156997443940525,0.440109515959095));
#84526=DIRECTION('center_axis',(0.079842234321559,0.987363722730416,-0.13688716760338));
#84527=DIRECTION('ref_axis',(0.925843445770208,-0.0225682581826276,0.377232802983714));
#84528=DIRECTION('',(0.421300264062744,0.,0.906921213502398));
#84529=DIRECTION('center_axis',(-0.0456476172175642,0.98736372183397,0.151753668319847));
#84530=DIRECTION('ref_axis',(0.950143101272476,-0.00399376292983926,0.311788609416672));
#84531=DIRECTION('',(-0.906921212507855,0.,0.421300266203668));
#84532=DIRECTION('center_axis',(4.32378293793031E-14,-1.,1.06813806392854E-14));
#84533=DIRECTION('ref_axis',(1.,4.32378293793031E-14,-1.52773325573375E-31));
#84534=DIRECTION('center_axis',(-0.0706968279110265,-0.987363721698004,
0.14182679435842));
#84535=DIRECTION('ref_axis',(0.948580963488652,-0.0225679997999443,0.315729062792722));
#84536=DIRECTION('center_axis',(0.0222910902134773,-0.987363722383866,-0.156894827885975));
#84537=DIRECTION('ref_axis',(0.971427156744944,-0.0156997459091039,0.236818067547269));
#84538=DIRECTION('center_axis',(0.0485488733164528,0.98736372271806,-0.150850541795637));
#84539=DIRECTION('ref_axis',(0.985291642253544,-0.022568258991991,0.169384336322413));
#84540=DIRECTION('',(0.606411752600289,0.,0.795150794697614));
#84541=DIRECTION('',(-0.795150795057726,0.,0.606411752128096));
#84542=DIRECTION('',(0.763168097828372,0.,0.646200011186184));
#84543=DIRECTION('center_axis',(0.0222910563515225,0.987363721854081,0.156894836030986));
#84544=DIRECTION('ref_axis',(0.993243163244486,-0.00399376358983429,-0.115983052729596));
#84545=DIRECTION('',(-0.6462000100523,0.,0.763168098788469));
#84546=DIRECTION('center_axis',(-6.55898797099622E-14,-1.,1.26914022202139E-14));
#84547=DIRECTION('ref_axis',(1.,-6.55898797099622E-14,-1.46963136636167E-31));
#84548=DIRECTION('center_axis',(-0.00461118059927081,-0.987363721673051,
0.158403340045037));
#84549=DIRECTION('ref_axis',(0.993479958729521,-0.0225680020847444,-0.111750869726782));
#84550=DIRECTION('center_axis',(-0.0456475817526598,-0.987363722372463,
-0.151753675484082));
#84551=DIRECTION('ref_axis',(0.981080735173516,-0.0156997448954984,-0.192961418634945));
#84552=DIRECTION('center_axis',(-0.0192787363169843,0.987363722720525,-0.157293386324687));
#84553=DIRECTION('ref_axis',(0.96534911195294,-0.0225682574057377,-0.259984164535724));
#84554=DIRECTION('',(0.884239552545667,0.,0.467033632315531));
#84555=DIRECTION('center_axis',(0.0554976572498314,0.987363721828398,0.148434803388402));
#84556=DIRECTION('ref_axis',(0.945088761644806,-0.00399376484876287,-0.326789354867965));
#84557=DIRECTION('',(-0.467033631299099,0.,0.884239553082522));
#84558=DIRECTION('center_axis',(2.72569548792655E-14,-1.,-1.17753642764545E-14));
#84559=DIRECTION('ref_axis',(1.,2.72569548792655E-14,-8.37905660890704E-32));
#84560=DIRECTION('center_axis',(0.0295486617759713,-0.987363721604755,0.155691225976474));
#84561=DIRECTION('ref_axis',(0.946229815089767,-0.0225680027411708,-0.32270702237085));
#84562=DIRECTION('center_axis',(-0.0772029153070725,-0.987363722443341,
-0.13839288085345));
#84563=DIRECTION('ref_axis',(0.916662612281878,-0.01569973864484,-0.399353444270922));
#84564=DIRECTION('center_axis',(-0.0526414311335554,0.987363722607825,-0.149471599329872));
#84565=DIRECTION('ref_axis',(0.886890876746755,-0.0225682654117284,-0.461427400724835));
#84566=DIRECTION('',(0.963964949091376,0.,0.266029278319627));
#84567=DIRECTION('center_axis',(0.0861092440564124,0.98736372182379,0.133034126878435));
#84568=DIRECTION('ref_axis',(0.852743060306908,-0.00399376025843779,-0.522315348211603));
#84569=DIRECTION('',(-0.266029277211529,0.,0.963964949397182));
#84570=DIRECTION('center_axis',(-5.4198781169427E-14,-1.,3.90588803916287E-14));
#84571=DIRECTION('ref_axis',(1.,-5.4198781169427E-14,-4.4243770373351E-31));
#84572=DIRECTION('center_axis',(0.0623268493950371,-0.98736372187317,0.145699157764377));
#84573=DIRECTION('ref_axis',(0.854735017319459,-0.0225679935913295,-0.518573751585216));
#84574=DIRECTION('center_axis',(-0.105148334878449,-0.987363722399287,-0.11856098583477));
#84575=DIRECTION('ref_axis',(0.809382363103314,-0.015699741278534,-0.587072149246651));
#84576=DIRECTION('center_axis',(-0.0835426830519901,0.987363722660821,-0.134660682019068));
#84577=DIRECTION('ref_axis',(0.766962608774369,-0.0225682608416332,-0.641294807670075));
#84578=DIRECTION('',(0.99861641532288,0.,0.0525856924237102));
#84579=DIRECTION('center_axis',(0.112694467126882,0.987363721854894,0.111412915965074));
#84580=DIRECTION('ref_axis',(0.720524038701269,-0.00399376641948853,-0.693418459145268));
#84581=DIRECTION('',(-0.0525856941427118,0.,0.99861641523236));
#84582=DIRECTION('center_axis',(9.89669757213282E-15,-1.,-1.10659647378638E-14));
#84583=DIRECTION('ref_axis',(7.27748752740703E-32,1.10659647378638E-14,
-1.));
#84584=DIRECTION('center_axis',(0.0921906888296262,-0.987363721661339,0.128894367759766));
#84585=DIRECTION('ref_axis',(0.723273756993294,-0.0225680022062431,-0.690192551192219));
#84586=DIRECTION('center_axis',(-0.128177133529277,-0.987363722357498,-0.0931853111416337));
#84587=DIRECTION('ref_axis',(0.664256296123621,-0.0156997428788034,-0.747340010392637));
#84588=DIRECTION('center_axis',(-0.11053756830992,0.987363722671541,-0.113553182008812));
#84589=DIRECTION('ref_axis',(0.611172022170688,-0.0225682598153682,-0.791175981033738));
#84590=DIRECTION('',(0.986573688235263,0.,-0.163316740360169));
#84591=DIRECTION('center_axis',(0.134010214694044,0.987363721846181,0.0845821679771451));
#84592=DIRECTION('ref_axis',(0.554614118231904,-0.00399376301988119,-0.832098088998399));
#84593=DIRECTION('',(0.163316741957422,0.,0.986573687970854));
#84594=DIRECTION('center_axis',(3.64323148098048E-14,-1.,-6.46737302459633E-14));
#84595=DIRECTION('ref_axis',(9.26601293729421E-32,6.46737302459633E-14,
-1.));
#84596=DIRECTION('center_axis',(0.117743806453333,-0.987363721981412,0.106062606779642));
#84597=DIRECTION('ref_axis',(0.557993023279549,-0.0225679909028752,-0.82953871022271));
#84598=DIRECTION('center_axis',(-0.145212512392438,-0.987363722361673,-0.0634523916710614));
#84599=DIRECTION('ref_axis',(0.488070340442066,-0.0156997468238425,-0.872663085463361));
#84600=DIRECTION('center_axis',(-0.132363838781167,0.987363722684511,-0.0871360620506701));
#84601=DIRECTION('ref_axis',(0.426803711705219,-0.022568259797764,-0.904062644579649));
#84602=DIRECTION('',(0.928399871491961,0.,-0.371582667267609));
#84603=DIRECTION('center_axis',(0.149059796702993,0.987363721816425,0.0537964482812778));
#84604=DIRECTION('ref_axis',(0.362771055313395,-0.00399376382293106,-0.931869739436437));
#84605=DIRECTION('',(0.371582668334801,0.,0.928399871064828));
#84606=DIRECTION('center_axis',(-8.67104292624063E-15,-1.,2.83974261068442E-14));
#84607=DIRECTION('ref_axis',(-5.0163862275377E-32,-2.83974261068442E-14,
-1.));
#84608=DIRECTION('center_axis',(0.137791344859856,-0.987363721744609,0.0782714907507665));
#84609=DIRECTION('ref_axis',(0.366621154304528,-0.0225679980487453,-0.930096562019497));
#84610=DIRECTION('center_axis',(-0.155457912687875,-0.987363722342947,-0.0307525150810445));
#84611=DIRECTION('ref_axis',(0.289062760137001,-0.0156997441135714,-0.957181403254758));
#84612=DIRECTION('center_axis',(-0.148000923706643,0.987363722699675,-0.0566445555955659));
#84613=DIRECTION('ref_axis',(0.222478534563419,-0.0225682585023063,-0.974676343904317));
#84614=DIRECTION('',(0.826815108418725,0.,-0.562473800714782));
#84615=DIRECTION('center_axis',(0.157139507936205,0.987363721861756,0.0204952627908948));
#84616=DIRECTION('ref_axis',(0.153965220883453,-0.0039937680742605,-0.988068196317885));
#84617=DIRECTION('',(0.562473799699905,0.,0.826815109109135));
#84618=DIRECTION('center_axis',(1.18185578346938E-15,-1.,-1.47987639615482E-14));
#84619=DIRECTION('ref_axis',(4.97525843814439E-33,1.47987639615482E-14,
-1.));
#84620=DIRECTION('center_axis',(0.151395916621486,-0.987363721839513,0.0468204786985774));
#84621=DIRECTION('ref_axis',(0.158106489918185,-0.0225679957185716,-0.987164131953242));
#84622=DIRECTION('center_axis',(-0.158434274587155,-0.987363722374232,0.00338531761313504));
#84623=DIRECTION('ref_axis',(0.0765389249906997,-0.015699744021737,-0.996942982822448));
#84624=DIRECTION('center_axis',(-0.156717649159304,0.987363722718713,-0.0235044145008221));
#84625=DIRECTION('ref_axis',(0.00775050626250672,-0.0225682595442366,-0.999715261118794));
#84626=DIRECTION('',(0.686569391286906,0.,-0.727064282541735));
#84627=DIRECTION('center_axis',(0.157871550275308,0.987363721803754,-0.0137642464199764));
#84628=DIRECTION('ref_axis',(-0.0620398544850762,-0.00399376025474478,-0.998065682374912));
#84629=DIRECTION('',(0.727064283330936,0.,0.686569390451156));
#84630=DIRECTION('center_axis',(-4.05414431250584E-15,-1.,-2.94136823488773E-14));
#84631=DIRECTION('ref_axis',(4.1025633915743E-32,2.94136823488773E-14,-1.));
#84632=DIRECTION('center_axis',(0.157921383722301,-0.987363721687767,0.0131801994717713));
#84633=DIRECTION('ref_axis',(-0.0578010613898766,-0.0225680004185413,-0.998073004674163));
#84634=DIRECTION('center_axis',(-0.154002425721324,-0.987363722322906,0.0373648593280209));
#84635=DIRECTION('ref_axis',(-0.13956378452677,-0.0156997468687922,-0.990088616234336));
#84636=DIRECTION('center_axis',(-0.158106432639921,0.987363722636627,0.010734764972707));
#84637=DIRECTION('ref_axis',(-0.207339927418302,-0.0225682625965862,-0.978008603245158));
#84638=DIRECTION('',(0.514220451397935,0.,-0.857658048037856));
#84639=DIRECTION('center_axis',(0.151221694258108,0.987363721834325,-0.0473801645330356));
#84640=DIRECTION('ref_axis',(-0.275144016599707,-0.00399376225466582,-0.961394726422209));
#84641=DIRECTION('',(0.85765804862894,0.,0.514220450412077));
#84642=DIRECTION('center_axis',(-2.31354740159072E-14,-1.,-6.26725925243937E-14));
#84643=DIRECTION('ref_axis',(-2.02413979510853E-31,6.26725925243937E-14,
-1.));
#84644=DIRECTION('center_axis',(0.157062622255562,-0.98736372175739,-0.0210763765292199));
#84645=DIRECTION('ref_axis',(-0.271005896921264,-0.0225679992448247,-0.962313093147956));
#84646=DIRECTION('center_axis',(-0.142369594341273,-0.987363722348708,0.0695972585437428));
#84647=DIRECTION('ref_axis',(-0.349140646055173,-0.0156997465692948,-0.936938806555602));
#84648=DIRECTION('center_axis',(-0.152102334687275,0.987363722657685,0.0444720020039294));
#84649=DIRECTION('ref_axis',(-0.412735373600482,-0.0225682618095411,-0.910571350821981));
#84650=DIRECTION('',(0.317827133913603,0.,-0.948148676605238));
#84651=DIRECTION('center_axis',(0.137500881589967,0.987363721812837,-0.0787806347390351));
#84652=DIRECTION('ref_axis',(-0.475382749181283,-0.00399375991611874,-0.879770022029949));
#84653=DIRECTION('',(0.948148676680187,0.,0.317827133690014));
#84654=DIRECTION('center_axis',(-3.60673343231128E-14,-1.,-5.62338991472549E-14));
#84655=DIRECTION('ref_axis',(-1.93076868610309E-33,5.62338991472549E-14,
-1.));
#84656=DIRECTION('center_axis',(0.148859786500606,-0.987363721793018,-0.0543474456624563));
#84657=DIRECTION('ref_axis',(-0.471538799476592,-0.0225679970353284,-0.881556490588089));
#84658=DIRECTION('center_axis',(-0.124079723161267,-0.987363722414623,0.0985753618292251));
#84659=DIRECTION('ref_axis',(-0.542392077558857,-0.0156997396972913,-0.839978780907485));
#84660=DIRECTION('center_axis',(-0.138986101500481,0.987363722635373,0.0761297761281104));
#84661=DIRECTION('ref_axis',(-0.59883177246696,-0.0225682627670856,-0.800556794862023));
#84662=DIRECTION('',(0.10657257433255,0.,-0.994304926267658));
#84663=DIRECTION('center_axis',(0.117350675322984,0.987363721832221,-0.106497416921091));
#84664=DIRECTION('ref_axis',(-0.653393114799153,-0.00399376605342258,-0.757008247884903));
#84665=DIRECTION('',(0.994304926390161,0.,0.106572573189616));
#84666=DIRECTION('center_axis',(0.,-1.,0.));
#84667=DIRECTION('ref_axis',(0.,0.,-1.));
#84668=DIRECTION('center_axis',(0.133696435217807,-0.987363721715313,-0.0850772839866021));
#84669=DIRECTION('ref_axis',(-0.650023071279847,-0.0225680003215464,-0.759579286293012));
#84670=DIRECTION('center_axis',(-0.0999880192034972,-0.987363722417943,
0.122944197377283));
#84671=DIRECTION('ref_axis',(-0.710281861740028,-0.0156997394700075,-0.70374227886613));
#84672=DIRECTION('center_axis',(-0.119371033888332,0.987363722615232,0.104227805943629));
#84673=DIRECTION('ref_axis',(-0.756927465696326,-0.0225682653976303,-0.653109091248529));
#84674=DIRECTION('',(-0.109665200773914,0.,-0.993968582873331));
#84675=DIRECTION('center_axis',(0.0917132874572295,0.987363721828803,-0.129234491217171));
#84676=DIRECTION('ref_axis',(-0.800851542707552,-0.00399376332935696,-0.598849610835144));
#84677=DIRECTION('',(0.993968582433906,0.,-0.10966520475671));
#84678=DIRECTION('center_axis',(3.1303237468505E-14,-1.,1.99401244391312E-14));
#84679=DIRECTION('ref_axis',(1.,3.1303237468505E-14,1.69915241587248E-31));
#84680=DIRECTION('center_axis',(0.112281583312903,-0.987363721782803,-0.111829007667775));
#84681=DIRECTION('ref_axis',(-0.798112985393402,-0.0225679969923309,-0.602085000691916));
#84682=DIRECTION('center_axis',(-0.0712209816399454,-0.987363722372648,
0.141564301703048));
#84683=DIRECTION('ref_axis',(-0.844959654147784,-0.0156997452244272,-0.534599570578153));
#84684=DIRECTION('center_axis',(-0.0941743020315624,0.98736372272103,0.127452265147924));
#84685=DIRECTION('ref_axis',(-0.879630072575917,-0.0225682586684263,-0.475122730587332));
#84686=DIRECTION('',(-0.320775152455513,0.,-0.947155373509089));
#84687=DIRECTION('center_axis',(0.0617874894451126,0.987363721814091,-0.145928705173099));
#84688=DIRECTION('ref_axis',(-0.910863042776533,-0.00399376005426055,-0.41268943187887));
#84689=DIRECTION('',(0.947155372266923,0.,-0.320775156123267));
#84690=DIRECTION('center_axis',(-9.0630598583574E-14,-1.,-3.31361281817047E-14));
#84691=DIRECTION('ref_axis',(1.,-9.0630598583574E-14,2.88384923956341E-31));
#84692=DIRECTION('center_axis',(0.0856165697309439,-0.987363721841294,-0.133351729569643));
#84693=DIRECTION('ref_axis',(-0.90888402603509,-0.0225679957248545,-0.416437885869201));
#84694=DIRECTION('center_axis',(-0.0391237406600589,-0.987363722421869,
0.15356501086509));
#84695=DIRECTION('ref_axis',(-0.940128071733025,-0.0156997387927986,-0.340459581949726));
#84696=DIRECTION('center_axis',(-0.0645740902690142,0.987363722699242,0.144717193047071));
#84697=DIRECTION('ref_axis',(-0.961202152072892,-0.0225682588743498,-0.274920163941863));
#84698=DIRECTION('',(-0.516886016398843,0.,-0.85605423078876));
#84699=DIRECTION('center_axis',(0.0289725594784648,0.987363721783673,-0.155799459892387));
#84700=DIRECTION('ref_axis',(-0.978283600768689,-0.00399377459283345,-0.207232348419715));
#84701=DIRECTION('',(0.856054231466657,0.,-0.516886015276125));
#84702=DIRECTION('center_axis',(-0.0319544625179998,0.987363722921529,0.155215305249591));
#84703=DIRECTION('ref_axis',(-0.997829489240866,-0.0225682578414181,-0.0618626231202355));
#84704=DIRECTION('',(-0.688827863670013,0.,-0.724924943860953));
#84705=DIRECTION('center_axis',(-3.67826898181065E-14,-1.,-4.9532785507768E-15));
#84706=DIRECTION('ref_axis',(1.,-3.67826898181065E-14,-3.24545121082182E-32));
#84707=DIRECTION('center_axis',(0.0549482210325186,-0.987363721850913,-0.148639072178465));
#84708=DIRECTION('ref_axis',(-0.977156658219623,-0.0225679947894841,-0.211318600478614));
#84709=DIRECTION('center_axis',(-0.00519719412118699,-0.987363723144184,
0.158385186782481));
#84710=DIRECTION('ref_axis',(-0.991337145602754,-0.015699656874459,-0.130400094026839));
#84711=DIRECTION('',(0.724924943069254,0.,-0.6888278645032));
#84712=DIRECTION('center_axis',(-0.00519706731890305,0.987363721807003,
-0.158385199279182));
#84713=DIRECTION('ref_axis',(-0.999960703086363,-0.0039937612537115,0.00791467965712267));
#84714=DIRECTION('center_axis',(-7.39750789299226E-15,-1.,6.13943474870816E-16));
#84715=DIRECTION('ref_axis',(1.,-7.39750789299226E-15,-2.44284292500047E-33));
#84716=DIRECTION('center_axis',(0.00215930891104003,0.987363722610884,0.158455724595244));
#84717=DIRECTION('ref_axis',(-0.987799426921624,-0.0225682652907615,0.154087525695875));
#84718=DIRECTION('center_axis',(0.0217105622614043,-0.987363721669521,-0.15697621672472));
#84719=DIRECTION('ref_axis',(-0.999738531004337,-0.0225680011955719,0.00368170440508826));
#84720=DIRECTION('center_axis',(0.0289725338067105,-0.987363722367395,0.155799460967041));
#84721=DIRECTION('ref_axis',(-0.996192397019456,-0.0156997433330986,0.0857567850371339));
#84722=DIRECTION('',(-0.828560885250734,0.,-0.559898972523187));
#84723=DIRECTION('center_axis',(-0.0391237013701955,0.987363721838545,-0.153565024625507));
#84724=DIRECTION('ref_axis',(-0.974880754886833,-0.0039937636615464,0.222691633437574));
#84725=DIRECTION('',(0.559898972904418,0.,-0.828560884993117));
#84726=DIRECTION('center_axis',(-5.67406285099299E-14,-1.,1.7518682747499E-14));
#84727=DIRECTION('ref_axis',(1.,-5.67406285099299E-14,-2.40727941335239E-31));
#84728=DIRECTION('center_axis',(-0.0125422691398479,-0.987363721795969,
-0.15797332802102));
#84729=DIRECTION('ref_axis',(-0.975573742112354,-0.0225679969457333,0.218509860680832));
#84730=DIRECTION('center_axis',(0.0617874444497453,-0.987363722445358,0.145928719953322));
#84731=DIRECTION('ref_axis',(-0.954466799122952,-0.0156997368295077,0.297903755658552));
#84732=DIRECTION('center_axis',(0.0361721262527808,0.987363722661402,0.154286928981594));
#84733=DIRECTION('ref_axis',(-0.931580962053001,-0.0225682611666196,0.362832722791536));
#84734=DIRECTION('',(-0.929551320671124,0.,-0.368692747743386));
#84735=DIRECTION('center_axis',(-0.0712209533168093,0.987363721839486,-0.141564319671038));
#84736=DIRECTION('ref_axis',(-0.904216466082979,-0.00399376523860615,0.427055771888904));
#84737=DIRECTION('',(0.368692746674862,0.,-0.929551321094939));
#84738=DIRECTION('center_axis',(2.58240326094427E-14,-1.,-1.4653331787943E-14));
#84739=DIRECTION('ref_axis',(1.,2.58240326094427E-14,8.15439645215452E-32));
#84740=DIRECTION('center_axis',(-0.0462086316812563,-0.987363721736649,
-0.151583783289969));
#84741=DIRECTION('ref_axis',(-0.905792208218432,-0.0225679996060896,0.423120740362082));
#84742=DIRECTION('center_axis',(0.0917132551112029,-0.987363722365354,0.129234510072732));
#84743=DIRECTION('ref_axis',(-0.868111393534543,-0.0156997432445028,0.496121080460778));
#84744=DIRECTION('center_axis',(0.0684935701650493,0.987363722660185,0.142903848865823));
#84745=DIRECTION('ref_axis',(-0.831802807343454,-0.0225682620060956,0.554612263879526));
#84746=DIRECTION('',(-0.987076969591494,0.,-0.160246859882096));
#84747=DIRECTION('center_axis',(-0.0999879913543567,0.987363721850669,-0.122944224582188));
#84748=DIRECTION('ref_axis',(-0.791272019556096,-0.00399376539654314,0.611451257996559));
#84749=DIRECTION('',(0.160246858747463,0.,-0.987076969775696));
#84750=DIRECTION('center_axis',(-7.72458675462459E-14,-1.,6.95175203573688E-14));
#84751=DIRECTION('ref_axis',(1.,-7.72458675462459E-14,-4.97137208957954E-31));
#84752=DIRECTION('center_axis',(-0.0777143321985765,-0.98736372173193,-0.138106348799036));
#84753=DIRECTION('ref_axis',(-0.79365683635452,-0.0225680000081501,0.60794696436726));
#84754=DIRECTION('center_axis',(0.117350647948898,-0.987363722424414,0.106497441594521));
#84755=DIRECTION('ref_axis',(-0.741164064492037,-0.0156997409901681,0.671140333789056));
#84756=DIRECTION('center_axis',(0.0976123325991251,0.987363722676726,0.124838742650328));
#84757=DIRECTION('ref_axis',(-0.69313047612766,-0.0225682612557523,0.720458754299603));
#84758=DIRECTION('',(-0.998447996527108,0.,0.0556919943169951));
#84759=DIRECTION('center_axis',(-0.12407970139484,0.987363721847796,-0.0985753949047921));
#84760=DIRECTION('ref_axis',(-0.64132857471426,-0.0039937650622799,0.767255960612626));
#84761=DIRECTION('',(-0.0556919954647224,0.,-0.998447996463089));
#84762=DIRECTION('center_axis',(-3.8890086548536E-14,-1.,5.43200255894411E-14));
#84763=DIRECTION('ref_axis',(2.22889452794712E-31,-5.43200255894411E-14,
-1.));
#84764=DIRECTION('center_axis',(-0.105586202327676,-0.987363721951747,-0.118171208217622));
#84765=DIRECTION('ref_axis',(-0.644410957040571,-0.0225679906816595,0.764346259389452));
#84766=DIRECTION('center_axis',(0.137500857919152,-0.987363722378517,0.0787806689634994));
#84767=DIRECTION('ref_axis',(-0.579560727718488,-0.0156997425922317,0.814777810798106));
#84768=DIRECTION('center_axis',(0.122166850809071,0.987363722695286,0.100936314915398));
#84769=DIRECTION('ref_axis',(-0.522048136227153,-0.0225682595929491,0.852617391988166));
#84770=DIRECTION('',(-0.963132705018756,0.,0.269026750571861));
#84771=DIRECTION('center_axis',(-0.142369580929604,0.987363721818591,-0.0695972934995943));
#84772=DIRECTION('ref_axis',(-0.461397319791492,-0.00399376042415553,0.887184627440592));
#84773=DIRECTION('',(-0.269026752423883,0.,-0.96313270450144));
#84774=DIRECTION('center_axis',(1.75357720910963E-14,-1.,-4.09401817561554E-14));
#84775=DIRECTION('ref_axis',(-1.24104711689061E-32,4.09401817561554E-14,
-1.));
#84776=DIRECTION('center_axis',(-0.128520969011961,-0.987363721781514,-0.0927105249364065));
#84777=DIRECTION('ref_axis',(-0.465033134446565,-0.0225679979504978,0.88500557587809));
#84778=DIRECTION('center_axis',(0.151221679088339,-0.987363722402413,0.0473802011113796));
#84779=DIRECTION('ref_axis',(-0.390857774145752,-0.0156997419415777,0.920317183634423));
#84780=DIRECTION('center_axis',(0.14100898137543,0.987363722679383,0.0723142192668541));
#84781=DIRECTION('ref_axis',(-0.326555403018843,-0.0225682609843977,0.944908589417697));
#84782=DIRECTION('',(-0.882782397777927,0.,0.469782117766793));
#84783=DIRECTION('center_axis',(-0.154002420805334,0.987363721837519,-0.0373648924159926));
#84784=DIRECTION('ref_axis',(-0.259891633084747,-0.00399376345168055,0.965629529843633));
#84785=DIRECTION('',(-0.469782117592815,0.,-0.882782397870512));
#84786=DIRECTION('center_axis',(-1.38747776376638E-15,-1.,7.2921159442934E-15));
#84787=DIRECTION('ref_axis',(-8.70967686797131E-33,-7.2921159442934E-15,
-1.));
#84788=DIRECTION('center_axis',(-0.145446243500322,-0.987363721891815,-0.0629147911352066));
#84789=DIRECTION('ref_axis',(-0.263910877837491,-0.0225679941728419,0.964283015612149));
#84790=DIRECTION('center_axis',(0.157871543102428,-0.98736372238965,0.0137642866619683));
#84791=DIRECTION('ref_axis',(-0.183878747956065,-0.0156997429578689,0.982823546788113));
#84792=DIRECTION('center_axis',(0.153257689853346,0.987363722748906,0.0403107864006331));
#84793=DIRECTION('ref_axis',(-0.115793303377786,-0.0225682571521611,0.993016910561937));
#84794=DIRECTION('',(-0.761154167861,0.,0.648570992835656));
#84795=DIRECTION('center_axis',(-4.25100139972006E-16,-1.,-1.48397940626387E-14));
#84796=DIRECTION('ref_axis',(0.0286342151763591,-1.48458815147681E-14,0.999589956792901));
#84797=DIRECTION('center_axis',(-0.155570611353887,-0.987363721584867,-0.0301772460814274));
#84798=DIRECTION('ref_axis',(-0.0504484436952952,-0.0225680051134673,0.998471651913023));
#84799=DIRECTION('center_axis',(0.157139508945422,-0.98736372241605,-0.0204952283498716));
#84800=DIRECTION('ref_axis',(0.0316982446689963,-0.0156997415914642,0.999374173870261));
#84801=DIRECTION('center_axis',(-0.15843427719912,0.987363721829461,-0.00338535426014318));
#84802=DIRECTION('ref_axis',(-0.0462337054453067,-0.00399376289762505,0.998922666845995));
#84803=DIRECTION('',(-0.648570992291408,0.,-0.761154168324748));
#84804=DIRECTION('center_axis',(-0.153405773087261,-0.987363727283469,-0.0397434123899093));
#84805=DIRECTION('ref_axis',(-0.157173522146972,-0.0153270656264595,0.987452057061606));
#84806=DIRECTION('',(0.562332021776287,0.,0.82691154139061));
#84807=DIRECTION('',(0.826911541049425,0.,-0.562332022278));
#84808=DIRECTION('center_axis',(0.153863114323219,-0.987363722524759,0.0379344367667496));
#84809=DIRECTION('ref_axis',(-0.219708301913583,0.00324330723637056,0.975560220093265));
#84810=DIRECTION('center_axis',(-0.141275571303142,-0.987363727223331,-0.0717919432570488));
#84811=DIRECTION('ref_axis',(-0.365771893840048,-0.0153270694356919,0.930578316220176));
#84812=DIRECTION('',(0.371423474713531,0.,0.928463570869491));
#84813=DIRECTION('center_axis',(-1.7351823490725E-14,-1.,5.67918761022166E-14));
#84814=DIRECTION('ref_axis',(-1.49127156747896E-31,-5.67918761022166E-14,
-1.));
#84815=DIRECTION('center_axis',(0.15047035997798,0.987363722444626,0.0497146896640039));
#84816=DIRECTION('ref_axis',(-0.221566403652918,-0.0153275630368041,0.975024817419364));
#84817=DIRECTION('center_axis',(-0.146402532268554,0.987363725081384,-0.0606561863190324));
#84818=DIRECTION('ref_axis',(-0.294469331016928,0.0150385452734834,0.955542597295641));
#84819=DIRECTION('',(0.928463571527175,0.,-0.37142347306949));
#84820=DIRECTION('center_axis',(0.14211109818593,-0.987363722486231,0.0701235715756216));
#84821=DIRECTION('ref_axis',(-0.424288253350281,0.00324330658409198,0.905521374143851));
#84822=DIRECTION('center_axis',(-0.122539482670012,-0.987363727276341,-0.10048355709238));
#84823=DIRECTION('ref_axis',(-0.557267181460097,-0.015327066655971,0.830191766699263));
#84824=DIRECTION('',(0.163147578338454,0.,0.986601676302193));
#84825=DIRECTION('center_axis',(2.91547221559089E-14,-1.,-5.17339845454345E-14));
#84826=DIRECTION('ref_axis',(-1.1435928490905E-30,5.17339845454345E-14,
-1.));
#84827=DIRECTION('center_axis',(0.136265258712005,0.98736372244224,0.0808990659597058));
#84828=DIRECTION('ref_axis',(-0.425987817925329,-0.0153275614763488,0.904599051977397));
#84829=DIRECTION('center_axis',(-0.129940438600569,0.987363725138663,-0.0907102899157286));
#84830=DIRECTION('ref_axis',(-0.492998214050994,0.0150385390808293,0.869900341007431));
#84831=DIRECTION('',(0.986601676591079,0.,-0.163147576591479));
#84832=DIRECTION('center_axis',(0.123714122094534,-0.987363722509705,0.0990338097124305));
#84833=DIRECTION('ref_axis',(-0.609028958882343,0.00324331036576084,0.793141354476338));
#84834=DIRECTION('center_axis',(-0.0980735815685175,-0.987363727196121,
-0.124476675789915));
#84835=DIRECTION('ref_axis',(-0.722705274136803,-0.0153270691020051,0.690986373011502));
#84836=DIRECTION('',(-0.0527569189652392,0.,0.998607384061071));
#84837=DIRECTION('center_axis',(9.89859460105397E-14,-1.,-1.10642673273612E-13));
#84838=DIRECTION('ref_axis',(3.23530552762749E-30,1.10642673273612E-13,
-1.));
#84839=DIRECTION('center_axis',(0.115688545146719,0.987363722462374,0.10830069292059));
#84840=DIRECTION('ref_axis',(-0.610490517346357,-0.0153275606209121,0.791875238983762));
#84841=DIRECTION('center_axis',(-0.107402468389288,0.987363725040729,-0.116522891560345));
#84842=DIRECTION('ref_axis',(-0.66847504879309,0.0150385452406436,0.743582511425679));
#84843=DIRECTION('',(0.998607383967675,0.,0.052756920733087));
#84844=DIRECTION('center_axis',(0.0995324170010677,-0.987363722526679,0.123313330196635));
#84845=DIRECTION('ref_axis',(-0.765292145204351,0.00324330536830047,0.643674928406265));
#84846=DIRECTION('center_axis',(-0.0690218637930236,-0.987363727041147,
-0.142649405333328));
#84847=DIRECTION('ref_axis',(-0.854350472246275,-0.0153270762106045,0.519471222790446));
#84848=DIRECTION('',(-0.266194559677108,0.,0.963919320481912));
#84849=DIRECTION('center_axis',(0.,-1.,0.));
#84850=DIRECTION('ref_axis',(0.,0.,-1.));
#84851=DIRECTION('center_axis',(0.0897023623906408,0.987363722436819,0.130638301417487));
#84852=DIRECTION('ref_axis',(-0.766447355673877,-0.0153275625774428,0.642124222254507));
#84853=DIRECTION('center_axis',(-0.0798424829433611,0.987363725095465,-0.136887005530275));
#84854=DIRECTION('ref_axis',(-0.812694733563037,0.0150385427962143,0.582495589914181));
#84855=DIRECTION('',(0.963919320010511,0.,0.2661945613841));
#84856=DIRECTION('center_axis',(0.0706966795421928,-0.987363722499517,0.141826862736246));
#84857=DIRECTION('ref_axis',(-0.885771123801721,0.00324330962918667,0.464110975071356));
#84858=DIRECTION('center_axis',(-0.0367427722384984,-0.987363727231605,
-0.154151999129244));
#84859=DIRECTION('ref_axis',(-0.946047190512105,-0.015327068845835,0.323666177233194));
#84860=DIRECTION('',(-0.467185239535495,0.,0.884159460708396));
#84861=DIRECTION('center_axis',(-8.17769184107928E-14,-1.,3.53120703705101E-14));
#84862=DIRECTION('ref_axis',(1.,-8.17769184107928E-14,4.80900128964418E-31));
#84863=DIRECTION('center_axis',(0.0595218018669185,0.987363722479098,0.146867404943148));
#84864=DIRECTION('ref_axis',(-0.886565968493784,-0.015327558313575,0.46234819072299));
#84865=DIRECTION('center_axis',(-0.0485491517023675,0.987363725125182,-0.150850436445856));
#84866=DIRECTION('ref_axis',(-0.918913715657819,0.015038541178121,0.394171822249098));
#84867=DIRECTION('',(0.88415945988124,0.,0.467185241100908));
#84868=DIRECTION('center_axis',(0.0385552524335785,-0.987363722507462,0.153708724495363));
#84869=DIRECTION('ref_axis',(-0.964832426832062,0.00324330488953956,0.262845713502707));
#84870=DIRECTION('center_axis',(-0.00274561996653052,-0.987363727123007,
-0.15844662171458));
#84871=DIRECTION('ref_axis',(-0.99350779309227,-0.0153270730418421,0.112726864131391));
#84872=DIRECTION('',(-0.646330857894656,0.,0.763057286272242));
#84873=DIRECTION('center_axis',(5.83040472254443E-14,-1.,-1.12712490979864E-14));
#84874=DIRECTION('ref_axis',(1.,5.83040472254443E-14,1.95425793165654E-31));
#84875=DIRECTION('center_axis',(0.0265580647611155,0.987363722491237,0.156229154463538));
#84876=DIRECTION('ref_axis',(-0.96522974321078,-0.0153275578722416,0.260953269362401));
#84877=DIRECTION('center_axis',(-0.0149857128551614,0.9873637250895,-0.157760269990921));
#84878=DIRECTION('ref_axis',(-0.982165313426428,0.0150385434514299,0.187417019805635));
#84879=DIRECTION('',(0.763057286545784,0.,0.646330857571712));
#84880=DIRECTION('center_axis',(0.00461101746230197,-0.987363722509209,
0.158403339581966));
#84881=DIRECTION('ref_axis',(-0.998779239687249,0.00324330703679607,0.0492900733335472));
#84882=DIRECTION('center_axis',(0.0313799112010356,-0.987363727124713,-0.155332454855419));
#84883=DIRECTION('ref_axis',(-0.994513076466955,-0.0153270729185943,-0.103483436220397));
#84884=DIRECTION('',(-0.795254762302715,0.,0.606275401970797));
#84885=DIRECTION('center_axis',(0.,-1.,0.));
#84886=DIRECTION('ref_axis',(0.,0.,-1.));
#84887=DIRECTION('center_axis',(-0.00764750030215644,0.987363722476008,
0.158285802513836));
#84888=DIRECTION('ref_axis',(-0.998760447427132,-0.0153275598347146,0.0473564627550317));
#84889=DIRECTION('center_axis',(0.0192784397313903,0.987363725081687,-0.157293407854043));
#84890=DIRECTION('ref_axis',(-0.999491953403475,0.0150385434598007,-0.0281011973466172));
#84891=DIRECTION('',(0.606275400562902,0.,0.795254763376047));
#84892=DIRECTION('center_axis',(-0.0295488213498787,-0.987363722475921,
0.155691190166067));
#84893=DIRECTION('ref_axis',(-0.986024244800647,0.00324330709653314,-0.166570314355205));
#84894=DIRECTION('center_axis',(0.0640381510629094,-0.987363727167838,-0.144955115403629));
#84895=DIRECTION('ref_axis',(-0.949016033550402,-0.0153270713953641,-0.314854964938944));
#84896=DIRECTION('',(-0.906993438031825,0.,0.421144753460387));
#84897=DIRECTION('center_axis',(-1.15295989682027E-13,-1.,-2.8503450786955E-14));
#84898=DIRECTION('ref_axis',(1.,-1.15295989682027E-13,1.50992885536303E-31));
#84899=DIRECTION('center_axis',(-0.041495475479177,0.987363722444346,0.152941181882454));
#84900=DIRECTION('ref_axis',(-0.985590222827933,-0.0153275606837138,-0.168454678027869));
#84901=DIRECTION('center_axis',(0.0526411530319517,0.987363725091179,-0.149471680868111));
#84902=DIRECTION('ref_axis',(-0.970083460286782,0.0150385428657411,-0.242305431855127));
#84903=DIRECTION('',(0.421144752952713,0.,0.906993438267554));
#84904=DIRECTION('center_axis',(-0.0623269906669315,-0.98736372250425,0.145699093054675));
#84905=DIRECTION('ref_axis',(-0.927163852952879,0.00324330825580986,-0.374642056807736));
#84906=DIRECTION('center_axis',(0.0937020379828365,-0.987363727189288,-0.127799836888554));
#84907=DIRECTION('ref_axis',(-0.859144055829087,-0.0153270694498359,-0.511504225080914));
#84908=DIRECTION('',(-0.976322108155361,0.,0.216321846162313));
#84909=DIRECTION('center_axis',(7.98547755975139E-14,-1.,3.94667141899776E-14));
#84910=DIRECTION('ref_axis',(1.,7.98547755975138E-14,-2.26916646106724E-30));
#84911=DIRECTION('center_axis',(-0.073403164279386,0.987363722488244,0.140445202794295));
#84912=DIRECTION('ref_axis',(-0.926334895999688,-0.0153275575962674,-0.37638906258203));
#84913=DIRECTION('center_axis',(0.0835424247531459,0.987363725082729,-0.134660824507808));
#84914=DIRECTION('ref_axis',(-0.895314942855587,0.0150385423990028,-0.445179733750325));
#84915=DIRECTION('',(0.216321844433724,0.,0.976322108538361));
#84916=DIRECTION('center_axis',(-0.0921908136359495,-0.987363722493434,
0.128894272118859));
#84917=DIRECTION('ref_axis',(-0.824950308713439,0.00324330202760705,-0.565195956412959));
#84918=DIRECTION('center_axis',(0.118984524740799,-0.987363727165298,-0.104668778298292));
#84919=DIRECTION('ref_axis',(-0.729099456103866,-0.0153270708733323,-0.684236117146333));
#84920=DIRECTION('',(-0.999999042317255,0.,0.00138396696961088));
#84921=DIRECTION('center_axis',(-2.31678794544605E-14,-1.,-1.85701401945779E-14));
#84922=DIRECTION('ref_axis',(1.,-2.31678794544605E-14,-7.0999417749956E-31));
#84923=DIRECTION('center_axis',(-0.101878611122322,0.987363722418195,0.12138215786627));
#84924=DIRECTION('ref_axis',(-0.82376517608398,-0.0153275631584234,-0.566723919099021));
#84925=DIRECTION('center_axis',(0.110537343690459,0.987363725132923,-0.113553379260571));
#84926=DIRECTION('ref_axis',(-0.778682493658275,0.0150385393935025,-0.627237926470523));
#84927=DIRECTION('',(0.00138396519504415,0.,0.999999042319711));
#84928=DIRECTION('center_axis',(-0.117743905255329,-0.987363722487702,0.106062492382807));
#84929=DIRECTION('ref_axis',(-0.684163005159501,0.00324330677383027,-0.72932192023296));
#84930=DIRECTION('center_axis',(0.138703424939811,-0.987363727212438,-0.0766435261136204));
#84931=DIRECTION('ref_axis',(-0.564962976342534,-0.0153270690604205,-0.82497388826326));
#84932=DIRECTION('',(-0.97691713277092,0.,-0.213618622078332));
#84933=DIRECTION('center_axis',(1.86341961019305E-14,-1.,2.31163898898676E-14));
#84934=DIRECTION('ref_axis',(-2.47023409854845E-31,-2.31163898898676E-14,
-1.));
#84935=DIRECTION('center_axis',(-0.125590320890986,0.987363722425395,0.0966434215907506));
#84936=DIRECTION('ref_axis',(-0.682677114237897,-0.0153275619638483,-0.730559390836955));
#84937=DIRECTION('center_axis',(0.13236366662272,0.987363725051147,-0.0871362967500453));
#84938=DIRECTION('ref_axis',(-0.625639715317128,0.0150385470019746,-0.779967171566837));
#84939=DIRECTION('',(-0.213618626551051,0.,0.976917131792888));
#84940=DIRECTION('center_axis',(-0.13779142013565,-0.987363722500148,0.0782713487021446));
#84941=DIRECTION('ref_axis',(-0.511385000068983,0.00324330953190384,-0.859345601401279));
#84942=DIRECTION('center_axis',(0.151936708248103,-0.987363727213298,-0.0450345075491616));
#84943=DIRECTION('ref_axis',(-0.374409458267511,-0.0153270686067452,-0.927136796016507));
#84944=DIRECTION('',(-0.908155662980834,0.,-0.418632645401481));
#84945=DIRECTION('center_axis',(1.32291984440385E-14,-1.,2.6581742884735E-14));
#84946=DIRECTION('ref_axis',(-2.29532064287214E-31,-2.6581742884735E-14,
-1.));
#84947=DIRECTION('center_axis',(-0.143429566062224,0.987363722443134,0.0673857491049875));
#84948=DIRECTION('ref_axis',(-0.509667831387102,-0.0153275583912248,-0.860234716576198));
#84949=DIRECTION('center_axis',(0.14800080553809,0.987363725055514,-0.0566448232813552));
#84950=DIRECTION('ref_axis',(-0.443342720814214,0.0150385466523101,-0.896226017261068));
#84951=DIRECTION('',(-0.418632647009715,0.,0.908155662239486));
#84952=DIRECTION('center_axis',(-0.15139595935967,-0.987363722529884,0.0468203259439202));
#84953=DIRECTION('ref_axis',(-0.314695199533534,0.00324330913949309,-0.949187237765223));
#84954=DIRECTION('center_axis',(0.15806560158646,-0.987363727076912,-0.0113197194267311));
#84955=DIRECTION('ref_axis',(-0.166348965609218,-0.0153270737247311,-0.985947819335172));
#84956=DIRECTION('',(-0.79692984530751,0.,-0.604071867957902));
#84957=DIRECTION('center_axis',(0.,-1.,0.));
#84958=DIRECTION('ref_axis',(0.,0.,-1.));
#84959=DIRECTION('center_axis',(-0.154562207296368,0.987363722441907,0.0349771880135615));
#84960=DIRECTION('ref_axis',(-0.312827044980643,-0.0153275612519601,-0.949686424981818));
#84961=DIRECTION('center_axis',(0.156717592653502,0.987363725001226,-0.0235046953733427));
#84962=DIRECTION('ref_axis',(-0.240315511502135,0.0150385517052381,-0.97057833114802));
#84963=DIRECTION('',(-0.604071869369054,0.,0.796929844237858));
#84964=DIRECTION('',(-0.648440472711469,0.,-0.761265363293068));
#84965=DIRECTION('',(-0.761265364441084,0.,0.648440471363705));
#84966=DIRECTION('center_axis',(-0.15706259615762,-0.987363722513704,-0.0210765355813124));
#84967=DIRECTION('ref_axis',(0.11294374790137,0.00324330843188972,-0.993596090350806));
#84968=DIRECTION('center_axis',(0.148209482175692,-0.987363727203217,0.0560965203607491));
#84969=DIRECTION('ref_axis',(0.263014511757221,-0.0153270696763623,-0.964670123690086));
#84970=DIRECTION('',(-0.46963074398653,0.,-0.88286293630589));
#84971=DIRECTION('center_axis',(0.,-1.,0.));
#84972=DIRECTION('ref_axis',(0.,0.,-1.));
#84973=DIRECTION('center_axis',(-0.154963399384117,0.987363722388463,-0.0331545556826997));
#84974=DIRECTION('ref_axis',(0.114848845116973,-0.0153275664721359,-0.993264722257536));
#84975=DIRECTION('center_axis',(0.152102401169859,0.987363725054083,0.0444717214158533));
#84976=DIRECTION('ref_axis',(0.189430811856307,0.0150385476419998,-0.98177890056992));
#84977=DIRECTION('',(-0.882862937137393,0.,0.46963074242338));
#84978=DIRECTION('center_axis',(-0.148859727349044,-0.9873637225025,-0.0543475947910742));
#84979=DIRECTION('ref_axis',(0.323896974311614,0.00324331006221809,-0.946086798857072));
#84980=DIRECTION('center_axis',(0.132685333069044,-0.987363727208248,0.0866456726085828));
#84981=DIRECTION('ref_axis',(0.464240939393531,-0.0153270698761599,-0.885576327100055));
#84982=DIRECTION('',(-0.26886160500068,0.,-0.963178818992849));
#84983=DIRECTION('center_axis',(4.67807765707652E-14,-1.,-1.09165795252073E-13));
#84984=DIRECTION('ref_axis',(2.870235819188E-31,1.09165795252073E-13,-1.));
#84985=DIRECTION('center_axis',(-0.144213194894241,0.987363722466965,-0.0656919627852075));
#84986=DIRECTION('ref_axis',(0.325686296658284,-0.0153275579518285,-0.945353638664519));
#84987=DIRECTION('center_axis',(0.138986227524642,0.98736372509821,0.0761295141101926));
#84988=DIRECTION('ref_axis',(0.39605546709624,0.0150385439839594,-0.918103430544741));
#84989=DIRECTION('',(-0.963178819468904,-2.49350829358902E-15,0.268861603295241));
#84990=DIRECTION('center_axis',(-0.133696343123587,-0.987363722536948,-0.0850774191743116));
#84991=DIRECTION('ref_axis',(0.519705138598534,0.00324331000604487,-0.854339540144598));
#84992=DIRECTION('center_axis',(0.110956963422593,-0.987363727101881,0.113143372194397));
#84993=DIRECTION('ref_axis',(0.643759976556952,-0.0153270733983734,-0.765073965969587));
#84994=DIRECTION('',(-0.0555207965247666,0.,-0.998457530971275));
#84995=DIRECTION('center_axis',(-1.72886217674519E-14,-1.,2.41392688765716E-14));
#84996=DIRECTION('ref_axis',(5.39604775529338E-31,-2.41392688765716E-14,
-1.));
#84997=DIRECTION('center_axis',(-0.126719736909377,0.987363722443892,-0.0951577000529103));
#84998=DIRECTION('ref_axis',(0.521295021806607,-0.0153275636165744,-0.853238868098042));
#84999=DIRECTION('center_axis',(0.11937121039447,0.987363725046559,0.104227580760289));
#85000=DIRECTION('ref_axis',(0.584161008503692,0.0150385463260237,-0.81149846473567));
#85001=DIRECTION('',(-0.998457531228927,-2.49350828872853E-15,0.0555207918912913));
#85002=DIRECTION('center_axis',(-0.112281469383263,-0.987363722483312,-0.111829115873426));
#85003=DIRECTION('ref_axis',(0.691212468285046,0.00324330645825146,-0.722644314065026));
#85004=DIRECTION('center_axis',(0.0840403717824719,-0.987363727152753,0.134350609279183));
#85005=DIRECTION('ref_axis',(0.793177513644596,-0.0153270718563438,-0.608797595853407));
#85006=DIRECTION('',(0.160416105690236,0.,-0.987049478514213));
#85007=DIRECTION('center_axis',(2.2073652675844E-14,-1.,-1.9858363567774E-14));
#85008=DIRECTION('ref_axis',(1.,2.2073652675844E-14,-3.01044548961814E-31));
#85009=DIRECTION('center_axis',(-0.103301011992431,0.987363722464074,-0.120173959255853));
#85010=DIRECTION('ref_axis',(0.692528568071411,-0.0153275573522582,-0.721227598189763));
#85011=DIRECTION('center_axis',(0.0941745282129391,0.987363725059354,0.127452079907653));
#85012=DIRECTION('ref_axis',(0.744951831282862,0.0150385470532171,-0.666948732040806));
#85013=DIRECTION('',(-0.987049478230213,0.,-0.160416107437699));
#85014=DIRECTION('center_axis',(-0.0856164309490843,-0.987363722505332,
-0.133351813755776));
#85015=DIRECTION('ref_axis',(0.830399471803581,0.00324331317645552,-0.557159042058884));
#85016=DIRECTION('center_axis',(0.0531941425906414,-0.987363727074868,0.14927576377588));
#85017=DIRECTION('ref_axis',(0.905506951271153,-0.0153270746360375,-0.424054527133861));
#85018=DIRECTION('',(0.368852126985954,0.,-0.929488089443828));
#85019=DIRECTION('center_axis',(-2.5826544115284E-14,-1.,1.4648903240881E-14));
#85020=DIRECTION('ref_axis',(1.,-2.5826544115284E-14,5.41840065352129E-31));
#85021=DIRECTION('center_axis',(-0.075052037718006,0.987363722424622,-0.139571025912148));
#85022=DIRECTION('ref_axis',(0.831380248175949,-0.0153275636330696,-0.555492528064935));
#85023=DIRECTION('center_axis',(0.0645743547481768,0.98736372508055,0.144717058786852));
#85024=DIRECTION('ref_axis',(0.870909534039187,0.0150385421285242,-0.491213218236536));
#85025=DIRECTION('',(-0.929488088790823,0.,-0.368852128631492));
#85026=DIRECTION('center_axis',(-0.0549480768125023,-0.987363722501825,
-0.14863912116918));
#85027=DIRECTION('ref_axis',(0.93075791777958,0.0032433041339868,-0.365621634300973));
#85028=DIRECTION('center_axis',(0.0198606187809754,-0.987363727155474,0.157220946820986));
#85029=DIRECTION('ref_axis',(0.975495890339712,-0.0153270721634695,-0.219483140102441));
#85030=DIRECTION('',(0.560041033052935,0.,-0.828464870285398));
#85031=DIRECTION('center_axis',(0.,-1.,0.));
#85032=DIRECTION('ref_axis',(0.,0.,-1.));
#85033=DIRECTION('center_axis',(-0.0432937216744962,0.987363722469847,-0.152441901110088));
#85034=DIRECTION('ref_axis',(0.931357513590266,-0.0153275594589119,-0.363783242879591));
#85035=DIRECTION('center_axis',(0.0319547486199412,0.987363725072818,0.155215232664082));
#85036=DIRECTION('ref_axis',(0.956144474632417,0.0150385461158406,-0.292509120816121));
#85037=DIRECTION('',(-0.828464869293675,0.,-0.560041034519984));
#85038=DIRECTION('center_axis',(-0.0217103961479561,-0.987363722531891,
-0.156976234274701));
#85039=DIRECTION('ref_axis',(0.987595158629252,0.00324331204516959,-0.156988163818294));
#85040=DIRECTION('center_axis',(-0.0144015673470265,-0.987363727150147,
0.157814654472007));
#85041=DIRECTION('ref_axis',(0.999871725773331,-0.0153270717692356,-0.00464896440519302));
#85042=DIRECTION('',(0.725043043015264,0.,-0.688703554350612));
#85043=DIRECTION('center_axis',(-1.47952256911602E-13,-1.,1.22535004851514E-14));
#85044=DIRECTION('ref_axis',(1.,-1.47952256911602E-13,4.67698059803635E-31));
#85045=DIRECTION('center_axis',(-0.00951103288197081,0.987363722430219,
-0.158184765013131));
#85046=DIRECTION('ref_axis',(0.987785536274728,-0.0153275626069874,-0.155063858300302));
#85047=DIRECTION('center_axis',(-0.00215902604927871,0.987363725041648,
0.158455713303118));
#85048=DIRECTION('ref_axis',(0.996671162633965,0.0150385495453836,-0.0801276207149027));
#85049=DIRECTION('',(-0.688703551631228,0.,-0.725043045598351));
#85050=DIRECTION('center_axis',(0.0125424252946417,-0.987363722492876,-0.157973311267251));
#85051=DIRECTION('ref_axis',(0.998253547486997,0.00324330660448014,0.058985895703088));
#85052=DIRECTION('center_axis',(-0.0479903557107524,-0.987363727048957,
0.15102912390247));
#85053=DIRECTION('ref_axis',(0.977494670715387,-0.0153270753681568,0.210402589061247));
#85054=DIRECTION('',(0.856142845888465,0.,-0.51673922575512));
#85055=DIRECTION('center_axis',(-1.17701884843292E-13,-1.,-1.58706731088539E-14));
#85056=DIRECTION('ref_axis',(1.,-1.17701884843292E-13,4.44617853897246E-31));
#85057=DIRECTION('center_axis',(0.0247163783165966,0.987363722430302,-0.156531084042401));
#85058=DIRECTION('ref_axis',(0.998025805201912,-0.0153275624701153,0.0609061407396708));
#85059=DIRECTION('center_axis',(-0.0361718358223352,0.987363725075744,0.154286981621242));
#85060=DIRECTION('ref_axis',(0.990594614933057,0.0150385416996737,0.136000555620831));
#85061=DIRECTION('',(-0.516739224239438,0.,-0.85614284680328));
#85062=DIRECTION('center_axis',(0.0462087799976181,-0.987363722484958,-0.151583733203066));
#85063=DIRECTION('ref_axis',(0.962234710082633,0.00324330366222394,0.272201843663019));
#85064=DIRECTION('center_axis',(-0.0793351628521738,-0.987363727125316,
0.137181639778887));
#85065=DIRECTION('ref_axis',(0.909411050441021,-0.0153270726115122,0.415615955156824));
#85066=DIRECTION('',(0.94721036075467,0.,-0.320612745347106));
#85067=DIRECTION('center_axis',(8.36537658803244E-14,-1.,3.06015386714305E-14));
#85068=DIRECTION('ref_axis',(1.,8.36537658803244E-14,-1.22694844227837E-30));
#85069=DIRECTION('center_axis',(0.0577880795530927,0.987363722415614,-0.147558183504497));
#85070=DIRECTION('ref_axis',(0.961599496605368,-0.015327562862503,0.27402823567107));
#85071=DIRECTION('center_axis',(-0.06849329531904,0.987363725143355,0.142903963441803));
#85072=DIRECTION('ref_axis',(0.938198964110948,0.0150385380395308,0.345769498531576));
#85073=DIRECTION('',(-0.320612743670349,0.,-0.94721036132222));
#85074=DIRECTION('center_axis',(0.0777144716089803,-0.987363722534733,-0.138106264611323));
#85075=DIRECTION('ref_axis',(0.881222846599685,0.0032433098799736,0.472689935974704));
#85076=DIRECTION('center_axis',(-0.10697034869677,-0.987363727119017,0.11691969410384));
#85077=DIRECTION('ref_axis',(0.798804382014933,-0.0153270734635542,0.601395577047906));
#85078=DIRECTION('',(0.99398737210975,0.,-0.10949476739257));
#85079=DIRECTION('center_axis',(-5.00797073109942E-14,-1.,-3.1912785667902E-14));
#85080=DIRECTION('ref_axis',(1.,-5.00797073109942E-14,-1.28384215650724E-31));
#85081=DIRECTION('center_axis',(0.0881576724725291,0.987363722452936,-0.131685627036921));
#85082=DIRECTION('ref_axis',(0.880209864213759,-0.0153275610711369,0.474337075097874));
#85083=DIRECTION('center_axis',(-0.097612092652736,0.987363725102616,0.124838911079198));
#85084=DIRECTION('ref_axis',(0.841934171533672,0.0150385435014291,0.539370645301786));
#85085=DIRECTION('',(-0.109494768473299,0.,-0.9939873719907));
#85086=DIRECTION('center_axis',(0.105586311494449,-0.987363722473641,-0.118171106316189));
#85087=DIRECTION('ref_axis',(0.759005982455155,0.00324330483115373,0.65107557132107));
#85088=DIRECTION('center_axis',(-0.129603722111918,-0.987363727025109,0.0911907109842997));
#85089=DIRECTION('ref_axis',(0.650846506593612,-0.0153270770696368,0.759054613030836));
#85090=DIRECTION('',(0.994286638431596,0.,0.106743058961212));
#85091=DIRECTION('center_axis',(-4.20485661031268E-14,-1.,-4.19323393028766E-14));
#85092=DIRECTION('ref_axis',(1.,-4.20485661031268E-14,1.98718392696402E-30));
#85093=DIRECTION('center_axis',(0.114405110205379,0.987363722454575,-0.109655598760575));
#85094=DIRECTION('ref_axis',(0.757662596725444,-0.0153275579906525,0.652466440124931));
#85095=DIRECTION('center_axis',(-0.122166652612043,0.987363725061852,0.100936531650103));
#85096=DIRECTION('ref_axis',(0.706301474123408,0.0150385445990266,0.70775141810345));
#85097=DIRECTION('',(0.106743061026633,0.,-0.99428663820986));
#85098=DIRECTION('center_axis',(0.128521060442471,-0.987363722513769,-0.0927103903912335));
#85099=DIRECTION('ref_axis',(0.601298842027583,0.0032433111868436,0.799017636544297));
#85100=DIRECTION('center_axis',(-0.14617696274712,-0.987363727185108,0.0611977597723875));
#85101=DIRECTION('ref_axis',(0.472455772832713,-0.0153270698767051,0.881221098048633));
#85102=DIRECTION('',(0.9480941669185,0.,0.317989702121177));
#85103=DIRECTION('center_axis',(3.20512805188825E-14,-1.,4.9991183218023E-14));
#85104=DIRECTION('ref_axis',(9.98304756685787E-31,-4.9991183218023E-14,
-1.));
#85105=DIRECTION('center_axis',(0.135303096653766,0.987363722448722,-0.0824981916656709));
#85106=DIRECTION('ref_axis',(0.599687867911419,-0.0153275617382559,0.800087199579531));
#85107=DIRECTION('center_axis',(-0.141008833775221,0.987363725092081,0.0723144741365186));
#85108=DIRECTION('ref_axis',(0.537642905377994,0.0150385428868407,0.843038521376425));
#85109=DIRECTION('',(0.317989704666138,0.,-0.948094166064923));
#85110=DIRECTION('center_axis',(0.145446300746767,-0.987363722521415,-0.0629146489121133));
#85111=DIRECTION('ref_axis',(0.415475637959499,0.00324330610647331,0.909598524200456));
#85112=DIRECTION('center_axis',(-0.155915135243843,-0.987363727241485,0.0283432660379365));
#85113=DIRECTION('ref_axis',(0.271973531750121,-0.0153270677699031,0.962182664061737));
#85114=DIRECTION('',(0.857569866383666,0.,0.514367499236393));
#85115=DIRECTION('center_axis',(-1.02776563488674E-14,-1.,-2.78562474690747E-14));
#85116=DIRECTION('ref_axis',(-1.53922069392155E-31,2.78562474690747E-14,
-1.));
#85117=DIRECTION('center_axis',(0.149874458591521,0.987363722433168,-0.051483262181182));
#85118=DIRECTION('ref_axis',(0.413672401964247,-0.0153275633457503,0.910296770100286));
#85119=DIRECTION('center_axis',(-0.153257600591622,0.987363725089412,0.0403110684360965));
#85120=DIRECTION('ref_axis',(0.343844748655256,0.0150385450137742,0.938906082090255));
#85121=DIRECTION('',(0.514367502868879,0.,-0.857569864204913));
#85122=DIRECTION('center_axis',(0.155570636345677,-0.987363722485842,-0.0301770877637659));
#85123=DIRECTION('ref_axis',(0.210225250933983,0.00324330197631951,0.977647597481851));
#85124=DIRECTION('center_axis',(-0.158362890807331,-0.987363727153055,-0.00583653300974646));
#85125=DIRECTION('ref_axis',(0.0587741088908879,-0.0153270715028807,0.998153637975251));
#85126=DIRECTION('',(0.726946551156652,0.,0.686694045235176));
#85127=DIRECTION('center_axis',(-1.61964027106475E-14,-1.,-1.17657504934848E-13));
#85128=DIRECTION('ref_axis',(7.00547276313006E-31,1.17657504934848E-13,
-1.));
#85129=DIRECTION('center_axis',(0.157437856145186,0.987363722433385,-0.0180610374811915));
#85130=DIRECTION('ref_axis',(0.20831407392069,-0.0153275596268245,0.977941875840508));
#85131=DIRECTION('center_axis',(-0.158340210916804,0.987363725114748,0.00642276687656476));
#85132=DIRECTION('ref_axis',(0.133968796643142,0.0150385424311846,0.990871436548422));
#85133=DIRECTION('center_axis',(9.475145798617E-15,-1.,-1.18388485589748E-13));
#85134=DIRECTION('ref_axis',(3.34507738867976E-31,1.18388485589748E-13,
-1.));
#85135=DIRECTION('center_axis',(0.158420663065506,-0.987363722652752,0.00397148626897056));
#85136=DIRECTION('ref_axis',(-0.00485502709988203,0.00324326475489117,0.999982954827526));
#85137=DIRECTION('center_axis',(0.157639635277696,0.987363722413663,0.0162057104426415));
#85138=DIRECTION('ref_axis',(-0.0067847896129553,-0.015327565251928,0.99985950631744));
#85139=DIRECTION('center_axis',(-0.156019010174988,0.98736372512438,-0.0277658562361314));
#85140=DIRECTION('ref_axis',(-0.0821713885434937,0.0150385398846669,0.996504744204949));
#85141=DIRECTION('',(0.686694046522226,0.,-0.726946549940868));
#85142=DIRECTION('center_axis',(0.161633027721701,-0.986495109307913,-0.0264983709137736));
#85143=DIRECTION('ref_axis',(0.0329757751559212,-0.021437402364222,0.99922621864758));
#85144=DIRECTION('center_axis',(0.152157772461857,-0.986495109388684,-0.0606251716010378));
#85145=DIRECTION('ref_axis',(0.247008917377821,-0.0214373972602293,0.968776048803099));
#85146=DIRECTION('center_axis',(0.135567786644849,-0.986495109332269,-0.0919172154045821));
#85147=DIRECTION('ref_axis',(0.449492204001712,-0.0214374003032971,0.893026985264118));
#85148=DIRECTION('center_axis',(0.112638805325703,-0.986495109394101,-0.118911305923026));
#85149=DIRECTION('ref_axis',(0.630957728715546,-0.0214373968278044,0.775520974952559));
#85150=DIRECTION('center_axis',(0.0844429508784094,-0.986495109298641,-0.140345243513304));
#85151=DIRECTION('ref_axis',(0.782920372643902,-0.0214374043459836,0.621752465048624));
#85152=DIRECTION('center_axis',(0.0522986471423926,-0.986495109339015,-0.155216786325707));
#85153=DIRECTION('ref_axis',(0.898274530838002,-0.0214373995791351,0.438911500358616));
#85154=DIRECTION('center_axis',(0.0177089115152549,-0.986495109323431,-0.162830567566096));
#85155=DIRECTION('ref_axis',(0.971626369491964,-0.021437401334743,0.235547523722664));
#85156=DIRECTION('center_axis',(-0.0177088730347992,-0.986495109302549,
-0.162830571877608));
#85157=DIRECTION('ref_axis',(0.999546039841321,-0.0214374020191855,0.0211696016070285));
#85158=DIRECTION('center_axis',(-0.0522986060263791,-0.986495109352257,
-0.155216800095144));
#85159=DIRECTION('ref_axis',(0.980728047866526,-0.0214373990674815,-0.1941981824043));
#85160=DIRECTION('center_axis',(-0.0844429212236144,-0.986495109321542,
-0.140345261195033));
#85161=DIRECTION('ref_axis',(0.916052301958489,-0.0214374031897024,-0.400485477665591));
#85162=DIRECTION('center_axis',(-0.112638775583892,-0.986495109307086,-0.118911334817845));
#85163=DIRECTION('ref_axis',(0.808542968252034,-0.0214374034631445,-0.588046517057068));
#85164=DIRECTION('center_axis',(-0.135567764890909,-0.986495109299295,-0.091917247843127));
#85165=DIRECTION('ref_axis',(0.663227066358007,-0.0214374025783219,-0.748111152316851));
#85166=DIRECTION('center_axis',(-0.152157756514673,-0.986495109323669,-0.0606252126833621));
#85167=DIRECTION('ref_axis',(0.486899401442756,-0.0214374011196443,-0.873194944275287));
#85168=DIRECTION('center_axis',(-0.16163302008143,-0.986495109394794,-0.0264984142829452));
#85169=DIRECTION('ref_axis',(0.287804863568124,-0.0214373958016446,-0.957449110171281));
#85170=DIRECTION('center_axis',(-0.16355050573217,-0.986495109320764,0.00886743260276391));
#85171=DIRECTION('ref_axis',(0.0752528885113876,-0.0214374029907239,-0.996934020145619));
#85172=DIRECTION('center_axis',(-0.157820551393897,-0.986495109400653,0.0438186340079117));
#85173=DIRECTION('ref_axis',(-0.140817826880512,-0.0214373956793978,-0.989803403560088));
#85174=DIRECTION('center_axis',(-0.14471108034547,-0.986495109311796,0.0767209393135648));
#85175=DIRECTION('ref_axis',(-0.350304059732387,-0.0214374033023344,-0.936390678870022));
#85176=DIRECTION('center_axis',(-0.124835082058921,-0.986495109341509,0.106035850223527));
#85177=DIRECTION('ref_axis',(-0.543410459690549,-0.021437402805147,-0.839193368693935));
#85178=DIRECTION('center_axis',(-0.0991219325973794,-0.986495109282782,
0.130392644881959));
#85179=DIRECTION('ref_axis',(-0.711107593841883,-0.0214374044549463,-0.702756307457032));
#85180=DIRECTION('center_axis',(-0.0687739571027954,-0.986495109354319,
0.148652420244118));
#85181=DIRECTION('ref_axis',(-0.84555412615911,-0.0214373992962003,-0.533459143371561));
#85182=DIRECTION('center_axis',(-0.0352101828835034,-0.986495109356184,
0.159961377331033));
#85183=DIRECTION('ref_axis',(-0.940463487107214,-0.0214374005833562,-0.3392180232157));
#85184=DIRECTION('center_axis',(-2.29072636489518E-8,-0.986495109393899,
0.163790717508406));
#85185=DIRECTION('ref_axis',(-0.991397821399262,-0.0214373980985389,-0.129115443257425));
#85186=DIRECTION('center_axis',(0.0352101442534024,-0.986495109312445,0.159961386103901));
#85187=DIRECTION('ref_axis',(-0.995975494961977,-0.0214374023636677,0.0870244288412309));
#85188=DIRECTION('center_axis',(0.0687739176294749,-0.986495109353612,0.148652438511108));
#85189=DIRECTION('ref_axis',(-0.953982461632991,-0.0214373995559519,0.299095136698905));
#85190=DIRECTION('center_axis',(0.0991219030583523,-0.986495109317149,0.130392667076936));
#85191=DIRECTION('ref_axis',(-0.867382267681587,-0.0214374007047037,0.497180489925514));
#85192=DIRECTION('center_axis',(0.124835057371591,-0.986495109317044,0.106035879515309));
#85193=DIRECTION('ref_axis',(-0.740224245270894,-0.021437401580189,0.672018232287358));
#85194=DIRECTION('center_axis',(0.144711062094892,-0.986495109348447,0.0767209732665392));
#85195=DIRECTION('ref_axis',(-0.578454156478538,-0.0214373999808668,0.8154331528303));
#85196=DIRECTION('center_axis',(0.1578205394305,-0.986495109336992,0.0438186785293996));
#85197=DIRECTION('ref_axis',(-0.389636195492413,-0.0214374002396133,0.920719323699228));
#85198=DIRECTION('center_axis',(0.163550503166418,-0.986495109376726,0.00886747369963931));
#85199=DIRECTION('ref_axis',(-0.182599282568975,-0.0214373983432661,0.982953681491436));
#85200=DIRECTION('center_axis',(-0.160229046173638,0.986495109397072,-0.0339713393604832));
#85201=DIRECTION('ref_axis',(-0.0830851096497846,0.020814952117708,0.996325048527247));
#85202=DIRECTION('center_axis',(0.157123543110423,0.986495109271922,0.0462557194626253));
#85203=DIRECTION('ref_axis',(-0.18963547562865,-0.0158280458834692,0.981726978006923));
#85204=DIRECTION('center_axis',(-0.149180147486952,0.98649510939812,-0.0676216143652457));
#85205=DIRECTION('ref_axis',(-0.295323059389635,0.020814949454296,0.955170680282828));
#85206=DIRECTION('center_axis',(0.143506470660469,0.986495109262567,0.0789512018883271));
#85207=DIRECTION('ref_axis',(-0.396244184410726,-0.0158280437673955,0.918008725095342));
#85208=DIRECTION('center_axis',(-0.131155749138624,0.986495109406565,-0.0981099820854892));
#85209=DIRECTION('ref_axis',(-0.493752032498834,0.020814951281715,0.869353592162827));
#85210=DIRECTION('center_axis',(0.123179189100121,0.986495109195954,0.107955022602464));
#85211=DIRECTION('ref_axis',(-0.58432495687368,-0.0158280522011428,0.811365403217372));
#85212=DIRECTION('center_axis',(-0.106998655213202,0.986495109384959,-0.124010833970759));
#85213=DIRECTION('ref_axis',(-0.669093708611319,0.0208149505950684,0.742886496665861));
#85214=DIRECTION('center_axis',(0.097092189150081,0.986495109219769,0.131910978661827));
#85215=DIRECTION('ref_axis',(-0.745083340957672,-0.0158280526239247,0.666783538922106));
#85216=DIRECTION('center_axis',(-0.0778384228895612,0.986495109391339,-0.144113077369946));
#85217=DIRECTION('ref_axis',(-0.8131493056209,0.0208149504930532,0.581682855690469));
#85218=DIRECTION('center_axis',(0.066465272464082,0.986495109238995,0.149698921184551));
#85219=DIRECTION('ref_axis',(-0.871002456793015,-0.0158280462852299,0.491023617773447));
#85220=DIRECTION('center_axis',(-0.0450385516176566,0.986495109416014,-0.15747675373359));
#85221=DIRECTION('ref_axis',(-0.919182947471826,0.0208149504743908,0.393280366804337));
#85222=DIRECTION('center_axis',(0.0327305050275662,0.986495109232261,0.160487113194395));
#85223=DIRECTION('ref_axis',(-0.956194466999986,-0.0158280494827267,0.292303975560005));
#85224=DIRECTION('center_axis',(-0.0101327330925777,0.986495109448707,-0.163476991512135));
#85225=DIRECTION('ref_axis',(-0.982236614171915,0.0208149459504699,0.186488529956059));
#85226=DIRECTION('center_axis',(-0.00253469703033147,0.986495109264329,
0.163771104620211));
#85227=DIRECTION('ref_axis',(-0.996675886002857,-0.0158280452887455,0.079916526718559));
#85228=DIRECTION('center_axis',(0.0252468874683863,0.986495109426824,-0.161833228201498));
#85229=DIRECTION('ref_axis',(-0.9993619893109,0.02081494807157,-0.029023305417169));
#85230=DIRECTION('center_axis',(-0.037681384372286,0.986495109269882,0.159397342068155));
#85231=DIRECTION('ref_axis',(-0.990553848653424,-0.0158280461198542,-0.136207730595283));
#85232=DIRECTION('center_axis',(0.0594459888264633,0.986495109421206,-0.15262232307394));
#85233=DIRECTION('ref_axis',(-0.969758308850799,0.0208149474045697,-0.24317804255192));
#85234=DIRECTION('center_axis',(-0.0710661339837401,0.986495109226173,0.14757033602132));
#85235=DIRECTION('ref_axis',(-0.938114613916673,-0.015828048803026,-0.345963067432148));
#85236=DIRECTION('center_axis',(0.0908654631635529,0.98649510941151,-0.136274967294975));
#85237=DIRECTION('ref_axis',(-0.894809806919867,0.0208149477677228,-0.44596204702806));
#85238=DIRECTION('center_axis',(-0.101127910663473,0.986495109187203,0.128843103170366));
#85239=DIRECTION('ref_axis',(-0.841810182221258,-0.0158280527582371,-0.539541555261961));
#85240=DIRECTION('center_axis',(0.118036168935702,0.986495109427504,-0.113555545433062));
#85241=DIRECTION('ref_axis',(-0.778020993295535,0.0208149479903139,-0.627893360318128));
#85242=DIRECTION('center_axis',(-0.126461053175876,0.986495109247567,0.104091313087494));
#85243=DIRECTION('ref_axis',(-0.706143642576749,-0.0158280504594505,-0.70789167876667));
#85244=DIRECTION('center_axis',(0.139687634455818,0.98649510944765,-0.0855263925113603));
#85245=DIRECTION('ref_axis',(-0.624852784076839,0.0208149483880809,-0.780465076832413));
#85246=DIRECTION('center_axis',(-0.145881020994131,0.986495109214407,0.074472325126622));
#85247=DIRECTION('ref_axis',(-0.537458610002052,-0.0158280534109935,-0.843141574861471));
#85248=DIRECTION('center_axis',(0.154807460829294,0.986495109447023,-0.0534981224782106));
#85249=DIRECTION('ref_axis',(-0.442467151133643,0.0208149463326911,-0.896543115626262));
#85250=DIRECTION('center_axis',(-0.158479752553331,0.986495109210154,0.0413710954058669));
#85251=DIRECTION('ref_axis',(-0.343642610869599,-0.0158280543008508,-0.938967107353487));
#85252=DIRECTION('center_axis',(0.162688663350698,0.986495109444919,-0.018968338314703));
#85253=DIRECTION('ref_axis',(-0.239392246518749,0.0208149460742025,-0.970699794131344));
#85254=DIRECTION('center_axis',(-0.163668146516347,0.986495109199942,0.0063354037359762));
#85255=DIRECTION('ref_axis',(-0.133758266319021,-0.0158280507412877,-0.99088758141429));
#85256=DIRECTION('center_axis',(0.16296272472669,0.986495109485003,0.0164483832587217));
#85257=DIRECTION('ref_axis',(-0.025123626692503,0.0208149448285755,-0.999467629017368));
#85258=DIRECTION('center_axis',(-0.161203600904315,0.986495109252866,-0.0289965252342124));
#85259=DIRECTION('ref_axis',(0.0823804677645385,-0.0158280478511732,-0.996475253798165));
#85260=DIRECTION('center_axis',(0.155616830226651,0.986495109422284,0.0510960001969397));
#85261=DIRECTION('ref_axis',(0.190319746929274,0.0208149470435386,-0.981501468113192));
#85262=DIRECTION('center_axis',(-0.151201354025936,0.986495109218322,-0.0629726133256001));
#85263=DIRECTION('ref_axis',(0.294667181714052,-0.015828049706957,-0.955468850807378));
#85264=DIRECTION('center_axis',(0.140994463552116,0.986495109354395,0.0833544268021333));
#85265=DIRECTION('ref_axis',(0.39686397774258,0.0208149520937682,-0.917641390162667));
#85266=DIRECTION('center_axis',(-0.134129102511911,0.986495109263272,-0.0940041661789216));
#85267=DIRECTION('ref_axis',(0.493175586742465,-0.0158280447577772,-0.869785786064805));
#85268=DIRECTION('center_axis',(0.11977935520278,0.986495109416186,0.111715286174963));
#85269=DIRECTION('ref_axis',(0.584851292792108,0.0208149490328238,-0.810873419971429));
#85270=DIRECTION('center_axis',(-0.110785115663833,0.986495109186654,-0.12064019934567));
#85271=DIRECTION('ref_axis',(0.668623649731056,-0.0158280532216668,-0.743432503830398));
#85272=DIRECTION('center_axis',(0.0929634964319924,0.986495109410282,0.134852465460354));
#85273=DIRECTION('ref_axis',(0.74549160979465,0.0208149489752835,-0.66618991108012));
#85274=DIRECTION('center_axis',(-0.0822609475935,0.986495109233674,-0.14163522146366));
#85275=DIRECTION('ref_axis',(0.812807611767165,-0.0158280497325542,-0.58231714648894));
#85276=DIRECTION('center_axis',(0.0618007681567064,0.986495109400869,0.151684093376358));
#85277=DIRECTION('ref_axis',(0.871273569082446,0.0208149483613273,-0.490356100954247));
#85278=DIRECTION('center_axis',(-0.0498903480221808,0.986495109248187,-0.156007540214033));
#85279=DIRECTION('ref_axis',(0.918985594304392,-0.0158280482471485,-0.393973286340191));
#85280=DIRECTION('center_axis',(0.0277483075383048,0.986495109427382,0.161423141168227));
#85281=DIRECTION('ref_axis',(0.956315744374027,0.0208149448057552,-0.291593784458935));
#85282=DIRECTION('center_axis',(-0.0151869309708522,0.986495109262656,-0.163085120500148));
#85283=DIRECTION('ref_axis',(0.982192832897511,-0.015828046811078,-0.187207670619844));
#85284=DIRECTION('center_axis',(-0.00760163979730092,0.98649510939943,0.163614223719695));
#85285=DIRECTION('ref_axis',(0.996641657828032,0.0208149484683471,-0.0791968673752444));
#85286=DIRECTION('center_axis',(0.0202266118953025,0.986495109261528,-0.162537022165174));
#85287=DIRECTION('ref_axis',(0.999473825620694,-0.0158280474677465,0.0283115667615459));
#85288=DIRECTION('center_axis',(-0.0425961376215212,0.986495109425181,0.158154886550903));
#85289=DIRECTION('ref_axis',(0.990365715286638,0.0208149467752881,0.136903206593304));
#85290=DIRECTION('center_axis',(0.0546943881994909,0.986495109174822,-0.154388870951374));
#85291=DIRECTION('ref_axis',(0.970020532949181,-0.0158280559788013,0.24250698608683));
#85292=DIRECTION('center_axis',(-0.0755988898492081,0.986495109447872,0.14530040223275));
#85293=DIRECTION('ref_axis',(0.937781371961546,0.0208149472751966,0.34660184127014));
#85294=DIRECTION('center_axis',(0.0866047015303078,0.986495109243973,-0.139021671370213));
#85295=DIRECTION('ref_axis',(0.895210158480271,-0.0158280492832253,0.44536304854536));
#85296=DIRECTION('center_axis',(-0.105066720103058,0.986495109422893,0.12565183409525));
#85297=DIRECTION('ref_axis',(0.841347414505468,0.0208149457481815,0.54009375680382));
#85298=DIRECTION('center_axis',(0.114465482555487,0.986495109200375,-0.117153970598861));
#85299=DIRECTION('ref_axis',(0.778540752379732,-0.0158280504998284,0.62739442912842));
#85300=DIRECTION('center_axis',(-0.129621752543377,0.986495109404068,0.100127920129402));
#85301=DIRECTION('ref_axis',(0.705572987566036,0.0208149521856119,0.70833148806378));
#85302=DIRECTION('center_axis',(0.13697398323435,0.986495109207171,-0.0898082815070361));
#85303=DIRECTION('ref_axis',(0.6254676446499,-0.015828049283185,0.780089545085688));
#85304=DIRECTION('center_axis',(-0.148115809468914,0.986495109426496,0.0699221428660026));
#85305=DIRECTION('ref_axis',(0.536806752086055,0.0208149488146366,0.843448426888488));
#85306=DIRECTION('center_axis',(0.153077736248759,0.986495109159638,-0.0582632497297413));
#85307=DIRECTION('ref_axis',(0.443148364745263,-0.015828056351047,0.896308540322889));
#85308=DIRECTION('center_axis',(-0.159684136636216,0.986495109476762,0.0364468858090491));
#85309=DIRECTION('ref_axis',(0.342940027684309,0.0208149437938576,0.939126655742847));
#85310=DIRECTION('center_axis',(0.16202373838693,0.986495109239524,-0.0239939085107565));
#85311=DIRECTION('ref_axis',(0.240107962164591,-0.0158280467462338,0.970617143595437));
#85312=DIRECTION('center_axis',(-0.163785813527936,0.986495109450472,0.00126740573369946));
#85313=DIRECTION('ref_axis',(0.133037809399803,0.0208149467552055,0.990892365124326));
#85314=DIRECTION('center_axis',(0.163393698449405,0.986495108418207,0.0113973845234563));
#85315=DIRECTION('ref_axis',(0.0258403863850521,-0.0158280630558587,0.999540767978661));
#85316=DIRECTION('center_axis',(-0.155457916630874,0.987363722298953,0.0307524965611573));
#85317=DIRECTION('ref_axis',(0.138178875923994,-0.00909007846864055,0.990365573271716));
#85318=DIRECTION('',(-0.727623861284462,0.,-0.68597632356335));
#85319=DIRECTION('center_axis',(-1.12148479625166E-14,-1.,-8.08785086650414E-14));
#85320=DIRECTION('ref_axis',(1.2877591139289E-31,8.08785086650414E-14,-1.));
#85321=DIRECTION('center_axis',(-0.153257680235064,-0.987363721873262,0.0403108444161852));
#85322=DIRECTION('ref_axis',(0.0669565413129348,0.0303233739208332,0.997294998768903));
#85323=DIRECTION('center_axis',(0.149059810413061,-0.987363723002569,-0.0537963885231106));
#85324=DIRECTION('ref_axis',(0.14224023693335,-0.0324282815239169,0.989300824600157));
#85325=DIRECTION('',(-0.513520954857275,0.,0.858077053021739));
#85326=DIRECTION('center_axis',(-0.145212520775725,0.987363722362003,0.0634523724805455));
#85327=DIRECTION('ref_axis',(0.347847652333208,-0.00909007383497536,0.937507003346615));
#85328=DIRECTION('',(-0.858077052117147,0.,-0.513520956368819));
#85329=DIRECTION('center_axis',(0.,-1.,0.));
#85330=DIRECTION('ref_axis',(0.,0.,-1.));
#85331=DIRECTION('center_axis',(-0.141008960123313,-0.987363721799518,0.0723142727208516));
#85332=DIRECTION('ref_axis',(0.279780078968391,0.0303233766047821,0.959585118811107));
#85333=DIRECTION('center_axis',(0.134010239664075,-0.98736372285364,-0.0845821166546276));
#85334=DIRECTION('ref_axis',(0.351585171224556,-0.0324282869747367,0.935594075215787));
#85335=DIRECTION('',(-0.317053919406352,0.,0.948407513777211));
#85336=DIRECTION('center_axis',(-0.128177146769656,0.987363722305179,0.0931852934837393));
#85337=DIRECTION('ref_axis',(0.541251461767044,-0.00909007676524374,0.84081164694564));
#85338=DIRECTION('',(-0.948407514082987,0.,-0.317053918491681));
#85339=DIRECTION('center_axis',(6.01886246066096E-14,-1.,9.36741191559153E-14));
#85340=DIRECTION('ref_axis',(-5.70917302974635E-32,-9.36741191559153E-14,
-1.));
#85341=DIRECTION('center_axis',(-0.122166815496601,-0.987363721684859,0.100936367539379));
#85342=DIRECTION('ref_axis',(0.479521412833519,0.0303233812058827,0.877006104417973));
#85343=DIRECTION('center_axis',(0.112694502133529,-0.987363722956722,-0.111412870791117));
#85344=DIRECTION('ref_axis',(0.5444903757614,-0.032428282988734,0.838139986616563));
#85345=DIRECTION('',(-0.105761793778192,0.,0.994391493817611));
#85346=DIRECTION('center_axis',(-0.105148352898413,0.987363722309484,0.118560970601255));
#85347=DIRECTION('ref_axis',(0.709346952146409,-0.00909007678427596,0.704800873995383));
#85348=DIRECTION('',(-0.99439149393359,0.,-0.105761792687731));
#85349=DIRECTION('center_axis',(2.63062048809266E-14,-1.,2.61817650590162E-14));
#85350=DIRECTION('ref_axis',(1.,2.63062048809266E-14,9.86486506770613E-32));
#85351=DIRECTION('center_axis',(-0.0976122912519061,-0.987363721798348,
0.1248387819272));
#85352=DIRECTION('ref_axis',(0.656840855817275,0.0303233765312807,0.753419261079096));
#85353=DIRECTION('center_axis',(0.0861092934143021,-0.987363722975803,-0.133034086380336));
#85354=DIRECTION('ref_axis',(0.711935815224303,-0.0324282828974503,0.70149540374063));
#85355=DIRECTION('',(0.110475636308035,0.,0.993878832545665));
#85356=DIRECTION('center_axis',(-0.0772029402071325,0.987363722355735,0.138392867587899));
#85357=DIRECTION('ref_axis',(0.844274169030345,-0.00909007489063781,0.53583439423632));
#85358=DIRECTION('',(-0.993878832740016,0.,0.110475634559585));
#85359=DIRECTION('center_axis',(-7.51667662639805E-14,-1.,-4.77950243231242E-14));
#85360=DIRECTION('ref_axis',(1.,-7.51667662639805E-14,2.19109677680993E-31));
#85361=DIRECTION('center_axis',(-0.0684935240125511,-0.987363721860461,
0.142903876512153));
#85362=DIRECTION('ref_axis',(0.803447151474661,0.0303233744073822,0.594603370114737));
#85363=DIRECTION('center_axis',(0.0554977124764765,-0.987363723067244,-0.14843477449934));
#85364=DIRECTION('ref_axis',(0.846091927685473,-0.0324282797104404,0.532049674918143));
#85365=DIRECTION('',(0.321547346824495,0.,0.946893501799504));
#85366=DIRECTION('center_axis',(-0.0456476012935844,0.987363722316211,0.151753669972159));
#85367=DIRECTION('ref_axis',(0.939724063897283,-0.00909007638497098,0.341812893618263));
#85368=DIRECTION('',(-0.946893502365445,0.,0.32154734515791));
#85369=DIRECTION('center_axis',(-2.09209816216792E-14,-1.,-7.62974259781717E-15));
#85370=DIRECTION('ref_axis',(1.,-2.09209816216792E-14,8.65847740393996E-32));
#85371=DIRECTION('center_axis',(-0.0361720699851638,-0.98736372173205,0.15428694812078));
#85372=DIRECTION('ref_axis',(0.912485152557324,0.0303233787472675,0.407984483851759));
#85373=DIRECTION('center_axis',(0.0222911163563204,-0.987363723032363,-0.156894820090594));
#85374=DIRECTION('ref_axis',(0.940685720889932,-0.0324282816366707,0.337725896347736));
#85375=DIRECTION('',(0.517583861605946,0.,0.855632483140441));
#85376=DIRECTION('center_axis',(-0.011957828115349,0.987363722256829,0.158018639147103));
#85377=DIRECTION('ref_axis',(0.991233505649836,-0.00909008090717694,0.1318086025502));
#85378=DIRECTION('',(-0.85563248405198,0.,0.517583860099056));
#85379=DIRECTION('center_axis',(-7.35734327801556E-15,-1.,-9.84656943244725E-16));
#85380=DIRECTION('ref_axis',(1.,-7.35734327801556E-15,-1.3470661391192E-32));
#85381=DIRECTION('center_axis',(-0.00215925495983984,-0.987363721794488,
0.158455730417539));
#85382=DIRECTION('ref_axis',(0.978856360877033,0.0303233776589315,0.202288698492838));
#85383=DIRECTION('center_axis',(-0.0119577902699399,-0.987363722876836,
-0.158018638136943));
#85384=DIRECTION('ref_axis',(0.9912940961874,-0.0324282856353993,0.127610427296341));
#85385=DIRECTION('',(0.689418728599909,0.,0.724363042027743));
#85386=DIRECTION('center_axis',(0.022291069413263,0.987363722349427,0.156894831057929));
#85387=DIRECTION('ref_axis',(0.996393970420733,-0.00909007440818482,-0.0843589133195836));
#85388=DIRECTION('',(-0.724363041876131,0.,0.689418728759206));
#85389=DIRECTION('center_axis',(-6.65730432814955E-14,-1.,5.57977600812412E-15));
#85390=DIRECTION('ref_axis',(1.,-6.65730432814955E-14,-6.37552911105267E-32));
#85391=DIRECTION('center_axis',(0.0319545255018942,-0.987363721775575,0.155215299572671));
#85392=DIRECTION('ref_axis',(0.999457333683558,0.0303233778893256,-0.0128658812187456));
#85393=DIRECTION('center_axis',(-0.0456475581498333,-0.987363722973715,
-0.151753678671865));
#85394=DIRECTION('ref_axis',(0.99555066093659,-0.0324282838992063,-0.0884719611632503));
#85395=DIRECTION('',(0.829017145402445,0.,0.559223186776784));
#85396=DIRECTION('center_axis',(0.0554976664419892,0.987363722365212,0.148434796380787));
#85397=DIRECTION('ref_axis',(0.954964160800323,-0.00909007353095526,-0.296581897880058));
#85398=DIRECTION('',(-0.559223188237572,0.,0.829017144417053));
#85399=DIRECTION('center_axis',(-1.13452649964229E-13,-1.,3.51298850837732E-14));
#85400=DIRECTION('ref_axis',(1.,-1.13452649964229E-13,6.09375410996373E-32));
#85401=DIRECTION('center_axis',(0.0645741449693705,-0.987363721836154,0.144717174527881));
#85402=DIRECTION('ref_axis',(0.973324792786892,0.0303233751357475,-0.227418866118733));
#85403=DIRECTION('center_axis',(-0.0772028993465973,-0.987363722956117,
-0.138392886098657));
#85404=DIRECTION('ref_axis',(0.953256383221609,-0.0324282845561554,-0.300417499836481));
#85405=DIRECTION('',(0.929851640370812,0.,0.367934677490054));
#85406=DIRECTION('center_axis',(0.0861092603282511,0.987363722268804,0.133034113043285));
#85407=DIRECTION('ref_axis',(0.868881288000507,-0.00909007908539792,-0.494937044304426));
#85408=DIRECTION('',(-0.367934678144954,0.,0.929851640111673));
#85409=DIRECTION('center_axis',(-4.51711327338588E-14,-1.,2.56801711754637E-14));
#85410=DIRECTION('ref_axis',(1.,-4.51711327338588E-14,2.69596667039635E-31));
#85411=DIRECTION('center_axis',(0.0941743527967696,-0.987363721783213,0.127452234902771));
#85412=DIRECTION('ref_axis',(0.901680666214819,0.0303233758618026,-0.431337998616797));
#85413=DIRECTION('center_axis',(-0.105148313696102,-0.987363723085985,-0.118560998902036));
#85414=DIRECTION('ref_axis',(0.866388897096936,-0.0324282793889344,-0.498315849319514));
#85415=DIRECTION('',(0.987207304850248,0.,0.159441955740358));
#85416=DIRECTION('center_axis',(0.112694470843253,0.987363722358728,0.111412907740871));
#85417=DIRECTION('ref_axis',(0.742170492605667,-0.00909007302830182,-0.670149483680919));
#85418=DIRECTION('',(-0.159441954225668,0.,0.987207305094882));
#85419=DIRECTION('center_axis',(2.20540451644059E-14,-1.,-1.98801378983789E-14));
#85420=DIRECTION('ref_axis',(1.,2.20540451644059E-14,-1.16398971375676E-31));
#85421=DIRECTION('center_axis',(0.119371070808828,-0.987363721830502,0.104227771092797));
#85422=DIRECTION('ref_axis',(0.787874952879634,0.0303233743726265,-0.615088246995154));
#85423=DIRECTION('center_axis',(-0.128177111842097,-0.987363723177813,-0.0931853322807025));
#85424=DIRECTION('ref_axis',(0.73901002942784,-0.0324282754283277,-0.672913503622723));
#85425=DIRECTION('',(0.998402253875163,0.,-0.0565061010599261));
#85426=DIRECTION('center_axis',(0.134010221267995,0.98736372231437,0.0845821520961454));
#85427=DIRECTION('ref_axis',(0.580756628251935,-0.00909007750398461,-0.814026479441802));
#85428=DIRECTION('',(0.0565060964350291,0.,0.998402254136916));
#85429=DIRECTION('center_axis',(-3.88457816059066E-14,-1.,5.43517179396169E-14));
#85430=DIRECTION('ref_axis',(1.14632904336126E-31,-5.43517179396169E-14,
-1.));
#85431=DIRECTION('center_axis',(0.138986130481117,-0.987363721883336,0.0761297329732144));
#85432=DIRECTION('ref_axis',(0.637229084006982,0.0303233733069723,-0.770077650322946));
#85433=DIRECTION('center_axis',(-0.145212496255406,-0.987363723096613,-0.0634524171649051));
#85434=DIRECTION('ref_axis',(0.577075873870543,-0.0324282798070519,-0.816046470775595));
#85435=DIRECTION('',(0.962913022721775,0.,-0.26981199134363));
#85436=DIRECTION('center_axis',(0.149059797608916,0.98736372234626,0.0537964360466986));
#85437=DIRECTION('ref_axis',(0.392187231442824,-0.00909007338534998,-0.919840500336369));
#85438=DIRECTION('',(0.26981198698136,0.,0.9629130239441));
#85439=DIRECTION('center_axis',(1.45853200714515E-14,-1.,-3.41287221346288E-14));
#85440=DIRECTION('ref_axis',(-1.8222568904173E-31,3.41287221346288E-14,
-1.));
#85441=DIRECTION('center_axis',(0.152102354641146,-0.987363721845998,0.0444719517790476));
#85442=DIRECTION('ref_axis',(0.456787090216585,0.0303233740596595,-0.889059079700052));
#85443=DIRECTION('center_axis',(-0.15545790539908,-0.987363722888087,-0.0307525344241499));
#85444=DIRECTION('ref_axis',(0.388158288051228,-0.032428286051492,-0.921022013678773));
#85445=DIRECTION('',(0.88239904984541,0.,-0.470501771337704));
#85446=DIRECTION('center_axis',(0.157139506714322,0.987363722300695,0.0204952510132345));
#85447=DIRECTION('ref_axis',(0.185279594329072,-0.00909007741256787,-0.98264380241158));
#85448=DIRECTION('',(0.470501770976394,0.,0.882399050038064));
#85449=DIRECTION('center_axis',(-2.21045022981612E-14,-1.,1.1669191756339E-13));
#85450=DIRECTION('ref_axis',(-6.30364264290393E-32,-1.1669191756339E-13,
-1.));
#85451=DIRECTION('center_axis',(0.158106441959231,-0.987363721757333,0.0107347085894193));
#85452=DIRECTION('ref_axis',(0.254986240945197,0.0303233778593733,-0.96646909401379));
#85453=DIRECTION('center_axis',(-0.158434270677612,-0.987363723095218,0.00338529029809263));
#85454=DIRECTION('ref_axis',(0.18109085788381,-0.0324282794849182,-0.982931588606528));
#85455=DIRECTION('',(0.760625076895703,0.,-0.64919141429736));
#85456=DIRECTION('',(0.649191412957105,0.,0.760625078039607));
#85457=DIRECTION('',(0.603285121269556,0.,-0.797525587335464));
#85458=DIRECTION('center_axis',(0.151221686215521,0.987363722343238,-0.047380179596961));
#85459=DIRECTION('ref_axis',(-0.244446218187792,-0.00909007671548458,-0.969620243661916));
#85460=DIRECTION('',(0.797525585226132,0.,0.603285124058033));
#85461=DIRECTION('center_axis',(-1.80851008879526E-15,-1.,-7.19925971614798E-15));
#85462=DIRECTION('ref_axis',(2.8446207780274E-34,7.19925971614798E-15,-1.));
#85463=DIRECTION('center_axis',(0.148000906469275,-0.987363721718874,-0.0566446177295607));
#85464=DIRECTION('ref_axis',(-0.174390597605054,0.0303233811261436,-0.984209536645541));
#85465=DIRECTION('center_axis',(-0.142369603550533,-0.987363723128967,0.0695972286356919));
#85466=DIRECTION('ref_axis',(-0.24836864875715,-0.0324282784717592,-0.968122627082905));
#85467=DIRECTION('',(0.41773622273295,0.,-0.908568350877801));
#85468=DIRECTION('center_axis',(0.137500868255779,0.987363722269032,-0.0787806522945108));
#85469=DIRECTION('ref_axis',(-0.447170891372606,-0.00909007952360674,-0.894402350378891));
#85470=DIRECTION('',(0.908568350643389,0.,0.417736223242793));
#85471=DIRECTION('center_axis',(4.63939863213034E-14,-1.,9.29903636253066E-14));
#85472=DIRECTION('ref_axis',(4.26143284160394E-31,-9.29903636253066E-14,
-1.));
#85473=DIRECTION('center_axis',(0.132363810189427,-0.987363721735688,-0.0871361162342473));
#85474=DIRECTION('ref_axis',(-0.381889396612541,0.0303233795313162,-0.923710442405362));
#85475=DIRECTION('center_axis',(-0.124079731074172,-0.987363722900472,0.0985753470025941));
#85476=DIRECTION('ref_axis',(-0.450679678382106,-0.0324282853365217,-0.892096538387822));
#85477=DIRECTION('',(0.212654444280544,0.,-0.977127467287525));
#85478=DIRECTION('center_axis',(0.11735066527046,0.987363722331918,-0.10649742336526));
#85479=DIRECTION('ref_axis',(-0.628986351769033,-0.0090900753738975,-0.777363196850725));
#85480=DIRECTION('',(0.977127466912818,0.,0.212654446002285));
#85481=DIRECTION('center_axis',(5.59710000100304E-14,-1.,6.92939698404936E-14));
#85482=DIRECTION('ref_axis',(-4.60810629483416E-31,-6.92939698404935E-14,
-1.));
#85483=DIRECTION('center_axis',(0.110537530305549,-0.987363721828821,-0.11355322633148));
#85484=DIRECTION('ref_axis',(-0.571531475732816,0.0303233763923442,-0.82001967359987));
#85485=DIRECTION('center_axis',(-0.0999880321937499,-0.98736372299158,0.122944182205695));
#85486=DIRECTION('ref_axis',(-0.631917422190177,-0.0324282824640613,-0.774357009414232));
#85487=DIRECTION('',(-0.00237082103812565,0.,-0.999997189599853));
#85488=DIRECTION('center_axis',(0.0917132760761384,0.987363722355005,-0.129234495273713));
#85489=DIRECTION('ref_axis',(-0.781391109084285,-0.00909007261383878,-0.623975404342116));
#85490=DIRECTION('',(0.999997189610847,0.,-0.00237081640126621));
#85491=DIRECTION('center_axis',(1.15930973899852E-14,-1.,9.27363413703666E-15));
#85492=DIRECTION('ref_axis',(1.,1.15930973899852E-14,5.91510523815103E-33));
#85493=DIRECTION('center_axis',(0.0835426346946244,-0.987363721744513,-0.134660718738259));
#85494=DIRECTION('ref_axis',(-0.734449379788685,0.0303233792619161,-0.677985693948002));
#85495=DIRECTION('center_axis',(-0.0712210092508804,-0.987363723228234,
0.141564281844558));
#85496=DIRECTION('ref_axis',(-0.783607409986975,-0.0324282744047808,-0.620409408401124));
#85497=DIRECTION('',(-0.21728522775494,0.,-0.976108154765385));
#85498=DIRECTION('center_axis',(0.0617874731962761,0.987363722349567,-0.145928708429927));
#85499=DIRECTION('ref_axis',(-0.89725888607618,-0.00909007401268137,-0.441411216341154));
#85500=DIRECTION('',(0.976108155148254,-9.35065609140375E-15,-0.217285226034981));
#85501=DIRECTION('center_axis',(-7.98936867010663E-14,-1.,-3.93878909193784E-14));
#85502=DIRECTION('ref_axis',(1.,-7.98936867010663E-14,-3.8090581129996E-31));
#85503=DIRECTION('center_axis',(0.0526413862943957,-0.987363721871389,-0.149471619986147));
#85504=DIRECTION('ref_axis',(-0.863025242613456,0.0303233731980806,-0.504249862320135));
#85505=DIRECTION('center_axis',(-0.0391237546118326,-0.98736372289731,0.153565004253697));
#85506=DIRECTION('ref_axis',(-0.898656789348412,-0.0324282859703908,-0.437452147356745));
#85507=DIRECTION('',(-0.422039619688627,0.,-0.906577387437542));
#85508=DIRECTION('center_axis',(0.0289725558770176,0.987363722280623,-0.155799457412744));
#85509=DIRECTION('ref_axis',(-0.97117183573339,-0.00909007579519604,-0.238207128357393));
#85510=DIRECTION('',(0.906577388181206,-9.35065607453509E-15,-0.422039618091173));
#85511=DIRECTION('',(-0.607059907517467,0.,-0.794656069431855));
#85512=DIRECTION('center_axis',(-3.60387703961403E-14,-1.,-8.87176788160941E-15));
#85513=DIRECTION('ref_axis',(1.,-3.60387703961403E-14,-1.27276260034576E-31));
#85514=DIRECTION('center_axis',(0.0192786812813638,-0.987363721912874,-0.157293398139934));
#85515=DIRECTION('ref_axis',(-0.951247007159819,0.03032337171749,-0.306935863817135));
#85516=DIRECTION('center_axis',(-0.00519712986202774,-0.987363722957762,
0.158385190053192));
#85517=DIRECTION('ref_axis',(-0.97168597329991,-0.0324282827858379,-0.234040115723286));
#85518=DIRECTION('',(0.794656070501523,0.,-0.607059906117246));
#85519=DIRECTION('center_axis',(-0.00519708766551451,0.987363722313707,
-0.15838519545279));
#85520=DIRECTION('ref_axis',(-0.999673869137803,-0.0090900790429132,-0.0238647402258607));
#85521=DIRECTION('center_axis',(4.45240460760042E-14,-1.,1.10049664697024E-15));
#85522=DIRECTION('ref_axis',(-0.999694677173031,-4.45376444353329E-14,-0.0247093591966371));
#85523=DIRECTION('center_axis',(-0.0149854786284753,-0.987363721847574,
-0.157760312530061));
#85524=DIRECTION('ref_axis',(-0.994989518555826,0.0303233755014844,-0.095269884340445));
#85525=DIRECTION('center_axis',(0.0289725116530487,-0.987363722953917,0.155799461369719));
#85526=DIRECTION('ref_axis',(-0.999280201885406,-0.0324282842135005,-0.0196846260526198));
#85527=DIRECTION('',(-0.763694749702693,0.,-0.645577516086597));
#85528=DIRECTION('center_axis',(-0.0391237164597122,0.987363722286895,-0.153565017898441));
#85529=DIRECTION('ref_axis',(-0.981432263325734,-0.0090900775719372,0.191593535885382));
#85530=DIRECTION('',(0.645577518758643,0.,-0.763694747443921));
#85531=DIRECTION('center_axis',(7.28661215438116E-15,-1.,-1.41609769132671E-15));
#85532=DIRECTION('ref_axis',(1.,7.28661215438116E-15,1.09542984455334E-33));
#85533=DIRECTION('center_axis',(-0.048548929510468,-0.987363721854955,-0.150850529359757));
#85534=DIRECTION('ref_axis',(-0.992207425625152,0.0303233748037648,0.120850806678399));
#85535=DIRECTION('center_axis',(0.0617874283044647,-0.987363722959389,0.1459287233114));
#85536=DIRECTION('ref_axis',(-0.980149198894436,-0.0324282832786011,0.195591294157482));
#85537=DIRECTION('',(-0.884620074177392,0.,-0.466312475023332));
#85538=DIRECTION('center_axis',(-0.0712209641420276,0.987363722345124,-0.141564310698214));
#85539=DIRECTION('ref_axis',(-0.917299976199164,-0.0090900767457838,0.398093109925014));
#85540=DIRECTION('',(0.466312478831761,0.,-0.884620072169843));
#85541=DIRECTION('center_axis',(4.08710163910781E-14,-1.,-1.76963780131983E-14));
#85542=DIRECTION('ref_axis',(1.,4.08710163910781E-14,-1.88174897648644E-31));
#85543=DIRECTION('center_axis',(-0.0798422872074384,-0.987363721854571,
-0.136887143074045));
#85544=DIRECTION('ref_axis',(-0.943030816223802,0.0303233747598678,0.331320649213783));
#85545=DIRECTION('center_axis',(0.0917132337652694,-0.987363722983189,0.129234520500883));
#85546=DIRECTION('ref_axis',(-0.915187508710007,-0.0324282825088845,0.40172158318255));
#85547=DIRECTION('',(-0.964181545972515,0.,-0.265243183524199));
#85548=DIRECTION('center_axis',(-0.0999879970270678,0.987363722361799,-0.122944215863811));
#85549=DIRECTION('ref_axis',(-0.810275761337678,-0.00909007322328466,0.585978294100934));
#85550=DIRECTION('',(0.265243185223135,0.,-0.964181545505143));
#85551=DIRECTION('center_axis',(-6.01854610169138E-15,-1.,4.34478449126022E-15));
#85552=DIRECTION('ref_axis',(1.,-6.01854610169138E-15,2.10202917262272E-32));
#85553=DIRECTION('center_axis',(-0.107402309026535,-0.987363721829395,-0.116523065660722));
#85554=DIRECTION('ref_axis',(-0.849759133394177,0.0303233754483682,0.526298307155356));
#85555=DIRECTION('center_axis',(0.117350631392854,-0.987363722976456,0.106497454719681));
#85556=DIRECTION('ref_axis',(-0.807432667974151,-0.0324282829819871,0.589067817106812));
#85557=DIRECTION('',(-0.998658961195706,0.,-0.0517714131882922));
#85558=DIRECTION('center_axis',(-0.124079706118009,0.9873637223582,-0.0985753838472311));
#85559=DIRECTION('ref_axis',(-0.665363952244306,-0.00909007427090294,0.746463784522455));
#85560=DIRECTION('',(0.0517714178151324,0.,-0.998658960955846));
#85561=DIRECTION('center_axis',(-4.94383559695101E-14,-1.,5.5370153410865E-14));
#85562=DIRECTION('ref_axis',(-1.76122624385495E-31,-5.5370153410865E-14,
-1.));
#85563=DIRECTION('center_axis',(-0.129940320557335,-0.987363721732702,-0.0907104960828901));
#85564=DIRECTION('ref_axis',(-0.71675365861586,0.0303233802018828,0.6966668396543));
#85565=DIRECTION('center_axis',(0.137500844342104,-0.987363722957578,0.0787806854029617));
#85566=DIRECTION('ref_axis',(-0.661923171710724,-0.0324282840967445,0.748869896005278));
#85567=DIRECTION('',(-0.986440193500669,0.,0.164121127970665));
#85568=DIRECTION('center_axis',(-0.142369586162368,0.987363722340887,-0.069597275385635));
#85569=DIRECTION('ref_axis',(-0.489340464185005,-0.00909007622411355,0.872045457889348));
#85570=DIRECTION('',(-0.164121129030201,0.,-0.986440193324386));
#85571=DIRECTION('center_axis',(-3.27416115837152E-14,-1.,5.82330736311059E-14));
#85572=DIRECTION('ref_axis',(-1.3715310984991E-31,-5.82330736311059E-14,
-1.));
#85573=DIRECTION('center_axis',(-0.146402462725365,-0.987363721749518,-0.0606564084074233));
#85574=DIRECTION('ref_axis',(-0.550233578611314,0.0303233787080033,0.834460006035231));
#85575=DIRECTION('center_axis',(0.151221665785124,-0.987363723189041,0.0473802271780921));
#85576=DIRECTION('ref_axis',(-0.4854628862946,-0.032428275889997,0.873655648956337));
#85577=DIRECTION('',(-0.928096578352929,0.,0.372339551014374));
#85578=DIRECTION('center_axis',(-0.154002421996287,0.987363722277982,-0.0373648758681921));
#85579=DIRECTION('ref_axis',(-0.290435959825997,-0.009090077635243,0.956851254756212));
#85580=DIRECTION('',(-0.372339549380154,0.,-0.928096579008556));
#85581=DIRECTION('center_axis',(1.94577414584816E-14,-1.,-6.39100954909678E-14));
#85582=DIRECTION('ref_axis',(-2.8111492504619E-31,6.39100954909678E-14,
-1.));
#85583=DIRECTION('center_axis',(-0.156018988142432,-0.987363721822666,-0.0277660974482387));
#85584=DIRECTION('ref_axis',(-0.357985189673304,0.0303233746749526,0.933234749097402));
#85585=DIRECTION('center_axis',(0.157871536511976,-0.987363723086416,0.0137643122704986));
#85586=DIRECTION('ref_axis',(-0.286302893437925,-0.0324282793787185,0.957590235907618));
#85587=DIRECTION('',(-0.826356198741165,0.,0.563147789485187));
#85588=DIRECTION('center_axis',(-0.158434274704725,0.987363722287983,-0.00338533726621558));
#85589=DIRECTION('ref_axis',(-0.0779509939136845,-0.00909007789139745,0.996915750217538));
#85590=DIRECTION('',(-0.563147788031161,0.,-0.826356199732059));
#85591=DIRECTION('center_axis',(-6.4338375555057E-15,-1.,8.13984748522599E-14));
#85592=DIRECTION('ref_axis',(-7.09766227055145E-32,-8.13984748522599E-14,
-1.));
#85593=DIRECTION('center_axis',(-0.158340241063287,-0.987363721828894,0.00642252880218966));
#85594=DIRECTION('ref_axis',(-0.148997811258801,0.0303233746239653,0.98837247290255));
#85595=DIRECTION('center_axis',(0.157139508177838,-0.987363722970566,-0.0204952075210409));
#85596=DIRECTION('ref_axis',(-0.0737556956995861,-0.0324282834517269,0.996748967285266));
#85597=DIRECTION('',(-0.68597632228297,0.,0.727623862491556));
#85598=DIRECTION('',(0.761200566737339,0.,-0.648516535794388));
#85599=DIRECTION('center_axis',(0.153863152436169,-0.987363722371363,0.03793428617189));
#85600=DIRECTION('ref_axis',(-0.188441790513884,0.00836476944115453,0.982048737191855));
#85601=DIRECTION('center_axis',(-0.153405752207115,-0.987363721985033,-0.0397436246161791));
#85602=DIRECTION('ref_axis',(-0.260336356464506,0.00158397740775573,0.965516686815074));
#85603=DIRECTION('',(0.469718957703108,0.,0.882816006183795));
#85604=DIRECTION('center_axis',(-5.55199781974668E-15,-1.,2.91680662988477E-14));
#85605=DIRECTION('ref_axis',(-1.37200428465795E-31,-2.91680662988477E-14,
-1.));
#85606=DIRECTION('center_axis',(0.157639630788376,0.987363722515582,0.0162057479024672));
#85607=DIRECTION('ref_axis',(-0.112073886978174,0.00158366860756381,0.993698614194135));
#85608=DIRECTION('center_axis',(-0.14640245848675,0.987363723292207,-0.0606563935260433));
#85609=DIRECTION('ref_axis',(-0.191341517099414,0.0318943943832642,0.981005184207005));
#85610=DIRECTION('',(0.882816006173184,0.,-0.469718957723051));
#85611=DIRECTION('center_axis',(0.142111167445554,-0.987363722349851,0.0701234331354898));
#85612=DIRECTION('ref_axis',(-0.395147576306963,0.00836476911063044,0.918579568451454));
#85613=DIRECTION('center_axis',(-0.141275512893773,-0.987363722159082,-0.0717921278467529));
#85614=DIRECTION('ref_axis',(-0.461807381783311,0.00158399341620002,0.886978823363501));
#85615=DIRECTION('',(0.268957842517584,0.,0.963151950082793));
#85616=DIRECTION('center_axis',(-2.33849344727135E-14,-1.,5.45852353395005E-14));
#85617=DIRECTION('ref_axis',(1.70718886853183E-32,-5.45852353395005E-14,
-1.));
#85618=DIRECTION('center_axis',(0.150470348483635,0.987363722496377,0.0497147234258606));
#85619=DIRECTION('ref_axis',(-0.323069488553992,0.00158367253386998,0.9463739205762));
#85620=DIRECTION('center_axis',(-0.129940323503184,0.987363723619674,-0.0907104713237707));
#85621=DIRECTION('ref_axis',(-0.397755173973421,0.0318943830411897,0.916937058858347));
#85622=DIRECTION('',(0.963151949602078,0.,-0.268957844239047));
#85623=DIRECTION('center_axis',(0.123714217828372,-0.987363722263984,0.0990336925703855));
#85624=DIRECTION('ref_axis',(-0.583376700032673,0.00836477655867606,0.81215863990486));
#85625=DIRECTION('center_axis',(-0.122539376667729,-0.987363722039492,-0.100483737819634));
#85626=DIRECTION('ref_axis',(-0.641684811093609,0.00158398009810487,0.76696681428782));
#85627=DIRECTION('',(0.0556205582211182,0.,0.998451978566406));
#85628=DIRECTION('center_axis',(1.72862098727691E-14,-1.,-2.41409965901546E-14));
#85629=DIRECTION('ref_axis',(5.0966387703121E-31,2.41409965901546E-14,-1.));
#85630=DIRECTION('center_axis',(0.136265238390394,0.987363722512308,0.0808990993339642));
#85631=DIRECTION('ref_axis',(-0.518958723024964,0.00158367098874867,0.854797833281354));
#85632=DIRECTION('center_axis',(-0.107402317333303,0.98736372348291,-0.116523043993025));
#85633=DIRECTION('ref_axis',(-0.585570242472141,0.0318943888650221,0.809993974724532));
#85634=DIRECTION('',(0.99845197842399,0.,-0.0556205607776467));
#85635=DIRECTION('center_axis',(0.099532535089522,-0.987363722350104,0.123313236295216));
#85636=DIRECTION('ref_axis',(-0.744327775711308,0.00836477204862553,0.667762078058668));
#85637=DIRECTION('center_axis',(-0.0980734501969365,-0.987363722134044,
-0.124476819448742));
#85638=DIRECTION('ref_axis',(-0.791557770193034,0.00158399262243925,0.61109229042298));
#85639=DIRECTION('',(-0.160317479600256,0.,0.987065502251305));
#85640=DIRECTION('center_axis',(6.62150057297851E-14,-1.,-5.95817081362791E-14));
#85641=DIRECTION('ref_axis',(1.,6.62150057297851E-14,-3.0643499606565E-30));
#85642=DIRECTION('center_axis',(0.115688518570161,0.987363722502101,0.108300720947907));
#85643=DIRECTION('ref_axis',(-0.690582021097443,0.00158367157795096,0.723252351618233));
#85644=DIRECTION('center_axis',(-0.0798423016070618,0.987363723489339,-0.136887122883619));
#85645=DIRECTION('ref_axis',(-0.746004697532087,0.0318943877439224,0.665176472291751));
#85646=DIRECTION('',(0.987065502661801,0.,0.160317477072854));
#85647=DIRECTION('center_axis',(0.0706968123188893,-0.987363722207916,0.141826798580794));
#85648=DIRECTION('ref_axis',(-0.870474915562179,0.00836477955372812,0.492141698944556));
#85649=DIRECTION('center_axis',(-0.0690217115090215,-0.987363722152823,
-0.142649512851912));
#85650=DIRECTION('ref_axis',(-0.90441836785597,0.00158399343718549,0.42664377043329));
#85651=DIRECTION('',(-0.368759251362437,0.,0.929524940243464));
#85652=DIRECTION('center_axis',(2.58250805724881E-14,-1.,-1.46514839927069E-14));
#85653=DIRECTION('ref_axis',(1.,2.58250805724881E-14,5.20492449486746E-31));
#85654=DIRECTION('center_axis',(0.089702331649604,0.987363722499697,0.130638322050482));
#85655=DIRECTION('ref_axis',(-0.829914475268389,0.00158367205682094,0.557888390023319));
#85656=DIRECTION('center_axis',(-0.048548946371977,0.987363723458484,-0.150850513437537));
#85657=DIRECTION('ref_axis',(-0.871556800476462,0.0318943896923164,0.489256059185154));
#85658=DIRECTION('',(0.929524940202268,0.,0.368759251466278));
#85659=DIRECTION('center_axis',(0.0385553978110738,-0.987363722333291,0.15370868914859));
#85660=DIRECTION('ref_axis',(-0.95591961231219,0.00836477265671015,0.293509327578042));
#85661=DIRECTION('center_axis',(-0.0367425853322626,-0.987363722085997,
-0.154152076637289));
#85662=DIRECTION('ref_axis',(-0.97498936820771,0.00158398468336746,0.222245861321313));
#85663=DIRECTION('',(-0.559958251059163,0.,0.828520824765898));
#85664=DIRECTION('center_axis',(2.83709405267253E-14,-1.,-8.75731150790992E-15));
#85665=DIRECTION('ref_axis',(1.,2.83709405267253E-14,3.25104264459992E-31));
#85666=DIRECTION('center_axis',(0.0595217627816455,0.987363722497361,0.146867420660677));
#85667=DIRECTION('ref_axis',(-0.930441048090257,0.0015836710718016,0.36643819126101));
#85668=DIRECTION('center_axis',(-0.0149854919230227,0.987363723258614,-0.157760302436043));
#85669=DIRECTION('ref_axis',(-0.95635587745199,0.0318943956067335,0.290458573968674));
#85670=DIRECTION('',(0.828520826199677,0.,0.559958248937727));
#85671=DIRECTION('center_axis',(0.00461116712645498,-0.987363722278625,
0.158403336662551));
#85672=DIRECTION('ref_axis',(-0.996666572634082,0.00836477445303214,0.0811527790170065));
#85673=DIRECTION('center_axis',(-0.00274543282601405,-0.987363722148695,
-0.158446655954841));
#85674=DIRECTION('ref_axis',(-0.999970949214054,0.00158399315517319,0.00745598374647318));
#85675=DIRECTION('',(-0.72497422441143,0.,0.688775996924287));
#85676=DIRECTION('center_axis',(0.,-1.,0.));
#85677=DIRECTION('ref_axis',(0.,0.,-1.));
#85678=DIRECTION('center_axis',(0.0265580251225395,0.98736372248948,0.156229161212971));
#85679=DIRECTION('ref_axis',(-0.987461233018084,0.00158367357248836,0.157853746437712));
#85680=DIRECTION('center_axis',(0.0192786623139663,0.987363723283692,-0.157293391859761));
#85681=DIRECTION('ref_axis',(-0.996436816101143,0.0318943955032277,0.0780795687340866));
#85682=DIRECTION('',(0.688775998780597,0.,0.724974222647806));
#85683=DIRECTION('center_axis',(-0.0295486712570818,-0.987363722331637,
0.155691219567303));
#85684=DIRECTION('ref_axis',(-0.99081051081007,0.00836477140751204,-0.134998378759112));
#85685=DIRECTION('center_axis',(0.0313801075564329,-0.987363722072691,-0.155332447300972));
#85686=DIRECTION('ref_axis',(-0.978194999555421,0.00158398726276867,-0.207682531352836));
#85687=DIRECTION('',(-0.856091208538384,0.,0.516824769784972));
#85688=DIRECTION('center_axis',(2.94258679130039E-14,-1.,3.96472806032467E-15));
#85689=DIRECTION('ref_axis',(1.,2.94258679130039E-14,-2.03061687717273E-31));
#85690=DIRECTION('center_axis',(-0.00764753657259386,0.987363722466856,
0.158285800818532));
#85691=DIRECTION('ref_axis',(-0.998308827638998,0.00158367492915277,-0.0581117598405685));
#85692=DIRECTION('center_axis',(0.0526413609300347,0.987363723434933,-0.14947161859075));
#85693=DIRECTION('ref_axis',(-0.989925476770943,0.0318943888980207,-0.137950347577098));
#85694=DIRECTION('',(0.516824771977019,0.,0.856091207215039));
#85695=DIRECTION('center_axis',(-0.0623268468155332,-0.987363722406808,
0.145699155251516));
#85696=DIRECTION('ref_axis',(-0.938625251787949,0.00836476882371502,-0.344837160625904));
#85697=DIRECTION('center_axis',(0.0640383424309129,-0.987363722105989,-0.144955065339949));
#85698=DIRECTION('ref_axis',(-0.910679739708499,0.00158398709049708,-0.413110036999052));
#85699=DIRECTION('',(-0.947178320273382,0.,0.320707389381808));
#85700=DIRECTION('center_axis',(1.39428040580449E-13,-1.,5.09886334668116E-14));
#85701=DIRECTION('ref_axis',(1.,1.39428040580449E-13,2.22957426837468E-30));
#85702=DIRECTION('center_axis',(-0.0414955103107478,0.987363722492926,0.152941172118444));
#85703=DIRECTION('ref_axis',(-0.962476611317351,0.00158367430440513,-0.271360027717359));
#85704=DIRECTION('center_axis',(0.0835426153607864,0.987363723422421,-0.134660718430034));
#85705=DIRECTION('ref_axis',(-0.937126322349836,0.0318943895417038,-0.347529860407468));
#85706=DIRECTION('',(0.320707392680363,0.,0.947178319156516));
#85707=DIRECTION('center_axis',(-0.0921906959890649,-0.987363722318877,
0.128894357602123));
#85708=DIRECTION('ref_axis',(-0.842550917106313,0.00836477377934728,-0.538551745557408));
#85709=DIRECTION('center_axis',(0.0937022132057685,-0.987363722093186,-0.127799747787823));
#85710=DIRECTION('ref_axis',(-0.800582108000364,0.00158399010146328,-0.599220977040234));
#85711=DIRECTION('',(-0.993976426077081,-1.24675414343594E-14,0.109594089270516));
#85712=DIRECTION('center_axis',(2.50414483022948E-14,-1.,1.59538909637361E-14));
#85713=DIRECTION('ref_axis',(1.,2.50414483022948E-14,8.64987797024603E-31));
#85714=DIRECTION('center_axis',(-0.0734031997935144,0.987363722515641,0.14044518404036));
#85715=DIRECTION('ref_axis',(-0.881640057253848,0.00158367420529362,-0.47191980401488));
#85716=DIRECTION('center_axis',(0.110537511239738,0.987363723356507,-0.113553231607469));
#85717=DIRECTION('ref_axis',(-0.840508183059939,0.0318943919763055,-0.540859262627296));
#85718=DIRECTION('',(0.109594089288516,0.,0.993976426075096));
#85719=DIRECTION('center_axis',(-0.11774380657933,-0.987363722266,0.106062603990463));
#85720=DIRECTION('ref_axis',(-0.707079838374903,0.00836477484011131,-0.707084247247523));
#85721=DIRECTION('center_axis',(0.118984675664632,-0.987363722112959,-0.104668654391976));
#85722=DIRECTION('ref_axis',(-0.653050145064529,0.00158399001390786,-0.757313012569329));
#85723=DIRECTION('',(-0.994297298974217,0.,-0.106643711734809));
#85724=DIRECTION('center_axis',(-2.10263781896676E-14,-1.,-2.09640690225964E-14));
#85725=DIRECTION('ref_axis',(1.,-2.10263781896676E-14,4.52823587212026E-31));
#85726=DIRECTION('center_axis',(-0.101878638090563,0.987363722508961,0.121382134492933));
#85727=DIRECTION('ref_axis',(-0.759578996500587,0.00158367209155293,-0.650413130293253));
#85728=DIRECTION('center_axis',(0.132363795336434,0.98736372331842,-0.0871361208622546));
#85729=DIRECTION('ref_axis',(-0.704588813393261,0.0318943940108991,-0.708898689286243));
#85730=DIRECTION('',(-0.106643708884035,0.,0.994297299279978));
#85731=DIRECTION('center_axis',(-0.137791344891649,-0.987363722327925,0.0782714833364976));
#85732=DIRECTION('ref_axis',(-0.538546495051158,0.00836477267704766,-0.842554273175428));
#85733=DIRECTION('center_axis',(0.138703546279527,-0.987363722114087,-0.0766433722020272));
#85734=DIRECTION('ref_axis',(-0.474982282313184,0.00158399133528933,-0.879993933195001));
#85735=DIRECTION('',(-0.948125934970738,0.,-0.317894969189297));
#85736=DIRECTION('center_axis',(4.80844140052452E-14,-1.,7.49819715214931E-14));
#85737=DIRECTION('ref_axis',(2.0155716587825E-30,-7.49819715214931E-14,
-1.));
#85738=DIRECTION('center_axis',(-0.125590341158658,0.987363722487909,0.0966433946137617));
#85739=DIRECTION('ref_axis',(-0.602000863538362,0.00158367561643957,-0.798493864892278));
#85740=DIRECTION('center_axis',(0.148000890406933,0.987363723485712,-0.0566446288997078));
#85741=DIRECTION('ref_axis',(-0.535723656273679,0.0318943877768316,-0.843790798798554));
#85742=DIRECTION('',(-0.317894965895091,0.,0.948125936075245));
#85743=DIRECTION('center_axis',(-0.151395913665258,-0.987363722405331,0.0468204763255448));
#85744=DIRECTION('ref_axis',(-0.34483131411186,0.0083647694638503,-0.938627399685149));
#85745=DIRECTION('center_axis',(0.151936793256339,-0.987363722132207,-0.0450343321502049));
#85746=DIRECTION('ref_axis',(-0.274704778256895,0.00158399311141727,-0.961527314104312));
#85747=DIRECTION('',(-0.857621255980855,0.,-0.514281811159816));
#85748=DIRECTION('center_axis',(4.11217595969307E-14,-1.,1.11420883109922E-13));
#85749=DIRECTION('ref_axis',(2.12336121339679E-30,-1.11420883109922E-13,
-1.));
#85750=DIRECTION('center_axis',(-0.143429583022958,0.987363722493762,0.067385712262476));
#85751=DIRECTION('ref_axis',(-0.416273840057586,0.00158367279585466,-0.909237912795208));
#85752=DIRECTION('center_axis',(0.156717633017502,0.98736372345637,-0.0235044911402842));
#85753=DIRECTION('ref_axis',(-0.341808656410646,0.0318943892618742,-0.939228188640205));
#85754=DIRECTION('',(-0.514281808963847,0.,0.857621257297692));
#85755=DIRECTION('center_axis',(-0.157921381073739,-0.987363722267462,0.0131801877795928));
#85756=DIRECTION('ref_axis',(-0.134992203354449,0.00836477513405653,-0.990811352160676));
#85757=DIRECTION('center_axis',(0.158065646082108,-0.987363722122479,-0.0113195302504295));
#85758=DIRECTION('ref_axis',(-0.0615823826120716,0.00158398821891373,-0.998100746985565));
#85759=DIRECTION('',(-0.727015160077822,0.,-0.686621407339604));
#85760=DIRECTION('center_axis',(-8.10407971111379E-15,-1.,-5.88279438136482E-14));
#85761=DIRECTION('ref_axis',(-2.99900690858271E-31,5.88279438136482E-14,
-1.));
#85762=DIRECTION('center_axis',(-0.15456221444901,0.98736372244984,0.0349771561824722));
#85763=DIRECTION('ref_axis',(-0.211082316846037,0.00158367759288358,-0.977467005826893));
#85764=DIRECTION('center_axis',(0.158106432629902,0.987363723460094,0.0107346893790416));
#85765=DIRECTION('ref_axis',(-0.13191106112732,0.0318943890127931,-0.990748313095594));
#85766=DIRECTION('',(-0.686621405562463,0.,0.727015161756224));
#85767=DIRECTION('center_axis',(-0.157062618066433,-0.987363722391757,-0.0210763780287661));
#85768=DIRECTION('ref_axis',(0.0811589922647188,0.00836476649861784,-0.996666066772617));
#85769=DIRECTION('center_axis',(0.156803523454507,-0.987363722103122,0.0229245568533188));
#85770=DIRECTION('ref_axis',(0.154419534208586,0.0015839866243612,-0.988004098392905));
#85771=DIRECTION('',(-0.562414644138898,0.,-0.826855348932398));
#85772=DIRECTION('center_axis',(-9.46331629412281E-15,-1.,1.18389433539854E-13));
#85773=DIRECTION('ref_axis',(3.25119361935713E-31,-1.18389433539854E-13,
-1.));
#85774=DIRECTION('center_axis',(-0.158467690465133,0.987363722444043,0.000933102400878574));
#85775=DIRECTION('ref_axis',(0.0039791834017034,0.00158367763717511,-0.999990828990245));
#85776=DIRECTION('center_axis',(0.152102351266528,0.987363723473008,0.0444719271980735));
#85777=DIRECTION('ref_axis',(0.0841545458583856,0.0318943886797806,-0.995942147106001));
#85778=DIRECTION('',(-0.826855347492317,0.,0.562414646256087));
#85779=DIRECTION('center_axis',(-0.148859780937109,-0.987363722285066,-0.0543474519617457));
#85780=DIRECTION('ref_axis',(0.293515284482669,0.00836477446767391,-0.955917783244544));
#85781=DIRECTION('center_axis',(0.14820944281693,-0.987363722100043,0.0560967141697563));
#85782=DIRECTION('ref_axis',(0.363200967923451,0.00158398863631637,-0.93170947611338));
#85783=DIRECTION('',(-0.371516244401546,0.,-0.928426453816225));
#85784=DIRECTION('center_axis',(-1.73461489318175E-14,-1.,5.67936105665548E-14));
#85785=DIRECTION('ref_axis',(-1.79164664649797E-31,-5.67936105665548E-14,
-1.));
#85786=DIRECTION('center_axis',(-0.154963392512639,0.987363722477644,-0.0331545851438956));
#85787=DIRECTION('ref_axis',(0.218854622341282,0.00158367475091716,-0.975756192014244));
#85788=DIRECTION('center_axis',(0.138986131040637,0.987363723275524,0.0761297138957497));
#85789=DIRECTION('ref_axis',(0.296285183575623,0.0318943948969972,-0.954566832425951));
#85790=DIRECTION('',(-0.928426452468148,0.,0.371516247770418));
#85791=DIRECTION('center_axis',(-0.133696426889398,-0.987363722309465,-0.0850772901790237));
#85792=DIRECTION('ref_axis',(0.492147125907155,0.00836477331035454,-0.870471847349926));
#85793=DIRECTION('center_axis',(0.132685252704572,-0.987363722101427,0.086645853869304));
#85794=DIRECTION('ref_axis',(0.55499952682238,0.00158398787712574,-0.831849154720578));
#85795=DIRECTION('',(-0.163246158252737,-1.24675414427253E-14,-0.986585369755564));
#85796=DIRECTION('center_axis',(1.45747765284724E-14,-1.,-2.58684491063667E-14));
#85797=DIRECTION('ref_axis',(5.35693019029158E-31,2.58684491063667E-14,
-1.));
#85798=DIRECTION('center_axis',(-0.144213177993266,0.987363722497658,-0.0656919994264963));
#85799=DIRECTION('ref_axis',(0.423496662042141,0.00158367336515953,-0.905896279503253));
#85800=DIRECTION('center_axis',(0.119371075236614,0.987363723315672,0.104227751952477));
#85801=DIRECTION('ref_axis',(0.494561850446257,0.031894393766983,-0.868557035392271));
#85802=DIRECTION('',(-0.986585369800573,0.,0.163246157980722));
#85803=DIRECTION('center_axis',(-0.112281577443688,-0.9873637223284,-0.111829008743547));
#85804=DIRECTION('ref_axis',(0.667766714850343,0.0083647716155623,-0.744323615864632));
#85805=DIRECTION('center_axis',(0.110956847896642,-0.987363722081101,0.11314352930237));
#85806=DIRECTION('ref_axis',(0.720846926519561,0.00158398805948769,-0.693092489866345));
#85807=DIRECTION('',(0.0526571372340305,0.,-0.998612650579952));
#85808=DIRECTION('center_axis',(1.97949782769355E-14,-1.,-2.21305130496739E-14));
#85809=DIRECTION('ref_axis',(-8.25466210470689E-31,2.21305130496739E-14,
-1.));
#85810=DIRECTION('center_axis',(-0.126719716998718,0.987363722469099,-0.0951577263060111));
#85811=DIRECTION('ref_axis',(0.60833646652202,0.00158367463533589,-0.793677664719219));
#85812=DIRECTION('center_axis',(0.094174361865117,0.987363723369365,0.127452215914363));
#85813=DIRECTION('ref_axis',(0.669713359057949,0.0318943909699352,-0.741934474548781));
#85814=DIRECTION('',(-0.998612650714781,0.,-0.0526571346770678));
#85815=DIRECTION('center_axis',(-0.0856165661101796,-0.987363722404662,
-0.133351727723007));
#85816=DIRECTION('ref_axis',(0.812162274774787,0.00836477053525665,-0.583371639734514));
#85817=DIRECTION('center_axis',(0.0840402268233821,-0.987363722129493,0.134350736872072));
#85818=DIRECTION('ref_axis',(0.852988322579091,0.00158399112249083,-0.521927593173452));
#85819=DIRECTION('',(0.266098244580432,0.,-0.963945913540388));
#85820=DIRECTION('center_axis',(-4.81791775471634E-14,-1.,3.4715557455305E-14));
#85821=DIRECTION('ref_axis',(1.,-4.81791775471634E-14,-1.60160519362453E-30));
#85822=DIRECTION('center_axis',(-0.103300975937542,0.987363722552576,-0.120173989521323));
#85823=DIRECTION('ref_axis',(0.764731136019292,0.00158366708520907,-0.644347562733969));
#85824=DIRECTION('center_axis',(0.0645741589271399,0.987363723386845,0.144717157719871));
#85825=DIRECTION('ref_axis',(0.813549812505479,0.0318943908738347,-0.580619884608758));
#85826=DIRECTION('',(-0.963945914018185,0.,-0.266098242849603));
#85827=DIRECTION('center_axis',(-0.0549482164094863,-0.987363722325894,
-0.148639070732333));
#85828=DIRECTION('ref_axis',(0.918582031228676,0.00836477290385111,-0.395141851083971));
#85829=DIRECTION('center_axis',(0.0531939751881081,-0.987363722116085,0.149275856228521));
#85830=DIRECTION('ref_axis',(0.945244934851768,0.00158399063008826,-0.326357938636032));
#85831=DIRECTION('',(0.467096893063886,0.,-0.884206136876501));
#85832=DIRECTION('center_axis',(1.09031187632399E-13,-1.,-4.7093656008092E-14));
#85833=DIRECTION('ref_axis',(1.,1.09031187632399E-13,-1.18181014932651E-30));
#85834=DIRECTION('center_axis',(-0.0750520055291037,0.987363722501096,-0.139571042680201));
#85835=DIRECTION('ref_axis',(0.885367824820323,0.00158367152393529,-0.464888488518951));
#85836=DIRECTION('center_axis',(0.0319545399072673,0.98736372339762,0.155215286288767));
#85837=DIRECTION('ref_axis',(0.919345582593993,0.0318943906489118,-0.392156152074713));
#85838=DIRECTION('',(-0.884206138072515,0.,-0.467096890799851));
#85839=DIRECTION('center_axis',(-0.0217105585997335,-0.987363722455224,
-0.156976212289159));
#85840=DIRECTION('ref_axis',(0.982049910802658,0.00836476579291928,-0.188435674397715));
#85841=DIRECTION('center_axis',(0.0198604336684252,-0.987363722123183,0.15722100180814));
#85842=DIRECTION('ref_axis',(0.993302943375519,0.00158399135114877,-0.115528150911064));
#85843=DIRECTION('',(0.646254610502261,0.,-0.763121863403592));
#85844=DIRECTION('center_axis',(0.,-1.,0.));
#85845=DIRECTION('ref_axis',(0.,0.,-1.));
#85846=DIRECTION('center_axis',(-0.0432936835437904,0.987363722495306,-0.152441911774364));
#85847=DIRECTION('ref_axis',(0.964605700418953,0.00158367242142303,-0.263691741814041));
#85848=DIRECTION('center_axis',(-0.00215923201411667,0.987363723575172,
0.158455719634478));
#85849=DIRECTION('ref_axis',(0.982153774465284,0.0318943847097455,-0.185355635273339));
#85850=DIRECTION('',(-0.763121866258997,0.,-0.646254607130491));
#85851=DIRECTION('center_axis',(0.0125422742197993,-0.987363722351044,-0.157973324148369));
#85852=DIRECTION('ref_axis',(0.999598229358044,0.00836477189981278,0.0270815519372187));
#85853=DIRECTION('center_axis',(-0.0144017728166543,-0.987363722007407,
0.157814667896928));
#85854=DIRECTION('ref_axis',(0.994915210037057,0.00158397858048353,0.100703603951277));
#85855=DIRECTION('',(0.795194177911862,-1.2467541437894E-14,-0.606354862613534));
#85856=DIRECTION('center_axis',(0.,-1.,0.));
#85857=DIRECTION('ref_axis',(0.,0.,-1.));
#85858=DIRECTION('center_axis',(-0.0095109963087418,0.987363722509277,-0.158184766718666));
#85859=DIRECTION('ref_axis',(0.998739685024105,0.00158367240317003,-0.0501650629389698));
#85860=DIRECTION('center_axis',(-0.0361720565381791,0.98736372327208,0.154286941417914));
#85861=DIRECTION('ref_axis',(0.999037547159214,0.0318943950411722,0.0301119067987736));
#85862=DIRECTION('',(-0.606354862831809,0.,-0.795194177745422));
#85863=DIRECTION('center_axis',(0.0462086372706431,-0.987363722333362,-0.151583777699325));
#85864=DIRECTION('ref_axis',(0.970406444941592,0.00836477114710228,0.241332472368468));
#85865=DIRECTION('center_axis',(-0.0479905467177105,-0.987363722122278,
0.151029095417331));
#85866=DIRECTION('ref_axis',(0.950006347883252,0.00158398786905911,0.312226568318515));
#85867=DIRECTION('',(0.906951352788388,0.,-0.421235377995858));
#85868=DIRECTION('center_axis',(0.,-1.,0.));
#85869=DIRECTION('ref_axis',(0.,0.,-1.));
#85870=DIRECTION('center_axis',(0.0247164153185022,0.987363722501068,-0.156531077753389));
#85871=DIRECTION('ref_axis',(0.986173711967527,0.00158367140532946,0.165707277477693));
#85872=DIRECTION('center_axis',(-0.0684934961390298,0.987363723561067,0.142903878121892));
#85873=DIRECTION('ref_axis',(0.969207435188215,0.0318943852159877,0.244171447486345));
#85874=DIRECTION('',(-0.421235379219833,0.,-0.90695135221991));
#85875=DIRECTION('center_axis',(0.0777143306467572,-0.987363722433298,-0.138106344657978));
#85876=DIRECTION('ref_axis',(0.895839535150784,0.00836476526275839,0.444298951116167));
#85877=DIRECTION('center_axis',(-0.0793353440989328,-0.98736372213029,0.137181570911415));
#85878=DIRECTION('ref_axis',(0.860676244930596,0.00158398939727591,0.509150166836621));
#85879=DIRECTION('',(0.976300488927256,0.,-0.21641939682108));
#85880=DIRECTION('center_axis',(2.66195733031672E-14,-1.,1.31529117696217E-14));
#85881=DIRECTION('ref_axis',(1.,2.66195733031672E-14,-2.69371696899743E-31));
#85882=DIRECTION('center_axis',(0.0577881148440998,0.987363722518325,-0.147558168996237));
#85883=DIRECTION('ref_axis',(0.927495351769603,0.00158367058952022,0.373831331529668));
#85884=DIRECTION('center_axis',(-0.0976122735639677,0.987363723325657,0.124838783677868));
#85885=DIRECTION('ref_axis',(0.894058259712442,0.0318943939332761,0.446813804481899));
#85886=DIRECTION('',(-0.216419402668503,0.,-0.976300487631041));
#85887=DIRECTION('center_axis',(0.105586202135494,-0.987363722288055,-0.118171205579362));
#85888=DIRECTION('ref_axis',(0.779384160790386,0.00836477417458723,0.626490511071056));
#85889=DIRECTION('center_axis',(-0.106970512095575,-0.98736372209358,0.116919587048206));
#85890=DIRECTION('ref_axis',(0.73110187581061,0.00158398776783174,0.682266471526308));
#85891=DIRECTION('',(0.999998899039541,0.,-0.00148388668929281));
#85892=DIRECTION('center_axis',(-2.31697352304947E-14,-1.,-1.85678253840655E-14));
#85893=DIRECTION('ref_axis',(1.,-2.31697352304947E-14,-7.4436340050474E-31));
#85894=DIRECTION('center_axis',(0.0881577081296384,0.98736372254722,-0.131685602459135));
#85895=DIRECTION('ref_axis',(0.825448339563568,0.0015836672265046,0.564475447393299));
#85896=DIRECTION('center_axis',(-0.122166803491906,0.987363723229867,0.100936366955741));
#85897=DIRECTION('ref_axis',(0.777103913440387,0.0318943968373218,0.628563644483213));
#85898=DIRECTION('',(-0.00148388924556319,0.,-0.999998899035747));
#85899=DIRECTION('center_axis',(0.12852096790079,-0.987363722400553,-0.0927105198840292));
#85900=DIRECTION('ref_axis',(0.626485654806589,0.00836476963973098,0.779388064413636));
#85901=DIRECTION('center_axis',(-0.129603853819052,-0.987363722117569,0.0911905769330912));
#85902=DIRECTION('ref_axis',(0.567341997927538,0.00158399122592401,0.823480751662955));
#85903=DIRECTION('',(0.976938472070387,0.,0.213521010181148));
#85904=DIRECTION('center_axis',(-3.72730121926079E-14,-1.,-4.62290562453021E-14));
#85905=DIRECTION('ref_axis',(-1.12700347311895E-30,4.62290562453021E-14,
-1.));
#85906=DIRECTION('center_axis',(0.114405139984501,0.987363722521768,-0.109655567086603));
#85907=DIRECTION('ref_axis',(0.684804280432006,0.0015836701562166,0.728725318272144));
#85908=DIRECTION('center_axis',(-0.141008943767301,0.987363723370658,0.0723142831621817));
#85909=DIRECTION('ref_axis',(0.623813053134467,0.0318943919879685,0.780922545774402));
#85910=DIRECTION('',(0.21352100493591,0.,-0.976938473216793));
#85911=DIRECTION('center_axis',(0.145446241810615,-0.987363722339979,-0.0629147880081431));
#85912=DIRECTION('ref_axis',(0.444293371274801,0.00836477215045521,0.895842302432823));
#85913=DIRECTION('center_axis',(-0.146177066759276,-0.987363722116811,0.061197593100471));
#85914=DIRECTION('ref_axis',(0.377053836385937,0.00158398999577492,0.926189988848044));
#85915=DIRECTION('',(0.908197487535578,0.,0.418541901885658));
#85916=DIRECTION('center_axis',(-2.6463709296946E-14,-1.,-5.31608424195587E-14));
#85917=DIRECTION('ref_axis',(-9.88265445775187E-31,5.31608424195587E-14,
-1.));
#85918=DIRECTION('center_axis',(0.135303116346826,0.987363722522324,-0.0824981584867021));
#85919=DIRECTION('ref_axis',(0.512139533901716,0.00158367135915935,0.858900803236299));
#85920=DIRECTION('center_axis',(-0.153257664669201,0.98736372347784,0.0403108642938551));
#85921=DIRECTION('ref_axis',(0.441353388196775,0.0318943881547522,0.896766376896157));
#85922=DIRECTION('',(0.418541898467425,0.,-0.908197489110867));
#85923=DIRECTION('center_axis',(0.155570609330718,-0.987363722322886,-0.0301772323642034));
#85924=DIRECTION('ref_axis',(0.241326424552547,0.00836477233750035,0.970407948955709));
#85925=DIRECTION('center_axis',(-0.155915202237607,-0.987363722117027,0.0283430760224913));
#85926=DIRECTION('ref_axis',(0.169135057023849,0.00158398703376236,0.985591610897037));
#85927=DIRECTION('',(0.796990199392675,0.,0.603992236764699));
#85928=DIRECTION('center_axis',(-4.3250978366289E-14,-1.,-1.72820660217093E-13));
#85929=DIRECTION('ref_axis',(1.82527821333089E-30,1.72820660217093E-13,
-1.));
#85930=DIRECTION('center_axis',(0.149874468447564,0.987363722435629,-0.0514832334417587));
#85931=DIRECTION('ref_axis',(0.315527715267146,0.00158367769808369,0.94891503985512));
#85932=DIRECTION('center_axis',(-0.158340230231295,0.987363723437144,0.00642254860944178));
#85933=DIRECTION('ref_axis',(0.238256526802803,0.0318943903744065,0.970678409824031));
#85934=DIRECTION('',(0.603992234724004,0.,-0.796990200939199));
#85935=DIRECTION('center_axis',(0.158420668035202,-0.987363722286791,0.0039713790114702));
#85936=DIRECTION('ref_axis',(0.0270753218508432,0.00836477428387887,0.999598398106886));
#85937=DIRECTION('center_axis',(-0.158362914949753,-0.987363722140767,-0.00583672587568806));
#85938=DIRECTION('ref_axis',(-0.0466922879302391,0.00158399001302859,0.998908064450117));
#85939=DIRECTION('',(0.648516533598729,0.,0.761200568607965));
#85940=DIRECTION('center_axis',(1.6961537084023E-15,-1.,5.93592969796357E-14));
#85941=DIRECTION('ref_axis',(0.0285626985659955,5.93835252853779E-14,0.999592002894495));
#85942=DIRECTION('center_axis',(0.157437860183184,0.98736372253255,-0.0180609968608128));
#85943=DIRECTION('ref_axis',(0.104162167762182,0.0015836710625599,0.994559065512476));
#85944=DIRECTION('center_axis',(-0.156018981952473,0.987363723488671,-0.0277660729866842));
#85945=DIRECTION('ref_axis',(0.0240190581876539,0.0318943875855101,0.9992025985176));
#85946=DIRECTION('center_axis',(-0.159684140538363,-0.986495108818778,0.0364468865220547));
#85947=DIRECTION('ref_axis',(0.0345447361073574,0.0313138932743736,0.998912459275223));
#85948=DIRECTION('center_axis',(-0.148115809490731,-0.986495108701721,0.0699221530452668));
#85949=DIRECTION('ref_axis',(0.248473749993952,0.0313138980921802,0.968132343923193));
#85950=DIRECTION('center_axis',(-0.12962174787917,-0.986495108694425,0.100127933159151));
#85951=DIRECTION('ref_axis',(0.450784409547227,0.0313138983123357,0.892083435493364));
#85952=DIRECTION('center_axis',(-0.105066723785353,-0.986495108928782,0.125651834895487));
#85953=DIRECTION('ref_axis',(0.632016888372423,0.0313138890706075,0.774321698755313));
#85954=DIRECTION('center_axis',(-0.0755988850223349,-0.986495108721425,
0.145300409676239));
#85955=DIRECTION('ref_axis',(0.783696961325252,0.0313138975870502,0.620353538417791));
#85956=DIRECTION('center_axis',(-0.0425961334791471,-0.986495108732847,
0.158154891985026));
#85957=DIRECTION('ref_axis',(0.898732234955032,0.0313138961805359,0.43737833709356));
#85958=DIRECTION('center_axis',(-0.0076016341106203,-0.98649510878029,0.163614227716942));
#85959=DIRECTION('ref_axis',(0.97174378815581,0.0313138950000823,0.233951811620515));
#85960=DIRECTION('center_axis',(0.0277483045209817,-0.986495108911177,0.161423144841548));
#85961=DIRECTION('ref_axis',(0.999317682535591,0.0313138888934835,0.0195859575732665));
#85962=DIRECTION('center_axis',(0.06180077703097,-0.986495108727566,0.151684094139618));
#85963=DIRECTION('ref_axis',(0.980164591732371,0.0313138968610427,-0.195695715276269));
#85964=DIRECTION('center_axis',(0.0929635090524299,-0.98649510864731,0.134852462341594));
#85965=DIRECTION('ref_axis',(0.915180094010994,0.0313139006406196,-0.401826872113722));
#85966=DIRECTION('center_axis',(0.119779364643231,-0.986495108721393,0.111715282188389));
#85967=DIRECTION('ref_axis',(0.807402792437604,0.031313897487759,-0.58916905094216));
#85968=DIRECTION('center_axis',(0.140994469775086,-0.986495108843429,0.0833544223231981));
#85969=DIRECTION('ref_axis',(0.661872236306209,0.0313138927496215,-0.748962337456219));
#85970=DIRECTION('center_axis',(0.155616833928388,-0.98649510884469,0.0510960000744523));
#85971=DIRECTION('ref_axis',(0.485393267343429,0.0313138915404638,-0.873734980537155));
#85972=DIRECTION('center_axis',(0.162962728474184,-0.986495108838192,0.016448384922926));
#85973=DIRECTION('ref_axis',(0.286217849566809,0.031313891402459,-0.95765274645593));
#85974=DIRECTION('center_axis',(0.162688667007504,-0.986495108715825,-0.0189683448691279));
#85975=DIRECTION('ref_axis',(0.0736591994292219,0.0313138971291646,-0.996791734609608));
#85976=DIRECTION('center_axis',(0.154807463159199,-0.986495108750943,-0.0534981285717385));
#85977=DIRECTION('ref_axis',(-0.142343667071612,0.0313138962284748,-0.989321848716381));
#85978=DIRECTION('center_axis',(0.139687633297746,-0.986495108711815,-0.0855264028902112));
#85979=DIRECTION('ref_axis',(-0.351690706253517,0.0313138985509523,-0.935592372185902));
#85980=DIRECTION('center_axis',(0.118036166693634,-0.986495108760817,-0.113555553555324));
#85981=DIRECTION('ref_axis',(-0.544593076327316,0.031313896742111,-0.838115637061602));
#85982=DIRECTION('center_axis',(0.0908654613277357,-0.986495108803846,-0.136274972917941));
#85983=DIRECTION('ref_axis',(-0.712030880213924,0.0313138942150547,-0.701449546047949));
#85984=DIRECTION('center_axis',(0.0594459848832865,-0.986495108759378,-0.152622328887617));
#85985=DIRECTION('ref_axis',(-0.846174912151683,0.0313138958326044,-0.53198445275485));
#85986=DIRECTION('center_axis',(0.0252468845082368,-0.986495108812974,-0.161833232405173));
#85987=DIRECTION('ref_axis',(-0.940752744030153,0.0313138932274296,-0.337644361260008));
#85988=DIRECTION('center_axis',(-0.0101327382908042,-0.986495108745157,
-0.163476995435478));
#85989=DIRECTION('ref_axis',(-0.991342024823339,0.0313138963622141,-0.127516389980966));
#85990=DIRECTION('center_axis',(-0.0450385595798584,-0.98649510879385,-0.157476755353867));
#85991=DIRECTION('ref_axis',(-0.995577253951608,0.0313138940938735,0.0885741014679431));
#85992=DIRECTION('center_axis',(-0.0778384300520701,-0.986495108830986,
-0.144113077337106));
#85993=DIRECTION('ref_axis',(-0.953260397127133,0.0313138934865127,0.300522969743973));
#85994=DIRECTION('center_axis',(-0.106998666375314,-0.986495108702445,-0.124010829769242));
#85995=DIRECTION('ref_axis',(-0.866370142673745,0.0313138977871995,0.498419718398908));
#85996=DIRECTION('center_axis',(-0.131155757433405,-0.986495108791424,-0.0981099771820695));
#85997=DIRECTION('ref_axis',(-0.738969385524146,0.0313138950364302,0.673010911676559));
#85998=DIRECTION('center_axis',(-0.149180151055395,-0.986495108909675,-0.0676216136185635));
#85999=DIRECTION('ref_axis',(-0.577015238312227,0.0313138897532672,0.816132866060425));
#86000=DIRECTION('center_axis',(-0.160229051121939,-0.986495108808044,-0.033971333126167));
#86001=DIRECTION('ref_axis',(-0.38808050329743,0.0313138924109167,0.921093352002115));
#86002=DIRECTION('center_axis',(-0.163785817251066,-0.986495108829472,0.00126740795685309));
#86003=DIRECTION('ref_axis',(-0.180999553561232,0.0313138929432056,0.982984537884181));
#86004=DIRECTION('center_axis',(0.163393689063109,0.986495109768771,0.0113974021885637));
#86005=DIRECTION('ref_axis',(-0.0794050099347329,0.00163495854620576,0.996841096317671));
#86006=DIRECTION('center_axis',(0.157123533358946,0.986495109699961,0.0462557434581015));
#86007=DIRECTION('ref_axis',(-0.291839933992601,0.00163496610135612,0.956465775557621));
#86008=DIRECTION('center_axis',(0.143506452626063,0.98649510974477,0.0789512286436251));
#86009=DIRECTION('ref_axis',(-0.490628746776434,0.00163496164287221,0.871367178482763));
#86010=DIRECTION('center_axis',(0.123179172730457,0.98649510972553,0.107955036441359));
#86011=DIRECTION('ref_axis',(-0.666476305501507,0.00163496401637486,0.74552442018872));
#86012=DIRECTION('center_axis',(0.0970921703789306,0.986495109704194,0.131910988855437));
#86013=DIRECTION('ref_axis',(-0.811160172091883,0.00163496371730446,0.58482176952086));
#86014=DIRECTION('center_axis',(0.0664652449160892,0.986495109728464,0.149698930190134));
#86015=DIRECTION('ref_axis',(-0.917915092029476,0.00163496284088318,0.396773500527729));
#86016=DIRECTION('center_axis',(0.0327304761927758,0.986495109770256,0.160487115768106));
#86017=DIRECTION('ref_axis',(-0.981749320862673,0.00163495903920392,0.190172547689251));
#86018=DIRECTION('center_axis',(-0.00253472577803093,0.986495109707266,
0.163771101507191));
#86019=DIRECTION('ref_axis',(-0.999678043570141,0.00163496356549726,-0.0253206654319272));
#86020=DIRECTION('center_axis',(-0.0376814169658792,0.986495109780748,0.159397331201352));
#86021=DIRECTION('ref_axis',(-0.970862931954814,0.00163495726033712,-0.239629911052146));
#86022=DIRECTION('center_axis',(-0.0710661533304047,0.986495109669065,0.147570323743763));
#86023=DIRECTION('ref_axis',(-0.896651348677815,0.0016349660250336,-0.442734328689737));
#86024=DIRECTION('center_axis',(-0.101127924003168,0.986495109680366,0.128843088924214));
#86025=DIRECTION('ref_axis',(-0.780513344196942,0.00163496565390908,-0.625136982122972));
#86026=DIRECTION('center_axis',(-0.126461067969803,0.986495109761011,0.10409129024826));
#86027=DIRECTION('ref_axis',(-0.627879402344894,0.00163496041797718,-0.778308925180388));
#86028=DIRECTION('center_axis',(-0.145881030927093,0.986495109831703,0.0744722974923257));
#86029=DIRECTION('ref_axis',(-0.445886520492454,0.00163495483425792,-0.895088005598233));
#86030=DIRECTION('center_axis',(-0.158479755726482,0.986495109780593,0.0413710696483741));
#86031=DIRECTION('ref_axis',(-0.243044480116943,0.00163495717991353,-0.97001376670628));
#86032=DIRECTION('center_axis',(-0.163668144146346,0.986495109748637,0.00633537952423184));
#86033=DIRECTION('ref_axis',(-0.0288379486012532,0.00163496263033163,-0.999582762765379));
#86034=DIRECTION('center_axis',(-0.161203593004104,0.986495109729878,-0.0289965529262278));
#86035=DIRECTION('ref_axis',(0.186717016147342,0.00163496130242488,-0.98241237918838));
#86036=DIRECTION('center_axis',(-0.151201340427938,0.986495109738066,-0.0629726378332434));
#86037=DIRECTION('ref_axis',(0.393541296294608,0.00163496009607257,-0.919305485144217));
#86038=DIRECTION('center_axis',(-0.134129084367225,0.986495109697267,-0.0940041875141071));
#86039=DIRECTION('ref_axis',(0.581964024137621,0.00163496488445213,-0.813212888178349));
#86040=DIRECTION('center_axis',(-0.110785101103599,0.986495109684906,-0.120640208642186));
#86041=DIRECTION('ref_axis',(0.743174760527573,0.00163496707339627,-0.669095361064066));
#86042=DIRECTION('center_axis',(-0.0822609321710779,0.986495109641854,-0.141635227577926));
#86043=DIRECTION('ref_axis',(0.869635471994105,0.00163497154988837,-0.493691677788497));
#86044=DIRECTION('center_axis',(-0.0498903167228879,0.986495109779128,-0.156007546866028));
#86045=DIRECTION('ref_axis',(0.95543299508861,0.0016349575170583,-0.295203520998523));
#86046=DIRECTION('center_axis',(-0.0151869031800958,0.986495109716005,-0.163085120345806));
#86047=DIRECTION('ref_axis',(0.996555533314269,0.00163496265415759,-0.0829119769263292));
#86048=DIRECTION('center_axis',(0.0202266359325298,0.986495109692222,-0.162537016559871));
#86049=DIRECTION('ref_axis',(0.991080242650887,0.00163496541075243,0.133256442677886));
#86050=DIRECTION('center_axis',(0.0546944116456743,0.986495109801367,-0.154388858641817));
#86051=DIRECTION('ref_axis',(0.93926314036049,0.00163495565976323,0.343193939457185));
#86052=DIRECTION('center_axis',(0.0866047237704853,0.986495109744136,-0.139021653966364));
#86053=DIRECTION('ref_axis',(0.843527139657631,0.00163495989678595,0.537084063780664));
#86054=DIRECTION('center_axis',(0.114465497175955,0.986495109730546,-0.117153951849609));
#86055=DIRECTION('ref_axis',(0.708348745149213,0.00163496368711045,0.705860738488321));
#86056=DIRECTION('center_axis',(0.136973995550169,0.986495109745676,-0.0898082568079875));
#86057=DIRECTION('ref_axis',(0.5400487517329,0.00163496073983085,0.841632148064174));
#86058=DIRECTION('center_axis',(0.153077741137595,0.986495109790513,-0.0582632262032798));
#86059=DIRECTION('ref_axis',(0.34649667925581,0.00163495710657844,0.938049773828637));
#86060=DIRECTION('center_axis',(0.162023740072934,0.986495109747255,-0.0239938762505992));
#86061=DIRECTION('ref_axis',(0.136742804768779,0.00163495871085023,0.990605235325345));
#86062=DIRECTION('center_axis',(0.155570611334107,0.98736372189594,-0.0301772360054662));
#86063=DIRECTION('ref_axis',(0.10656539603492,0.0135959508125922,0.994212737038418));
#86064=DIRECTION('',(-0.603590599317291,0.,0.797294417649963));
#86065=DIRECTION('',(-0.797294417685632,0.,-0.603590599270175));
#86066=DIRECTION('center_axis',(-2.16690239644328E-14,-1.,-8.63994232248037E-14));
#86067=DIRECTION('ref_axis',(2.20896655942274E-31,8.63994232248037E-14,
-1.));
#86068=DIRECTION('center_axis',(-0.153257677595439,-0.987363722047016,0.0403108501958945));
#86069=DIRECTION('ref_axis',(0.171510441839821,0.0135962682989244,0.985088478172521));
#86070=DIRECTION('center_axis',(0.157437855436751,-0.987363722701725,-0.0180610289869838));
#86071=DIRECTION('ref_axis',(0.239571732524885,0.0204448268811709,0.970663378328875));
#86072=DIRECTION('center_axis',(0.145446242574693,0.987363721859127,-0.062914793788077));
#86073=DIRECTION('ref_axis',(0.317800305140332,0.0135959530681929,0.94806018591273));
#86074=DIRECTION('',(-0.418084253477456,0.,0.908408254582816));
#86075=DIRECTION('',(-0.908408255110073,0.,-0.418084252331839));
#86076=DIRECTION('center_axis',(0.,-1.,0.));
#86077=DIRECTION('ref_axis',(0.,0.,-1.));
#86078=DIRECTION('center_axis',(-0.141008954754318,-0.987363721980961,0.072314280712722));
#86079=DIRECTION('ref_axis',(0.379265525348352,0.0135962744649355,0.925187982305711));
#86080=DIRECTION('center_axis',(0.149874459410224,-0.98736372263828,-0.0514832558641257));
#86081=DIRECTION('ref_axis',(0.442634611781386,0.0204448284590848,0.896468967361626));
#86082=DIRECTION('center_axis',(0.128520970205328,0.987363721862734,-0.0927105224170952));
#86083=DIRECTION('ref_axis',(0.514175227362223,0.0135959513014948,0.857577393402609));
#86084=DIRECTION('',(-0.213028754318377,0.,0.977045930257918));
#86085=DIRECTION('',(-0.977045930401007,0.,-0.213028753662108));
#86086=DIRECTION('center_axis',(6.52685246616099E-14,-1.,8.08679734183554E-14));
#86087=DIRECTION('ref_axis',(6.18340889097101E-32,-8.08679734183554E-14,
-1.));
#86088=DIRECTION('center_axis',(-0.122166801556987,-0.987363721726011,0.100936384008427));
#86089=DIRECTION('ref_axis',(0.569286579566093,0.0135962907662992,0.822026721708812));
#86090=DIRECTION('center_axis',(0.135303100939358,-0.987363722605958,-0.0824981827551266));
#86091=DIRECTION('ref_axis',(0.625000388726575,0.0204448305551808,0.780356663965395));
#86092=DIRECTION('center_axis',(0.105586198250978,0.987363721838476,-0.118171212806577));
#86093=DIRECTION('ref_axis',(0.686507884976537,0.0135959534087707,0.726995236515308));
#86094=DIRECTION('',(0.00198773449113936,0.,0.999998024453845));
#86095=DIRECTION('',(-0.999998024453727,0.,0.00198773455025544));
#86096=DIRECTION('center_axis',(5.2152947146657E-14,-1.,4.17513353568119E-14));
#86097=DIRECTION('ref_axis',(1.,5.2152947146657E-14,1.83929845959689E-31));
#86098=DIRECTION('center_axis',(-0.0976122826634162,-0.987363722002467,
0.124838787028203));
#86099=DIRECTION('ref_axis',(0.732688419148167,0.0135962746535594,0.680428410460428));
#86100=DIRECTION('center_axis',(0.114405116851751,-0.987363722685321,-0.109655589748638));
#86101=DIRECTION('ref_axis',(0.778141843300161,0.020444828126451,0.627755749243532));
#86102=DIRECTION('center_axis',(0.077714336524821,0.987363721911229,-0.138106345082737));
#86103=DIRECTION('ref_axis',(0.826740198628292,0.0135959500333555,0.562419589021171));
#86104=DIRECTION('',(0.216911277181653,0.,0.976191322349991));
#86105=DIRECTION('',(-0.976191322337167,0.,0.216911277239366));
#86106=DIRECTION('center_axis',(7.32220417368825E-14,-1.,3.61336193395029E-14));
#86107=DIRECTION('ref_axis',(1.,7.32220417368825E-14,4.40866552489188E-31));
#86108=DIRECTION('center_axis',(-0.0684935153893333,-0.987363722021411,
0.142903879533191));
#86109=DIRECTION('ref_axis',(0.861830567147825,0.0135962712680681,0.507014018481997));
#86110=DIRECTION('center_axis',(0.0881576752415342,-0.987363722731981,-0.131685623090954));
#86111=DIRECTION('ref_axis',(0.894898249330239,0.0204448245006342,0.445801673950212));
#86112=DIRECTION('center_axis',(0.0462086360162934,0.987363721869846,-0.151583781100878));
#86113=DIRECTION('ref_axis',(0.928315057984613,0.0135959512476378,0.371545829244113));
#86114=DIRECTION('',(0.421692289376655,0.,0.906738999426117));
#86115=DIRECTION('',(-0.906738999989211,0.,0.421692288165868));
#86116=DIRECTION('center_axis',(-4.32424423825748E-14,-1.,-1.06626877233512E-14));
#86117=DIRECTION('ref_axis',(1.,-4.32424423825748E-14,1.06587266596841E-31));
#86118=DIRECTION('center_axis',(-0.0361720451580659,-0.987363721718911,
0.154286954025493));
#86119=DIRECTION('ref_axis',(0.950674474606201,0.0135962922486553,0.309892213792654));
#86120=DIRECTION('center_axis',(0.0577880837103379,-0.987363722692009,-0.147558180026943));
#86121=DIRECTION('ref_axis',(0.969810207301856,0.020444826699476,0.243002409194558));
#86122=DIRECTION('center_axis',(0.0125422746948997,0.987363721956659,-0.157973326575631));
#86123=DIRECTION('ref_axis',(0.986482938283097,0.0135959480903535,0.163298997767508));
#86124=DIRECTION('',(0.606755441382883,0.,0.794888567254721));
#86125=DIRECTION('',(-0.794888567218748,0.,0.60675544143001));
#86126=DIRECTION('',(0.763447380573604,0.,0.645870031117177));
#86127=DIRECTION('',(-0.645870029654529,0.,0.763447381810991));
#86128=DIRECTION('center_axis',(5.10100782136153E-14,-1.,-9.89314317053015E-15));
#86129=DIRECTION('ref_axis',(1.,5.10100782136153E-14,9.10962590624933E-32));
#86130=DIRECTION('center_axis',(0.0319545315684787,-0.987363721993528,0.155215296937275));
#86131=DIRECTION('ref_axis',(0.992929149174126,0.0135962725467901,-0.117927291553649));
#86132=DIRECTION('center_axis',(-0.009511024361953,-0.987363722641815,-0.158184764204658));
#86133=DIRECTION('ref_axis',(0.982209968780626,0.0204448300012928,-0.186669724792695));
#86134=DIRECTION('center_axis',(-0.0549482154845397,0.987363722017389,-0.148639073123564));
#86135=DIRECTION('ref_axis',(0.96387513573961,0.0135959452699276,-0.266007279928886));
#86136=DIRECTION('',(0.884441369774467,0.,0.466651329615018));
#86137=DIRECTION('',(-0.466651329562727,0.,0.884441369802057));
#86138=DIRECTION('center_axis',(5.45037230112174E-14,-1.,-2.35742925329388E-14));
#86139=DIRECTION('ref_axis',(1.,5.45037230112174E-14,1.05938335290951E-31));
#86140=DIRECTION('center_axis',(0.0645741461527722,-0.987363722058208,0.144717172484823));
#86141=DIRECTION('ref_axis',(0.944364136417791,0.0135962653503995,-0.328620631452744));
#86142=DIRECTION('center_axis',(-0.043293709194828,-0.987363722575933,-0.152441903967217));
#86143=DIRECTION('ref_axis',(0.919117972571777,0.0204448313293298,-0.393451599777483));
#86144=DIRECTION('center_axis',(-0.0856165677881559,0.987363721914613,-0.133351730274106));
#86145=DIRECTION('ref_axis',(0.884156568761363,0.0135959498463249,-0.466992839413957));
#86146=DIRECTION('',(0.964079864249621,0.,0.265612528598395));
#86147=DIRECTION('',(-0.265612528541396,0.,0.964079864265324));
#86148=DIRECTION('center_axis',(-4.21414701015372E-14,-1.,3.03973494430455E-14));
#86149=DIRECTION('ref_axis',(1.,-4.21414701015372E-14,-3.74202457519215E-31));
#86150=DIRECTION('center_axis',(0.0941743565822621,-0.987363722016396,0.127452230299223));
#86151=DIRECTION('ref_axis',(0.851641705444955,0.0135962698329562,-0.523948038447934));
#86152=DIRECTION('center_axis',(-0.0750520328118397,-0.98736372270104,-0.139571026594901));
#86153=DIRECTION('ref_axis',(0.813049042287908,0.0204448268834036,-0.581836114286852));
#86154=DIRECTION('center_axis',(-0.112281580731656,0.987363721908427,-0.111829009150301));
#86155=DIRECTION('ref_axis',(0.763095823305131,0.0135959506265528,-0.646142333066658));
#86156=DIRECTION('',(0.998639054975845,0.,0.0521539823690411));
#86157=DIRECTION('',(-0.05215398216031,0.,0.998639054986746));
#86158=DIRECTION('center_axis',(-9.8919126969435E-15,-1.,1.10702419355046E-14));
#86159=DIRECTION('ref_axis',(3.04300242946951E-32,-1.10702419355046E-14,
-1.));
#86160=DIRECTION('center_axis',(0.11937107706672,-0.98736372199191,0.104227762396657));
#86161=DIRECTION('ref_axis',(0.719097454151467,0.0135962733631525,-0.694776217773402));
#86162=DIRECTION('center_axis',(-0.103301005450512,-0.987363722780564,-0.120173962278935));
#86163=DIRECTION('ref_axis',(0.668962840739906,0.0204448234264662,-0.743014620922265));
#86164=DIRECTION('center_axis',(-0.133696432457323,0.987363721861109,-0.0850772866325803));
#86165=DIRECTION('ref_axis',(0.606353563973455,0.0135959524929253,-0.795078930378927));
#86166=DIRECTION('',(0.986502993673533,0.,-0.163743224205332));
#86167=DIRECTION('',(0.163743224263852,0.,0.986502993663819));
#86168=DIRECTION('center_axis',(1.45617409646071E-14,-1.,-2.58757892796229E-14));
#86169=DIRECTION('ref_axis',(7.31829950293539E-33,2.58757892796229E-14,
-1.));
#86170=DIRECTION('center_axis',(0.138986134014219,-0.987363722017432,0.076129724783847));
#86171=DIRECTION('ref_axis',(0.552929007076716,0.0135962705645634,-0.833117431434424));
#86172=DIRECTION('center_axis',(-0.126719731068657,-0.98736372256976,-0.0951577065248656));
#86173=DIRECTION('ref_axis',(0.493596682389456,0.0204448315520646,-0.869450587438372));
#86174=DIRECTION('center_axis',(-0.148859783585737,0.987363721978464,-0.0543474502772831));
#86175=DIRECTION('ref_axis',(0.421258887391482,0.0135959476505099,-0.906838519253111));
#86176=DIRECTION('',(0.928239148269088,0.,-0.37198398301631));
#86177=DIRECTION('',(0.371983982078545,0.,0.928239148644889));
#86178=DIRECTION('center_axis',(2.38116057765714E-14,-1.,-7.8103221770465E-14));
#86179=DIRECTION('ref_axis',(-2.79864792815286E-31,7.8103221770465E-14,
-1.));
#86180=DIRECTION('center_axis',(0.152102356226166,-0.987363722014895,0.0444719426081411));
#86181=DIRECTION('ref_axis',(0.360906212233439,0.0135962715702553,-0.932503001266323));
#86182=DIRECTION('center_axis',(-0.144213189673931,-0.987363722716407,-0.0656919704961667));
#86183=DIRECTION('ref_axis',(0.295150489684352,0.020444826116553,-0.955232012405443));
#86184=DIRECTION('center_axis',(-0.157062621723428,0.987363721820909,-0.0210763775190806));
#86185=DIRECTION('ref_axis',(0.216466612364278,0.0135959542449752,-0.976195347130738));
#86186=DIRECTION('',(0.826571873636816,0.,-0.562831180472905));
#86187=DIRECTION('',(0.562831181859169,0.,0.826571872692878));
#86188=DIRECTION('center_axis',(4.70183251359275E-15,-1.,-5.91970933019358E-14));
#86189=DIRECTION('ref_axis',(-6.63462100443905E-32,5.91970933019358E-14,
-1.));
#86190=DIRECTION('center_axis',(0.158106440927349,-0.987363722001391,0.0107347013394576));
#86191=DIRECTION('ref_axis',(0.152007846781394,0.0135962733988064,-0.988285766297658));
#86192=DIRECTION('center_axis',(-0.154963397163516,-0.987363722655234,-0.0331545581171144));
#86193=DIRECTION('ref_axis',(0.0829033887011708,0.0204448284530127,-0.996347849463926));
#86194=DIRECTION('center_axis',(-0.15792138294966,0.987363721859615,0.0131801958557069));
#86195=DIRECTION('ref_axis',(0.00155260087807025,0.0135959528525333,-0.99990636536455));
#86196=DIRECTION('',(0.686255015216422,0.,-0.727361020463916));
#86197=DIRECTION('',(0.727361020504861,0.,0.686255015173024));
#86198=DIRECTION('center_axis',(-5.08357432511528E-15,-1.,-3.67649082105399E-14));
#86199=DIRECTION('ref_axis',(-5.70858969985437E-32,3.67649082105399E-14,
-1.));
#86200=DIRECTION('center_axis',(0.156717643447317,-0.98736372201751,-0.02350448204169));
#86201=DIRECTION('ref_axis',(-0.0639982407964878,0.0135962738668925,-0.99785738786256));
#86202=DIRECTION('center_axis',(-0.158467688440349,-0.987363722742572,0.000933130377306471));
#86203=DIRECTION('ref_axis',(-0.133220182211163,0.0204448247090343,-0.990875568471764));
#86204=DIRECTION('center_axis',(-0.15139591711616,0.987363721932101,0.0468204751465142));
#86205=DIRECTION('ref_axis',(-0.213434009684826,0.0135959484370491,-0.976862873537507));
#86206=DIRECTION('',(0.513849635801822,0.,-0.857880266579396));
#86207=DIRECTION('',(0.857880267877561,0.,0.513849633634515));
#86208=DIRECTION('center_axis',(-2.05889466985223E-14,-1.,-5.57000749948014E-14));
#86209=DIRECTION('ref_axis',(-2.77140440273355E-31,5.57000749948014E-14,
-1.));
#86210=DIRECTION('center_axis',(0.148000904436245,-0.987363722001798,-0.0566446181098321));
#86211=DIRECTION('ref_axis',(-0.277011838133409,0.0135962708098426,-0.960770307073452));
#86212=DIRECTION('center_axis',(-0.154562208248359,-0.987363722638707,0.0349771782513351));
#86213=DIRECTION('ref_axis',(-0.343114525414335,0.0204448298680979,-0.939071047036038));
#86214=DIRECTION('center_axis',(-0.137791347031469,0.987363721984853,0.0782714838972129));
#86215=DIRECTION('ref_axis',(-0.418440681523933,0.0135959471253179,-0.908142360132789));
#86216=DIRECTION('',(0.317417216373473,0.,-0.948285985739384));
#86217=DIRECTION('',(0.948285986047992,0.,0.317417215451505));
#86218=DIRECTION('center_axis',(4.01018227942412E-14,-1.,6.24647791306544E-14));
#86219=DIRECTION('ref_axis',(-5.68566147680559E-31,-6.24647791306544E-14,
-1.));
#86220=DIRECTION('center_axis',(0.132363804604318,-0.98736372196756,-0.0871361220908843));
#86221=DIRECTION('ref_axis',(-0.477072672688627,0.0135962753491566,-0.878758673510743));
#86222=DIRECTION('center_axis',(-0.143429568774726,-0.987363722694813,0.0673857396437633));
#86223=DIRECTION('ref_axis',(-0.536965214303182,0.0204448268453923,-0.843356607659891));
#86224=DIRECTION('center_axis',(-0.11774380298488,0.987363721851963,0.10606261183517));
#86225=DIRECTION('ref_axis',(-0.603881533767801,0.0135959535221113,-0.796958118863264));
#86226=DIRECTION('',(0.106142721135687,0.,-0.994350905239147));
#86227=DIRECTION('',(0.994350904942087,0.,0.106142723918561));
#86228=DIRECTION('center_axis',(-3.15554073413638E-14,-1.,-3.14302085104392E-14));
#86229=DIRECTION('ref_axis',(1.,-3.15554073413638E-14,-3.88230226445637E-31));
#86230=DIRECTION('center_axis',(0.110537521518214,-0.98736372195799,-0.113553233762299));
#86231=DIRECTION('ref_axis',(-0.654826117545247,0.0135962759388342,-0.755657261634674));
#86232=DIRECTION('center_axis',(-0.125590323971213,-0.987363722658905,0.0966434152022493));
#86233=DIRECTION('ref_axis',(-0.705708007468931,0.0204448281709577,-0.708207750024872));
#86234=DIRECTION('center_axis',(-0.0921906931258788,0.98736372187097,0.128894363081076));
#86235=DIRECTION('ref_axis',(-0.761085557922345,0.0135959516747523,-0.648509000415639));
#86236=DIRECTION('',(-0.110094884194222,0.,-0.993921081612751));
#86237=DIRECTION('',(0.993921081291397,0.,-0.110094887095358));
#86238=DIRECTION('center_axis',(5.63613377604692E-14,-1.,3.58678618036695E-14));
#86239=DIRECTION('ref_axis',(1.,5.63613377604692E-14,-4.20975683792422E-31));
#86240=DIRECTION('center_axis',(0.0835426327848654,-0.987363722032105,-0.134660717814369));
#86241=DIRECTION('ref_axis',(-0.80196062057044,0.0135962689252322,-0.597222156760436));
#86242=DIRECTION('center_axis',(-0.101878612833617,-0.987363722718959,0.121382153983431));
#86243=DIRECTION('ref_axis',(-0.841452678222415,0.0204448262750383,-0.539943885409317));
#86244=DIRECTION('center_axis',(-0.0623268517272042,0.987363721958143,0.145699156190894));
#86245=DIRECTION('ref_axis',(-0.882702065230997,0.0135959474982537,-0.469736324174061));
#86246=DIRECTION('',(-0.321184582171429,0.,-0.947016612407282));
#86247=DIRECTION('',(0.947016612388014,0.,-0.321184582228242));
#86248=DIRECTION('center_axis',(-0.0295486726347458,0.98736372195704,0.15569122168146));
#86249=DIRECTION('ref_axis',(-0.963044405676187,0.0135959478040231,-0.268999299068065));
#86250=DIRECTION('',(-0.51725604351836,0.,-0.855830699054277));
#86251=DIRECTION('center_axis',(-3.48634287493128E-14,-1.,-1.27295943479517E-14));
#86252=DIRECTION('ref_axis',(1.,-3.48634287493128E-14,5.74501590485154E-32));
#86253=DIRECTION('center_axis',(0.05264137310468,-0.987363721985138,-0.149471623879952));
#86254=DIRECTION('ref_axis',(-0.911596337546528,0.0135962747113278,-0.410861605270839));
#86255=DIRECTION('center_axis',(-0.0734031758498871,-0.987363722626589,
0.140445195774421));
#86256=DIRECTION('ref_axis',(-0.937851956604742,0.0204448298265036,-0.346432845478055));
#86257=DIRECTION('',(0.855830699792872,0.,-0.517256042296312));
#86258=DIRECTION('center_axis',(-1.02997516282883E-13,-1.,-1.38246550625899E-14));
#86259=DIRECTION('ref_axis',(1.,-1.02997516282883E-13,-1.76484519791174E-31));
#86260=DIRECTION('center_axis',(0.00461117005004301,0.987363721951836,0.158403338614394));
#86261=DIRECTION('ref_axis',(-0.998355860480601,0.0135959481915025,-0.0556841632496482));
#86262=DIRECTION('center_axis',(0.0192786466928749,-0.987363721692602,-0.157293403761965));
#86263=DIRECTION('ref_axis',(-0.978606822198162,0.0135962945650253,-0.205289620588369));
#86264=DIRECTION('center_axis',(-0.0414954808748873,-0.98736372271376,0.152941178679215));
#86265=DIRECTION('ref_axis',(-0.99039832053053,0.0204448259328905,-0.136722989225951));
#86266=DIRECTION('',(-0.6891411857498,0.,-0.724627094513695));
#86267=DIRECTION('',(0.724627094472951,0.,-0.689141185792642));
#86268=DIRECTION('center_axis',(1.47944833905471E-14,-1.,-1.23428272891312E-15));
#86269=DIRECTION('ref_axis',(1.,1.47944833905471E-14,-1.04793950114792E-32));
#86270=DIRECTION('center_axis',(-0.0149854826176444,-0.987363722043136,
-0.157760310927184));
#86271=DIRECTION('ref_axis',(-0.999858739051166,0.0135962683570005,0.0098814690090491));
#86272=DIRECTION('center_axis',(-0.00764751232626353,-0.987363722585862,
0.158285801247647));
#86273=DIRECTION('ref_axis',(-0.996634759231673,0.0204448312899083,0.0793798813601607));
#86274=DIRECTION('center_axis',(0.0385554024431205,0.987363721891044,0.153708690827534));
#86275=DIRECTION('ref_axis',(-0.986985304127919,0.0135959516543579,0.16023470140432));
#86276=DIRECTION('',(-0.828802852674338,0.,-0.559540732564555));
#86277=DIRECTION('',(0.559540732515555,0.,-0.828802852707419));
#86278=DIRECTION('center_axis',(-4.96414180061546E-14,-1.,1.5350308719234E-14));
#86279=DIRECTION('ref_axis',(1.,-4.96414180061546E-14,-8.98706406991303E-33));
#86280=DIRECTION('center_axis',(-0.0485489594385595,-0.987363721707173,
-0.150850520695132));
#86281=DIRECTION('ref_axis',(-0.974358371712792,0.0135962938640854,0.224590525771589));
#86282=DIRECTION('center_axis',(0.0265580544860549,-0.987363722702375,0.156229154875853));
#86283=DIRECTION('ref_axis',(-0.956269664959881,0.0204448268694524,0.291771035114516));
#86284=DIRECTION('center_axis',(0.0706968220400096,0.987363721900133,0.14182679587779));
#86285=DIRECTION('ref_axis',(-0.929464413230009,0.0135959506144346,0.368661165117625));
#86286=DIRECTION('',(-0.929710620732484,0.,-0.368290865617407));
#86287=DIRECTION('',(0.368290866546792,0.,-0.929710620364322));
#86288=DIRECTION('center_axis',(-4.51809666877942E-14,-1.,2.56628645547669E-14));
#86289=DIRECTION('ref_axis',(1.,-4.51809666877942E-14,-2.20183821085922E-31));
#86290=DIRECTION('center_axis',(-0.0798422943103286,-0.987363721988475,
-0.136887137965287));
#86291=DIRECTION('ref_axis',(-0.903298092113965,0.0135962716534009,0.428797968955542));
#86292=DIRECTION('center_axis',(0.059521789918778,-0.987363722621634,0.146867408827195));
#86293=DIRECTION('ref_axis',(-0.871190463336196,0.0204448296496739,0.490519301896122));
#86294=DIRECTION('center_axis',(0.0995325402727057,0.987363721842399,0.123313236176773));
#86295=DIRECTION('ref_axis',(-0.82848279735365,0.0135959524090879,0.559849448126155));
#86296=DIRECTION('',(-0.987146152503824,0.,-0.159820128885245));
#86297=DIRECTION('',(0.159820128826887,0.,-0.987146152513272));
#86298=DIRECTION('center_axis',(3.86079034210145E-14,-1.,-3.47754532654341E-14));
#86299=DIRECTION('ref_axis',(1.,3.86079034210145E-14,3.58398621757385E-31));
#86300=DIRECTION('center_axis',(-0.107402316184702,-0.987363721994453,-0.116523057664233));
#86301=DIRECTION('ref_axis',(-0.790000597333135,0.0135962746960822,0.61295529814798));
#86302=DIRECTION('center_axis',(0.0897023546254517,-0.98736372263455,0.130638305254982));
#86303=DIRECTION('ref_axis',(-0.745375363963095,0.0204448301796836,0.66633143083289));
#86304=DIRECTION('center_axis',(0.123714222696916,0.987363721947433,0.0990336896445395));
#86305=DIRECTION('ref_axis',(-0.688762246509255,0.0135959484644339,0.724859791938329));
#86306=DIRECTION('',(-0.998423827575672,0.,0.0561236182827234));
#86307=DIRECTION('',(-0.0561236183417539,0.,-0.998423827572354));
#86308=DIRECTION('center_axis',(-2.59110665239106E-14,-1.,3.62245547218756E-14));
#86309=DIRECTION('ref_axis',(5.84001265530547E-32,-3.62245547218756E-14,
-1.));
#86310=DIRECTION('center_axis',(-0.129940334603434,-0.987363721715944,-0.0907104761446398));
#86311=DIRECTION('ref_axis',(-0.639763549392157,0.0135962927576524,0.768451522018402));
#86312=DIRECTION('center_axis',(0.11568853959148,-0.987363722702958,0.108300696661411));
#86313=DIRECTION('ref_axis',(-0.58470734183779,0.020444826339279,0.810986641984282));
#86314=DIRECTION('center_axis',(0.142111167041916,0.987363721998744,0.0701234388972172));
#86315=DIRECTION('ref_axis',(-0.516835941609039,0.0135959455452013,0.855976494844239));
#86316=DIRECTION('',(-0.963016313438974,0.,0.269443092415463));
#86317=DIRECTION('',(-0.269443091726455,0.,-0.963016313631752));
#86318=DIRECTION('center_axis',(-8.75903587034078E-15,-1.,2.04738791027141E-14));
#86319=DIRECTION('ref_axis',(-3.62806814991581E-32,-2.04738791027141E-14,
-1.));
#86320=DIRECTION('center_axis',(-0.14640246408389,-0.987363721985062,-0.060656401294257));
#86321=DIRECTION('ref_axis',(-0.459611873173492,0.013596274118306,0.888015803557602));
#86322=DIRECTION('center_axis',(0.136265253015123,-0.987363722600714,0.0808990736212951));
#86323=DIRECTION('ref_axis',(-0.39669905330566,0.0204448300118289,0.917721019717964));
#86324=DIRECTION('center_axis',(0.153863154833479,0.987363721917656,0.0379342882574982));
#86325=DIRECTION('ref_axis',(-0.320742961130513,0.0135959494123135,0.947068689718337));
#86326=DIRECTION('',(-0.882579228239459,0.,0.470163701151249));
#86327=DIRECTION('',(-0.470163700157015,0.,-0.882579228769103));
#86328=DIRECTION('center_axis',(1.66119026794174E-14,-1.,-8.75125797881813E-14));
#86329=DIRECTION('ref_axis',(7.00951663590181E-32,8.75125797881813E-14,
-1.));
#86330=DIRECTION('center_axis',(-0.156018993575103,-0.987363721745371,-0.0277660696704074));
#86331=DIRECTION('ref_axis',(-0.257969252019171,0.0135962909953125,0.966057454752998));
#86332=DIRECTION('center_axis',(0.150470357297635,-0.987363722706508,0.0497146925754064));
#86333=DIRECTION('ref_axis',(-0.190141558768352,0.0204448255908761,0.981543782383496));
#86334=DIRECTION('center_axis',(0.158420670878443,0.987363721854469,0.00397137307680872));
#86335=DIRECTION('ref_axis',(-0.109652395100579,0.0135959518425372,0.993877005641142));
#86336=DIRECTION('',(-0.760873717902008,0.,0.648899981049449));
#86337=DIRECTION('center_axis',(-1.51030376905466E-15,-1.,-5.19386305601871E-14));
#86338=DIRECTION('ref_axis',(0.0290663354547457,-5.19605846959252E-14,0.999577484812074));
#86339=DIRECTION('center_axis',(-0.158340239529416,-0.987363722011645,0.00642253852296898));
#86340=DIRECTION('ref_axis',(-0.0442642795989572,0.0135962721816249,0.998927332159026));
#86341=DIRECTION('center_axis',(0.157639633367977,-0.98736372267693,0.0162057129791808));
#86342=DIRECTION('ref_axis',(0.0253067453442215,0.0204448270264858,0.99947064873759));
#86343=DIRECTION('',(-0.648899979430115,0.,-0.760873719283033));
#86344=DIRECTION('center_axis',(-0.158362916807467,-0.987363722049377,-0.00583669093171205));
#86345=DIRECTION('ref_axis',(-0.150968894543394,0.018371221016767,0.988367791421138));
#86346=DIRECTION('',(0.563065840553494,0.,0.826412039603603));
#86347=DIRECTION('',(0.82641203914066,0.,-0.563065841232956));
#86348=DIRECTION('center_axis',(-0.15340576406886,-0.987363722034686,-0.039743577597651));
#86349=DIRECTION('ref_axis',(-0.359909186701557,0.0183712220704353,0.932806451268141));
#86350=DIRECTION('',(0.372247514396375,0.,0.928133496877319));
#86351=DIRECTION('center_axis',(1.73014035762452E-14,-1.,-5.68072586656539E-14));
#86352=DIRECTION('ref_axis',(-4.14833769841157E-31,5.68072586656539E-14,
-1.));
#86353=DIRECTION('center_axis',(0.157639635048058,0.987363722095099,0.0162057320855101));
#86354=DIRECTION('ref_axis',(-0.21543524078911,0.018370881756947,0.976345311726138));
#86355=DIRECTION('center_axis',(-0.156429986875914,0.987363722026089,-0.0253483654855673));
#86356=DIRECTION('ref_axis',(-0.287973013507099,-0.0210448339910764,0.957407258408838));
#86357=DIRECTION('',(0.928133496571451,0.,-0.372247515159002));
#86358=DIRECTION('center_axis',(-0.141275528519,-0.987363722023162,-0.0717920989680929));
#86359=DIRECTION('ref_axis',(-0.552020522473789,0.0183712225113625,0.8336281190982));
#86360=DIRECTION('',(0.164023306625657,0.,0.98645646375478));
#86361=DIRECTION('center_axis',(1.45543938869861E-14,-1.,-2.58799230889811E-14));
#86362=DIRECTION('ref_axis',(3.67946996634454E-31,2.58799230889811E-14,
-1.));
#86363=DIRECTION('center_axis',(0.150470353914268,0.987363722120268,0.0497147144588495));
#86364=DIRECTION('ref_axis',(-0.420283866394558,0.0183708800064232,0.907206692224121));
#86365=DIRECTION('center_axis',(-0.147323591242544,0.987363722045255,-0.0583835580650956));
#86366=DIRECTION('ref_axis',(-0.487054623391906,-0.021044833616294,0.873117923771257));
#86367=DIRECTION('',(0.98645646307743,0.,-0.164023310699326));
#86368=DIRECTION('center_axis',(-0.122539408226903,-0.987363722003608,-0.100483699685982));
#86369=DIRECTION('ref_axis',(-0.718319992977518,0.018371225795244,0.695470262305699));
#86370=DIRECTION('',(-0.0518704469154818,0.,0.998653822271155));
#86371=DIRECTION('center_axis',(1.97775386860055E-14,-1.,-2.21461003884614E-14));
#86372=DIRECTION('ref_axis',(-1.13301816167624E-30,2.21461003884614E-14,
-1.));
#86373=DIRECTION('center_axis',(0.136265247913238,0.987363722105047,0.0808990882644076));
#86374=DIRECTION('ref_axis',(-0.605480484557487,0.018370882320908,0.795648096524325));
#86375=DIRECTION('center_axis',(-0.131328506624462,0.987363722081932,-0.0886888023614173));
#86376=DIRECTION('ref_axis',(-0.66336210148133,-0.0210448308065385,0.748002565112312));
#86377=DIRECTION('',(0.998653822462692,0.,0.0518704432278523));
#86378=DIRECTION('center_axis',(-0.0980734813275416,-0.987363721991955,
-0.124476796048459));
#86379=DIRECTION('ref_axis',(-0.851031619179291,0.0183712277123154,0.524792988853144));
#86380=DIRECTION('',(-0.265338796268726,0.,0.964155238120223));
#86381=DIRECTION('center_axis',(0.,-1.,0.));
#86382=DIRECTION('ref_axis',(0.,0.,-1.));
#86383=DIRECTION('center_axis',(0.115688529441642,0.987363722089161,0.108300713099541));
#86384=DIRECTION('ref_axis',(-0.762365509257207,0.0183708822016604,0.64688587941161));
#86385=DIRECTION('center_axis',(-0.109192647626212,0.987363722133983,-0.114847054459851));
#86386=DIRECTION('ref_axis',(-0.808651505534936,-0.0210448304026786,0.587911436960877));
#86387=DIRECTION('',(0.964155239073708,0.,0.26533879280407));
#86388=DIRECTION('center_axis',(-0.0690217373890758,-0.987363722105139,
-0.142649500659764));
#86389=DIRECTION('ref_axis',(-0.943949953433183,0.0183712184221452,0.329576976967713));
#86390=DIRECTION('',(-0.466400199211432,0.,0.884573826300291));
#86391=DIRECTION('center_axis',(8.17455424435588E-14,-1.,-3.53846501850613E-14));
#86392=DIRECTION('ref_axis',(1.,8.17455424435588E-14,-6.2833906170899E-31));
#86393=DIRECTION('center_axis',(0.0897023381817425,0.987363722254612,0.130638319417566));
#86394=DIRECTION('ref_axis',(-0.883603169697384,0.0183708757720218,0.46787599791409));
#86395=DIRECTION('center_axis',(-0.0819510660883673,0.987363722030276,-0.135635184172474));
#86396=DIRECTION('ref_axis',(-0.916129262541471,-0.0210448342814313,0.400330225270697));
#86397=DIRECTION('',(0.884573827309106,0.,0.466400197298114));
#86398=DIRECTION('center_axis',(-0.0367426329069288,-0.987363721970691,
-0.154152066036269));
#86399=DIRECTION('ref_axis',(-0.992730235309415,0.0183712295096434,0.118950316640258));
#86400=DIRECTION('',(-0.645653245721451,0.,0.763630726391595));
#86401=DIRECTION('center_axis',(2.91470103242875E-14,-1.,-5.6615004967518E-15));
#86402=DIRECTION('ref_axis',(1.,2.91470103242875E-14,2.0698037467484E-32));
#86403=DIRECTION('center_axis',(0.0595217788484243,0.987363722020597,0.146867417354402));
#86404=DIRECTION('ref_axis',(-0.963524527467881,0.0183708844563654,0.266988755516199));
#86405=DIRECTION('center_axis',(-0.0508775378651978,0.987363722085364,-0.150081166208527));
#86406=DIRECTION('ref_axis',(-0.980769834430407,-0.0210448317193077,0.194030015536922));
#86407=DIRECTION('',(0.763630725504702,0.,0.645653246770403));
#86408=DIRECTION('center_axis',(-0.00274546586929473,-0.987363722062483,
-0.158446655919526));
#86409=DIRECTION('ref_axis',(-0.995091555744463,0.0183712228409193,-0.0972383353281675));
#86410=DIRECTION('',(-0.794716264791645,0.,0.606981102239283));
#86411=DIRECTION('center_axis',(2.9682624687141E-14,-1.,7.36607880923249E-16));
#86412=DIRECTION('ref_axis',(-0.999692221971624,-2.96917631589623E-14,-0.0248084930908046));
#86413=DIRECTION('center_axis',(0.026558039131714,0.98736372202967,0.15622916173748));
#86414=DIRECTION('ref_axis',(-0.998392549720632,0.0183708840716378,0.0536174158344317));
#86415=DIRECTION('center_axis',(-0.0174250346579384,0.987363722105934,-0.157509518557722));
#86416=DIRECTION('ref_axis',(-0.999550698583589,-0.0210448314459766,-0.0213428215208139));
#86417=DIRECTION('',(0.606981102892691,0.,0.794716264292592));
#86418=DIRECTION('center_axis',(0.0313800669307913,-0.987363722011099,-0.155332455899623));
#86419=DIRECTION('ref_axis',(-0.950923500765827,0.0183712248308667,-0.308880225636862));
#86420=DIRECTION('',(-0.90661923571427,0.,0.4219497143415));
#86421=DIRECTION('center_axis',(5.76606249419919E-14,-1.,1.42005465698906E-14));
#86422=DIRECTION('ref_axis',(1.,5.76606249419919E-14,6.7939237826861E-31));
#86423=DIRECTION('center_axis',(-0.00764752810225059,0.987363722126267,
0.158285803352323));
#86424=DIRECTION('ref_axis',(-0.986576846474386,0.0183708803886285,-0.162261014277621));
#86425=DIRECTION('center_axis',(0.0168422438111064,0.987363722105163,-0.157572900887325));
#86426=DIRECTION('ref_axis',(-0.971593683228542,-0.021044830978553,-0.235717690892048));
#86427=DIRECTION('',(0.421949717449873,-2.49350828777751E-15,0.906619234267602));
#86428=DIRECTION('center_axis',(0.0640383063061008,-0.987363722036451,-0.144955081772845));
#86429=DIRECTION('ref_axis',(-0.862291320331763,0.0183712229205566,-0.506079220131501));
#86430=DIRECTION('',(-0.976129697219472,0.,0.217188430184996));
#86431=DIRECTION('center_axis',(1.33149634599131E-13,-1.,6.56596890341522E-14));
#86432=DIRECTION('ref_axis',(1.,1.33149634599131E-13,-2.52920306949116E-30));
#86433=DIRECTION('center_axis',(-0.041495503895507,0.98736372218836,0.152941175825237));
#86434=DIRECTION('ref_axis',(-0.928629905547145,0.0183708786055248,-0.370552303113557));
#86435=DIRECTION('center_axis',(0.0503220003050336,0.987363722191509,-0.150268347916085));
#86436=DIRECTION('ref_axis',(-0.898206026753204,-0.0210448277626684,-0.439070664846402));
#86437=DIRECTION('',(0.217188431596517,0.,0.976129696905409));
#86438=DIRECTION('center_axis',(0.0937021797661748,-0.987363721991622,-0.127799773090246));
#86439=DIRECTION('ref_axis',(-0.733339355073252,0.018371228609779,-0.679614514456625));
#86440=DIRECTION('',(-0.99999741978848,0.,0.00227165498764559));
#86441=DIRECTION('center_axis',(6.95530666805971E-14,-1.,5.5648702500083E-14));
#86442=DIRECTION('ref_axis',(1.,6.95530666805971E-14,-2.69781625273742E-30));
#86443=DIRECTION('center_axis',(-0.0734031933831537,0.98736372216877,0.140445189829294));
#86444=DIRECTION('ref_axis',(-0.827261262436935,0.018370879413501,-0.561516976110984));
#86445=DIRECTION('center_axis',(0.0814487490481949,0.987363722058279,-0.135937418107396));
#86446=DIRECTION('ref_axis',(-0.782819254446178,-0.0210448328580041,-0.62189318204842));
#86447=DIRECTION('',(0.00227165580984504,0.,0.999997419786612));
#86448=DIRECTION('center_axis',(0.118984650603525,-0.987363722022246,-0.104668683736512));
#86449=DIRECTION('ref_axis',(-0.570097257187399,0.0183712249409984,-0.82137178880308));
#86450=DIRECTION('',(-0.97710637405149,0.,-0.212751342623141));
#86451=DIRECTION('center_axis',(5.5964128605694E-14,-1.,6.92995201892614E-14));
#86452=DIRECTION('ref_axis',(1.46790450287485E-30,-6.92995201892614E-14,
-1.));
#86453=DIRECTION('center_axis',(-0.101878629409016,0.987363722040531,0.121382145589907));
#86454=DIRECTION('ref_axis',(-0.687210802807775,0.0183708831942544,-0.726225738427767));
#86455=DIRECTION('center_axis',(0.108767048569711,0.987363722075025,-0.115250203798458));
#86456=DIRECTION('ref_axis',(-0.630828724288943,-0.0210448335494104,-0.775636664678032));
#86457=DIRECTION('',(-0.21275134122214,0.,0.977106374356539));
#86458=DIRECTION('center_axis',(0.138703528583435,-0.987363722005588,-0.0766434056248631));
#86459=DIRECTION('ref_axis',(-0.380198045567245,0.0183712251232356,-0.924722630973374));
#86460=DIRECTION('',(-0.908526921025632,0.,-0.417826320104041));
#86461=DIRECTION('center_axis',(1.32527900101837E-14,-1.,2.65699897642818E-14));
#86462=DIRECTION('ref_axis',(-3.85703025017377E-31,-2.65699897642817E-14,
-1.));
#86463=DIRECTION('center_axis',(-0.125590338476727,0.987363722139054,0.0966434016630939));
#86464=DIRECTION('ref_axis',(-0.515027128630378,0.018370879941791,-0.856976993591375));
#86465=DIRECTION('center_axis',(0.130999522454367,0.987363722018216,-0.0891740184081779));
#86466=DIRECTION('ref_axis',(-0.449341343911688,-0.0210448341519091,-0.893112239087091));
#86467=DIRECTION('',(-0.41782632044881,0.,0.908526920867075));
#86468=DIRECTION('center_axis',(0.151936783382105,-0.987363721993645,-0.0450343685017907));
#86469=DIRECTION('ref_axis',(-0.172521198272612,0.0183712264494477,-0.984834470449387));
#86470=DIRECTION('',(-0.797465757841021,0.,-0.603364205990914));
#86471=DIRECTION('center_axis',(7.23118474322659E-15,-1.,2.87977562494652E-14));
#86472=DIRECTION('ref_axis',(9.73713914984225E-33,-2.87977562494652E-14,
-1.));
#86473=DIRECTION('center_axis',(-0.143429581007702,0.987363722192312,0.0673857209688961));
#86474=DIRECTION('ref_axis',(-0.318761360374116,0.0183708783634438,-0.947656955844571));
#86475=DIRECTION('center_axis',(0.147106605348864,0.987363722149102,-0.0589281498657818));
#86476=DIRECTION('ref_axis',(-0.246843263567107,-0.0210448291783784,-0.968826877412261));
#86477=DIRECTION('',(-0.603364203506953,0.,0.797465759720391));
#86478=DIRECTION('',(-0.649115982975384,0.,-0.760689450857511));
#86479=DIRECTION('',(-0.760689450324139,0.,0.649115983600434));
#86480=DIRECTION('center_axis',(0.15680352997555,-0.987363722031627,0.0229245153287668));
#86481=DIRECTION('ref_axis',(0.256945263434263,0.0183712248304825,-0.966251328432166));
#86482=DIRECTION('',(-0.470414265591835,0.,-0.882445702991235));
#86483=DIRECTION('center_axis',(-3.31741108596706E-14,-1.,1.75034588439747E-13));
#86484=DIRECTION('ref_axis',(1.88543075864206E-30,-1.75034588439748E-13,
-1.));
#86485=DIRECTION('center_axis',(-0.158467693351964,0.987363721969067,0.000933114729498503));
#86486=DIRECTION('ref_axis',(0.108610850412292,0.0183708869075653,-0.99391458067932));
#86487=DIRECTION('center_axis',(0.158253627755301,0.987363722053648,0.00828671675958859));
#86488=DIRECTION('ref_axis',(0.182770968834695,-0.0210448325953407,-0.982930255904386));
#86489=DIRECTION('',(-0.882445701968546,0.,0.470414267510287));
#86490=DIRECTION('center_axis',(0.148209457615993,-0.98736372200383,0.0560966767635802));
#86491=DIRECTION('ref_axis',(0.458653501977566,0.0183712253838114,-0.888425271591039));
#86492=DIRECTION('',(-0.269716499743633,0.,-0.962939774734663));
#86493=DIRECTION('center_axis',(1.16709635174659E-14,-1.,-2.73018206340956E-14));
#86494=DIRECTION('ref_axis',(-1.0314733824329E-31,2.73018206340956E-14,
-1.));
#86495=DIRECTION('center_axis',(-0.154963396044541,0.987363722152497,-0.0331545783189781));
#86496=DIRECTION('ref_axis',(0.31973384434166,0.0183708788110592,-0.94732928783724));
#86497=DIRECTION('center_axis',(0.152772346968418,0.987363722044585,0.0421128293044433));
#86498=DIRECTION('ref_axis',(0.389798836580696,-0.0210448335722502,-0.920659536408683));
#86499=DIRECTION('',(-0.962939774722175,0.,0.269716499788217));
#86500=DIRECTION('center_axis',(0.132685277493759,-0.987363721998059,0.0866458170862475));
#86501=DIRECTION('ref_axis',(0.638915607237054,0.0183712283842684,-0.769057439205005));
#86502=DIRECTION('',(-0.0564070903287917,0.,-0.99840785261367));
#86503=DIRECTION('center_axis',(1.72671872884761E-14,-1.,-2.41546070876787E-14));
#86504=DIRECTION('ref_axis',(2.74088008315019E-31,2.41546070876787E-14,
-1.));
#86505=DIRECTION('center_axis',(-0.144213188967013,0.987363721902049,-0.0656919842880165));
#86506=DIRECTION('ref_axis',(0.515906438873904,0.0183708884535525,-0.856447929991003));
#86507=DIRECTION('center_axis',(0.140147600266339,0.987363722073609,0.0739697943253586));
#86508=DIRECTION('ref_axis',(0.578600140813818,-0.0210448321666288,-0.815339801609923));
#86509=DIRECTION('',(-0.998407852567306,0.,0.0564070911494373));
#86510=DIRECTION('center_axis',(0.110956879050134,-0.987363721968771,0.113143499731222));
#86511=DIRECTION('ref_axis',(0.789302732667269,0.0183712271502386,-0.613729333026356));
#86512=DIRECTION('',(0.159539850457337,0.,-0.987191489082058));
#86513=DIRECTION('center_axis',(-2.20560165650436E-14,-1.,1.98779509493039E-14));
#86514=DIRECTION('ref_axis',(1.,-2.20560165650436E-14,-6.51911231040562E-31));
#86515=DIRECTION('center_axis',(-0.126719727502218,0.987363722008613,-0.0951577170967375));
#86516=DIRECTION('ref_axis',(0.687955821391077,0.0183708850872274,-0.725520019293224));
#86517=DIRECTION('center_axis',(0.12096970734739,0.987363722095569,0.102368013528986));
#86518=DIRECTION('ref_axis',(0.740346747930026,-0.0210448314755895,-0.671895682303137));
#86519=DIRECTION('',(-0.987191489212964,0.,-0.159539849647322));
#86520=DIRECTION('center_axis',(0.0840402580818046,-0.98736372204253,0.13435071795813));
#86521=DIRECTION('ref_axis',(0.902782938705594,0.0183712241368421,-0.429703925634623));
#86522=DIRECTION('',(0.368026888566917,0.,-0.929815147914764));
#86523=DIRECTION('center_axis',(0.,-1.,0.));
#86524=DIRECTION('ref_axis',(0.,0.,-1.));
#86525=DIRECTION('center_axis',(-0.103300989412016,0.987363722147504,-0.120173981266849));
#86526=DIRECTION('ref_axis',(0.827837155414535,0.0183708794019659,-0.560667597516718));
#86527=DIRECTION('center_axis',(0.0961354049611609,0.987363722122848,0.125979617989056));
#86528=DIRECTION('ref_axis',(0.867475562994424,-0.0210448304182839,-0.497034468342159));
#86529=DIRECTION('',(-0.929815148606724,0.,-0.368026886818689));
#86530=DIRECTION('center_axis',(0.053194013979902,-0.987363721990877,0.149275843233354));
#86531=DIRECTION('ref_axis',(0.974050017223779,0.0183712276662062,-0.225586041102707));
#86532=DIRECTION('',(0.559305393715518,0.,-0.828961685821926));
#86533=DIRECTION('center_axis',(-8.5092100362368E-14,-1.,2.63389760788361E-14));
#86534=DIRECTION('ref_axis',(1.,-8.5092100362368E-14,-6.58426787095862E-31));
#86535=DIRECTION('center_axis',(-0.0750520182169393,0.98736372208175,-0.139571038824097));
#86536=DIRECTION('ref_axis',(0.929009743068865,0.0183708817694427,-0.369598982663825));
#86537=DIRECTION('center_axis',(0.0668059196099684,0.987363722094998,0.143700554611937));
#86538=DIRECTION('ref_axis',(0.954042184755361,-0.0210448313464778,-0.298932475286338));
#86539=DIRECTION('',(-0.828961684948636,0.,-0.559305395009845));
#86540=DIRECTION('center_axis',(0.0198604736064091,-0.987363721987085,0.157220997617807));
#86541=DIRECTION('ref_axis',(0.99977159965937,0.0183712272039706,-0.0109200057492469));
#86542=DIRECTION('',(0.724431404105314,0.,-0.689346894347108));
#86543=DIRECTION('center_axis',(8.87647956210514E-14,-1.,-7.43089918185425E-15));
#86544=DIRECTION('ref_axis',(1.,8.87647956210513E-14,-3.94182071300882E-31));
#86545=DIRECTION('center_axis',(-0.0432936985365139,0.98736372200008,-0.152441910723981));
#86546=DIRECTION('ref_axis',(0.986742867208569,0.0183708839620664,-0.161248332194369));
#86547=DIRECTION('center_axis',(0.0343526625781289,0.987363722125914,0.154702213311425));
#86548=DIRECTION('ref_axis',(0.995998854493829,-0.0210448311515057,-0.0868527312684218));
#86549=DIRECTION('',(-0.689346896451424,0.,-0.724431402102911));
#86550=DIRECTION('center_axis',(-0.014401724422129,-0.987363722031899,0.157814672160051));
#86551=DIRECTION('ref_axis',(0.978744973309671,0.0183712233283643,0.204256640955612));
#86552=DIRECTION('',(0.855683805531922,0.,-0.517499009612973));
#86553=DIRECTION('center_axis',(2.94289825351575E-14,-1.,3.94154609637067E-15));
#86554=DIRECTION('ref_axis',(1.,2.94289825351575E-14,-2.14150802636011E-31));
#86555=DIRECTION('center_axis',(-0.00951100661057945,0.987363722136511,
-0.158184768426005));
#86556=DIRECTION('ref_axis',(0.998336992161528,0.0183708797645671,0.0546421161609756));
#86557=DIRECTION('center_axis',(0.000293112974508184,0.987363722118915,
0.158470168575244));
#86558=DIRECTION('ref_axis',(0.991383724636723,-0.0210448306235249,0.129288149609488));
#86559=DIRECTION('',(-0.517499010316405,0.,-0.855683805106501));
#86560=DIRECTION('center_axis',(-0.0479905100827411,-0.987363722040683,
0.151029107591772));
#86561=DIRECTION('ref_axis',(0.911953320089083,0.0183712227089235,0.409882471148349));
#86562=DIRECTION('',(0.946925383165727,0.,-0.321453447199499));
#86563=DIRECTION('center_axis',(2.78936333747509E-14,-1.,1.01757562670739E-14));
#86564=DIRECTION('ref_axis',(1.,2.78936333747509E-14,-2.28033888729291E-31));
#86565=DIRECTION('center_axis',(0.0247164011025826,0.987363722070318,-0.156531082715173));
#86566=DIRECTION('ref_axis',(0.963249988847597,0.0183708832253758,0.267977554348538));
#86567=DIRECTION('center_axis',(-0.0337801386902987,0.987363722008994,0.154828236089577));
#86568=DIRECTION('ref_axis',(0.940412594373351,-0.0210448336306716,0.339383658005864));
#86569=DIRECTION('',(-0.321453447977455,0.,-0.946925382901634));
#86570=DIRECTION('center_axis',(-0.0793353132184248,-0.987363722067417,
0.137181589222863));
#86571=DIRECTION('ref_axis',(0.802519742299411,0.018371221794083,0.596342654377062));
#86572=DIRECTION('',(0.993889783075419,0.,-0.110377076869685));
#86573=DIRECTION('center_axis',(-7.51620268031192E-14,-1.,-4.78024781847107E-14));
#86574=DIRECTION('ref_axis',(1.,-7.51620268031192E-14,4.45701823373997E-31));
#86575=DIRECTION('center_axis',(0.057788096969252,0.987363721938313,-0.147558179877612));
#86576=DIRECTION('ref_axis',(0.883122486736232,0.0183708880663981,0.468782661680726));
#86577=DIRECTION('center_axis',(-0.0662738728966525,0.987363722051591,0.143946705928643));
#86578=DIRECTION('ref_axis',(0.845468815551909,-0.0210448325433083,0.53360996706628));
#86579=DIRECTION('',(-0.110377077686295,0.,-0.99388978298473));
#86580=DIRECTION('center_axis',(-0.106970483905427,-0.987363722071512,0.116919613025908));
#86581=DIRECTION('ref_axis',(0.655561234390894,0.0183712221816143,0.754918516238303));
#86582=DIRECTION('',(0.994381001052632,0.,0.105860402160414));
#86583=DIRECTION('center_axis',(-4.20857737396286E-14,-1.,-4.18949978672253E-14));
#86584=DIRECTION('ref_axis',(1.,-4.20857737396286E-14,4.26600455538985E-31));
#86585=DIRECTION('center_axis',(0.0881576982960553,0.987363722200972,-0.131685611638414));
#86586=DIRECTION('ref_axis',(0.761701158200427,0.0183708771844214,0.647668014084069));
#86587=DIRECTION('center_axis',(-0.0956687127568795,0.987363722041466,0.126334388809476));
#86588=DIRECTION('ref_axis',(0.710991853905636,-0.0210448335406359,0.702885267067872));
#86589=DIRECTION('',(0.105860401342926,0.,-0.994381001139661));
#86590=DIRECTION('center_axis',(-0.129603830352234,-0.987363721976718,0.0911906118101647));
#86591=DIRECTION('ref_axis',(0.477949413275875,0.0183712293018593,0.878195226748122));
#86592=DIRECTION('',(0.948376068001928,0.,0.317147968054664));
#86593=DIRECTION('center_axis',(0.,-1.,0.));
#86594=DIRECTION('ref_axis',(0.,0.,-1.));
#86595=DIRECTION('center_axis',(0.114405130916887,0.987363722064272,-0.109655580666363));
#86596=DIRECTION('ref_axis',(0.60466353119606,0.0183708827655051,0.79626912831525));
#86597=DIRECTION('center_axis',(-0.120590190775855,0.987363722103883,0.102814814894587));
#86598=DIRECTION('ref_axis',(0.543269704745646,-0.0210448326431497,0.839294431605858));
#86599=DIRECTION('',(0.317147963824605,0.,-0.948376069416509));
#86600=DIRECTION('center_axis',(-0.14617705182175,-0.987363722017283,0.0611976303861404));
#86601=DIRECTION('ref_axis',(0.277989205306797,0.0183712262658596,0.960408506719086));
#86602=DIRECTION('',(0.85802612362603,0.,0.513606046669321));
#86603=DIRECTION('center_axis',(-4.12095214699751E-14,-1.,-1.11388455919924E-13));
#86604=DIRECTION('ref_axis',(7.91583898807535E-31,1.11388455919924E-13,
-1.));
#86605=DIRECTION('center_axis',(0.135303109888205,0.987363721994031,-0.0824981754020864));
#86606=DIRECTION('ref_axis',(0.419352507557114,0.0183708858640293,0.907637584588767));
#86607=DIRECTION('center_axis',(-0.139873004629083,0.987363722041037,0.0744877370666017));
#86608=DIRECTION('ref_axis',(0.35014486756981,-0.0210448345286272,0.936459121720848));
#86609=DIRECTION('',(0.513606044697418,0.,-0.858026124806392));
#86610=DIRECTION('center_axis',(-0.155915195768687,-0.987363722021331,0.028343114941639));
#86611=DIRECTION('ref_axis',(0.0650305337710549,0.0183712223399492,0.997714151381641));
#86612=DIRECTION('',(0.727555834386069,0.,0.686048473397318));
#86613=DIRECTION('center_axis',(0.,-1.,0.));
#86614=DIRECTION('ref_axis',(0.,0.,-1.));
#86615=DIRECTION('center_axis',(0.14987446749451,0.987363722004551,-0.0514832444835786));
#86616=DIRECTION('ref_axis',(0.214433030125156,0.0183708851604601,0.976565914912949));
#86617=DIRECTION('center_axis',(-0.152615514008743,0.987363722134678,0.0426776885058355));
#86618=DIRECTION('ref_axis',(0.140647645910758,-0.0210448290467592,0.989836024233385));
#86619=DIRECTION('center_axis',(-2.34251248529641E-15,-1.,2.95992134304517E-14));
#86620=DIRECTION('ref_axis',(1.57742281693884E-32,-2.95992134304517E-14,
-1.));
#86621=DIRECTION('center_axis',(0.157437861538929,0.987363721967134,-0.0180610159530712));
#86622=DIRECTION('ref_axis',(-0.000513102483762423,0.0183708870102229,0.999831109356125));
#86623=DIRECTION('center_axis',(-0.158221889080688,0.987363722241387,0.00887208078028815));
#86624=DIRECTION('ref_axis',(-0.0754261047720061,-0.0210448262853796,0.996929294386287));
#86625=DIRECTION('',(0.686048471277825,0.,-0.727555836384645));
#86626=DIRECTION('center_axis',(0.163393692715905,-0.986495109888097,0.0113973394935624));
#86627=DIRECTION('ref_axis',(0.0258341094970031,0.0158269796852664,0.999540947385618));
#86628=DIRECTION('center_axis',(-0.1596841371995,-0.986495109005799,0.0364468960885218));
#86629=DIRECTION('ref_axis',(0.139259431844732,0.0140402165467154,0.99015639318322));
#86630=DIRECTION('center_axis',(0.162023729773524,-0.986495109914706,-0.0239939389148123));
#86631=DIRECTION('ref_axis',(0.240101877481402,0.0158269783313953,0.970618666205634));
#86632=DIRECTION('center_axis',(-0.148115806239777,-0.986495109048686,0.0699221550366034));
#86633=DIRECTION('ref_axis',(0.348857978478882,0.0140402144241546,0.937070425971576));
#86634=DIRECTION('center_axis',(0.15307771473187,-0.986495110034312,-0.0582632914523267));
#86635=DIRECTION('ref_axis',(0.443142750284692,0.0158269724739011,0.896311335314035));
#86636=DIRECTION('center_axis',(-0.129621746388249,-0.986495109054191,0.100127931544702));
#86637=DIRECTION('ref_axis',(0.542144315518207,0.0140402112031747,0.840168086528324));
#86638=DIRECTION('center_axis',(0.136973958783133,-0.986495109992773,-0.0898083101701765));
#86639=DIRECTION('ref_axis',(0.625462761400192,0.0158269746406774,0.780093482202851));
#86640=DIRECTION('center_axis',(-0.105066715113658,-0.986495109010335,0.125651841506255));
#86641=DIRECTION('ref_axis',(0.710080586202779,0.0140402132056087,0.703980421255491));
#86642=DIRECTION('center_axis',(0.114465449777524,-0.986495110036968,-0.117153995580092));
#86643=DIRECTION('ref_axis',(0.778536828715126,0.0158269720084483,0.627399325223767));
#86644=DIRECTION('center_axis',(-0.0755988798103096,-0.986495109009909,
0.145300410429407));
#86645=DIRECTION('ref_axis',(0.844814278286775,0.014040215547775,0.534875413110537));
#86646=DIRECTION('center_axis',(0.0866046692179544,-0.986495109923494,-0.139021686677592));
#86647=DIRECTION('ref_axis',(0.89520737956913,0.0158269765333149,0.445368672426323));
#86648=DIRECTION('center_axis',(-0.0425961353136749,-0.986495109055382,
0.158154889479112));
#86649=DIRECTION('ref_axis',(0.940045392205716,0.0140402069799854,0.340760228284876));
#86650=DIRECTION('center_axis',(0.0546943469278652,-0.98649510991499,-0.154388880842975));
#86651=DIRECTION('ref_axis',(0.970019027659476,0.015826976159292,0.242513077594213));
#86652=DIRECTION('center_axis',(-0.00760162579462577,-0.986495109024877,
0.163614226628601));
#86653=DIRECTION('ref_axis',(0.991321029569393,0.0140402163257876,0.13071147103068));
#86654=DIRECTION('center_axis',(0.0202265769071983,-0.986495109950068,-0.162537022340207));
#86655=DIRECTION('ref_axis',(0.999473664960509,0.0158269756080494,0.0283178370203542));
#86656=DIRECTION('center_axis',(0.0277483150287501,-0.986495109025233,0.161423142338262));
#86657=DIRECTION('ref_axis',(0.996243597198247,0.0140402127555468,-0.0854492098692269));
#86658=DIRECTION('center_axis',(-0.015186968293509,-0.986495110040764,-0.163085112317813));
#86659=DIRECTION('ref_axis',(0.982194024074973,0.0158269715953397,-0.187201511856963));
#86660=DIRECTION('center_axis',(0.0618007766378345,-0.986495109035607,0.151684092296411));
#86661=DIRECTION('ref_axis',(0.954582921692536,0.0140402106311878,-0.297614378178163));
#86662=DIRECTION('center_axis',(-0.0498903763927462,-0.986495109833052,
-0.156007527442959));
#86663=DIRECTION('ref_axis',(0.918988082572133,0.0158269797608328,-0.393967525060181));
#86664=DIRECTION('center_axis',(0.0929635057152368,-0.986495109045637,0.134852461728253));
#86665=DIRECTION('ref_axis',(0.868287009737066,0.0140402117084069,-0.495863429965397));
#86666=DIRECTION('center_axis',(-0.0822609770536424,-0.986495109954466,
-0.141635199333024));
#86667=DIRECTION('ref_axis',(0.8128112796066,0.0158269756738695,-0.582312056019194));
#86668=DIRECTION('center_axis',(0.119779364423865,-0.986495109030295,0.11171527969585));
#86669=DIRECTION('ref_axis',(0.741390961601542,0.014040212596467,-0.670926459819395));
#86670=DIRECTION('center_axis',(-0.110785145530173,-0.986495110071091,-0.120640164686907));
#86671=DIRECTION('ref_axis',(0.668628322217801,0.0158269710235375,-0.743428324531981));
#86672=DIRECTION('center_axis',(0.140994470581036,-0.986495109053583,0.0833544184727661));
#86673=DIRECTION('ref_axis',(0.579828297438555,0.0140402095968446,-0.81461771279784));
#86674=DIRECTION('center_axis',(-0.134129119682768,-0.986495110072653,-0.0940041331850318));
#86675=DIRECTION('ref_axis',(0.493181049503002,0.0158269710266419,-0.869782708151432));
#86676=DIRECTION('center_axis',(0.155616836747567,-0.986495109020785,0.051095988088611));
#86677=DIRECTION('ref_axis',(0.391153502999558,0.0140402166268495,-0.920218348767425));
#86678=DIRECTION('center_axis',(-0.151201364507911,-0.986495110021318,-0.0629725755783759));
#86679=DIRECTION('ref_axis',(0.294673181296257,0.0158269734645186,-0.955467018340087));
#86680=DIRECTION('center_axis',(0.162962728442398,-0.986495108997506,0.0164483756829379));
#86681=DIRECTION('ref_axis',(0.184188810225888,0.0140402136861454,-0.982790595491847));
#86682=DIRECTION('center_axis',(-0.161203602974457,-0.986495109981873,-0.0289964889237524));
#86683=DIRECTION('ref_axis',(0.0823867191797638,0.0158269747516762,-0.996474754006846));
#86684=DIRECTION('center_axis',(0.16268866488224,-0.986495109019677,-0.0189683472946162));
#86685=DIRECTION('ref_axis',(-0.031388350063932,0.0140402130897802,-0.999408647099202));
#86686=DIRECTION('center_axis',(-0.163668140770209,-0.986495109923555,0.00633543950610209));
#86687=DIRECTION('ref_axis',(-0.133752052438717,0.0158269775873577,-0.990888437337362));
#86688=DIRECTION('center_axis',(0.154807460333412,-0.986495109016584,-0.05349813185034));
#86689=DIRECTION('ref_axis',(-0.245497824500102,0.0140402131910535,-0.969295460929879));
#86690=DIRECTION('center_axis',(-0.158479740056268,-0.986495109801126,0.0413711291864477));
#86691=DIRECTION('ref_axis',(-0.343636726738424,0.0158269814347735,-0.938969278887848));
#86692=DIRECTION('center_axis',(0.139687631289941,-0.986495109047706,-0.0855264022951965));
#86693=DIRECTION('ref_axis',(-0.448128094060664,0.0140402122128746,-0.893859096141318));
#86694=DIRECTION('center_axis',(-0.145880998923126,-0.986495109926484,0.0744723589281599));
#86695=DIRECTION('ref_axis',(-0.537453330319667,0.0158269761416644,-0.843144960581815));
#86696=DIRECTION('center_axis',(0.118036163879493,-0.986495109044257,-0.113555554018166));
#86697=DIRECTION('ref_axis',(-0.629804389132666,0.0140402125730394,-0.776626875571618));
#86698=DIRECTION('center_axis',(-0.126461025342854,-0.986495109956398,0.10409134018423));
#86699=DIRECTION('ref_axis',(-0.70613921349188,0.0158269745844066,-0.707896120941889));
#86700=DIRECTION('center_axis',(0.0908654531084785,-0.986495109005427,-0.136274976939132));
#86701=DIRECTION('ref_axis',(-0.782031736374587,0.0140402162115408,-0.623080440739141));
#86702=DIRECTION('center_axis',(-0.101127876712809,-0.986495109938006,0.128843124069392));
#86703=DIRECTION('ref_axis',(-0.841806811906979,0.0158269759318603,-0.539546845287655));
#86704=DIRECTION('center_axis',(0.0594459811192609,-0.986495109049417,-0.152622328478988));
#86705=DIRECTION('ref_axis',(-0.897692144812778,0.0140402125023846,-0.440399461369247));
#86706=DIRECTION('center_axis',(-0.0710661011877669,-0.986495109933049,
0.147570347089622));
#86707=DIRECTION('ref_axis',(-0.93811245894817,0.0158269770340597,-0.345968959827586));
#86708=DIRECTION('center_axis',(0.0252468774281873,-0.986495109027206,-0.161833232203796));
#86709=DIRECTION('ref_axis',(-0.971377467360531,0.0140402131190302,-0.237125891289441));
#86710=DIRECTION('center_axis',(-0.0376813519130728,-0.986495109949852,
0.159397345533208));
#86711=DIRECTION('ref_axis',(-0.990553010817809,0.0158269764618599,-0.13621394780216));
#86712=DIRECTION('center_axis',(-0.0101327460188599,-0.986495108992418,
-0.163476993464387));
#86713=DIRECTION('ref_axis',(-0.99964225913962,0.0140402175746079,-0.0227645784651067));
#86714=DIRECTION('center_axis',(-0.0025346599444412,-0.98649511006807,0.163771100352759));
#86715=DIRECTION('ref_axis',(-0.99667640424643,0.0158269710860104,0.0799102759640404));
#86716=DIRECTION('center_axis',(-0.0450385678145862,-0.986495108996407,
-0.157476751729825));
#86717=DIRECTION('ref_axis',(-0.981164889711611,0.0140402156784061,0.192661183274957));
#86718=DIRECTION('center_axis',(0.0327305405511363,-0.986495109972786,0.160487101397622));
#86719=DIRECTION('ref_axis',(-0.956196316558089,0.0158269753346832,0.292297983319246));
#86720=DIRECTION('center_axis',(-0.0778384347764789,-0.986495109011886,
-0.144113073547044));
#86721=DIRECTION('ref_axis',(-0.916809341545154,0.0140402127225352,0.399078317730051));
#86722=DIRECTION('center_axis',(0.0664652972180809,-0.986495109850739,0.149698906162638));
#86723=DIRECTION('ref_axis',(-0.871005552933621,0.0158269801331046,0.491018160009041));
#86724=DIRECTION('center_axis',(-0.106998668569342,-0.986495109004646,-0.124010825472212));
#86725=DIRECTION('ref_axis',(-0.809584805429825,0.0140402153031817,0.586834998250269));
#86726=DIRECTION('center_axis',(0.0970922175602582,-0.986495109914703,0.131910952553644));
#86727=DIRECTION('ref_axis',(-0.745087536041886,0.0158269772062907,0.66677887671067));
#86728=DIRECTION('center_axis',(-0.131155762220523,-0.98649510897064,-0.0981099689805202));
#86729=DIRECTION('ref_axis',(-0.664504985384022,0.0140402174317722,0.74715192343609));
#86730=DIRECTION('center_axis',(0.123179213512161,-0.986495110027753,0.107954987146756));
#86731=DIRECTION('ref_axis',(-0.584330053200728,0.0158269728669726,0.811361754001446));
#86732=DIRECTION('center_axis',(-0.149180154404103,-0.986495109054244,-0.0676216041219363));
#86733=DIRECTION('ref_axis',(-0.48835365175152,0.0140402134121568,0.872532855099621));
#86734=DIRECTION('center_axis',(0.143506481236003,-0.986495109925275,0.0789511743850581));
#86735=DIRECTION('ref_axis',(-0.396249950523607,0.0158269773943524,0.918006254606469));
#86736=DIRECTION('center_axis',(-0.160229052463089,-0.986495108976717,-0.0339713219023875));
#86737=DIRECTION('ref_axis',(-0.28936744084067,0.014040216551562,0.957115121863878));
#86738=DIRECTION('center_axis',(0.157123548865898,-0.986495109968347,0.0462556850595121));
#86739=DIRECTION('ref_axis',(-0.189641636534491,0.0158269742616208,0.981725805191165));
#86740=DIRECTION('center_axis',(-0.163785816046288,-0.986495109021849,0.0012674139114061));
#86741=DIRECTION('ref_axis',(-0.0768507322934788,0.0140402118077792,0.996943748362137));
#86742=DIRECTION('center_axis',(-0.163746589113265,0.986495109212932,0.00380184859464142));
#86743=DIRECTION('ref_axis',(-0.0762928037604484,-0.0165058445169965,0.996948827769585));
#86744=DIRECTION('center_axis',(0.163385855644741,0.986495983400253,0.0114340242435876));
#86745=DIRECTION('ref_axis',(-0.183100330941314,0.0189330377687653,0.982911902914004));
#86746=DIRECTION('center_axis',(-0.160735569747077,0.986495109243657,-0.031487712784955));
#86747=DIRECTION('ref_axis',(-0.288823649385265,-0.0165058446405764,0.957240020396389));
#86748=DIRECTION('center_axis',(0.157107995693868,0.98649598417733,0.0462898573237903));
#86749=DIRECTION('ref_axis',(-0.390116547996733,0.0189330090465228,0.920570812131015));
#86750=DIRECTION('center_axis',(-0.150208734751245,0.986495109188334,-0.0653049427832729));
#86751=DIRECTION('ref_axis',(-0.487849419977123,-0.0165058455838431,0.872771734469871));
#86752=DIRECTION('center_axis',(0.143483944818749,0.98649598426314,0.0789812041687666));
#86753=DIRECTION('ref_axis',(-0.57889135101082,0.0189330049272192,0.815184853299724));
#86754=DIRECTION('center_axis',(-0.132658304626714,0.986495109226924,-0.0960685884403693));
#86755=DIRECTION('ref_axis',(-0.664063896654305,-0.0165058442549272,0.747493610852783));
#86756=DIRECTION('center_axis',(0.123150816988761,0.986495981727044,0.107979416146764));
#86757=DIRECTION('ref_axis',(-0.740597844773079,0.0189330996251722,0.671681747597814));
#86758=DIRECTION('center_axis',(-0.108904925617282,0.986495109062018,-0.122340169090171));
#86759=DIRECTION('ref_axis',(-0.809227481863439,-0.0165058503434508,0.58726351793841));
#86760=DIRECTION('center_axis',(0.0970592346619194,0.986495982026364,0.131928702004838));
#86761=DIRECTION('ref_axis',(-0.867674800138622,0.0189330983424895,0.49677155614181));
#86762=DIRECTION('center_axis',(-0.0800592635376213,0.986495109206599,-0.142891265769723));
#86763=DIRECTION('ref_axis',(-0.916552489471739,-0.0165058442070702,0.399573636705639));
#86764=DIRECTION('center_axis',(0.0664292055707529,0.986495983699788,0.149709167359338));
#86765=DIRECTION('ref_axis',(-0.954180245093614,0.0189330269066743,0.298632885605793));
#86766=DIRECTION('center_axis',(-0.0474701296011309,0.98649510908173,-0.156760921640174));
#86767=DIRECTION('ref_axis',(-0.981020522367194,-0.0165058500441775,0.193200133562884));
#86768=DIRECTION('center_axis',(0.0326930102895807,0.986495985677644,0.160489368246307));
#86769=DIRECTION('ref_axis',(-0.996069284688432,0.018932952693861,0.0865304767267995));
#86770=DIRECTION('center_axis',(-0.0126613353093269,0.986495109225124,-0.163300612561913));
#86771=DIRECTION('ref_axis',(-0.999617125580531,-0.016505845105072,-0.0222071908057615));
#86772=DIRECTION('center_axis',(-0.00257165866145818,0.98649598158772,0.16376527373961));
#86773=DIRECTION('ref_axis',(-0.991383228009754,0.0189331052978054,-0.129618026310932));
#86774=DIRECTION('center_axis',(0.0227394843069944,0.986495109192044,-0.162204548005379));
#86775=DIRECTION('ref_axis',(-0.97147274280131,-0.0165058452943239,-0.236576133760823));
#86776=DIRECTION('center_axis',(-0.0377162304408249,0.986495981670314,0.159383700890832));
#86777=DIRECTION('ref_axis',(-0.940341195460543,0.0189331020324126,-0.339705716418294));
#86778=DIRECTION('center_axis',(0.0570770288022208,0.986495109144714,-0.153523979940172));
#86779=DIRECTION('ref_axis',(-0.897903374253699,-0.0165058476851046,-0.439883038427282));
#86780=DIRECTION('center_axis',(-0.0710972329446366,0.986495981748296,0.147549522066601));
#86781=DIRECTION('ref_axis',(-0.845329852427979,0.018933099101845,-0.53390914803222));
#86782=DIRECTION('center_axis',(0.088745716900431,0.986495109151901,-0.137664800697958));
#86783=DIRECTION('ref_axis',(-0.782349042285949,-0.0165058478410961,-0.622621500609563));
#86784=DIRECTION('center_axis',(-0.101153799510025,0.986495981517584,0.128816098739029));
#86785=DIRECTION('ref_axis',(-0.710791826200741,0.0189331070572685,-0.703147578580324));
#86786=DIRECTION('center_axis',(0.116264754633492,0.986495109150606,-0.115368567868151));
#86787=DIRECTION('ref_axis',(-0.63021293651818,-0.0165058475711234,-0.77624687544691));
#86788=DIRECTION('center_axis',(-0.126480538716153,0.986495981850945,0.104059363432665));
#86789=DIRECTION('ref_axis',(-0.543017961707908,0.0189330962803664,-0.839507612310828));
#86790=DIRECTION('center_axis',(0.138347381237138,0.986495109182418,-0.087677828805208));
#86791=DIRECTION('ref_axis',(-0.448608776393294,-0.0165058468718704,-0.893575806947544));
#86792=DIRECTION('center_axis',(-0.145893181782997,0.986495981861824,0.0744369349161404));
#86793=DIRECTION('ref_axis',(-0.349853182694279,0.0189330947671037,-0.936613201103435));
#86794=DIRECTION('center_axis',(0.153961037350114,0.986495109136802,-0.0558873744887531));
#86795=DIRECTION('ref_axis',(-0.246028168759599,-0.0165058488472811,-0.96912212704624));
#86796=DIRECTION('center_axis',(-0.158484017824289,0.986495981700585,0.0413339350034501));
#86797=DIRECTION('ref_axis',(-0.140329663760193,0.0189331099927658,-0.989923796468674));
#86798=DIRECTION('center_axis',(0.16237564746021,0.986495109135972,-0.0214836859659558));
#86799=DIRECTION('ref_axis',(-0.0319435566139225,-0.0165058480456351,-0.999353374022997));
#86800=DIRECTION('center_axis',(-0.163664315062582,0.986495983653055,0.00629811173985892));
#86801=DIRECTION('ref_axis',(0.0757555163317556,0.0189330280744371,-0.996946659652983));
#86802=DIRECTION('center_axis',(0.163197752493999,0.98649510914378,0.0139245544384616));
#86803=DIRECTION('ref_axis',(0.183634698391597,-0.0165058483007756,-0.982855968348618));
#86804=DIRECTION('center_axis',(-0.161191868054319,0.986495981535451,-0.0290320527618295));
#86805=DIRECTION('ref_axis',(0.288298462114998,0.0189331062348063,-0.957353400908164));
#86806=DIRECTION('center_axis',(0.156388911180579,0.986495109171284,0.048681701294124));
#86807=DIRECTION('ref_axis',(0.390626404147077,-0.0165058460816333,-0.920401308901858));
#86808=DIRECTION('center_axis',(-0.151182256635406,0.986495981655841,-0.0630047891473777));
#86809=DIRECTION('ref_axis',(0.487360887744349,0.0189331030435584,-0.872995362362357));
#86810=DIRECTION('center_axis',(0.142267496094813,0.986495109287409,0.0811625462078183));
#86811=DIRECTION('ref_axis',(0.579352849964745,-0.016505842071336,-0.814909708136579));
#86812=DIRECTION('center_axis',(-0.134103531952461,0.986495981849888,-0.0940314868110691));
#86813=DIRECTION('ref_axis',(0.663634858768959,0.0189331041865345,-0.747817030959155));
#86814=DIRECTION('center_axis',(0.121493814933404,0.98649510921518,0.109848315542195));
#86815=DIRECTION('ref_axis',(0.740989400275716,-0.016505844661274,-0.671313835527805));
#86816=DIRECTION('center_axis',(-0.110754275835824,0.98649598164166,-0.120661379856773));
#86817=DIRECTION('ref_axis',(0.808877999520859,0.0189331028534798,-0.587671608559979));
#86818=DIRECTION('center_axis',(0.0950392159143356,0.986495109219244,0.133397702097527));
#86819=DIRECTION('ref_axis',(0.867978110778369,-0.0165058442422676,-0.496328073269549));
#86820=DIRECTION('center_axis',(-0.0822261980276879,0.986495983852485,-0.141649307096185));
#86821=DIRECTION('ref_axis',(0.916298905042974,0.0189330215273502,-0.400047318842275));
#86822=DIRECTION('center_axis',(0.064140691289718,0.986495109175035,0.150709559400232));
#86823=DIRECTION('ref_axis',(0.954381129773572,-0.0165058468249323,-0.298134560480182));
#86824=DIRECTION('center_axis',(-0.0498534589114977,0.986495981677122,-0.156013815956958));
#86825=DIRECTION('ref_axis',(0.980874694402299,0.0189331024249501,-0.193717246299246));
#86826=DIRECTION('center_axis',(0.0302430200186192,0.986495109093,0.16097440627548));
#86827=DIRECTION('ref_axis',(0.996158346896073,-0.016505849461692,-0.0860006095491782));
#86828=DIRECTION('center_axis',(-0.0151495071665771,0.986495982983799,-0.163083316097745));
#86829=DIRECTION('ref_axis',(0.999585871964159,0.0189330533656895,0.0216708112424038));
#86830=DIRECTION('center_axis',(-0.00506879005589042,0.986495109267348,
0.163712268199342));
#86831=DIRECTION('ref_axis',(0.991356307130926,-0.0165058434051812,0.1301546366643));
#86832=DIRECTION('center_axis',(0.0202627268826977,0.986495981675467,-0.16252722860319));
#86833=DIRECTION('ref_axis',(0.971557523482164,0.0189331022783203,0.236045580774823));
#86834=DIRECTION('center_axis',(-0.0401435778617752,0.986495109147451,0.158795128340308));
#86835=DIRECTION('ref_axis',(0.940199548977773,-0.0165058484342841,0.340223992495321));
#86836=DIRECTION('center_axis',(0.054727547497996,0.986495981988391,-0.154371542279058));
#86837=DIRECTION('ref_axis',(0.898100225758627,0.0189330993522306,0.439383115562287));
#86838=DIRECTION('center_axis',(-0.0733413035779035,0.986495109199414,0.146452902720055));
#86839=DIRECTION('ref_axis',(0.845080103326574,-0.0165058468114072,0.534384857553605));
#86840=DIRECTION('center_axis',(0.0866333614647967,0.98649598183897,-0.138997620471991));
#86841=DIRECTION('ref_axis',(0.782648761242793,0.0189331052907383,0.622175581366845));
#86842=DIRECTION('center_axis',(-0.1031096704265,0.986495109194321,0.127262702313847));
#86843=DIRECTION('ref_axis',(0.710445651810553,-0.016505845860293,0.703558478646881));
#86844=DIRECTION('center_axis',(0.114488301191737,0.98649598151416,-0.117124324316706));
#86845=DIRECTION('ref_axis',(0.630601508918483,0.0189331076900093,0.775875811185612));
#86846=DIRECTION('center_axis',(-0.128056743368114,0.986495109232669,0.102121838692695));
#86847=DIRECTION('ref_axis',(0.542591550572572,-0.0165058447424131,0.839834487465591));
#86848=DIRECTION('center_axis',(0.136989899075835,0.986495981729044,-0.0897744149724316));
#86849=DIRECTION('ref_axis',(0.449068030412752,0.0189330998910831,0.893296950509586));
#86850=DIRECTION('center_axis',(-0.147016025755215,0.986495109314145,0.0722058686701834));
#86851=DIRECTION('ref_axis',(0.349366471721126,-0.0165058408723137,0.93684076856968));
#86852=DIRECTION('center_axis',(0.153085996471795,0.986495981709713,-0.0582267615004277));
#86853=DIRECTION('ref_axis',(0.246536630648454,0.0189331013475293,0.968948516393865));
#86854=DIRECTION('center_axis',(-0.159100999133471,0.986495109064463,0.0389136462776891));
#86855=DIRECTION('ref_axis',(0.139805408798706,-0.0165058509385653,0.990041415575844));
#86856=DIRECTION('center_axis',(0.162023961952645,0.986495981990121,-0.0239564870236498));
#86857=DIRECTION('ref_axis',(0.0324774513921005,0.0189331004002128,0.999293126595149));
#86858=DIRECTION('center_axis',(-0.15836291160918,0.987363722905755,-0.00583668710401735));
#86859=DIRECTION('ref_axis',(0.132413884601793,0.0270949580336305,0.990824114772051));
#86860=DIRECTION('',(-0.72694655115667,0.,-0.686694045235156));
#86861=DIRECTION('center_axis',(-2.0245503388309E-15,-1.,-1.47071881168559E-14));
#86862=DIRECTION('ref_axis',(-1.83209071492823E-32,1.47071881168559E-14,
-1.));
#86863=DIRECTION('center_axis',(-0.15834023719723,-0.987363722465014,0.00642252632184778));
#86864=DIRECTION('ref_axis',(0.0607081672435869,-0.00324287698160672,0.998150290376558));
#86865=DIRECTION('center_axis',(0.157437856145224,-0.987363722433383,-0.0180610374809706));
#86866=DIRECTION('ref_axis',(0.135803012302186,0.00353155705231592,0.990729564489946));
#86867=DIRECTION('center_axis',(0.155570627572672,0.987363722621189,-0.0301771285624221));
#86868=DIRECTION('ref_axis',(0.138060268971994,0.00851653687434142,0.990387212523995));
#86869=DIRECTION('',(-0.514367502868879,0.,0.857569864204913));
#86870=DIRECTION('center_axis',(-0.155915188834612,0.98736372298566,0.0283431194924692));
#86871=DIRECTION('ref_axis',(0.342316018190414,0.0270949546174172,0.939194126432092));
#86872=DIRECTION('',(-0.857569866383719,0.,-0.514367499236305));
#86873=DIRECTION('center_axis',(2.56941408722281E-15,-1.,6.96406186728433E-15));
#86874=DIRECTION('ref_axis',(-9.62012929511592E-33,-6.96406186728433E-15,
-1.));
#86875=DIRECTION('center_axis',(-0.153257677401923,-0.98736372244662,0.0403108411438247));
#86876=DIRECTION('ref_axis',(0.27386165228357,-0.00324287777277629,0.961763629564075));
#86877=DIRECTION('center_axis',(0.149874458590937,-0.987363722433169,-0.0514832621828552));
#86878=DIRECTION('ref_axis',(0.345605584671512,0.0035315609454342,0.938373224213666));
#86879=DIRECTION('center_axis',(0.145446283705042,0.987363722654481,-0.0629146862209245));
#86880=DIRECTION('ref_axis',(0.347736469892643,0.00851653269792382,0.937553633760442));
#86881=DIRECTION('',(-0.317989704666151,0.,0.948094166064919));
#86882=DIRECTION('center_axis',(-0.146177046567747,0.987363722929969,0.0611976282105879));
#86883=DIRECTION('ref_axis',(0.536211834736705,0.0270949566464369,0.843648464475948));
#86884=DIRECTION('',(-0.948094166918618,0.,-0.317989702120825));
#86885=DIRECTION('center_axis',(4.40705107135704E-14,-1.,6.87378769249437E-14));
#86886=DIRECTION('ref_axis',(6.13250777988043E-31,-6.87378769249437E-14,
-1.));
#86887=DIRECTION('center_axis',(-0.141008958275276,-0.987363722445226,0.0723142675080716));
#86888=DIRECTION('ref_axis',(0.474209669804676,-0.00324287656832448,0.880405970456416));
#86889=DIRECTION('center_axis',(0.13530309665382,-0.987363722448703,-0.0824981916658008));
#86890=DIRECTION('ref_axis',(0.539248023675166,0.00353155953696141,0.842139594752358));
#86891=DIRECTION('center_axis',(0.128521034514222,0.987363722653669,-0.0927104248446941));
#86892=DIRECTION('ref_axis',(0.541152901773958,0.00851652945533707,0.840881088875033));
#86893=DIRECTION('',(-0.106743061026616,0.,0.994286638209862));
#86894=DIRECTION('center_axis',(-0.129603832284082,0.9873637227692,0.0911906004839699));
#86895=DIRECTION('ref_axis',(0.705034980934041,0.02709496374429,0.708654738641485));
#86896=DIRECTION('',(-0.994286638431604,0.,-0.106743058961141));
#86897=DIRECTION('center_axis',(-6.30728491548966E-14,-1.,-6.28985089545158E-14));
#86898=DIRECTION('ref_axis',(1.,-6.30728491548966E-14,8.34113152972558E-31));
#86899=DIRECTION('center_axis',(-0.122166818764846,-0.98736372241398,0.100936356451412));
#86900=DIRECTION('ref_axis',(0.652384170649037,-0.00324287878729627,0.757881506321232));
#86901=DIRECTION('center_axis',(0.114405110202945,-0.987363722454584,-0.109655598763029));
#86902=DIRECTION('ref_axis',(0.707675823845859,0.00353155565455917,0.70652845410411));
#86903=DIRECTION('center_axis',(0.105586278763573,0.98736372261356,-0.11817113439226));
#86904=DIRECTION('ref_axis',(0.709265625848057,0.00851653576707507,0.70488987835611));
#86905=DIRECTION('',(0.109494768473299,0.,0.9939873719907));
#86906=DIRECTION('center_axis',(-0.106970480047799,0.987363722863142,0.116919609870118));
#86907=DIRECTION('ref_axis',(0.840891476130767,0.0270949599582825,0.540525104426685));
#86908=DIRECTION('',(-0.993987372109725,0.,0.109494767392795));
#86909=DIRECTION('center_axis',(6.88595975526522E-14,-1.,4.3880080293387E-14));
#86910=DIRECTION('ref_axis',(1.,6.88595975526522E-14,3.91605303123208E-31));
#86911=DIRECTION('center_axis',(-0.0976122921152477,-0.987363722456686,
0.124838776045279));
#86912=DIRECTION('ref_axis',(0.800053913492653,-0.0032428775879435,0.599919343953868));
#86913=DIRECTION('center_axis',(0.0881576724751072,-0.987363722452903,-0.131685627035442));
#86914=DIRECTION('ref_axis',(0.843013489298349,0.00353155875429685,0.537880827836229));
#86915=DIRECTION('center_axis',(0.07771443415297,0.987363722672603,-0.1381062847027));
#86916=DIRECTION('ref_axis',(0.844213877071177,0.00851653011734737,0.535938801054012));
#86917=DIRECTION('',(0.320612743670323,0.,0.947210361322229));
#86918=DIRECTION('center_axis',(-0.0793353088483608,0.987363722876107,0.137181585929636));
#86919=DIRECTION('ref_axis',(0.937428820871696,0.0270949592767233,0.347121115723165));
#86920=DIRECTION('',(-0.947210360754578,0.,0.320612745347376));
#86921=DIRECTION('center_axis',(0.,-1.,0.));
#86922=DIRECTION('ref_axis',(0.,0.,-1.));
#86923=DIRECTION('center_axis',(-0.0684935224953906,-0.987363722485225,
0.142903872922647));
#86924=DIRECTION('ref_axis',(0.910314022305051,-0.0032428753198789,0.413905622762555));
#86925=DIRECTION('center_axis',(0.0577880795527804,-0.987363722415584,-0.147558183504823));
#86926=DIRECTION('ref_axis',(0.938932780253383,0.00353156027763765,0.344082493375728));
#86927=DIRECTION('center_axis',(0.0462087395804152,0.987363722621269,-0.151583744635957));
#86928=DIRECTION('ref_axis',(0.939687625507126,0.00851653610917604,0.341927821449909));
#86929=DIRECTION('',(0.516739224239444,0.,0.856142846803276));
#86930=DIRECTION('center_axis',(-0.047990510290617,0.987363722793048,0.151029102607078));
#86931=DIRECTION('ref_axis',(0.990133034822597,0.0270949619669287,0.137486131624267));
#86932=DIRECTION('',(-0.856142845888396,0.,0.516739225755234));
#86933=DIRECTION('center_axis',(-7.35636780272307E-14,-1.,-9.91917069305592E-15));
#86934=DIRECTION('ref_axis',(1.,-7.35636780272307E-14,-1.13104790148456E-31));
#86935=DIRECTION('center_axis',(-0.0361720754548826,-0.987363722423393,
0.154286942414149));
#86936=DIRECTION('ref_axis',(0.978008860380544,-0.00324287732998205,0.208538132637109));
#86937=DIRECTION('center_axis',(0.02471637831391,-0.98736372243031,-0.156531084042774));
#86938=DIRECTION('ref_axis',(0.990948618920442,0.00353156016155522,0.134195241132066));
#86939=DIRECTION('center_axis',(0.0125423821788183,0.987363722633,-0.157973313814658));
#86940=DIRECTION('ref_axis',(0.991222625357522,0.00851653447638002,0.131928676260526));
#86941=DIRECTION('',(0.688703551631228,0.,0.725043045598351));
#86942=DIRECTION('center_axis',(-0.0144017228910838,0.987363722894221,0.15781466690467));
#86943=DIRECTION('ref_axis',(0.99653972906016,0.0270949585737063,-0.0785775516581714));
#86944=DIRECTION('',(-0.725043043015455,0.,0.688703554350411));
#86945=DIRECTION('center_axis',(-2.21928385368045E-14,-1.,1.83802507277912E-15));
#86946=DIRECTION('ref_axis',(1.,-2.21928385368045E-14,-2.13614459626393E-32));
#86947=DIRECTION('center_axis',(-0.00215926571236271,-0.987363722398442,
0.158455726507681));
#86948=DIRECTION('ref_axis',(0.999973090886145,-0.0032428822627582,-0.00658036611741906));
#86949=DIRECTION('center_axis',(-0.0095110328850321,-0.987363722430227,
-0.158184765012899));
#86950=DIRECTION('ref_axis',(0.996628801083753,0.00353155993727947,-0.0819668282585741));
#86951=DIRECTION('center_axis',(-0.0217104385133635,0.987363722671077,-0.156976227539939));
#86952=DIRECTION('ref_axis',(0.996409156842823,0.00851652826540035,-0.0842393073694228));
#86953=DIRECTION('',(0.828464869293673,1.87013121872489E-15,0.560041034519987));
#86954=DIRECTION('center_axis',(0.0198604695456076,0.987363722899584,0.157220992400195));
#86955=DIRECTION('ref_axis',(0.956349333116399,0.0270949588163081,-0.290967036371067));
#86956=DIRECTION('',(-0.560041033053189,0.,0.828464870285227));
#86957=DIRECTION('center_axis',(4.25577224838883E-14,-1.,-1.31317146727204E-14));
#86958=DIRECTION('ref_axis',(1.,4.25577224838883E-14,-1.08572151518037E-32));
#86959=DIRECTION('center_axis',(0.0319545165155947,-0.987363722426653,0.15521529728103));
#86960=DIRECTION('ref_axis',(0.975179691686365,-0.00324287950557378,-0.221391175648441));
#86961=DIRECTION('center_axis',(-0.0432937216746018,-0.987363722469846,
-0.152441901110066));
#86962=DIRECTION('ref_axis',(0.955707728024584,0.00353155703424488,-0.294296222705968));
#86963=DIRECTION('center_axis',(-0.0549481159469274,0.987363722638201,-0.148639105796278));
#86964=DIRECTION('ref_axis',(0.955004703283605,0.00851653533058213,-0.296468354689258));
#86965=DIRECTION('',(0.929488088790823,0.,0.368852128631492));
#86966=DIRECTION('center_axis',(0.0531940068768264,0.98736372282302,0.149275840260425));
#86967=DIRECTION('ref_axis',(0.871441105152733,0.0270949610725341,-0.489751225965449));
#86968=DIRECTION('',(-0.368852126985839,0.,0.929488089443874));
#86969=DIRECTION('center_axis',(-6.45663602884179E-14,-1.,3.66222581023245E-14));
#86970=DIRECTION('ref_axis',(1.,-6.45663602884179E-14,2.10025872039675E-31));
#86971=DIRECTION('center_axis',(0.0645741407431292,-0.987363722430153,0.144717172360982));
#86972=DIRECTION('ref_axis',(0.904787972919877,-0.00324287734543557,-0.425849982747519));
#86973=DIRECTION('center_axis',(-0.0750520377175071,-0.987363722424591,
-0.139571025912634));
#86974=DIRECTION('ref_axis',(0.870098824602278,0.00353156085805394,-0.492864650288129));
#86975=DIRECTION('center_axis',(-0.0856164675832888,0.987363722648476,-0.133351789175487));
#86976=DIRECTION('ref_axis',(0.868945292031076,0.00851652843073849,-0.494834869628764));
#86977=DIRECTION('',(0.987049478230213,-1.87013121704985E-15,0.160416107437701));
#86978=DIRECTION('center_axis',(0.0840402554793423,0.987363722896862,0.134350713307433));
#86979=DIRECTION('ref_axis',(0.745785259666093,0.0270949585837386,-0.66563519264243));
#86980=DIRECTION('',(-0.160416105690125,0.,0.987049478514231));
#86981=DIRECTION('center_axis',(4.96657185207468E-14,-1.,-4.46813180275799E-14));
#86982=DIRECTION('ref_axis',(1.,4.96657185207468E-14,-2.32209169568253E-31));
#86983=DIRECTION('center_axis',(0.0941743444094941,-0.987363722412064,0.127452236228457));
#86984=DIRECTION('ref_axis',(0.792089375903309,-0.00324288094989723,-0.610396514000736));
#86985=DIRECTION('center_axis',(-0.103301011994103,-0.987363722464081,-0.120173959254356));
#86986=DIRECTION('ref_axis',(0.743805065498613,0.00353155516523428,-0.668387277449773));
#86987=DIRECTION('center_axis',(-0.11228149913824,0.987363722622966,-0.111829084765048));
#86988=DIRECTION('ref_axis',(0.742254964002065,0.00851653420417142,-0.670063457487007));
#86989=DIRECTION('',(0.998457531228928,0.,-0.0555207918912755));
#86990=DIRECTION('center_axis',(0.110956872201526,0.987363722845984,0.113143498792342));
#86991=DIRECTION('ref_axis',(0.585257325062038,0.0270949599090236,-0.810394796755727));
#86992=DIRECTION('',(0.0555207965249884,0.,0.998457530971263));
#86993=DIRECTION('center_axis',(2.16107772093633E-14,-1.,-3.01740860957852E-14));
#86994=DIRECTION('ref_axis',(2.18320417523822E-31,3.01740860957852E-14,
-1.));
#86995=DIRECTION('center_axis',(0.119371065794289,-0.987363722406043,0.104227771383728));
#86996=DIRECTION('ref_axis',(0.642353557624346,-0.00324287839619577,-0.766401585819767));
#86997=DIRECTION('center_axis',(-0.126719736910895,-0.9873637224439,-0.0951577000508082));
#86998=DIRECTION('ref_axis',(0.582731810288293,0.00353156143387916,-0.812656855845054));
#86999=DIRECTION('center_axis',(-0.13369636490729,0.987363722672937,-0.0850773833637106));
#87000=DIRECTION('ref_axis',(0.580857619958026,0.00851652967266056,-0.813960621933907));
#87001=DIRECTION('',(0.9631788194689,0.,-0.268861603295255));
#87002=DIRECTION('center_axis',(0.132685271195736,0.987363722952293,0.0866458158568595));
#87003=DIRECTION('ref_axis',(0.397363406138617,0.0270949567738405,-0.917261242383728));
#87004=DIRECTION('',(0.26886160500055,0.,0.963178818992885));
#87005=DIRECTION('center_axis',(-1.46189926784329E-14,-1.,3.41143110164411E-14));
#87006=DIRECTION('ref_axis',(2.80296443029282E-32,-3.41143110164411E-14,
-1.));
#87007=DIRECTION('center_axis',(0.138986126964955,-0.987363722455319,0.0761297319741655));
#87008=DIRECTION('ref_axis',(0.462582001950055,-0.00324287689216964,-0.886570569792017));
#87009=DIRECTION('center_axis',(-0.144213194896543,-0.987363722466983,-0.0656919627798898));
#87010=DIRECTION('ref_axis',(0.394410661594976,0.00353155551480209,-0.918927504287394));
#87011=DIRECTION('center_axis',(-0.148859741286094,0.98736372264215,-0.0543475540799514));
#87012=DIRECTION('ref_axis',(0.392300018065111,0.00851653069053326,-0.919797893306519));
#87013=DIRECTION('',(0.882862937137387,1.87013121653348E-15,-0.469630742423393));
#87014=DIRECTION('center_axis',(0.148209452542795,0.987363722947302,0.0560966735609954));
#87015=DIRECTION('ref_axis',(0.19088921752838,0.0270949566362958,-0.981237570599638));
#87016=DIRECTION('',(0.469630743986495,0.,0.882862936305909));
#87017=DIRECTION('center_axis',(0.,-1.,0.));
#87018=DIRECTION('ref_axis',(0.,0.,-1.));
#87019=DIRECTION('center_axis',(0.152102349520003,-0.987363722407373,0.0444719568306875));
#87020=DIRECTION('ref_axis',(0.261180626874225,-0.00324288151993721,-0.965284498925076));
#87021=DIRECTION('center_axis',(-0.154963399384707,-0.987363722388471,-0.0331545556796895));
#87022=DIRECTION('ref_axis',(0.18764731161762,0.0035315638300726,-0.982230122985237));
#87023=DIRECTION('center_axis',(-0.15706260107623,0.987363722655006,-0.0210764923082087));
#87024=DIRECTION('ref_axis',(0.185398901952652,0.00851653249045242,-0.982626437578946));
#87025=DIRECTION('',(0.761265364441084,0.,-0.648440471363705));
#87026=DIRECTION('',(0.648440472711532,0.,0.761265363293015));
#87027=DIRECTION('',(0.604071869369054,0.,-0.796929844237858));
#87028=DIRECTION('center_axis',(0.158065638931242,0.987363722829192,-0.0113195684606789));
#87029=DIRECTION('ref_axis',(-0.238764600494895,0.0270949602251595,-0.970699401813409));
#87030=DIRECTION('',(0.796929845307366,0.,0.604071867958091));
#87031=DIRECTION('center_axis',(2.34182590397253E-14,-1.,9.36135301163808E-14));
#87032=DIRECTION('ref_axis',(-8.69630141945268E-32,-9.36135301163808E-14,
-1.));
#87033=DIRECTION('center_axis',(0.156717644371601,-0.987363722359724,-0.0235044615034313));
#87034=DIRECTION('ref_axis',(-0.168271322623861,-0.00324288391144424,-0.985735383196907));
#87035=DIRECTION('center_axis',(-0.154562207294442,-0.987363722441959,0.034977188020583));
#87036=DIRECTION('ref_axis',(-0.242123637853155,0.00353155854253617,-0.970238976792323));
#87037=DIRECTION('center_axis',(-0.151395946244086,0.987363722665093,0.0468203655024876));
#87038=DIRECTION('ref_axis',(-0.24433064533845,0.00851652983106372,-0.969654579975845));
#87039=DIRECTION('',(0.418632647009714,0.,-0.908155662239486));
#87040=DIRECTION('center_axis',(0.151936777370572,0.987363722957365,-0.0450343676542403));
#87041=DIRECTION('ref_axis',(-0.44185409481804,0.0270949552799474,-0.8966776579635));
#87042=DIRECTION('',(0.908155662980674,0.,0.418632645401827));
#87043=DIRECTION('center_axis',(9.92189883306421E-15,-1.,1.99363071636205E-14));
#87044=DIRECTION('ref_axis',(-1.29111785430247E-31,-1.99363071636205E-14,
-1.));
#87045=DIRECTION('center_axis',(0.148000906784593,-0.987363722409755,-0.0566446048630474));
#87046=DIRECTION('ref_axis',(-0.376241204684736,-0.00324288035874891,-0.926516076290292));
#87047=DIRECTION('center_axis',(-0.143429566060712,-0.987363722443142,0.0673857491080862));
#87048=DIRECTION('ref_axis',(-0.44503562198399,0.00353155572008162,-0.895505903542528));
#87049=DIRECTION('center_axis',(-0.137791397644641,0.987363722642848,0.0782713864959209));
#87050=DIRECTION('ref_axis',(-0.447065403159386,0.00851653186774189,-0.894460728027162));
#87051=DIRECTION('',(0.213618626551052,1.87013121746126E-15,-0.976917131792888));
#87052=DIRECTION('center_axis',(0.138703522518533,0.987363722956564,-0.0766434043496538));
#87053=DIRECTION('ref_axis',(-0.624282981195083,0.0270949558569211,-0.780728264351491));
#87054=DIRECTION('',(0.97691713277104,0.,0.213618622077782));
#87055=DIRECTION('center_axis',(-5.12440392804277E-14,-1.,-6.35700721972811E-14));
#87056=DIRECTION('ref_axis',(-3.8654389694051E-31,6.35700721972811E-14,
-1.));
#87057=DIRECTION('center_axis',(0.132363811790207,-0.987363722409503,-0.0871361061674017));
#87058=DIRECTION('ref_axis',(-0.56661846094771,-0.00324287919072601,-0.823973909446047));
#87059=DIRECTION('center_axis',(-0.125590320889639,-0.987363722425399,0.0966434215924563));
#87060=DIRECTION('ref_axis',(-0.627138234454523,0.00353155971536402,-0.778899969810784));
#87061=DIRECTION('center_axis',(-0.117743875713536,0.987363722627784,0.106062523874179));
#87062=DIRECTION('ref_axis',(-0.628895878264022,0.00851653394903831,-0.777442887260549));
#87063=DIRECTION('',(-0.00138396519504165,0.,-0.999999042319711));
#87064=DIRECTION('center_axis',(0.118984646214767,0.987363722909371,-0.104668680357086));
#87065=DIRECTION('ref_axis',(-0.777521090773876,0.0270949576384109,-0.628272883922563));
#87066=DIRECTION('',(0.999999042317255,0.,-0.00138396696952341));
#87067=DIRECTION('center_axis',(-2.31678794545486E-14,-1.,-1.85701401946468E-14));
#87068=DIRECTION('ref_axis',(1.,-2.31678794545486E-14,-1.73093210128079E-31));
#87069=DIRECTION('center_axis',(0.110537527352398,-0.987363722487205,-0.113553223481447));
#87070=DIRECTION('ref_axis',(-0.730501271666092,-0.00324287296146556,-0.682903635858807));
#87071=DIRECTION('center_axis',(-0.101878611119281,-0.987363722418207,0.121382157868727));
#87072=DIRECTION('ref_axis',(-0.779916560199733,0.00353156097293767,-0.625873539305913));
#87073=DIRECTION('center_axis',(-0.0921907795654185,0.987363722627442,0.128894295461047));
#87074=DIRECTION('ref_axis',(-0.781319882146542,0.00851653674625868,-0.624072680354111));
#87075=DIRECTION('',(-0.216321844433724,0.,-0.976322108538361));
#87076=DIRECTION('center_axis',(0.0937021776712861,0.987363722933383,-0.127799767350289));
#87077=DIRECTION('ref_axis',(-0.894403178552326,0.0270949561808685,-0.446440161214304));
#87078=DIRECTION('',(0.97632210815536,0.,-0.216321846162316));
#87079=DIRECTION('center_axis',(-0.0623268466247098,0.987363722160776,0.145699157000437));
#87080=DIRECTION('ref_axis',(-0.897210243280335,0.00851664566298019,-0.441521512612345));
#87081=DIRECTION('',(-0.421144752952744,0.,-0.906993438267539));
#87082=DIRECTION('center_axis',(1.996369424311E-14,-1.,9.86667873383296E-15));
#87083=DIRECTION('ref_axis',(1.,1.996369424311E-14,-1.41826297981486E-31));
#87084=DIRECTION('center_axis',(0.0835426374854572,-0.987363722437547,-0.134660711925359));
#87085=DIRECTION('ref_axis',(-0.860226652654134,-0.0032428756551188,-0.50990154914547));
#87086=DIRECTION('center_axis',(-0.0734031620397199,-0.987363722481538,
0.140445204011996));
#87087=DIRECTION('ref_axis',(-0.896226855125206,0.00353155234490209,-0.443581956678153));
#87088=DIRECTION('',(0.90699343803103,0.,-0.421144753462099));
#87089=DIRECTION('center_axis',(0.0640383013215094,0.987363722930161,-0.144955077887422));
#87090=DIRECTION('ref_axis',(-0.969463967507944,0.027094957164752,-0.243732392184538));
#87091=DIRECTION('center_axis',(-7.92659929065579E-14,-1.,-1.95961224160717E-14));
#87092=DIRECTION('ref_axis',(1.,-7.92659929065579E-14,2.13008784219506E-31));
#87093=DIRECTION('center_axis',(-0.0295487779255952,0.987363722618801,0.155691197501488));
#87094=DIRECTION('ref_axis',(-0.971148037060758,0.00851653427239421,-0.238325321267012));
#87095=DIRECTION('center_axis',(0.05264138558487,-0.987363722444023,-0.149471616453384));
#87096=DIRECTION('ref_axis',(-0.949728792505462,-0.00324287704961478,-0.313057030642274));
#87097=DIRECTION('center_axis',(-0.0414954754768436,-0.987363722444349,
0.152941181883068));
#87098=DIRECTION('ref_axis',(-0.970630577874648,0.00353155855321122,-0.240548975031929));
#87099=DIRECTION('',(-0.606275400562902,0.,-0.795254763376047));
#87100=DIRECTION('center_axis',(0.0313800671770485,0.987363722868791,-0.155332450397991));
#87101=DIRECTION('ref_axis',(-0.999193698214912,0.0270949595955448,-0.0296279700979335));
#87102=DIRECTION('',(0.795254762302624,0.,-0.606275401970917));
#87103=DIRECTION('center_axis',(-8.16253850365633E-14,-1.,-2.09813056959433E-15));
#87104=DIRECTION('ref_axis',(-0.999669805779023,8.16523461650324E-14,-0.0256959026642592));
#87105=DIRECTION('center_axis',(0.0192786812535226,-0.987363722432654,-0.157293394880581));
#87106=DIRECTION('ref_axis',(-0.994822668868896,-0.00324287838217591,-0.101574313900534));
#87107=DIRECTION('center_axis',(-0.00764750029647438,-0.987363722476038,
0.158285802513925));
#87108=DIRECTION('ref_axis',(-0.999648693396266,0.00353155762759509,-0.0262681916366585));
#87109=DIRECTION('center_axis',(0.00461105941972974,0.98736372264553,0.158403337510889));
#87110=DIRECTION('ref_axis',(-0.999676034875211,0.00851653231120432,-0.0239852866059154));
#87111=DIRECTION('',(-0.763057286545784,0.,-0.646330857571712));
#87112=DIRECTION('center_axis',(-0.00274546700816765,0.987363722872233,
-0.158446650853819));
#87113=DIRECTION('ref_axis',(-0.982202242647199,0.0270949591400856,0.185861824288935));
#87114=DIRECTION('',(0.646330857894588,0.,-0.763057286272299));
#87115=DIRECTION('center_axis',(2.91520236126574E-14,-1.,-5.63562454897997E-15));
#87116=DIRECTION('ref_axis',(1.,2.91520236126574E-14,4.88564478945882E-32));
#87117=DIRECTION('center_axis',(-0.0149854773444683,-0.987363722451026,
-0.157760308875241));
#87118=DIRECTION('ref_axis',(-0.993399742862264,-0.00324287466414407,0.114657902671822));
#87119=DIRECTION('center_axis',(0.0265580647803664,-0.987363722491441,0.156229154458978));
#87120=DIRECTION('ref_axis',(-0.981924347057675,0.00353155553646724,0.189240864431687));
#87121=DIRECTION('center_axis',(0.0385552928309168,0.98736372264335,0.15370871348947));
#87122=DIRECTION('ref_axis',(-0.981460292520777,0.00851653480253085,0.191476272263664));
#87123=DIRECTION('',(-0.88415945988124,0.,-0.467185241100908));
#87124=DIRECTION('center_axis',(-0.0367426288065956,0.987363722975676,-0.15415206057654));
#87125=DIRECTION('ref_axis',(-0.91928410143936,0.0270949559871885,0.39266092777469));
#87126=DIRECTION('',(0.467185239535493,0.,-0.884159460708398));
#87127=DIRECTION('center_axis',(-1.36294864018309E-14,-1.,5.88534506176603E-15));
#87128=DIRECTION('ref_axis',(1.,-1.36294864018309E-14,7.0077482906534E-32));
#87129=DIRECTION('center_axis',(-0.0485489273147898,-0.98736372247699,-0.150850525994987));
#87130=DIRECTION('ref_axis',(-0.945526549719031,-0.00324287530838049,0.32552884286367));
#87131=DIRECTION('center_axis',(0.0595218018727172,-0.987363722479134,0.146867404940558));
#87132=DIRECTION('ref_axis',(-0.918286310020471,0.00353155562112468,0.395901226247004));
#87133=DIRECTION('center_axis',(0.0706967180234564,0.987363722640494,0.141826842572968));
#87134=DIRECTION('ref_axis',(-0.917352557164235,0.00851653082876537,0.397984615992731));
#87135=DIRECTION('',(-0.963919320010511,0.,-0.2661945613841));
#87136=DIRECTION('center_axis',(-0.0690217369231991,0.987363722785221,-0.142649496177916));
#87137=DIRECTION('ref_axis',(-0.813381258259928,0.0270949631238604,0.581099640065981));
#87138=DIRECTION('',(0.266194559677452,0.,-0.963919320481817));
#87139=DIRECTION('center_axis',(-4.21598147701531E-14,-1.,3.03718997949049E-14));
#87140=DIRECTION('ref_axis',(1.,-4.21598147701531E-14,1.83273274081679E-31));
#87141=DIRECTION('center_axis',(-0.0798422822123721,-0.987363722443673,
-0.136887141738341));
#87142=DIRECTION('ref_axis',(-0.853441585256062,-0.00324287810098406,0.521178418871352));
#87143=DIRECTION('center_axis',(0.0897023623928398,-0.98736372243683,0.130638301415894));
#87144=DIRECTION('ref_axis',(-0.811710225602143,0.00353156010617074,0.584049687728822));
#87145=DIRECTION('center_axis',(0.0995324486587646,0.987363722660884,0.123313303569528));
#87146=DIRECTION('ref_axis',(-0.810350436308831,0.00851653338126038,0.585883639499562));
#87147=DIRECTION('',(-0.998607383967675,0.,-0.052756920733087));
#87148=DIRECTION('center_axis',(-0.0980734771944362,0.987363722940225,-0.124476791783094));
#87149=DIRECTION('ref_axis',(-0.669445610333536,0.02709495584999,0.742366781431286));
#87150=DIRECTION('',(0.0527569189650408,0.,-0.998607384061081));
#87151=DIRECTION('center_axis',(4.45436757048174E-14,-1.,-4.97892029732121E-14));
#87152=DIRECTION('ref_axis',(-1.17560233778818E-31,4.97892029732121E-14,
-1.));
#87153=DIRECTION('center_axis',(-0.107402302702658,-0.987363722394039,-0.116523066705065));
#87154=DIRECTION('ref_axis',(-0.721450640681184,-0.00324287910373861,0.692458270797474));
#87155=DIRECTION('center_axis',(0.115688545148596,-0.987363722462385,0.108300692918484));
#87156=DIRECTION('ref_axis',(-0.667179472758881,0.0035315585640653,0.744888635450488));
#87157=DIRECTION('center_axis',(0.123714148172352,0.987363722648617,0.0990337757507747));
#87158=DIRECTION('ref_axis',(-0.665457230495865,0.00851652976932358,0.746387394790039));
#87159=DIRECTION('',(-0.986601676591079,0.,0.163147576591479));
#87160=DIRECTION('center_axis',(-0.122539405670769,0.98736372302042,-0.100483692811866));
#87161=DIRECTION('ref_axis',(-0.494207430073928,0.0270949533761717,0.868921676309935));
#87162=DIRECTION('',(-0.163147578338245,0.,-0.986601676302228));
#87163=DIRECTION('center_axis',(-2.55103818864632E-14,-1.,4.52672364773351E-14));
#87164=DIRECTION('ref_axis',(2.30773181488144E-31,-4.52672364773351E-14,
-1.));
#87165=DIRECTION('center_axis',(-0.12994031340418,-0.987363722485979,-0.0907104981303418));
#87166=DIRECTION('ref_axis',(-0.555725466069267,-0.00324287493191982,0.831359543232814));
#87167=DIRECTION('center_axis',(0.136265258713363,-0.987363722442251,0.0808990659572843));
#87168=DIRECTION('ref_axis',(-0.491452149815892,0.00353155907475124,0.870897417915474));
#87169=DIRECTION('center_axis',(0.142111116604461,0.987363722627063,0.0701235322660115));
#87170=DIRECTION('ref_axis',(-0.489447982345426,0.00851653410216828,0.871990906618227));
#87171=DIRECTION('',(-0.928463571527175,0.,0.37142347306949));
#87172=DIRECTION('center_axis',(-0.141275525387784,0.987363722972098,-0.0717920920790242));
#87173=DIRECTION('ref_axis',(-0.295860660461752,0.0270949555521446,0.954846758896297));
#87174=DIRECTION('',(-0.371423474713337,0.,-0.928463570869569));
#87175=DIRECTION('center_axis',(4.33795587267854E-15,-1.,-1.41979690255456E-14));
#87176=DIRECTION('ref_axis',(-9.32044726918642E-33,1.41979690255456E-14,
-1.));
#87177=DIRECTION('center_axis',(-0.146402455491522,-0.987363722435009,-0.0606564147088839));
#87178=DIRECTION('ref_axis',(-0.364015186036907,-0.0032428792593312,0.931387367355079));
#87179=DIRECTION('center_axis',(0.150470359978484,-0.987363722444644,0.0497146896621282));
#87180=DIRECTION('ref_axis',(-0.292745071069821,0.00353156062358516,0.956184005013621));
#87181=DIRECTION('center_axis',(0.153863123526249,0.987363722660625,0.0379343959026435));
#87182=DIRECTION('ref_axis',(-0.290552692081676,0.00851653190555025,0.956821091849669));
#87183=DIRECTION('',(-0.826911541049425,0.,0.562332022278));
#87184=DIRECTION('center_axis',(-0.153405760191542,0.987363723027589,-0.0397435678966314));
#87185=DIRECTION('ref_axis',(-0.0836797723377556,0.0270949527568631,0.996124268972805));
#87186=DIRECTION('',(-0.562332021776287,0.,-0.82691154139061));
#87187=DIRECTION('center_axis',(6.51416273654917E-15,-1.,-8.13920838429517E-14));
#87188=DIRECTION('ref_axis',(-3.02306769725167E-32,8.13920838429517E-14,
-1.));
#87189=DIRECTION('center_axis',(-0.156018984352937,-0.987363722479574,-0.0277660953819161));
#87190=DIRECTION('ref_axis',(-0.155283961225101,-0.00324287333498782,0.987864553042964));
#87191=DIRECTION('center_axis',(0.157639635277682,-0.987363722413661,0.016205710442862));
#87192=DIRECTION('ref_axis',(-0.0803495567989669,0.00353156288138682,0.996760491184228));
#87193=DIRECTION('center_axis',(0.158420663065514,0.987363722652751,0.00397148626885451));
#87194=DIRECTION('ref_axis',(-0.0780714789323286,0.00851653284668103,0.996911386656603));
#87195=DIRECTION('',(-0.686694046522226,0.,0.726946549940868));
#87196=DIRECTION('',(0.760779449282709,0.,-0.64901050033809));
#87197=DIRECTION('center_axis',(0.158463151347264,-0.987363722875478,0.00151934675762116));
#87198=DIRECTION('ref_axis',(-0.181684484803401,-0.0276461711805923,0.982968177104822));
#87199=DIRECTION('center_axis',(-0.1583438731014,-0.987366232511757,-0.00592796312298457));
#87200=DIRECTION('ref_axis',(-0.254496684801816,0.0350112965860882,0.966439675580554));
#87201=DIRECTION('',(0.470291906521109,0.,0.882510919286974));
#87202=DIRECTION('center_axis',(-2.76653169601616E-14,-1.,1.45858321561486E-13));
#87203=DIRECTION('ref_axis',(-7.16568994862189E-31,-1.45858321561486E-13,
-1.));
#87204=DIRECTION('center_axis',(0.149682993082549,0.987363722771234,0.0520372994800879));
#87205=DIRECTION('ref_axis',(-0.116999345722024,-0.0345726402853016,0.992530042691062));
#87206=DIRECTION('center_axis',(-0.156429978772876,0.98736372254834,-0.0253483951484592));
#87207=DIRECTION('ref_axis',(-0.186229725703106,-0.00428129196166639,0.982496900658564));
#87208=DIRECTION('',(0.882510921618164,0.,-0.470291902146591));
#87209=DIRECTION('center_axis',(0.154431756916398,-0.987363722835662,0.0355487170488168));
#87210=DIRECTION('ref_axis',(-0.388745904643052,-0.0276461730162438,0.920930133474202));
#87211=DIRECTION('center_axis',(-0.153367540844493,-0.987366232745327,-0.0398286310286096));
#87212=DIRECTION('ref_axis',(-0.456302657595336,0.0350112876543126,0.889135588314977));
#87213=DIRECTION('',(0.269582982049911,0.,0.962977162651886));
#87214=DIRECTION('center_axis',(4.66989958556477E-14,-1.,-1.09200807760306E-13));
#87215=DIRECTION('ref_axis',(-1.34852716042978E-30,1.09200807760306E-13,
-1.));
#87216=DIRECTION('center_axis',(0.1349970075158,0.987363722840858,0.0829981131087992));
#87217=DIRECTION('ref_axis',(-0.32762858532778,-0.0345726381238089,0.944173841392187));
#87218=DIRECTION('center_axis',(-0.147323577184204,0.98736372254447,-0.0583835850969862));
#87219=DIRECTION('ref_axis',(-0.393083569634015,-0.00428129206822049,0.919492782909146));
#87220=DIRECTION('',(0.962977163988183,0.,-0.269582977276527));
#87221=DIRECTION('center_axis',(0.143179307552801,-0.987363722692721,0.0679158670641323));
#87222=DIRECTION('ref_axis',(-0.577629997206268,-0.0276461773922787,0.815830420616369));
#87223=DIRECTION('center_axis',(-0.141219909593753,-0.987366232973952,-0.0718669542777509));
#87224=DIRECTION('ref_axis',(-0.636772424978514,0.0350112793450637,0.770256508642156));
#87225=DIRECTION('',(0.0562686569827914,0.,0.998415664060492));
#87226=DIRECTION('center_axis',(0.,-1.,0.));
#87227=DIRECTION('ref_axis',(0.,0.,-1.));
#87228=DIRECTION('center_axis',(0.113998714502817,0.987363722957846,0.110078025411647));
#87229=DIRECTION('ref_axis',(-0.522938275540814,-0.0345726334276287,0.851669121779273));
#87230=DIRECTION('center_axis',(-0.131328487686392,0.987363722542039,-0.0886888252821752));
#87231=DIRECTION('ref_axis',(-0.581557263221753,-0.00428129011378238,0.81349420412747));
#87232=DIRECTION('',(0.998415664339409,0.,-0.056268652033758));
#87233=DIRECTION('center_axis',(0.125231945585741,-0.98736372287055,0.097107355869765));
#87234=DIRECTION('ref_axis',(-0.739504754353445,-0.0276461698608584,0.672583383366461));
#87235=DIRECTION('center_axis',(-0.122469001945228,-0.987366232743165,-0.100544845721249));
#87236=DIRECTION('ref_axis',(-0.787467419312884,0.0350112873268973,0.615361091783044));
#87237=DIRECTION('',(-0.159676728324535,0.,0.987169358535592));
#87238=DIRECTION('center_axis',(-6.6176317490642E-14,-1.,5.9624677248181E-14));
#87239=DIRECTION('ref_axis',(1.,-6.6176317490642E-14,1.52215481233823E-30));
#87240=DIRECTION('center_axis',(0.0876699622063549,0.987363722805222,0.132010820067707));
#87241=DIRECTION('ref_axis',(-0.693795956342581,-0.034572638888989,0.719341298413302));
#87242=DIRECTION('center_axis',(-0.109192625788737,0.987363722537062,-0.114847071756822));
#87243=DIRECTION('ref_axis',(-0.742837983763109,-0.00428129121212216,0.66945754191309));
#87244=DIRECTION('',(0.987169358123943,0.,0.159676730869475));
#87245=DIRECTION('center_axis',(0.101428888160009,-0.987363722703554,0.121758201923339));
#87246=DIRECTION('ref_axis',(-0.866801089322196,-0.0276461779428406,0.497887096031828));
#87247=DIRECTION('center_axis',(-0.097991569270547,-0.987366232948689,-0.124521381234754));
#87248=DIRECTION('ref_axis',(-0.901341314070176,0.0350112810043919,0.431692072839751));
#87249=DIRECTION('',(-0.368155805865995,0.,0.929764111270789));
#87250=DIRECTION('center_axis',(-2.58155649983822E-14,-1.,1.46682444274038E-14));
#87251=DIRECTION('ref_axis',(1.,-2.58155649983822E-14,3.81511095375126E-31));
#87252=DIRECTION('center_axis',(0.0572418606348332,0.987363722728194,0.147770932295171));
#87253=DIRECTION('ref_axis',(-0.832212508054769,-0.0345726417617727,0.553377876210102));
#87254=DIRECTION('center_axis',(-0.0819510393314511,0.987363722535972,-0.135635196657812));
#87255=DIRECTION('ref_axis',(-0.869384427205194,-0.00428129367737856,0.494117787837622));
#87256=DIRECTION('',(0.929764109056227,0.,0.368155811458791));
#87257=DIRECTION('center_axis',(0.0728831202913177,-0.987363722758493,0.140715776503882));
#87258=DIRECTION('ref_axis',(-0.953566769668903,-0.0276461750994164,0.299910161190959));
#87259=DIRECTION('center_axis',(-0.0689321668874775,-0.987366232873716,
-0.142675430782474));
#87260=DIRECTION('ref_axis',(-0.973069489809453,0.0350112832333832,0.227837613330903));
#87261=DIRECTION('',(-0.559420330169213,0.,0.828884125914696));
#87262=DIRECTION('center_axis',(8.50957512599141E-14,-1.,-2.63271769752319E-14));
#87263=DIRECTION('ref_axis',(1.,8.50957512599141E-14,-5.62014004724192E-31));
#87264=DIRECTION('center_axis',(0.0241371969399978,0.987363722764857,0.156621437523103));
#87265=DIRECTION('ref_axis',(-0.93171572713276,-0.0345726403955516,0.361539121464817));
#87266=DIRECTION('center_axis',(-0.0508775060530495,0.987363722578641,-0.150081173747645));
#87267=DIRECTION('ref_axis',(-0.955279421173268,-0.00428128798470859,0.295673634360688));
#87268=DIRECTION('',(0.828884125374412,0.,0.559420330969743));
#87269=DIRECTION('center_axis',(0.0409294185900453,-0.987363722835548,0.153093636452364));
#87270=DIRECTION('ref_axis',(-0.995744728148929,-0.0276461730218223,0.0879097575975621));
#87271=DIRECTION('center_axis',(-0.036649578451434,-0.987366232673174,-0.15415813626311));
#87272=DIRECTION('ref_axis',(-0.999298017642841,0.035011290644136,0.0133297210218571));
#87273=DIRECTION('',(-0.724526977917467,0.,0.689246442333787));
#87274=DIRECTION('center_axis',(-1.77531649047457E-13,-1.,1.48371821668093E-14));
#87275=DIRECTION('ref_axis',(1.,-1.77531649047457E-13,1.72309228978644E-31));
#87276=DIRECTION('center_axis',(-0.0100960932869904,0.98736372289332,0.158148498616284));
#87277=DIRECTION('ref_axis',(-0.987652955733019,-0.0345726365893217,0.152795195706845));
#87278=DIRECTION('center_axis',(-0.0174250066752681,0.987363722557612,-0.157509518822014));
#87279=DIRECTION('ref_axis',(-0.996506610362838,-0.00428129225189455,0.0834041128471496));
#87280=DIRECTION('',(0.689246440251503,0.,0.724526979898355));
#87281=DIRECTION('center_axis',(0.0070619071952816,-0.987363722761738,0.158313007806833));
#87282=DIRECTION('ref_axis',(-0.991362769072797,-0.0276461750575922,-0.128201205536457));
#87283=DIRECTION('center_axis',(-0.0026532898277805,-0.987366232668752,
-0.158432580735802));
#87284=DIRECTION('ref_axis',(-0.97880048130708,0.0350112911956791,-0.201801455103376));
#87285=DIRECTION('',(-0.855755550708435,0.,0.517380360500573));
#87286=DIRECTION('center_axis',(2.94284356015184E-14,-1.,3.94562661660699E-15));
#87287=DIRECTION('ref_axis',(1.,2.94284356015184E-14,-2.12214508197234E-31));
#87288=DIRECTION('center_axis',(-0.0438573043099532,0.987363722881898,0.152280713143399));
#87289=DIRECTION('ref_axis',(-0.997408629008132,-0.034572636386421,-0.0630932610776304));
#87290=DIRECTION('center_axis',(0.016842266717739,0.987363722512254,-0.157572895888073));
#87291=DIRECTION('ref_axis',(-0.991138258333607,-0.00428129664525406,-0.132765294284534));
#87292=DIRECTION('',(0.517380356258672,0.,0.855755553273042));
#87293=DIRECTION('center_axis',(-0.0271358127186797,-0.987363722769501,
0.156129839002188));
#87294=DIRECTION('ref_axis',(-0.940625789107942,-0.0276461754538182,-0.33831762272728));
#87295=DIRECTION('center_axis',(0.0314670689078621,-0.987366232801023,-0.155298892135983));
#87296=DIRECTION('ref_axis',(-0.912535322196976,0.0350112862613325,-0.407496620326093));
#87297=DIRECTION('',(-0.946969945721879,0.,0.321322146606022));
#87298=DIRECTION('center_axis',(-5.57844440175138E-14,-1.,-2.035924760324E-14));
#87299=DIRECTION('ref_axis',(1.,-5.57844440175138E-14,-8.55013534209805E-31));
#87300=DIRECTION('center_axis',(-0.0755677933535081,0.987363722995108,0.139292451772959));
#87301=DIRECTION('ref_axis',(-0.960526584060122,-0.0345726329790713,-0.276031545955689));
#87302=DIRECTION('center_axis',(0.0503220214550908,0.98736372254472,-0.150268338512501));
#87303=DIRECTION('ref_axis',(-0.939425383102902,-0.00428129350617084,-0.342726742621407));
#87304=DIRECTION('',(0.321322141912006,0.,0.946969947314634));
#87305=DIRECTION('center_axis',(-0.0600646941385593,-0.987363722798142,
0.146646211748671));
#87306=DIRECTION('ref_axis',(-0.84590619296491,-0.0276461737180322,-0.532614684159538));
#87307=DIRECTION('center_axis',(0.0641160512521902,-0.987366232586723,-0.144903604921779));
#87308=DIRECTION('ref_axis',(-0.803601026101154,0.0350112937354277,-0.594137694613079));
#87309=DIRECTION('',(-0.993905077902487,0.,0.110239267593957));
#87310=DIRECTION('center_axis',(7.51553974837504E-14,-1.,4.78128993183431E-14));
#87311=DIRECTION('ref_axis',(1.,7.51553974837504E-14,7.6276596824472E-31));
#87312=DIRECTION('center_axis',(-0.103744825459102,0.987363722817035,0.119791026606108));
#87313=DIRECTION('ref_axis',(-0.87873138215879,-0.0345726390575195,-0.47606290617722));
#87314=DIRECTION('center_axis',(0.0814487732528563,0.987363722547936,-0.135937400048282));
#87315=DIRECTION('ref_axis',(-0.843786021557471,-0.00428129117531677,-0.536662669066974));
#87316=DIRECTION('',(0.110239262352301,0.,0.993905078483866));
#87317=DIRECTION('center_axis',(-0.0901850156524691,-0.987363722797321,
0.130305571084201));
#87318=DIRECTION('ref_axis',(-0.711632962922774,-0.0276461737828286,-0.702007275715091));
#87319=DIRECTION('center_axis',(0.0937670542025258,-0.98736623292584,-0.127732774275111));
#87320=DIRECTION('ref_axis',(-0.657091237794409,0.0350112811773555,-0.752997553385223));
#87321=DIRECTION('',(-0.994366313661193,0.,-0.105998274777704));
#87322=DIRECTION('center_axis',(2.10399820468787E-14,-1.,2.09504164275063E-14));
#87323=DIRECTION('ref_axis',(1.,2.10399820468787E-14,1.6752221775065E-31));
#87324=DIRECTION('center_axis',(-0.12707085922723,0.987363722782335,0.0946883079828834));
#87325=DIRECTION('ref_axis',(-0.755847677170102,-0.0345726392425312,-0.653834093277773));
#87326=DIRECTION('center_axis',(0.108767068286513,0.98736372251492,-0.115250181422144));
#87327=DIRECTION('ref_axis',(-0.708692162259974,-0.00428129244825316,-0.705504847386788));
#87328=DIRECTION('',(-0.105998282549184,0.,0.994366312832763));
#87329=DIRECTION('center_axis',(-0.116088384586537,-0.987363722707326,0.107871989161319));
#87330=DIRECTION('ref_axis',(-0.544084566223478,-0.0276461767386126,-0.838574787189042));
#87331=DIRECTION('center_axis',(0.119033597923905,-0.987366232659441,-0.104589316706792));
#87332=DIRECTION('ref_axis',(-0.479856595381014,0.0350112912223035,-0.876648080677925));
#87333=DIRECTION('',(-0.94833208570079,0.,-0.317279459200228));
#87334=DIRECTION('center_axis',(1.12310510839231E-13,-1.,1.74885070496406E-13));
#87335=DIRECTION('ref_axis',(2.80148662775557E-30,-1.74885070496406E-13,
-1.));
#87336=DIRECTION('center_axis',(-0.144455198836148,0.987363722863726,0.0651580716557243));
#87337=DIRECTION('ref_axis',(-0.597621377110798,-0.0345726367517376,-0.801032722432876));
#87338=DIRECTION('center_axis',(0.130999534217845,0.987363722517991,-0.0891739955935754));
#87339=DIRECTION('ref_axis',(-0.540460646669499,-0.00428129707550931,-0.841358401572682));
#87340=DIRECTION('',(-0.317279463900984,0.,0.948332084128078));
#87341=DIRECTION('center_axis',(-0.136563593350214,-0.987363722837716,0.0803944263946385));
#87342=DIRECTION('ref_axis',(-0.351095380460181,-0.0276461718789811,-0.935931473453029));
#87343=DIRECTION('center_axis',(0.138734270925482,-0.987366232734516,-0.0765553690241583));
#87344=DIRECTION('ref_axis',(-0.280184390699922,0.0350112884613783,-0.959307519457858));
#87345=DIRECTION('',(-0.85795490315098,0.,-0.513725008306187));
#87346=DIRECTION('center_axis',(-2.059703798478E-14,-1.,-5.56970842119747E-14));
#87347=DIRECTION('ref_axis',(-9.34353377149569E-31,5.56970842119747E-14,
-1.));
#87348=DIRECTION('center_axis',(-0.155084976578115,0.987363722815606,0.032581112741468));
#87349=DIRECTION('ref_axis',(-0.411450964096934,-0.0345726385626235,-0.910775953133657));
#87350=DIRECTION('center_axis',(0.147106613134512,0.987363722546665,-0.0589281237685905));
#87351=DIRECTION('ref_axis',(-0.346957789155213,-0.00428129112961885,-0.937870973583675));
#87352=DIRECTION('',(-0.513725012558988,0.,0.857954900604495));
#87353=DIRECTION('center_axis',(-0.150653237000636,-0.987363722747342,0.0491577174382569));
#87354=DIRECTION('ref_axis',(-0.141689365085258,-0.0276461757563053,-0.989525044042741));
#87355=DIRECTION('center_axis',(0.151947881918142,-0.987366232725817,-0.0449417807103583));
#87356=DIRECTION('ref_axis',(-0.067411075721759,0.0350112894293617,-0.997110804515992));
#87357=DIRECTION('',(-0.727460703861421,0.,-0.686149345505369));
#87358=DIRECTION('center_axis',(-1.2213395960312E-14,-1.,-8.82340075326601E-14));
#87359=DIRECTION('ref_axis',(-6.8312927238905E-32,8.82340075326601E-14,
-1.));
#87360=DIRECTION('center_axis',(-0.158463151597563,0.987363722911698,-0.00151929711346461));
#87361=DIRECTION('ref_axis',(-0.206041562667633,-0.0345726345089346,-0.977932312277589));
#87362=DIRECTION('center_axis',(0.156335146712928,0.987363722543225,-0.0259268453120185));
#87363=DIRECTION('ref_axis',(-0.137231572949308,-0.00428129286093705,-0.990529740046859));
#87364=DIRECTION('',(-0.686149350632658,0.,0.727460699025302));
#87365=DIRECTION('center_axis',(-0.157698504326823,-0.987363722731835,0.0156224443098921));
#87366=DIRECTION('ref_axis',(0.0743418882063654,-0.0276461754851028,-0.996849523568607));
#87367=DIRECTION('center_axis',(0.158056579374827,-0.987366232721537,-0.0112267625613302));
#87368=DIRECTION('ref_axis',(0.148514306471102,0.0350112882390293,-0.988290296658452));
#87369=DIRECTION('',(-0.562951250125031,0.,-0.826490102773569));
#87370=DIRECTION('center_axis',(1.17330831551609E-14,-1.,-1.47994441068827E-13));
#87371=DIRECTION('ref_axis',(4.1412559795609E-31,1.47994441068827E-13,-1.));
#87372=DIRECTION('center_axis',(-0.154431767114463,0.987363722967678,-0.0355486690793248));
#87373=DIRECTION('ref_axis',(0.00900211458576799,-0.0345726332720927,-0.999361643731446));
#87374=DIRECTION('center_axis',(0.158253623050005,0.987363722546468,0.00828674789823349));
#87375=DIRECTION('ref_axis',(0.078911438306756,-0.00428129000922054,-0.99687243690465));
#87376=DIRECTION('',(-0.826490105990566,0.,0.562951245402036));
#87377=DIRECTION('center_axis',(-0.157369964369938,-0.987363722781335,-0.018643316485744));
#87378=DIRECTION('ref_axis',(0.28689699642415,-0.0276461754527353,-0.957562427430002));
#87379=DIRECTION('center_axis',(0.156774723284306,-0.987366233007562,0.0230132148033821));
#87380=DIRECTION('ref_axis',(0.357495326215101,0.0350112783984714,-0.933258432653712));
#87381=DIRECTION('',(-0.372118820942155,0.,-0.928185101744593));
#87382=DIRECTION('center_axis',(1.73092801111523E-14,-1.,-5.68048588197779E-14));
#87383=DIRECTION('ref_axis',(-3.73483020556181E-31,5.68048588197779E-14,
-1.));
#87384=DIRECTION('center_axis',(-0.143179323934678,0.987363722859351,-0.0679158301055866));
#87385=DIRECTION('ref_axis',(0.223624860699663,-0.0345726379955593,-0.974061935597057));
#87386=DIRECTION('center_axis',(0.152772335844917,0.987363722537645,0.04211285809693));
#87387=DIRECTION('ref_axis',(0.291364638567275,-0.00428129121433651,-0.9566024868973));
#87388=DIRECTION('',(-0.928185103589145,0.,0.372118816341243));
#87389=DIRECTION('center_axis',(-0.149682979293308,-0.987363722808054,-0.0520373384455801));
#87390=DIRECTION('ref_axis',(0.486037120909077,-0.0276461734877023,-0.873500776296108));
#87391=DIRECTION('center_axis',(0.148162258618649,-0.987366232901802,0.0561771060693289));
#87392=DIRECTION('ref_axis',(0.549760259598465,0.0350112827382477,-0.834588441716785));
#87393=DIRECTION('',(-0.163886529631915,0.,-0.986479196640866));
#87394=DIRECTION('center_axis',(-1.45579821417781E-14,-1.,2.58779046247183E-14));
#87395=DIRECTION('ref_axis',(3.97422477312386E-31,-2.58779046247183E-14,
-1.));
#87396=DIRECTION('center_axis',(-0.125231975789399,0.987363722872469,-0.097107316898887));
#87397=DIRECTION('ref_axis',(0.427791161340583,-0.034572636188313,-0.90321617296518));
#87398=DIRECTION('center_axis',(0.140147584035429,0.987363722542533,0.0739698188181151));
#87399=DIRECTION('ref_axis',(0.490193954158814,-0.00428129181852567,-0.871602867048125));
#87400=DIRECTION('',(-0.986479197453234,0.,0.16388652474204));
#87401=DIRECTION('center_axis',(-0.134996984326904,-0.987363722815423,-0.0829981511282625));
#87402=DIRECTION('ref_axis',(0.66245069095475,-0.0276461728301328,-0.748595198476066));
#87403=DIRECTION('center_axis',(0.132621887525639,-0.987366233003682,0.0867142253223539));
#87404=DIRECTION('ref_axis',(0.716319015462737,0.035011278959132,-0.696894022382271));
#87405=DIRECTION('',(0.0520089118984746,0.,-0.998646620723836));
#87406=DIRECTION('center_axis',(-5.93418274472076E-14,-1.,6.64300732659738E-14));
#87407=DIRECTION('ref_axis',(-2.84771056551696E-30,-6.64300732659738E-14,
-1.));
#87408=DIRECTION('center_axis',(-0.10142891811791,0.987363722837423,-0.121758175881763));
#87409=DIRECTION('ref_axis',(0.611954418604463,-0.0345726379864004,-0.790137027516832));
#87410=DIRECTION('center_axis',(0.120969685025489,0.987363722554852,0.102368035477193));
#87411=DIRECTION('ref_axis',(0.666102343611793,-0.0042812889172255,-0.745848066565896));
#87412=DIRECTION('',(-0.998646620316722,0.,-0.0520089197156425));
#87413=DIRECTION('center_axis',(-0.113998684179924,-0.987363722714415,-0.110078058998048));
#87414=DIRECTION('ref_axis',(0.807888800879984,-0.0276461771046428,-0.588686142442813));
#87415=DIRECTION('center_axis',(0.110880275037949,-0.987366232725912,0.113196674333434));
#87416=DIRECTION('ref_axis',(0.84938348857533,0.035011289492792,-0.526613614468572));
#87417=DIRECTION('',(0.26547247756443,0.,-0.964118438603786));
#87418=DIRECTION('center_axis',(2.40783168670246E-14,-1.,-1.73734121000225E-14));
#87419=DIRECTION('ref_axis',(1.,2.40783168670246E-14,4.08008794519545E-31));
#87420=DIRECTION('center_axis',(-0.0728831555136991,0.987363722760243,-0.140715758248324));
#87421=DIRECTION('ref_axis',(0.767503369580905,-0.0345726406209256,-0.640111951304187));
#87422=DIRECTION('center_axis',(0.0961353783662722,0.987363722591744,0.12597963460872));
#87423=DIRECTION('ref_axis',(0.81086452814338,-0.0042812878077453,-0.585218239269352));
#87424=DIRECTION('',(-0.964118437085268,0.,-0.265472483079246));
#87425=DIRECTION('center_axis',(-0.0876699255670326,-0.987363722825506,
-0.132010844248598));
#87426=DIRECTION('ref_axis',(0.915550928733872,-0.0276461726499358,-0.401250776986605));
#87427=DIRECTION('center_axis',(0.0839540246621183,-0.98736623247613,0.134386177521815));
#87428=DIRECTION('ref_axis',(0.942731734454702,0.0350112977016713,-0.331709339460428));
#87429=DIRECTION('',(0.466522844039702,0.,-0.884509149748666));
#87430=DIRECTION('center_axis',(-1.6350089538668E-13,-1.,7.07466299821404E-14));
#87431=DIRECTION('ref_axis',(1.,-1.6350089538668E-13,-1.81849133261287E-30));
#87432=DIRECTION('center_axis',(-0.0409294619248677,0.987363722825902,-0.153093624929051));
#87433=DIRECTION('ref_axis',(0.887164714821792,-0.0345726379632342,-0.460155953432563));
#87434=DIRECTION('center_axis',(0.0668058915489451,0.987363722561016,0.143700564455411));
#87435=DIRECTION('ref_axis',(0.91771158853251,-0.00428129039750786,-0.397224257599745));
#87436=DIRECTION('',(-0.88450914743618,0.,-0.466522848424086));
#87437=DIRECTION('center_axis',(-0.0572418275556243,-0.987363722669453,
-0.147770945501514));
#87438=DIRECTION('ref_axis',(0.980402912820427,-0.0276461782575986,-0.195053370545015));
#87439=DIRECTION('center_axis',(0.053102164630045,-0.987366232647523,0.149291937957282));
#87440=DIRECTION('ref_axis',(0.99199889342554,0.0350112918481292,-0.121294702628058));
#87441=DIRECTION('',(0.64575912037299,0.,-0.763541196305152));
#87442=DIRECTION('center_axis',(-2.91477949413467E-14,-1.,5.65745894311796E-15));
#87443=DIRECTION('ref_axis',(1.,-2.91477949413467E-14,2.51222006692366E-32));
#87444=DIRECTION('center_axis',(-0.00706194962947178,0.987363722828334,
-0.158313005498612));
#87445=DIRECTION('ref_axis',(0.9653432251743,-0.0345726379281121,-0.258683571795296));
#87446=DIRECTION('center_axis',(0.0343526394950947,0.987363722496506,0.154702216071917));
#87447=DIRECTION('ref_axis',(0.981647474883865,-0.00428129655811406,-0.190656511963041));
#87448=DIRECTION('',(-0.763541191686731,0.,-0.645759125833779));
#87449=DIRECTION('',(0.794800418951332,0.,-0.606870903928329));
#87450=DIRECTION('',(-0.606870901804627,0.,-0.794800420572888));
#87451=DIRECTION('center_axis',(0.0100961397169233,-0.98736372283294,-0.158148496029187));
#87452=DIRECTION('ref_axis',(0.971690369534208,-0.0276461723068847,0.234634854425451));
#87453=DIRECTION('center_axis',(-0.0144918387531781,-0.987366232640024,
0.15779071345234));
#87454=DIRECTION('ref_axis',(0.951244135720145,0.0350112914715787,0.306445433523697));
#87455=DIRECTION('',(0.906677731515565,0.,-0.421824004975759));
#87456=DIRECTION('center_axis',(2.88293275590696E-14,-1.,7.10427075007399E-15));
#87457=DIRECTION('ref_axis',(1.,2.88293275590696E-14,-2.33857374721434E-31));
#87458=DIRECTION('center_axis',(0.0600646558953371,0.987363722772028,-0.146646227588495));
#87459=DIRECTION('ref_axis',(0.984740195112118,-0.0345726400867478,0.170562248718703));
#87460=DIRECTION('center_axis',(-0.0337801645468462,0.987363722504648,0.154828227287382));
#87461=DIRECTION('ref_axis',(0.970973710277041,-0.00428129541679956,0.239147913351531));
#87462=DIRECTION('',(-0.421824000481472,0.,-0.906677733606493));
#87463=DIRECTION('center_axis',(0.0438573487855876,-0.987363722845839,-0.15228070056808));
#87464=DIRECTION('ref_axis',(0.898533230833495,-0.0276461728542834,0.438033928154466));
#87465=DIRECTION('center_axis',(-0.0480733690119884,-0.987366232709415,
0.150986336127));
#87466=DIRECTION('ref_axis',(0.863127866602312,0.0350112889476249,0.503770280525527));
#87467=DIRECTION('',(0.976159801597288,0.,-0.217053085086444));
#87468=DIRECTION('center_axis',(1.06512422773008E-13,-1.,5.25425203349921E-14));
#87469=DIRECTION('ref_axis',(1.,1.06512422773008E-13,-2.10878361398876E-32));
#87470=DIRECTION('center_axis',(0.0901849798539102,0.987363722846681,-0.130305595486506));
#87471=DIRECTION('ref_axis',(0.925051675281031,-0.0345726381980344,0.37826463057995));
#87472=DIRECTION('center_axis',(-0.0662738964295295,0.987363722501191,0.143946692010062));
#87473=DIRECTION('ref_axis',(0.896863152081214,-0.00428129419318685,0.442287414425258));
#87474=DIRECTION('',(-0.217053076899258,0.,-0.976159803417742));
#87475=DIRECTION('center_axis',(0.0755678353822223,-0.987363722751612,-0.13929243069788));
#87476=DIRECTION('ref_axis',(0.783361677221614,-0.0276461756599869,0.620951021926784));
#87477=DIRECTION('center_axis',(-0.0794070357866266,-0.987366232591193,
0.137122009197124));
#87478=DIRECTION('ref_axis',(0.734652698085276,0.0350112936683274,0.677539388162558));
#87479=DIRECTION('',(0.999997725152046,0.,-0.00213300040646513));
#87480=DIRECTION('center_axis',(9.27271328152013E-14,-1.,7.42111278501564E-14));
#87481=DIRECTION('ref_axis',(1.,9.27271328152013E-14,1.68823144866391E-30));
#87482=DIRECTION('center_axis',(0.116088355864864,0.987363722833873,-0.107872018912356));
#87483=DIRECTION('ref_axis',(0.822108766551035,-0.0345726372684886,0.568279780312688));
#87484=DIRECTION('center_axis',(-0.0956687346786959,0.987363722549271,0.126334368240095));
#87485=DIRECTION('ref_axis',(0.780816270242319,-0.00428129210391877,0.624746046536347));
#87486=DIRECTION('',(-0.00213299544913877,0.,-0.99999772516262));
#87487=DIRECTION('center_axis',(0.103744855571448,-0.98736372273247,-0.11979100122437));
#87488=DIRECTION('ref_axis',(0.631561003133862,-0.0276461768120529,0.774833135731963));
#87489=DIRECTION('center_axis',(-0.107027725080779,-0.987366232739294,0.116846003398692));
#87490=DIRECTION('ref_axis',(0.571825985200744,0.0350112887521891,0.819627508267694));
#87491=DIRECTION('',(0.977076865850012,0.,0.212886820213741));
#87492=DIRECTION('center_axis',(5.59545188505727E-14,-1.,6.930727908743E-14));
#87493=DIRECTION('ref_axis',(1.90179785867072E-30,-6.930727908743E-14,-1.));
#87494=DIRECTION('center_axis',(0.136563569902686,0.987363722841023,-0.0803944661836259));
#87495=DIRECTION('ref_axis',(0.68072496630421,-0.0345726372125825,0.731722797927125));
#87496=DIRECTION('center_axis',(-0.120590206989186,0.987363722543446,0.10281479165691));
#87497=DIRECTION('ref_axis',(0.628259286757571,-0.00428129314207606,0.777992248760809));
#87498=DIRECTION('',(0.212886825057003,0.,-0.977076864794756));
#87499=DIRECTION('center_axis',(0.127070884961093,-0.987363722842759,-0.0946882728181883));
#87500=DIRECTION('ref_axis',(0.450229235832201,-0.0276461724272758,0.892484915475928));
#87501=DIRECTION('center_axis',(-0.129643916496959,-0.987366232921069,0.0911064048384507));
#87502=DIRECTION('ref_axis',(0.382261324293031,0.0350112812986391,0.923390757010035));
#87503=DIRECTION('',(0.90846897872148,0.,0.417952287588848));
#87504=DIRECTION('center_axis',(-3.97473170466724E-14,-1.,-7.97154810525488E-14));
#87505=DIRECTION('ref_axis',(1.34542241016887E-30,7.97154810525487E-14,
-1.));
#87506=DIRECTION('center_axis',(0.150653221823406,0.987363722937457,-0.0491577601331854));
#87507=DIRECTION('ref_axis',(0.507511223892755,-0.0345726343239725,0.860951270734168));
#87508=DIRECTION('center_axis',(-0.139873017737147,0.987363722559245,0.0744877055832257));
#87509=DIRECTION('ref_axis',(0.446325598059899,-0.00428128909263173,0.894860397537057));
#87510=DIRECTION('',(0.417952293183605,0.,-0.908468976147544));
#87511=DIRECTION('center_axis',(0.144455217576619,-0.98736372279966,-0.0651580310789709));
#87512=DIRECTION('ref_axis',(0.247845252571248,-0.0276461738326995,0.968405090780871));
#87513=DIRECTION('center_axis',(-0.146198094728699,-0.987366232569038,0.061106790785668));
#87514=DIRECTION('ref_axis',(0.174822551263119,0.035011294342318,0.983977278618937));
#87515=DIRECTION('',(0.797382090536838,0.,0.603474773036207));
#87516=DIRECTION('center_axis',(-7.22719159625212E-15,-1.,-2.8798758529663E-14));
#87517=DIRECTION('ref_axis',(1.69754332887121E-32,2.8798758529663E-14,-1.));
#87518=DIRECTION('center_axis',(0.157698499589171,0.987363722825349,-0.0156224862231097));
#87519=DIRECTION('ref_axis',(0.310566820979779,-0.03457263809742,0.949922619165108));
#87520=DIRECTION('center_axis',(-0.152615518808298,0.987363722561227,0.0426776614742487));
#87521=DIRECTION('ref_axis',(0.243522219297542,-0.00428129052954995,0.969885869192763));
#87522=DIRECTION('',(0.60347477560539,0.,-0.797382088592429));
#87523=DIRECTION('center_axis',(0.155084985266925,-0.98736372273477,-0.0325810738327332));
#87524=DIRECTION('ref_axis',(0.0338722990281305,-0.0276461769946432,0.9990437208932));
#87525=DIRECTION('center_axis',(-0.155916218266008,-0.987366232783829,0.0282498715023055));
#87526=DIRECTION('ref_axis',(-0.0407907327075091,0.0350112867431234,0.998554117675039));
#87527=DIRECTION('',(0.649010505773103,0.,0.760779444646174));
#87528=DIRECTION('center_axis',(0.,-1.,0.));
#87529=DIRECTION('ref_axis',(0.0292115385192369,0.,0.999573251951721));
#87530=DIRECTION('center_axis',(0.157369968982369,0.987363722822651,0.0186432753636022));
#87531=DIRECTION('ref_axis',(0.0991006546873935,-0.0345726382874032,0.994476642723387));
#87532=DIRECTION('center_axis',(-0.158221888564979,0.987363722509714,0.00887206011545954));
#87533=DIRECTION('ref_axis',(0.0293320137080374,-0.00428129435385591,0.999560555189373));
#87534=DIRECTION('center_axis',(-0.16378581394621,-0.986495109396061,0.00126739403137102));
#87535=DIRECTION('ref_axis',(0.0279022377807928,-0.00334831589290775,0.999605048960591));
#87536=DIRECTION('center_axis',(0.162023731906375,-0.986495109491454,-0.0239939419140432));
#87537=DIRECTION('ref_axis',(0.13673669353806,-0.00163604997374152,0.990606077096624));
#87538=DIRECTION('center_axis',(-0.159684138304561,-0.986495109470319,0.0364468786739426));
#87539=DIRECTION('ref_axis',(0.242135436420398,-0.00334830841955299,0.970236682083414));
#87540=DIRECTION('center_axis',(0.153077721675863,-0.986495109421554,-0.0582632835830904));
#87541=DIRECTION('ref_axis',(0.346490890519673,-0.00163604293581091,0.938051910157639));
#87542=DIRECTION('center_axis',(-0.148115812598509,-0.986495109422795,0.0699221362888171));
#87543=DIRECTION('ref_axis',(0.445046649327853,-0.00334831284885684,0.895501127147876));
#87544=DIRECTION('center_axis',(0.13697396453894,-0.986495109434819,-0.089808307520348));
#87545=DIRECTION('ref_axis',(0.540043558052671,-0.00163604532087848,0.841635478554415));
#87546=DIRECTION('center_axis',(-0.129621748464855,-0.986495109530296,0.100127924165659));
#87547=DIRECTION('ref_axis',(0.627147978031225,-0.00334830330694471,0.778892933923726));
#87548=DIRECTION('center_axis',(0.114465459146429,-0.986495109423811,-0.117153991589281));
#87549=DIRECTION('ref_axis',(0.708344388266892,-0.00163604390614199,0.705865108197834));
#87550=DIRECTION('center_axis',(-0.105066725885366,-0.986495109424266,0.125651829249456));
#87551=DIRECTION('ref_axis',(0.779924561865009,-0.00334830996305795,0.625864575303687));
#87552=DIRECTION('center_axis',(0.0866046722159151,-0.986495109483246,-0.13902168793398));
#87553=DIRECTION('ref_axis',(0.843523823647868,-0.00163604705472412,0.537089268454058));
#87554=DIRECTION('center_axis',(-0.0755988969195904,-0.98649510943077,0.145300398670181));
#87555=DIRECTION('ref_axis',(0.896232743138345,-0.00334831229899437,0.443571481197186));
#87556=DIRECTION('center_axis',(0.0546943551485009,-0.986495109420496,-0.154388881090361));
#87557=DIRECTION('ref_axis',(0.939261021775134,-0.00163604133811556,0.343199732433856));
#87558=DIRECTION('center_axis',(-0.0425961438623839,-0.986495109459446,
0.158154884656308));
#87559=DIRECTION('ref_axis',(0.970634076275854,-0.00334831006889112,0.240537478975321));
#87560=DIRECTION('center_axis',(0.0202265784150031,-0.986495109504033,-0.162537024859717));
#87561=DIRECTION('ref_axis',(0.991079418779179,-0.00163604856804703,0.133262556696951));
#87562=DIRECTION('center_axis',(-0.00760164204240845,-0.986495109429919,
0.163614223431558));
#87563=DIRECTION('ref_axis',(0.99964963868433,-0.00334830736092119,0.0262562129048713));
#87564=DIRECTION('center_axis',(-0.0151869653104653,-0.986495109510341,
-0.163085115804104));
#87565=DIRECTION('ref_axis',(0.996556043201398,-0.00163605039412049,-0.0829058266823295));
#87566=DIRECTION('center_axis',(0.0277482981921578,-0.986495109405202,0.161423142910355));
#87567=DIRECTION('ref_axis',(0.981922695164601,-0.0033483111612951,-0.189252766249411));
#87568=DIRECTION('center_axis',(-0.0498903778715741,-0.98649510947419,-0.15600752923926));
#87569=DIRECTION('ref_axis',(0.955434815240343,-0.00163604664715935,-0.295197623936948));
#87570=DIRECTION('center_axis',(0.0618007641807002,-0.986495109440824,0.151684094736456));
#87571=DIRECTION('ref_axis',(0.918282137943364,-0.00334830913939569,-0.395912495332078));
#87572=DIRECTION('center_axis',(-0.0822609769858708,-0.98649510948161,-0.141635202665852));
#87573=DIRECTION('ref_axis',(0.869638516258114,-0.00163604780339735,-0.49368631172838));
#87574=DIRECTION('center_axis',(0.0929634947864884,-0.986495109470967,0.134852466150781));
#87575=DIRECTION('ref_axis',(0.81170372863756,-0.003348307097733,-0.584059796386861));
#87576=DIRECTION('center_axis',(-0.110785141534113,-0.986495109446713,-0.120640173462175));
#87577=DIRECTION('ref_axis',(0.743178886612869,-0.00163604553725314,-0.66909077549153));
#87578=DIRECTION('center_axis',(0.119779353350238,-0.986495109452289,0.111715287842424));
#87579=DIRECTION('ref_axis',(0.667170953063073,-0.0033483085449882,-0.744897112505344));
#87580=DIRECTION('center_axis',(-0.134129119919762,-0.986495109493058,-0.0940041389292526));
#87581=DIRECTION('ref_axis',(0.581969039393171,-0.00163605002861843,-0.813209296877559));
#87582=DIRECTION('center_axis',(0.140994461083604,-0.986495109424135,0.0833544301522559));
#87583=DIRECTION('ref_axis',(0.491442007146395,-0.00334831305064004,-0.870903865195027));
#87584=DIRECTION('center_axis',(-0.151201364943228,-0.986495109443453,-0.0629725835856714));
#87585=DIRECTION('ref_axis',(0.393546966780992,-0.00163604463201623,-0.919303055741382));
#87586=DIRECTION('center_axis',(0.155616827764946,-0.986495109435589,0.0510960074373685));
#87587=DIRECTION('ref_axis',(0.292733778957593,-0.00334831188603403,-0.956188121378174));
#87588=DIRECTION('center_axis',(-0.161203605678199,-0.986495109504632,-0.0289964901288311));
#87589=DIRECTION('ref_axis',(0.186723073336949,-0.00163604993960994,-0.982411226128956));
#87590=DIRECTION('center_axis',(0.16296272405839,-0.986495109424208,0.0164483935260796));
#87591=DIRECTION('ref_axis',(0.0803376455401133,-0.00334831203061902,-0.996762083706848));
#87592=DIRECTION('center_axis',(-0.163668143673876,-0.986495109448053,0.00633543853423027));
#87593=DIRECTION('ref_axis',(-0.028831781957428,-0.0016360466685548,-0.99958293888024));
#87594=DIRECTION('center_axis',(0.162688663305374,-0.986495109493919,-0.0189683361550779));
#87595=DIRECTION('ref_axis',(-0.135814987330012,-0.00334830488654736,-0.990728559228478));
#87596=DIRECTION('center_axis',(-0.158479742471285,-0.986495109454043,0.0413711282114918));
#87597=DIRECTION('ref_axis',(-0.24303849268562,-0.00163604274440781,-0.970015265053721));
#87598=DIRECTION('center_axis',(0.154807463282918,-0.98649510940734,-0.0534981161098913));
#87599=DIRECTION('ref_axis',(-0.345617063849709,-0.00334831002481114,-0.938369668092423));
#87600=DIRECTION('center_axis',(-0.145881002803882,-0.986495109476937,0.0744723572812044));
#87601=DIRECTION('ref_axis',(-0.445880998647102,-0.00163604585829139,-0.895090754281046));
#87602=DIRECTION('center_axis',(0.139687636995712,-0.98649510943774,-0.08552638847733));
#87603=DIRECTION('ref_axis',(-0.539258470200199,-0.0033483099529629,-0.842133653963431));
#87604=DIRECTION('center_axis',(-0.12646103108995,-0.98649510948253,0.104091337693001));
#87605=DIRECTION('ref_axis',(-0.627874600291905,-0.0016360454288523,-0.778312796800641));
#87606=DIRECTION('center_axis',(0.118036173957979,-0.986495109402125,-0.113555540433086));
#87607=DIRECTION('ref_axis',(-0.707684749028207,-0.00334831214599302,-0.706520406498395));
#87608=DIRECTION('center_axis',(-0.101127883902599,-0.986495109422555,0.128843122372763));
#87609=DIRECTION('ref_axis',(-0.780509485663125,-0.00163604296041615,-0.625141796837578));
#87610=DIRECTION('center_axis',(0.0908654643575122,-0.986495109472117,-0.136274966060128));
#87611=DIRECTION('ref_axis',(-0.843020475033029,-0.0033483062137657,-0.537871051015562));
#87612=DIRECTION('center_axis',(-0.071066104503773,-0.986495109454203,0.147570348693763));
#87613=DIRECTION('ref_axis',(-0.89664861531436,-0.00163604600655692,-0.442739860424047));
#87614=DIRECTION('center_axis',(0.0594459877428719,-0.986495109509029,-0.152622322928339));
#87615=DIRECTION('ref_axis',(-0.938937501589155,-0.00334830299426047,-0.34407144167538));
#87616=DIRECTION('center_axis',(-0.0376813513430268,-0.986495109508868,
0.159397348397173));
#87617=DIRECTION('ref_axis',(-0.970861451591853,-0.00163605045407286,-0.239635901216558));
#87618=DIRECTION('center_axis',(0.0252468968154617,-0.986495109386897,-0.161833226986684));
#87619=DIRECTION('ref_axis',(-0.990950853825989,-0.00334831436270505,-0.134183434493504));
#87620=DIRECTION('center_axis',(-0.00253466500971984,-0.986495109498837,
0.163771103703207));
#87621=DIRECTION('ref_axis',(-0.999677885568108,-0.00163604943518171,-0.0253268325757907));
#87622=DIRECTION('center_axis',(-0.010132729717057,-0.986495109483762,-0.163476991509819));
#87623=DIRECTION('ref_axis',(-0.996628445590177,-0.00334830604890707,0.081978840484062));
#87624=DIRECTION('center_axis',(0.0327305358517654,-0.986495109457993,0.160487105520406));
#87625=DIRECTION('ref_axis',(-0.981750492616112,-0.00163604488853,0.190166489174997));
#87626=DIRECTION('center_axis',(-0.0450385505003737,-0.986495109440284,
-0.157476753901098));
#87627=DIRECTION('ref_axis',(-0.955704798411601,-0.00334830901293553,0.294307878113712));
#87628=DIRECTION('center_axis',(0.0664652997818561,-0.986495109455715,0.149698907627493));
#87629=DIRECTION('ref_axis',(-0.917917538204367,-0.00163604722328872,0.396767836910097));
#87630=DIRECTION('center_axis',(-0.0778384232825467,-0.986495109488177,
-0.144113076494802));
#87631=DIRECTION('ref_axis',(-0.870093457590691,-0.0033483064689008,0.492875404033988));
#87632=DIRECTION('center_axis',(0.0970922171638184,-0.986495109489498,0.131910956025336));
#87633=DIRECTION('ref_axis',(-0.811163778570785,-0.00163604589998996,0.584816764199334));
#87634=DIRECTION('center_axis',(-0.106998645562323,-0.986495109310941,-0.12401084288651));
#87635=DIRECTION('ref_axis',(-0.743797514851689,-0.00334832064433674,0.66839662300861));
#87636=DIRECTION('center_axis',(0.123179209311741,-0.986495109425282,0.107954997444934));
#87637=DIRECTION('ref_axis',(-0.666480903457418,-0.00163604240632611,0.745520307363809));
#87638=DIRECTION('center_axis',(-0.13115574995207,-0.986495109501473,-0.0981099800437549));
#87639=DIRECTION('ref_axis',(-0.582722423500651,-0.00334830642559605,0.812664362448365));
#87640=DIRECTION('center_axis',(0.143506484117382,-0.986495109477908,0.0789511747375405));
#87641=DIRECTION('ref_axis',(-0.49063412094358,-0.00163604904476048,0.871364150461472));
#87642=DIRECTION('center_axis',(-0.149180147807827,-0.986495109495363,-0.0676216122387367));
#87643=DIRECTION('ref_axis',(-0.394399880085478,-0.00334830475442072,0.918932817698787));
#87644=DIRECTION('center_axis',(0.157123550617762,-0.986495109493207,0.046255689242015));
#87645=DIRECTION('ref_axis',(-0.291845832604245,-0.00163604775031448,0.956463973884691));
#87646=DIRECTION('center_axis',(-0.160229045095317,-0.986495109390512,-0.0339713446369772));
#87647=DIRECTION('ref_axis',(-0.187635640680993,-0.00334831465490897,0.982232994322225));
#87648=DIRECTION('center_axis',(0.163393695261222,-0.986495109401722,0.0113973451016927));
#87649=DIRECTION('ref_axis',(-0.0794111591883371,-0.00163604091525733,0.996840604693894));
#87650=DIRECTION('center_axis',(0.156388912663533,0.986495110500922,0.048681669586124));
#87651=DIRECTION('ref_axis',(-0.0847582830594673,-0.0357022416614575,0.995761710146136));
#87652=DIRECTION('center_axis',(-0.160735557249259,0.986495110220615,-0.0314877459750204));
#87653=DIRECTION('ref_axis',(-0.18718085442266,0.000856146315673481,0.982325096264515));
#87654=DIRECTION('center_axis',(0.142267507527056,0.986495108892049,0.0811625309739932));
#87655=DIRECTION('ref_axis',(-0.296836013366402,-0.0357022594544976,0.954260829039202));
#87656=DIRECTION('center_axis',(-0.150208717742484,0.986495110197419,-0.0653049666621294));
#87657=DIRECTION('ref_axis',(-0.393975526808956,0.000856139022975812,0.919120531432945));
#87658=DIRECTION('center_axis',(0.121493832547411,0.986495110620511,0.109848283440242));
#87659=DIRECTION('ref_axis',(-0.495034021429636,-0.0357022382722387,0.868139774350626));
#87660=DIRECTION('center_axis',(-0.132658279393524,0.986495110257214,-0.09606861270445));
#87661=DIRECTION('ref_axis',(-0.582348345137894,0.000856146012755316,0.812938910330389));
#87662=DIRECTION('center_axis',(0.0950392389665278,0.986495110605003,0.133397675426094));
#87663=DIRECTION('ref_axis',(-0.670084790738196,-0.0357022400622654,0.741425467107709));
#87664=DIRECTION('center_axis',(-0.108904892632645,0.986495110251071,-0.122340188864495));
#87665=DIRECTION('ref_axis',(-0.743491199728451,0.00085614329103587,0.668745170408739));
#87666=DIRECTION('center_axis',(0.0641407206135473,0.986495110682393,0.150709537053595));
#87667=DIRECTION('ref_axis',(-0.813803139234317,-0.0357022364465081,0.580042930208694));
#87668=DIRECTION('center_axis',(-0.0800592318971177,0.986495110224998,-0.142891276466454));
#87669=DIRECTION('ref_axis',(-0.869869231963275,0.000856144207940989,0.493281650075002));
#87670=DIRECTION('center_axis',(0.0302430480138401,0.986495110576137,0.160974391926818));
#87671=DIRECTION('ref_axis',(-0.919468959214345,-0.0357022389103626,0.391538226969062));
#87672=DIRECTION('center_axis',(-0.0474700944979826,0.986495110139844,-0.156760925611356));
#87673=DIRECTION('ref_axis',(-0.955573145865708,0.000856140779035256,0.294752828524647));
#87674=DIRECTION('center_axis',(-0.00506877555079224,0.986495108775113,
0.16371227161454));
#87675=DIRECTION('ref_axis',(-0.982141430286934,-0.0357022625894564,0.184725632655374));
#87676=DIRECTION('center_axis',(-0.0126613009637376,0.98649511023473,-0.16330060912585));
#87677=DIRECTION('ref_axis',(-0.996595522149375,0.000856144484601801,0.0824416899901725));
#87678=DIRECTION('center_axis',(-0.0401435441044833,0.986495110627201,0.158795127681416));
#87679=DIRECTION('ref_axis',(-0.998890061000584,-0.0357022375529674,-0.0307245222576411));
#87680=DIRECTION('center_axis',(0.0227395142084494,0.986495110181865,-0.162204537793593));
#87681=DIRECTION('ref_axis',(-0.991018199204409,0.000856141725757606,-0.13372432788014));
#87682=DIRECTION('center_axis',(-0.0733412699600103,0.986495110625005,0.146452909952692));
#87683=DIRECTION('ref_axis',(-0.968931701865205,-0.0357022384448084,-0.244738038095078));
#87684=DIRECTION('center_axis',(0.0570770554642903,0.986495110139408,-0.153523963636179));
#87685=DIRECTION('ref_axis',(-0.939101966597582,0.000856138904126028,-0.343637546491547));
#87686=DIRECTION('center_axis',(-0.103109656079224,0.986495108998291,0.127262715457723));
#87687=DIRECTION('ref_axis',(-0.893667172076722,-0.0357022550788138,-0.447307874438492));
#87688=DIRECTION('center_axis',(0.0887457420158007,0.98649511016544,-0.137664777244365));
#87689=DIRECTION('ref_axis',(-0.843274368614031,0.000856141453340625,-0.537482656706633));
#87690=DIRECTION('center_axis',(-0.128056731448259,0.986495108989023,0.102121855993337));
#87691=DIRECTION('ref_axis',(-0.776615760027788,-0.0357022549333386,-0.62896208969153));
#87692=DIRECTION('center_axis',(0.116264778148262,0.986495110253181,-0.115368534742798));
#87693=DIRECTION('ref_axis',(-0.708016200426445,0.000856148759243582,-0.706195671852358));
#87694=DIRECTION('center_axis',(-0.14701601859467,0.986495108895636,0.0722058889673023));
#87695=DIRECTION('ref_axis',(-0.623250656744172,-0.0357022582606523,-0.781206738080931));
#87696=DIRECTION('center_axis',(0.138347393324671,0.986495110212549,-0.0876777981418294));
#87697=DIRECTION('ref_axis',(-0.539651979497943,0.000856141284190815,-0.841887764518557));
#87698=DIRECTION('center_axis',(-0.159100984330672,0.986495110516033,0.038913670001308));
#87699=DIRECTION('ref_axis',(-0.440743048472606,-0.0357022410037261,-0.89692302635755));
#87700=DIRECTION('center_axis',(0.153961042610626,0.986495110180795,-0.0558873415688195));
#87701=DIRECTION('ref_axis',(-0.346054235065791,0.000856139963462675,-0.938214119173972));
#87702=DIRECTION('center_axis',(-0.163746580379322,0.98649511053951,0.00380188055029804));
#87703=DIRECTION('ref_axis',(-0.237626784347645,-0.0357022419978828,-0.970700191241829));
#87704=DIRECTION('center_axis',(0.162375645555585,0.986495110193823,-0.0214836517865166));
#87705=DIRECTION('ref_axis',(-0.136275375117657,0.000856141339044354,-0.990670625969373));
#87706=DIRECTION('center_axis',(-0.160735568247923,0.986495110466998,-0.0314876821110047));
#87707=DIRECTION('ref_axis',(-0.0233993533168982,-0.0357022441336381,-0.999088494593033));
#87708=DIRECTION('center_axis',(0.163197743665279,0.986495110172426,0.0139245850371073));
#87709=DIRECTION('ref_axis',(0.0798755669367271,0.000856138430815477,-0.996804474725873));
#87710=DIRECTION('center_axis',(-0.150208740918371,0.986495110672989,-0.0653049061710207));
#87711=DIRECTION('ref_axis',(0.191922203698308,-0.0357022365974855,-0.980760530419899));
#87712=DIRECTION('center_axis',(0.156388896590614,0.986495110143671,0.0486817284594198));
#87713=DIRECTION('ref_axis',(0.292291616845161,0.000856140246125589,-0.956328854393676));
#87714=DIRECTION('center_axis',(-0.132658318227324,0.986495110593608,-0.0960685556256756));
#87715=DIRECTION('ref_axis',(0.398269690649453,-0.0357022399347559,-0.916573294163446));
#87716=DIRECTION('center_axis',(0.142267476719927,0.986495110210636,0.0811625689480725));
#87717=DIRECTION('ref_axis',(0.491040435894112,0.000856143201521635,-0.871136359782864));
#87718=DIRECTION('center_axis',(-0.108904939865473,0.98649511054227,-0.122340144470624));
#87719=DIRECTION('ref_axis',(0.585994532833131,-0.0357022411327852,-0.809528107892356));
#87720=DIRECTION('center_axis',(0.121493790101187,0.986495110177345,0.109848334366241));
#87721=DIRECTION('ref_axis',(0.666828750295423,0.000856141722682205,-0.745210496974375));
#87722=DIRECTION('center_axis',(-0.0800592794798436,0.986495108881712,-0.142891259080559));
#87723=DIRECTION('ref_axis',(0.746318920951353,-0.0357022584185192,-0.66463028592882));
#87724=DIRECTION('center_axis',(0.0950391876824411,0.986495110247087,0.133397714610294));
#87725=DIRECTION('ref_axis',(0.81143689427034,0.000856141536668781,-0.584439418279238));
#87726=DIRECTION('center_axis',(-0.0474701529820085,0.986495110541533,-0.156760905373482));
#87727=DIRECTION('ref_axis',(0.871746264002991,-0.0357022413027112,-0.488655094276924));
#87728=DIRECTION('center_axis',(0.0641406633761717,0.986495110174397,0.150709564738503));
#87729=DIRECTION('ref_axis',(0.918103148850275,0.00085613707607792,-0.396340604910116));
#87730=DIRECTION('center_axis',(-0.0126613729171963,0.986495110734072,-0.163300600530505));
#87731=DIRECTION('ref_axis',(0.956411720781313,-0.0357022349766519,-0.289830934804756));
#87732=DIRECTION('center_axis',(0.0302429834584108,0.986495110181741,0.160974406472113));
#87733=DIRECTION('ref_axis',(0.981839921951651,0.000856142423214422,-0.189709342632688));
#87734=DIRECTION('center_axis',(0.022739465422101,0.986495108959912,-0.162204552064631));
#87735=DIRECTION('ref_axis',(0.996356429529177,-0.0357022555345247,-0.0774545949935659));
#87736=DIRECTION('center_axis',(-0.00506882451442394,0.98649511023803,0.163712261283324));
#87737=DIRECTION('ref_axis',(0.999666951069067,0.000856147178261841,0.0257925173700458));
#87738=DIRECTION('center_axis',(0.0570769958324413,0.986495110611179,-0.153523982774619));
#87739=DIRECTION('ref_axis',(0.989712619250393,-0.0357022389867386,0.138543427949004));
#87740=DIRECTION('center_axis',(-0.040143616149589,0.986495110223746,0.158795111974751));
#87741=DIRECTION('ref_axis',(0.970750664504711,0.000856148292627332,0.240088347017847));
#87742=DIRECTION('center_axis',(0.0887456881072519,0.98649511049776,-0.137664809615175));
#87743=DIRECTION('ref_axis',(0.936790945359738,-0.0357022412121723,0.348063319906647));
#87744=DIRECTION('center_axis',(-0.0733413333034938,0.986495110181623,0.146452881217863));
#87745=DIRECTION('ref_axis',(0.896443156372571,0.000856145515749334,0.443157911367537));
#87746=DIRECTION('center_axis',(0.116264744835295,0.986495108930328,-0.115368579626017));
#87747=DIRECTION('ref_axis',(0.840065968072642,-0.0357022576022493,0.541308154463128));
#87748=DIRECTION('center_axis',(-0.103109690306789,0.986495110153459,0.127262678771715));
#87749=DIRECTION('ref_axis',(0.780218961813407,0.000856140399447746,0.6255059061675));
#87750=DIRECTION('center_axis',(0.138347353699895,0.986495110711692,-0.087677855049969));
#87751=DIRECTION('ref_axis',(0.704060443534308,-0.0357022349542924,0.709242019531797));
#87752=DIRECTION('center_axis',(-0.128056758497583,0.986495110176505,0.102121810603498));
#87753=DIRECTION('ref_axis',(0.627512595764402,0.000856142745096334,0.778605939597575));
#87754=DIRECTION('center_axis',(0.153961016969757,0.986495110699521,-0.0558874030491539));
#87755=DIRECTION('ref_axis',(0.535133832406667,-0.0357022359846592,0.844012518721997));
#87756=DIRECTION('center_axis',(-0.147016033672443,0.986495110214052,0.0722058402553995));
#87757=DIRECTION('ref_axis',(0.44546443861938,0.000856144275045226,0.895299224249916));
#87758=DIRECTION('center_axis',(0.162375647399458,0.98649510885926,-0.021483699131286));
#87759=DIRECTION('ref_axis',(0.341184955381354,-0.0357022593273061,0.939317930681805));
#87760=DIRECTION('center_axis',(-0.159101001719445,0.986495110234289,0.0389136060486129));
#87761=DIRECTION('ref_axis',(0.242586858202287,0.000856144391280358,0.970129312640498));
#87762=DIRECTION('center_axis',(0.163197746490851,0.986495110577267,0.0139245232397132));
#87763=DIRECTION('ref_axis',(0.131282652802152,-0.0357022392364338,0.990701880076309));
#87764=DIRECTION('center_axis',(-0.16374658378085,0.986495110232372,0.00380181374105046));
#87765=DIRECTION('ref_axis',(0.0283661888251914,0.000856146182459187,0.999597232061618));
#87766=DIRECTION('center_axis',(0.158420667740754,0.98736372234608,0.00397137601677981));
#87767=DIRECTION('ref_axis',(0.100692121386749,-0.0201568010854275,0.994713426098511));
#87768=DIRECTION('',(-0.603992234724004,0.,0.796990200939199));
#87769=DIRECTION('center_axis',(-0.155915203883767,0.987363722011716,0.028343070635579));
#87770=DIRECTION('ref_axis',(0.241038780754158,0.0102046916675105,0.970461833582609));
#87771=DIRECTION('',(-0.796990199392668,0.,-0.603992236764708));
#87772=DIRECTION('center_axis',(5.40637229578749E-15,-1.,2.16025825271405E-14));
#87773=DIRECTION('ref_axis',(2.85199720979946E-32,-2.16025825271405E-14,
-1.));
#87774=DIRECTION('center_axis',(-0.158340230226139,-0.987363723437772,0.00642254863998973));
#87775=DIRECTION('ref_axis',(0.165682556882615,-0.020156456391398,0.985973127225373));
#87776=DIRECTION('center_axis',(0.149874468456674,-0.987363722435678,-0.0514832334142992));
#87777=DIRECTION('ref_axis',(0.245294997189495,-0.0133103743988677,0.969357105656717));
#87778=DIRECTION('center_axis',(0.155570608715075,0.987363722361946,-0.0301772342600132));
#87779=DIRECTION('ref_axis',(0.312171979328333,-0.0201568001148959,0.949811749101557));
#87780=DIRECTION('',(-0.418541898467443,0.,0.908197489110859));
#87781=DIRECTION('center_axis',(-0.146177069397483,0.987363722011113,0.0611975885041637));
#87782=DIRECTION('ref_axis',(0.444024037449279,0.0102046886099544,0.895956761511187));
#87783=DIRECTION('',(-0.908197487535576,0.,-0.418541901885662));
#87784=DIRECTION('center_axis',(9.9238909863824E-15,-1.,1.99353159073878E-14));
#87785=DIRECTION('ref_axis',(-1.38974827776255E-31,-1.99353159073878E-14,
-1.));
#87786=DIRECTION('center_axis',(-0.153257664657612,-0.987363723478468,0.0403108643225515));
#87787=DIRECTION('ref_axis',(0.373764067895711,-0.0201564538811349,0.927304771322238));
#87788=DIRECTION('center_axis',(0.13530311636008,-0.987363722522325,-0.0824981584649473));
#87789=DIRECTION('ref_axis',(0.447943259549841,-0.013310367689315,0.893962902102676));
#87790=DIRECTION('center_axis',(0.145446240991836,0.987363722371625,-0.0629147894043416));
#87791=DIRECTION('ref_axis',(0.509055019458456,-0.0201567997961947,0.8604979317733));
#87792=DIRECTION('',(-0.21352100493591,0.,0.976938473216793));
#87793=DIRECTION('center_axis',(-0.129603856677957,0.987363722010123,0.091190574033264));
#87794=DIRECTION('ref_axis',(0.626247222002202,0.0102046859892758,0.779557747263399));
#87795=DIRECTION('',(-0.976938472070386,0.,-0.21352101018115));
#87796=DIRECTION('center_axis',(-1.86365060963677E-14,-1.,-2.31145281227288E-14));
#87797=DIRECTION('ref_axis',(2.57068877191084E-31,2.31145281227288E-14,
-1.));
#87798=DIRECTION('center_axis',(-0.141008943747592,-0.987363723371414,0.0723142831902936));
#87799=DIRECTION('ref_axis',(0.564368787726565,-0.0201564581084856,0.82527667399277));
#87800=DIRECTION('center_axis',(0.11440513999799,-0.987363722521747,-0.109655567072713));
#87801=DIRECTION('ref_axis',(0.629646193568477,-0.0133103666202319,0.776767986637686));
#87802=DIRECTION('center_axis',(0.128520967516312,0.987363722411292,-0.0927105203026545));
#87803=DIRECTION('ref_axis',(0.682135215609266,-0.0201567981133334,0.73094818634122));
#87804=DIRECTION('',(0.00148388924556568,0.,0.999998899035747));
#87805=DIRECTION('center_axis',(-0.10697051813911,0.987363721991061,0.116919582384686));
#87806=DIRECTION('ref_axis',(0.779187780646539,0.0102046930062637,0.626707480992344));
#87807=DIRECTION('',(-0.999998899039541,0.,0.00148388668928533));
#87808=DIRECTION('center_axis',(-2.89621690381482E-14,-1.,-2.32097817301061E-14));
#87809=DIRECTION('ref_axis',(1.,-2.89621690381482E-14,1.79017293909041E-31));
#87810=DIRECTION('center_axis',(-0.122166803468733,-0.987363723230526,0.100936366977346));
#87811=DIRECTION('ref_axis',(0.728584246530449,-0.0201564625201907,0.684659559727556));
#87812=DIRECTION('center_axis',(0.0881577081516817,-0.987363722547253,-0.131685602444131));
#87813=DIRECTION('ref_axis',(0.781907570454382,-0.0133103640089616,0.623252264717966));
#87814=DIRECTION('center_axis',(0.105586199074021,0.987363722361599,-0.118171207700302));
#87815=DIRECTION('ref_axis',(0.823319527157923,-0.0201568003226023,0.567220115652829));
#87816=DIRECTION('',(0.216419402668491,0.,0.976300487631043));
#87817=DIRECTION('center_axis',(-0.0793353484309201,0.987363722023703,0.137181569173284));
#87818=DIRECTION('ref_axis',(0.895694387222186,0.0102046883173652,0.444553066612996));
#87819=DIRECTION('',(-0.976300488927256,0.,0.21641939682108));
#87820=DIRECTION('center_axis',(-1.33097866516519E-14,-1.,-6.57645588484366E-15));
#87821=DIRECTION('ref_axis',(1.,-1.33097866516519E-14,-6.73429246899876E-32));
#87822=DIRECTION('center_axis',(-0.0976122735306192,-0.987363723326527,
0.124838783697059));
#87823=DIRECTION('ref_axis',(0.858731920403179,-0.0201564599673544,0.512028520692209));
#87824=DIRECTION('center_axis',(0.0577881148582087,-0.987363722518273,-0.147558168991057));
#87825=DIRECTION('ref_axis',(0.897607820319684,-0.0133103672525045,0.440593957090368));
#87826=DIRECTION('center_axis',(0.0777143295770213,0.987363722455775,-0.138106345099239));
#87827=DIRECTION('ref_axis',(0.926006332830839,-0.0201567935764935,0.376969461932788));
#87828=DIRECTION('',(0.421235379219816,0.,0.906951352219918));
#87829=DIRECTION('center_axis',(-0.0479905531030168,0.987363722018253,0.151029094068421));
#87830=DIRECTION('ref_axis',(0.970319318195053,0.0102046915939821,0.241611847819925));
#87831=DIRECTION('',(-0.90695135278839,0.,0.421235377995853));
#87832=DIRECTION('center_axis',(-5.76494193762726E-14,-1.,-1.42459652129957E-14));
#87833=DIRECTION('ref_axis',(1.,-5.76494193762726E-14,1.74390848177407E-32));
#87834=DIRECTION('center_axis',(-0.0684934961056325,-0.987363723561827,
0.14290387813265));
#87835=DIRECTION('ref_axis',(0.948726241396025,-0.0201564508034618,0.315455601277865));
#87836=DIRECTION('center_axis',(0.0247164153401507,-0.987363722501066,-0.156531077749984));
#87837=DIRECTION('ref_axis',(0.971336925194111,-0.0133103682563698,0.237333966914409));
#87838=DIRECTION('center_axis',(0.0462086345200734,0.987363722388363,-0.151583778179547));
#87839=DIRECTION('ref_axis',(0.985394110347962,-0.0201567982226793,0.169092136945984));
#87840=DIRECTION('',(0.606354862831809,0.,0.795194177745422));
#87841=DIRECTION('',(-0.795194177911868,0.,0.606354862613527));
#87842=DIRECTION('',(0.763121866258984,0.,0.646254607130507));
#87843=DIRECTION('center_axis',(0.019860431055013,0.987363722013889,0.157221002824649));
#87844=DIRECTION('ref_axis',(0.982088143785789,0.0102046850143543,-0.188145534730805));
#87845=DIRECTION('',(-0.646254610502266,0.,0.763121863403588));
#87846=DIRECTION('center_axis',(7.28786518901112E-15,-1.,-1.40963438107777E-15));
#87847=DIRECTION('ref_axis',(1.,7.28786518901112E-15,2.85675081165747E-33));
#87848=DIRECTION('center_axis',(-0.00215923198134159,-0.98736372357585,
0.158455719630701));
#87849=DIRECTION('ref_axis',(0.993496985649308,-0.0201564503692403,-0.112060059852969));
#87850=DIRECTION('center_axis',(-0.0432936835167879,-0.987363722495348,
-0.15244191178176));
#87851=DIRECTION('ref_axis',(0.981215463559103,-0.013310369158375,-0.192455314671647));
#87852=DIRECTION('center_axis',(-0.0217105580192843,0.987363722442619,-0.156976212448723));
#87853=DIRECTION('ref_axis',(0.965319418559905,-0.0201567957597029,-0.260292381248219));
#87854=DIRECTION('',(0.884206138072509,0.,0.467096890799863));
#87855=DIRECTION('center_axis',(0.0531939704811207,0.987363722010318,0.14927585860542));
#87856=DIRECTION('ref_axis',(0.918681740755121,0.0102046879671231,-0.394866716179819));
#87857=DIRECTION('',(-0.467096893063886,0.,0.884206136876501));
#87858=DIRECTION('center_axis',(6.8144492270499E-15,-1.,-2.94335350051688E-15));
#87859=DIRECTION('ref_axis',(1.,6.8144492270499E-15,-2.58910475522156E-32));
#87860=DIRECTION('center_axis',(0.0319545399416091,-0.987363723398425,0.155215286276574));
#87861=DIRECTION('ref_axis',(0.946179978578477,-0.0201564559808906,-0.323012639720991));
#87862=DIRECTION('center_axis',(-0.075052005512317,-0.987363722501073,-0.139571042689389));
#87863=DIRECTION('ref_axis',(0.916902987768194,-0.0133103685324798,-0.398888136087411));
#87864=DIRECTION('center_axis',(-0.0549482178462372,0.98736372235751,-0.148639069991186));
#87865=DIRECTION('ref_axis',(0.886795619052634,-0.0201568012751914,-0.461722030437587));
#87866=DIRECTION('',(0.96394591401818,0.,0.266098242849622));
#87867=DIRECTION('center_axis',(0.0840402245882483,0.987363722020711,0.134350739069664));
#87868=DIRECTION('ref_axis',(0.812318799598595,0.0102046851148157,-0.583124371142559));
#87869=DIRECTION('',(-0.266098244580434,0.,0.963945913540387));
#87870=DIRECTION('center_axis',(-1.20447943868174E-14,-1.,8.67888936384583E-15));
#87871=DIRECTION('ref_axis',(1.,-1.20447943868174E-14,-1.00100324375465E-31));
#87872=DIRECTION('center_axis',(0.0645741589563264,-0.987363723387579,0.144717157701843));
#87873=DIRECTION('ref_axis',(0.85462064542993,-0.020156456556257,-0.51886151299169));
#87874=DIRECTION('center_axis',(-0.103300975920256,-0.987363722552581,-0.120173989536141));
#87875=DIRECTION('ref_axis',(0.809717148348452,-0.0133103638859008,-0.586669390614233));
#87876=DIRECTION('center_axis',(-0.0856165659527258,0.987363722399913,-0.133351727859263));
#87877=DIRECTION('ref_axis',(0.766806244018913,-0.0201567998990961,-0.641562068354602));
#87878=DIRECTION('',(0.99861265071478,0.,0.0526571346770876));
#87879=DIRECTION('center_axis',(0.110956844469907,0.987363721975615,0.113143533583412));
#87880=DIRECTION('ref_axis',(0.667972736265682,0.0102046905761982,-0.744115775868233));
#87881=DIRECTION('',(-0.0526571372340356,0.,0.998612650579951));
#87882=DIRECTION('center_axis',(0.,-1.,0.));
#87883=DIRECTION('ref_axis',(0.,0.,-1.));
#87884=DIRECTION('center_axis',(0.0941743618905338,-0.987363723370125,0.127452215889697));
#87885=DIRECTION('ref_axis',(0.72310020247839,-0.0201564567588206,-0.69044899480457));
#87886=DIRECTION('center_axis',(-0.126719716985301,-0.9873637224691,-0.0951577263238632));
#87887=DIRECTION('ref_axis',(0.664669831879971,-0.0133103712189968,-0.747018640066406));
#87888=DIRECTION('center_axis',(-0.112281578563455,0.987363722364124,-0.111829007303832));
#87889=DIRECTION('ref_axis',(0.61096185800018,-0.0201567995340252,-0.791403381027345));
#87890=DIRECTION('',(0.986585369800577,0.,-0.1632461579807));
#87891=DIRECTION('center_axis',(0.132685249336737,0.987363721998344,0.0866458602013091));
#87892=DIRECTION('ref_axis',(0.492393009084558,0.0102046921590675,-0.870313155629968));
#87893=DIRECTION('',(0.16324615825273,0.,0.986585369755565));
#87894=DIRECTION('center_axis',(-2.91495530570904E-14,-1.,5.1736898213001E-14));
#87895=DIRECTION('ref_axis',(-3.85548631941165E-31,-5.1736898213001E-14,
-1.));
#87896=DIRECTION('center_axis',(0.11937107525839,-0.987363723316579,0.104227751918948));
#87897=DIRECTION('ref_axis',(0.557768397564044,-0.0201564591618209,-0.829751849550753));
#87898=DIRECTION('center_axis',(-0.144213177987697,-0.9873637224976,-0.0656919994395904));
#87899=DIRECTION('ref_axis',(0.488543295503504,-0.0133103699190332,-0.872438125296685));
#87900=DIRECTION('center_axis',(-0.133696428325244,0.987363722375555,-0.0850772871556274));
#87901=DIRECTION('ref_axis',(0.426549576840701,-0.0201567997556429,-0.904239548969536));
#87902=DIRECTION('',(0.928426452468147,0.,-0.37151624777042));
#87903=DIRECTION('center_axis',(0.148209440985322,0.987363721996551,0.056096720830506));
#87904=DIRECTION('ref_axis',(0.293789531228519,0.0102046913623145,-0.955815659850123));
#87905=DIRECTION('',(0.371516244401546,0.,0.928426453816225));
#87906=DIRECTION('center_axis',(-4.33653723296519E-15,-1.,1.41984026416763E-14));
#87907=DIRECTION('ref_axis',(-1.11977916956078E-32,-1.41984026416763E-14,
-1.));
#87908=DIRECTION('center_axis',(0.138986131053651,-0.987363723276318,0.0761297138617028));
#87909=DIRECTION('ref_axis',(0.366355960441036,-0.0201564609952252,-0.930256430953032));
#87910=DIRECTION('center_axis',(-0.154963392508389,-0.987363722477634,-0.0331545851640646));
#87911=DIRECTION('ref_axis',(0.289573017145001,-0.0133103715252556,-0.957063373947306));
#87912=DIRECTION('center_axis',(-0.14885978163699,0.987363722346439,-0.0543474489297465));
#87913=DIRECTION('ref_axis',(0.222192310197494,-0.0201568014481594,-0.974794481234111));
#87914=DIRECTION('',(0.826855347492317,0.,-0.562414646256087));
#87915=DIRECTION('center_axis',(0.156803523203429,0.987363721998679,0.0229245630690647));
#87916=DIRECTION('ref_axis',(0.0814487825518928,0.0102046924843558,-0.996625285687712));
#87917=DIRECTION('',(0.562414644138879,0.,0.82685534893241));
#87918=DIRECTION('center_axis',(1.1829145367693E-15,-1.,-1.47986791925367E-14));
#87919=DIRECTION('ref_axis',(5.07998996178402E-33,1.47986791925367E-14,
-1.));
#87920=DIRECTION('center_axis',(0.152102351271975,-0.987363723473821,0.0444719271614001));
#87921=DIRECTION('ref_axis',(0.157813128528872,-0.0201564541640345,-0.987263254567627));
#87922=DIRECTION('center_axis',(-0.158467690465378,-0.987363722444021,0.000933102381670069));
#87923=DIRECTION('ref_axis',(0.0770626253115131,-0.0133103745061621,-0.996937403105432));
#87924=DIRECTION('center_axis',(-0.157062618092258,0.987363722440241,-0.0210763755649886));
#87925=DIRECTION('ref_axis',(0.00744557762538648,-0.0201567941043528,-0.999769106856808));
#87926=DIRECTION('',(0.686621405562476,0.,-0.727015161756211));
#87927=DIRECTION('center_axis',(0.158065647204977,0.987363722018725,-0.0113195236208035));
#87928=DIRECTION('ref_axis',(-0.13470042036027,0.0102046916006389,-0.990833821094184));
#87929=DIRECTION('',(0.727015160077817,0.,0.686621407339609));
#87930=DIRECTION('center_axis',(4.05203985556794E-15,-1.,2.94139719068973E-14));
#87931=DIRECTION('ref_axis',(4.21776386687562E-32,-2.94139719068973E-14,
-1.));
#87932=DIRECTION('center_axis',(0.158106432646324,-0.987363723454409,0.0107346896601449));
#87933=DIRECTION('ref_axis',(-0.0581088698147696,-0.020156454815659,-0.998106746083862));
#87934=DIRECTION('center_axis',(-0.154562215242167,-0.987363722455789,0.0349771525096206));
#87935=DIRECTION('ref_axis',(-0.139051128634763,-0.0133103707271488,-0.990195747141193));
#87936=DIRECTION('center_axis',(-0.1579213804655,0.987363722325964,0.0131801906847718));
#87937=DIRECTION('ref_axis',(-0.207649299429248,-0.0201568019413548,-0.977995639960649));
#87938=DIRECTION('',(0.514281808963848,0.,-0.857621257297691));
#87939=DIRECTION('center_axis',(0.151936795015725,0.987363722024644,-0.0450343285726719));
#87940=DIRECTION('ref_axis',(-0.344551184645105,0.0102046842600743,-0.93871206745136));
#87941=DIRECTION('',(0.85762125598085,0.,0.514281811159825));
#87942=DIRECTION('center_axis',(2.57010997481761E-15,-1.,6.9638051943949E-15));
#87943=DIRECTION('ref_axis',(-1.02824123169305E-32,-6.9638051943949E-15,
-1.));
#87944=DIRECTION('center_axis',(0.156717633007204,-0.987363723457172,-0.0235044911752826));
#87945=DIRECTION('ref_axis',(-0.271313764309302,-0.0201564546398896,-0.962279875417057));
#87946=DIRECTION('center_axis',(-0.143429583031234,-0.98736372249374,0.067385712245179));
#87947=DIRECTION('ref_axis',(-0.348663004676317,-0.0133103695970175,-0.937153639074871));
#87948=DIRECTION('center_axis',(-0.151395913459791,0.987363722414849,0.0468204767892139));
#87949=DIRECTION('ref_axis',(-0.413034727711651,-0.0201567986262182,-0.910492184026477));
#87950=DIRECTION('',(0.317894965895107,0.,-0.948125936075239));
#87951=DIRECTION('center_axis',(0.138703549433781,0.987363722008433,-0.0766433678547938));
#87952=DIRECTION('ref_axis',(-0.538291114974621,0.0102046874629256,-0.842697181609838));
#87953=DIRECTION('',(0.948125934970735,0.,0.317894969189305));
#87954=DIRECTION('center_axis',(-8.01406900089253E-15,-1.,-1.24969952536102E-14));
#87955=DIRECTION('ref_axis',(5.5988101841633E-32,1.24969952536102E-14,-1.));
#87956=DIRECTION('center_axis',(0.148000890389814,-0.98736372348648,-0.0566446289310448));
#87957=DIRECTION('ref_axis',(-0.471832327136548,-0.0201564532152196,-0.881457867661689));
#87958=DIRECTION('center_axis',(-0.125590341172455,-0.987363722487913,0.096643394595795));
#87959=DIRECTION('ref_axis',(-0.541971788445821,-0.0133103722979742,-0.840291267667425));
#87960=DIRECTION('center_axis',(-0.137791343910941,0.987363722360094,0.0782714846571654));
#87961=DIRECTION('ref_axis',(-0.59910710905729,-0.0201568003086184,-0.800415126842525));
#87962=DIRECTION('',(0.106643708884049,0.,-0.994297299279976));
#87963=DIRECTION('center_axis',(0.118984681183102,0.987363722010516,-0.104668649085082));
#87964=DIRECTION('ref_axis',(-0.706861150377732,0.0102046904694457,-0.707278713364889));
#87965=DIRECTION('',(0.99429729897422,0.,0.106643711734782));
#87966=DIRECTION('center_axis',(3.67961618320588E-14,-1.,3.6687120789681E-14));
#87967=DIRECTION('ref_axis',(1.,3.67961618320588E-14,3.26072068933872E-31));
#87968=DIRECTION('center_axis',(0.132363795311791,-0.987363723319243,-0.0871361208903633));
#87969=DIRECTION('ref_axis',(-0.650288534780861,-0.020156459527977,-0.759419869816335));
#87970=DIRECTION('center_axis',(-0.101878638104898,-0.987363722508935,0.12138213448111));
#87971=DIRECTION('ref_axis',(-0.70993857336524,-0.0133103689258311,-0.704137810465527));
#87972=DIRECTION('center_axis',(-0.117743803763562,0.987363722339622,0.106062606430982));
#87973=DIRECTION('ref_axis',(-0.757165912618984,-0.0201568014598007,-0.652911543873112));
#87974=DIRECTION('',(-0.109594089288496,0.,-0.993976426075098));
#87975=DIRECTION('center_axis',(0.0937022149624435,0.987363721983078,-0.127799747350516));
#87976=DIRECTION('ref_axis',(-0.842379146931304,0.0102046844862637,-0.538788675855223));
#87977=DIRECTION('',(0.993976426077082,0.,-0.109594089270505));
#87978=DIRECTION('center_axis',(-0.0921906923785673,0.987363722375303,0.128894359752262));
#87979=DIRECTION('ref_axis',(-0.879820474071797,-0.0201567989720614,-0.4748785495885));
#87980=DIRECTION('',(-0.32070739268036,0.,-0.947178319156517));
#87981=DIRECTION('center_axis',(1.87810864945458E-14,-1.,1.19654184080002E-14));
#87982=DIRECTION('ref_axis',(1.,1.87810864945458E-14,1.40607568508052E-31));
#87983=DIRECTION('center_axis',(0.1105375112111,-0.987363723357273,-0.113553231628687));
#87984=DIRECTION('ref_axis',(-0.798337974541286,-0.0201564572799021,-0.60187224195442));
#87985=DIRECTION('center_axis',(-0.0734032001647778,-0.987363722506507,
0.140445183910534));
#87986=DIRECTION('ref_axis',(-0.844709418820668,-0.0133103702887437,-0.535059652560746));
#87987=DIRECTION('',(0.947178320273384,0.,-0.320707389381802));
#87988=DIRECTION('center_axis',(0.0640383463728579,0.98736372199852,-0.144955064330502));
#87989=DIRECTION('ref_axis',(-0.938508429326151,0.0102046901058309,-0.345105480083415));
#87990=DIRECTION('center_axis',(2.0914206087111E-14,-1.,7.64829502003661E-15));
#87991=DIRECTION('ref_axis',(1.,2.0914206087111E-14,-8.25113485215167E-32));
#87992=DIRECTION('center_axis',(-0.0623268462666147,0.987363722417612,0.145699155413112));
#87993=DIRECTION('ref_axis',(-0.961335611757529,-0.0201567975226239,-0.274640756408094));
#87994=DIRECTION('center_axis',(0.083542615329035,-0.987363723423162,-0.134660718444295));
#87995=DIRECTION('ref_axis',(-0.909058017628497,-0.0201564551633859,-0.416181736625472));
#87996=DIRECTION('center_axis',(-0.0414955103318477,-0.987363722492924,
0.152941172112732));
#87997=DIRECTION('ref_axis',(-0.939982590838262,-0.0133103712526337,-0.340962700215295));
#87998=DIRECTION('',(-0.516824771977019,0.,-0.856091207215039));
#87999=DIRECTION('center_axis',(0.031380114436834,0.987363721969213,-0.155332446568753));
#88000=DIRECTION('ref_axis',(-0.990754100555664,0.0102046929717233,-0.135285536823009));
#88001=DIRECTION('',(0.856091208538387,0.,-0.516824769784967));
#88002=DIRECTION('center_axis',(0.,-1.,0.));
#88003=DIRECTION('ref_axis',(0.,0.,-1.));
#88004=DIRECTION('center_axis',(0.0526413608956559,-0.987363723435698,-0.149471618597803));
#88005=DIRECTION('ref_axis',(-0.977271517149688,-0.0201564542919456,-0.211031038281868));
#88006=DIRECTION('center_axis',(-0.00764753659104346,-0.987363722466829,
0.158285800817808));
#88007=DIRECTION('ref_axis',(-0.991303222019907,-0.0133103718993134,-0.130922710072981));
#88008=DIRECTION('center_axis',(-0.0295486682057246,0.987363722391953,0.15569121976391));
#88009=DIRECTION('ref_axis',(-0.997899763805172,-0.0201567984337628,-0.0615610662227575));
#88010=DIRECTION('',(-0.688775998780597,0.,-0.724974222647806));
#88011=DIRECTION('center_axis',(-0.00274542668702897,0.98736372204418,-0.158446656712502));
#88012=DIRECTION('ref_axis',(-0.996673211614824,0.0102046860210861,0.0808602104412514));
#88013=DIRECTION('',(0.72497422441144,0.,-0.688775996924277));
#88014=DIRECTION('center_axis',(-4.43853102088631E-14,-1.,3.68048528203422E-15));
#88015=DIRECTION('ref_axis',(1.,-4.43853102088631E-14,1.95112896246476E-32));
#88016=DIRECTION('center_axis',(0.0192786622826518,-0.987363723284348,-0.157293391859486));
#88017=DIRECTION('ref_axis',(-0.999788887210023,-0.0201564613367866,0.00398723936106009));
#88018=DIRECTION('center_axis',(0.0265580251024745,-0.987363722489466,0.156229161216469));
#88019=DIRECTION('ref_axis',(-0.996271616158001,-0.0133103700314487,0.08523908075261));
#88020=DIRECTION('center_axis',(0.00461116960966125,0.987363722328054,0.158403336282166));
#88021=DIRECTION('ref_axis',(-0.987803231645009,-0.0201568018434885,0.154397146641767));
#88022=DIRECTION('',(-0.828520826199668,0.,-0.559958248937739));
#88023=DIRECTION('center_axis',(-0.0367425811626304,0.987363721979082,-0.154152078315933));
#88024=DIRECTION('ref_axis',(-0.955988990855962,0.0102046928250184,0.293225022135811));
#88025=DIRECTION('',(0.559958251059167,0.,-0.828520824765895));
#88026=DIRECTION('center_axis',(2.83709405267036E-14,-1.,-8.75731150790327E-15));
#88027=DIRECTION('ref_axis',(1.,2.83709405267036E-14,7.1912366624173E-32));
#88028=DIRECTION('center_axis',(-0.0149854919521789,-0.98736372325921,-0.157760302429548));
#88029=DIRECTION('ref_axis',(-0.975557240018475,-0.0201564612391877,0.218819077134168));
#88030=DIRECTION('center_axis',(0.0595217627739908,-0.987363722497261,0.146867420664453));
#88031=DIRECTION('ref_axis',(-0.954655456726566,-0.0133103678476456,0.297415186313596));
#88032=DIRECTION('center_axis',(0.0385553986902689,0.987363722351512,0.153708688811013));
#88033=DIRECTION('ref_axis',(-0.931518118380999,-0.0201568010621421,0.363135922897837));
#88034=DIRECTION('',(-0.929524940202268,0.,-0.368759251466278));
#88035=DIRECTION('center_axis',(-0.0690217051008174,0.987363722050075,-0.142649516663741));
#88036=DIRECTION('ref_axis',(-0.870603787481898,0.0102046870362355,0.491878958265819));
#88037=DIRECTION('',(0.368759251362441,0.,-0.929524940243462));
#88038=DIRECTION('center_axis',(-1.29125402862554E-14,-1.,7.32574199636004E-15));
#88039=DIRECTION('ref_axis',(1.,-1.29125402862554E-14,-8.16791645553628E-32));
#88040=DIRECTION('center_axis',(-0.0485489464021499,-0.98736372345918,-0.150850513423275));
#88041=DIRECTION('ref_axis',(-0.905709621322346,-0.0201564548701381,0.423419176669174));
#88042=DIRECTION('center_axis',(0.0897023316329448,-0.987363722499683,0.130638322062027));
#88043=DIRECTION('ref_axis',(-0.868400668737379,-0.0133103683712337,0.495684488995061));
#88044=DIRECTION('center_axis',(0.070696815366875,0.987363722280158,0.141826796558527));
#88045=DIRECTION('ref_axis',(-0.831676253499289,-0.020156805758294,0.554894866210716));
#88046=DIRECTION('',(-0.987065502661801,0.,-0.160317477072854));
